#195096=CARTESIAN_POINT('Ctrl Pts',(-0.153561366595031,59.100861741971,
40.0326492435185));
#195097=CARTESIAN_POINT('Ctrl Pts',(-0.151842962926936,59.0985314603578,
40.0348233715062));
#195098=CARTESIAN_POINT('Ctrl Pts',(-0.150055686179523,59.096225375957,
40.0369753512356));
#195099=CARTESIAN_POINT('Ctrl Pts',(-0.148286670996087,59.0939428540559,
40.0391053430352));
#195100=CARTESIAN_POINT('Ctrl Pts',(-0.146452235168277,59.0916862380348,
40.041211089324));
#195101=CARTESIAN_POINT('Ctrl Pts',(-0.14455211660934,59.0894604907299,
40.0432881154904));
#195102=CARTESIAN_POINT('Ctrl Pts',(-0.144419986080793,59.0893057166152,
40.043432547828));
#195103=CARTESIAN_POINT('Ctrl Pts',(-0.144287542501473,59.0891510807051,
40.0435768364421));
#195104=CARTESIAN_POINT('Ctrl Pts',(-0.144154785043317,59.0889965840074,
40.0437209807855));
#195105=CARTESIAN_POINT('Ctrl Pts',(-0.138334211748934,59.0822228828154,
40.0500407968419));
#195106=CARTESIAN_POINT('Ctrl Pts',(-0.131883990153598,59.0757535782847,
40.0560490279343));
#195107=CARTESIAN_POINT('Ctrl Pts',(-0.12480841721487,59.0697047694309,
40.0616647108613));
#195108=CARTESIAN_POINT('Ctrl Pts',(-0.118212753509711,59.0640662283034,
40.0668995033484));
#195109=CARTESIAN_POINT('Ctrl Pts',(-0.111072931137106,59.0587927761315,
40.0717933267479));
#195110=CARTESIAN_POINT('Ctrl Pts',(-0.10338954476808,59.05400766547,40.076246030307));
#195111=CARTESIAN_POINT('Ctrl Pts',(-0.100578862632356,59.0522572100839,
40.0778748868746));
#195112=CARTESIAN_POINT('Ctrl Pts',(-0.0976954648433502,59.0505724231958,
40.0794443522247));
#195113=CARTESIAN_POINT('Ctrl Pts',(-0.0947395585247239,59.048960544286,
40.0809482021492));
#195114=CARTESIAN_POINT('Ctrl Pts',(-0.0940287618032278,59.0485729412563,
40.0813098278168));
#195115=CARTESIAN_POINT('Ctrl Pts',(-0.0933131922161319,59.0481896206935,
40.0816679525672));
#195116=CARTESIAN_POINT('Ctrl Pts',(-0.0925929271965458,59.0478106940136,
40.082022419258));
#195117=CARTESIAN_POINT('Ctrl Pts',(-0.0918951704588219,59.0474436087926,
40.0823658088648));
#195118=CARTESIAN_POINT('Ctrl Pts',(-0.0911930071928013,59.047080647127,
40.0827057654616));
#195119=CARTESIAN_POINT('Ctrl Pts',(-0.090486511587203,59.0467219102889,
40.0830421470151));
#195120=CARTESIAN_POINT('Ctrl Pts',(-0.0827460357491811,59.0427915336441,
40.0867275956807));
#195121=CARTESIAN_POINT('Ctrl Pts',(-0.0744802459935432,59.0393660724129,
40.0899823432031));
#195122=CARTESIAN_POINT('Ctrl Pts',(-0.0658168714599912,59.0365841602689,
40.0926299529357));
#195123=CARTESIAN_POINT('Ctrl Pts',(-0.0622239118135568,59.0354304183829,
40.0937279956085));
#195124=CARTESIAN_POINT('Ctrl Pts',(-0.0585629032857854,59.0343871039216,
40.0947220371803));
#195125=CARTESIAN_POINT('Ctrl Pts',(-0.0548440714993534,59.0334626554262,
40.0956014538693));
#195126=CARTESIAN_POINT('Ctrl Pts',(-0.0485012163577852,59.0318859121827,
40.097101390674));
#195127=CARTESIAN_POINT('Ctrl Pts',(-0.0419914004937971,59.0306571138137,
40.0982667904316));
#195128=CARTESIAN_POINT('Ctrl Pts',(-0.0353717968082022,59.0298212958157,
40.0990539325583));
#195129=CARTESIAN_POINT('Ctrl Pts',(-0.0320619949654048,59.0294033868167,
40.0994475036216));
#195130=CARTESIAN_POINT('Ctrl Pts',(-0.0287246785540554,59.0290851681639,
40.0997467259952));
#195131=CARTESIAN_POINT('Ctrl Pts',(-0.0253670368742458,59.0288723192866,
40.0999473488896));
#195132=CARTESIAN_POINT('Ctrl Pts',(-0.0220093951944362,59.0286594704093,
40.100147971784));
#195133=CARTESIAN_POINT('Ctrl Pts',(-0.0186314705073834,59.0285519740191,
40.10025));
#195134=CARTESIAN_POINT('Ctrl Pts',(-0.0152399999993761,59.0285534841296,
40.10025));
#195135=CARTESIAN_POINT('Origin',(6.10537907909441,57.9430040808457,39.92499));
#195136=CARTESIAN_POINT('Ctrl Pts',(6.73887200051396,62.2936141127569,39.92499));
#195137=CARTESIAN_POINT('Ctrl Pts',(6.73998108195387,62.3041663177856,39.934835464202));
#195138=CARTESIAN_POINT('Ctrl Pts',(6.74025426844153,62.3147747227671,39.9446440828461));
#195139=CARTESIAN_POINT('Ctrl Pts',(6.73970068257655,62.3253809467526,39.9543641760336));
#195140=CARTESIAN_POINT('Ctrl Pts',(6.73916508495579,62.3356425316146,39.9637684240719));
#195141=CARTESIAN_POINT('Ctrl Pts',(6.73785543637705,62.3459033574831,39.9730909636404));
#195142=CARTESIAN_POINT('Ctrl Pts',(6.73573381164837,62.3561113603653,39.982280897715));
#195143=CARTESIAN_POINT('Ctrl Pts',(6.73372688529716,62.3657675025193,39.990974009466));
#195144=CARTESIAN_POINT('Ctrl Pts',(6.73099321743859,62.3753772873486,39.9995492765013));
#195145=CARTESIAN_POINT('Ctrl Pts',(6.72746117704619,62.3848821415117,40.0079462328707));
#195146=CARTESIAN_POINT('Ctrl Pts',(6.72420791240112,62.3936367996045,40.0156804369703));
#195147=CARTESIAN_POINT('Ctrl Pts',(6.72027708243738,62.4023029415008,40.0232638017437));
#195148=CARTESIAN_POINT('Ctrl Pts',(6.71558140886323,62.4108128192398,40.0306257269982));
#195149=CARTESIAN_POINT('Ctrl Pts',(6.71421937245567,62.4132812112865,40.0327611416662));
#195150=CARTESIAN_POINT('Ctrl Pts',(6.71279278199565,62.415736279296,40.0348777427276));
#195151=CARTESIAN_POINT('Ctrl Pts',(6.71129899689659,62.4181758915948,40.0369733168701));
#195152=CARTESIAN_POINT('Ctrl Pts',(6.70967963780731,62.42082058818,40.039245053974));
#195153=CARTESIAN_POINT('Ctrl Pts',(6.70798448411237,62.4234440047028,40.041487875195));
#195154=CARTESIAN_POINT('Ctrl Pts',(6.70621108803186,62.4260429761972,40.0436985701601));
#195155=CARTESIAN_POINT('Ctrl Pts',(6.70134398857332,62.4331758738575,40.0497658398386));
#195156=CARTESIAN_POINT('Ctrl Pts',(6.69585818364757,62.4400912556837,40.0555581699984));
#195157=CARTESIAN_POINT('Ctrl Pts',(6.68976801333951,62.4466864116141,40.0609828468885));
#195158=CARTESIAN_POINT('Ctrl Pts',(6.68419583815079,62.4527206212309,40.0659461317303));
#195159=CARTESIAN_POINT('Ctrl Pts',(6.67811620689403,62.4584752900412,40.0706039980705));
#195160=CARTESIAN_POINT('Ctrl Pts',(6.67150703079275,62.4638645712583,40.0748843180601));
#195161=CARTESIAN_POINT('Ctrl Pts',(6.66826062508144,62.4665117685875,40.0769867972568));
#195162=CARTESIAN_POINT('Ctrl Pts',(6.66488629458054,62.4690703232299,40.0789976708174));
#195163=CARTESIAN_POINT('Ctrl Pts',(6.66138078591774,62.4715267736418,40.08090504915));
#195164=CARTESIAN_POINT('Ctrl Pts',(6.66071564979311,62.4719928611813,40.0812669556104));
#195165=CARTESIAN_POINT('Ctrl Pts',(6.66004526561052,62.4724551899379,40.0816253922032));
#195166=CARTESIAN_POINT('Ctrl Pts',(6.65936969820921,62.4729136358128,40.0819801989139));
#195167=CARTESIAN_POINT('Ctrl Pts',(6.65871524228918,62.4733577552541,40.0823239179149));
#195168=CARTESIAN_POINT('Ctrl Pts',(6.65805592206515,62.4737982306999,40.0826642303498));
#195169=CARTESIAN_POINT('Ctrl Pts',(6.65739180030973,62.4742349489458,40.0830009916099));
#195170=CARTESIAN_POINT('Ctrl Pts',(6.65015433826458,62.4789942144025,40.0866709464313));
#195171=CARTESIAN_POINT('Ctrl Pts',(6.6423416549749,62.483310062658,40.0899175831879));
#195172=CARTESIAN_POINT('Ctrl Pts',(6.63406423386157,62.4870273554129,40.0925642067064));
#195173=CARTESIAN_POINT('Ctrl Pts',(6.63056862752539,62.4885971912264,40.0936818922529));
#195174=CARTESIAN_POINT('Ctrl Pts',(6.62699051141418,62.490060506939,40.0946930094791));
#195175=CARTESIAN_POINT('Ctrl Pts',(6.62333954252063,62.491407022622,40.0955863397546));
#195176=CARTESIAN_POINT('Ctrl Pts',(6.61719140213135,62.4936745213866,40.0970906856166));
#195177=CARTESIAN_POINT('Ctrl Pts',(6.61083770188589,62.495608491139,40.0982599215483));
#195178=CARTESIAN_POINT('Ctrl Pts',(6.60433062536211,62.4971561593221,40.0990497370454));
#195179=CARTESIAN_POINT('Ctrl Pts',(6.60270385623117,62.4975430763678,40.0992471909196));
#195180=CARTESIAN_POINT('Ctrl Pts',(6.60106746196622,62.4979056188883,40.0994209989363));
#195181=CARTESIAN_POINT('Ctrl Pts',(6.5994222184581,62.4982426563695,40.0995705982975));
#195182=CARTESIAN_POINT('Ctrl Pts',(6.59695435319593,62.4987482125912,40.0997949973393));
#195183=CARTESIAN_POINT('Ctrl Pts',(6.59446659126666,62.4991963674672,40.0999649129781));
#195184=CARTESIAN_POINT('Ctrl Pts',(6.59196174500359,62.4995849724121,40.1000786629733));
#195185=CARTESIAN_POINT('Ctrl Pts',(6.58945689874052,62.4999735773569,40.1001924129685));
#195186=CARTESIAN_POINT('Ctrl Pts',(6.58693497617713,62.5003026407461,40.10025));
#195187=CARTESIAN_POINT('Ctrl Pts',(6.58439859103091,62.500570298093,40.10025));
#195188=CARTESIAN_POINT('Ctrl Pts',(6.18532049829458,58.7035958781038,40.10025));
#195189=CARTESIAN_POINT('Ctrl Pts',(6.19390281910209,58.7026899760169,40.10025));
#195190=CARTESIAN_POINT('Ctrl Pts',(6.20248552904414,58.7025003609928,40.0995786334241));
#195191=CARTESIAN_POINT('Ctrl Pts',(6.21093474935464,58.7029569544313,40.0983063763367));
#195192=CARTESIAN_POINT('Ctrl Pts',(6.21639207873535,58.7032518669434,40.0974846287993));
#195193=CARTESIAN_POINT('Ctrl Pts',(6.22179377937559,58.7038154335198,40.0964130309338));
#195194=CARTESIAN_POINT('Ctrl Pts',(6.22710604846914,58.7046202140515,40.0951176960924));
#195195=CARTESIAN_POINT('Ctrl Pts',(6.23414715684692,58.7056869045457,40.0934008039614));
#195196=CARTESIAN_POINT('Ctrl Pts',(6.24102913891695,58.7071827955651,40.0912909372156));
#195197=CARTESIAN_POINT('Ctrl Pts',(6.247679224408,58.7090548163569,40.0888630467851));
#195198=CARTESIAN_POINT('Ctrl Pts',(6.25100426715352,58.7099908267527,40.0876491015699));
#195199=CARTESIAN_POINT('Ctrl Pts',(6.25427153376716,58.7110208470227,40.0863558569271));
#195200=CARTESIAN_POINT('Ctrl Pts',(6.25747333351573,58.7121380880307,40.0849936342771));
#195201=CARTESIAN_POINT('Ctrl Pts',(6.25907423339001,58.7126967085346,40.0843125229521));
#195202=CARTESIAN_POINT('Ctrl Pts',(6.26065878288398,58.713277132457,40.0836141747074));
#195203=CARTESIAN_POINT('Ctrl Pts',(6.2622261232057,58.7138784999415,40.0828999161609));
#195204=CARTESIAN_POINT('Ctrl Pts',(6.26261795828614,58.7140288418126,40.0827213515243));
#195205=CARTESIAN_POINT('Ctrl Pts',(6.26300871814066,58.7141804926177,40.0825417925842));
#195206=CARTESIAN_POINT('Ctrl Pts',(6.2633983900511,58.7143334388435,40.082361260236));
#195207=CARTESIAN_POINT('Ctrl Pts',(6.26456740578241,58.7147922775207,40.0818196631917));
#195208=CARTESIAN_POINT('Ctrl Pts',(6.26572662828426,58.715262775183,40.0812693052021));
#195209=CARTESIAN_POINT('Ctrl Pts',(6.2668757296522,58.7157445651923,40.0807107531875));
#195210=CARTESIAN_POINT('Ctrl Pts',(6.27496985131196,58.7191382318077,40.0767763849182));
#195211=CARTESIAN_POINT('Ctrl Pts',(6.2826071619282,58.7230632421217,40.0724140586138));
#195212=CARTESIAN_POINT('Ctrl Pts',(6.28978339589494,58.7274000190313,40.0677221223769));
#195213=CARTESIAN_POINT('Ctrl Pts',(6.29326386161416,58.7295033511461,40.0654465383721));
#195214=CARTESIAN_POINT('Ctrl Pts',(6.2966359740898,58.731704109697,40.0630928000679));
#195215=CARTESIAN_POINT('Ctrl Pts',(6.29989941779205,58.7339915094193,40.0606689262479));
#195216=CARTESIAN_POINT('Ctrl Pts',(6.30489552208994,58.7374933585781,40.0569581447805));
#195217=CARTESIAN_POINT('Ctrl Pts',(6.30963480180928,58.7411954596216,40.0530843804605));
#195218=CARTESIAN_POINT('Ctrl Pts',(6.31410463171103,58.7450534628849,40.0490800251457));
#195219=CARTESIAN_POINT('Ctrl Pts',(6.31618044384123,58.7468451395591,40.0472203818218));
#195220=CARTESIAN_POINT('Ctrl Pts',(6.31819823791584,58.7486702031823,40.0453323608818));
#195221=CARTESIAN_POINT('Ctrl Pts',(6.32015576082374,58.7505249478604,40.0434201572162));
#195222=CARTESIAN_POINT('Ctrl Pts',(6.3203057972416,58.750667106732,40.0432735943397));
#195223=CARTESIAN_POINT('Ctrl Pts',(6.32045551058247,58.7508094261758,40.0431268995707));
#195224=CARTESIAN_POINT('Ctrl Pts',(6.32060490094056,58.7509519047345,40.0429800745037));
#195225=CARTESIAN_POINT('Ctrl Pts',(6.3227033850744,58.7529532989256,40.0409176249753));
#195226=CARTESIAN_POINT('Ctrl Pts',(6.32473679726686,58.7549876922214,40.0388310783332));
#195227=CARTESIAN_POINT('Ctrl Pts',(6.32670504965044,58.7570493794209,40.036725739981));
#195228=CARTESIAN_POINT('Ctrl Pts',(6.3337628526564,58.7644422230598,40.0291763710714));
#195229=CARTESIAN_POINT('Ctrl Pts',(6.34003880539004,58.7722418109929,40.0213310894587));
#195230=CARTESIAN_POINT('Ctrl Pts',(6.34560292136835,58.7803396486563,40.0132837551308));
#195231=CARTESIAN_POINT('Ctrl Pts',(6.35171732586353,58.7892383587484,40.0044405431308));
#195232=CARTESIAN_POINT('Ctrl Pts',(6.35697262978608,58.7984976730916,39.9953528710578));
#195233=CARTESIAN_POINT('Ctrl Pts',(6.36142852992988,58.8080148760677,39.9861103629527));
#195234=CARTESIAN_POINT('Ctrl Pts',(6.36623978380702,58.8182910667901,39.9761307737519));
#195235=CARTESIAN_POINT('Ctrl Pts',(6.3701196826395,58.8288688921899,39.9659696935964));
#195236=CARTESIAN_POINT('Ctrl Pts',(6.37309732670023,58.8396533761938,39.9557128217449));
#195237=CARTESIAN_POINT('Ctrl Pts',(6.37604999138599,58.8503473894549,39.9455419945122));
#195238=CARTESIAN_POINT('Ctrl Pts',(6.37811557911308,58.8612460403482,39.9352756289321));
#195239=CARTESIAN_POINT('Ctrl Pts',(6.37927424642637,58.872270023448,39.92499));
#195240=CARTESIAN_POINT('Origin',(-0.0151565136854075,0.0015930137801936,
39.92499));
#195241=CARTESIAN_POINT('Ctrl Pts',(6.55408556366009,62.5037563256534,40.10025));
#195242=CARTESIAN_POINT('Ctrl Pts',(6.54554330587477,62.5046505412977,40.10025));
#195243=CARTESIAN_POINT('Ctrl Pts',(6.53700226086738,62.5048232320878,40.0995859581842));
#195244=CARTESIAN_POINT('Ctrl Pts',(6.5285945717753,62.5043472028589,40.0983275959621));
#195245=CARTESIAN_POINT('Ctrl Pts',(6.52322245869558,62.5040430428431,40.0975235624068));
#195246=CARTESIAN_POINT('Ctrl Pts',(6.51790471489673,62.5034749678471,40.096477705949));
#195247=CARTESIAN_POINT('Ctrl Pts',(6.51267356740911,62.5026702669706,40.0952149915961));
#195248=CARTESIAN_POINT('Ctrl Pts',(6.50553410072716,62.5015720117389,40.0934916398701));
#195249=CARTESIAN_POINT('Ctrl Pts',(6.49855818190839,62.5000273428097,40.091364392163));
#195250=CARTESIAN_POINT('Ctrl Pts',(6.49182203260242,62.4980940659028,40.0889118607713));
#195251=CARTESIAN_POINT('Ctrl Pts',(6.48845395794943,62.4971274274494,40.0876855950754));
#195252=CARTESIAN_POINT('Ctrl Pts',(6.48514561818799,62.4960636607365,40.0863782327526));
#195253=CARTESIAN_POINT('Ctrl Pts',(6.48190505740227,62.4949101555729,40.0850006373334));
#195254=CARTESIAN_POINT('Ctrl Pts',(6.48028477700941,62.4943334029911,40.0843118396237));
#195255=CARTESIAN_POINT('Ctrl Pts',(6.47868142404744,62.4937342176672,40.0836054919164));
#195256=CARTESIAN_POINT('Ctrl Pts',(6.47709589524329,62.4931135352113,40.0828829920417));
#195257=CARTESIAN_POINT('Ctrl Pts',(6.47669951304225,62.4929583645973,40.0827023670731));
#195258=CARTESIAN_POINT('Ctrl Pts',(6.47630424448236,62.4928018504534,40.0825207326933));
#195259=CARTESIAN_POINT('Ctrl Pts',(6.47591010283136,62.4926440074816,40.0823381109275));
#195260=CARTESIAN_POINT('Ctrl Pts',(6.47472767787837,62.492170478566,40.0817902456303));
#195261=CARTESIAN_POINT('Ctrl Pts',(6.47355539694531,62.4916849899863,40.0812334935553));
#195262=CARTESIAN_POINT('Ctrl Pts',(6.47239360181873,62.4911879405751,40.0806684524227));
#195263=CARTESIAN_POINT('Ctrl Pts',(6.46436487665231,62.4877530207468,40.0767636676136));
#195264=CARTESIAN_POINT('Ctrl Pts',(6.45678933786444,62.4837949925046,40.0724404510887));
#195265=CARTESIAN_POINT('Ctrl Pts',(6.44966853564036,62.4794326364364,40.0677949937408));
#195266=CARTESIAN_POINT('Ctrl Pts',(6.44612951648131,62.4772645574451,40.0654862141905));
#195267=CARTESIAN_POINT('Ctrl Pts',(6.44270272394404,62.474996003895,40.0630972003215));
#195268=CARTESIAN_POINT('Ctrl Pts',(6.43938822718986,62.4726384024733,40.0606363359906));
#195269=CARTESIAN_POINT('Ctrl Pts',(6.43207595228416,62.4674371815966,40.0552073017123));
#195270=CARTESIAN_POINT('Ctrl Pts',(6.42530381744052,62.4618132330509,40.0494204304519));
#195271=CARTESIAN_POINT('Ctrl Pts',(6.41913840445487,62.455895762341,40.0434049749851));
#195272=CARTESIAN_POINT('Ctrl Pts',(6.41688610134127,62.4537340356674,40.0412074532442));
#195273=CARTESIAN_POINT('Ctrl Pts',(6.4147074139753,62.4515361835425,40.0389814735788));
#195274=CARTESIAN_POINT('Ctrl Pts',(6.41260146153701,62.4493074469122,40.0367321210017));
#195275=CARTESIAN_POINT('Ctrl Pts',(6.40552779014142,62.4418213564085,40.0291767837138));
#195276=CARTESIAN_POINT('Ctrl Pts',(6.39923601079921,62.4339335724859,40.0213235332571));
#195277=CARTESIAN_POINT('Ctrl Pts',(6.39365709371064,62.4257522463021,40.0132649215851));
#195278=CARTESIAN_POINT('Ctrl Pts',(6.38752520296412,62.4167599996842,40.0044075527522));
#195279=CARTESIAN_POINT('Ctrl Pts',(6.38225398283479,62.4074126717497,39.9953016253706));
#195280=CARTESIAN_POINT('Ctrl Pts',(6.37778536209598,62.3978127557438,39.9860353422341));
#195281=CARTESIAN_POINT('Ctrl Pts',(6.3729724660951,62.3874732348817,39.9760551582674));
#195282=CARTESIAN_POINT('Ctrl Pts',(6.36908997057791,62.3768396913499,39.9658879738131));
#195283=CARTESIAN_POINT('Ctrl Pts',(6.36611161569965,62.3660067738133,39.9556174643225));
#195284=CARTESIAN_POINT('Ctrl Pts',(6.36317347866869,62.355320137241,39.9454856413885));
#195285=CARTESIAN_POINT('Ctrl Pts',(6.36111515612501,62.344438041129,39.9352519465104));
#195286=CARTESIAN_POINT('Ctrl Pts',(6.35995915837865,62.3334394572618,39.92499));
#195287=CARTESIAN_POINT('Ctrl Pts',(6.00036140429106,58.9120953679529,39.92499));
#195288=CARTESIAN_POINT('Ctrl Pts',(5.99925510810176,58.9015696628136,39.9348107241731));
#195289=CARTESIAN_POINT('Ctrl Pts',(5.99898299131239,58.8909945468879,39.9446038383187));
#195290=CARTESIAN_POINT('Ctrl Pts',(5.99953795195324,58.8804276387757,39.9543158069411));
#195291=CARTESIAN_POINT('Ctrl Pts',(6.00007381527955,58.8702243592762,39.9636935671423));
#195292=CARTESIAN_POINT('Ctrl Pts',(6.0013809572776,58.8600274753995,39.9729968321026));
#195293=CARTESIAN_POINT('Ctrl Pts',(6.00349883564084,58.8498890377446,39.9821731151378));
#195294=CARTESIAN_POINT('Ctrl Pts',(6.00550089397251,58.8403050389987,39.9908475764398));
#195295=CARTESIAN_POINT('Ctrl Pts',(6.00822762538762,58.8307723843828,39.9994093733896));
#195296=CARTESIAN_POINT('Ctrl Pts',(6.01175153639814,58.8213500689001,40.0077966115894));
#195297=CARTESIAN_POINT('Ctrl Pts',(6.01499699932078,58.8126722744117,40.015521117265));
#195298=CARTESIAN_POINT('Ctrl Pts',(6.01891888229525,58.8040875818502,40.0230979941079));
#195299=CARTESIAN_POINT('Ctrl Pts',(6.02360485257848,58.7956642413002,40.0304554104807));
#195300=CARTESIAN_POINT('Ctrl Pts',(6.0250021143232,58.7931525711866,40.032649243522));
#195301=CARTESIAN_POINT('Ctrl Pts',(6.02646752363906,58.7906554330073,40.034823371508));
#195302=CARTESIAN_POINT('Ctrl Pts',(6.02800395803763,58.7881751602883,40.0369753512355));
#195303=CARTESIAN_POINT('Ctrl Pts',(6.0295246938641,58.7857202298424,40.0391053430351));
#195304=CARTESIAN_POINT('Ctrl Pts',(6.03111319985562,58.7832842250419,40.041211089324));
#195305=CARTESIAN_POINT('Ctrl Pts',(6.03277025542088,58.7808720541406,40.0432881154904));
#195306=CARTESIAN_POINT('Ctrl Pts',(6.0328854838242,58.7807043164936,40.0434325478279));
#195307=CARTESIAN_POINT('Ctrl Pts',(6.03300103800968,58.7805366835714,40.0435768364421));
#195308=CARTESIAN_POINT('Ctrl Pts',(6.0331169189062,58.7803691562897,40.0437209807855));
#195309=CARTESIAN_POINT('Ctrl Pts',(6.03819756191488,58.7730241465597,40.050040796842));
#195310=CARTESIAN_POINT('Ctrl Pts',(6.04393622206048,58.7659160498049,40.0560490279345));
#195311=CARTESIAN_POINT('Ctrl Pts',(6.05034076157633,58.7591607781928,40.0616647108615));
#195312=CARTESIAN_POINT('Ctrl Pts',(6.05631090550653,58.7528636909922,40.0668995033486));
#195313=CARTESIAN_POINT('Ctrl Pts',(6.06286038933357,58.7468728126824,40.0717933267482));
#195314=CARTESIAN_POINT('Ctrl Pts',(6.07000150504423,58.741310782788,40.0762460303072));
#195315=CARTESIAN_POINT('Ctrl Pts',(6.07261381755745,58.7392761202953,40.0778748868748));
#195316=CARTESIAN_POINT('Ctrl Pts',(6.07530531160718,58.7372991657064,40.0794443522247));
#195317=CARTESIAN_POINT('Ctrl Pts',(6.07807653793614,58.735387140493,40.0809482021492));
#195318=CARTESIAN_POINT('Ctrl Pts',(6.07874292528977,58.7349273623042,40.0813098278168));
#195319=CARTESIAN_POINT('Ctrl Pts',(6.07941450700242,58.7344713442222,40.0816679525672));
#195320=CARTESIAN_POINT('Ctrl Pts',(6.08009121771133,58.7340192051468,40.082022419258));
#195321=CARTESIAN_POINT('Ctrl Pts',(6.0807467812106,58.7335811954174,40.0823658088648));
#195322=CARTESIAN_POINT('Ctrl Pts',(6.08140715812765,58.7331468260467,40.0827057654616));
#195323=CARTESIAN_POINT('Ctrl Pts',(6.08207228526599,58.7327162055065,40.0830421470151));
#195324=CARTESIAN_POINT('Ctrl Pts',(6.08935952173653,58.727998259832,40.0867275956806));
#195325=CARTESIAN_POINT('Ctrl Pts',(6.09722197243233,58.7237275533351,40.089982343203));
#195326=CARTESIAN_POINT('Ctrl Pts',(6.10554709909211,58.7200553115703,40.0926299529355));
#195327=CARTESIAN_POINT('Ctrl Pts',(6.10899977726353,58.7185323234525,40.0937279956084));
#195328=CARTESIAN_POINT('Ctrl Pts',(6.11253167434641,58.7171120447815,40.0947220371802));
#195329=CARTESIAN_POINT('Ctrl Pts',(6.11613350280284,58.7158039367398,40.0956014538692));
#195330=CARTESIAN_POINT('Ctrl Pts',(6.12227679657208,58.7135728221601,40.097101390674));
#195331=CARTESIAN_POINT('Ctrl Pts',(6.12862250657844,58.7116702942287,40.0982667904316));
#195332=CARTESIAN_POINT('Ctrl Pts',(6.13511848061154,58.7101471179285,40.0990539325582));
#195333=CARTESIAN_POINT('Ctrl Pts',(6.13836646762808,58.7093855297784,40.0994475036216));
#195334=CARTESIAN_POINT('Ctrl Pts',(6.14165223896418,58.7087202098048,40.0997467259952));
#195335=CARTESIAN_POINT('Ctrl Pts',(6.14496923836549,58.7081575578109,40.0999473488896));
#195336=CARTESIAN_POINT('Ctrl Pts',(6.14828623776681,58.707594905817,40.100147971784));
#195337=CARTESIAN_POINT('Ctrl Pts',(6.15163442139651,58.7071349090266,40.10025));
#195338=CARTESIAN_POINT('Ctrl Pts',(6.15500747092375,58.7067819056642,40.10025));
#195339=CARTESIAN_POINT('Origin',(12.128626347365,56.9874003490101,39.92499));
#195340=CARTESIAN_POINT('Ctrl Pts',(13.21341150919,61.2479592423876,39.92499));
#195341=CARTESIAN_POINT('Ctrl Pts',(13.2156175207415,61.2583377107545,39.9348354642021));
#195342=CARTESIAN_POINT('Ctrl Pts',(13.2169980909554,61.2688594460197,39.9446440828464));
#195343=CARTESIAN_POINT('Ctrl Pts',(13.217556189986,61.2794654334803,39.954364176034));
#195344=CARTESIAN_POINT('Ctrl Pts',(13.2180961541214,61.2897267895029,39.9637684240723));
#195345=CARTESIAN_POINT('Ctrl Pts',(13.2178662282945,61.3000683010471,39.9730909636408));
#195346=CARTESIAN_POINT('Ctrl Pts',(13.2168232529023,61.310442153594,39.9822808977153));
#195347=CARTESIAN_POINT('Ctrl Pts',(13.2158366624041,61.3202551793184,39.9909740094663));
#195348=CARTESIAN_POINT('Ctrl Pts',(13.2141224659046,61.3300980668413,39.9995492765015));
#195349=CARTESIAN_POINT('Ctrl Pts',(13.2116033021983,61.3399200511732,40.0079462328709));
#195350=CARTESIAN_POINT('Ctrl Pts',(13.2092829702343,61.3489668090869,40.0156804369705));
#195351=CARTESIAN_POINT('Ctrl Pts',(13.2062795322632,61.3579963605666,40.0232638017438));
#195352=CARTESIAN_POINT('Ctrl Pts',(13.2024991065229,61.3669504518477,40.0306257269983));
#195353=CARTESIAN_POINT('Ctrl Pts',(13.2014025487207,61.3695476933571,40.0327611416663));
#195354=CARTESIAN_POINT('Ctrl Pts',(13.2002403977587,61.3721384315556,40.0348777427276));
#195355=CARTESIAN_POINT('Ctrl Pts',(13.1990098046953,61.3747208224638,40.0369733168701));
#195356=CARTESIAN_POINT('Ctrl Pts',(13.1976757626944,61.3775203002415,40.039245053974));
#195357=CARTESIAN_POINT('Ctrl Pts',(13.1962641169264,61.3803065372248,40.041487875195));
#195358=CARTESIAN_POINT('Ctrl Pts',(13.1947721021916,61.3830766416485,40.0436985701601));
#195359=CARTESIAN_POINT('Ctrl Pts',(13.1906772560442,61.390679214976,40.0497658398386));
#195360=CARTESIAN_POINT('Ctrl Pts',(13.185944357167,61.3981301363757,40.0555581699984));
#195361=CARTESIAN_POINT('Ctrl Pts',(13.1805769309636,61.4053257594952,40.0609828468885));
#195362=CARTESIAN_POINT('Ctrl Pts',(13.1756660273918,61.41190936399,40.0659461317304));
#195363=CARTESIAN_POINT('Ctrl Pts',(13.1702212276784,61.418268002635,40.0706039980706));
#195364=CARTESIAN_POINT('Ctrl Pts',(13.164211590619,61.4243186078272,40.0748843180603));
#195365=CARTESIAN_POINT('Ctrl Pts',(13.1612596765267,61.4272906453324,40.0769867972569));
#195366=CARTESIAN_POINT('Ctrl Pts',(13.1581712727464,61.4301878975265,40.0789976708174));
#195367=CARTESIAN_POINT('Ctrl Pts',(13.1549417366136,61.4329973166794,40.0809050491499));
#195368=CARTESIAN_POINT('Ctrl Pts',(13.1543289635885,61.4335303765996,40.0812669556104));
#195369=CARTESIAN_POINT('Ctrl Pts',(13.1537105783551,61.4340602468993,40.0816253922032));
#195370=CARTESIAN_POINT('Ctrl Pts',(13.1530866324254,61.434586797382,40.0819801989139));
#195371=CARTESIAN_POINT('Ctrl Pts',(13.1524821848061,61.4350968931621,40.0823239179149));
#195372=CARTESIAN_POINT('Ctrl Pts',(13.1518725186287,61.4356038733671,40.0826642303498));
#195373=CARTESIAN_POINT('Ctrl Pts',(13.1512576844889,61.4361076188514,40.0830009916099));
#195374=CARTESIAN_POINT('Ctrl Pts',(13.1445573487227,61.4415973333394,40.0866709464312));
#195375=CARTESIAN_POINT('Ctrl Pts',(13.1372385931155,61.4467061867047,40.0899175831878));
#195376=CARTESIAN_POINT('Ctrl Pts',(13.1293950794805,61.4512683418497,40.0925642067062));
#195377=CARTESIAN_POINT('Ctrl Pts',(13.1260827149666,61.453194968297,40.0936818922528));
#195378=CARTESIAN_POINT('Ctrl Pts',(13.1226771582924,61.4550242827915,40.094693009479));
#195379=CARTESIAN_POINT('Ctrl Pts',(13.1191869390034,61.4567450522887,40.0955863397545));
#195380=CARTESIAN_POINT('Ctrl Pts',(13.1133094969318,61.4596427851247,40.0970906856166));
#195381=CARTESIAN_POINT('Ctrl Pts',(13.1071927578073,61.4622303029111,40.0982599215483));
#195382=CARTESIAN_POINT('Ctrl Pts',(13.1008831031063,61.464449667515,40.0990497370454));
#195383=CARTESIAN_POINT('Ctrl Pts',(13.0993056894311,61.465004508666,40.0992471909196));
#195384=CARTESIAN_POINT('Ctrl Pts',(13.0977161555177,61.4655361149184,40.0994209989363));
#195385=CARTESIAN_POINT('Ctrl Pts',(13.0961151548356,61.4660432808487,40.0995705982975));
#195386=CARTESIAN_POINT('Ctrl Pts',(13.0937136538125,61.466804029744,40.0997949973393));
#195387=CARTESIAN_POINT('Ctrl Pts',(13.0912863650439,61.4675097715122,40.0999649129781));
#195388=CARTESIAN_POINT('Ctrl Pts',(13.0888358608685,61.4681580753691,40.1000786629733));
#195389=CARTESIAN_POINT('Ctrl Pts',(13.086385356693,61.4688063792261,40.1001924129685));
#195390=CARTESIAN_POINT('Ctrl Pts',(13.0839116459757,61.4693972526618,40.10025));
#195391=CARTESIAN_POINT('Ctrl Pts',(13.0814171332239,61.4699285681953,40.10025));
#195392=CARTESIAN_POINT('Ctrl Pts',(12.2876333308477,57.7354693911203,40.10025));
#195393=CARTESIAN_POINT('Ctrl Pts',(12.2960739442514,57.7336713548545,40.10025));
#195394=CARTESIAN_POINT('Ctrl Pts',(12.3045898170438,57.7325856410803,40.099578633424));
#195395=CARTESIAN_POINT('Ctrl Pts',(12.3130404786523,57.7321565492374,40.0983063763364));
#195396=CARTESIAN_POINT('Ctrl Pts',(12.3184987389629,57.7318793999342,40.0974846287991));
#195397=CARTESIAN_POINT('Ctrl Pts',(12.3239297572695,57.731875247767,40.0964130309337));
#195398=CARTESIAN_POINT('Ctrl Pts',(12.3292970476689,57.732120336302,40.0951176960923));
#195399=CARTESIAN_POINT('Ctrl Pts',(12.3364110836364,57.7324451871156,40.0934008039614));
#195400=CARTESIAN_POINT('Ctrl Pts',(12.3434117286781,57.7332135204775,40.0912909372156));
#195401=CARTESIAN_POINT('Ctrl Pts',(12.3502210637615,57.7343801629265,40.0888630467851));
#195402=CARTESIAN_POINT('Ctrl Pts',(12.3536257313032,57.734963484151,40.0876491015699));
#195403=CARTESIAN_POINT('Ctrl Pts',(12.3569827659245,57.735646339504,40.0863558569271));
#195404=CARTESIAN_POINT('Ctrl Pts',(12.3602838093647,57.7364227809414,40.0849936342771));
#195405=CARTESIAN_POINT('Ctrl Pts',(12.3619343310847,57.7368110016601,40.0843125229521));
#195406=CARTESIAN_POINT('Ctrl Pts',(12.3635708710714,57.7372226154359,40.0836141747074));
#195407=CARTESIAN_POINT('Ctrl Pts',(12.3651924853579,57.7376568568911,40.0828999161609));
#195408=CARTESIAN_POINT('Ctrl Pts',(12.3655978889295,57.7377654172549,40.0827213515243));
#195409=CARTESIAN_POINT('Ctrl Pts',(12.3660023599863,57.737875391774,40.0825417925841));
#195410=CARTESIAN_POINT('Ctrl Pts',(12.3664058844671,57.7379867683383,40.082361260236));
#195411=CARTESIAN_POINT('Ctrl Pts',(12.3676164579098,57.7383208980313,40.0818196631917));
#195412=CARTESIAN_POINT('Ctrl Pts',(12.3688185104671,57.7386676465114,40.0812693052021));
#195413=CARTESIAN_POINT('Ctrl Pts',(12.3700116777068,57.7390266834245,40.0807107531874));
#195414=CARTESIAN_POINT('Ctrl Pts',(12.3784161936773,57.7415556930806,40.0767763849182));
#195415=CARTESIAN_POINT('Ctrl Pts',(12.3864219416033,57.7446608854351,40.0724140586138));
#195416=CARTESIAN_POINT('Ctrl Pts',(12.3940121800354,57.7482237843184,40.0677221223769));
#195417=CARTESIAN_POINT('Ctrl Pts',(12.397693437473,57.7499517864267,40.0654465383721));
#195418=CARTESIAN_POINT('Ctrl Pts',(12.401277119073,57.751788007257,40.0630928000679));
#195419=CARTESIAN_POINT('Ctrl Pts',(12.4047617836671,57.7537217536092,40.0606689262479));
#195420=CARTESIAN_POINT('Ctrl Pts',(12.410096561694,57.7566821841673,40.0569581447805));
#195421=CARTESIAN_POINT('Ctrl Pts',(12.4151968540761,57.7598686150879,40.0530843804606));
#195422=CARTESIAN_POINT('Ctrl Pts',(12.4200454689344,57.763238259355,40.0490800251458));
#195423=CARTESIAN_POINT('Ctrl Pts',(12.422297190758,57.7648031395848,40.0472203818218));
#195424=CARTESIAN_POINT('Ctrl Pts',(12.4244947022414,57.7664072884047,40.0453323608818));
#195425=CARTESIAN_POINT('Ctrl Pts',(12.426635375245,57.7680472557361,40.0434201572162));
#195426=CARTESIAN_POINT('Ctrl Pts',(12.426799449396,57.7681729527702,40.0432735943397));
#195427=CARTESIAN_POINT('Ctrl Pts',(12.4269632190243,57.7682988432678,40.0431268995707));
#195428=CARTESIAN_POINT('Ctrl Pts',(12.4271266840712,57.7684249257695,40.0429800745037));
#195429=CARTESIAN_POINT('Ctrl Pts',(12.4294228751485,57.7701960047921,40.0409176249753));
#195430=CARTESIAN_POINT('Ctrl Pts',(12.4316578001011,57.7720067040169,40.0388310783332));
#195431=CARTESIAN_POINT('Ctrl Pts',(12.4338307751869,57.7738513586812,40.036725739981));
#195432=CARTESIAN_POINT('Ctrl Pts',(12.4416226773936,57.7804659622463,40.029176371072));
#195433=CARTESIAN_POINT('Ctrl Pts',(12.4486795287417,57.7875668075252,40.02133108946));
#195434=CARTESIAN_POINT('Ctrl Pts',(12.4550596184368,57.7950386758933,40.0132837551328));
#195435=CARTESIAN_POINT('Ctrl Pts',(12.4620706960749,57.8032495086139,40.0044405431337));
#195436=CARTESIAN_POINT('Ctrl Pts',(12.4682650727914,57.8119087706204,39.9953528710616));
#195437=CARTESIAN_POINT('Ctrl Pts',(12.4736913816495,57.8209080689672,39.9861103629574));
#195438=CARTESIAN_POINT('Ctrl Pts',(12.4795504333984,57.8306250526661,39.9761307737579));
#195439=CARTESIAN_POINT('Ctrl Pts',(12.4845147615727,57.8407393717674,39.965969693604));
#195440=CARTESIAN_POINT('Ctrl Pts',(12.4886033793277,57.8511535286802,39.9557128217539));
#195441=CARTESIAN_POINT('Ctrl Pts',(12.4926576977815,57.8614803215184,39.9455419945183));
#195442=CARTESIAN_POINT('Ctrl Pts',(12.4958511892337,57.872103355754,39.9352756289352));
#195443=CARTESIAN_POINT('Ctrl Pts',(12.4981558292594,57.8829458346104,39.92499));
#195444=CARTESIAN_POINT('Origin',(-0.0149069694351787,0.0031685741680573,
39.92499));
#195445=CARTESIAN_POINT('Ctrl Pts',(13.0516031943535,61.4762657165314,40.10025));
#195446=CARTESIAN_POINT('Ctrl Pts',(13.0432012029373,61.478047942648,40.10025));
#195447=CARTESIAN_POINT('Ctrl Pts',(13.0347249977711,61.4791124697292,40.0995859581842));
#195448=CARTESIAN_POINT('Ctrl Pts',(13.0263136082758,61.4795178910586,40.0983275959621));
#195449=CARTESIAN_POINT('Ctrl Pts',(13.0209391308145,61.4797769359879,40.0975235624068));
#195450=CARTESIAN_POINT('Ctrl Pts',(13.0155911381662,61.4797678285535,40.096477705949));
#195451=CARTESIAN_POINT('Ctrl Pts',(13.0103045333058,61.4795143397207,40.0952149915961));
#195452=CARTESIAN_POINT('Ctrl Pts',(13.0030893784377,61.4791683783268,40.0934916398701));
#195453=CARTESIAN_POINT('Ctrl Pts',(12.9959902125627,61.4783613533297,40.091364392163));
#195454=CARTESIAN_POINT('Ctrl Pts',(12.9890888821233,61.4771427864513,40.0889118607713));
#195455=CARTESIAN_POINT('Ctrl Pts',(12.9856382169037,61.4765335030121,40.0876855950754));
#195456=CARTESIAN_POINT('Ctrl Pts',(12.9822368066738,61.4758213793958,40.0863782327526));
#195457=CARTESIAN_POINT('Ctrl Pts',(12.978893423897,61.4750129240932,40.0850006373334));
#195458=CARTESIAN_POINT('Ctrl Pts',(12.9772217325086,61.474608696442,40.0843118396237));
#195459=CARTESIAN_POINT('Ctrl Pts',(12.9755645309608,61.4741803895392,40.0836054919164));
#195460=CARTESIAN_POINT('Ctrl Pts',(12.9739228088661,61.473728840136,40.0828829920417));
#195461=CARTESIAN_POINT('Ctrl Pts',(12.9735123783424,61.4736159527852,40.0827023670731));
#195462=CARTESIAN_POINT('Ctrl Pts',(12.9731029149221,61.4735016128573,40.0825207326933));
#195463=CARTESIAN_POINT('Ctrl Pts',(12.972694433337,61.4733858335869,40.0823381109275));
#195464=CARTESIAN_POINT('Ctrl Pts',(12.9714689885818,61.4730384957756,40.0817902456303));
#195465=CARTESIAN_POINT('Ctrl Pts',(12.9702523821512,61.4726782034776,40.0812334935553));
#195466=CARTESIAN_POINT('Ctrl Pts',(12.9690449956487,61.4723053176142,40.0806684524227));
#195467=CARTESIAN_POINT('Ctrl Pts',(12.9607012057877,61.4697284449398,40.0767636676136));
#195468=CARTESIAN_POINT('Ctrl Pts',(12.9527534399842,61.4665839586184,40.0724404510887));
#195469=CARTESIAN_POINT('Ctrl Pts',(12.9452156558837,61.4629898265069,40.0677949937407));
#195470=CARTESIAN_POINT('Ctrl Pts',(12.9414693978767,61.4612035527132,40.0654862141904));
#195471=CARTESIAN_POINT('Ctrl Pts',(12.9378242492511,61.4593056238947,40.0630972003215));
#195472=CARTESIAN_POINT('Ctrl Pts',(12.9342814732034,61.4573073969126,40.0606363359906));
#195473=CARTESIAN_POINT('Ctrl Pts',(12.9264655800794,61.4528990097269,40.0552073017123));
#195474=CARTESIAN_POINT('Ctrl Pts',(12.919142681,61.4480137506081,40.0494204304519));
#195475=CARTESIAN_POINT('Ctrl Pts',(12.912392498672,61.4427731575666,40.0434049749851));
#195476=CARTESIAN_POINT('Ctrl Pts',(12.9099265719433,61.4408587028412,40.0412074532442));
#195477=CARTESIAN_POINT('Ctrl Pts',(12.9075300815496,61.4389006256225,40.0389814735788));
#195478=CARTESIAN_POINT('Ctrl Pts',(12.9052026993241,61.4369042302168,40.0367321210016));
#195479=CARTESIAN_POINT('Ctrl Pts',(12.8973852687046,61.430198549301,40.029176783714));
#195480=CARTESIAN_POINT('Ctrl Pts',(12.8903034584561,61.4230116455102,40.0213235332574));
#195481=CARTESIAN_POINT('Ctrl Pts',(12.8838999218057,61.4154582931175,40.0132649215856));
#195482=CARTESIAN_POINT('Ctrl Pts',(12.8768616764782,61.4071562640844,40.004407552753));
#195483=CARTESIAN_POINT('Ctrl Pts',(12.8706422708197,61.3984111343304,39.9953016253716));
#195484=CARTESIAN_POINT('Ctrl Pts',(12.8651946651854,61.3893309057279,39.9860353422353));
#195485=CARTESIAN_POINT('Ctrl Pts',(12.8593273605059,61.3795511104661,39.9760551582689));
#195486=CARTESIAN_POINT('Ctrl Pts',(12.8543546257409,61.3693816498889,39.9658879738149));
#195487=CARTESIAN_POINT('Ctrl Pts',(12.8502602383795,61.3589193990669,39.9556174643247));
#195488=CARTESIAN_POINT('Ctrl Pts',(12.8462211390717,61.3485984239558,39.94548564139));
#195489=CARTESIAN_POINT('Ctrl Pts',(12.8430366034502,61.3379910943963,39.9352519465111));
#195490=CARTESIAN_POINT('Ctrl Pts',(12.8407372733105,61.3271735965892,39.92499));
#195491=CARTESIAN_POINT('Ctrl Pts',(12.1254815933798,57.9621601888119,39.92499));
#195492=CARTESIAN_POINT('Ctrl Pts',(12.1232811218139,57.9518077840282,39.9348107241723));
#195493=CARTESIAN_POINT('Ctrl Pts',(12.1219050950923,57.9413190436447,39.944603838317));
#195494=CARTESIAN_POINT('Ctrl Pts',(12.1213524729341,57.9307520129788,39.9543158069386));
#195495=CARTESIAN_POINT('Ctrl Pts',(12.1208188676186,57.9205486151425,39.9636935671393));
#195496=CARTESIAN_POINT('Ctrl Pts',(12.1210529843541,57.9102709573189,39.972996832099));
#195497=CARTESIAN_POINT('Ctrl Pts',(12.1220995054498,57.8999666805161,39.9821731151337));
#195498=CARTESIAN_POINT('Ctrl Pts',(12.1230887956353,57.8902259118377,39.9908475764355));
#195499=CARTESIAN_POINT('Ctrl Pts',(12.1248041559922,57.880460457057,39.9994093733849));
#195500=CARTESIAN_POINT('Ctrl Pts',(12.1273238624912,57.8707214090022,40.0077966115845));
#195501=CARTESIAN_POINT('Ctrl Pts',(12.1296444699056,57.8617519091283,40.01552111726));
#195502=CARTESIAN_POINT('Ctrl Pts',(12.1326475236733,57.8528042960108,40.0230979941027));
#195503=CARTESIAN_POINT('Ctrl Pts',(12.1364273448772,57.8439372821293,40.0304554104754));
#195504=CARTESIAN_POINT('Ctrl Pts',(12.1375544112595,57.8412933175823,40.0326492435185));
#195505=CARTESIAN_POINT('Ctrl Pts',(12.1387507708943,57.8386566820012,40.0348233715062));
#195506=CARTESIAN_POINT('Ctrl Pts',(12.1400195294497,57.836029395347,40.0369753512356));
#195507=CARTESIAN_POINT('Ctrl Pts',(12.1412753244192,57.833428953088,40.0391053430352));
#195508=CARTESIAN_POINT('Ctrl Pts',(12.1426004965704,57.8308402488864,40.041211089324));
#195509=CARTESIAN_POINT('Ctrl Pts',(12.1439963340944,57.828268082638,40.0432881154904));
#195510=CARTESIAN_POINT('Ctrl Pts',(12.144093397906,57.8280892192274,40.043432547828));
#195511=CARTESIAN_POINT('Ctrl Pts',(12.1441907966618,57.8279104259145,40.0435768364421));
#195512=CARTESIAN_POINT('Ctrl Pts',(12.1442885313814,57.8277317035127,40.0437209807855));
#195513=CARTESIAN_POINT('Ctrl Pts',(12.1485735795163,57.8198958587083,40.050040796842));
#195514=CARTESIAN_POINT('Ctrl Pts',(12.1535378042507,57.812226847525,40.0560490279346));
#195515=CARTESIAN_POINT('Ctrl Pts',(12.1592011408685,57.804839125324,40.0616647108616));
#195516=CARTESIAN_POINT('Ctrl Pts',(12.1644803548775,57.7979524842553,40.0668995033488));
#195517=CARTESIAN_POINT('Ctrl Pts',(12.1703677426437,57.791309817124,40.0717933267485));
#195518=CARTESIAN_POINT('Ctrl Pts',(12.176888348138,57.7850318067599,40.0762460303076));
#195519=CARTESIAN_POINT('Ctrl Pts',(12.1792736699861,57.7827352293489,40.0778748868751));
#195520=CARTESIAN_POINT('Ctrl Pts',(12.1817437717245,57.7804877669873,40.0794443522249));
#195521=CARTESIAN_POINT('Ctrl Pts',(12.1842999559281,57.7782965440187,40.0809482021492));
#195522=CARTESIAN_POINT('Ctrl Pts',(12.1849146328346,57.777769628097,40.0813098278168));
#195523=CARTESIAN_POINT('Ctrl Pts',(12.185534868683,57.7772459087254,40.0816679525672));
#195524=CARTESIAN_POINT('Ctrl Pts',(12.1861606108972,57.7767255109846,40.082022419258));
#195525=CARTESIAN_POINT('Ctrl Pts',(12.1867667986671,57.7762213756732,40.0823658088648));
#195526=CARTESIAN_POINT('Ctrl Pts',(12.1873781540075,57.7757203576391,40.0827057654616));
#195527=CARTESIAN_POINT('Ctrl Pts',(12.1879946254064,57.7752225713656,40.0830421470151));
#195528=CARTESIAN_POINT('Ctrl Pts',(12.194748782022,57.7697687474614,40.0867275956806));
#195529=CARTESIAN_POINT('Ctrl Pts',(12.202121751003,57.7646995864528,40.089982343203));
#195530=CARTESIAN_POINT('Ctrl Pts',(12.2100174179595,57.7601772489163,40.0926299529355));
#195531=CARTESIAN_POINT('Ctrl Pts',(12.2132919863911,57.7583017007434,40.0937279956084));
#195532=CARTESIAN_POINT('Ctrl Pts',(12.2166560758253,57.7565200187331,40.0947220371802));
#195533=CARTESIAN_POINT('Ctrl Pts',(12.2201014385652,57.7548425830506,40.0956014538692));
#195534=CARTESIAN_POINT('Ctrl Pts',(12.22597786375,57.7519815416929,40.097101390674));
#195535=CARTESIAN_POINT('Ctrl Pts',(12.232089942972,57.7494261286933,40.0982667904316));
#195536=CARTESIAN_POINT('Ctrl Pts',(12.2383911161017,57.7472322823293,40.0990539325582));
#195537=CARTESIAN_POINT('Ctrl Pts',(12.2415417026666,57.7461353591472,40.0994475036216));
#195538=CARTESIAN_POINT('Ctrl Pts',(12.2447399293291,57.7451302272376,40.0997467259952));
#195539=CARTESIAN_POINT('Ctrl Pts',(12.2479799447123,57.7442239366601,40.0999473488896));
#195540=CARTESIAN_POINT('Ctrl Pts',(12.2512199600955,57.7433176460826,40.100147971784));
#195541=CARTESIAN_POINT('Ctrl Pts',(12.2545017192674,57.7425101887131,40.10025));
#195542=CARTESIAN_POINT('Ctrl Pts',(12.2578193919774,57.7418065394564,40.10025));
#195543=CARTESIAN_POINT('Origin',(18.0189898472955,55.4074307335705,39.92499));
#195544=CARTESIAN_POINT('Ctrl Pts',(19.5431821162873,59.5312589135993,39.92499));
#195545=CARTESIAN_POINT('Ctrl Pts',(19.5464608884259,59.5413499366324,39.9348354642013));
#195546=CARTESIAN_POINT('Ctrl Pts',(19.5489337165498,59.5516697238473,39.9446440828447));
#195547=CARTESIAN_POINT('Ctrl Pts',(19.5505973858261,59.562159273364,39.9543641760315));
#195548=CARTESIAN_POINT('Ctrl Pts',(19.5522069957576,59.5723079749826,39.9637684240691));
#195549=CARTESIAN_POINT('Ctrl Pts',(19.5530593117981,59.5826168684372,39.973090963637));
#195550=CARTESIAN_POINT('Ctrl Pts',(19.5531064127995,59.5930429125487,39.982280897711));
#195551=CARTESIAN_POINT('Ctrl Pts',(19.5531509674464,59.6029053082793,39.9909740094614));
#195552=CARTESIAN_POINT('Ctrl Pts',(19.552475023402,59.6128734577595,39.999549276496));
#195553=CARTESIAN_POINT('Ctrl Pts',(19.550996336867,59.6229049605437,40.0079462328649));
#195554=CARTESIAN_POINT('Ctrl Pts',(19.549634359627,59.6321447001047,40.0156804369639));
#195555=CARTESIAN_POINT('Ctrl Pts',(19.5475912199442,59.6414387315114,40.0232638017367));
#195556=CARTESIAN_POINT('Ctrl Pts',(19.5447674611739,59.6507389334358,40.0306257269907));
#195557=CARTESIAN_POINT('Ctrl Pts',(19.543948396093,59.6534365684895,40.0327611416612));
#195558=CARTESIAN_POINT('Ctrl Pts',(19.5430634173972,59.6561345922103,40.0348777427251));
#195559=CARTESIAN_POINT('Ctrl Pts',(19.5421094990035,59.6588314685159,40.03697331687));
#195560=CARTESIAN_POINT('Ctrl Pts',(19.5410753901343,59.6617550558217,40.039245053974));
#195561=CARTESIAN_POINT('Ctrl Pts',(19.5399627185796,59.66467358667,40.041487875195));
#195562=CARTESIAN_POINT('Ctrl Pts',(19.5387684320161,59.6675844741793,40.04369857016));
#195563=CARTESIAN_POINT('Ctrl Pts',(19.5354907031712,59.6755734277897,40.0497658398386));
#195564=CARTESIAN_POINT('Ctrl Pts',(19.5315625649731,59.6834782549088,40.0555581699984));
#195565=CARTESIAN_POINT('Ctrl Pts',(19.5269766895189,59.6911955084647,40.0609828468885));
#195566=CARTESIAN_POINT('Ctrl Pts',(19.5227808624515,59.6982563764886,40.0659461317302));
#195567=CARTESIAN_POINT('Ctrl Pts',(19.5180305486469,59.7051493183924,40.0706039980703));
#195568=CARTESIAN_POINT('Ctrl Pts',(19.5126862934709,59.7117949558626,40.0748843180598));
#195569=CARTESIAN_POINT('Ctrl Pts',(19.5100612127859,59.7150592712795,40.0769867972566));
#195570=CARTESIAN_POINT('Ctrl Pts',(19.507292572924,59.7182634781242,40.0789976708173));
#195571=CARTESIAN_POINT('Ctrl Pts',(19.5043743927945,59.7213950854343,40.0809050491499));
#195572=CARTESIAN_POINT('Ctrl Pts',(19.5038206965385,59.7219892774191,40.0812669556104));
#195573=CARTESIAN_POINT('Ctrl Pts',(19.5032610854122,59.7225808838921,40.0816253922032));
#195574=CARTESIAN_POINT('Ctrl Pts',(19.5026955970365,59.7231697699853,40.0819801989139));
#195575=CARTESIAN_POINT('Ctrl Pts',(19.5021477801725,59.7237402533881,40.0823239179149));
#195576=CARTESIAN_POINT('Ctrl Pts',(19.5015944476719,59.7243081837712,40.0826642303498));
#195577=CARTESIAN_POINT('Ctrl Pts',(19.5010356373992,59.7248734373528,40.0830009916099));
#195578=CARTESIAN_POINT('Ctrl Pts',(19.4949458381923,59.7310334544117,40.0866709464313));
#195579=CARTESIAN_POINT('Ctrl Pts',(19.4882011960852,59.7368793392206,40.089917583188));
#195580=CARTESIAN_POINT('Ctrl Pts',(19.4808775251046,59.7422363728294,40.0925642067065));
#195581=CARTESIAN_POINT('Ctrl Pts',(19.4777846933723,59.7444986813876,40.093681892253));
#195582=CARTESIAN_POINT('Ctrl Pts',(19.4745890081271,59.7466739523115,40.0946930094791));
#195583=CARTESIAN_POINT('Ctrl Pts',(19.4712977780161,59.7487501225118,40.0955863397546));
#195584=CARTESIAN_POINT('Ctrl Pts',(19.4657554287474,59.7522463412518,40.0970906856166));
#195585=CARTESIAN_POINT('Ctrl Pts',(19.4599426670177,59.755459057686,40.0982599215483));
#195586=CARTESIAN_POINT('Ctrl Pts',(19.453899564037,59.7583258028885,40.0990497370453));
#195587=CARTESIAN_POINT('Ctrl Pts',(19.4523887882919,59.7590424891891,40.0992471909196));
#195588=CARTESIAN_POINT('Ctrl Pts',(19.4508635299961,59.7597373347841,40.0994209989363));
#195589=CARTESIAN_POINT('Ctrl Pts',(19.4493243130386,59.7604090725472,40.0995705982975));
#195590=CARTESIAN_POINT('Ctrl Pts',(19.4470154876024,59.761416679192,40.0997949973393));
#195591=CARTESIAN_POINT('Ctrl Pts',(19.4446752658781,59.7623722755977,40.0999649129781));
#195592=CARTESIAN_POINT('Ctrl Pts',(19.4423059520268,59.7632731754139,40.1000786629733));
#195593=CARTESIAN_POINT('Ctrl Pts',(19.4399366381755,59.7641740752301,40.1001924129685));
#195594=CARTESIAN_POINT('Ctrl Pts',(19.4375382417965,59.7650202849789,40.10025));
#195595=CARTESIAN_POINT('Ctrl Pts',(19.4351129318427,59.7658094374949,40.10025));
#195596=CARTESIAN_POINT('Ctrl Pts',(18.2553202812755,56.134781019564,40.10025));
#195597=CARTESIAN_POINT('Ctrl Pts',(18.2635267101477,56.1321105487809,40.10025));
#195598=CARTESIAN_POINT('Ctrl Pts',(18.2718824441053,56.1301406315641,40.0995786334241));
#195599=CARTESIAN_POINT('Ctrl Pts',(18.2802419597942,56.1288305556596,40.0983063763366));
#195600=CARTESIAN_POINT('Ctrl Pts',(18.2856413491931,56.1279843810469,40.0974846287992));
#195601=CARTESIAN_POINT('Ctrl Pts',(18.2910421817938,56.1274125556281,40.0964130309338));
#195602=CARTESIAN_POINT('Ctrl Pts',(18.296405688343,56.127095266925,40.0951176960924));
#195603=CARTESIAN_POINT('Ctrl Pts',(18.3035147090335,56.1266747189246,40.0934008039614));
#195604=CARTESIAN_POINT('Ctrl Pts',(18.3105573165147,56.1267070766079,40.0912909372156));
#195605=CARTESIAN_POINT('Ctrl Pts',(18.3174512966905,56.1271555587353,40.0888630467851));
#195606=CARTESIAN_POINT('Ctrl Pts',(18.3208982867784,56.127379799799,40.0876491015699));
#195607=CARTESIAN_POINT('Ctrl Pts',(18.3243083090334,56.1277080087288,40.0863558569271));
#195608=CARTESIAN_POINT('Ctrl Pts',(18.3276724292425,56.1281351437408,40.0849936342771));
#195609=CARTESIAN_POINT('Ctrl Pts',(18.329354489347,56.1283487112468,40.0843125229521));
#195610=CARTESIAN_POINT('Ctrl Pts',(18.3310250895519,56.1285870051494,40.0836141747074));
#195611=CARTESIAN_POINT('Ctrl Pts',(18.3326832110576,56.1288493629351,40.0828999161609));
#195612=CARTESIAN_POINT('Ctrl Pts',(18.333097741434,56.1289149523815,40.0827213515243));
#195613=CARTESIAN_POINT('Ctrl Pts',(18.3335114922235,56.1289820457107,40.0825417925842));
#195614=CARTESIAN_POINT('Ctrl Pts',(18.3339244481761,56.1290506323486,40.0823612602361));
#195615=CARTESIAN_POINT('Ctrl Pts',(18.3351633160341,56.1292563922626,40.0818196631917));
#195616=CARTESIAN_POINT('Ctrl Pts',(18.3363950287075,56.1294755925117,40.0812693052022));
#195617=CARTESIAN_POINT('Ctrl Pts',(18.337619189229,56.129707942645,40.0807107531875));
#195618=CARTESIAN_POINT('Ctrl Pts',(18.3462420178748,56.1313445869827,40.0767763849182));
#195619=CARTESIAN_POINT('Ctrl Pts',(18.354528490461,56.1335959402407,40.0724140586137));
#195620=CARTESIAN_POINT('Ctrl Pts',(18.3624495731179,56.136345925232,40.0677221223768));
#195621=CARTESIAN_POINT('Ctrl Pts',(18.3662912896469,56.1376796649811,40.065446538372));
#195622=CARTESIAN_POINT('Ctrl Pts',(18.3700472768056,56.139131230071,40.0630928000679));
#195623=CARTESIAN_POINT('Ctrl Pts',(18.3737149835769,56.1406901365232,40.0606689262479));
#195624=CARTESIAN_POINT('Ctrl Pts',(18.3793299863885,56.143076713384,40.0569581447805));
#195625=CARTESIAN_POINT('Ctrl Pts',(18.3847354115627,56.1457125629777,40.0530843804605));
#195626=CARTESIAN_POINT('Ctrl Pts',(18.3899096889384,56.1485569297208,40.0490800251457));
#195627=CARTESIAN_POINT('Ctrl Pts',(18.3923126501199,56.1498778683511,40.0472203818218));
#195628=CARTESIAN_POINT('Ctrl Pts',(18.3946658026165,56.1512435269775,40.0453323608818));
#195629=CARTESIAN_POINT('Ctrl Pts',(18.3969661720543,56.1526507491368,40.0434201572162));
#195630=CARTESIAN_POINT('Ctrl Pts',(18.3971424863078,56.1527586071706,40.0432735943397));
#195631=CARTESIAN_POINT('Ctrl Pts',(18.3973185179292,56.1528666894393,40.0431268995707));
#195632=CARTESIAN_POINT('Ctrl Pts',(18.3974942667076,56.1529749944977,40.0429800745037));
#195633=CARTESIAN_POINT('Ctrl Pts',(18.3999630071785,56.1544963540394,40.0409176249753));
#195634=CARTESIAN_POINT('Ctrl Pts',(18.4023749585858,56.1560635207936,40.0388310783332));
#195635=CARTESIAN_POINT('Ctrl Pts',(18.404728848804,56.1576709325002,40.036725739981));
#195636=CARTESIAN_POINT('Ctrl Pts',(18.4131694805014,56.1634348250116,40.0291763710716));
#195637=CARTESIAN_POINT('Ctrl Pts',(18.4209299141247,56.1697591292905,40.0213310894592));
#195638=CARTESIAN_POINT('Ctrl Pts',(18.4280560759394,56.1765231650108,40.0132837551316));
#195639=CARTESIAN_POINT('Ctrl Pts',(18.4358870118872,56.1839561607597,40.0044405431321));
#195640=CARTESIAN_POINT('Ctrl Pts',(18.4429525945108,56.1919204977441,39.9953528710597));
#195641=CARTESIAN_POINT('Ctrl Pts',(18.4492898603079,56.2003032932673,39.9861103629551));
#195642=CARTESIAN_POINT('Ctrl Pts',(18.4561325169321,56.2093546086376,39.9761307737553));
#195643=CARTESIAN_POINT('Ctrl Pts',(18.4621268842298,56.2188946068458,39.965969693601));
#195644=CARTESIAN_POINT('Ctrl Pts',(18.4672816799273,56.2288243369868,39.9557128217506));
#195645=CARTESIAN_POINT('Ctrl Pts',(18.4723932321855,56.2386707668949,39.945541994516));
#195646=CARTESIAN_POINT('Ctrl Pts',(18.4766796388007,56.2489017962824,39.9352756289341));
#195647=CARTESIAN_POINT('Ctrl Pts',(18.4801050014197,56.2594439784237,39.92499));
#195648=CARTESIAN_POINT('Origin',(-0.0144941013083342,0.004709418994269,
39.92499));
#195649=CARTESIAN_POINT('Ctrl Pts',(19.406124729226,59.7752282754835,40.10025));
#195650=CARTESIAN_POINT('Ctrl Pts',(19.3979550581551,59.77787898563,40.10025));
#195651=CARTESIAN_POINT('Ctrl Pts',(19.3896365599076,59.7798236858208,40.0995859581842));
#195652=CARTESIAN_POINT('Ctrl Pts',(19.3813136269527,59.7811061158277,40.0983275959621));
#195653=CARTESIAN_POINT('Ctrl Pts',(19.3759956690096,59.7819255275517,40.0975235624069));
#195654=CARTESIAN_POINT('Ctrl Pts',(19.3706760212385,59.7824754874619,40.0964777059491));
#195655=CARTESIAN_POINT('Ctrl Pts',(19.3653918801545,59.7827759879493,40.0952149915961));
#195656=CARTESIAN_POINT('Ctrl Pts',(19.3581800878468,59.7831861108188,40.0934916398701));
#195657=CARTESIAN_POINT('Ctrl Pts',(19.3510354548625,59.7831255716885,40.0913643921631));
#195658=CARTESIAN_POINT('Ctrl Pts',(19.3440445557102,59.7826350657122,40.0889118607713));
#195659=CARTESIAN_POINT('Ctrl Pts',(19.340549106134,59.7823898127241,40.0876855950754));
#195660=CARTESIAN_POINT('Ctrl Pts',(19.337091891998,59.7820371343797,40.0863782327527));
#195661=CARTESIAN_POINT('Ctrl Pts',(19.3336823180315,59.7815825865437,40.0850006373334));
#195662=CARTESIAN_POINT('Ctrl Pts',(19.3319775310482,59.7813553126257,40.0843118396238));
#195663=CARTESIAN_POINT('Ctrl Pts',(19.3302846375616,59.781102576764,40.0836054919165));
#195664=CARTESIAN_POINT('Ctrl Pts',(19.328604709227,59.7808251076834,40.0828829920418));
#195665=CARTESIAN_POINT('Ctrl Pts',(19.3281847271434,59.7807557404133,40.0827023670731));
#195666=CARTESIAN_POINT('Ctrl Pts',(19.3277655550296,59.7806848274336,40.0825207326933));
#195667=CARTESIAN_POINT('Ctrl Pts',(19.3273472089201,59.7806123803664,40.0823381109276));
#195668=CARTESIAN_POINT('Ctrl Pts',(19.3260921705918,59.7803950391651,40.0817902456304));
#195669=CARTESIAN_POINT('Ctrl Pts',(19.3248445680583,59.7801638905866,40.0812334935553));
#195670=CARTESIAN_POINT('Ctrl Pts',(19.3236048185592,59.7799192536867,40.0806684524227));
#195671=CARTESIAN_POINT('Ctrl Pts',(19.3150373803115,59.7782286609224,40.0767636676137));
#195672=CARTESIAN_POINT('Ctrl Pts',(19.3068044648779,59.775932168172,40.0724404510889));
#195673=CARTESIAN_POINT('Ctrl Pts',(19.2989322844411,59.7731456380808,40.067794993741));
#195674=CARTESIAN_POINT('Ctrl Pts',(19.2950198323727,59.7717607402743,40.0654862141906));
#195675=CARTESIAN_POINT('Ctrl Pts',(19.2911962646697,59.7702542302926,40.0630972003216));
#195676=CARTESIAN_POINT('Ctrl Pts',(19.287464024724,59.7686372707428,40.0606363359906));
#195677=CARTESIAN_POINT('Ctrl Pts',(19.2792301459423,59.7650700164608,40.0552073017123));
#195678=CARTESIAN_POINT('Ctrl Pts',(19.271436713842,59.76097697069,40.0494204304519));
#195679=CARTESIAN_POINT('Ctrl Pts',(19.2641757185818,59.7564706723511,40.0434049749851));
#195680=CARTESIAN_POINT('Ctrl Pts',(19.2615231854473,59.7548244647405,40.0412074532442));
#195681=CARTESIAN_POINT('Ctrl Pts',(19.2589351484761,59.7531276155317,40.0389814735788));
#195682=CARTESIAN_POINT('Ctrl Pts',(19.2564118357502,59.7513854342764,40.0367321210016));
#195683=CARTESIAN_POINT('Ctrl Pts',(19.247936295312,59.7455336317916,40.0291767837139));
#195684=CARTESIAN_POINT('Ctrl Pts',(19.240142043952,59.739126349354,40.0213235332572));
#195685=CARTESIAN_POINT('Ctrl Pts',(19.2329840462272,59.7322837268613,40.0132649215853));
#195686=CARTESIAN_POINT('Ctrl Pts',(19.225116558807,59.7247628741799,40.0044075527525));
#195687=CARTESIAN_POINT('Ctrl Pts',(19.2180171087291,59.7167157560773,39.995301625371));
#195688=CARTESIAN_POINT('Ctrl Pts',(19.2116502033063,59.7082546997624,39.9860353422346));
#195689=CARTESIAN_POINT('Ctrl Pts',(19.2047927733658,59.6991417795837,39.9760551582679));
#195690=CARTESIAN_POINT('Ctrl Pts',(19.1987842816757,59.6895478206984,39.9658879738136));
#195691=CARTESIAN_POINT('Ctrl Pts',(19.1936187207959,59.6795708631997,39.9556174643231));
#195692=CARTESIAN_POINT('Ctrl Pts',(19.1885229124294,59.6697286283143,39.9454856413889));
#195693=CARTESIAN_POINT('Ctrl Pts',(19.1842470541694,59.6595122814315,39.9352519465106));
#195694=CARTESIAN_POINT('Ctrl Pts',(19.1808295835788,59.6489943884562,39.92499));
#195695=CARTESIAN_POINT('Ctrl Pts',(18.1177524687112,56.3771794532805,39.92499));
#195696=CARTESIAN_POINT('Ctrl Pts',(18.1144819305957,56.3671137719648,39.9348107241721));
#195697=CARTESIAN_POINT('Ctrl Pts',(18.1120170699786,56.3568263239574,39.9446038383167));
#195698=CARTESIAN_POINT('Ctrl Pts',(18.1103629196656,56.3463749453362,39.9543158069381));
#195699=CARTESIAN_POINT('Ctrl Pts',(18.1087656919999,56.3362832197247,39.9636935671387));
#195700=CARTESIAN_POINT('Ctrl Pts',(18.1079242184411,56.3260373921235,39.9729968320983));
#195701=CARTESIAN_POINT('Ctrl Pts',(18.1078879163654,56.3156801719855,39.9821731151329));
#195702=CARTESIAN_POINT('Ctrl Pts',(18.1078535995347,56.3058893552744,39.9908475764345));
#195703=CARTESIAN_POINT('Ctrl Pts',(18.1085387949867,56.2959980926949,39.9994093733839));
#195704=CARTESIAN_POINT('Ctrl Pts',(18.110026690543,56.2860490151161,40.0077966115834));
#195705=CARTESIAN_POINT('Ctrl Pts',(18.1113970173889,56.2768860815744,40.0155211172587));
#195706=CARTESIAN_POINT('Ctrl Pts',(18.1134483398646,56.2676735798224,40.0230979941013));
#195707=CARTESIAN_POINT('Ctrl Pts',(18.1162805994776,56.258460041469,40.030455410474));
#195708=CARTESIAN_POINT('Ctrl Pts',(18.1171251221214,56.2557127503189,40.0326492435175));
#195709=CARTESIAN_POINT('Ctrl Pts',(18.1180393245076,56.2529655048686,40.0348233715058));
#195710=CARTESIAN_POINT('Ctrl Pts',(18.1190265064346,56.250219989383,40.0369753512355));
#195711=CARTESIAN_POINT('Ctrl Pts',(18.1200036017947,56.2475025263004,40.0391053430352));
#195712=CARTESIAN_POINT('Ctrl Pts',(18.1210509212422,56.2447894850828,40.041211089324));
#195713=CARTESIAN_POINT('Ctrl Pts',(18.122170247637,56.2420855046789,40.0432881154904));
#195714=CARTESIAN_POINT('Ctrl Pts',(18.1222480834054,56.2418974751697,40.0434325478279));
#195715=CARTESIAN_POINT('Ctrl Pts',(18.1223262596104,56.2417094803629,40.0435768364421));
#195716=CARTESIAN_POINT('Ctrl Pts',(18.1224047773509,56.2415215209612,40.0437209807855));
#195717=CARTESIAN_POINT('Ctrl Pts',(18.125847282728,56.233280692238,40.050040796842));
#195718=CARTESIAN_POINT('Ctrl Pts',(18.129982682966,56.2251347899176,40.0560490279344));
#195719=CARTESIAN_POINT('Ctrl Pts',(18.1348427679844,56.2171955585584,40.0616647108614));
#195720=CARTESIAN_POINT('Ctrl Pts',(18.1393732118986,56.2097948151026,40.0668995033484));
#195721=CARTESIAN_POINT('Ctrl Pts',(18.1445340001512,56.2025731376012,40.071793326748));
#195722=CARTESIAN_POINT('Ctrl Pts',(18.1503626543103,56.1956479299631,40.076246030307));
#195723=CARTESIAN_POINT('Ctrl Pts',(18.1524948514085,56.1931145994159,40.0778748868747));
#195724=CARTESIAN_POINT('Ctrl Pts',(18.1547164978844,56.1906212529491,40.0794443522247));
#195725=CARTESIAN_POINT('Ctrl Pts',(18.1570296338743,56.1881748397223,40.0809482021492));
#195726=CARTESIAN_POINT('Ctrl Pts',(18.1575858658048,56.1875865590687,40.0813098278168));
#195727=CARTESIAN_POINT('Ctrl Pts',(18.1581479603552,56.1870008763865,40.0816679525672));
#195728=CARTESIAN_POINT('Ctrl Pts',(18.1587158783119,56.186417921567,40.082022419258));
#195729=CARTESIAN_POINT('Ctrl Pts',(18.1592660488324,56.1858531840856,40.0823658088648));
#195730=CARTESIAN_POINT('Ctrl Pts',(18.1598216844591,56.1852910066464,40.0827057654616));
#195731=CARTESIAN_POINT('Ctrl Pts',(18.160382745929,56.1847315084902,40.0830421470151));
#195732=CARTESIAN_POINT('Ctrl Pts',(18.1665298227365,56.1786015595921,40.0867275956807));
#195733=CARTESIAN_POINT('Ctrl Pts',(18.1733325302119,56.1727894828604,40.0899823432032));
#195734=CARTESIAN_POINT('Ctrl Pts',(18.1807122308859,56.1674665972286,40.0926299529357));
#195735=CARTESIAN_POINT('Ctrl Pts',(18.1837728127205,56.165259037899,40.0937279956085));
#195736=CARTESIAN_POINT('Ctrl Pts',(18.186932236838,56.1631354730305,40.0947220371803));
#195737=CARTESIAN_POINT('Ctrl Pts',(18.1901833857459,56.1611070880436,40.0956014538692));
#195738=CARTESIAN_POINT('Ctrl Pts',(18.1957285590022,56.1576474660758,40.097101390674));
#195739=CARTESIAN_POINT('Ctrl Pts',(18.2015400422208,56.1544671656476,40.0982667904316));
#195740=CARTESIAN_POINT('Ctrl Pts',(18.2075773774757,56.1516266854592,40.0990539325582));
#195741=CARTESIAN_POINT('Ctrl Pts',(18.2105960451031,56.150206445365,40.0994475036216));
#195742=CARTESIAN_POINT('Ctrl Pts',(18.2136716866515,56.148872513955,40.0997467259952));
#195743=CARTESIAN_POINT('Ctrl Pts',(18.2167992197301,56.1476325143032,40.0999473488896));
#195744=CARTESIAN_POINT('Ctrl Pts',(18.2199267528088,56.1463925146513,40.100147971784));
#195745=CARTESIAN_POINT('Ctrl Pts',(18.2231061318825,56.145246443375,40.10025));
#195746=CARTESIAN_POINT('Ctrl Pts',(18.2263320786588,56.1441998575526,40.10025));
#195747=CARTESIAN_POINT('Origin',(23.7119335237431,53.2204057122635,39.92499));
#195748=CARTESIAN_POINT('Ctrl Pts',(25.6588335304447,57.1623216544368,39.92499));
#195749=CARTESIAN_POINT('Ctrl Pts',(25.6631491402573,57.1720146727777,39.9348354642023));
#195750=CARTESIAN_POINT('Ctrl Pts',(25.6666871334692,57.1820194461958,39.9446440828468));
#195751=CARTESIAN_POINT('Ctrl Pts',(25.6694381454826,57.1922776320709,39.9543641760345));
#195752=CARTESIAN_POINT('Ctrl Pts',(25.6720997659869,57.2022024879885,39.963768424073));
#195753=CARTESIAN_POINT('Ctrl Pts',(25.6740249857417,57.2123658169611,39.9730909636417));
#195754=CARTESIAN_POINT('Ctrl Pts',(25.6751616470875,57.2227298227177,39.9822808977164));
#195755=CARTESIAN_POINT('Ctrl Pts',(25.6762368587291,57.2325335339847,39.9909740094676));
#195756=CARTESIAN_POINT('Ctrl Pts',(25.6766065729233,57.2425177322924,39.999549276503));
#195757=CARTESIAN_POINT('Ctrl Pts',(25.6761845643577,57.2526488462869,40.0079462328725));
#195758=CARTESIAN_POINT('Ctrl Pts',(25.6757958639483,57.2619803349768,40.0156804369723));
#195759=CARTESIAN_POINT('Ctrl Pts',(25.6747354076183,57.2714370189594,40.0232638017457));
#195760=CARTESIAN_POINT('Ctrl Pts',(25.6728992535084,57.2809814365707,40.0306257270004));
#195761=CARTESIAN_POINT('Ctrl Pts',(25.6723666549989,57.2837499093074,40.0327611416676));
#195762=CARTESIAN_POINT('Ctrl Pts',(25.6717685445833,57.286525658431,40.0348777427283));
#195763=CARTESIAN_POINT('Ctrl Pts',(25.6711017521911,57.2893074725857,40.0369733168701));
#195764=CARTESIAN_POINT('Ctrl Pts',(25.6703789063668,57.2923231379853,40.039245053974));
#195765=CARTESIAN_POINT('Ctrl Pts',(25.669577399688,57.295341986664,40.041487875195));
#195766=CARTESIAN_POINT('Ctrl Pts',(25.6686939261493,57.2983617649661,40.0436985701601));
#195767=CARTESIAN_POINT('Ctrl Pts',(25.66626922609,57.306649570212,40.0497658398386));
#195768=CARTESIAN_POINT('Ctrl Pts',(25.6631888860751,57.3149216961103,40.0555581699984));
#195769=CARTESIAN_POINT('Ctrl Pts',(25.6594348051813,57.3230760282577,40.0609828468885));
#195770=CARTESIAN_POINT('Ctrl Pts',(25.6560000249773,57.3305367994636,40.0659461317305));
#195771=CARTESIAN_POINT('Ctrl Pts',(25.6519962425132,57.3378885241129,40.0706039980707));
#195772=CARTESIAN_POINT('Ctrl Pts',(25.6473759219981,57.3450563828668,40.0748843180604));
#195773=CARTESIAN_POINT('Ctrl Pts',(25.6451064356541,57.3485772116719,40.076986797257));
#195774=CARTESIAN_POINT('Ctrl Pts',(25.6426878935087,57.3520532672061,40.0789976708175));
#195775=CARTESIAN_POINT('Ctrl Pts',(25.6401130415753,57.3554727521278,40.08090504915));
#195776=CARTESIAN_POINT('Ctrl Pts',(25.6396244885003,57.3561215660855,40.0812669556105));
#195777=CARTESIAN_POINT('Ctrl Pts',(25.6391297826978,57.3567684269674,40.0816253922033));
#195778=CARTESIAN_POINT('Ctrl Pts',(25.638628947485,57.3574131967119,40.0819801989139));
#195779=CARTESIAN_POINT('Ctrl Pts',(25.6381437633725,57.3580378174019,40.0823239179149));
#195780=CARTESIAN_POINT('Ctrl Pts',(25.6376528269754,57.3586604755988,40.0826642303498));
#195781=CARTESIAN_POINT('Ctrl Pts',(25.6371561630121,57.3592810442412,40.0830009916099));
#195782=CARTESIAN_POINT('Ctrl Pts',(25.6317436214796,57.3660438734344,40.0866709464312));
#195783=CARTESIAN_POINT('Ctrl Pts',(25.6256469885835,57.3725627409491,40.0899175831877));
#195784=CARTESIAN_POINT('Ctrl Pts',(25.6189233999302,57.3786559602401,40.0925642067061));
#195785=CARTESIAN_POINT('Ctrl Pts',(25.6160839866903,57.3812291645838,40.0936818922527));
#195786=CARTESIAN_POINT('Ctrl Pts',(25.6131331854698,57.383726559214,40.094693009479));
#195787=CARTESIAN_POINT('Ctrl Pts',(25.6100770039418,57.3861353831629,40.0955863397546));
#195788=CARTESIAN_POINT('Ctrl Pts',(25.6049304706145,57.3901917825028,40.0970906856166));
#195789=CARTESIAN_POINT('Ctrl Pts',(25.5994853721135,57.3939944983911,40.0982599215483));
#195790=CARTESIAN_POINT('Ctrl Pts',(25.5937750303537,57.397477215531,40.0990497370454));
#195791=CARTESIAN_POINT('Ctrl Pts',(25.5923474449137,57.398347894816,40.0992471909196));
#195792=CARTESIAN_POINT('Ctrl Pts',(25.5909031732848,57.3991983668799,40.0994209989363));
#195793=CARTESIAN_POINT('Ctrl Pts',(25.589442604035,57.4000273167765,40.0995705982975));
#195794=CARTESIAN_POINT('Ctrl Pts',(25.5872517501602,57.4012707416214,40.0997949973393));
#195795=CARTESIAN_POINT('Ctrl Pts',(25.5850242354392,57.4024657229507,40.0999649129781));
#195796=CARTESIAN_POINT('Ctrl Pts',(25.5827620706104,57.4036093482794,40.1000786629733));
#195797=CARTESIAN_POINT('Ctrl Pts',(25.5804999057817,57.404752973608,40.1001924129685));
#195798=CARTESIAN_POINT('Ctrl Pts',(25.5782031010737,57.4058452484193,40.10025));
#195799=CARTESIAN_POINT('Ctrl Pts',(25.5758735661215,57.4068835917977,40.10025));
#195800=CARTESIAN_POINT('Ctrl Pts',(24.0229981225303,53.9190682401992,40.10025));
#195801=CARTESIAN_POINT('Ctrl Pts',(24.0308804555195,53.9155545931355,40.10025));
#195802=CARTESIAN_POINT('Ctrl Pts',(24.0389845034729,53.9127220553012,40.099578633424));
#195803=CARTESIAN_POINT('Ctrl Pts',(24.0471612846392,53.910545348801,40.0983063763365));
#195804=CARTESIAN_POINT('Ctrl Pts',(24.052442646286,53.9091394197449,40.0974846287991));
#195805=CARTESIAN_POINT('Ctrl Pts',(24.0577541205282,53.9080061861136,40.0964130309337));
#195806=CARTESIAN_POINT('Ctrl Pts',(24.0630550795266,53.9071299964539,40.0951176960924));
#195807=CARTESIAN_POINT('Ctrl Pts',(24.0700811970216,53.9059686572513,40.0934008039614));
#195808=CARTESIAN_POINT('Ctrl Pts',(24.0770886066611,53.9052646847383,40.0912909372156));
#195809=CARTESIAN_POINT('Ctrl Pts',(24.0839917000397,53.9049900928802,40.0888630467851));
#195810=CARTESIAN_POINT('Ctrl Pts',(24.0874432467291,53.9048527969511,40.0876491015699));
#195811=CARTESIAN_POINT('Ctrl Pts',(24.0908688957004,53.904822763532,40.0863558569271));
#195812=CARTESIAN_POINT('Ctrl Pts',(24.0942592346735,53.904895912338,40.0849936342771));
#195813=CARTESIAN_POINT('Ctrl Pts',(24.09595440416,53.904932486741,40.0843125229521));
#195814=CARTESIAN_POINT('Ctrl Pts',(24.0976407611376,53.9049948499725,40.0836141747074));
#195815=CARTESIAN_POINT('Ctrl Pts',(24.0993172231363,53.9050824496419,40.0828999161609));
#195816=CARTESIAN_POINT('Ctrl Pts',(24.099736338636,53.9051043495593,40.0827213515243));
#195817=CARTESIAN_POINT('Ctrl Pts',(24.100154836018,53.90512782661,40.0825417925842));
#195818=CARTESIAN_POINT('Ctrl Pts',(24.1005726990106,53.9051528718721,40.082361260236));
#195819=CARTESIAN_POINT('Ctrl Pts',(24.1018262879885,53.9052280076583,40.0818196631917));
#195820=CARTESIAN_POINT('Ctrl Pts',(24.1030741658761,53.9053172580725,40.0812693052021));
#195821=CARTESIAN_POINT('Ctrl Pts',(24.1043159075206,53.9054203757494,40.0807107531874));
#195822=CARTESIAN_POINT('Ctrl Pts',(24.1130625753263,53.9061467233508,40.0767763849181));
#195823=CARTESIAN_POINT('Ctrl Pts',(24.121538984245,53.9075195712147,40.0724140586137));
#195824=CARTESIAN_POINT('Ctrl Pts',(24.1297041260875,53.9094265129029,40.0677221223767));
#195825=CARTESIAN_POINT('Ctrl Pts',(24.1336642110577,53.910351377561,40.065446538372));
#195826=CARTESIAN_POINT('Ctrl Pts',(24.137551352394,53.9114023832598,40.0630928000679));
#195827=CARTESIAN_POINT('Ctrl Pts',(24.1413619171797,53.9125693701068,40.0606689262479));
#195828=CARTESIAN_POINT('Ctrl Pts',(24.1471956256301,53.9143559454347,40.0569581447805));
#195829=CARTESIAN_POINT('Ctrl Pts',(24.152846960627,53.9164123347818,40.0530843804605));
#195830=CARTESIAN_POINT('Ctrl Pts',(24.1582902100545,53.9187002605236,40.0490800251457));
#195831=CARTESIAN_POINT('Ctrl Pts',(24.1608180832483,53.9197627850743,40.0472203818218));
#195832=CARTESIAN_POINT('Ctrl Pts',(24.1633010951269,53.9208749910655,40.0453323608818));
#195833=CARTESIAN_POINT('Ctrl Pts',(24.16573595767,53.9220340502324,40.0434201572162));
#195834=CARTESIAN_POINT('Ctrl Pts',(24.1659225802901,53.9221228875506,40.0432735943397));
#195835=CARTESIAN_POINT('Ctrl Pts',(24.1661089452653,53.9222119774185,40.0431268995707));
#195836=CARTESIAN_POINT('Ctrl Pts',(24.1662950522348,53.9223013184207,40.0429800745037));
#195837=CARTESIAN_POINT('Ctrl Pts',(24.1689092940621,53.923556290148,40.0409176249753));
#195838=CARTESIAN_POINT('Ctrl Pts',(24.1714718460797,53.9248627542247,40.0388310783332));
#195839=CARTESIAN_POINT('Ctrl Pts',(24.1739808617166,53.9262153118346,40.036725739981));
#195840=CARTESIAN_POINT('Ctrl Pts',(24.182977745577,53.9310653428794,40.0291763710716));
#195841=CARTESIAN_POINT('Ctrl Pts',(24.1913567365406,53.9365438157568,40.0213310894591));
#195842=CARTESIAN_POINT('Ctrl Pts',(24.1991508947546,53.9425259106383,40.0132837551314));
#195843=CARTESIAN_POINT('Ctrl Pts',(24.2077158916391,53.9490996319582,40.0044405431318));
#195844=CARTESIAN_POINT('Ctrl Pts',(24.2155752681678,53.9562817849777,39.9953528710593));
#195845=CARTESIAN_POINT('Ctrl Pts',(24.2227540584938,53.9639562340148,39.9861103629547));
#195846=CARTESIAN_POINT('Ctrl Pts',(24.2305053504153,53.972242712951,39.9761307737548));
#195847=CARTESIAN_POINT('Ctrl Pts',(24.2374640812941,53.9811038680491,39.9659696936003));
#195848=CARTESIAN_POINT('Ctrl Pts',(24.2436285779137,53.9904403792169,39.9557128217498));
#195849=CARTESIAN_POINT('Ctrl Pts',(24.2497413607405,53.999698566649,39.9455419945155));
#195850=CARTESIAN_POINT('Ctrl Pts',(24.2550737197511,54.0094254978903,39.9352756289338));
#195851=CARTESIAN_POINT('Ctrl Pts',(24.2595822759739,54.0195518809638,39.92499));
#195852=CARTESIAN_POINT('Origin',(-0.0139224327744698,0.0061986664404702,
39.92499));
#195853=CARTESIAN_POINT('Ctrl Pts',(25.5480287005725,57.4192809246786,40.10025));
#195854=CARTESIAN_POINT('Ctrl Pts',(25.5401808584723,57.4227710771202,40.10025));
#195855=CARTESIAN_POINT('Ctrl Pts',(25.5321112063506,57.4255746438785,40.0995859581841));
#195856=CARTESIAN_POINT('Ctrl Pts',(25.5239679177306,57.4277200319913,40.0983275959619));
#195857=CARTESIAN_POINT('Ctrl Pts',(25.5187647439664,57.4290908328635,40.0975235624067));
#195858=CARTESIAN_POINT('Ctrl Pts',(25.5135317242471,57.4301938346423,40.0964777059489));
#195859=CARTESIAN_POINT('Ctrl Pts',(25.5083079410954,57.4310450321038,40.0952149915961));
#195860=CARTESIAN_POINT('Ctrl Pts',(25.5011785252539,57.4322067458446,40.0934916398701));
#195861=CARTESIAN_POINT('Ctrl Pts',(25.4940667032544,57.4328933558604,40.091364392163));
#195862=CARTESIAN_POINT('Ctrl Pts',(25.4870628291431,57.4331362848725,40.0889118607713));
#195863=CARTESIAN_POINT('Ctrl Pts',(25.4835608920875,57.4332577493785,40.0876855950754));
#195864=CARTESIAN_POINT('Ctrl Pts',(25.4800857520069,57.4332683803238,40.0863782327526));
#195865=CARTESIAN_POINT('Ctrl Pts',(25.4766473428565,57.4331727200755,40.0850006373333));
#195866=CARTESIAN_POINT('Ctrl Pts',(25.4749281382814,57.4331248899514,40.0843118396237));
#195867=CARTESIAN_POINT('Ctrl Pts',(25.4732181005511,57.4330504941579,40.0836054919164));
#195868=CARTESIAN_POINT('Ctrl Pts',(25.4715183716231,57.4329501454091,40.0828829920417));
#195869=CARTESIAN_POINT('Ctrl Pts',(25.4710934393911,57.4329250582219,40.082702367073));
#195870=CARTESIAN_POINT('Ctrl Pts',(25.4706691511212,57.4328983491279,40.0825207326932));
#195871=CARTESIAN_POINT('Ctrl Pts',(25.470245523975,57.4328700280093,40.0823381109275));
#195872=CARTESIAN_POINT('Ctrl Pts',(25.4689746425362,57.4327850646536,40.0817902456303));
#195873=CARTESIAN_POINT('Ctrl Pts',(25.4677097128942,57.4326855923068,40.0812334935553));
#195874=CARTESIAN_POINT('Ctrl Pts',(25.4664511833533,57.4325718846634,40.0806684524226));
#195875=CARTESIAN_POINT('Ctrl Pts',(25.457753963365,57.4317860942974,40.0767636676136));
#195876=CARTESIAN_POINT('Ctrl Pts',(25.4493260998454,57.4303627559729,40.0724404510888));
#195877=CARTESIAN_POINT('Ctrl Pts',(25.4412057723283,57.4284143577088,40.0677949937408));
#195878=CARTESIAN_POINT('Ctrl Pts',(25.4371699918423,57.4274460091197,40.0654862141905));
#195879=CARTESIAN_POINT('Ctrl Pts',(25.4332098968701,57.4263474236136,40.0630972003215));
#195880=CARTESIAN_POINT('Ctrl Pts',(25.4293290842285,57.4251294472435,40.0606363359906));
#195881=CARTESIAN_POINT('Ctrl Pts',(25.4207674318881,57.4224424094494,40.0552073017123));
#195882=CARTESIAN_POINT('Ctrl Pts',(25.4125888532397,57.4191864212926,40.0494204304519));
#195883=CARTESIAN_POINT('Ctrl Pts',(25.404896598031,57.4154637896038,40.0434049749851));
#195884=CARTESIAN_POINT('Ctrl Pts',(25.4020865201988,57.414103865303,40.0412074532442));
#195885=CARTESIAN_POINT('Ctrl Pts',(25.3993352917247,57.4126868351392,40.0389814735788));
#195886=CARTESIAN_POINT('Ctrl Pts',(25.3966436944405,57.4112179557367,40.0367321210016));
#195887=CARTESIAN_POINT('Ctrl Pts',(25.387602903979,57.4062841452558,40.0291767837142));
#195888=CARTESIAN_POINT('Ctrl Pts',(25.379181606957,57.4007266836991,40.0213235332579));
#195889=CARTESIAN_POINT('Ctrl Pts',(25.3713475726791,57.394669760311,40.0132649215864));
#195890=CARTESIAN_POINT('Ctrl Pts',(25.3627370410054,57.3880124840178,40.004407552754));
#195891=CARTESIAN_POINT('Ctrl Pts',(25.3548353295691,57.3807515434774,39.9953016253728));
#195892=CARTESIAN_POINT('Ctrl Pts',(25.3476188815065,57.3730023605543,39.9860353422369));
#195893=CARTESIAN_POINT('Ctrl Pts',(25.3398464577429,57.3646561585202,39.9760551582708));
#195894=CARTESIAN_POINT('Ctrl Pts',(25.3328680394203,57.3557428147491,39.9658879738171));
#195895=CARTESIAN_POINT('Ctrl Pts',(25.3266878999881,57.3463604602089,39.9556174643273));
#195896=CARTESIAN_POINT('Ctrl Pts',(25.3205912133042,57.3371047991325,39.9454856413917));
#195897=CARTESIAN_POINT('Ctrl Pts',(25.3152708796023,57.3273913673584,39.9352519465119));
#195898=CARTESIAN_POINT('Ctrl Pts',(25.3107727110829,57.3172883154487,39.92499));
#195899=CARTESIAN_POINT('Ctrl Pts',(23.9115214566121,54.1745185419757,39.92499));
#195900=CARTESIAN_POINT('Ctrl Pts',(23.9072166846468,54.1648498658383,39.9348107241724));
#195901=CARTESIAN_POINT('Ctrl Pts',(23.9036899956627,54.1548764216397,39.9446038383174));
#195902=CARTESIAN_POINT('Ctrl Pts',(23.9009524404119,54.144655202554,39.9543158069391));
#195903=CARTESIAN_POINT('Ctrl Pts',(23.8983090899566,54.1347857162244,39.9636935671399));
#195904=CARTESIAN_POINT('Ctrl Pts',(23.8964012454639,54.1246839742766,39.9729968320997));
#195905=CARTESIAN_POINT('Ctrl Pts',(23.8952825179501,54.1143872866741,39.9821731151345));
#195906=CARTESIAN_POINT('Ctrl Pts',(23.8942249700857,54.1046536921668,39.9908475764363));
#195907=CARTESIAN_POINT('Ctrl Pts',(23.8938724934883,54.0947449925308,39.9994093733858));
#195908=CARTESIAN_POINT('Ctrl Pts',(23.8943122764069,54.0846948896039,40.0077966115854));
#195909=CARTESIAN_POINT('Ctrl Pts',(23.894717309097,54.0754389134112,40.0155211172608));
#195910=CARTESIAN_POINT('Ctrl Pts',(23.8957944255627,54.0660624571215,40.0230979941035));
#195911=CARTESIAN_POINT('Ctrl Pts',(23.8976480927559,54.0566033397501,40.0304554104762));
#195912=CARTESIAN_POINT('Ctrl Pts',(23.8982008188942,54.0537828218952,40.032649243519));
#195913=CARTESIAN_POINT('Ctrl Pts',(23.8988228478387,54.0509550659734,40.0348233715065));
#195914=CARTESIAN_POINT('Ctrl Pts',(23.899517637365,54.0481214021,40.0369753512355));
#195915=CARTESIAN_POINT('Ctrl Pts',(23.9002053278545,54.0453166912881,40.0391053430352));
#195916=CARTESIAN_POINT('Ctrl Pts',(23.9009633199472,54.0425090377017,40.041211089324));
#195917=CARTESIAN_POINT('Ctrl Pts',(23.9017938716385,54.0397028685174,40.0432881154904));
#195918=CARTESIAN_POINT('Ctrl Pts',(23.9018516265789,54.0395077330003,40.0434325478279));
#195919=CARTESIAN_POINT('Ctrl Pts',(23.9019097237182,54.0393125964102,40.0435768364421));
#195920=CARTESIAN_POINT('Ctrl Pts',(23.9019681642229,54.0391174593309,40.0437209807855));
#195921=CARTESIAN_POINT('Ctrl Pts',(23.9045304100328,54.030561934933,40.050040796842));
#195922=CARTESIAN_POINT('Ctrl Pts',(23.9077916774641,54.022028389686,40.0560490279344));
#195923=CARTESIAN_POINT('Ctrl Pts',(23.9117952627748,54.0136246330485,40.0616647108614));
#195924=CARTESIAN_POINT('Ctrl Pts',(23.9155273001027,54.0057908712994,40.0668995033484));
#195925=CARTESIAN_POINT('Ctrl Pts',(23.9199049461658,53.9980693056376,40.071793326748));
#195926=CARTESIAN_POINT('Ctrl Pts',(23.9249777890354,53.9905727747493,40.0762460303071));
#195927=CARTESIAN_POINT('Ctrl Pts',(23.9268335005857,53.9878304467659,40.0778748868747));
#195928=CARTESIAN_POINT('Ctrl Pts',(23.9287823509752,53.9851185338199,40.0794443522247));
#195929=CARTESIAN_POINT('Ctrl Pts',(23.930827095549,53.9824437337504,40.0809482021492));
#195930=CARTESIAN_POINT('Ctrl Pts',(23.9313187883101,53.9818005336909,40.0813098278168));
#195931=CARTESIAN_POINT('Ctrl Pts',(23.931816583137,53.9811593045602,40.0816679525672));
#195932=CARTESIAN_POINT('Ctrl Pts',(23.9323204546083,53.9805201796369,40.082022419258));
#195933=CARTESIAN_POINT('Ctrl Pts',(23.932808580096,53.9799010273674,40.0823658088648));
#195934=CARTESIAN_POINT('Ctrl Pts',(23.9333024083488,53.9792838498568,40.0827057654616));
#195935=CARTESIAN_POINT('Ctrl Pts',(23.9338019127828,53.9786687697969,40.0830421470151));
#195936=CARTESIAN_POINT('Ctrl Pts',(23.939274561122,53.9719298569081,40.0867275956806));
#195937=CARTESIAN_POINT('Ctrl Pts',(23.9454324752048,53.9654385427825,40.089982343203));
#195938=CARTESIAN_POINT('Ctrl Pts',(23.9522153560509,53.9593734277044,40.0926299529355));
#195939=CARTESIAN_POINT('Ctrl Pts',(23.9550284189138,53.9568580436998,40.0937279956084));
#195940=CARTESIAN_POINT('Ctrl Pts',(23.9579485624032,53.9544158621938,40.0947220371802));
#195941=CARTESIAN_POINT('Ctrl Pts',(23.9609698772118,53.9520587513129,40.0956014538692));
#195942=CARTESIAN_POINT('Ctrl Pts',(23.966123044461,53.9480384530772,40.097101390674));
#195943=CARTESIAN_POINT('Ctrl Pts',(23.9715702598501,53.9442681092573,40.0982667904315));
#195944=CARTESIAN_POINT('Ctrl Pts',(23.9772776109217,53.9408121161403,40.0990539325582));
#195945=CARTESIAN_POINT('Ctrl Pts',(23.9801312864576,53.9390841195818,40.0994475036216));
#195946=CARTESIAN_POINT('Ctrl Pts',(23.9830506455193,53.937436003503,40.0997467259952));
#195947=CARTESIAN_POINT('Ctrl Pts',(23.9860314303864,53.9358758804724,40.0999473488896));
#195948=CARTESIAN_POINT('Ctrl Pts',(23.9890122152535,53.9343157574419,40.100147971784));
#195949=CARTESIAN_POINT('Ctrl Pts',(23.9920543802867,53.932843628855,40.10025));
#195950=CARTESIAN_POINT('Ctrl Pts',(23.9951532569813,53.9314655730802,40.10025));
#195951=CARTESIAN_POINT('Origin',(29.1450842944635,50.4502867888872,39.92499));
#195952=CARTESIAN_POINT('Ctrl Pts',(31.4933613949865,54.1671020372435,39.92499));
#195953=CARTESIAN_POINT('Ctrl Pts',(31.498666559748,54.1762908521529,39.9348354642007));
#195954=CARTESIAN_POINT('Ctrl Pts',(31.503230955053,54.1858709973805,39.9446440828436));
#195955=CARTESIAN_POINT('Ctrl Pts',(31.50703916914,54.1957854287804,39.9543641760299));
#195956=CARTESIAN_POINT('Ctrl Pts',(31.5107236389456,54.2053777001966,39.9637684240672));
#195957=CARTESIAN_POINT('Ctrl Pts',(31.5137006693043,54.2152841131259,39.9730909636348));
#195958=CARTESIAN_POINT('Ctrl Pts',(31.5159144374956,54.2254725303094,39.9822808977085));
#195959=CARTESIAN_POINT('Ctrl Pts',(31.5180085258885,54.2351101455984,39.9909740094586));
#195960=CARTESIAN_POINT('Ctrl Pts',(31.519419847656,54.245001003765,39.9995492764931));
#195961=CARTESIAN_POINT('Ctrl Pts',(31.520059140675,54.2551207303624,40.0079462328618));
#195962=CARTESIAN_POINT('Ctrl Pts',(31.5206479757804,54.2644417304357,40.0156804369606));
#195963=CARTESIAN_POINT('Ctrl Pts',(31.5205818213861,54.2739574575829,40.0232638017333));
#195964=CARTESIAN_POINT('Ctrl Pts',(31.5197533892273,54.2836415202415,40.0306257269871));
#195965=CARTESIAN_POINT('Ctrl Pts',(31.5195130925487,54.2864504987044,40.0327611416589));
#195966=CARTESIAN_POINT('Ctrl Pts',(31.5192084034343,54.2892735615522,40.0348777427239));
#195967=CARTESIAN_POINT('Ctrl Pts',(31.5188360425585,54.2921098354277,40.03697331687));
#195968=CARTESIAN_POINT('Ctrl Pts',(31.5184323794292,54.2951845386598,40.039245053974));
#195969=CARTESIAN_POINT('Ctrl Pts',(31.517950819101,54.2982706300311,40.041487875195));
#195970=CARTESIAN_POINT('Ctrl Pts',(31.5173878381082,54.301366213803,40.0436985701601));
#195971=CARTESIAN_POINT('Ctrl Pts',(31.5158427323556,54.3098620677556,40.0497658398386));
#195972=CARTESIAN_POINT('Ctrl Pts',(31.5136439393738,54.3184108612909,40.0555581699984));
#195973=CARTESIAN_POINT('Ctrl Pts',(31.5107627835363,54.3269129314604,40.0609828468885));
#195974=CARTESIAN_POINT('Ctrl Pts',(31.5081266823666,54.3346918640771,40.0659461317303));
#195975=CARTESIAN_POINT('Ctrl Pts',(31.5049132975218,54.3424218244375,40.0706039980704));
#195976=CARTESIAN_POINT('Ctrl Pts',(31.5010675328665,54.3500333719143,40.07488431806));
#195977=CARTESIAN_POINT('Ctrl Pts',(31.4991785058305,54.3537721391709,40.0769867972568));
#195978=CARTESIAN_POINT('Ctrl Pts',(31.4971365594552,54.3574819590032,40.0789976708174));
#195979=CARTESIAN_POINT('Ctrl Pts',(31.494933246334,54.3611518569447,40.0809050491499));
#195980=CARTESIAN_POINT('Ctrl Pts',(31.4945151891298,54.3618481843338,40.0812669556104));
#195981=CARTESIAN_POINT('Ctrl Pts',(31.4940908087514,54.3625432124814,40.0816253922032));
#195982=CARTESIAN_POINT('Ctrl Pts',(31.4936601139568,54.363236801645,40.0819801989139));
#195983=CARTESIAN_POINT('Ctrl Pts',(31.4932428783745,54.3639087161471,40.0823239179149));
#195984=CARTESIAN_POINT('Ctrl Pts',(31.4928197168828,54.3645792801845,40.0826642303498));
#195985=CARTESIAN_POINT('Ctrl Pts',(31.4923906407832,54.3652483648077,40.0830009916099));
#195986=CARTESIAN_POINT('Ctrl Pts',(31.4877146578623,54.3725399111641,40.0866709464313));
#195987=CARTESIAN_POINT('Ctrl Pts',(31.4823328301623,54.3796603393085,40.089917583188));
#195988=CARTESIAN_POINT('Ctrl Pts',(31.4762829888796,54.3864229856965,40.0925642067064));
#195989=CARTESIAN_POINT('Ctrl Pts',(31.4737281033385,54.3892788932598,40.0936818922529));
#195990=CARTESIAN_POINT('Ctrl Pts',(31.471054515739,54.3920710496177,40.0946930094791));
#195991=CARTESIAN_POINT('Ctrl Pts',(31.4682668669592,54.3947861357352,40.0955863397545));
#195992=CARTESIAN_POINT('Ctrl Pts',(31.4635725360693,54.3993582729149,40.0970906856166));
#195993=CARTESIAN_POINT('Ctrl Pts',(31.4585547584357,54.4037093249064,40.0982599215483));
#195994=CARTESIAN_POINT('Ctrl Pts',(31.4532397415962,54.4077698566063,40.0990497370453));
#195995=CARTESIAN_POINT('Ctrl Pts',(31.4519109873863,54.4087849895313,40.0992471909196));
#195996=CARTESIAN_POINT('Ctrl Pts',(31.4505635261664,54.4097817701141,40.0994209989363));
#195997=CARTESIAN_POINT('Ctrl Pts',(31.4491976069265,54.4107588499956,40.0995705982975));
#195998=CARTESIAN_POINT('Ctrl Pts',(31.4471487280667,54.412224469818,40.0997949973393));
#195999=CARTESIAN_POINT('Ctrl Pts',(31.4450583254664,54.4136457436052,40.0999649129781));
#196000=CARTESIAN_POINT('Ctrl Pts',(31.4429280944115,54.4150195646478,40.1000786629733));
#196001=CARTESIAN_POINT('Ctrl Pts',(31.4407978633565,54.4163933856905,40.1001924129685));
#196002=CARTESIAN_POINT('Ctrl Pts',(31.4386278145925,54.4177197583726,40.10025));
#196003=CARTESIAN_POINT('Ctrl Pts',(31.4364195775141,54.418995916306,40.10025));
#196004=CARTESIAN_POINT('Ctrl Pts',(29.5274749692191,51.1126068659043,40.10025));
#196005=CARTESIAN_POINT('Ctrl Pts',(29.534946845835,51.1082885388128,40.10025));
#196006=CARTESIAN_POINT('Ctrl Pts',(29.5427104181384,51.1046244142385,40.0995786334241));
#196007=CARTESIAN_POINT('Ctrl Pts',(29.550614878256,51.1016049255945,40.0983063763367));
#196008=CARTESIAN_POINT('Ctrl Pts',(29.5557203484479,51.0996546457478,40.0974846287993));
#196009=CARTESIAN_POINT('Ctrl Pts',(29.5608842707089,51.0979724198484,40.0964130309339));
#196010=CARTESIAN_POINT('Ctrl Pts',(29.5660646037411,51.0965469289494,40.0951176960924));
#196011=CARTESIAN_POINT('Ctrl Pts',(29.5729308384271,51.0946575224199,40.0934008039614));
#196012=CARTESIAN_POINT('Ctrl Pts',(29.5798262755784,51.093224932581,40.0912909372156));
#196013=CARTESIAN_POINT('Ctrl Pts',(29.5866628504243,51.0922302752231,40.0888630467851));
#196014=CARTESIAN_POINT('Ctrl Pts',(29.5900811378472,51.0917329465441,40.0876491015699));
#196015=CARTESIAN_POINT('Ctrl Pts',(29.5934848814079,51.0913449998286,40.0863558569271));
#196016=CARTESIAN_POINT('Ctrl Pts',(29.5968642938815,51.091063360995,40.0849936342771));
#196017=CARTESIAN_POINT('Ctrl Pts',(29.5985540001184,51.0909225415782,40.0843125229521));
#196018=CARTESIAN_POINT('Ctrl Pts',(29.6002376377887,51.090808290874,40.0836141747074));
#196019=CARTESIAN_POINT('Ctrl Pts',(29.6019140726121,51.0907201726668,40.0828999161609));
#196020=CARTESIAN_POINT('Ctrl Pts',(29.6023331813179,51.090698143115,40.0827213515243));
#196021=CARTESIAN_POINT('Ctrl Pts',(29.6027518401475,51.0906777466677,40.0825417925842));
#196022=CARTESIAN_POINT('Ctrl Pts',(29.6031700319857,51.0906589761527,40.0823612602361));
#196023=CARTESIAN_POINT('Ctrl Pts',(29.6044246075002,51.0906026646078,40.0818196631917));
#196024=CARTESIAN_POINT('Ctrl Pts',(29.6056749785909,51.090560987341,40.0812693052022));
#196025=CARTESIAN_POINT('Ctrl Pts',(29.606920696577,51.0905337427827,40.0807107531875));
#196026=CARTESIAN_POINT('Ctrl Pts',(29.6156953732198,51.0903418356314,40.0767763849182));
#196027=CARTESIAN_POINT('Ctrl Pts',(29.6242688491611,51.0908211368928,40.0724140586137));
#196028=CARTESIAN_POINT('Ctrl Pts',(29.6325885911864,51.0918641424257,40.0677221223768));
#196029=CARTESIAN_POINT('Ctrl Pts',(29.6366236570783,51.0923699989822,40.065446538372));
#196030=CARTESIAN_POINT('Ctrl Pts',(29.6405993642582,51.0930089302513,40.0630928000679));
#196031=CARTESIAN_POINT('Ctrl Pts',(29.644511037713,51.0937712117411,40.0606689262479));
#196032=CARTESIAN_POINT('Ctrl Pts',(29.6504995364717,51.0949382114429,40.0569581447805));
#196033=CARTESIAN_POINT('Ctrl Pts',(29.6563348640826,51.0963926103113,40.0530843804605));
#196034=CARTESIAN_POINT('Ctrl Pts',(29.661987448182,51.0980990280587,40.0490800251457));
#196035=CARTESIAN_POINT('Ctrl Pts',(29.6646125374804,51.0988914972884,40.0472203818218));
#196036=CARTESIAN_POINT('Ctrl Pts',(29.6671982043432,51.099738065083,40.0453323608818));
#196037=CARTESIAN_POINT('Ctrl Pts',(29.6697408831281,51.1006362623625,40.0434201572162));
#196038=CARTESIAN_POINT('Ctrl Pts',(29.6699357694383,51.1007051056449,40.0432735943397));
#196039=CARTESIAN_POINT('Ctrl Pts',(29.6701304259137,51.1007742270247,40.0431268995707));
#196040=CARTESIAN_POINT('Ctrl Pts',(29.6703248520474,51.1008436251321,40.0429800745037));
#196041=CARTESIAN_POINT('Ctrl Pts',(29.6730559530505,51.1018184593121,40.0409176249753));
#196042=CARTESIAN_POINT('Ctrl Pts',(29.6757410298223,51.1028499068175,40.0388310783332));
#196043=CARTESIAN_POINT('Ctrl Pts',(29.6783776815774,51.1039327914264,40.036725739981));
#196044=CARTESIAN_POINT('Ctrl Pts',(29.6878322458589,51.1078158230496,40.0291763710714));
#196045=CARTESIAN_POINT('Ctrl Pts',(29.6967379921843,51.1123884412304,40.0213310894587));
#196046=CARTESIAN_POINT('Ctrl Pts',(29.7051147523695,51.1175230541898,40.0132837551309));
#196047=CARTESIAN_POINT('Ctrl Pts',(29.7143199702928,51.1231654780145,40.0044405431309));
#196048=CARTESIAN_POINT('Ctrl Pts',(29.7228870317529,51.1294867578978,39.995352871058));
#196049=CARTESIAN_POINT('Ctrl Pts',(29.7308286942788,51.1363687775796,39.9861103629529));
#196050=CARTESIAN_POINT('Ctrl Pts',(29.7394036967218,51.1437996316849,39.9761307737523));
#196051=CARTESIAN_POINT('Ctrl Pts',(29.7472505498704,51.1518848590038,39.965969693597));
#196052=CARTESIAN_POINT('Ctrl Pts',(29.7543572078975,51.1605258584289,39.9557128217457));
#196053=CARTESIAN_POINT('Ctrl Pts',(29.7614042483641,51.1690943687453,39.9455419945127));
#196054=CARTESIAN_POINT('Ctrl Pts',(29.7677241373282,51.1782106315454,39.9352756289324));
#196055=CARTESIAN_POINT('Ctrl Pts',(29.7732664904686,51.1878102687781,39.92499));
#196056=CARTESIAN_POINT('Origin',(-0.0131982271536719,0.00761999999999528,
39.92499));
#196057=CARTESIAN_POINT('Ctrl Pts',(31.4100231232068,54.434235916306,40.10025));
#196058=CARTESIAN_POINT('Ctrl Pts',(31.4025830926779,54.4385272722021,40.10025));
#196059=CARTESIAN_POINT('Ctrl Pts',(31.3948506994797,54.4421589890638,40.0995859581841));
#196060=CARTESIAN_POINT('Ctrl Pts',(31.3869762747693,54.4451438299614,40.0983275959619));
#196061=CARTESIAN_POINT('Ctrl Pts',(31.3819448922441,54.4470510012006,40.0975235624067));
#196062=CARTESIAN_POINT('Ctrl Pts',(31.3768558346353,54.4486949601298,40.096477705949));
#196063=CARTESIAN_POINT('Ctrl Pts',(31.3717496422771,54.4500875286677,40.0952149915962));
#196064=CARTESIAN_POINT('Ctrl Pts',(31.3647807142736,54.451988105301,40.0934916398702));
#196065=CARTESIAN_POINT('Ctrl Pts',(31.3577796218689,54.45341434182,40.0913643921631));
#196066=CARTESIAN_POINT('Ctrl Pts',(31.3508395087091,54.4543880442393,40.0889118607714));
#196067=CARTESIAN_POINT('Ctrl Pts',(31.3473694521293,54.454874895449,40.0876855950755));
#196068=CARTESIAN_POINT('Ctrl Pts',(31.343914460466,54.4552487192091,40.0863782327527));
#196069=CARTESIAN_POINT('Ctrl Pts',(31.340484888062,54.4555129946222,40.0850006373334));
#196070=CARTESIAN_POINT('Ctrl Pts',(31.33877010186,54.4556451323288,40.0843118396238));
#196071=CARTESIAN_POINT('Ctrl Pts',(31.3370616554174,54.4557498916993,40.0836054919165));
#196072=CARTESIAN_POINT('Ctrl Pts',(31.3353607484818,54.4558277627243,40.0828829920418));
#196073=CARTESIAN_POINT('Ctrl Pts',(31.3349355217479,54.4558472304805,40.0827023670731));
#196074=CARTESIAN_POINT('Ctrl Pts',(31.334510765913,54.4558650179025,40.0825207326933));
#196075=CARTESIAN_POINT('Ctrl Pts',(31.3340864990776,54.4558811330246,40.0823381109276));
#196076=CARTESIAN_POINT('Ctrl Pts',(31.3328136985713,54.4559294783908,40.0817902456304));
#196077=CARTESIAN_POINT('Ctrl Pts',(31.3315453006546,54.4559627721155,40.0812334935553));
#196078=CARTESIAN_POINT('Ctrl Pts',(31.3302817797851,54.4559812395334,40.0806684524227));
#196079=CARTESIAN_POINT('Ctrl Pts',(31.3215500666183,54.4561088608493,40.0767636676136));
#196080=CARTESIAN_POINT('Ctrl Pts',(31.313019592449,54.4555742713435,40.0724404510887));
#196081=CARTESIAN_POINT('Ctrl Pts',(31.3047400858592,54.4544853519654,40.0677949937407));
#196082=CARTESIAN_POINT('Ctrl Pts',(31.3006251938112,54.4539441620235,40.0654862141904));
#196083=CARTESIAN_POINT('Ctrl Pts',(31.296571959199,54.4532655373256,40.0630972003215));
#196084=CARTESIAN_POINT('Ctrl Pts',(31.2925850928569,54.4524598885392,40.0606363359906));
#196085=CARTESIAN_POINT('Ctrl Pts',(31.2837894702125,54.4506825069815,40.0552073017124));
#196086=CARTESIAN_POINT('Ctrl Pts',(31.2753153512353,54.4482992497263,40.0494204304519));
#196087=CARTESIAN_POINT('Ctrl Pts',(31.2672761140357,54.4454010706195,40.0434049749851));
#196088=CARTESIAN_POINT('Ctrl Pts',(31.2643392793066,54.4443423292438,40.0412074532442));
#196089=CARTESIAN_POINT('Ctrl Pts',(31.2614550023645,54.443220643404,40.0389814735788));
#196090=CARTESIAN_POINT('Ctrl Pts',(31.2586246102252,54.4420411592045,40.0367321210016));
#196091=CARTESIAN_POINT('Ctrl Pts',(31.2491176225323,54.4380793965873,40.0291767837142));
#196092=CARTESIAN_POINT('Ctrl Pts',(31.2401615453403,54.433432644623,40.021323533258));
#196093=CARTESIAN_POINT('Ctrl Pts',(31.2317373058279,54.4282277812592,40.0132649215865));
#196094=CARTESIAN_POINT('Ctrl Pts',(31.222478068687,54.4225070198657,40.0044075527542));
#196095=CARTESIAN_POINT('Ctrl Pts',(31.2138606686962,54.4161118092708,39.9953016253731));
#196096=CARTESIAN_POINT('Ctrl Pts',(31.2058737429085,54.4091594014087,39.9860353422371));
#196097=CARTESIAN_POINT('Ctrl Pts',(31.1972714816225,54.4016713602542,39.9760551582709));
#196098=CARTESIAN_POINT('Ctrl Pts',(31.1893995936785,54.3935362880559,39.9658879738171));
#196099=CARTESIAN_POINT('Ctrl Pts',(31.1822725865947,54.3848513315129,39.9556174643269));
#196100=CARTESIAN_POINT('Ctrl Pts',(31.1752418181697,54.3762836512066,39.9454856413915));
#196101=CARTESIAN_POINT('Ctrl Pts',(31.1689352997164,54.3671795569343,39.9352519465119));
#196102=CARTESIAN_POINT('Ctrl Pts',(31.1634057161447,54.3576020372435,39.92499));
#196103=CARTESIAN_POINT('Ctrl Pts',(29.4433108116267,51.3783102687781,39.92499));
#196104=CARTESIAN_POINT('Ctrl Pts',(29.4380189697937,51.3691445298578,39.9348107241733));
#196105=CARTESIAN_POINT('Ctrl Pts',(29.433469091585,51.3595943606091,39.9446038383191));
#196106=CARTESIAN_POINT('Ctrl Pts',(29.4296781246243,51.3497152868736,39.9543158069416));
#196107=CARTESIAN_POINT('Ctrl Pts',(29.42601761248,51.3401761719831,39.963693567143));
#196108=CARTESIAN_POINT('Ctrl Pts',(29.423064299797,51.330329192487,39.9729968321034));
#196109=CARTESIAN_POINT('Ctrl Pts',(29.4208754038577,51.3202058500836,39.9821731151387));
#196110=CARTESIAN_POINT('Ctrl Pts',(29.4188062116754,51.310636121078,39.9908475764409));
#196111=CARTESIAN_POINT('Ctrl Pts',(29.4174199248359,51.3008185461718,39.9994093733908));
#196112=CARTESIAN_POINT('Ctrl Pts',(29.4168067767633,51.290777528927,40.0077966115908));
#196113=CARTESIAN_POINT('Ctrl Pts',(29.4162420776748,51.2815299204951,40.0155211172665));
#196114=CARTESIAN_POINT('Ctrl Pts',(29.4163331870173,51.2720922400845,40.0230979941095));
#196115=CARTESIAN_POINT('Ctrl Pts',(29.4171879526256,51.262491179764,40.0304554104825));
#196116=CARTESIAN_POINT('Ctrl Pts',(29.4174428264751,51.2596283373899,40.0326492435232));
#196117=CARTESIAN_POINT('Ctrl Pts',(29.4177658668987,51.256751052484,40.0348233715086));
#196118=CARTESIAN_POINT('Ctrl Pts',(29.4181606517648,51.2538602864391,40.0369753512356));
#196119=CARTESIAN_POINT('Ctrl Pts',(29.4185514029028,51.2509990568964,40.0391053430352));
#196120=CARTESIAN_POINT('Ctrl Pts',(29.4190117629207,51.2481275521815,40.041211089324));
#196121=CARTESIAN_POINT('Ctrl Pts',(29.4195444402105,51.2452499391936,40.0432881154904));
#196122=CARTESIAN_POINT('Ctrl Pts',(29.4195814815475,51.2450498356142,40.043432547828));
#196123=CARTESIAN_POINT('Ctrl Pts',(29.4196188630967,51.244849695198,40.0435768364421));
#196124=CARTESIAN_POINT('Ctrl Pts',(29.4196565860791,51.2446495184039,40.0437209807855));
#196125=CARTESIAN_POINT('Ctrl Pts',(29.4213104998207,51.2358730344468,40.0500407968419));
#196126=CARTESIAN_POINT('Ctrl Pts',(29.4236619033169,51.2270453415806,40.0560490279344));
#196127=CARTESIAN_POINT('Ctrl Pts',(29.4267651248013,51.2182691329813,40.0616647108614));
#196128=CARTESIAN_POINT('Ctrl Pts',(29.429657866561,51.210088181272,40.0668995033484));
#196129=CARTESIAN_POINT('Ctrl Pts',(29.4332044080282,51.2019513265394,40.0717933267479));
#196130=CARTESIAN_POINT('Ctrl Pts',(29.4374658604801,51.1939656059622,40.0762460303069));
#196131=CARTESIAN_POINT('Ctrl Pts',(29.4390247549186,51.1910443260617,40.0778748868746));
#196132=CARTESIAN_POINT('Ctrl Pts',(29.440679457209,51.1881435589221,40.0794443522246));
#196133=CARTESIAN_POINT('Ctrl Pts',(29.4424334077173,51.185269677679,40.0809482021492));
#196134=CARTESIAN_POINT('Ctrl Pts',(29.4428551742202,51.184578605248,40.0813098278168));
#196135=CARTESIAN_POINT('Ctrl Pts',(29.4432832153794,51.1838888551092,40.0816679525672));
#196136=CARTESIAN_POINT('Ctrl Pts',(29.4437175198439,51.1832005624685,40.0820224192581));
#196137=CARTESIAN_POINT('Ctrl Pts',(29.4441382522939,51.1825337789729,40.0823658088648));
#196138=CARTESIAN_POINT('Ctrl Pts',(29.4445648626871,51.1818683633169,40.0827057654617));
#196139=CARTESIAN_POINT('Ctrl Pts',(29.4449973374102,51.181204440299,40.0830421470151));
#196140=CARTESIAN_POINT('Ctrl Pts',(29.4497355978007,51.1739303963593,40.0867275956806));
#196141=CARTESIAN_POINT('Ctrl Pts',(29.4551812510957,51.1668309650357,40.089982343203));
#196142=CARTESIAN_POINT('Ctrl Pts',(29.4612929974521,51.1600900711813,40.0926299529355));
#196143=CARTESIAN_POINT('Ctrl Pts',(29.4638277208378,51.1572944215752,40.0937279956084));
#196144=CARTESIAN_POINT('Ctrl Pts',(29.4664765899958,51.1545603804836,40.0947220371802));
#196145=CARTESIAN_POINT('Ctrl Pts',(29.4692349685477,51.1519003687086,40.0956014538692));
#196146=CARTESIAN_POINT('Ctrl Pts',(29.4739396706111,51.1473634414338,40.097101390674));
#196147=CARTESIAN_POINT('Ctrl Pts',(29.4789629373388,51.1430443628981,40.0982667904316));
#196148=CARTESIAN_POINT('Ctrl Pts',(29.4842777732944,51.139010721436,40.0990539325583));
#196149=CARTESIAN_POINT('Ctrl Pts',(29.4869351912722,51.1369939007049,40.0994475036216));
#196150=CARTESIAN_POINT('Ctrl Pts',(29.4896662827385,51.135049657062,40.0997467259952));
#196151=CARTESIAN_POINT('Ctrl Pts',(29.4924676612914,51.1331865036872,40.0999473488896));
#196152=CARTESIAN_POINT('Ctrl Pts',(29.4952690398443,51.1313233503124,40.100147971784));
#196153=CARTESIAN_POINT('Ctrl Pts',(29.4981406602403,51.1295412933643,40.10025));
#196154=CARTESIAN_POINT('Ctrl Pts',(29.5010785149117,51.1278468659044,40.10025));
#196155=CARTESIAN_POINT('Origin',(34.2589154226527,47.1274239660506,39.92499));
#196156=CARTESIAN_POINT('Ctrl Pts',(36.9828414016752,50.5784163149353,39.92499));
#196157=CARTESIAN_POINT('Ctrl Pts',(36.9890779968915,50.5870002518363,39.9348354642018));
#196158=CARTESIAN_POINT('Ctrl Pts',(36.9946187858206,50.5960508068001,39.9446440828459));
#196159=CARTESIAN_POINT('Ctrl Pts',(36.9994424783912,50.6055128591423,39.9543641760333));
#196160=CARTESIAN_POINT('Ctrl Pts',(37.0041094296764,50.6146674511263,39.9637684240716));
#196161=CARTESIAN_POINT('Ctrl Pts',(37.0081056536714,50.6242084112816,39.9730909636401));
#196162=CARTESIAN_POINT('Ctrl Pts',(37.0113722742002,50.6341096134638,39.9822808977147));
#196163=CARTESIAN_POINT('Ctrl Pts',(37.0144622960735,50.6434755410474,39.9909740094658));
#196164=CARTESIAN_POINT('Ctrl Pts',(37.0168997626771,50.6531646927637,39.9995492765011));
#196165=CARTESIAN_POINT('Ctrl Pts',(37.0185933530516,50.6631621581244,40.0079462328707));
#196166=CARTESIAN_POINT('Ctrl Pts',(37.0201532722701,50.6723705467567,40.0156804369703));
#196167=CARTESIAN_POINT('Ctrl Pts',(37.0210821446117,50.6818410607736,40.0232638017438));
#196168=CARTESIAN_POINT('Ctrl Pts',(37.021270510878,50.6915586678658,40.0306257269984));
#196169=CARTESIAN_POINT('Ctrl Pts',(37.0213251487716,50.6943773762884,40.0327611416663));
#196170=CARTESIAN_POINT('Ctrl Pts',(37.0213172191971,50.6972168227826,40.0348777427277));
#196171=CARTESIAN_POINT('Ctrl Pts',(37.0212433695029,50.7000764815582,40.0369733168701));
#196172=CARTESIAN_POINT('Ctrl Pts',(37.0211633116864,50.7031765355309,40.039245053974));
#196173=CARTESIAN_POINT('Ctrl Pts',(37.0210069737846,50.7062960577318,40.041487875195));
#196174=CARTESIAN_POINT('Ctrl Pts',(37.0207706534752,50.70943353111,40.0436985701601));
#196175=CARTESIAN_POINT('Ctrl Pts',(37.0201220705314,50.7180443514156,40.0497658398386));
#196176=CARTESIAN_POINT('Ctrl Pts',(37.0188289150186,50.7267761502169,40.0555581699984));
#196177=CARTESIAN_POINT('Ctrl Pts',(37.0168522507837,50.7355328079485,40.0609828468886));
#196178=CARTESIAN_POINT('Ctrl Pts',(37.0150437103243,50.743544674363,40.0659461317305));
#196179=CARTESIAN_POINT('Ctrl Pts',(37.0126559296154,50.7515681793716,40.0706039980706));
#196180=CARTESIAN_POINT('Ctrl Pts',(37.0096268558221,50.7595400218645,40.0748843180603));
#196181=CARTESIAN_POINT('Ctrl Pts',(37.0081389846697,50.7634557648559,40.076986797257));
#196182=CARTESIAN_POINT('Ctrl Pts',(37.0064960060565,50.7673587034235,40.0789976708175));
#196183=CARTESIAN_POINT('Ctrl Pts',(37.0046883717073,50.7712388062146,40.08090504915));
#196184=CARTESIAN_POINT('Ctrl Pts',(37.0043453906961,50.7719750179265,40.0812669556105));
#196185=CARTESIAN_POINT('Ctrl Pts',(37.003995985342,50.772710598466,40.0816253922033));
#196186=CARTESIAN_POINT('Ctrl Pts',(37.003640149748,50.7734454079405,40.0819801989139));
#196187=CARTESIAN_POINT('Ctrl Pts',(37.0032954340162,50.774157254619,40.0823239179149));
#196188=CARTESIAN_POINT('Ctrl Pts',(37.0029446836758,50.7748683776568,40.0826642303498));
#196189=CARTESIAN_POINT('Ctrl Pts',(37.0025878964874,50.7755786476298,40.0830009916099));
#196190=CARTESIAN_POINT('Ctrl Pts',(36.9986997032258,50.7833190234411,40.0866709464312));
#196191=CARTESIAN_POINT('Ctrl Pts',(36.9940916451531,50.7909629993138,40.0899175831877));
#196192=CARTESIAN_POINT('Ctrl Pts',(36.9887818345687,50.7983209798294,40.0925642067062));
#196193=CARTESIAN_POINT('Ctrl Pts',(36.9865394685866,50.8014283006919,40.0936818922527));
#196194=CARTESIAN_POINT('Ctrl Pts',(36.9841723869928,50.8044846273286,40.0946930094791));
#196195=CARTESIAN_POINT('Ctrl Pts',(36.9816838130239,50.8074762285636,40.0955863397546));
#196196=CARTESIAN_POINT('Ctrl Pts',(36.9774931166431,50.8125140102914,40.0970906856166));
#196197=CARTESIAN_POINT('Ctrl Pts',(36.9729576356987,50.8173657273499,40.0982599215483));
#196198=CARTESIAN_POINT('Ctrl Pts',(36.9680961762161,50.8219595855747,40.0990497370453));
#196199=CARTESIAN_POINT('Ctrl Pts',(36.9668808113454,50.8231080501309,40.0992471909196));
#196200=CARTESIAN_POINT('Ctrl Pts',(36.9656449236016,50.8242402182961,40.0994209989363));
#196201=CARTESIAN_POINT('Ctrl Pts',(36.9643886196688,50.8253547230709,40.0995705982975));
#196202=CARTESIAN_POINT('Ctrl Pts',(36.9625041637695,50.8270264802331,40.0997949973393));
#196203=CARTESIAN_POINT('Ctrl Pts',(36.9605737761782,50.8286584747052,40.0999649129781));
#196204=CARTESIAN_POINT('Ctrl Pts',(36.9585988181543,50.830247439591,40.1000786629733));
#196205=CARTESIAN_POINT('Ctrl Pts',(36.9566238601303,50.8318364044769,40.1001924129685));
#196206=CARTESIAN_POINT('Ctrl Pts',(36.9546043428198,50.8333823430146,40.10025));
#196207=CARTESIAN_POINT('Ctrl Pts',(36.9525415975228,50.8348823336496,40.10025));
#196208=CARTESIAN_POINT('Ctrl Pts',(34.7084426211237,47.746145074786,40.10025));
#196209=CARTESIAN_POINT('Ctrl Pts',(34.7154221779238,47.7410693801611,40.10025));
#196210=CARTESIAN_POINT('Ctrl Pts',(34.7227602152557,47.7366138137618,40.0995786334239));
#196211=CARTESIAN_POINT('Ctrl Pts',(34.7303057514069,47.7327846251232,40.0983063763362));
#196212=CARTESIAN_POINT('Ctrl Pts',(34.7351793935427,47.7303113621607,40.0974846287989));
#196213=CARTESIAN_POINT('Ctrl Pts',(34.7401391868082,47.7280985748129,40.0964130309336));
#196214=CARTESIAN_POINT('Ctrl Pts',(34.74514213706,47.7261394006514,40.0951176960923));
#196215=CARTESIAN_POINT('Ctrl Pts',(34.751773261033,47.7235426275284,40.0934008039614));
#196216=CARTESIAN_POINT('Ctrl Pts',(34.7584811778437,47.7213971161176,40.0912909372156));
#196217=CARTESIAN_POINT('Ctrl Pts',(34.7651763312121,47.7196932909341,40.0888630467851));
#196218=CARTESIAN_POINT('Ctrl Pts',(34.7685239078963,47.7188413783424,40.0876491015699));
#196219=CARTESIAN_POINT('Ctrl Pts',(34.7718684539197,47.7180997687558,40.0863558569271));
#196220=CARTESIAN_POINT('Ctrl Pts',(34.7751999143437,47.7174664279766,40.0849936342771));
#196221=CARTESIAN_POINT('Ctrl Pts',(34.7768656445557,47.7171497575869,40.0843125229521));
#196222=CARTESIAN_POINT('Ctrl Pts',(34.7785281166323,47.7168601447017,40.0836141747074));
#196223=CARTESIAN_POINT('Ctrl Pts',(34.7801861569095,47.7165972740594,40.0828999161609));
#196224=CARTESIAN_POINT('Ctrl Pts',(34.7806006669788,47.7165315563988,40.0827213515243));
#196225=CARTESIAN_POINT('Ctrl Pts',(34.7810149003422,47.7164675099213,40.0825417925842));
#196226=CARTESIAN_POINT('Ctrl Pts',(34.7814288392286,47.716405129283,40.082361260236));
#196227=CARTESIAN_POINT('Ctrl Pts',(34.7826706558879,47.716217987368,40.0818196631917));
#196228=CARTESIAN_POINT('Ctrl Pts',(34.7839098208543,47.7160458390451,40.0812693052021));
#196229=CARTESIAN_POINT('Ctrl Pts',(34.7851458668351,47.7158885307485,40.0807107531875));
#196230=CARTESIAN_POINT('Ctrl Pts',(34.793852415122,47.7147804714195,40.076776384918));
#196231=CARTESIAN_POINT('Ctrl Pts',(34.8024290252897,47.7143609747534,40.0724140586133));
#196232=CARTESIAN_POINT('Ctrl Pts',(34.8108122146636,47.7145286167443,40.0677221223761));
#196233=CARTESIAN_POINT('Ctrl Pts',(34.8148780524504,47.7146099229287,40.0654465383716));
#196234=CARTESIAN_POINT('Ctrl Pts',(34.8188987667937,47.7148297795036,40.0630928000677));
#196235=CARTESIAN_POINT('Ctrl Pts',(34.8228686918044,47.7151790039206,40.0606689262479));
#196236=CARTESIAN_POINT('Ctrl Pts',(34.8289463696258,47.7157136421034,40.0569581447805));
#196237=CARTESIAN_POINT('Ctrl Pts',(34.8349017567801,47.7165501157948,40.0530843804605));
#196238=CARTESIAN_POINT('Ctrl Pts',(34.8407017446573,47.7176563296778,40.0490800251458));
#196239=CARTESIAN_POINT('Ctrl Pts',(34.8433952890326,47.7181700611279,40.0472203818218));
#196240=CARTESIAN_POINT('Ctrl Pts',(34.8460552817724,47.7187417155518,40.0453323608818));
#196241=CARTESIAN_POINT('Ctrl Pts',(34.8486779186782,47.7193692101067,40.0434201572162));
#196242=CARTESIAN_POINT('Ctrl Pts',(34.8488789334633,47.7194173050919,40.0432735943397));
#196243=CARTESIAN_POINT('Ctrl Pts',(34.8490797487417,47.7194657006753,40.0431268995707));
#196244=CARTESIAN_POINT('Ctrl Pts',(34.8492803638663,47.7195143955475,40.0429800745037));
#196245=CARTESIAN_POINT('Ctrl Pts',(34.8520984015311,47.720198411693,40.0409176249753));
#196246=CARTESIAN_POINT('Ctrl Pts',(34.8548765847941,47.7209435418723,40.0388310783332));
#196247=CARTESIAN_POINT('Ctrl Pts',(34.8576119849591,47.7217448891699,40.036725739981));
#196248=CARTESIAN_POINT('Ctrl Pts',(34.8674206434763,47.7246183780644,40.0291763710716));
#196249=CARTESIAN_POINT('Ctrl Pts',(34.8767555719428,47.7282350429865,40.0213310894592));
#196250=CARTESIAN_POINT('Ctrl Pts',(34.885623156561,47.7324659181294,40.0132837551315));
#196251=CARTESIAN_POINT('Ctrl Pts',(34.8953677412285,47.7371152248823,40.004440543132));
#196252=CARTESIAN_POINT('Ctrl Pts',(34.9045486251012,47.7425063743635,39.9953528710595));
#196253=CARTESIAN_POINT('Ctrl Pts',(34.9131661493101,47.7485205638414,39.9861103629549));
#196254=CARTESIAN_POINT('Ctrl Pts',(34.9224709127522,47.7550143791219,39.976130773755));
#196255=CARTESIAN_POINT('Ctrl Pts',(34.9311199164044,47.7622350952177,39.9659696936006));
#196256=CARTESIAN_POINT('Ctrl Pts',(34.9390908738059,47.7700859103005,39.9557128217502));
#196257=CARTESIAN_POINT('Ctrl Pts',(34.9469949630648,47.7778708651112,39.9455419945158));
#196258=CARTESIAN_POINT('Ctrl Pts',(34.9542331399582,47.7862765797896,39.9352756289339));
#196259=CARTESIAN_POINT('Ctrl Pts',(34.9607485668371,47.7952442955498,39.92499));
#196260=CARTESIAN_POINT('Origin',(-0.0123294189942718,0.00895784724493288,
39.92499));
#196261=CARTESIAN_POINT('Ctrl Pts',(36.9278827595333,50.8527980281381,40.10025));
#196262=CARTESIAN_POINT('Ctrl Pts',(36.9209320551076,50.8578435704952,40.10025));
#196263=CARTESIAN_POINT('Ctrl Pts',(36.9136216385513,50.8622636476101,40.0995859581842));
#196264=CARTESIAN_POINT('Ctrl Pts',(36.9061023515959,50.866055238751,40.0983275959621));
#196265=CARTESIAN_POINT('Ctrl Pts',(36.9012978851891,50.8684778849903,40.0975235624068));
#196266=CARTESIAN_POINT('Ctrl Pts',(36.8964085464706,50.8706447895119,40.0964777059491));
#196267=CARTESIAN_POINT('Ctrl Pts',(36.8914758894172,50.8725634718542,40.0952149915962));
#196268=CARTESIAN_POINT('Ctrl Pts',(36.8847438022853,50.8751820882647,40.0934916398702));
#196269=CARTESIAN_POINT('Ctrl Pts',(36.8779301449089,50.8773323251411,40.0913643921631));
#196270=CARTESIAN_POINT('Ctrl Pts',(36.8711298300328,50.8790261328801,40.0889118607714));
#196271=CARTESIAN_POINT('Ctrl Pts',(36.8677296725947,50.8798730367497,40.0876855950755));
#196272=CARTESIAN_POINT('Ctrl Pts',(36.8643326829605,50.8806059576333,40.0863782327527));
#196273=CARTESIAN_POINT('Ctrl Pts',(36.8609495224157,50.8812272732511,40.0850006373334));
#196274=CARTESIAN_POINT('Ctrl Pts',(36.8592579421434,50.88153793106,40.0843118396238));
#196275=CARTESIAN_POINT('Ctrl Pts',(36.8575698050851,50.881820697829,40.0836054919165));
#196276=CARTESIAN_POINT('Ctrl Pts',(36.8558863556343,50.8820759354565,40.0828829920418));
#196277=CARTESIAN_POINT('Ctrl Pts',(36.8554654932716,50.8821397448634,40.0827023670731));
#196278=CARTESIAN_POINT('Ctrl Pts',(36.8550449235855,50.8822018339186,40.0825207326933));
#196279=CARTESIAN_POINT('Ctrl Pts',(36.8546246654171,50.8822622087207,40.0823381109276));
#196280=CARTESIAN_POINT('Ctrl Pts',(36.853363890912,50.8824433331269,40.0817902456304));
#196281=CARTESIAN_POINT('Ctrl Pts',(36.8521059215537,50.8826090281502,40.0812334935553));
#196282=CARTESIAN_POINT('Ctrl Pts',(36.8508512527545,50.8827594682965,40.0806684524227));
#196283=CARTESIAN_POINT('Ctrl Pts',(36.8421807128862,50.8837991030484,40.0767636676137));
#196284=CARTESIAN_POINT('Ctrl Pts',(36.8336410897275,50.8841591194357,40.0724404510888));
#196285=CARTESIAN_POINT('Ctrl Pts',(36.825293116072,50.8839416093724,40.0677949937408));
#196286=CARTESIAN_POINT('Ctrl Pts',(36.8211441960801,50.8838335074679,40.0654862141905));
#196287=CARTESIAN_POINT('Ctrl Pts',(36.8170422299143,50.8835822787324,40.0630972003216));
#196288=CARTESIAN_POINT('Ctrl Pts',(36.8129929908136,50.8831977843863,40.0606363359906));
#196289=CARTESIAN_POINT('Ctrl Pts',(36.8040597645475,50.8823495324292,40.0552073017124));
#196290=CARTESIAN_POINT('Ctrl Pts',(36.7953829494622,50.8808651175409,40.0494204304519));
#196291=CARTESIAN_POINT('Ctrl Pts',(36.7870848098368,50.8788231440727,40.0434049749851));
#196292=CARTESIAN_POINT('Ctrl Pts',(36.7840533947866,50.8780771854142,40.0412074532442));
#196293=CARTESIAN_POINT('Ctrl Pts',(36.7810676701183,50.8772631333232,40.0389814735788));
#196294=CARTESIAN_POINT('Ctrl Pts',(36.7781294934924,50.8763859670022,40.0367321210017));
#196295=CARTESIAN_POINT('Ctrl Pts',(36.7682604691136,50.8734396581487,40.0291767837136));
#196296=CARTESIAN_POINT('Ctrl Pts',(36.7588677364067,50.8697545265632,40.0213235332565));
#196297=CARTESIAN_POINT('Ctrl Pts',(36.7499455893902,50.8654587487954,40.0132649215842));
#196298=CARTESIAN_POINT('Ctrl Pts',(36.7401390929214,50.8607371801604,40.004407552751));
#196299=CARTESIAN_POINT('Ctrl Pts',(36.730900418413,50.8552777667761,39.995301625369));
#196300=CARTESIAN_POINT('Ctrl Pts',(36.7222305213302,50.84919830601,39.9860353422322));
#196301=CARTESIAN_POINT('Ctrl Pts',(36.7128926706965,50.8426504662806,39.9760551582652));
#196302=CARTESIAN_POINT('Ctrl Pts',(36.7042135591825,50.8353827952082,39.9658879738106));
#196303=CARTESIAN_POINT('Ctrl Pts',(36.696217769428,50.8274903908632,39.9556174643197));
#196304=CARTESIAN_POINT('Ctrl Pts',(36.688329949834,50.8197045606266,39.9454856413866));
#196305=CARTESIAN_POINT('Ctrl Pts',(36.6811063421666,50.8113095502195,39.9352519465094));
#196306=CARTESIAN_POINT('Ctrl Pts',(36.6746059268184,50.8023624960587,39.92499));
#196307=CARTESIAN_POINT('Ctrl Pts',(34.6525130919802,48.0191904766733,39.92499));
#196308=CARTESIAN_POINT('Ctrl Pts',(34.6462921588066,48.0106280967246,39.934810724173));
#196309=CARTESIAN_POINT('Ctrl Pts',(34.6407689407914,48.0016058360797,39.9446038383186));
#196310=CARTESIAN_POINT('Ctrl Pts',(34.6359660967484,47.9921771448948,39.9543158069409));
#196311=CARTESIAN_POINT('Ctrl Pts',(34.6313285282523,47.9830729139833,39.9636935671419));
#196312=CARTESIAN_POINT('Ctrl Pts',(34.6273621044907,47.9735885825078,39.972996832102));
#196313=CARTESIAN_POINT('Ctrl Pts',(34.6241270221279,47.9637494987625,39.9821731151371));
#196314=CARTESIAN_POINT('Ctrl Pts',(34.6210688561301,47.9544484832132,39.9908475764388));
#196315=CARTESIAN_POINT('Ctrl Pts',(34.6186639474969,47.9448295964431,39.9994093733883));
#196316=CARTESIAN_POINT('Ctrl Pts',(34.6170045862113,47.9349076763676,40.007796611588));
#196317=CARTESIAN_POINT('Ctrl Pts',(34.6154763423052,47.925769754431,40.0155211172632));
#196318=CARTESIAN_POINT('Ctrl Pts',(34.6145804463109,47.9163742511024,40.0230979941057));
#196319=CARTESIAN_POINT('Ctrl Pts',(34.6144269453424,47.9067364390602,40.0304554104783));
#196320=CARTESIAN_POINT('Ctrl Pts',(34.6143811744522,47.9038626380626,40.0326492435204));
#196321=CARTESIAN_POINT('Ctrl Pts',(34.614401687057,47.9009673483035,40.0348233715072));
#196322=CARTESIAN_POINT('Ctrl Pts',(34.614492141918,47.8980511519202,40.0369753512356));
#196323=CARTESIAN_POINT('Ctrl Pts',(34.6145816725532,47.8951647518763,40.0391053430352));
#196324=CARTESIAN_POINT('Ctrl Pts',(34.6147393566957,47.8922608568395,40.041211089324));
#196325=CARTESIAN_POINT('Ctrl Pts',(34.61496832346,47.8893433277781,40.0432881154904));
#196326=CARTESIAN_POINT('Ctrl Pts',(34.614984245361,47.889140448513,40.043432547828));
#196327=CARTESIAN_POINT('Ctrl Pts',(34.6150005017601,47.8889374970511,40.0435768364421));
#196328=CARTESIAN_POINT('Ctrl Pts',(34.6150170939194,47.888734473721,40.0437209807855));
#196329=CARTESIAN_POINT('Ctrl Pts',(34.6157445549675,47.8798331871997,40.0500407968419));
#196330=CARTESIAN_POINT('Ctrl Pts',(34.6171603320598,47.8708080647648,40.0560490279342));
#196331=CARTESIAN_POINT('Ctrl Pts',(34.6193291901739,47.8617555581816,40.0616647108611));
#196332=CARTESIAN_POINT('Ctrl Pts',(34.6213509428813,47.8533170487311,40.0668995033481));
#196333=CARTESIAN_POINT('Ctrl Pts',(34.6240275231022,47.8448540540106,40.0717933267476));
#196334=CARTESIAN_POINT('Ctrl Pts',(34.6274308957716,47.8364666369703,40.0762460303065));
#196335=CARTESIAN_POINT('Ctrl Pts',(34.6286758935245,47.8333984113065,40.0778748868743));
#196336=CARTESIAN_POINT('Ctrl Pts',(34.6300183184514,47.830340571385,40.0794443522245));
#196337=CARTESIAN_POINT('Ctrl Pts',(34.6314622582454,47.8272990958126,40.0809482021492));
#196338=CARTESIAN_POINT('Ctrl Pts',(34.631809477528,47.8265677225443,40.0813098278168));
#196339=CARTESIAN_POINT('Ctrl Pts',(34.6321630753109,47.8258370084444,40.0816679525672));
#196340=CARTESIAN_POINT('Ctrl Pts',(34.6325230544381,47.8251070891645,40.082022419258));
#196341=CARTESIAN_POINT('Ctrl Pts',(34.6328717842176,47.8243999798622,40.0823658088648));
#196342=CARTESIAN_POINT('Ctrl Pts',(34.6332265027185,47.823693616494,40.0827057654616));
#196343=CARTESIAN_POINT('Ctrl Pts',(34.6335872094469,47.8229881245976,40.0830421470151));
#196344=CARTESIAN_POINT('Ctrl Pts',(34.6375391685168,47.815258645554,40.0867275956808));
#196345=CARTESIAN_POINT('Ctrl Pts',(34.6422128973073,47.8076288798872,40.0899823432034));
#196346=CARTESIAN_POINT('Ctrl Pts',(34.6475865476024,47.8002860618997,40.092629952936));
#196347=CARTESIAN_POINT('Ctrl Pts',(34.6498151605508,47.7972407764148,40.0937279956087));
#196348=CARTESIAN_POINT('Ctrl Pts',(34.6521637338122,47.7942448304644,40.0947220371803));
#196349=CARTESIAN_POINT('Ctrl Pts',(34.6546289547343,47.7913110614415,40.0956014538692));
#196350=CARTESIAN_POINT('Ctrl Pts',(34.6588336459116,47.7863072126522,40.097101390674));
#196351=CARTESIAN_POINT('Ctrl Pts',(34.6633779280164,47.781486720129,40.0982667904316));
#196352=CARTESIAN_POINT('Ctrl Pts',(34.6682420184012,47.776919623742,40.0990539325582));
#196353=CARTESIAN_POINT('Ctrl Pts',(34.6706740635936,47.7746360755484,40.0994475036216));
#196354=CARTESIAN_POINT('Ctrl Pts',(34.6731869650549,47.7724170058816,40.0997467259952));
#196355=CARTESIAN_POINT('Ctrl Pts',(34.6757782448039,47.7702712352608,40.0999473488896));
#196356=CARTESIAN_POINT('Ctrl Pts',(34.6783695245528,47.7681254646399,40.100147971784));
#196357=CARTESIAN_POINT('Ctrl Pts',(34.6810391382375,47.766053003919,40.10025));
#196358=CARTESIAN_POINT('Ctrl Pts',(34.6837837831351,47.7640607692759,40.10025));
#196359=CARTESIAN_POINT('Origin',(38.9973987043324,43.2882232241944,39.92499));
#196360=CARTESIAN_POINT('Ctrl Pts',(42.0671296588101,46.4355828792665,39.92499));
#196361=CARTESIAN_POINT('Ctrl Pts',(42.0742293550387,46.4434678907495,39.9348354642026));
#196362=CARTESIAN_POINT('Ctrl Pts',(42.0806858315487,46.4518896956747,39.9446440828474));
#196363=CARTESIAN_POINT('Ctrl Pts',(42.0864721532177,46.4607957007331,39.9543641760356));
#196364=CARTESIAN_POINT('Ctrl Pts',(42.0920704538875,46.4694123136588,39.9637684240743));
#196365=CARTESIAN_POINT('Ctrl Pts',(42.0970420880528,46.4784832882836,39.9730909636433));
#196366=CARTESIAN_POINT('Ctrl Pts',(42.1013257711412,46.487988795821,39.9822808977183));
#196367=CARTESIAN_POINT('Ctrl Pts',(42.1053778715688,46.496980420636,39.9909740094698));
#196368=CARTESIAN_POINT('Ctrl Pts',(42.1088147776146,46.5063617095277,39.9995492765054));
#196369=CARTESIAN_POINT('Ctrl Pts',(42.1115441100144,46.5161273793285,40.0079462328752));
#196370=CARTESIAN_POINT('Ctrl Pts',(42.1140580225451,46.5251222674863,40.0156804369753));
#196371=CARTESIAN_POINT('Ctrl Pts',(42.1159717447031,46.5344438074388,40.023263801749));
#196372=CARTESIAN_POINT('Ctrl Pts',(42.1171748456151,46.5440884908269,40.0306257270039));
#196373=CARTESIAN_POINT('Ctrl Pts',(42.1175238194559,46.5468860468525,40.0327611416699));
#196374=CARTESIAN_POINT('Ctrl Pts',(42.1178127362988,46.5497107674255,40.0348777427294));
#196375=CARTESIAN_POINT('Ctrl Pts',(42.118038206898,46.5525624800837,40.03697331687));
#196376=CARTESIAN_POINT('Ctrl Pts',(42.1182826315244,46.5556539199569,40.039245053974));
#196377=CARTESIAN_POINT('Ctrl Pts',(42.1184532289198,46.5587726948494,40.041487875195));
#196378=CARTESIAN_POINT('Ctrl Pts',(42.1185461584685,46.5619176830189,40.0436985701601));
#196379=CARTESIAN_POINT('Ctrl Pts',(42.118801204344,46.5705491277284,40.0497658398386));
#196380=CARTESIAN_POINT('Ctrl Pts',(42.1184278543826,46.5793682643807,40.0555581699984));
#196381=CARTESIAN_POINT('Ctrl Pts',(42.1173773384972,46.5882835698999,40.0609828468886));
#196382=CARTESIAN_POINT('Ctrl Pts',(42.1164161734959,46.5964405904273,40.0659461317308));
#196383=CARTESIAN_POINT('Ctrl Pts',(42.114880157948,46.6046697328847,40.0706039980713));
#196384=CARTESIAN_POINT('Ctrl Pts',(42.1127009621828,46.6129145292196,40.0748843180612));
#196385=CARTESIAN_POINT('Ctrl Pts',(42.1116305483418,46.6169643462457,40.0769867972576));
#196386=CARTESIAN_POINT('Ctrl Pts',(42.1104045383081,46.6210176421366,40.0789976708178));
#196387=CARTESIAN_POINT('Ctrl Pts',(42.1090123875513,46.6250654385587,40.08090504915));
#196388=CARTESIAN_POINT('Ctrl Pts',(42.1087482405049,46.6258334685039,40.0812669556105));
#196389=CARTESIAN_POINT('Ctrl Pts',(42.1084776383333,46.6266015422609,40.0816253922033));
#196390=CARTESIAN_POINT('Ctrl Pts',(42.1082005605491,46.6273695213201,40.081980198914));
#196391=CARTESIAN_POINT('Ctrl Pts',(42.1079321414455,46.6281135010337,40.082323917915));
#196392=CARTESIAN_POINT('Ctrl Pts',(42.1076576451506,46.6288573918592,40.0826642303499));
#196393=CARTESIAN_POINT('Ctrl Pts',(42.1073770559085,46.6296010653155,40.08300099161));
#196394=CARTESIAN_POINT('Ctrl Pts',(42.1043192521653,46.6377054654042,40.0866709464311));
#196395=CARTESIAN_POINT('Ctrl Pts',(42.1005354505683,46.6457892400059,40.0899175831875));
#196396=CARTESIAN_POINT('Ctrl Pts',(42.0960238460782,46.6536619390745,40.0925642067058));
#196397=CARTESIAN_POINT('Ctrl Pts',(42.094118567486,46.6569866287789,40.0936818922525));
#196398=CARTESIAN_POINT('Ctrl Pts',(42.0920839261391,46.6602736399403,40.094693009479));
#196399=CARTESIAN_POINT('Ctrl Pts',(42.0899216923184,46.6635089796838,40.0955863397546));
#196400=CARTESIAN_POINT('Ctrl Pts',(42.0862805445931,46.668957210969,40.0970906856167));
#196401=CARTESIAN_POINT('Ctrl Pts',(42.0822770520161,46.674256436667,40.0982599215483));
#196402=CARTESIAN_POINT('Ctrl Pts',(42.0779224130577,46.6793332901445,40.0990497370454));
#196403=CARTESIAN_POINT('Ctrl Pts',(42.0768337533181,46.6806025035139,40.0992471909196));
#196404=CARTESIAN_POINT('Ctrl Pts',(42.0757229796951,46.68185765499,40.0994209989363));
#196405=CARTESIAN_POINT('Ctrl Pts',(42.0745900553981,46.6830973739106,40.0995705982975));
#196406=CARTESIAN_POINT('Ctrl Pts',(42.0728906689526,46.6849569522914,40.0997949973393));
#196407=CARTESIAN_POINT('Ctrl Pts',(42.0711414461008,46.6867817869756,40.0999649129781));
#196408=CARTESIAN_POINT('Ctrl Pts',(42.0693433991613,46.6885684866728,40.1000786629733));
#196409=CARTESIAN_POINT('Ctrl Pts',(42.0675453522218,46.69035518637,40.1001924129685));
#196410=CARTESIAN_POINT('Ctrl Pts',(42.0656984926182,46.6921037531358,40.10025));
#196411=CARTESIAN_POINT('Ctrl Pts',(42.0638038389718,46.6938111422612,40.10025));
#196412=CARTESIAN_POINT('Ctrl Pts',(39.5091373124628,43.8565665267052,40.10025));
#196413=CARTESIAN_POINT('Ctrl Pts',(39.5155480799608,43.8507890749202,40.10025));
#196414=CARTESIAN_POINT('Ctrl Pts',(39.5223801852473,43.8455908828145,40.099578633424));
#196415=CARTESIAN_POINT('Ctrl Pts',(39.5294841269575,43.8409939475737,40.0983063763365));
#196416=CARTESIAN_POINT('Ctrl Pts',(39.5340725443954,43.8380247990812,40.0974846287991));
#196417=CARTESIAN_POINT('Ctrl Pts',(39.5387738681339,43.8353056940455,40.0964130309337));
#196418=CARTESIAN_POINT('Ctrl Pts',(39.5435446222369,43.8328343017432,40.0951176960924));
#196419=CARTESIAN_POINT('Ctrl Pts',(39.5498679835149,43.8295586128165,40.0934008039614));
#196420=CARTESIAN_POINT('Ctrl Pts',(39.5563148866448,43.8267236865057,40.0912909372156));
#196421=CARTESIAN_POINT('Ctrl Pts',(39.5627952650345,43.8243293609619,40.0888630467851));
#196422=CARTESIAN_POINT('Ctrl Pts',(39.5660354542293,43.82313219819,40.0876491015699));
#196423=CARTESIAN_POINT('Ctrl Pts',(39.5692841591691,43.8220450509621,40.0863558569271));
#196424=CARTESIAN_POINT('Ctrl Pts',(39.572531167366,43.8210669472514,40.0849936342771));
#196425=CARTESIAN_POINT('Ctrl Pts',(39.5741546714645,43.820577895396,40.0843125229521));
#196426=CARTESIAN_POINT('Ctrl Pts',(39.5757777635552,43.8201160933891,40.0836141747074));
#196427=CARTESIAN_POINT('Ctrl Pts',(39.57739924345,43.8196813503774,40.0828999161609));
#196428=CARTESIAN_POINT('Ctrl Pts',(39.5778046134237,43.8195726646245,40.0827213515243));
#196429=CARTESIAN_POINT('Ctrl Pts',(39.5782098828935,43.8194656698234,40.0825417925842));
#196430=CARTESIAN_POINT('Ctrl Pts',(39.5786150336271,43.8193603625171,40.0823612602361));
#196431=CARTESIAN_POINT('Ctrl Pts',(39.5798304858281,43.819044440598,40.0818196631917));
#196432=CARTESIAN_POINT('Ctrl Pts',(39.5810448681195,43.8187437073119,40.0812693052022));
#196433=CARTESIAN_POINT('Ctrl Pts',(39.5822576997166,43.8184580587797,40.0807107531875));
#196434=CARTESIAN_POINT('Ctrl Pts',(39.5908007288817,43.816445987403,40.0767763849182));
#196435=CARTESIAN_POINT('Ctrl Pts',(39.5992865061392,43.8151322889027,40.0724140586137));
#196436=CARTESIAN_POINT('Ctrl Pts',(39.6076412948839,43.8144227306307,40.0677221223768));
#196437=CARTESIAN_POINT('Ctrl Pts',(39.6116933583968,43.8140785956355,40.065446538372));
#196438=CARTESIAN_POINT('Ctrl Pts',(39.6157150281166,43.8138769687215,40.0630928000679));
#196439=CARTESIAN_POINT('Ctrl Pts',(39.6196997093547,43.8138093098899,40.0606689262479));
#196440=CARTESIAN_POINT('Ctrl Pts',(39.6257999779287,43.8137057289459,40.0569581447805));
#196441=CARTESIAN_POINT('Ctrl Pts',(39.6318101761586,43.8139151128795,40.0530843804605));
#196442=CARTESIAN_POINT('Ctrl Pts',(39.6376940219325,43.8144090029874,40.0490800251457));
#196443=CARTESIAN_POINT('Ctrl Pts',(39.6404265103489,43.8146383681085,40.0472203818218));
#196444=CARTESIAN_POINT('Ctrl Pts',(39.6431316855286,43.8149288459962,40.0453323608818));
#196445=CARTESIAN_POINT('Ctrl Pts',(39.6458055463966,43.8152787628648,40.0434201572162));
#196446=CARTESIAN_POINT('Ctrl Pts',(39.6460104872966,43.8153055826141,40.0432735943397));
#196447=CARTESIAN_POINT('Ctrl Pts',(39.6462152612038,43.8153327221689,40.0431268995707));
#196448=CARTESIAN_POINT('Ctrl Pts',(39.6464198673379,43.815360180295,40.0429800745037));
#196449=CARTESIAN_POINT('Ctrl Pts',(39.6492939666541,43.8157458841819,40.0409176249753));
#196450=CARTESIAN_POINT('Ctrl Pts',(39.6521348180511,43.816196533233,40.0388310783332));
#196451=CARTESIAN_POINT('Ctrl Pts',(39.6549389970093,43.8167075634905,40.036725739981));
#196452=CARTESIAN_POINT('Ctrl Pts',(39.6649942840468,43.8185400271106,40.029176371072));
#196453=CARTESIAN_POINT('Ctrl Pts',(39.6746561192245,43.8211611138364,40.0213310894599));
#196454=CARTESIAN_POINT('Ctrl Pts',(39.6839173731629,43.8244418968093,40.0132837551326));
#196455=CARTESIAN_POINT('Ctrl Pts',(39.6940945608659,43.8280471477127,40.0044405431333));
#196456=CARTESIAN_POINT('Ctrl Pts',(39.7037886794665,43.8324491002301,39.995352871061));
#196457=CARTESIAN_POINT('Ctrl Pts',(39.7129876499599,43.8375295667859,39.9861103629567));
#196458=CARTESIAN_POINT('Ctrl Pts',(39.7229202294665,43.8430151956431,39.9761307737567));
#196459=CARTESIAN_POINT('Ctrl Pts',(39.7322766233292,43.8492922888401,39.9659696936022));
#196460=CARTESIAN_POINT('Ctrl Pts',(39.7410245486281,43.8562669044084,39.9557128217517));
#196461=CARTESIAN_POINT('Ctrl Pts',(39.7496990878225,43.8631830101187,39.9455419945167));
#196462=CARTESIAN_POINT('Ctrl Pts',(39.7577762496639,43.8707860819054,39.9352756289344));
#196463=CARTESIAN_POINT('Ctrl Pts',(39.7651933659004,43.8790236240215,39.92499));
#196464=CARTESIAN_POINT('Origin',(-0.0113255271402735,0.010197550440905,
39.92499));
#196465=CARTESIAN_POINT('Ctrl Pts',(42.0411527846901,46.7142062431418,40.10025));
#196466=CARTESIAN_POINT('Ctrl Pts',(42.0347675597388,46.7199506919427,40.10025));
#196467=CARTESIAN_POINT('Ctrl Pts',(42.027959214277,46.7251107020217,40.099585958184));
#196468=CARTESIAN_POINT('Ctrl Pts',(42.0208774479568,46.7296675019402,40.0983275959617));
#196469=CARTESIAN_POINT('Ctrl Pts',(42.0163525364088,46.7325790801597,40.0975235624065));
#196470=CARTESIAN_POINT('Ctrl Pts',(42.0117164851997,46.7352451892138,40.0964777059488));
#196471=CARTESIAN_POINT('Ctrl Pts',(42.0070114066753,46.7376689638747,40.0952149915961));
#196472=CARTESIAN_POINT('Ctrl Pts',(42.0005899185703,46.740976929953,40.0934916398701));
#196473=CARTESIAN_POINT('Ctrl Pts',(41.9940383480783,46.7438276087415,40.0913643921631));
#196474=CARTESIAN_POINT('Ctrl Pts',(41.9874523371586,46.7462229640883,40.0889118607713));
#196475=CARTESIAN_POINT('Ctrl Pts',(41.9841593316988,46.7474206417617,40.0876855950754));
#196476=CARTESIAN_POINT('Ctrl Pts',(41.9808575622229,46.7485046297342,40.0863782327526));
#196477=CARTESIAN_POINT('Ctrl Pts',(41.9775578801523,46.7494761782928,40.0850006373334));
#196478=CARTESIAN_POINT('Ctrl Pts',(41.9759080391171,46.7499619525721,40.0843118396237));
#196479=CARTESIAN_POINT('Ctrl Pts',(41.9742587070261,46.7504196286876,40.0836054919164));
#196480=CARTESIAN_POINT('Ctrl Pts',(41.9726111592845,46.7508494364808,40.0828829920417));
#196481=CARTESIAN_POINT('Ctrl Pts',(41.9721992723491,46.7509568884291,40.0827023670731));
#196482=CARTESIAN_POINT('Ctrl Pts',(41.9717874966612,46.751062598857,40.0825207326932));
#196483=CARTESIAN_POINT('Ctrl Pts',(41.9713758515963,46.7511665718601,40.0823381109275));
#196484=CARTESIAN_POINT('Ctrl Pts',(41.9701409164017,46.7514784908694,40.0817902456303));
#196485=CARTESIAN_POINT('Ctrl Pts',(41.9689071581774,46.7517747718019,40.0812334935553));
#196486=CARTESIAN_POINT('Ctrl Pts',(41.9676750878624,46.7520555364228,40.0806684524227));
#196487=CARTESIAN_POINT('Ctrl Pts',(41.9591607175417,46.7539957941549,40.0767636676136));
#196488=CARTESIAN_POINT('Ctrl Pts',(41.9507055072917,46.7552464720204,40.0724404510887));
#196489=CARTESIAN_POINT('Ctrl Pts',(41.9423805287167,46.7559027543576,40.0677949937407));
#196490=CARTESIAN_POINT('Ctrl Pts',(41.9382430372167,46.7562289248776,40.0654862141904));
#196491=CARTESIAN_POINT('Ctrl Pts',(41.9341372814972,46.756407844619,40.0630972003215));
#196492=CARTESIAN_POINT('Ctrl Pts',(41.9300700339489,46.7564487173138,40.0606363359906));
#196493=CARTESIAN_POINT('Ctrl Pts',(41.9210970783574,46.7565388885834,40.0552073017123));
#196494=CARTESIAN_POINT('Ctrl Pts',(41.9123126321659,46.7559695796221,40.0494204304519));
#196495=CARTESIAN_POINT('Ctrl Pts',(41.903846506269,46.7548061840812,40.0434049749851));
#196496=CARTESIAN_POINT('Ctrl Pts',(41.9007537237153,46.754381181019,40.0412074532442));
#196497=CARTESIAN_POINT('Ctrl Pts',(41.8976992635451,46.7538836816018,40.0389814735788));
#196498=CARTESIAN_POINT('Ctrl Pts',(41.8946854937106,46.7533184435772,40.0367321210017));
#196499=CARTESIAN_POINT('Ctrl Pts',(41.8845625597433,46.7514198688641,40.0291767837137));
#196500=CARTESIAN_POINT('Ctrl Pts',(41.8748360802674,46.7487367327307,40.0213235332568));
#196501=CARTESIAN_POINT('Ctrl Pts',(41.8655137786572,46.7453971059997,40.0132649215846));
#196502=CARTESIAN_POINT('Ctrl Pts',(41.8552674648883,46.7417264606175,40.0044075527515));
#196503=CARTESIAN_POINT('Ctrl Pts',(41.8455087367141,46.7372626589199,39.9953016253697));
#196504=CARTESIAN_POINT('Ctrl Pts',(41.8362508575433,46.7321227530947,39.986035342233));
#196505=CARTESIAN_POINT('Ctrl Pts',(41.8262797250076,46.7265868542934,39.976055158266));
#196506=CARTESIAN_POINT('Ctrl Pts',(41.8168884800858,46.7202662104726,39.9658879738113));
#196507=CARTESIAN_POINT('Ctrl Pts',(41.8081115112066,46.7132528291601,39.9556174643203));
#196508=CARTESIAN_POINT('Ctrl Pts',(41.7994530610437,46.7063341521769,39.9454856413871));
#196509=CARTESIAN_POINT('Ctrl Pts',(41.791391507518,46.6987402031241,39.9352519465097));
#196510=CARTESIAN_POINT('Ctrl Pts',(41.7839914803032,46.6905216402892,39.92499));
#196511=CARTESIAN_POINT('Ctrl Pts',(39.4820551873935,44.1339623850442,39.92499));
#196512=CARTESIAN_POINT('Ctrl Pts',(39.4749733207254,44.1260971752943,39.9348107241722));
#196513=CARTESIAN_POINT('Ctrl Pts',(39.4685372764365,44.1177016730294,39.9446038383168));
#196514=CARTESIAN_POINT('Ctrl Pts',(39.4627751762759,44.1088266671093,39.9543158069383));
#196515=CARTESIAN_POINT('Ctrl Pts',(39.457211361599,44.100257068036,39.9636935671389));
#196516=CARTESIAN_POINT('Ctrl Pts',(39.4522752837276,44.0912392969017,39.9729968320986));
#196517=CARTESIAN_POINT('Ctrl Pts',(39.4480294591806,44.0817922708751,39.9821731151332));
#196518=CARTESIAN_POINT('Ctrl Pts',(39.4440158252738,44.0728618726545,39.9908475764349));
#196519=CARTESIAN_POINT('Ctrl Pts',(39.4406186435292,44.0635470605566,39.9994093733843));
#196520=CARTESIAN_POINT('Ctrl Pts',(39.43793124934,44.0538529442829,40.0077966115839));
#196521=CARTESIAN_POINT('Ctrl Pts',(39.4354562043761,44.0449248258259,40.0155211172592));
#196522=CARTESIAN_POINT('Ctrl Pts',(39.4335831186691,44.0356744386791,40.0230979941019));
#196523=CARTESIAN_POINT('Ctrl Pts',(39.4324230329126,44.0261054688002,40.0304554104745));
#196524=CARTESIAN_POINT('Ctrl Pts',(39.4320771187579,44.0232521951443,40.0326492435179));
#196525=CARTESIAN_POINT('Ctrl Pts',(39.431794878803,44.0203706219328,40.0348233715059));
#196526=CARTESIAN_POINT('Ctrl Pts',(39.4315800126161,44.0174609456692,40.0369753512355));
#196527=CARTESIAN_POINT('Ctrl Pts',(39.4313673418322,44.014580999127,40.0391053430352));
#196528=CARTESIAN_POINT('Ctrl Pts',(39.4312206224788,44.01167652945,40.041211089324));
#196529=CARTESIAN_POINT('Ctrl Pts',(39.4311433701099,44.0087510493741,40.0432881154904));
#196530=CARTESIAN_POINT('Ctrl Pts',(39.4311379981313,44.0085476172109,40.043432547828));
#196531=CARTESIAN_POINT('Ctrl Pts',(39.4311329512716,44.0083440782819,40.0435768364421));
#196532=CARTESIAN_POINT('Ctrl Pts',(39.4311282308207,44.008140432782,40.0437209807855));
#196533=CARTESIAN_POINT('Ctrl Pts',(39.4309212689598,43.9992118680539,40.0500407968421));
#196534=CARTESIAN_POINT('Ctrl Pts',(39.4313859080982,43.99008819718,40.0560490279346));
#196535=CARTESIAN_POINT('Ctrl Pts',(39.4325966403789,43.980858573769,40.0616647108617));
#196536=CARTESIAN_POINT('Ctrl Pts',(39.4337252532884,43.9722549606522,40.0668995033488));
#196537=CARTESIAN_POINT('Ctrl Pts',(39.4355025470901,43.9635585482846,40.0717933267485));
#196538=CARTESIAN_POINT('Ctrl Pts',(39.4380105519142,43.954861329077,40.0762460303076));
#196539=CARTESIAN_POINT('Ctrl Pts',(39.4389280125254,43.9516797737732,40.077874886875));
#196540=CARTESIAN_POINT('Ctrl Pts',(39.4399434521999,43.9484983634047,40.0794443522249));
#196541=CARTESIAN_POINT('Ctrl Pts',(39.4410615611728,43.9453226165467,40.0809482021492));
#196542=CARTESIAN_POINT('Ctrl Pts',(39.441330429028,43.9445589555196,40.0813098278169));
#196543=CARTESIAN_POINT('Ctrl Pts',(39.4416057093433,43.9437952833152,40.0816679525672));
#196544=CARTESIAN_POINT('Ctrl Pts',(39.4418874191266,43.9430317345445,40.0820224192581));
#196545=CARTESIAN_POINT('Ctrl Pts',(39.4421603254791,43.942292046673,40.0823658088648));
#196546=CARTESIAN_POINT('Ctrl Pts',(39.4424392657175,43.9415524746574,40.0827057654617));
#196547=CARTESIAN_POINT('Ctrl Pts',(39.442724252473,43.9408131433995,40.0830421470151));
#196548=CARTESIAN_POINT('Ctrl Pts',(39.445846611731,43.9327129150432,40.0867275956805));
#196549=CARTESIAN_POINT('Ctrl Pts',(39.4496972096654,43.9246364083437,40.0899823432028));
#196550=CARTESIAN_POINT('Ctrl Pts',(39.4542738890611,43.9167721156746,40.0926299529352));
#196551=CARTESIAN_POINT('Ctrl Pts',(39.456171974423,43.9135105590948,40.0937279956082));
#196552=CARTESIAN_POINT('Ctrl Pts',(39.4581945203286,43.910285532495,40.0947220371802));
#196553=CARTESIAN_POINT('Ctrl Pts',(39.4603395741455,43.9071101492104,40.0956014538693));
#196554=CARTESIAN_POINT('Ctrl Pts',(39.4639981869602,43.9016942021211,40.097101390674));
#196555=CARTESIAN_POINT('Ctrl Pts',(39.4680136963365,43.8964251099352,40.0982667904316));
#196556=CARTESIAN_POINT('Ctrl Pts',(39.4723737491585,43.8913745966871,40.0990539325582));
#196557=CARTESIAN_POINT('Ctrl Pts',(39.4745537755695,43.888849340063,40.0994475036216));
#196558=CARTESIAN_POINT('Ctrl Pts',(39.4768209551515,43.8863797569638,40.0997467259952));
#196559=CARTESIAN_POINT('Ctrl Pts',(39.4791737454933,43.8839748786089,40.0999473488896));
#196560=CARTESIAN_POINT('Ctrl Pts',(39.481526535835,43.8815700002539,40.100147971784));
#196561=CARTESIAN_POINT('Ctrl Pts',(39.4839648939622,43.8792298420736,40.10025));
#196562=CARTESIAN_POINT('Ctrl Pts',(39.4864862581822,43.876961627587,40.10025));
#196563=CARTESIAN_POINT('Origin',(43.3086183250771,38.9747476500508,39.92499));
#196564=CARTESIAN_POINT('Ctrl Pts',(46.6905216402902,41.7839914803021,39.92499));
#196565=CARTESIAN_POINT('Ctrl Pts',(46.6984066517725,41.7910911765301,39.9348354642018));
#196566=CARTESIAN_POINT('Ctrl Pts',(46.7057080773548,41.7987919603583,39.9446440828458));
#196567=CARTESIAN_POINT('Ctrl Pts',(46.7123936319703,41.8070443420764,39.9543641760331));
#196568=CARTESIAN_POINT('Ctrl Pts',(46.7188619458706,41.8150285705283,39.9637684240712));
#196569=CARTESIAN_POINT('Ctrl Pts',(46.7247545199412,41.8235301761251,39.9730909636396));
#196570=CARTESIAN_POINT('Ctrl Pts',(46.7300083326608,41.8325358446865,39.982280897714));
#196571=CARTESIAN_POINT('Ctrl Pts',(46.7349781159823,41.8410546526084,39.9909740094649));
#196572=CARTESIAN_POINT('Ctrl Pts',(46.7393768060084,41.8500252953099,39.9995492765001));
#196573=CARTESIAN_POINT('Ctrl Pts',(46.743111977297,41.8594521748273,40.0079462328694));
#196574=CARTESIAN_POINT('Ctrl Pts',(46.7465523401882,41.8681350126322,40.0156804369689));
#196575=CARTESIAN_POINT('Ctrl Pts',(46.7494299450227,41.8772054497762,40.0232638017421));
#196576=CARTESIAN_POINT('Ctrl Pts',(46.7516345991556,41.8866715402891,40.0306257269965));
#196577=CARTESIAN_POINT('Ctrl Pts',(46.7522740855143,41.8894172933139,40.0327611416651));
#196578=CARTESIAN_POINT('Ctrl Pts',(46.7528566833419,41.8921963397415,40.0348777427271));
#196579=CARTESIAN_POINT('Ctrl Pts',(46.7533790039321,41.8950088623274,40.0369733168701));
#196580=CARTESIAN_POINT('Ctrl Pts',(46.753945233034,41.898057817639,40.039245053974));
#196581=CARTESIAN_POINT('Ctrl Pts',(46.7544408966258,41.9011416752728,40.041487875195));
#196582=CARTESIAN_POINT('Ctrl Pts',(46.7548620578771,41.9042597210851,40.0436985701601));
#196583=CARTESIAN_POINT('Ctrl Pts',(46.7560179382359,41.9128172222839,40.0497658398386));
#196584=CARTESIAN_POINT('Ctrl Pts',(46.7565684843263,41.9216270724806,40.0555581699984));
#196585=CARTESIAN_POINT('Ctrl Pts',(46.7564556264623,41.9306033478345,40.0609828468885));
#196586=CARTESIAN_POINT('Ctrl Pts',(46.7563523676439,41.9388161524503,40.0659461317306));
#196587=CARTESIAN_POINT('Ctrl Pts',(46.7556849461651,41.9471607721488,40.070603998071));
#196588=CARTESIAN_POINT('Ctrl Pts',(46.7543795041532,41.955588190611,40.0748843180608));
#196589=CARTESIAN_POINT('Ctrl Pts',(46.7537382753015,41.9597277110298,40.0769867972572));
#196590=CARTESIAN_POINT('Ctrl Pts',(46.7529426662697,41.9638869554867,40.0789976708176));
#196591=CARTESIAN_POINT('Ctrl Pts',(46.7519812518,41.968058097036,40.0809050491499));
#196592=CARTESIAN_POINT('Ctrl Pts',(46.7517988327686,41.9688495305176,40.0812669556104));
#196593=CARTESIAN_POINT('Ctrl Pts',(46.7516099985535,41.9696416823153,40.0816253922032));
#196594=CARTESIAN_POINT('Ctrl Pts',(46.7514147143012,41.9704344168199,40.0819801989139));
#196595=CARTESIAN_POINT('Ctrl Pts',(46.7512255326818,41.9712023783711,40.0823239179149));
#196596=CARTESIAN_POINT('Ctrl Pts',(46.751030297871,41.9719708867607,40.0826642303498));
#196597=CARTESIAN_POINT('Ctrl Pts',(46.7508289807697,41.9727398158583,40.0830009916099));
#196598=CARTESIAN_POINT('Ctrl Pts',(46.7486350684821,41.9811194467227,40.0866709464314));
#196599=CARTESIAN_POINT('Ctrl Pts',(46.7457169794822,41.9895544525285,40.0899175831881));
#196600=CARTESIAN_POINT('Ctrl Pts',(46.7420530111684,41.9978556152131,40.0925642067066));
#196601=CARTESIAN_POINT('Ctrl Pts',(46.7405056945977,42.0013612477617,40.093681892253));
#196602=CARTESIAN_POINT('Ctrl Pts',(46.7388257854549,42.0048429302643,40.0946930094791));
#196603=CARTESIAN_POINT('Ctrl Pts',(46.7370135816694,42.0082865614558,40.0955863397545));
#196604=CARTESIAN_POINT('Ctrl Pts',(46.733961875776,42.0140855503361,40.0970906856166));
#196605=CARTESIAN_POINT('Ctrl Pts',(46.7305342346691,42.0197742252481,40.0982599215483));
#196606=CARTESIAN_POINT('Ctrl Pts',(46.7267341265709,42.0252784509096,40.0990497370453));
#196607=CARTESIAN_POINT('Ctrl Pts',(46.7257840995464,42.026654507325,40.0992471909196));
#196608=CARTESIAN_POINT('Ctrl Pts',(46.7248106099125,42.0280188904098,40.0994209989363));
#196609=CARTESIAN_POINT('Ctrl Pts',(46.723813477807,42.0293702408562,40.0995705982975));
#196610=CARTESIAN_POINT('Ctrl Pts',(46.7223177796487,42.0313972665257,40.0997949973393));
#196611=CARTESIAN_POINT('Ctrl Pts',(46.7207688863879,42.0333949481511,40.0999649129781));
#196612=CARTESIAN_POINT('Ctrl Pts',(46.7191674503113,42.0353598072039,40.1000786629733));
#196613=CARTESIAN_POINT('Ctrl Pts',(46.7175660142347,42.0373246662567,40.1001924129685));
#196614=CARTESIAN_POINT('Ctrl Pts',(46.7159120469168,42.0392567035858,40.10025));
#196615=CARTESIAN_POINT('Ctrl Pts',(46.7142062431428,42.041152784689,40.10025));
#196616=CARTESIAN_POINT('Ctrl Pts',(43.8769616275879,39.4864862581812,40.10025));
#196617=CARTESIAN_POINT('Ctrl Pts',(43.8827333680738,39.4800703482071,40.10025));
#196618=CARTESIAN_POINT('Ctrl Pts',(43.8889846873397,39.4741864828754,40.0995786334241));
#196619=CARTESIAN_POINT('Ctrl Pts',(43.895569202337,39.468872166017,40.0983063763367));
#196620=CARTESIAN_POINT('Ctrl Pts',(43.8998221234153,39.4654396626066,40.0974846287993));
#196621=CARTESIAN_POINT('Ctrl Pts',(43.90421346894,39.4622440309668,40.0964130309338));
#196622=CARTESIAN_POINT('Ctrl Pts',(43.9086997575138,39.4592874976149,40.0951176960923));
#196623=CARTESIAN_POINT('Ctrl Pts',(43.9146460760275,39.4553687820177,40.0934008039613));
#196624=CARTESIAN_POINT('Ctrl Pts',(43.9207613318567,39.4518755008528,40.0912909372156));
#196625=CARTESIAN_POINT('Ctrl Pts',(43.9269559348858,39.4488169076804,40.0888630467851));
#196626=CARTESIAN_POINT('Ctrl Pts',(43.9300532364004,39.4472876110942,40.0876491015698));
#196627=CARTESIAN_POINT('Ctrl Pts',(43.9331705067656,39.4458668372377,40.0863558569271));
#196628=CARTESIAN_POINT('Ctrl Pts',(43.936297487834,39.4445546869044,40.084993634277));
#196629=CARTESIAN_POINT('Ctrl Pts',(43.9378609783682,39.4438986117377,40.084312522952));
#196630=CARTESIAN_POINT('Ctrl Pts',(43.9394269075365,39.4432696802085,40.0836141747073));
#196631=CARTESIAN_POINT('Ctrl Pts',(43.9409940617759,39.4426678279629,40.0828999161609));
#196632=CARTESIAN_POINT('Ctrl Pts',(43.9413858503357,39.4425173649016,40.0827213515243));
#196633=CARTESIAN_POINT('Ctrl Pts',(43.9417777156948,39.4423685940343,40.0825417925841));
#196634=CARTESIAN_POINT('Ctrl Pts',(43.9421696393595,39.4422215138288,40.082361260236));
#196635=CARTESIAN_POINT('Ctrl Pts',(43.9433454103534,39.4417802732124,40.0818196631917));
#196636=CARTESIAN_POINT('Ctrl Pts',(43.9445217049433,39.4413542498599,40.0812693052021));
#196637=CARTESIAN_POINT('Ctrl Pts',(43.9456980341199,39.4409433907172,40.0807107531874));
#196638=CARTESIAN_POINT('Ctrl Pts',(43.953983944948,39.4380493519679,40.0767763849183));
#196639=CARTESIAN_POINT('Ctrl Pts',(43.962285917344,39.4358558447891,40.0724140586141));
#196640=CARTESIAN_POINT('Ctrl Pts',(43.9705207686456,39.4342768603232,40.0677221223774));
#196641=CARTESIAN_POINT('Ctrl Pts',(43.9745146626288,39.4335110545633,40.0654465383724));
#196642=CARTESIAN_POINT('Ctrl Pts',(43.97849322547,39.432890153227,40.0630928000681));
#196643=CARTESIAN_POINT('Ctrl Pts',(43.982449005934,39.4324063524311,40.0606689262479));
#196644=CARTESIAN_POINT('Ctrl Pts',(43.9885050294416,39.4316656872148,40.0569581447805));
#196645=CARTESIAN_POINT('Ctrl Pts',(43.9945041897575,39.4312456873364,40.0530843804605));
#196646=CARTESIAN_POINT('Ctrl Pts',(44.0004074287827,39.4311218425057,40.0490800251457));
#196647=CARTESIAN_POINT('Ctrl Pts',(44.0031489235253,39.4310643283256,40.0472203818218));
#196648=CARTESIAN_POINT('Ctrl Pts',(44.0058696426795,39.4310704471407,40.0453323608818));
#196649=CARTESIAN_POINT('Ctrl Pts',(44.0085654321305,39.4311389525606,40.0434201572162));
#196650=CARTESIAN_POINT('Ctrl Pts',(44.0087720537699,39.4311442032311,40.0432735943397));
#196651=CARTESIAN_POINT('Ctrl Pts',(44.0089785427603,39.4311497894108,40.0431268995707));
#196652=CARTESIAN_POINT('Ctrl Pts',(44.0091848981962,39.4311557099535,40.0429800745037));
#196653=CARTESIAN_POINT('Ctrl Pts',(44.0120835699302,39.4312388757294,40.0409176249753));
#196654=CARTESIAN_POINT('Ctrl Pts',(44.0149559644988,39.4313901062469,40.0388310783332));
#196655=CARTESIAN_POINT('Ctrl Pts',(44.0177981990788,39.4316052205101,40.036725739981));
#196656=CARTESIAN_POINT('Ctrl Pts',(44.0279899468071,39.4323765820008,40.0291763710725));
#196657=CARTESIAN_POINT('Ctrl Pts',(44.0378728316076,39.4339733733557,40.021331089461));
#196658=CARTESIAN_POINT('Ctrl Pts',(44.0474262866297,39.4362681192138,40.0132837551344));
#196659=CARTESIAN_POINT('Ctrl Pts',(44.057924573969,39.4387898143842,40.0044405431362));
#196660=CARTESIAN_POINT('Ctrl Pts',(44.0680257165045,39.4421543412245,39.9953528710651));
#196661=CARTESIAN_POINT('Ctrl Pts',(44.0777053474358,39.4462454222028,39.9861103629619));
#196662=CARTESIAN_POINT('Ctrl Pts',(44.088156919585,39.4506627629378,39.9761307737641));
#196663=CARTESIAN_POINT('Ctrl Pts',(44.0981181930469,39.4559274600877,39.9659696936119));
#196664=CARTESIAN_POINT('Ctrl Pts',(44.1075472421415,39.461949460792,39.9557128217636));
#196665=CARTESIAN_POINT('Ctrl Pts',(44.1168971912083,39.4679209431018,39.9455419945248));
#196666=CARTESIAN_POINT('Ctrl Pts',(44.1257248429258,39.4746380711531,39.9352756289384));
#196667=CARTESIAN_POINT('Ctrl Pts',(44.1339623850452,39.4820551873925,39.92499));
#196668=CARTESIAN_POINT('Origin',(-0.0101975504409074,0.0113255271402718,
39.92499));
#196669=CARTESIAN_POINT('Ctrl Pts',(46.6938111422609,42.0638038389695,40.10025));
#196670=CARTESIAN_POINT('Ctrl Pts',(46.6880613546461,42.07018425683,40.10025));
#196671=CARTESIAN_POINT('Ctrl Pts',(46.6818296739378,42.0760276657218,40.0995859581842));
#196672=CARTESIAN_POINT('Ctrl Pts',(46.6752630175681,42.0812997491639,40.0983275959621));
#196673=CARTESIAN_POINT('Ctrl Pts',(46.6710672367553,42.0846683595044,40.0975235624068));
#196674=CARTESIAN_POINT('Ctrl Pts',(46.6667352666015,42.0878044626432,40.096477705949));
#196675=CARTESIAN_POINT('Ctrl Pts',(46.6623093164294,42.0907067742411,40.0952149915961));
#196676=CARTESIAN_POINT('Ctrl Pts',(46.6562687825189,42.0946678472186,40.0934916398701));
#196677=CARTESIAN_POINT('Ctrl Pts',(46.6500510792886,42.098187735286,40.0913643921631));
#196678=CARTESIAN_POINT('Ctrl Pts',(46.6437515300393,42.101258394226,40.0889118607713));
#196679=CARTESIAN_POINT('Ctrl Pts',(46.6406017554146,42.1027937236961,40.0876855950755));
#196680=CARTESIAN_POINT('Ctrl Pts',(46.6374313809743,42.1042169023584,40.0863782327527));
#196681=CARTESIAN_POINT('Ctrl Pts',(46.6342513293852,42.1055280393685,40.0850006373334));
#196682=CARTESIAN_POINT('Ctrl Pts',(46.6326613035906,42.1061836078735,40.0843118396238));
#196683=CARTESIAN_POINT('Ctrl Pts',(46.6310688468945,42.1068111789402,40.0836054919165));
#196684=CARTESIAN_POINT('Ctrl Pts',(46.6294752517399,42.1074108478349,40.0828829920418));
#196685=CARTESIAN_POINT('Ctrl Pts',(46.6290768529512,42.1075607650586,40.0827023670731));
#196686=CARTESIAN_POINT('Ctrl Pts',(46.6286783827623,42.1077089386736,40.0825207326933));
#196687=CARTESIAN_POINT('Ctrl Pts',(46.6282798608704,42.1078553707278,40.0823381109276));
#196688=CARTESIAN_POINT('Ctrl Pts',(46.6270842951947,42.1082946668902,40.0817902456304));
#196689=CARTESIAN_POINT('Ctrl Pts',(46.6258882654176,42.108718287616,40.0812334935553));
#196690=CARTESIAN_POINT('Ctrl Pts',(46.6246922924071,42.1091263005955,40.0806684524227));
#196691=CARTESIAN_POINT('Ctrl Pts',(46.616427376857,42.1119459234381,40.0767636676137));
#196692=CARTESIAN_POINT('Ctrl Pts',(46.608149216569,42.1140735600934,40.0724404510889));
#196693=CARTESIAN_POINT('Ctrl Pts',(46.599938443282,42.1155964444644,40.067794993741));
#196694=CARTESIAN_POINT('Ctrl Pts',(46.5958577114965,42.1163533138166,40.0654862141906));
#196695=CARTESIAN_POINT('Ctrl Pts',(46.5917931497418,42.1169604217528,40.0630972003216));
#196696=CARTESIAN_POINT('Ctrl Pts',(46.5877524553609,42.1174262136787,40.0606363359906));
#196697=CARTESIAN_POINT('Ctrl Pts',(46.5788380800233,42.1184538202395,40.0552073017124));
#196698=CARTESIAN_POINT('Ctrl Pts',(46.5700422469563,42.1188058546733,40.0494204304519));
#196699=CARTESIAN_POINT('Ctrl Pts',(46.5615008914348,42.1185337834648,40.0434049749851));
#196700=CARTESIAN_POINT('Ctrl Pts',(46.5583806265506,42.1184343924214,40.0412074532442));
#196701=CARTESIAN_POINT('Ctrl Pts',(46.5552908961832,42.1182588963858,40.0389814735788));
#196702=CARTESIAN_POINT('Ctrl Pts',(46.5522345526332,42.1180117795237,40.0367321210016));
#196703=CARTESIAN_POINT('Ctrl Pts',(46.5419686180606,42.117181740133,40.0291767837139));
#196704=CARTESIAN_POINT('Ctrl Pts',(46.5320149571606,42.1155299964529,40.0213235332572));
#196705=CARTESIAN_POINT('Ctrl Pts',(46.5223946380443,42.1131831104082,40.0132649215852));
#196706=CARTESIAN_POINT('Ctrl Pts',(46.5118207677339,42.1106036046381,40.0044075527524));
#196707=CARTESIAN_POINT('Ctrl Pts',(46.5016489045623,42.107184320973,39.9953016253708));
#196708=CARTESIAN_POINT('Ctrl Pts',(46.4919044745653,42.1030402839728,39.9860353422344));
#196709=CARTESIAN_POINT('Ctrl Pts',(46.4814093059429,42.0985769785657,39.9760551582678));
#196710=CARTESIAN_POINT('Ctrl Pts',(46.4714088200582,42.0932726122933,39.9658879738136));
#196711=CARTESIAN_POINT('Ctrl Pts',(46.4619468343622,42.0872150940869,39.9556174643231));
#196712=CARTESIAN_POINT('Ctrl Pts',(46.4526126174212,42.0812393728293,39.9454856413889));
#196713=CARTESIAN_POINT('Ctrl Pts',(46.4438014421035,42.0745296860248,39.9352519465105));
#196714=CARTESIAN_POINT('Ctrl Pts',(46.4355828792675,42.067129658809,39.92499));
#196715=CARTESIAN_POINT('Ctrl Pts',(43.8790236240225,39.7651933658994,39.92499));
#196716=CARTESIAN_POINT('Ctrl Pts',(43.8711584142728,39.7581114992315,39.9348107241718));
#196717=CARTESIAN_POINT('Ctrl Pts',(43.8638800583581,39.7504347382259,39.9446038383161));
#196718=CARTESIAN_POINT('Ctrl Pts',(43.857221832855,39.7422106539921,39.9543158069372));
#196719=CARTESIAN_POINT('Ctrl Pts',(43.8507927303151,39.7342695770775,39.9636935671376));
#196720=CARTESIAN_POINT('Ctrl Pts',(43.8449410790361,39.7258171668717,39.972996832097));
#196721=CARTESIAN_POINT('Ctrl Pts',(43.8397310304473,39.7168657021576,39.9821731151314));
#196722=CARTESIAN_POINT('Ctrl Pts',(43.8348059028446,39.7084037645775,39.990847576433));
#196723=CARTESIAN_POINT('Ctrl Pts',(43.8304536682228,39.6994950821822,39.9994093733823));
#196724=CARTESIAN_POINT('Ctrl Pts',(43.8267676847832,39.6901349804769,40.0077966115818));
#196725=CARTESIAN_POINT('Ctrl Pts',(43.8233729558724,39.6815144838336,40.0155211172571));
#196726=CARTESIAN_POINT('Ctrl Pts',(43.8205432023716,39.6725105620462,40.0230979940998));
#196727=CARTESIAN_POINT('Ctrl Pts',(43.8183892419697,39.6631152739669,40.0304554104725));
#196728=CARTESIAN_POINT('Ctrl Pts',(43.8177469744581,39.6603137887169,40.0326492435165));
#196729=CARTESIAN_POINT('Ctrl Pts',(43.8171650742235,39.6574775031728,40.0348233715053));
#196730=CARTESIAN_POINT('Ctrl Pts',(43.8166472411075,39.6546062260516,40.0369753512355));
#196731=CARTESIAN_POINT('Ctrl Pts',(43.81613469897,39.6517642863081,40.0391053430352));
#196732=CARTESIAN_POINT('Ctrl Pts',(43.8156851836086,39.6488910639685,40.041211089324));
#196733=CARTESIAN_POINT('Ctrl Pts',(43.8153025584996,39.6459896850499,40.0432881154904));
#196734=CARTESIAN_POINT('Ctrl Pts',(43.8152759514979,39.6457879288341,40.043432547828));
#196735=CARTESIAN_POINT('Ctrl Pts',(43.815249656674,39.6455860324532,40.0435768364421));
#196736=CARTESIAN_POINT('Ctrl Pts',(43.815223675331,39.6453839959661,40.0437209807855));
#196737=CARTESIAN_POINT('Ctrl Pts',(43.8140845580787,39.6365259762551,40.050040796842));
#196738=CARTESIAN_POINT('Ctrl Pts',(43.8135929685794,39.6274037177898,40.0560490279344));
#196739=CARTESIAN_POINT('Ctrl Pts',(43.8138323099903,39.618098099237,40.0616647108614));
#196740=CARTESIAN_POINT('Ctrl Pts',(43.8140554177825,39.6094236454401,40.0668995033485));
#196741=CARTESIAN_POINT('Ctrl Pts',(43.8149139527621,39.6005890951397,40.0717933267481));
#196742=CARTESIAN_POINT('Ctrl Pts',(43.8164991115148,39.5916773623189,40.0762460303072));
#196743=CARTESIAN_POINT('Ctrl Pts',(43.817078983094,39.5884173351599,40.0778748868748));
#196744=CARTESIAN_POINT('Ctrl Pts',(43.817756312147,39.5851472105413,40.0794443522247));
#196745=CARTESIAN_POINT('Ctrl Pts',(43.8185363400632,39.581871986544,40.0809482021491));
#196746=CARTESIAN_POINT('Ctrl Pts',(43.8187239107186,39.5810844045881,40.0813098278168));
#196747=CARTESIAN_POINT('Ctrl Pts',(43.8189178575375,39.5802961412316,40.0816679525672));
#196748=CARTESIAN_POINT('Ctrl Pts',(43.8191182115055,39.5795073285703,40.082022419258));
#196749=CARTESIAN_POINT('Ctrl Pts',(43.819312304412,39.5787431663046,40.0823658088648));
#196750=CARTESIAN_POINT('Ctrl Pts',(43.8195124102603,39.5779784885475,40.0827057654616));
#196751=CARTESIAN_POINT('Ctrl Pts',(43.8197185546683,39.577213418196,40.0830421470151));
#196752=CARTESIAN_POINT('Ctrl Pts',(43.8219771048936,39.5688311883225,40.0867275956807));
#196753=CARTESIAN_POINT('Ctrl Pts',(43.824962384016,39.5603964284863,40.0899823432032));
#196754=CARTESIAN_POINT('Ctrl Pts',(43.8286919494561,39.5520968239707,40.0926299529357));
#196755=CARTESIAN_POINT('Ctrl Pts',(43.8302387114104,39.5486547305936,40.0937279956085));
#196756=CARTESIAN_POINT('Ctrl Pts',(43.8319130705232,39.5452359574122,40.0947220371803));
#196757=CARTESIAN_POINT('Ctrl Pts',(43.8337144555755,39.5418537500311,40.0956014538692));
#196758=CARTESIAN_POINT('Ctrl Pts',(43.8367869054999,39.5360850428914,40.097101390674));
#196759=CARTESIAN_POINT('Ctrl Pts',(43.8402296473868,39.5304250803195,40.0982667904316));
#196760=CARTESIAN_POINT('Ctrl Pts',(43.8440378929946,39.52494648469,40.0990539325582));
#196761=CARTESIAN_POINT('Ctrl Pts',(43.8459420157984,39.5222071868753,40.0994475036216));
#196762=CARTESIAN_POINT('Ctrl Pts',(43.8479386338072,39.5195141476131,40.0997467259952));
#196763=CARTESIAN_POINT('Ctrl Pts',(43.8500271570785,39.5168765098746,40.0999473488896));
#196764=CARTESIAN_POINT('Ctrl Pts',(43.8521156803499,39.5142388721361,40.100147971784));
#196765=CARTESIAN_POINT('Ctrl Pts',(43.8542960677578,39.5116566557593,40.10025));
#196766=CARTESIAN_POINT('Ctrl Pts',(43.8565665267061,39.5091373124617,40.10025));
#196767=CARTESIAN_POINT('Origin',(47.1453396605412,34.2342565846631,39.92499));
#196768=CARTESIAN_POINT('Ctrl Pts',(50.8023624960595,36.6746059268172,39.92499));
#196769=CARTESIAN_POINT('Ctrl Pts',(50.8109464329608,36.6808425220337,39.9348354642024));
#196770=CARTESIAN_POINT('Ctrl Pts',(50.8190128116699,36.6877379133671,39.944644082847));
#196771=CARTESIAN_POINT('Ctrl Pts',(50.8265243508974,36.6952462569251,39.9543641760349));
#196772=CARTESIAN_POINT('Ctrl Pts',(50.8337918098282,36.7025106240267,39.9637684240734));
#196773=CARTESIAN_POINT('Ctrl Pts',(50.8405407635302,36.7103497152267,39.9730909636422));
#196774=CARTESIAN_POINT('Ctrl Pts',(50.8467071440096,36.7187568768241,39.9822808977171));
#196775=CARTESIAN_POINT('Ctrl Pts',(50.8525401602392,36.726709534012,39.9909740094683));
#196776=CARTESIAN_POINT('Ctrl Pts',(50.8578524412773,36.7351712462859,39.9995492765038));
#196777=CARTESIAN_POINT('Ctrl Pts',(50.8625525281361,36.7441560526567,40.0079462328735));
#196778=CARTESIAN_POINT('Ctrl Pts',(50.866881648052,36.7524317091221,40.0156804369733));
#196779=CARTESIAN_POINT('Ctrl Pts',(50.8706916079218,36.7611516658517,40.0232638017468));
#196780=CARTESIAN_POINT('Ctrl Pts',(50.8738736606229,36.7703354510224,40.0306257270015));
#196781=CARTESIAN_POINT('Ctrl Pts',(50.8747966531518,36.7729993179964,40.0327611416684));
#196782=CARTESIAN_POINT('Ctrl Pts',(50.8756665488992,36.7757022424592,40.0348777427287));
#196783=CARTESIAN_POINT('Ctrl Pts',(50.8764799968257,36.7784447603813,40.03697331687));
#196784=CARTESIAN_POINT('Ctrl Pts',(50.8773618266786,36.7814178261388,40.039245053974));
#196785=CARTESIAN_POINT('Ctrl Pts',(50.8781771258728,36.7844329791242,40.041487875195));
#196786=CARTESIAN_POINT('Ctrl Pts',(50.8789219044958,36.7874899206169,40.0436985701601));
#196787=CARTESIAN_POINT('Ctrl Pts',(50.8809659552707,36.7958797205311,40.0497658398386));
#196788=CARTESIAN_POINT('Ctrl Pts',(50.8824343655147,36.8045837617098,40.0555581699984));
#196789=CARTESIAN_POINT('Ctrl Pts',(50.8832604021666,36.8135226609472,40.0609828468886));
#196790=CARTESIAN_POINT('Ctrl Pts',(50.8840161808564,36.8217012684452,40.0659461317304));
#196791=CARTESIAN_POINT('Ctrl Pts',(50.8842246658559,36.8300699399849,40.0706039980705));
#196792=CARTESIAN_POINT('Ctrl Pts',(50.8838072802932,36.8385876480138,40.0748843180601));
#196793=CARTESIAN_POINT('Ctrl Pts',(50.8836022618683,36.8427715183736,40.0769867972569));
#196794=CARTESIAN_POINT('Ctrl Pts',(50.8832457706974,36.8469911418441,40.0789976708175));
#196795=CARTESIAN_POINT('Ctrl Pts',(50.8827256259729,36.8512399286211,40.0809050491501));
#196796=CARTESIAN_POINT('Ctrl Pts',(50.8826269335777,36.8520460945283,40.0812669556106));
#196797=CARTESIAN_POINT('Ctrl Pts',(50.8825219362263,36.8528536453859,40.0816253922033));
#196798=CARTESIAN_POINT('Ctrl Pts',(50.8824105850811,36.8536624499707,40.081980198914));
#196799=CARTESIAN_POINT('Ctrl Pts',(50.8823027136591,36.8544459794122,40.082323917915));
#196800=CARTESIAN_POINT('Ctrl Pts',(50.8821888793662,36.8552306854272,40.0826642303499));
#196801=CARTESIAN_POINT('Ctrl Pts',(50.8820690400779,36.856016445618,40.08300099161));
#196802=CARTESIAN_POINT('Ctrl Pts',(50.8807630562085,36.8645794982668,40.0866709464312));
#196803=CARTESIAN_POINT('Ctrl Pts',(50.8787426510003,36.8732733195862,40.0899175831876));
#196804=CARTESIAN_POINT('Ctrl Pts',(50.8759664620674,36.8819119966094,40.092564206706));
#196805=CARTESIAN_POINT('Ctrl Pts',(50.8747940602417,36.8855601635604,40.0936818922527));
#196806=CARTESIAN_POINT('Ctrl Pts',(50.8734872887382,36.889198371364,40.094693009479));
#196807=CARTESIAN_POINT('Ctrl Pts',(50.8720449698708,36.8928125648611,40.0955863397546));
#196808=CARTESIAN_POINT('Ctrl Pts',(50.8696161409378,36.898898776401,40.0970906856167));
#196809=CARTESIAN_POINT('Ctrl Pts',(50.8668019052541,36.9049145742142,40.0982599215483));
#196810=CARTESIAN_POINT('Ctrl Pts',(50.863597962796,36.9107858666116,40.0990497370454));
#196811=CARTESIAN_POINT('Ctrl Pts',(50.8627969771814,36.912253689711,40.0992471909196));
#196812=CARTESIAN_POINT('Ctrl Pts',(50.8619714372928,36.913712355938,40.0994209989363));
#196813=CARTESIAN_POINT('Ctrl Pts',(50.8611210221667,36.9151605322318,40.0995705982975));
#196814=CARTESIAN_POINT('Ctrl Pts',(50.8598453994776,36.9173327966726,40.0997949973393));
#196815=CARTESIAN_POINT('Ctrl Pts',(50.8585138058065,36.9194814382213,40.0999649129781));
#196816=CARTESIAN_POINT('Ctrl Pts',(50.8571265262615,36.9216029292227,40.1000786629733));
#196817=CARTESIAN_POINT('Ctrl Pts',(50.8557392467166,36.923724420224,40.1001924129685));
#196818=CARTESIAN_POINT('Ctrl Pts',(50.8542962928989,36.9258187603134,40.10025));
#196819=CARTESIAN_POINT('Ctrl Pts',(50.8527980281403,36.9278827595331,40.10025));
#196820=CARTESIAN_POINT('Ctrl Pts',(47.7640607692767,34.683783783134,40.10025));
#196821=CARTESIAN_POINT('Ctrl Pts',(47.7691302463545,34.6767997090224,40.10025));
#196822=CARTESIAN_POINT('Ctrl Pts',(47.7747322888384,34.6702946353241,40.0995786334241));
#196823=CARTESIAN_POINT('Ctrl Pts',(47.7807252357994,34.6643211616153,40.0983063763366));
#196824=CARTESIAN_POINT('Ctrl Pts',(47.7845960646242,34.6604629105133,40.0974846287992));
#196825=CARTESIAN_POINT('Ctrl Pts',(47.7886293194339,34.6568257642789,40.0964130309338));
#196826=CARTESIAN_POINT('Ctrl Pts',(47.7927819897612,34.6534164822759,40.0951176960924));
#196827=CARTESIAN_POINT('Ctrl Pts',(47.7982861164005,34.6488976742765,40.0934008039614));
#196828=CARTESIAN_POINT('Ctrl Pts',(47.8040027249066,34.644784311377,40.0912909372157));
#196829=CARTESIAN_POINT('Ctrl Pts',(47.8098436832081,34.6410949611628,40.0888630467852));
#196830=CARTESIAN_POINT('Ctrl Pts',(47.8127641623589,34.6392502860557,40.0876491015699));
#196831=CARTESIAN_POINT('Ctrl Pts',(47.815715844683,34.6375114518661,40.0863558569271));
#196832=CARTESIAN_POINT('Ctrl Pts',(47.8186885387641,34.6358796311039,40.0849936342771));
#196833=CARTESIAN_POINT('Ctrl Pts',(47.8201748858046,34.6350637207227,40.0843125229521));
#196834=CARTESIAN_POINT('Ctrl Pts',(47.8216664954028,34.6342745503767,40.0836141747074));
#196835=CARTESIAN_POINT('Ctrl Pts',(47.8231621539169,34.6335121829164,40.082899916161));
#196836=CARTESIAN_POINT('Ctrl Pts',(47.8235360685455,34.6333215910513,40.0827213515243));
#196837=CARTESIAN_POINT('Ctrl Pts',(47.823910236435,34.6331326740826,40.0825417925842));
#196838=CARTESIAN_POINT('Ctrl Pts',(47.824284639033,34.6329454324195,40.0823612602361));
#196839=CARTESIAN_POINT('Ctrl Pts',(47.8254078468268,34.6323837074302,40.0818196631917));
#196840=CARTESIAN_POINT('Ctrl Pts',(47.8265331659854,34.6318370616124,40.0812693052022));
#196841=CARTESIAN_POINT('Ctrl Pts',(47.827660104633,34.631305493318,40.0807107531875));
#196842=CARTESIAN_POINT('Ctrl Pts',(47.8355981149521,34.6275611948897,40.076776384918));
#196843=CARTESIAN_POINT('Ctrl Pts',(47.8436253243409,34.6245119115559,40.0724140586133));
#196844=CARTESIAN_POINT('Ctrl Pts',(47.8516500154464,34.6220808005802,40.0677221223762));
#196845=CARTESIAN_POINT('Ctrl Pts',(47.8555419819605,34.6209017143842,40.0654465383716));
#196846=CARTESIAN_POINT('Ctrl Pts',(47.8594338479549,34.6198683413508,40.0630928000677));
#196847=CARTESIAN_POINT('Ctrl Pts',(47.8633173872852,34.6189736992135,40.0606689262479));
#196848=CARTESIAN_POINT('Ctrl Pts',(47.8692628146655,34.617604064608,40.0569581447805));
#196849=CARTESIAN_POINT('Ctrl Pts',(47.8751852090117,34.6165592825241,40.0530843804606));
#196850=CARTESIAN_POINT('Ctrl Pts',(47.881043164166,34.6158190596248,40.0490800251458));
#196851=CARTESIAN_POINT('Ctrl Pts',(47.8837636288446,34.6154752962809,40.0472203818218));
#196852=CARTESIAN_POINT('Ctrl Pts',(47.886470083205,34.6151969889843,40.0453323608818));
#196853=CARTESIAN_POINT('Ctrl Pts',(47.8891582656055,34.6149833323957,40.0434201572162));
#196854=CARTESIAN_POINT('Ctrl Pts',(47.8893643041946,34.61496695646,40.0432735943397));
#196855=CARTESIAN_POINT('Ctrl Pts',(47.8895702459314,34.6149509280612,40.0431268995707));
#196856=CARTESIAN_POINT('Ctrl Pts',(47.8897760897959,34.614935246154,40.0429800745037));
#196857=CARTESIAN_POINT('Ctrl Pts',(47.8926675754936,34.6147149626372,40.0409176249753));
#196858=CARTESIAN_POINT('Ctrl Pts',(47.8955400426778,34.614565117708,40.0388310783332));
#196859=CARTESIAN_POINT('Ctrl Pts',(47.8983891927627,34.6144819591398,40.036725739981));
#196860=CARTESIAN_POINT('Ctrl Pts',(47.9086057382628,34.6141837673035,40.0291763710718));
#196861=CARTESIAN_POINT('Ctrl Pts',(47.9186013937337,34.6147387685075,40.0213310894596));
#196862=CARTESIAN_POINT('Ctrl Pts',(47.9283423801886,34.6160223355356,40.0132837551323));
#196863=CARTESIAN_POINT('Ctrl Pts',(47.9390467457337,34.6174328467537,40.0044405431329));
#196864=CARTESIAN_POINT('Ctrl Pts',(47.9494442419749,34.619723085458,39.9953528710606));
#196865=CARTESIAN_POINT('Ctrl Pts',(47.959498481284,34.6227799581211,39.9861103629562));
#196866=CARTESIAN_POINT('Ctrl Pts',(47.9703545364683,34.6260806134269,39.9761307737563));
#196867=CARTESIAN_POINT('Ctrl Pts',(47.9808115517364,34.6302752334091,39.965969693602));
#196868=CARTESIAN_POINT('Ctrl Pts',(47.9908184179945,34.6352786409532,39.9557128217515));
#196869=CARTESIAN_POINT('Ctrl Pts',(48.000741336927,34.6402400750492,39.9455419945166));
#196870=CARTESIAN_POINT('Ctrl Pts',(48.0102227609135,34.6459976651,39.9352756289343));
#196871=CARTESIAN_POINT('Ctrl Pts',(48.019190476674,34.6525130919791,39.92499));
#196872=CARTESIAN_POINT('Origin',(-0.00895784724493606,0.012329418994271,
39.92499));
#196873=CARTESIAN_POINT('Ctrl Pts',(50.8348823336491,36.9525415975206,40.10025));
#196874=CARTESIAN_POINT('Ctrl Pts',(50.829830979246,36.9594880792485,40.10025));
#196875=CARTESIAN_POINT('Ctrl Pts',(50.8242442388878,36.9659508653435,40.0995859581841));
#196876=CARTESIAN_POINT('Ctrl Pts',(50.8182646381287,36.9718804702604,40.0983275959618));
#196877=CARTESIAN_POINT('Ctrl Pts',(50.8144439579048,36.9756692055211,40.0975235624065));
#196878=CARTESIAN_POINT('Ctrl Pts',(50.810463530779,36.9792409429414,40.0964777059488));
#196879=CARTESIAN_POINT('Ctrl Pts',(50.8063652005968,36.9825899931423,40.095214991596));
#196880=CARTESIAN_POINT('Ctrl Pts',(50.8007718022343,36.9871607746745,40.09349163987));
#196881=CARTESIAN_POINT('Ctrl Pts',(50.7949560887235,36.9913113073904,40.091364392163));
#196882=CARTESIAN_POINT('Ctrl Pts',(50.7890120203243,36.9950236271418,40.0889118607712));
#196883=CARTESIAN_POINT('Ctrl Pts',(50.7860399861247,36.9968797870175,40.0876855950754));
#196884=CARTESIAN_POINT('Ctrl Pts',(50.7830357420058,36.9986265637265,40.0863782327526));
#196885=CARTESIAN_POINT('Ctrl Pts',(50.7800101622089,37.0002629240965,40.0850006373333));
#196886=CARTESIAN_POINT('Ctrl Pts',(50.7784973723104,37.0010811042815,40.0843118396237));
#196887=CARTESIAN_POINT('Ctrl Pts',(50.7769792382978,37.0018716944995,40.0836054919164));
#196888=CARTESIAN_POINT('Ctrl Pts',(50.7754570554923,37.0026346543979,40.0828829920417));
#196889=CARTESIAN_POINT('Ctrl Pts',(50.7750765097909,37.0028253943725,40.082702367073));
#196890=CARTESIAN_POINT('Ctrl Pts',(50.7746957108236,37.0030144077534,40.0825207326932));
#196891=CARTESIAN_POINT('Ctrl Pts',(50.7743146783939,37.0032016945184,40.0823381109275));
#196892=CARTESIAN_POINT('Ctrl Pts',(50.7731715811049,37.0037635548134,40.0817902456303));
#196893=CARTESIAN_POINT('Ctrl Pts',(50.7720263837275,37.004309874055,40.0812334935552));
#196894=CARTESIAN_POINT('Ctrl Pts',(50.770879611352,37.0048406651177,40.0806684524226));
#196895=CARTESIAN_POINT('Ctrl Pts',(50.7629547027171,37.0085087606927,40.0767636676138));
#196896=CARTESIAN_POINT('Ctrl Pts',(50.7549442896476,37.0114900453053,40.0724404510891));
#196897=CARTESIAN_POINT('Ctrl Pts',(50.746937680599,37.0138628466703,40.0677949937414));
#196898=CARTESIAN_POINT('Ctrl Pts',(50.7429584178792,37.0150421224356,40.0654862141909));
#196899=CARTESIAN_POINT('Ctrl Pts',(50.7389795822785,37.0160707669652,40.0630972003217));
#196900=CARTESIAN_POINT('Ctrl Pts',(50.7350097117581,37.0169563748084,40.0606363359906));
#196901=CARTESIAN_POINT('Ctrl Pts',(50.726251584436,37.018910157988,40.0552073017123));
#196902=CARTESIAN_POINT('Ctrl Pts',(50.7175407334812,37.020179678854,40.0494204304519));
#196903=CARTESIAN_POINT('Ctrl Pts',(50.7090177292136,37.0208019128469,40.0434049749851));
#196904=CARTESIAN_POINT('Ctrl Pts',(50.7059041682739,37.0210292227713,40.0412074532442));
#196905=CARTESIAN_POINT('Ctrl Pts',(50.7028130194418,37.0211776528886,40.0389814735788));
#196906=CARTESIAN_POINT('Ctrl Pts',(50.6997475881157,37.021251364653,40.0367321210017));
#196907=CARTESIAN_POINT('Ctrl Pts',(50.6894511286649,37.0214989546697,40.029176783714));
#196908=CARTESIAN_POINT('Ctrl Pts',(50.6793793407323,37.020896700292,40.0213235332574));
#196909=CARTESIAN_POINT('Ctrl Pts',(50.6695664063391,37.019568267908,40.0132649215856));
#196910=CARTESIAN_POINT('Ctrl Pts',(50.6587808290224,37.0181081633547,40.0044075527529));
#196911=CARTESIAN_POINT('Ctrl Pts',(50.6483072759147,37.0157708601093,39.9953016253715));
#196912=CARTESIAN_POINT('Ctrl Pts',(50.6381830571056,37.0126680948705,39.9860353422352));
#196913=CARTESIAN_POINT('Ctrl Pts',(50.6272788396598,37.0093262837653,39.9760551582688));
#196914=CARTESIAN_POINT('Ctrl Pts',(50.6167786802283,37.0050963107879,39.9658879738147));
#196915=CARTESIAN_POINT('Ctrl Pts',(50.6067353452107,37.0000610231245,39.9556174643244));
#196916=CARTESIAN_POINT('Ctrl Pts',(50.5968276291265,36.9950937288458,39.9454856413898));
#196917=CARTESIAN_POINT('Ctrl Pts',(50.5873633690981,36.9893418170231,39.935251946511));
#196918=CARTESIAN_POINT('Ctrl Pts',(50.5784163149361,36.982841401674,39.92499));
#196919=CARTESIAN_POINT('Ctrl Pts',(47.7952442955506,34.960748566836,39.92499));
#196920=CARTESIAN_POINT('Ctrl Pts',(47.786681915603,34.9545276336631,39.9348107241719));
#196921=CARTESIAN_POINT('Ctrl Pts',(47.7786409912526,34.9476537221162,39.9446038383163));
#196922=CARTESIAN_POINT('Ctrl Pts',(47.7711595893187,34.9401706643562,39.9543158069375));
#196923=CARTESIAN_POINT('Ctrl Pts',(47.7639356375086,34.9329451137005,39.963693567138));
#196924=CARTESIAN_POINT('Ctrl Pts',(47.7572325247378,34.9251506707979,39.9729968320975));
#196925=CARTESIAN_POINT('Ctrl Pts',(47.7511153344897,34.9167928415166,39.9821731151319));
#196926=CARTESIAN_POINT('Ctrl Pts',(47.7453326739199,34.9088920753355,39.9908475764335));
#196927=CARTESIAN_POINT('Ctrl Pts',(47.7400730704142,34.9004871280313,39.9994093733829));
#196928=CARTESIAN_POINT('Ctrl Pts',(47.7354288821303,34.8915635921269,40.0077966115824));
#196929=CARTESIAN_POINT('Ctrl Pts',(47.7311516626329,34.8833451652624,40.0155211172578));
#196930=CARTESIAN_POINT('Ctrl Pts',(47.7273962447101,34.8746863576854,40.0230979941005));
#196931=CARTESIAN_POINT('Ctrl Pts',(47.7242720089038,34.865567688148,40.0304554104732));
#196932=CARTESIAN_POINT('Ctrl Pts',(47.7233404248529,34.8628486849635,40.032649243517));
#196933=CARTESIAN_POINT('Ctrl Pts',(47.7224652397594,34.860088762026,40.0348233715055));
#196934=CARTESIAN_POINT('Ctrl Pts',(47.7216501132023,34.8572873423615,40.0369753512355));
#196935=CARTESIAN_POINT('Ctrl Pts',(47.7208433152302,34.8545145463033,40.0391053430352));
#196936=CARTESIAN_POINT('Ctrl Pts',(47.7200959288452,34.8517040509262,40.041211089324));
#196937=CARTESIAN_POINT('Ctrl Pts',(47.7194121231169,34.8488585612795,40.0432881154904));
#196938=CARTESIAN_POINT('Ctrl Pts',(47.7193645726039,34.8486606914944,40.0434325478279));
#196939=CARTESIAN_POINT('Ctrl Pts',(47.7193173179074,34.8484626496805,40.0435768364421));
#196940=CARTESIAN_POINT('Ctrl Pts',(47.7192703603294,34.8482644357603,40.0437209807855));
#196941=CARTESIAN_POINT('Ctrl Pts',(47.7172115680926,34.8395740113841,40.0500407968419));
#196942=CARTESIAN_POINT('Ctrl Pts',(47.7157691359132,34.8305531107003,40.0560490279342));
#196943=CARTESIAN_POINT('Ctrl Pts',(47.7150344641797,34.8212734513099,40.0616647108611));
#196944=CARTESIAN_POINT('Ctrl Pts',(47.714349622439,34.8126231959642,40.0668995033481));
#196945=CARTESIAN_POINT('Ctrl Pts',(47.7142799923075,34.8037473009128,40.0717933267476));
#196946=CARTESIAN_POINT('Ctrl Pts',(47.7149249376578,34.7947186932888,40.0762460303065));
#196947=CARTESIAN_POINT('Ctrl Pts',(47.7151608670107,34.7914159118141,40.0778748868743));
#196948=CARTESIAN_POINT('Ctrl Pts',(47.7154926644833,34.7880929011149,40.0794443522245));
#196949=CARTESIAN_POINT('Ctrl Pts',(47.7159260651937,34.7847540840174,40.0809482021492));
#196950=CARTESIAN_POINT('Ctrl Pts',(47.7160302835859,34.7839512100456,40.0813098278168));
#196951=CARTESIAN_POINT('Ctrl Pts',(47.7161407719865,34.7831469919153,40.0816679525672));
#196952=CARTESIAN_POINT('Ctrl Pts',(47.7162575750192,34.7823415577599,40.082022419258));
#196953=CARTESIAN_POINT('Ctrl Pts',(47.716370727957,34.7815612934218,40.0823658088648));
#196954=CARTESIAN_POINT('Ctrl Pts',(47.7164898070138,34.7807798878926,40.0827057654616));
#196955=CARTESIAN_POINT('Ctrl Pts',(47.716614850513,34.7799974607183,40.0830421470151));
#196956=CARTESIAN_POINT('Ctrl Pts',(47.7179848465564,34.7714250667928,40.0867275956807));
#196957=CARTESIAN_POINT('Ctrl Pts',(47.7200720995238,34.7627244668144,40.0899823432033));
#196958=CARTESIAN_POINT('Ctrl Pts',(47.7229136891084,34.7540804826564,40.0926299529359));
#196959=CARTESIAN_POINT('Ctrl Pts',(47.7240921810077,34.7504955647771,40.0937279956086));
#196960=CARTESIAN_POINT('Ctrl Pts',(47.7254000086992,34.7469205018079,40.0947220371803));
#196961=CARTESIAN_POINT('Ctrl Pts',(47.7268379886356,34.7433685265016,40.0956014538692));
#196962=CARTESIAN_POINT('Ctrl Pts',(47.7292906132656,34.737310262474,40.097101390674));
#196963=CARTESIAN_POINT('Ctrl Pts',(47.7321228682624,34.7313214412505,40.0982667904316));
#196964=CARTESIAN_POINT('Ctrl Pts',(47.7353375827201,34.7254747878799,40.0990539325582));
#196965=CARTESIAN_POINT('Ctrl Pts',(47.7369449399489,34.7225514611946,40.0994475036216));
#196966=CARTESIAN_POINT('Ctrl Pts',(47.7386491210198,34.7196644712711,40.0997467259952));
#196967=CARTESIAN_POINT('Ctrl Pts',(47.7404504949227,34.7168229726601,40.0999473488896));
#196968=CARTESIAN_POINT('Ctrl Pts',(47.7422518688256,34.7139814740491,40.100147971784));
#196969=CARTESIAN_POINT('Ctrl Pts',(47.7441503967336,34.7111854907788,40.10025));
#196970=CARTESIAN_POINT('Ctrl Pts',(47.7461450747869,34.7084426211226,40.10025));
#196971=CARTESIAN_POINT('Origin',(50.4655267888879,29.1186878401549,39.92499));
#196972=CARTESIAN_POINT('Ctrl Pts',(54.3576020372442,31.1634057161433,39.92499));
#196973=CARTESIAN_POINT('Ctrl Pts',(54.3667908521541,31.1687108809051,39.9348354642012));
#196974=CARTESIAN_POINT('Ctrl Pts',(54.3755338070554,31.174725332392,39.9446440828447));
#196975=CARTESIAN_POINT('Ctrl Pts',(54.3837890328981,31.1814073748053,39.9543641760315));
#196976=CARTESIAN_POINT('Ctrl Pts',(54.3917760130576,31.1878722906292,39.9637684240692));
#196977=CARTESIAN_POINT('Ctrl Pts',(54.3993074034411,31.1949629807075,39.9730909636371));
#196978=CARTESIAN_POINT('Ctrl Pts',(54.4063187915247,31.2026795247176,39.9822808977112));
#196979=CARTESIAN_POINT('Ctrl Pts',(54.4129511329155,31.2099789001937,39.9909740094617));
#196980=CARTESIAN_POINT('Ctrl Pts',(54.4191188025025,31.2178389737479,39.9995492764965));
#196981=CARTESIAN_POINT('Ctrl Pts',(54.4247323097961,31.2262832675516,40.0079462328655));
#196982=CARTESIAN_POINT('Ctrl Pts',(54.4299027559928,31.2340610728517,40.0156804369646));
#196983=CARTESIAN_POINT('Ctrl Pts',(54.4346033281805,31.2423350114943,40.0232638017375));
#196984=CARTESIAN_POINT('Ctrl Pts',(54.4387279162148,31.2511358718486,40.0306257269917));
#196985=CARTESIAN_POINT('Ctrl Pts',(54.4399243024172,31.2536886668937,40.0327611416619));
#196986=CARTESIAN_POINT('Ctrl Pts',(54.4410719653269,31.2562858555917,40.0348777427254));
#196987=CARTESIAN_POINT('Ctrl Pts',(54.4421676282861,31.258928321256,40.03697331687));
#196988=CARTESIAN_POINT('Ctrl Pts',(54.4433553973776,31.2617929239288,40.039245053974));
#196989=CARTESIAN_POINT('Ctrl Pts',(54.4444813995856,31.2647063376188,40.041487875195));
#196990=CARTESIAN_POINT('Ctrl Pts',(54.4455416356299,31.2676686823013,40.04369857016));
#196991=CARTESIAN_POINT('Ctrl Pts',(54.448451461773,31.2757988605273,40.0497658398386));
#196992=CARTESIAN_POINT('Ctrl Pts',(54.4508216479607,31.2843017293915,40.0555581699984));
#196993=CARTESIAN_POINT('Ctrl Pts',(54.4525775288979,31.2931053160618,40.0609828468885));
#196994=CARTESIAN_POINT('Ctrl Pts',(54.4541840646265,31.3011601199075,40.0659461317306));
#196995=CARTESIAN_POINT('Ctrl Pts',(54.4552661718989,31.3094611543726,40.0706039980708));
#196996=CARTESIAN_POINT('Ctrl Pts',(54.4557414157489,31.3179758301775,40.0748843180606));
#196997=CARTESIAN_POINT('Ctrl Pts',(54.4559748539755,31.3221582111183,40.0769867972571));
#196998=CARTESIAN_POINT('Ctrl Pts',(54.4560613864574,31.3263919825238,40.0789976708176));
#196999=CARTESIAN_POINT('Ctrl Pts',(54.4559882102927,31.3306718639307,40.08090504915));
#197000=CARTESIAN_POINT('Ctrl Pts',(54.4559743258282,31.3314839297411,40.0812669556105));
#197001=CARTESIAN_POINT('Ctrl Pts',(54.4559543157134,31.3322980319624,40.0816253922032));
#197002=CARTESIAN_POINT('Ctrl Pts',(54.4559281176618,31.3331140451952,40.0819801989139));
#197003=CARTESIAN_POINT('Ctrl Pts',(54.4559027382992,31.3339045580144,40.0823239179149));
#197004=CARTESIAN_POINT('Ctrl Pts',(54.4558715517163,31.3346968642514,40.0826642303498));
#197005=CARTESIAN_POINT('Ctrl Pts',(54.4558345032254,31.3354908465822,40.0830009916099));
#197006=CARTESIAN_POINT('Ctrl Pts',(54.4554307564065,31.34414350242,40.0866709464312));
#197007=CARTESIAN_POINT('Ctrl Pts',(54.4543301709718,31.3530008879285,40.0899175831878));
#197008=CARTESIAN_POINT('Ctrl Pts',(54.4524721779262,31.3618824321384,40.0925642067062));
#197009=CARTESIAN_POINT('Ctrl Pts',(54.4516875359255,31.3656331634099,40.0936818922528));
#197010=CARTESIAN_POINT('Ctrl Pts',(54.4507682193239,31.3693880355472,40.0946930094791));
#197011=CARTESIAN_POINT('Ctrl Pts',(54.4497115877225,31.3731331934886,40.0955863397546));
#197012=CARTESIAN_POINT('Ctrl Pts',(54.4479322465079,31.3794399458808,40.0970906856166));
#197013=CARTESIAN_POINT('Ctrl Pts',(54.4457622496024,31.3857169562553,40.0982599215483));
#197014=CARTESIAN_POINT('Ctrl Pts',(54.4431895758475,31.39189098828,40.0990497370453));
#197015=CARTESIAN_POINT('Ctrl Pts',(54.4425464074088,31.3934344962862,40.0992471909196));
#197016=CARTESIAN_POINT('Ctrl Pts',(54.4418778620531,31.3949714642028,40.0994209989363));
#197017=CARTESIAN_POINT('Ctrl Pts',(54.4411834812327,31.3965005998217,40.0995705982975));
#197018=CARTESIAN_POINT('Ctrl Pts',(54.4401419100021,31.39879430325,40.0997949973393));
#197019=CARTESIAN_POINT('Ctrl Pts',(54.4390422051397,31.4010703637557,40.0999649129781));
#197020=CARTESIAN_POINT('Ctrl Pts',(54.4378842814515,31.4033252432064,40.1000786629733));
#197021=CARTESIAN_POINT('Ctrl Pts',(54.4367263577634,31.4055801226571,40.1001924129685));
#197022=CARTESIAN_POINT('Ctrl Pts',(54.435510226749,31.4078138194776,40.10025));
#197023=CARTESIAN_POINT('Ctrl Pts',(54.4342359163082,31.4100231232063,40.10025));
#197024=CARTESIAN_POINT('Ctrl Pts',(51.1278468659051,29.5010785149105,40.10025));
#197025=CARTESIAN_POINT('Ctrl Pts',(51.1321585373228,29.493602795639,40.10025));
#197026=CARTESIAN_POINT('Ctrl Pts',(51.1370499258748,29.486547784523,40.099578633424));
#197027=CARTESIAN_POINT('Ctrl Pts',(51.1423856448182,29.4799806005918,40.0983063763365));
#197028=CARTESIAN_POINT('Ctrl Pts',(51.145831971779,29.4757388736045,40.0974846287991));
#197029=CARTESIAN_POINT('Ctrl Pts',(51.1494629466902,29.4717000621106,40.0964130309337));
#197030=CARTESIAN_POINT('Ctrl Pts',(51.1532365012463,29.4678753842634,40.0951176960923));
#197031=CARTESIAN_POINT('Ctrl Pts',(51.158238131648,29.4628059928677,40.0934008039614));
#197032=CARTESIAN_POINT('Ctrl Pts',(51.1634934604718,29.4581176150984,40.0912909372156));
#197033=CARTESIAN_POINT('Ctrl Pts',(51.1689167792842,29.4538379291355,40.0888630467851));
#197034=CARTESIAN_POINT('Ctrl Pts',(51.1716284386905,29.451698086154,40.0876491015699));
#197035=CARTESIAN_POINT('Ctrl Pts',(51.1743821937243,29.4496602426627,40.0863558569271));
#197036=CARTESIAN_POINT('Ctrl Pts',(51.1771680313595,29.4477266300412,40.0849936342771));
#197037=CARTESIAN_POINT('Ctrl Pts',(51.1785609501771,29.4467598237305,40.0843125229521));
#197038=CARTESIAN_POINT('Ctrl Pts',(51.1799618978183,29.4458190608831,40.0836141747074));
#197039=CARTESIAN_POINT('Ctrl Pts',(51.1813696738596,29.4449045308654,40.0828999161609));
#197040=CARTESIAN_POINT('Ctrl Pts',(51.1817216178699,29.444675898361,40.0827213515243));
#197041=CARTESIAN_POINT('Ctrl Pts',(51.1820739888281,29.4444489051048,40.0825417925841));
#197042=CARTESIAN_POINT('Ctrl Pts',(51.1824267683262,29.4442235534429,40.082361260236));
#197043=CARTESIAN_POINT('Ctrl Pts',(51.1834851068203,29.4435474984572,40.0818196631917));
#197044=CARTESIAN_POINT('Ctrl Pts',(51.1845471213155,29.44288621934,40.0812693052021));
#197045=CARTESIAN_POINT('Ctrl Pts',(51.1856123224583,29.4422397658673,40.0807107531874));
#197046=CARTESIAN_POINT('Ctrl Pts',(51.1931154617654,29.4376862310777,40.0767763849181));
#197047=CARTESIAN_POINT('Ctrl Pts',(51.20077996036,29.4338145801754,40.0724140586136));
#197048=CARTESIAN_POINT('Ctrl Pts',(51.2085065710735,29.4305579784506,40.0677221223766));
#197049=CARTESIAN_POINT('Ctrl Pts',(51.2122539689199,29.4289785301332,40.0654465383719));
#197050=CARTESIAN_POINT('Ctrl Pts',(51.2160164979702,29.4275440072536,40.0630928000678));
#197051=CARTESIAN_POINT('Ctrl Pts',(51.2197852472982,29.4262483256613,40.0606689262479));
#197052=CARTESIAN_POINT('Ctrl Pts',(51.2255549392047,29.4242647276699,40.0569581447805));
#197053=CARTESIAN_POINT('Ctrl Pts',(51.2313356805893,29.4226066102317,40.0530843804605));
#197054=CARTESIAN_POINT('Ctrl Pts',(51.2370841708902,29.4212581193007,40.0490800251457));
#197055=CARTESIAN_POINT('Ctrl Pts',(51.2397537995247,29.4206318731362,40.0472203818218));
#197056=CARTESIAN_POINT('Ctrl Pts',(51.2424163366108,29.4200721889209,40.0453323608818));
#197057=CARTESIAN_POINT('Ctrl Pts',(51.245067459672,29.4195787111901,40.0434201572162));
#197058=CARTESIAN_POINT('Ctrl Pts',(51.2452706578087,29.4195408880665,40.0432735943397));
#197059=CARTESIAN_POINT('Ctrl Pts',(51.2454737959512,29.4195034206996,40.0431268995707));
#197060=CARTESIAN_POINT('Ctrl Pts',(51.2456768729759,29.4194663081567,40.0429800745037));
#197061=CARTESIAN_POINT('Ctrl Pts',(51.2485294929149,29.4189449888195,40.0409176249753));
#197062=CARTESIAN_POINT('Ctrl Pts',(51.2513705613631,29.4184957101759,40.0388310783332));
#197063=CARTESIAN_POINT('Ctrl Pts',(51.2541954110684,29.4181151898791,40.036725739981));
#197064=CARTESIAN_POINT('Ctrl Pts',(51.2643248197289,29.4167507117679,40.0291763710718));
#197065=CARTESIAN_POINT('Ctrl Pts',(51.2743237313762,29.4162578421115,40.0213310894596));
#197066=CARTESIAN_POINT('Ctrl Pts',(51.2841455249771,29.4165161672802,40.0132837551322));
#197067=CARTESIAN_POINT('Ctrl Pts',(51.2949386894578,29.4168000406897,40.0044405431328));
#197068=CARTESIAN_POINT('Ctrl Pts',(51.305518622259,29.4179908989228,39.9953528710605));
#197069=CARTESIAN_POINT('Ctrl Pts',(51.3158373135951,29.4199800715332,39.986110362956));
#197070=CARTESIAN_POINT('Ctrl Pts',(51.3269789106,29.4221278787384,39.9761307737562));
#197071=CARTESIAN_POINT('Ctrl Pts',(51.3378170984252,29.4252064644171,39.9659696936018));
#197072=CARTESIAN_POINT('Ctrl Pts',(51.3482921445245,29.4291364604191,39.9557128217513));
#197073=CARTESIAN_POINT('Ctrl Pts',(51.3586793157504,29.4330334877928,39.9455419945165));
#197074=CARTESIAN_POINT('Ctrl Pts',(51.3687106315444,29.437768458484,39.9352756289343));
#197075=CARTESIAN_POINT('Ctrl Pts',(51.3783102687789,29.4433108116255,39.92499));
#197076=CARTESIAN_POINT('Origin',(-0.00761999999999908,0.0131982271536721,
39.92499));
#197077=CARTESIAN_POINT('Ctrl Pts',(54.4189959163067,31.4364195775128,40.10025));
#197078=CARTESIAN_POINT('Ctrl Pts',(54.4146983388121,31.4438560159995,40.10025));
#197079=CARTESIAN_POINT('Ctrl Pts',(54.4098177483016,31.4508673716598,40.0995859581842));
#197080=CARTESIAN_POINT('Ctrl Pts',(54.4044907169114,31.4573895320582,40.0983275959621));
#197081=CARTESIAN_POINT('Ctrl Pts',(54.4010869974477,31.4615568820638,40.0975235624069));
#197082=CARTESIAN_POINT('Ctrl Pts',(54.3975017237414,31.4655251210641,40.0964777059491));
#197083=CARTESIAN_POINT('Ctrl Pts',(54.3937759157112,31.469284216974,40.0952149915961));
#197084=CARTESIAN_POINT('Ctrl Pts',(54.3886909353396,31.474414628622,40.0934916398701));
#197085=CARTESIAN_POINT('Ctrl Pts',(54.3833409297224,31.4791503318816,40.0913643921631));
#197086=CARTESIAN_POINT('Ctrl Pts',(54.3778174666306,31.4834636394923,40.0889118607713));
#197087=CARTESIAN_POINT('Ctrl Pts',(54.3750557350847,31.4856202932976,40.0876855950754));
#197088=CARTESIAN_POINT('Ctrl Pts',(54.3722505364145,31.487671530002,40.0863782327527));
#197089=CARTESIAN_POINT('Ctrl Pts',(54.3694125772951,31.4896151854254,40.0850006373334));
#197090=CARTESIAN_POINT('Ctrl Pts',(54.3679935977354,31.4905870131371,40.0843118396238));
#197091=CARTESIAN_POINT('Ctrl Pts',(54.3665664194003,31.4915319606345,40.0836054919165));
#197092=CARTESIAN_POINT('Ctrl Pts',(54.3651323262972,31.4924498523882,40.0828829920418));
#197093=CARTESIAN_POINT('Ctrl Pts',(54.3647738030214,31.4926793253266,40.0827023670731));
#197094=CARTESIAN_POINT('Ctrl Pts',(54.3644148473889,31.4929071076033,40.0825207326933));
#197095=CARTESIAN_POINT('Ctrl Pts',(54.3640554790925,31.4931331971262,40.0823381109276));
#197096=CARTESIAN_POINT('Ctrl Pts',(54.3629773742032,31.4938114656946,40.0817902456304));
#197097=CARTESIAN_POINT('Ctrl Pts',(54.3618955562477,31.4944744978644,40.0812334935553));
#197098=CARTESIAN_POINT('Ctrl Pts',(54.3608105487854,31.4951222515522,40.0806684524227));
#197099=CARTESIAN_POINT('Ctrl Pts',(54.3533124740225,31.499598631437,40.0767636676137));
#197100=CARTESIAN_POINT('Ctrl Pts',(54.3456575719328,31.503400900429,40.0724404510889));
#197101=CARTESIAN_POINT('Ctrl Pts',(54.3379428492064,31.5065976218797,40.067794993741));
#197102=CARTESIAN_POINT('Ctrl Pts',(54.3341086531879,31.5081863836659,40.0654862141906));
#197103=CARTESIAN_POINT('Ctrl Pts',(54.330259136697,31.509625294744,40.0630972003216));
#197104=CARTESIAN_POINT('Ctrl Pts',(54.3264035847699,31.5109210155995,40.0606363359906));
#197105=CARTESIAN_POINT('Ctrl Pts',(54.3178976613389,31.5137795693406,40.0552073017123));
#197106=CARTESIAN_POINT('Ctrl Pts',(54.3093672304024,31.5159526675024,40.0494204304519));
#197107=CARTESIAN_POINT('Ctrl Pts',(54.300955957207,31.517462389371,40.0434049749851));
#197108=CARTESIAN_POINT('Ctrl Pts',(54.297883213037,31.5180139098082,40.0412074532442));
#197109=CARTESIAN_POINT('Ctrl Pts',(54.2948245130138,31.5184846398469,40.0389814735788));
#197110=CARTESIAN_POINT('Ctrl Pts',(54.2917835794187,31.5188783726364,40.0367321210016));
#197111=CARTESIAN_POINT('Ctrl Pts',(54.2815694052538,31.5202008794127,40.0291767837137));
#197112=CARTESIAN_POINT('Ctrl Pts',(54.2714898389044,31.5206547127624,40.0213235332569));
#197113=CARTESIAN_POINT('Ctrl Pts',(54.2615918017967,31.5203592886222,40.0132649215848));
#197114=CARTESIAN_POINT('Ctrl Pts',(54.2507126865157,31.5200345824968,40.0044075527519));
#197115=CARTESIAN_POINT('Ctrl Pts',(54.240052193911,31.5188048676543,39.9953016253702));
#197116=CARTESIAN_POINT('Ctrl Pts',(54.2296591093493,31.5167773687219,39.9860353422336));
#197117=CARTESIAN_POINT('Ctrl Pts',(54.2184653119679,31.5145936655002,39.9760551582668));
#197118=CARTESIAN_POINT('Ctrl Pts',(54.2075805209331,31.5114844302865,39.9658879738124));
#197119=CARTESIAN_POINT('Ctrl Pts',(54.1970658734737,31.5075265408309,39.9556174643217));
#197120=CARTESIAN_POINT('Ctrl Pts',(54.1866932092582,31.503622096247,39.945485641388));
#197121=CARTESIAN_POINT('Ctrl Pts',(54.1766795569337,31.4988909785561,39.9352519465101));
#197122=CARTESIAN_POINT('Ctrl Pts',(54.1671020372442,31.4933613949852,39.92499));
#197123=CARTESIAN_POINT('Ctrl Pts',(51.1878102687789,29.7732664904673,39.92499));
#197124=CARTESIAN_POINT('Ctrl Pts',(51.1786445298598,29.7679746486351,39.9348107241719));
#197125=CARTESIAN_POINT('Ctrl Pts',(51.1699291351238,29.7619788985606,39.9446038383162));
#197126=CARTESIAN_POINT('Ctrl Pts',(51.1617065245643,29.7553188532212,39.9543158069374));
#197127=CARTESIAN_POINT('Ctrl Pts',(51.1537668706118,29.7488879934694,39.9636935671378));
#197128=CARTESIAN_POINT('Ctrl Pts',(51.1462857370555,29.7418369154177,39.9729968320973));
#197129=CARTESIAN_POINT('Ctrl Pts',(51.1393284263646,29.7341642916958,39.9821731151318));
#197130=CARTESIAN_POINT('Ctrl Pts',(51.1327515888668,29.7269112593616,39.9908475764334));
#197131=CARTESIAN_POINT('Ctrl Pts',(51.1266422417939,29.71910213351,39.9994093733828));
#197132=CARTESIAN_POINT('Ctrl Pts',(51.1210907313644,29.7107129315334,40.0077966115823));
#197133=CARTESIAN_POINT('Ctrl Pts',(51.1159778833923,29.7029866172523,40.0155211172576));
#197134=CARTESIAN_POINT('Ctrl Pts',(51.1113379461921,29.6947677915936,40.0230979941003));
#197135=CARTESIAN_POINT('Ctrl Pts',(51.1072776647626,29.6860256466498,40.030455410473));
#197136=CARTESIAN_POINT('Ctrl Pts',(51.1060669708021,29.6834189154984,40.0326492435169));
#197137=CARTESIAN_POINT('Ctrl Pts',(51.1049080895607,29.6807655934603,40.0348233715054));
#197138=CARTESIAN_POINT('Ctrl Pts',(51.1038046002597,29.6780647241921,40.0369753512355));
#197139=CARTESIAN_POINT('Ctrl Pts',(51.1027123859004,29.6753914511531,40.0391053430352));
#197140=CARTESIAN_POINT('Ctrl Pts',(51.1016753170134,29.672674475114,40.041211089324));
#197141=CARTESIAN_POINT('Ctrl Pts',(51.1006978225844,29.6699160505193,40.0432881154904));
#197142=CARTESIAN_POINT('Ctrl Pts',(51.1006298495335,29.6697242350676,40.043432547828));
#197143=CARTESIAN_POINT('Ctrl Pts',(51.1005621526966,29.6695322176083,40.0435768364421));
#197144=CARTESIAN_POINT('Ctrl Pts',(51.1004947333607,29.6693399979282,40.0437209807855));
#197145=CARTESIAN_POINT('Ctrl Pts',(51.097538822698,29.6609123829947,40.0500407968419));
#197146=CARTESIAN_POINT('Ctrl Pts',(51.0951613514272,29.6520916749677,40.0560490279343));
#197147=CARTESIAN_POINT('Ctrl Pts',(51.0934607157666,29.6429396446296,40.0616647108612));
#197148=CARTESIAN_POINT('Ctrl Pts',(51.0918754277624,29.6344083617422,40.0668995033483));
#197149=CARTESIAN_POINT('Ctrl Pts',(51.0908783954022,29.6255883681029,40.071793326748));
#197150=CARTESIAN_POINT('Ctrl Pts',(51.090576061194,29.6165418049894,40.0762460303071));
#197151=CARTESIAN_POINT('Ctrl Pts',(51.0904654634293,29.613232455165,40.0778748868747));
#197152=CARTESIAN_POINT('Ctrl Pts',(51.0904480940787,29.6098929659865,40.0794443522246));
#197153=CARTESIAN_POINT('Ctrl Pts',(51.0905301191544,29.6065271365686,40.0809482021491));
#197154=CARTESIAN_POINT('Ctrl Pts',(51.0905498434448,29.605717767036,40.0813098278168));
#197155=CARTESIAN_POINT('Ctrl Pts',(51.0905756628932,29.604906405314,40.0816679525672));
#197156=CARTESIAN_POINT('Ctrl Pts',(51.0906076352721,29.6040931741697,40.082022419258));
#197157=CARTESIAN_POINT('Ctrl Pts',(51.0906386085141,29.6033053564986,40.0823658088648));
#197158=CARTESIAN_POINT('Ctrl Pts',(51.0906753561242,29.6025157844399,40.0827057654616));
#197159=CARTESIAN_POINT('Ctrl Pts',(51.0907179287118,29.6017245728787,40.083042147015));
#197160=CARTESIAN_POINT('Ctrl Pts',(51.09118436061,29.5930559358433,40.0867275956805));
#197161=CARTESIAN_POINT('Ctrl Pts',(51.0923507190419,29.5841848213171,40.089982343203));
#197162=CARTESIAN_POINT('Ctrl Pts',(51.0942731997208,29.5752911628167,40.0926299529355));
#197163=CARTESIAN_POINT('Ctrl Pts',(51.0950705097614,29.571602697545,40.0937279956084));
#197164=CARTESIAN_POINT('Ctrl Pts',(51.0959974771977,29.5679105139257,40.0947220371802));
#197165=CARTESIAN_POINT('Ctrl Pts',(51.0970562972094,29.5642276868784,40.0956014538692));
#197166=CARTESIAN_POINT('Ctrl Pts',(51.0988622250761,29.5579462415715,40.097101390674));
#197167=CARTESIAN_POINT('Ctrl Pts',(51.1010529624044,29.5516941764749,40.0982667904315));
#197168=CARTESIAN_POINT('Ctrl Pts',(51.1036389246282,29.5455435225212,40.0990539325582));
#197169=CARTESIAN_POINT('Ctrl Pts',(51.1049319057401,29.5424681955444,40.0994475036216));
#197170=CARTESIAN_POINT('Ctrl Pts',(51.1063249785084,29.5394188854253,40.0997467259952));
#197171=CARTESIAN_POINT('Ctrl Pts',(51.1078194668134,29.5364046579951,40.0999473488896));
#197172=CARTESIAN_POINT('Ctrl Pts',(51.1093139551183,29.5333904305649,40.100147971784));
#197173=CARTESIAN_POINT('Ctrl Pts',(51.110909822857,29.5304113137787,40.10025));
#197174=CARTESIAN_POINT('Ctrl Pts',(51.1126068659051,29.5274749692178,40.10025));
#197175=CARTESIAN_POINT('Origin',(53.2328030451451,23.6840886581929,39.92499));
#197176=CARTESIAN_POINT('Ctrl Pts',(57.3172883154493,25.3107727110816,39.92499));
#197177=CARTESIAN_POINT('Ctrl Pts',(57.3269813337904,25.3150883208943,39.9348354642023));
#197178=CARTESIAN_POINT('Ctrl Pts',(57.3363050752422,25.3201559369469,39.9446440828468));
#197179=CARTESIAN_POINT('Ctrl Pts',(57.3452135417197,25.3259384683622,39.9543641760346));
#197180=CARTESIAN_POINT('Ctrl Pts',(57.3538325360831,25.3315331019391,39.9637684240732));
#197181=CARTESIAN_POINT('Ctrl Pts',(57.3620638476599,25.3377977038129,39.9730909636419));
#197182=CARTESIAN_POINT('Ctrl Pts',(57.3698434251136,25.3447390861666,39.9822808977167));
#197183=CARTESIAN_POINT('Ctrl Pts',(57.3772024263461,25.3513052064475,39.9909740094679));
#197184=CARTESIAN_POINT('Ctrl Pts',(57.3841579102039,25.3584775246735,39.9995492765034));
#197185=CARTESIAN_POINT('Ctrl Pts',(57.3906233351723,25.3662887884623,40.007946232873));
#197186=CARTESIAN_POINT('Ctrl Pts',(57.3965784591597,25.3734835273369,40.0156804369728));
#197187=CARTESIAN_POINT('Ctrl Pts',(57.4021181432129,25.381220796892,40.0232638017464));
#197188=CARTESIAN_POINT('Ctrl Pts',(57.4071400767309,25.389542308365,40.0306257270011));
#197189=CARTESIAN_POINT('Ctrl Pts',(57.4085967487453,25.3919560625171,40.0327611416681));
#197190=CARTESIAN_POINT('Ctrl Pts',(57.4100096047789,25.3944190601,40.0348777427285));
#197191=CARTESIAN_POINT('Ctrl Pts',(57.4113754784549,25.3969325220918,40.0369733168701));
#197192=CARTESIAN_POINT('Ctrl Pts',(57.4128561733383,25.3996572764936,40.039245053974));
#197193=CARTESIAN_POINT('Ctrl Pts',(57.4142805418443,25.4024370309181,40.041487875195));
#197194=CARTESIAN_POINT('Ctrl Pts',(57.4156446191419,25.405272322722,40.04369857016));
#197195=CARTESIAN_POINT('Ctrl Pts',(57.419388339989,25.413053803326,40.0497658398386));
#197196=CARTESIAN_POINT('Ctrl Pts',(57.4226343338645,25.421262340665,40.0555581699984));
#197197=CARTESIAN_POINT('Ctrl Pts',(57.4253008212881,25.4298341608304,40.0609828468885));
#197198=CARTESIAN_POINT('Ctrl Pts',(57.4277405125138,25.4376769109067,40.0659461317304));
#197199=CARTESIAN_POINT('Ctrl Pts',(57.4296843862655,25.445819360426,40.0706039980707));
#197200=CARTESIAN_POINT('Ctrl Pts',(57.431047052657,25.4542377154365,40.0748843180603));
#197201=CARTESIAN_POINT('Ctrl Pts',(57.4317163899372,25.4583727839179,40.076986797257));
#197202=CARTESIAN_POINT('Ctrl Pts',(57.432244998004,25.4625743171735,40.0789976708175));
#197203=CARTESIAN_POINT('Ctrl Pts',(57.4326195921325,25.4668384019344,40.08090504915));
#197204=CARTESIAN_POINT('Ctrl Pts',(57.4326906677197,25.4676474704851,40.0812669556105));
#197205=CARTESIAN_POINT('Ctrl Pts',(57.4327558640766,25.4684592045959,40.0816253922033));
#197206=CARTESIAN_POINT('Ctrl Pts',(57.4328151061499,25.4692734860648,40.081980198914));
#197207=CARTESIAN_POINT('Ctrl Pts',(57.4328724969083,25.4700623212378,40.0823239179149));
#197208=CARTESIAN_POINT('Ctrl Pts',(57.4329242997221,25.470853547024,40.0826642303499));
#197209=CARTESIAN_POINT('Ctrl Pts',(57.4329704479396,25.4716470524583,40.08300099161));
#197210=CARTESIAN_POINT('Ctrl Pts',(57.4334733617059,25.4802945111765,40.0866709464312));
#197211=CARTESIAN_POINT('Ctrl Pts',(57.4333046542892,25.4892184175045,40.0899175831877));
#197212=CARTESIAN_POINT('Ctrl Pts',(57.4323852136916,25.4982455208437,40.0925642067062));
#197213=CARTESIAN_POINT('Ctrl Pts',(57.4319969282178,25.5020577226394,40.0936818922527));
#197214=CARTESIAN_POINT('Ctrl Pts',(57.431475138743,25.505888119946,40.0946930094791));
#197215=CARTESIAN_POINT('Ctrl Pts',(57.4308157710843,25.509723209598,40.0955863397546));
#197216=CARTESIAN_POINT('Ctrl Pts',(57.4297054124229,25.5161814047435,40.0970906856166));
#197217=CARTESIAN_POINT('Ctrl Pts',(57.4282034292359,25.5226508554403,40.0982599215483));
#197218=CARTESIAN_POINT('Ctrl Pts',(57.4262902109372,25.5290599831058,40.0990497370454));
#197219=CARTESIAN_POINT('Ctrl Pts',(57.4258119063625,25.5306622650222,40.0992471909196));
#197220=CARTESIAN_POINT('Ctrl Pts',(57.4253076802627,25.5322606952864,40.0994209989363));
#197221=CARTESIAN_POINT('Ctrl Pts',(57.4247769415294,25.5338540367005,40.0995705982975));
#197222=CARTESIAN_POINT('Ctrl Pts',(57.4239808334294,25.5362440488215,40.0997949973393));
#197223=CARTESIAN_POINT('Ctrl Pts',(57.4231250659722,25.5386225912888,40.0999649129781));
#197224=CARTESIAN_POINT('Ctrl Pts',(57.4222091845949,25.5409861542576,40.1000786629733));
#197225=CARTESIAN_POINT('Ctrl Pts',(57.4212933032176,25.5433497172264,40.1001924129685));
#197226=CARTESIAN_POINT('Ctrl Pts',(57.4203173191904,25.5456982979273,40.10025));
#197227=CARTESIAN_POINT('Ctrl Pts',(57.4192809246792,25.5480287005711,40.10025));
#197228=CARTESIAN_POINT('Ctrl Pts',(53.9314655730807,23.9951532569801,40.10025));
#197229=CARTESIAN_POINT('Ctrl Pts',(53.934972199264,23.9872677980937,40.10025));
#197230=CARTESIAN_POINT('Ctrl Pts',(53.9390993428073,23.9797401457383,40.0995786334241));
#197231=CARTESIAN_POINT('Ctrl Pts',(53.9437193744796,23.9726512030264,40.0983063763366));
#197232=CARTESIAN_POINT('Ctrl Pts',(53.9467034408972,23.968072473402,40.0974846287992));
#197233=CARTESIAN_POINT('Ctrl Pts',(53.9498923541892,23.9636762467123,40.0964130309338));
#197234=CARTESIAN_POINT('Ctrl Pts',(53.9532454491208,23.9594780769915,40.0951176960923));
#197235=CARTESIAN_POINT('Ctrl Pts',(53.9576897843756,23.9539136435126,40.0934008039614));
#197236=CARTESIAN_POINT('Ctrl Pts',(53.9624262550348,23.9487016177214,40.0912909372156));
#197237=CARTESIAN_POINT('Ctrl Pts',(53.9673725153423,23.9438784851447,40.0888630467851));
#197238=CARTESIAN_POINT('Ctrl Pts',(53.9698456454961,23.9414669188563,40.0876491015699));
#197239=CARTESIAN_POINT('Ctrl Pts',(53.9723713025231,23.9391523931029,40.0863558569271));
#197240=CARTESIAN_POINT('Ctrl Pts',(53.9749397614924,23.9369381736868,40.0849936342771));
#197241=CARTESIAN_POINT('Ctrl Pts',(53.9762239909771,23.9358310639788,40.0843125229521));
#197242=CARTESIAN_POINT('Ctrl Pts',(53.9775189275858,23.9347490158246,40.0836141747074));
#197243=CARTESIAN_POINT('Ctrl Pts',(53.9788233972652,23.9336923430319,40.0828999161609));
#197244=CARTESIAN_POINT('Ctrl Pts',(53.9791495146851,23.9334281748337,40.0827213515243));
#197245=CARTESIAN_POINT('Ctrl Pts',(53.9794762280621,23.9331655922755,40.0825417925842));
#197246=CARTESIAN_POINT('Ctrl Pts',(53.9798035193342,23.9329045996148,40.0823612602361));
#197247=CARTESIAN_POINT('Ctrl Pts',(53.9807853931506,23.9321216216326,40.0818196631917));
#197248=CARTESIAN_POINT('Ctrl Pts',(53.9817724673294,23.9313529543285,40.0812693052022));
#197249=CARTESIAN_POINT('Ctrl Pts',(53.9827642604008,23.930598698357,40.0807107531875));
#197250=CARTESIAN_POINT('Ctrl Pts',(53.9897503227319,23.9252858166859,40.076776384918));
#197251=CARTESIAN_POINT('Ctrl Pts',(53.9969681366824,23.9206342168324,40.0724140586134));
#197252=CARTESIAN_POINT('Ctrl Pts',(54.0043120126403,23.9165878043684,40.0677221223762));
#197253=CARTESIAN_POINT('Ctrl Pts',(54.0078737845436,23.9146252986961,40.0654465383717));
#197254=CARTESIAN_POINT('Ctrl Pts',(54.0114657535938,23.9128053429035,40.0630928000677));
#197255=CARTESIAN_POINT('Ctrl Pts',(54.0150784217127,23.9111228176148,40.0606689262479));
#197256=CARTESIAN_POINT('Ctrl Pts',(54.0206091641934,23.9085469889523,40.0569581447805));
#197257=CARTESIAN_POINT('Ctrl Pts',(54.0261849176042,23.9062937028415,40.0530843804605));
#197258=CARTESIAN_POINT('Ctrl Pts',(54.0317609613889,23.9043517182276,40.0490800251457));
#197259=CARTESIAN_POINT('Ctrl Pts',(54.0343505049692,23.9034498505265,40.0472203818218));
#197260=CARTESIAN_POINT('Ctrl Pts',(54.0369399534677,23.9026149214098,40.0453323608818));
#197261=CARTESIAN_POINT('Ctrl Pts',(54.0395249709305,23.9018470291822,40.0434201572162));
#197262=CARTESIAN_POINT('Ctrl Pts',(54.0397231023336,23.9017881732686,40.0432735943397));
#197263=CARTESIAN_POINT('Ctrl Pts',(54.0399212112578,23.901729677434,40.0431268995707));
#197264=CARTESIAN_POINT('Ctrl Pts',(54.0401192964882,23.9016715408682,40.0429800745037));
#197265=CARTESIAN_POINT('Ctrl Pts',(54.0429017967675,23.9008548973944,40.0409176249753));
#197266=CARTESIAN_POINT('Ctrl Pts',(54.0456803391393,23.9001111074273,40.0388310783332));
#197267=CARTESIAN_POINT('Ctrl Pts',(54.0484499388205,23.8994373944618,40.036725739981));
#197268=CARTESIAN_POINT('Ctrl Pts',(54.0583812307207,23.8970215795832,40.0291763710716));
#197269=CARTESIAN_POINT('Ctrl Pts',(54.0682738483763,23.8954862390495,40.0213310894591));
#197270=CARTESIAN_POINT('Ctrl Pts',(54.0780688394974,23.8947164920944,40.0132837551314));
#197271=CARTESIAN_POINT('Ctrl Pts',(54.0888325507452,23.8938706175186,40.0044405431318));
#197272=CARTESIAN_POINT('Ctrl Pts',(54.0994790041488,23.8939490479886,39.9953528710593));
#197273=CARTESIAN_POINT('Ctrl Pts',(54.1099490937704,23.8948487267552,39.9861103629547));
#197274=CARTESIAN_POINT('Ctrl Pts',(54.1212541629277,23.8958201540345,39.9761307737549));
#197275=CARTESIAN_POINT('Ctrl Pts',(54.1323547778559,23.897748975781,39.9659696936005));
#197276=CARTESIAN_POINT('Ctrl Pts',(54.1431832369993,23.9005625023823,39.9557128217501));
#197277=CARTESIAN_POINT('Ctrl Pts',(54.1539208564967,23.9033524263863,39.9455419945157));
#197278=CARTESIAN_POINT('Ctrl Pts',(54.1643921589026,23.907012900388,39.9352756289339));
#197279=CARTESIAN_POINT('Ctrl Pts',(54.1745185419763,23.9115214566108,39.92499));
#197280=CARTESIAN_POINT('Origin',(-0.00619866644047451,0.013922432774471,
39.92499));
#197281=CARTESIAN_POINT('Ctrl Pts',(57.4068835917983,25.5758735661201,40.10025));
#197282=CARTESIAN_POINT('Ctrl Pts',(57.40338687637,25.5837184861902,40.10025));
#197283=CARTESIAN_POINT('Ctrl Pts',(57.3992659084774,25.5912015935366,40.0995859581842));
#197284=CARTESIAN_POINT('Ctrl Pts',(57.394649810526,25.5982448512631,40.098327595962));
#197285=CARTESIAN_POINT('Ctrl Pts',(57.3917003436858,25.6027451576541,40.0975235624068));
#197286=CARTESIAN_POINT('Ctrl Pts',(57.3885495044087,25.6070664213766,40.096477705949));
#197287=CARTESIAN_POINT('Ctrl Pts',(57.3852370392635,25.6111943775534,40.0952149915961));
#197288=CARTESIAN_POINT('Ctrl Pts',(57.380716188992,25.6168282094536,40.0934916398701));
#197289=CARTESIAN_POINT('Ctrl Pts',(57.3758905070496,25.6220971979008,40.0913643921631));
#197290=CARTESIAN_POINT('Ctrl Pts',(57.3708481654827,25.6269642358701,40.0889118607713));
#197291=CARTESIAN_POINT('Ctrl Pts',(57.3683269946992,25.6293977548547,40.0876855950754));
#197292=CARTESIAN_POINT('Ctrl Pts',(57.3657515758214,25.631730977776,40.0863782327527));
#197293=CARTESIAN_POINT('Ctrl Pts',(57.3631323306535,25.6339606331571,40.0850006373334));
#197294=CARTESIAN_POINT('Ctrl Pts',(57.3618227080695,25.6350754608477,40.0843118396237));
#197295=CARTESIAN_POINT('Ctrl Pts',(57.3605021218765,25.6361644125821,40.0836054919164));
#197296=CARTESIAN_POINT('Ctrl Pts',(57.3591718306999,25.6372271795769,40.0828829920418));
#197297=CARTESIAN_POINT('Ctrl Pts',(57.3588392579057,25.6374928713256,40.0827023670731));
#197298=CARTESIAN_POINT('Ctrl Pts',(57.3585060784011,25.6377569268679,40.0825207326933));
#197299=CARTESIAN_POINT('Ctrl Pts',(57.3581723115522,25.6380193420644,40.0823381109275));
#197300=CARTESIAN_POINT('Ctrl Pts',(57.3571710110054,25.638806587654,40.0817902456303));
#197301=CARTESIAN_POINT('Ctrl Pts',(57.3561644250956,25.6395790684325,40.0812334935553));
#197302=CARTESIAN_POINT('Ctrl Pts',(57.3551530701153,25.6403366878206,40.0806684524227));
#197303=CARTESIAN_POINT('Ctrl Pts',(57.3481639797008,25.6455723078605,40.0767636676136));
#197304=CARTESIAN_POINT('Ctrl Pts',(57.3409484573002,25.6501539027771,40.0724404510887));
#197305=CARTESIAN_POINT('Ctrl Pts',(57.3336101450127,25.6541395203644,40.0677949937408));
#197306=CARTESIAN_POINT('Ctrl Pts',(57.3299630239493,25.6561203613649,40.0654862141905));
#197307=CARTESIAN_POINT('Ctrl Pts',(57.3262850026764,25.6579537739806,40.0630972003215));
#197308=CARTESIAN_POINT('Ctrl Pts',(57.3225860115762,25.6596454116597,40.0606363359906));
#197309=CARTESIAN_POINT('Ctrl Pts',(57.3144254847134,25.6633774170491,40.0552073017123));
#197310=CARTESIAN_POINT('Ctrl Pts',(57.3061689349815,25.6664302835887,40.0494204304519));
#197311=CARTESIAN_POINT('Ctrl Pts',(57.2979615485277,25.6688109525042,40.0434049749851));
#197312=CARTESIAN_POINT('Ctrl Pts',(57.2949632867555,25.6696806408808,40.0412074532442));
#197313=CARTESIAN_POINT('Ctrl Pts',(57.2919705472986,25.6704685134241,40.0389814735788));
#197314=CARTESIAN_POINT('Ctrl Pts',(57.2889874285393,25.6711779534198,40.0367321210016));
#197315=CARTESIAN_POINT('Ctrl Pts',(57.278967448291,25.6735608872944,40.0291767837143));
#197316=CARTESIAN_POINT('Ctrl Pts',(57.2689905373642,25.6750658360784,40.0213235332581));
#197317=CARTESIAN_POINT('Ctrl Pts',(57.2591158425087,25.6758066569109,40.0132649215867));
#197318=CARTESIAN_POINT('Ctrl Pts',(57.2482623831279,25.6766209067617,40.0044075527544));
#197319=CARTESIAN_POINT('Ctrl Pts',(57.2375317496152,25.6765122533356,39.9953016253734));
#197320=CARTESIAN_POINT('Ctrl Pts',(57.2269836681111,25.6755822344125,39.9860353422375));
#197321=CARTESIAN_POINT('Ctrl Pts',(57.2156229323817,25.6745805641843,39.9760551582714));
#197322=CARTESIAN_POINT('Ctrl Pts',(57.2044727657929,25.6726261321667,39.9658879738178));
#197323=CARTESIAN_POINT('Ctrl Pts',(57.1936020065706,25.669789004385,39.9556174643279));
#197324=CARTESIAN_POINT('Ctrl Pts',(57.1828780393004,25.6669901874073,39.9454856413921));
#197325=CARTESIAN_POINT('Ctrl Pts',(57.1724247063471,25.6633316989627,39.9352519465122));
#197326=CARTESIAN_POINT('Ctrl Pts',(57.1623216544374,25.6588335304434,39.92499));
#197327=CARTESIAN_POINT('Ctrl Pts',(54.0195518809644,24.2595822759726,39.92499));
#197328=CARTESIAN_POINT('Ctrl Pts',(54.0098832048288,24.2552775040081,39.9348107241706));
#197329=CARTESIAN_POINT('Ctrl Pts',(54.0005888273967,24.250225606099,39.9446038383138));
#197330=CARTESIAN_POINT('Ctrl Pts',(53.9917150968546,24.2444615420316,39.9543158069337));
#197331=CARTESIAN_POINT('Ctrl Pts',(53.9831467292703,24.2388958310295,39.9636935671335));
#197332=CARTESIAN_POINT('Ctrl Pts',(53.9749695397937,24.2326653709158,39.9729968320924));
#197333=CARTESIAN_POINT('Ctrl Pts',(53.9672483344123,24.2257620156253,39.9821731151263));
#197334=CARTESIAN_POINT('Ctrl Pts',(53.9599493771946,24.2192361828783,39.9908475764277));
#197335=CARTESIAN_POINT('Ctrl Pts',(53.9530572218394,24.2121084368968,39.9994093733768));
#197336=CARTESIAN_POINT('Ctrl Pts',(53.9466592127742,24.204345482701,40.0077966115762));
#197337=CARTESIAN_POINT('Ctrl Pts',(53.9407667537595,24.1971959321197,40.0155211172516));
#197338=CARTESIAN_POINT('Ctrl Pts',(53.9352931334045,24.1895071355534,40.0230979940944));
#197339=CARTESIAN_POINT('Ctrl Pts',(53.9303412916447,24.1812372959729,40.0304554104673));
#197340=CARTESIAN_POINT('Ctrl Pts',(53.9288647523896,24.1787713967446,40.0326492435131));
#197341=CARTESIAN_POINT('Ctrl Pts',(53.9274348719444,24.1762537459554,40.0348233715036));
#197342=CARTESIAN_POINT('Ctrl Pts',(53.9260551099579,24.1736830183703,40.0369753512356));
#197343=CARTESIAN_POINT('Ctrl Pts',(53.9246894457405,24.1711385572892,40.0391053430352));
#197344=CARTESIAN_POINT('Ctrl Pts',(53.9233740566953,24.1685448683462,40.041211089324));
#197345=CARTESIAN_POINT('Ctrl Pts',(53.9221135831991,24.1659037306806,40.0432881154904));
#197346=CARTESIAN_POINT('Ctrl Pts',(53.9220259323373,24.1657200711326,40.043432547828));
#197347=CARTESIAN_POINT('Ctrl Pts',(53.9219385350609,24.1655361818113,40.0435768364421));
#197348=CARTESIAN_POINT('Ctrl Pts',(53.9218513926274,24.1653520623703,40.0437209807855));
#197349=CARTESIAN_POINT('Ctrl Pts',(53.9180307491145,24.1572795915923,40.0500407968419));
#197350=CARTESIAN_POINT('Ctrl Pts',(53.9147442868251,24.1487557177452,40.0560490279343));
#197351=CARTESIAN_POINT('Ctrl Pts',(53.9120963197575,24.139831588019,40.0616647108613));
#197352=CARTESIAN_POINT('Ctrl Pts',(53.909627954237,24.131512748111,40.0668995033483));
#197353=CARTESIAN_POINT('Ctrl Pts',(53.9077144433433,24.1228452895804,40.0717933267478));
#197354=CARTESIAN_POINT('Ctrl Pts',(53.9064681420134,24.1138798870166,40.0762460303068));
#197355=CARTESIAN_POINT('Ctrl Pts',(53.9060122288632,24.1106002267709,40.0778748868745));
#197356=CARTESIAN_POINT('Ctrl Pts',(53.9056458829919,24.107280847255,40.0794443522246));
#197357=CARTESIAN_POINT('Ctrl Pts',(53.9053756337488,24.1039248822475,40.0809482021492));
#197358=CARTESIAN_POINT('Ctrl Pts',(53.9053106478341,24.1031178847761,40.0813098278168));
#197359=CARTESIAN_POINT('Ctrl Pts',(53.9052515154469,24.1023082689112,40.0816679525672));
#197360=CARTESIAN_POINT('Ctrl Pts',(53.9051983068759,24.1014961507086,40.082022419258));
#197361=CARTESIAN_POINT('Ctrl Pts',(53.9051467610728,24.1007094111998,40.0823658088648));
#197362=CARTESIAN_POINT('Ctrl Pts',(53.9051007746217,24.0999203233282,40.0827057654617));
#197363=CARTESIAN_POINT('Ctrl Pts',(53.9050604098637,24.0991289960595,40.0830421470151));
#197364=CARTESIAN_POINT('Ctrl Pts',(53.9046181672912,24.0904590913151,40.0867275956807));
#197365=CARTESIAN_POINT('Ctrl Pts',(53.9048508523207,24.0815146560278,40.0899823432032));
#197366=CARTESIAN_POINT('Ctrl Pts',(53.9058331609935,24.072468763968,40.0926299529357));
#197367=CARTESIAN_POINT('Ctrl Pts',(53.9062405536795,24.0687171629018,40.0937279956085));
#197368=CARTESIAN_POINT('Ctrl Pts',(53.9067765048114,24.0649483109693,40.0947220371803));
#197369=CARTESIAN_POINT('Ctrl Pts',(53.9074445642445,24.0611749820054,40.0956014538692));
#197370=CARTESIAN_POINT('Ctrl Pts',(53.9085840092244,24.0547391762485,40.097101390674));
#197371=CARTESIAN_POINT('Ctrl Pts',(53.9101092267075,24.0482923662123,40.0982667904316));
#197372=CARTESIAN_POINT('Ctrl Pts',(53.9120381043535,24.0419050995271,40.0990539325582));
#197373=CARTESIAN_POINT('Ctrl Pts',(53.9130025431765,24.0387114661845,40.0994475036216));
#197374=CARTESIAN_POINT('Ctrl Pts',(53.9140692448457,24.0355332447496,40.0997467259952));
#197375=CARTESIAN_POINT('Ctrl Pts',(53.9152404736262,24.0323793130068,40.0999473488896));
#197376=CARTESIAN_POINT('Ctrl Pts',(53.9164117024067,24.029225381264,40.100147971784));
#197377=CARTESIAN_POINT('Ctrl Pts',(53.9176874253156,24.026095770789,40.10025));
#197378=CARTESIAN_POINT('Ctrl Pts',(53.9190682401998,24.022998122529,40.10025));
#197379=CARTESIAN_POINT('Origin',(55.4168495715594,17.9900016446776,39.92499));
#197380=CARTESIAN_POINT('Ctrl Pts',(59.6489943884567,19.1808295835774,39.92499));
#197381=CARTESIAN_POINT('Ctrl Pts',(59.6590854114904,19.1841083557162,39.9348354642021));
#197382=CARTESIAN_POINT('Ctrl Pts',(59.668887786629,19.1881736144719,39.9446440828463));
#197383=CARTESIAN_POINT('Ctrl Pts',(59.6783518907173,19.1929932802638,39.9543641760339));
#197384=CARTESIAN_POINT('Ctrl Pts',(59.6875084677778,19.1976563356168,39.9637684240722));
#197385=CARTESIAN_POINT('Ctrl Pts',(59.6963495165752,19.203026212996,39.9730909636406));
#197386=CARTESIAN_POINT('Ctrl Pts',(59.7048120487199,19.2091163824545,39.9822808977152));
#197387=CARTESIAN_POINT('Ctrl Pts',(59.712817083036,19.2148773077512,39.9909740094661));
#197388=CARTESIAN_POINT('Ctrl Pts',(59.7204841754277,19.2212832892283,39.9995492765013));
#197389=CARTESIAN_POINT('Ctrl Pts',(59.7277306815216,19.2283759411601,40.0079462328707));
#197390=CARTESIAN_POINT('Ctrl Pts',(59.7344052377146,19.234908786543,40.0156804369702));
#197391=CARTESIAN_POINT('Ctrl Pts',(59.7407233396953,19.2420246158644,40.0232638017434));
#197392=CARTESIAN_POINT('Ctrl Pts',(59.7465875973423,19.2497756062331,40.0306257269979));
#197393=CARTESIAN_POINT('Ctrl Pts',(59.7482885955682,19.2520238739014,40.032761141666));
#197394=CARTESIAN_POINT('Ctrl Pts',(59.7499511651817,19.2543256952568,40.0348777427275));
#197395=CARTESIAN_POINT('Ctrl Pts',(59.7515722847792,19.2566826155657,40.0369733168701));
#197396=CARTESIAN_POINT('Ctrl Pts',(59.7533296826515,19.2592376687171,40.039245053974));
#197397=CARTESIAN_POINT('Ctrl Pts',(59.755036811776,19.2618533083049,40.041487875195));
#197398=CARTESIAN_POINT('Ctrl Pts',(59.7566897852106,19.26453048318,40.04369857016));
#197399=CARTESIAN_POINT('Ctrl Pts',(59.7612263837727,19.271878010632,40.0497658398386));
#197400=CARTESIAN_POINT('Ctrl Pts',(59.7653126215478,19.279702281993,40.0555581699984));
#197401=CARTESIAN_POINT('Ctrl Pts',(59.7688605008636,19.2879484209979,40.0609828468885));
#197402=CARTESIAN_POINT('Ctrl Pts',(59.7721066178187,19.2954931904941,40.0659461317305));
#197403=CARTESIAN_POINT('Ctrl Pts',(59.7748909605622,19.303387844687,40.0706039980707));
#197404=CARTESIAN_POINT('Ctrl Pts',(59.7771261198371,19.3116176456442,40.0748843180604));
#197405=CARTESIAN_POINT('Ctrl Pts',(59.7782240227715,19.3156600969904,40.076986797257));
#197406=CARTESIAN_POINT('Ctrl Pts',(59.7791889148826,19.3197833592182,40.0789976708175));
#197407=CARTESIAN_POINT('Ctrl Pts',(59.7800071751725,19.323984929128,40.08090504915));
#197408=CARTESIAN_POINT('Ctrl Pts',(59.7801624320925,19.3247821360946,40.0812669556104));
#197409=CARTESIAN_POINT('Ctrl Pts',(59.7803121206161,19.3255826085659,40.0816253922032));
#197410=CARTESIAN_POINT('Ctrl Pts',(59.7804561537457,19.3263862368329,40.0819801989139));
#197411=CARTESIAN_POINT('Ctrl Pts',(59.7805956858399,19.3271647517165,40.0823239179149));
#197412=CARTESIAN_POINT('Ctrl Pts',(59.780729910488,19.3279462282165,40.0826642303498));
#197413=CARTESIAN_POINT('Ctrl Pts',(59.7808587498045,19.3287305629428,40.0830009916099));
#197414=CARTESIAN_POINT('Ctrl Pts',(59.7822628141275,19.3372780811743,40.0866709464312));
#197415=CARTESIAN_POINT('Ctrl Pts',(59.7830278331225,19.3461707361368,40.0899175831878));
#197416=CARTESIAN_POINT('Ctrl Pts',(59.7830570185565,19.3552444957722,40.0925642067062));
#197417=CARTESIAN_POINT('Ctrl Pts',(59.7830693437465,19.3590764008114,40.0936818922528));
#197418=CARTESIAN_POINT('Ctrl Pts',(59.7829507982332,19.3629403566526,40.094693009479));
#197419=CARTESIAN_POINT('Ctrl Pts',(59.7826959186874,19.3668233599702,40.0955863397546));
#197420=CARTESIAN_POINT('Ctrl Pts',(59.7822667079009,19.3733622405315,40.0970906856166));
#197421=CARTESIAN_POINT('Ctrl Pts',(59.7814491944745,19.3799532508949,40.0982599215483));
#197422=CARTESIAN_POINT('Ctrl Pts',(59.7802163932513,19.386527254457,40.0990497370454));
#197423=CARTESIAN_POINT('Ctrl Pts',(59.7799081929455,19.3881707553476,40.0992471909196));
#197424=CARTESIAN_POINT('Ctrl Pts',(59.7795738105081,19.3898131352229,40.0994209989363));
#197425=CARTESIAN_POINT('Ctrl Pts',(59.7792125287466,19.3914532254502,40.0995705982975));
#197426=CARTESIAN_POINT('Ctrl Pts',(59.7786706061044,19.3939133607911,40.0997949973393));
#197427=CARTESIAN_POINT('Ctrl Pts',(59.7780681520198,19.3963683254111,40.0999649129781));
#197428=CARTESIAN_POINT('Ctrl Pts',(59.7774043475416,19.3988146762076,40.1000786629733));
#197429=CARTESIAN_POINT('Ctrl Pts',(59.7767405430633,19.4012610270041,40.1001924129685));
#197430=CARTESIAN_POINT('Ctrl Pts',(59.7760153991104,19.4036987600447,40.10025));
#197431=CARTESIAN_POINT('Ctrl Pts',(59.7752282754839,19.4061247292246,40.10025));
#197432=CARTESIAN_POINT('Ctrl Pts',(56.144199857553,18.2263320786575,40.10025));
#197433=CARTESIAN_POINT('Ctrl Pts',(56.1468630191714,18.2181232748942,40.10025));
#197434=CARTESIAN_POINT('Ctrl Pts',(56.1501806998576,18.2102054558342,40.0995786334241));
#197435=CARTESIAN_POINT('Ctrl Pts',(56.1540344262249,18.2026724222816,40.0983063763368));
#197436=CARTESIAN_POINT('Ctrl Pts',(56.1565235380433,18.1978068555399,40.0974846287994));
#197437=CARTESIAN_POINT('Ctrl Pts',(56.1592354513147,18.1931013796336,40.0964130309339));
#197438=CARTESIAN_POINT('Ctrl Pts',(56.1621313494122,18.1885757140651,40.0951176960924));
#197439=CARTESIAN_POINT('Ctrl Pts',(56.165969696453,18.1825772036006,40.0934008039614));
#197440=CARTESIAN_POINT('Ctrl Pts',(56.1701354151838,18.1768986338326,40.0912909372156));
#197441=CARTESIAN_POINT('Ctrl Pts',(56.1745504247235,18.171584897892,40.0888630467851));
#197442=CARTESIAN_POINT('Ctrl Pts',(56.1767579294933,18.1689280299216,40.0876491015699));
#197443=CARTESIAN_POINT('Ctrl Pts',(56.1790278168867,18.1663621803347,40.0863558569271));
#197444=CARTESIAN_POINT('Ctrl Pts',(56.1813507566161,18.1638916135752,40.0849936342771));
#197445=CARTESIAN_POINT('Ctrl Pts',(56.1825122264809,18.1626563301955,40.0843125229521));
#197446=CARTESIAN_POINT('Ctrl Pts',(56.1836869644606,18.1614448518806,40.0836141747074));
#197447=CARTESIAN_POINT('Ctrl Pts',(56.1848738357354,18.160257613441,40.0828999161609));
#197448=CARTESIAN_POINT('Ctrl Pts',(56.1851705535541,18.1599608038311,40.0827213515243));
#197449=CARTESIAN_POINT('Ctrl Pts',(56.1854680298098,18.1596655088804,40.0825417925842));
#197450=CARTESIAN_POINT('Ctrl Pts',(56.1857662469844,18.1593717347111,40.082361260236));
#197451=CARTESIAN_POINT('Ctrl Pts',(56.186660898508,18.1584904122031,40.0818196631917));
#197452=CARTESIAN_POINT('Ctrl Pts',(56.1875622177791,18.1576227783918,40.0812693052021));
#197453=CARTESIAN_POINT('Ctrl Pts',(56.1884697364866,18.1567689837079,40.0807107531874));
#197454=CARTESIAN_POINT('Ctrl Pts',(56.1948621810804,18.150754964199,40.0767763849182));
#197455=CARTESIAN_POINT('Ctrl Pts',(56.2015542305059,18.1453743792962,40.0724140586139));
#197456=CARTESIAN_POINT('Ctrl Pts',(56.2084349106659,18.1405824894349,40.0677221223771));
#197457=CARTESIAN_POINT('Ctrl Pts',(56.2117720331084,18.1382584280302,40.0654465383723));
#197458=CARTESIAN_POINT('Ctrl Pts',(56.2151540877945,18.1360729791405,40.063092800068));
#197459=CARTESIAN_POINT('Ctrl Pts',(56.2185710935571,18.1340220442544,40.0606689262479));
#197460=CARTESIAN_POINT('Ctrl Pts',(56.22380229064,18.1308822062386,40.0569581447805));
#197461=CARTESIAN_POINT('Ctrl Pts',(56.2291119669557,18.1280584389292,40.0530843804605));
#197462=CARTESIAN_POINT('Ctrl Pts',(56.2344544719219,18.1255442374224,40.0490800251457));
#197463=CARTESIAN_POINT('Ctrl Pts',(56.2369355588666,18.1243766292358,40.0472203818218));
#197464=CARTESIAN_POINT('Ctrl Pts',(56.2394235482377,18.123275602876,40.0453323608818));
#197465=CARTESIAN_POINT('Ctrl Pts',(56.2419141381099,18.1222417093394,40.0434201572162));
#197466=CARTESIAN_POINT('Ctrl Pts',(56.2421050320102,18.1221624654736,40.0432735943397));
#197467=CARTESIAN_POINT('Ctrl Pts',(56.2422959411933,18.1220835820639,40.0431268995707));
#197468=CARTESIAN_POINT('Ctrl Pts',(56.2424868643662,18.1220050584315,40.0429800745037));
#197469=CARTESIAN_POINT('Ctrl Pts',(56.2451687593305,18.1209020381379,40.0409176249753));
#197470=CARTESIAN_POINT('Ctrl Pts',(56.2478543333342,18.1198718859658,40.0388310783332));
#197471=CARTESIAN_POINT('Ctrl Pts',(56.2505383386776,18.1189123616719,40.036725739981));
#197472=CARTESIAN_POINT('Ctrl Pts',(56.2601627045041,18.1154716781997,40.0291763710722));
#197473=CARTESIAN_POINT('Ctrl Pts',(56.2698406425778,18.112910688301,40.0213310894603));
#197474=CARTESIAN_POINT('Ctrl Pts',(56.2795015152455,18.1111213027306,40.0132837551333));
#197475=CARTESIAN_POINT('Ctrl Pts',(56.2901178437866,18.1091549477485,40.0044405431344));
#197476=CARTESIAN_POINT('Ctrl Pts',(56.3007141730202,18.1081200911546,39.9953528710626));
#197477=CARTESIAN_POINT('Ctrl Pts',(56.3112209484336,18.1079204190081,39.9861103629587));
#197478=CARTESIAN_POINT('Ctrl Pts',(56.3225656290391,18.1077048232008,39.9761307737596));
#197479=CARTESIAN_POINT('Ctrl Pts',(56.3338070504095,18.1084627484397,39.965969693606));
#197480=CARTESIAN_POINT('Ctrl Pts',(56.3448702837321,18.1101289800536,39.9557128217563));
#197481=CARTESIAN_POINT('Ctrl Pts',(56.3558407078974,18.1117812336967,39.9455419945199));
#197482=CARTESIAN_POINT('Ctrl Pts',(56.3666372711377,18.1143271060903,39.935275628936));
#197483=CARTESIAN_POINT('Ctrl Pts',(56.377179453281,18.1177524687099,39.92499));
#197484=CARTESIAN_POINT('Origin',(-0.00470941899427373,0.0144941013083365,
39.92499));
#197485=CARTESIAN_POINT('Ctrl Pts',(59.7658094374954,19.4351129318413,40.10025));
#197486=CARTESIAN_POINT('Ctrl Pts',(59.7631518948792,19.4432803829093,40.10025));
#197487=CARTESIAN_POINT('Ctrl Pts',(59.759835699791,19.4511532554524,40.099585958184));
#197488=CARTESIAN_POINT('Ctrl Pts',(59.7559811102134,19.4586404431018,40.0983275959617));
#197489=CARTESIAN_POINT('Ctrl Pts',(59.7535182109726,19.4634243995791,40.0975235624065));
#197490=CARTESIAN_POINT('Ctrl Pts',(59.7508363273794,19.4680513433538,40.0964777059488));
#197491=CARTESIAN_POINT('Ctrl Pts',(59.7479734971809,19.4725029330454,40.0952149915961));
#197492=CARTESIAN_POINT('Ctrl Pts',(59.744066308391,19.4785784597565,40.0934916398701));
#197493=CARTESIAN_POINT('Ctrl Pts',(59.7398178213045,19.4843230052514,40.0913643921631));
#197494=CARTESIAN_POINT('Ctrl Pts',(59.7353118462119,19.4896904492926,40.0889118607713));
#197495=CARTESIAN_POINT('Ctrl Pts',(59.7330588586655,19.4923741713132,40.0876855950754));
#197496=CARTESIAN_POINT('Ctrl Pts',(59.7307414364082,19.4949638171728,40.0863782327526));
#197497=CARTESIAN_POINT('Ctrl Pts',(59.72836960219,19.4974550439408,40.0850006373334));
#197498=CARTESIAN_POINT('Ctrl Pts',(59.7271836850809,19.4987006573248,40.0843118396237));
#197499=CARTESIAN_POINT('Ctrl Pts',(59.7259841596486,19.499921682513,40.0836054919164));
#197500=CARTESIAN_POINT('Ctrl Pts',(59.724772245347,19.5011176808515,40.0828829920418));
#197501=CARTESIAN_POINT('Ctrl Pts',(59.7244692667716,19.5014166804361,40.0827023670731));
#197502=CARTESIAN_POINT('Ctrl Pts',(59.7241655137792,19.5017141161961,40.0825207326933));
#197503=CARTESIAN_POINT('Ctrl Pts',(59.7238610051972,19.5020099819905,40.0823381109275));
#197504=CARTESIAN_POINT('Ctrl Pts',(59.7229474794513,19.5028975793738,40.0817902456303));
#197505=CARTESIAN_POINT('Ctrl Pts',(59.7220271539531,19.5037710453001,40.0812334935553));
#197506=CARTESIAN_POINT('Ctrl Pts',(59.7211005320716,19.5046302297518,40.0806684524227));
#197507=CARTESIAN_POINT('Ctrl Pts',(59.7146969999425,19.5105677273982,40.0767636676135));
#197508=CARTESIAN_POINT('Ctrl Pts',(59.7079999120043,19.5158784513267,40.0724404510885));
#197509=CARTESIAN_POINT('Ctrl Pts',(59.7011184102408,19.5206092977904,40.0677949937404));
#197510=CARTESIAN_POINT('Ctrl Pts',(59.6976983227541,19.5229605154966,40.0654862141902));
#197511=CARTESIAN_POINT('Ctrl Pts',(59.6942320938701,19.5251683423976,40.0630972003214));
#197512=CARTESIAN_POINT('Ctrl Pts',(59.6907301905173,19.5272373629636,40.0606363359906));
#197513=CARTESIAN_POINT('Ctrl Pts',(59.6830044686629,19.5318019313695,40.0552073017123));
#197514=CARTESIAN_POINT('Ctrl Pts',(59.6751122606222,19.5357011184421,40.0494204304519));
#197515=CARTESIAN_POINT('Ctrl Pts',(59.6671986827534,19.5389266512976,40.0434049749851));
#197516=CARTESIAN_POINT('Ctrl Pts',(59.6643077529625,19.5401049791258,40.0412074532442));
#197517=CARTESIAN_POINT('Ctrl Pts',(59.6614137631516,19.5412013620773,40.0389814735788));
#197518=CARTESIAN_POINT('Ctrl Pts',(59.6585211429015,19.5422187365061,40.0367321210016));
#197519=CARTESIAN_POINT('Ctrl Pts',(59.6488051375691,19.545635989557,40.0291767837141));
#197520=CARTESIAN_POINT('Ctrl Pts',(59.6390401911876,19.5481755652415,40.0213235332577));
#197521=CARTESIAN_POINT('Ctrl Pts',(59.6292970278066,19.5499445144584,40.0132649215861));
#197522=CARTESIAN_POINT('Ctrl Pts',(59.6185881370972,19.5518887991936,40.0044075527536));
#197523=CARTESIAN_POINT('Ctrl Pts',(59.6079049297416,19.5529023976132,39.9953016253723));
#197524=CARTESIAN_POINT('Ctrl Pts',(59.5973174182825,19.5530800481811,39.9860353422362));
#197525=CARTESIAN_POINT('Ctrl Pts',(59.5859142148021,19.5532713854545,39.9760551582698));
#197526=CARTESIAN_POINT('Ctrl Pts',(59.5746208362169,19.5524931697985,39.9658879738159));
#197527=CARTESIAN_POINT('Ctrl Pts',(59.5635130675436,19.5508078878555,39.9556174643256));
#197528=CARTESIAN_POINT('Ctrl Pts',(59.5525552912515,19.5491453629089,39.9454856413906));
#197529=CARTESIAN_POINT('Ctrl Pts',(59.5417768065759,19.5465995868767,39.9352519465114));
#197530=CARTESIAN_POINT('Ctrl Pts',(59.5312589135998,19.5431821162859,39.92499));
#197531=CARTESIAN_POINT('Ctrl Pts',(56.2594439784241,18.4801050014183,39.92499));
#197532=CARTESIAN_POINT('Ctrl Pts',(56.249378297109,18.4768344633031,39.9348107241714));
#197533=CARTESIAN_POINT('Ctrl Pts',(56.2396067681233,18.472781767209,39.9446038383154));
#197534=CARTESIAN_POINT('Ctrl Pts',(56.2301791400456,18.4679768367041,39.9543158069361));
#197535=CARTESIAN_POINT('Ctrl Pts',(56.2210759356573,18.4633372535452,39.9636935671363));
#197536=CARTESIAN_POINT('Ctrl Pts',(56.2122922812589,18.4579956735935,39.9729968320954));
#197537=CARTESIAN_POINT('Ctrl Pts',(56.2038917763283,18.4519372213383,39.9821731151296));
#197538=CARTESIAN_POINT('Ctrl Pts',(56.1959506682935,18.4462100865672,39.9908475764309));
#197539=CARTESIAN_POINT('Ctrl Pts',(56.1883512165526,18.4398418135318,39.9994093733799));
#197540=CARTESIAN_POINT('Ctrl Pts',(56.1811768067782,18.4327901596668,40.0077966115791));
#197541=CARTESIAN_POINT('Ctrl Pts',(56.1745692957356,18.4262957047575,40.0155211172542));
#197542=CARTESIAN_POINT('Ctrl Pts',(56.1683219623566,18.4192211773477,40.0230979940965));
#197543=CARTESIAN_POINT('Ctrl Pts',(56.1625328136815,18.4115142492234,40.0304554104689));
#197544=CARTESIAN_POINT('Ctrl Pts',(56.1608066064065,18.409216198829,40.0326492435142));
#197545=CARTESIAN_POINT('Ctrl Pts',(56.1591213928284,18.4068618032005,40.0348233715041));
#197546=CARTESIAN_POINT('Ctrl Pts',(56.1574804751189,18.4044493827308,40.0369753512356));
#197547=CARTESIAN_POINT('Ctrl Pts',(56.1558563235463,18.4020616112557,40.0391053430352));
#197548=CARTESIAN_POINT('Ctrl Pts',(56.1542770260205,18.3996196264076,40.041211089324));
#197549=CARTESIAN_POINT('Ctrl Pts',(56.1527473834686,18.397124712528,40.0432881154904));
#197550=CARTESIAN_POINT('Ctrl Pts',(56.152641015117,18.3969512210961,40.043432547828));
#197551=CARTESIAN_POINT('Ctrl Pts',(56.1525348749439,18.3967774746428,40.0435768364421));
#197552=CARTESIAN_POINT('Ctrl Pts',(56.1524289641635,18.3966034726919,40.0437209807855));
#197553=CARTESIAN_POINT('Ctrl Pts',(56.1477854475703,18.3889745897485,40.050040796842));
#197554=CARTESIAN_POINT('Ctrl Pts',(56.1436260014308,18.3808409394268,40.0560490279345));
#197555=CARTESIAN_POINT('Ctrl Pts',(56.1400597146376,18.3722424849452,40.0616647108616));
#197556=CARTESIAN_POINT('Ctrl Pts',(56.1367353155299,18.364227230967,40.0668995033487));
#197557=CARTESIAN_POINT('Ctrl Pts',(56.1339262909284,18.3558072700341,40.0717933267483));
#197558=CARTESIAN_POINT('Ctrl Pts',(56.131749677215,18.347021254846,40.0762460303074));
#197559=CARTESIAN_POINT('Ctrl Pts',(56.1309534437593,18.3438072168237,40.0778748868749));
#197560=CARTESIAN_POINT('Ctrl Pts',(56.1302421351293,18.3405443147874,40.0794443522248));
#197561=CARTESIAN_POINT('Ctrl Pts',(56.1296225724749,18.3372349828458,40.0809482021492));
#197562=CARTESIAN_POINT('Ctrl Pts',(56.1294735883543,18.3364391990689,40.0813098278168));
#197563=CARTESIAN_POINT('Ctrl Pts',(56.1293301519983,18.335640199382,40.0816679525672));
#197564=CARTESIAN_POINT('Ctrl Pts',(56.1291923454417,18.334838091858,40.082022419258));
#197565=CARTESIAN_POINT('Ctrl Pts',(56.1290588453401,18.3340610501941,40.0823658088648));
#197566=CARTESIAN_POINT('Ctrl Pts',(56.1289306286649,18.3332810919215,40.0827057654616));
#197567=CARTESIAN_POINT('Ctrl Pts',(56.128807768806,18.3324983188925,40.0830421470151));
#197568=CARTESIAN_POINT('Ctrl Pts',(56.127461697065,18.3239221357303,40.0867275956805));
#197569=CARTESIAN_POINT('Ctrl Pts',(56.1267581593462,18.3150023767871,40.089982343203));
#197570=CARTESIAN_POINT('Ctrl Pts',(56.1267895336333,18.3059033598548,40.0926299529354));
#197571=CARTESIAN_POINT('Ctrl Pts',(56.1268025454853,18.3021297263201,40.0937279956083));
#197572=CARTESIAN_POINT('Ctrl Pts',(56.12694160832,18.2983254984043,40.0947220371802));
#197573=CARTESIAN_POINT('Ctrl Pts',(56.1272115877757,18.294503008905,40.0956014538692));
#197574=CARTESIAN_POINT('Ctrl Pts',(56.1276720658711,18.2879833547327,40.097101390674));
#197575=CARTESIAN_POINT('Ctrl Pts',(56.1285150529072,18.2814124323567,40.0982667904316));
#197576=CARTESIAN_POINT('Ctrl Pts',(56.1297657127889,18.2748585331707,40.0990539325582));
#197577=CARTESIAN_POINT('Ctrl Pts',(56.1303910427298,18.2715815835777,40.0994475036216));
#197578=CARTESIAN_POINT('Ctrl Pts',(56.1311196862931,18.2683092720861,40.0997467259952));
#197579=CARTESIAN_POINT('Ctrl Pts',(56.1319548233213,18.2650501911668,40.0999473488896));
#197580=CARTESIAN_POINT('Ctrl Pts',(56.1327899603496,18.2617911102474,40.100147971784));
#197581=CARTESIAN_POINT('Ctrl Pts',(56.1337315613411,18.2585452947508,40.10025));
#197582=CARTESIAN_POINT('Ctrl Pts',(56.1347810195644,18.2553202812742,40.10025));
#197583=CARTESIAN_POINT('Origin',(56.9937374973465,12.0988124084933,39.92499));
#197584=CARTESIAN_POINT('Ctrl Pts',(61.3271735965895,12.840737273309,39.92499));
#197585=CARTESIAN_POINT('Ctrl Pts',(61.3375520649562,12.8429432848604,39.9348354642016));
#197586=CARTESIAN_POINT('Ctrl Pts',(61.3477256769083,12.8459616464936,39.9446440828453));
#197587=CARTESIAN_POINT('Ctrl Pts',(61.3576417279026,12.8497656413953,39.9543641760325));
#197588=CARTESIAN_POINT('Ctrl Pts',(61.3672355662859,12.853446029114,39.9637684240705));
#197589=CARTESIAN_POINT('Ctrl Pts',(61.376589487923,12.8578623484984,39.9730909636387));
#197590=CARTESIAN_POINT('Ctrl Pts',(61.3856422574854,12.8630345798907,39.982280897713));
#197591=CARTESIAN_POINT('Ctrl Pts',(61.394205620054,12.8679271923002,39.9909740094639));
#197592=CARTESIAN_POINT('Ctrl Pts',(61.4025003187107,12.8734966517548,39.9995492764989));
#197593=CARTESIAN_POINT('Ctrl Pts',(61.4104485116927,12.8797929832509,40.0079462328682));
#197594=CARTESIAN_POINT('Ctrl Pts',(61.417769372257,12.8855923599211,40.0156804369676));
#197595=CARTESIAN_POINT('Ctrl Pts',(61.4247966697177,12.8920087864938,40.0232638017408));
#197596=CARTESIAN_POINT('Ctrl Pts',(61.4314390014596,12.8991043342859,40.0306257269952));
#197597=CARTESIAN_POINT('Ctrl Pts',(61.4333656894045,12.9011624829789,40.0327611416642));
#197598=CARTESIAN_POINT('Ctrl Pts',(61.4352597571376,12.9032779088702,40.0348777427266));
#197599=CARTESIAN_POINT('Ctrl Pts',(61.4371183613309,12.9054524645837,40.0369733168701));
#197600=CARTESIAN_POINT('Ctrl Pts',(61.4391332077733,12.9078098227875,40.039245053974));
#197601=CARTESIAN_POINT('Ctrl Pts',(61.4411043938524,12.9102326900441,40.041487875195));
#197602=CARTESIAN_POINT('Ctrl Pts',(61.4430281531013,12.9127224163021,40.0436985701601));
#197603=CARTESIAN_POINT('Ctrl Pts',(61.4483079254551,12.9195554895538,40.0497658398386));
#197604=CARTESIAN_POINT('Ctrl Pts',(61.4531896374537,12.9269097705824,40.0555581699984));
#197605=CARTESIAN_POINT('Ctrl Pts',(61.4575800373535,12.9347398820023,40.0609828468885));
#197606=CARTESIAN_POINT('Ctrl Pts',(61.4615970149013,12.9419040088446,40.0659461317303));
#197607=CARTESIAN_POINT('Ctrl Pts',(61.4651913207946,12.9494643722274,40.0706039980704));
#197608=CARTESIAN_POINT('Ctrl Pts',(61.4682744840801,12.9574154517093,40.07488431806));
#197609=CARTESIAN_POINT('Ctrl Pts',(61.4697889238145,12.9613209959778,40.0769867972567));
#197610=CARTESIAN_POINT('Ctrl Pts',(61.4711795284101,12.9653208118544,40.0789976708173));
#197611=CARTESIAN_POINT('Ctrl Pts',(61.4724324898305,12.9694138336343,40.0809050491499));
#197612=CARTESIAN_POINT('Ctrl Pts',(61.4726702270561,12.9701904446504,40.0812669556104));
#197613=CARTESIAN_POINT('Ctrl Pts',(61.4729027677276,12.9709708853385,40.0816253922032));
#197614=CARTESIAN_POINT('Ctrl Pts',(61.4731300138564,12.9717550556841,40.0819801989139));
#197615=CARTESIAN_POINT('Ctrl Pts',(61.4733501585437,12.9725147207063,40.0823239179149));
#197616=CARTESIAN_POINT('Ctrl Pts',(61.4735653344327,12.9732778859001,40.0826642303498));
#197617=CARTESIAN_POINT('Ctrl Pts',(61.4737754532575,12.9740444565829,40.0830009916099));
#197618=CARTESIAN_POINT('Ctrl Pts',(61.4760652849148,12.9823983859293,40.0866709464313));
#197619=CARTESIAN_POINT('Ctrl Pts',(61.4777556486134,12.9911623597379,40.0899175831879));
#197620=CARTESIAN_POINT('Ctrl Pts',(61.4787331403172,13.0001833616603,40.0925642067064));
#197621=CARTESIAN_POINT('Ctrl Pts',(61.4791459411337,13.0039929867894,40.0936818922529));
#197622=CARTESIAN_POINT('Ctrl Pts',(61.4794319383913,13.0078481668562,40.0946930094791));
#197623=CARTESIAN_POINT('Ctrl Pts',(61.4795843394719,13.0117365408424,40.0955863397545));
#197624=CARTESIAN_POINT('Ctrl Pts',(61.4798409790836,13.0182844654757,40.0970906856166));
#197625=CARTESIAN_POINT('Ctrl Pts',(61.4797168922659,13.0249248230168,40.0982599215483));
#197626=CARTESIAN_POINT('Ctrl Pts',(61.4791780149468,13.031591676317,40.0990497370453));
#197627=CARTESIAN_POINT('Ctrl Pts',(61.4790432956171,13.033258389642,40.0992471909196));
#197628=CARTESIAN_POINT('Ctrl Pts',(61.4788824204062,13.0349267248709,40.0994209989363));
#197629=CARTESIAN_POINT('Ctrl Pts',(61.478694553895,13.0365955947397,40.0995705982975));
#197630=CARTESIAN_POINT('Ctrl Pts',(61.4784127541283,13.0390988995427,40.0997949973393));
#197631=CARTESIAN_POINT('Ctrl Pts',(61.4780702140293,13.0416033892093,40.0999649129781));
#197632=CARTESIAN_POINT('Ctrl Pts',(61.4776657592308,13.0441057251022,40.1000786629733));
#197633=CARTESIAN_POINT('Ctrl Pts',(61.4772613044323,13.0466080609951,40.1001924129685));
#197634=CARTESIAN_POINT('Ctrl Pts',(61.4767949453823,13.0491082380621,40.10025));
#197635=CARTESIAN_POINT('Ctrl Pts',(61.4762657165317,13.0516031943521,40.10025));
#197636=CARTESIAN_POINT('Ctrl Pts',(57.7418065394567,12.257819391976,40.10025));
#197637=CARTESIAN_POINT('Ctrl Pts',(57.7435970583547,12.2493771807065,40.10025));
#197638=CARTESIAN_POINT('Ctrl Pts',(57.7460689269805,12.2411559442234,40.099578633424));
#197639=CARTESIAN_POINT('Ctrl Pts',(57.7491141258108,12.2332613533211,40.0983063763364));
#197640=CARTESIAN_POINT('Ctrl Pts',(57.7510810117996,12.2281622576305,40.0974846287991));
#197641=CARTESIAN_POINT('Ctrl Pts',(57.7532862127607,12.2231990866875,40.0964130309337));
#197642=CARTESIAN_POINT('Ctrl Pts',(57.755693185958,12.2183955094112,40.0951176960923));
#197643=CARTESIAN_POINT('Ctrl Pts',(57.7588834910513,12.212028642897,40.0934008039613));
#197644=CARTESIAN_POINT('Ctrl Pts',(57.7624328173676,12.2059457447511,40.0912909372156));
#197645=CARTESIAN_POINT('Ctrl Pts',(57.766268204371,12.2001996238494,40.0888630467851));
#197646=CARTESIAN_POINT('Ctrl Pts',(57.7681858978727,12.1973265633985,40.0876491015698));
#197647=CARTESIAN_POINT('Ctrl Pts',(57.7701751462712,12.1945375019631,40.086355856927));
#197648=CARTESIAN_POINT('Ctrl Pts',(57.7722271161469,12.1918376559067,40.084993634277));
#197649=CARTESIAN_POINT('Ctrl Pts',(57.7732531010848,12.1904877328784,40.084312522952));
#197650=CARTESIAN_POINT('Ctrl Pts',(57.7742947697605,12.1891600976128,40.0836141747073));
#197651=CARTESIAN_POINT('Ctrl Pts',(57.7753510390206,12.1878553011591,40.0828999161609));
#197652=CARTESIAN_POINT('Ctrl Pts',(57.7756151063356,12.1875291020457,40.0827213515243));
#197653=CARTESIAN_POINT('Ctrl Pts',(57.7758800862579,12.1872043300158,40.0825417925841));
#197654=CARTESIAN_POINT('Ctrl Pts',(57.7761459620051,12.1868809929891,40.082361260236));
#197655=CARTESIAN_POINT('Ctrl Pts',(57.7769435892466,12.1859109819091,40.0818196631917));
#197656=CARTESIAN_POINT('Ctrl Pts',(57.7777492785675,12.1849538875683,40.0812693052021));
#197657=CARTESIAN_POINT('Ctrl Pts',(57.7785625799463,12.1840099085251,40.0807107531874));
#197658=CARTESIAN_POINT('Ctrl Pts',(57.7842913698425,12.1773606420343,40.0767763849182));
#197659=CARTESIAN_POINT('Ctrl Pts',(57.7903843352498,12.171310022896,40.0724140586138));
#197660=CARTESIAN_POINT('Ctrl Pts',(57.7967264334406,12.1658251565853,40.067722122377));
#197661=CARTESIAN_POINT('Ctrl Pts',(57.7998023442099,12.1631650023516,40.0654465383722));
#197662=CARTESIAN_POINT('Ctrl Pts',(57.8029374300325,12.1606380046006,40.063092800068));
#197663=CARTESIAN_POINT('Ctrl Pts',(57.8061213360081,12.1582411305891,40.0606689262479));
#197664=CARTESIAN_POINT('Ctrl Pts',(57.8109956736034,12.1545716839424,40.0569581447805));
#197665=CARTESIAN_POINT('Ctrl Pts',(57.8159810988991,12.15120837322,40.0530843804605));
#197666=CARTESIAN_POINT('Ctrl Pts',(57.8210315314442,12.148149500938,40.0490800251457));
#197667=CARTESIAN_POINT('Ctrl Pts',(57.8233769784456,12.1467289448257,40.0472203818218));
#197668=CARTESIAN_POINT('Ctrl Pts',(57.8257362497573,12.1453738842979,40.0453323608818));
#197669=CARTESIAN_POINT('Ctrl Pts',(57.828105124615,12.1440853170063,40.0434201572162));
#197670=CARTESIAN_POINT('Ctrl Pts',(57.828286689539,12.1439865534006,40.0432735943397));
#197671=CARTESIAN_POINT('Ctrl Pts',(57.8284683073401,12.143888146679,40.0431268995707));
#197672=CARTESIAN_POINT('Ctrl Pts',(57.8286499766612,12.1437900963014,40.0429800745037));
#197673=CARTESIAN_POINT('Ctrl Pts',(57.831201882908,12.1424127841091,40.0409176249753));
#197674=CARTESIAN_POINT('Ctrl Pts',(57.8337650648328,12.1411075562948,40.0388310783332));
#197675=CARTESIAN_POINT('Ctrl Pts',(57.8363340693142,12.1398727334214,40.036725739981));
#197676=CARTESIAN_POINT('Ctrl Pts',(57.8455460625016,12.1354448782036,40.0291763710723));
#197677=CARTESIAN_POINT('Ctrl Pts',(57.8549032874792,12.1318862976811,40.0213310894606));
#197678=CARTESIAN_POINT('Ctrl Pts',(57.8643241951516,12.1290968783783,40.0132837551337));
#197679=CARTESIAN_POINT('Ctrl Pts',(57.8746768262695,12.1260315867866,40.0044405431349));
#197680=CARTESIAN_POINT('Ctrl Pts',(57.8851069357333,12.1238947812343,39.9953528710631));
#197681=CARTESIAN_POINT('Ctrl Pts',(57.8955352825089,12.1225979458248,39.9861103629593));
#197682=CARTESIAN_POINT('Ctrl Pts',(57.9067952798687,12.1211976890439,39.9761307737602));
#197683=CARTESIAN_POINT('Ctrl Pts',(57.9180543443172,12.1207764137882,39.9659696936065));
#197684=CARTESIAN_POINT('Ctrl Pts',(57.9292311407202,12.121277094833,39.9557128217568));
#197685=CARTESIAN_POINT('Ctrl Pts',(57.9403141752885,12.1217735756784,39.9455419945202));
#197686=CARTESIAN_POINT('Ctrl Pts',(57.9513177099548,12.1231769533525,39.9352756289361));
#197687=CARTESIAN_POINT('Ctrl Pts',(57.9621601888122,12.1254815933784,39.92499));
#197688=CARTESIAN_POINT('Origin',(-0.00316857416806234,0.0149069694351821,
39.92499));
#197689=CARTESIAN_POINT('Ctrl Pts',(61.4699285681956,13.0814171332224,40.10025));
#197690=CARTESIAN_POINT('Ctrl Pts',(61.468139314985,13.0898176309843,40.10025));
#197691=CARTESIAN_POINT('Ctrl Pts',(61.465664225629,13.097994011884,40.0995859581841));
#197692=CARTESIAN_POINT('Ctrl Pts',(61.4626133761157,13.1058430982609,40.0983275959618));
#197693=CARTESIAN_POINT('Ctrl Pts',(61.4606640285135,13.1108582907973,40.0975235624066));
#197694=CARTESIAN_POINT('Ctrl Pts',(61.4584804838814,13.1157402208608,40.0964777059489));
#197695=CARTESIAN_POINT('Ctrl Pts',(61.4560986543957,13.12046667152,40.095214991596));
#197696=CARTESIAN_POINT('Ctrl Pts',(61.4528479350655,13.1269173282999,40.09349163987));
#197697=CARTESIAN_POINT('Ctrl Pts',(61.4492231901485,13.1330744923999,40.091364392163));
#197698=CARTESIAN_POINT('Ctrl Pts',(61.4453029499362,13.1388835356729,40.0889118607712));
#197699=CARTESIAN_POINT('Ctrl Pts',(61.4433428298301,13.1417880573095,40.0876855950754));
#197700=CARTESIAN_POINT('Ctrl Pts',(61.4413087943565,13.1446057534054,40.0863782327526));
#197701=CARTESIAN_POINT('Ctrl Pts',(61.4392103574,13.1473312571584,40.0850006373333));
#197702=CARTESIAN_POINT('Ctrl Pts',(61.4381611389218,13.148694009035,40.0843118396237));
#197703=CARTESIAN_POINT('Ctrl Pts',(61.4370958165018,13.1500337298695,40.0836054919164));
#197704=CARTESIAN_POINT('Ctrl Pts',(61.436015557062,13.1513498559435,40.0828829920417));
#197705=CARTESIAN_POINT('Ctrl Pts',(61.435745492202,13.151678887462,40.0827023670731));
#197706=CARTESIAN_POINT('Ctrl Pts',(61.4354744937032,13.1520064446712,40.0825207326932));
#197707=CARTESIAN_POINT('Ctrl Pts',(61.435202579648,13.152332519496,40.0823381109275));
#197708=CARTESIAN_POINT('Ctrl Pts',(61.4343868374822,13.1533107439703,40.0817902456303));
#197709=CARTESIAN_POINT('Ctrl Pts',(61.4335628556744,13.1542756251689,40.0812334935553));
#197710=CARTESIAN_POINT('Ctrl Pts',(61.4327311191548,13.1552269612796,40.0806684524227));
#197711=CARTESIAN_POINT('Ctrl Pts',(61.4269833037496,13.1618012840653,40.0767636676137));
#197712=CARTESIAN_POINT('Ctrl Pts',(61.4208780249712,13.1677829516029,40.0724404510888));
#197713=CARTESIAN_POINT('Ctrl Pts',(61.4145287289054,13.1732071947987,40.0677949937409));
#197714=CARTESIAN_POINT('Ctrl Pts',(61.4113731461892,13.1759030287778,40.0654862141905));
#197715=CARTESIAN_POINT('Ctrl Pts',(61.4081566864226,13.1784610805508,40.0630972003216));
#197716=CARTESIAN_POINT('Ctrl Pts',(61.4048902384028,13.1808848153819,40.0606363359906));
#197717=CARTESIAN_POINT('Ctrl Pts',(61.3976839661819,13.1862319364375,40.0552073017123));
#197718=CARTESIAN_POINT('Ctrl Pts',(61.3902425685154,13.1909347237336,40.0494204304519));
#197719=CARTESIAN_POINT('Ctrl Pts',(61.3827095020468,13.1949697809162,40.0434049749851));
#197720=CARTESIAN_POINT('Ctrl Pts',(61.3799575778688,13.1964438381897,40.0412074532442));
#197721=CARTESIAN_POINT('Ctrl Pts',(61.377194044862,13.1978367193484,40.0389814735788));
#197722=CARTESIAN_POINT('Ctrl Pts',(61.374423615274,13.1991508816431,40.0367321210016));
#197723=CARTESIAN_POINT('Ctrl Pts',(61.3651180354457,13.2035650137306,40.0291767837143));
#197724=CARTESIAN_POINT('Ctrl Pts',(61.3556720404061,13.2071113921929,40.0213235332581));
#197725=CARTESIAN_POINT('Ctrl Pts',(61.3461671566372,13.2098890888164,40.0132649215866));
#197726=CARTESIAN_POINT('Ctrl Pts',(61.3357201634477,13.2129421064455,40.0044075527543));
#197727=CARTESIAN_POINT('Ctrl Pts',(61.3252014297054,13.2150668515146,39.9953016253732));
#197728=CARTESIAN_POINT('Ctrl Pts',(61.3146904872832,13.2163502251969,39.9860353422374));
#197729=CARTESIAN_POINT('Ctrl Pts',(61.3033697519365,13.2177324736408,39.9760551582714));
#197730=CARTESIAN_POINT('Ctrl Pts',(61.2920568939748,13.2181390006405,39.9658879738179));
#197731=CARTESIAN_POINT('Ctrl Pts',(61.2808338148893,13.2176240288382,39.9556174643282));
#197732=CARTESIAN_POINT('Ctrl Pts',(61.2697622852632,13.217116010894,39.9454856413923));
#197733=CARTESIAN_POINT('Ctrl Pts',(61.2587767401965,13.2157108393287,39.9352519465122));
#197734=CARTESIAN_POINT('Ctrl Pts',(61.2479592423879,13.2134115091886,39.92499));
#197735=CARTESIAN_POINT('Ctrl Pts',(57.8829458346107,12.498155829258,39.92499));
#197736=CARTESIAN_POINT('Ctrl Pts',(57.8725934298277,12.4959553576923,39.9348107241715));
#197737=CARTESIAN_POINT('Ctrl Pts',(57.8624518082053,12.4929462656001,39.9446038383155));
#197738=CARTESIAN_POINT('Ctrl Pts',(57.8525735736588,12.4891531124825,39.9543158069363));
#197739=CARTESIAN_POINT('Ctrl Pts',(57.8430352690785,12.485490489411,39.9636935671367));
#197740=CARTESIAN_POINT('Ctrl Pts',(57.833741385314,12.4810963130892,39.972996832096));
#197741=CARTESIAN_POINT('Ctrl Pts',(57.8247536185241,12.4759491415402,39.9821731151303));
#197742=CARTESIAN_POINT('Ctrl Pts',(57.8162573641132,12.471083452432,39.990847576432));
#197743=CARTESIAN_POINT('Ctrl Pts',(57.8080338771698,12.4655444244744,39.9994093733814));
#197744=CARTESIAN_POINT('Ctrl Pts',(57.8001616710205,12.4592813303353,40.0077966115809));
#197745=CARTESIAN_POINT('Ctrl Pts',(57.7929115012229,12.4535131257044,40.0155211172564));
#197746=CARTESIAN_POINT('Ctrl Pts',(57.7859589019109,12.447130377453,40.0230979940993));
#197747=CARTESIAN_POINT('Ctrl Pts',(57.7793958734443,12.4400707995013,40.0304554104721));
#197748=CARTESIAN_POINT('Ctrl Pts',(57.7774389108381,12.4379657758621,40.0326492435163));
#197749=CARTESIAN_POINT('Ctrl Pts',(57.7755168276803,12.4358004306458,40.0348233715052));
#197750=CARTESIAN_POINT('Ctrl Pts',(57.7736327324862,12.4335727482754,40.0369753512355));
#197751=CARTESIAN_POINT('Ctrl Pts',(57.7717678881029,12.4313678273303,40.0391053430352));
#197752=CARTESIAN_POINT('Ctrl Pts',(57.7699419852107,12.4291043014742,40.041211089324));
#197753=CARTESIAN_POINT('Ctrl Pts',(57.7681599326869,12.4267829461791,40.0432881154904));
#197754=CARTESIAN_POINT('Ctrl Pts',(57.7680360122396,12.4266215236718,40.043432547828));
#197755=CARTESIAN_POINT('Ctrl Pts',(57.7679122920636,12.4264598236889,40.0435768364421));
#197756=CARTESIAN_POINT('Ctrl Pts',(57.7677887733171,12.4262978456301,40.0437209807855));
#197757=CARTESIAN_POINT('Ctrl Pts',(57.7623732589831,12.4191961341592,40.0500407968421));
#197758=CARTESIAN_POINT('Ctrl Pts',(57.7573864007558,12.4115418213379,40.0560490279346));
#197759=CARTESIAN_POINT('Ctrl Pts',(57.7529408672214,12.4033632485677,40.0616647108616));
#197760=CARTESIAN_POINT('Ctrl Pts',(57.7487968573387,12.3957393973195,40.0668995033488));
#197761=CARTESIAN_POINT('Ctrl Pts',(57.7451230952908,12.3876591848383,40.0717933267485));
#197762=CARTESIAN_POINT('Ctrl Pts',(57.7420400166293,12.3791488184473,40.0762460303076));
#197763=CARTESIAN_POINT('Ctrl Pts',(57.7409121865685,12.3760356163212,40.077874886875));
#197764=CARTESIAN_POINT('Ctrl Pts',(57.7398637084259,12.3728649408017,40.0794443522248));
#197765=CARTESIAN_POINT('Ctrl Pts',(57.7389016204183,12.3696384996591,40.0809482021492));
#197766=CARTESIAN_POINT('Ctrl Pts',(57.738670270393,12.3688626483501,40.0813098278168));
#197767=CARTESIAN_POINT('Ctrl Pts',(57.7384441015869,12.3680830188489,40.0816679525672));
#197768=CARTESIAN_POINT('Ctrl Pts',(57.7382232068823,12.3672997100614,40.082022419258));
#197769=CARTESIAN_POINT('Ctrl Pts',(57.7380092151371,12.3665408796735,40.0823658088648));
#197770=CARTESIAN_POINT('Ctrl Pts',(57.7378001730067,12.365778596386,40.0827057654616));
#197771=CARTESIAN_POINT('Ctrl Pts',(57.7375961641251,12.3650129538219,40.0830421470151));
#197772=CARTESIAN_POINT('Ctrl Pts',(57.7353610110592,12.3566244546988,40.0867275956806));
#197773=CARTESIAN_POINT('Ctrl Pts',(57.7337289586986,12.3478270988449,40.089982343203));
#197774=CARTESIAN_POINT('Ctrl Pts',(57.7328090548569,12.3387746477733,40.0926299529355));
#197775=CARTESIAN_POINT('Ctrl Pts',(57.7324275433144,12.3350203264891,40.0937279956084));
#197776=CARTESIAN_POINT('Ctrl Pts',(57.7321681942504,12.3312224025075,40.0947220371802));
#197777=CARTESIAN_POINT('Ctrl Pts',(57.7320371357771,12.3273926324681,40.0956014538692));
#197778=CARTESIAN_POINT('Ctrl Pts',(57.7318136018936,12.3208605605759,40.097101390674));
#197779=CARTESIAN_POINT('Ctrl Pts',(57.7319651225404,12.3142375182607,40.0982667904316));
#197780=CARTESIAN_POINT('Ctrl Pts',(57.7325238621659,12.3075887924647,40.0990539325582));
#197781=CARTESIAN_POINT('Ctrl Pts',(57.7328032319787,12.3042644295667,40.0994475036216));
#197782=CARTESIAN_POINT('Ctrl Pts',(57.7331858342648,12.3009338801479,40.0997467259952));
#197783=CARTESIAN_POINT('Ctrl Pts',(57.7336757296049,12.2976053572247,40.0999473488896));
#197784=CARTESIAN_POINT('Ctrl Pts',(57.734165624945,12.2942768343015,40.100147971784));
#197785=CARTESIAN_POINT('Ctrl Pts',(57.7347627876419,12.2909503756171,40.10025));
#197786=CARTESIAN_POINT('Ctrl Pts',(57.7354693911206,12.2876333308464,40.10025));
#197787=CARTESIAN_POINT('Origin',(57.9461901084063,6.07506605172221,39.92499));
#197788=CARTESIAN_POINT('Ctrl Pts',(62.333439457262,6.35995915837717,39.92499));
#197789=CARTESIAN_POINT('Ctrl Pts',(62.3439916622903,6.36106823981704,39.9348354642019));
#197790=CARTESIAN_POINT('Ctrl Pts',(62.3544250468349,6.3630066345261,39.944644082846));
#197791=CARTESIAN_POINT('Ctrl Pts',(62.3646844024058,6.36575328117367,39.9543641760333));
#197792=CARTESIAN_POINT('Ctrl Pts',(62.374610390011,6.36841067816039,39.9637684240714));
#197793=CARTESIAN_POINT('Ctrl Pts',(62.3843747009654,6.37182505343089,39.9730909636397));
#197794=CARTESIAN_POINT('Ctrl Pts',(62.3939185239082,6.37602267870788,39.9822808977141));
#197795=CARTESIAN_POINT('Ctrl Pts',(62.4029463927373,6.37999337374501,39.9909740094648));
#197796=CARTESIAN_POINT('Ctrl Pts',(62.4117778192049,6.38466529101412,39.9995492764998));
#197797=CARTESIAN_POINT('Ctrl Pts',(62.4203406170097,6.3900963181494,40.007946232869));
#197798=CARTESIAN_POINT('Ctrl Pts',(62.4282275730652,6.39509868692286,40.0156804369683));
#197799=CARTESIAN_POINT('Ctrl Pts',(62.4358870734644,6.40074541103499,40.0232638017414));
#197800=CARTESIAN_POINT('Ctrl Pts',(62.4432347045248,6.40710777594438,40.0306257269957));
#197801=CARTESIAN_POINT('Ctrl Pts',(62.4453659729914,6.40895325615324,40.0327611416646));
#197802=CARTESIAN_POINT('Ctrl Pts',(62.4474707870406,6.41085910953056,40.0348777427268));
#197803=CARTESIAN_POINT('Ctrl Pts',(62.4495465125726,6.41282747575996,40.03697331687));
#197804=CARTESIAN_POINT('Ctrl Pts',(62.4517967325057,6.41496131130661,40.039245053974));
#197805=CARTESIAN_POINT('Ctrl Pts',(62.4540103788123,6.41716486079117,40.041487875195));
#197806=CARTESIAN_POINT('Ctrl Pts',(62.4561838467663,6.41943986047027,40.04369857016));
#197807=CARTESIAN_POINT('Ctrl Pts',(62.4621489466212,6.42568361494116,40.0497658398386));
#197808=CARTESIAN_POINT('Ctrl Pts',(62.467772647785,6.4324873305955,40.0555581699984));
#197809=CARTESIAN_POINT('Ctrl Pts',(62.4729574661287,6.43981562609108,40.0609828468885));
#197810=CARTESIAN_POINT('Ctrl Pts',(62.4777012934231,6.44652061860752,40.0659461317308));
#197811=CARTESIAN_POINT('Ctrl Pts',(62.4820661824991,6.45366385825773,40.0706039980712));
#197812=CARTESIAN_POINT('Ctrl Pts',(62.4859635700134,6.46124910257484,40.0748843180611));
#197813=CARTESIAN_POINT('Ctrl Pts',(62.4878779540287,6.46497494980442,40.0769867972575));
#197814=CARTESIAN_POINT('Ctrl Pts',(62.4896790353534,6.4688074965091,40.0789976708177));
#197815=CARTESIAN_POINT('Ctrl Pts',(62.4913529701966,6.47274712615487,40.08090504915));
#197816=CARTESIAN_POINT('Ctrl Pts',(62.4916705830287,6.47349463250775,40.0812669556104));
#197817=CARTESIAN_POINT('Ctrl Pts',(62.4919834280839,6.47424649074103,40.0816253922032));
#197818=CARTESIAN_POINT('Ctrl Pts',(62.4922913974558,6.47500261163075,40.0819801989139));
#197819=CARTESIAN_POINT('Ctrl Pts',(62.4925897427848,6.47573510374267,40.0823239179149));
#197820=CARTESIAN_POINT('Ctrl Pts',(62.4928835124027,6.47647159623262,40.0826642303498));
#197821=CARTESIAN_POINT('Ctrl Pts',(62.4931726086302,6.47721200416321,40.0830009916099));
#197822=CARTESIAN_POINT('Ctrl Pts',(62.4963231197467,6.48528081722581,40.0866709464311));
#197823=CARTESIAN_POINT('Ctrl Pts',(62.4989203081702,6.49382008994854,40.0899175831876));
#197824=CARTESIAN_POINT('Ctrl Pts',(62.5008353965403,6.50268949817224,40.0925642067059));
#197825=CARTESIAN_POINT('Ctrl Pts',(62.5016441502512,6.50643510434183,40.0936818922526));
#197826=CARTESIAN_POINT('Ctrl Pts',(62.5023315568341,6.51023927047563,40.094693009479));
#197827=CARTESIAN_POINT('Ctrl Pts',(62.5028895688031,6.51409041329205,40.0955863397546));
#197828=CARTESIAN_POINT('Ctrl Pts',(62.5038292470156,6.52057564156488,40.0970906856166));
#197829=CARTESIAN_POINT('Ctrl Pts',(62.5043999463278,6.52719259313698,40.0982599215483));
#197830=CARTESIAN_POINT('Ctrl Pts',(62.5045608969644,6.53387925273521,40.0990497370454));
#197831=CARTESIAN_POINT('Ctrl Pts',(62.5046011346236,6.53555091763477,40.0992471909196));
#197832=CARTESIAN_POINT('Ctrl Pts',(62.5046155292217,6.5372269295873,40.0994209989363));
#197833=CARTESIAN_POINT('Ctrl Pts',(62.5046031362658,6.53890629460996,40.0995705982975));
#197834=CARTESIAN_POINT('Ctrl Pts',(62.5045845468319,6.54142534214396,40.0997949973393));
#197835=CARTESIAN_POINT('Ctrl Pts',(62.5045056736598,6.5439519171443,40.0999649129781));
#197836=CARTESIAN_POINT('Ctrl Pts',(62.5043649998326,6.54648282201788,40.1000786629733));
#197837=CARTESIAN_POINT('Ctrl Pts',(62.5042243260054,6.54901372689146,40.1001924129685));
#197838=CARTESIAN_POINT('Ctrl Pts',(62.5040218613862,6.55154895552175,40.10025));
#197839=CARTESIAN_POINT('Ctrl Pts',(62.5037563256536,6.55408556365861,40.10025));
#197840=CARTESIAN_POINT('Ctrl Pts',(58.7067819056644,6.15500747092236,40.10025));
#197841=CARTESIAN_POINT('Ctrl Pts',(58.7076801645418,6.14642434678071,40.10025));
#197842=CARTESIAN_POINT('Ctrl Pts',(58.7092791387969,6.13798976646238,40.099578633424));
#197843=CARTESIAN_POINT('Ctrl Pts',(58.7114824462543,6.12982011300101,40.0983063763365));
#197844=CARTESIAN_POINT('Ctrl Pts',(58.7129055567993,6.1245433551203,40.0974846287991));
#197845=CARTESIAN_POINT('Ctrl Pts',(58.7145798848071,6.11937686667937,40.0964130309337));
#197846=CARTESIAN_POINT('Ctrl Pts',(58.7164715618026,6.11434800669255,40.0951176960923));
#197847=CARTESIAN_POINT('Ctrl Pts',(58.7189788712982,6.10768254085054,40.0934008039614));
#197848=CARTESIAN_POINT('Ctrl Pts',(58.7218729180382,6.10126195983161,40.0912909372156));
#197849=CARTESIAN_POINT('Ctrl Pts',(58.7250866612027,6.09514640967194,40.0888630467851));
#197850=CARTESIAN_POINT('Ctrl Pts',(58.7266935327849,6.0920886345921,40.0876491015698));
#197851=CARTESIAN_POINT('Ctrl Pts',(58.7283803475667,6.08910691884893,40.0863558569271));
#197852=CARTESIAN_POINT('Ctrl Pts',(58.7301388657774,6.08620737357386,40.0849936342771));
#197853=CARTESIAN_POINT('Ctrl Pts',(58.7310181248828,6.08475760093632,40.0843125229521));
#197854=CARTESIAN_POINT('Ctrl Pts',(58.7319153115143,6.08332835456963,40.0836141747074));
#197855=CARTESIAN_POINT('Ctrl Pts',(58.7328294060528,6.0819202957249,40.0828999161609));
#197856=CARTESIAN_POINT('Ctrl Pts',(58.7330579296874,6.08156828101372,40.0827213515243));
#197857=CARTESIAN_POINT('Ctrl Pts',(58.7332875101007,6.08121759017488,40.0825417925841));
#197858=CARTESIAN_POINT('Ctrl Pts',(58.7335181314302,6.08086823283901,40.082361260236));
#197859=CARTESIAN_POINT('Ctrl Pts',(58.7342099954187,6.0798201608314,40.0818196631917));
#197860=CARTESIAN_POINT('Ctrl Pts',(58.7349112274886,6.07878409208698,40.0812693052021));
#197861=CARTESIAN_POINT('Ctrl Pts',(58.7356214008386,6.07776027111639,40.0807107531874));
#197862=CARTESIAN_POINT('Ctrl Pts',(58.7406237702163,6.07054860839872,40.076776384918));
#197863=CARTESIAN_POINT('Ctrl Pts',(58.7460508958015,6.06389424687405,40.0724140586135));
#197864=CARTESIAN_POINT('Ctrl Pts',(58.7517849266684,6.05777649745699,40.0677221223764));
#197865=CARTESIAN_POINT('Ctrl Pts',(58.7545659254424,6.05480939560084,40.0654465383718));
#197866=CARTESIAN_POINT('Ctrl Pts',(58.757419693745,6.05196853530499,40.0630928000678));
#197867=CARTESIAN_POINT('Ctrl Pts',(58.7603356163932,6.04925198282152,40.0606689262479));
#197868=CARTESIAN_POINT('Ctrl Pts',(58.7647996902381,6.04509313076913,40.0569581447805));
#197869=CARTESIAN_POINT('Ctrl Pts',(58.7694062431512,6.04122712576998,40.0530843804605));
#197870=CARTESIAN_POINT('Ctrl Pts',(58.7741092696794,6.03765709635755,40.0490800251457));
#197871=CARTESIAN_POINT('Ctrl Pts',(58.7762933795293,6.03599915622953,40.0472203818218));
#197872=CARTESIAN_POINT('Ctrl Pts',(58.7784980841112,6.03440490786043,40.0453323608818));
#197873=CARTESIAN_POINT('Ctrl Pts',(58.7807192900658,6.03287578462677,40.0434201572162));
#197874=CARTESIAN_POINT('Ctrl Pts',(58.7808895367502,6.03275858335596,40.0432735943397));
#197875=CARTESIAN_POINT('Ctrl Pts',(58.7810598733266,6.03264173148699,40.0431268995707));
#197876=CARTESIAN_POINT('Ctrl Pts',(58.7812302983889,6.0325252286247,40.0429800745037));
#197877=CARTESIAN_POINT('Ctrl Pts',(58.7836242566994,6.03088871465425,40.0409176249753));
#197878=CARTESIAN_POINT('Ctrl Pts',(58.7860369637877,6.02932271154683,40.0388310783332));
#197879=CARTESIAN_POINT('Ctrl Pts',(58.7884628208564,6.02782611907177,40.036725739981));
#197880=CARTESIAN_POINT('Ctrl Pts',(58.7971615128802,6.02245960461633,40.0291763710719));
#197881=CARTESIAN_POINT('Ctrl Pts',(58.8060955050474,6.01794242202273,40.0213310894597));
#197882=CARTESIAN_POINT('Ctrl Pts',(58.8151732302893,6.01418353044908,40.0132837551324));
#197883=CARTESIAN_POINT('Ctrl Pts',(58.8251487383915,6.01005288622384,40.0044405431332));
#197884=CARTESIAN_POINT('Ctrl Pts',(58.8352983536241,6.0068375430019,39.9953528710611));
#197885=CARTESIAN_POINT('Ctrl Pts',(58.8455340166129,6.0044577527297,39.9861103629569));
#197886=CARTESIAN_POINT('Ctrl Pts',(58.8565859638396,6.00188817648163,39.9761307737576));
#197887=CARTESIAN_POINT('Ctrl Pts',(58.8677393147001,6.00029231631139,39.9659696936038));
#197888=CARTESIAN_POINT('Ctrl Pts',(58.8789072188634,5.99962196122093,39.9557128217539));
#197889=CARTESIAN_POINT('Ctrl Pts',(58.8899814357874,5.99895722972078,39.9455419945182));
#197890=CARTESIAN_POINT('Ctrl Pts',(58.9010713848501,5.99920273697604,39.9352756289351));
#197891=CARTESIAN_POINT('Ctrl Pts',(58.9120953679531,6.00036140428966,39.92499));
#197892=CARTESIAN_POINT('Origin',(-0.00159301378019881,0.0151565136854119,
39.92499));
#197893=CARTESIAN_POINT('Ctrl Pts',(62.5005702980932,6.58439859102944,40.10025));
#197894=CARTESIAN_POINT('Ctrl Pts',(62.4996689377206,6.59294009787364,40.10025));
#197895=CARTESIAN_POINT('Ctrl Pts',(62.4980620716938,6.60133040498961,40.0995859581842));
#197896=CARTESIAN_POINT('Ctrl Pts',(62.4958483879906,6.60945539386096,40.0983275959621));
#197897=CARTESIAN_POINT('Ctrl Pts',(62.4944339494872,6.61464687495747,40.0975235624068));
#197898=CARTESIAN_POINT('Ctrl Pts',(62.4927726671884,6.61973030386259,40.096477705949));
#197899=CARTESIAN_POINT('Ctrl Pts',(62.4908979342377,6.62467983150676,40.0952149915961));
#197900=CARTESIAN_POINT('Ctrl Pts',(62.4883392999284,6.63143494361006,40.0934916398701));
#197901=CARTESIAN_POINT('Ctrl Pts',(62.4853780106449,6.63793726713676,40.0913643921631));
#197902=CARTESIAN_POINT('Ctrl Pts',(62.482086456285,6.64412426454807,40.0889118607713));
#197903=CARTESIAN_POINT('Ctrl Pts',(62.4804406791051,6.64721776325373,40.0876855950754));
#197904=CARTESIAN_POINT('Ctrl Pts',(62.4787123157335,6.65023263831788,40.0863782327527));
#197905=CARTESIAN_POINT('Ctrl Pts',(62.4769102669531,6.65316255786655,40.0850006373334));
#197906=CARTESIAN_POINT('Ctrl Pts',(62.476009242563,6.65462751764088,40.0843118396237));
#197907=CARTESIAN_POINT('Ctrl Pts',(62.4750897950507,6.65607125585996,40.0836054919164));
#197908=CARTESIAN_POINT('Ctrl Pts',(62.4741530260211,6.65749308991676,40.0828829920418));
#197909=CARTESIAN_POINT('Ctrl Pts',(62.4739188337637,6.65784854843096,40.0827023670731));
#197910=CARTESIAN_POINT('Ctrl Pts',(62.4736835588747,6.65820263830418,40.0825207326933));
#197911=CARTESIAN_POINT('Ctrl Pts',(62.4734472184935,6.65855534961529,40.0823381109275));
#197912=CARTESIAN_POINT('Ctrl Pts',(62.4727381973496,6.65961348354863,40.0817902456303));
#197913=CARTESIAN_POINT('Ctrl Pts',(62.4720195869493,6.66065920857923,40.0812334935553));
#197914=CARTESIAN_POINT('Ctrl Pts',(62.4712918484711,6.66169227331133,40.0806684524227));
#197915=CARTESIAN_POINT('Ctrl Pts',(62.4662627240579,6.66883139158041,40.0767636676137));
#197916=CARTESIAN_POINT('Ctrl Pts',(62.460816145151,6.67541846632582,40.0724404510889));
#197917=CARTESIAN_POINT('Ctrl Pts',(62.4550686189991,6.68147667711046,40.067794993741));
#197918=CARTESIAN_POINT('Ctrl Pts',(62.4522121142782,6.68448759124099,40.0654862141906));
#197919=CARTESIAN_POINT('Ctrl Pts',(62.4492806638355,6.6873678413353,40.0630972003216));
#197920=CARTESIAN_POINT('Ctrl Pts',(62.4462854590369,6.69011973548525,40.0606363359906));
#197921=CARTESIAN_POINT('Ctrl Pts',(62.4396775898762,6.69619082501338,40.0552073017123));
#197922=CARTESIAN_POINT('Ctrl Pts',(62.4327685320937,6.70164568781131,40.0494204304519));
#197923=CARTESIAN_POINT('Ctrl Pts',(62.425698510878,6.7064460603901,40.0434049749851));
#197924=CARTESIAN_POINT('Ctrl Pts',(62.4231157429702,6.70819969702901,40.0412074532442));
#197925=CARTESIAN_POINT('Ctrl Pts',(62.4205129446134,6.70987381569732,40.0389814735788));
#197926=CARTESIAN_POINT('Ctrl Pts',(62.4178950590936,6.71147036762092,40.0367321210016));
#197927=CARTESIAN_POINT('Ctrl Pts',(62.409101858649,6.71683301659034,40.0291767837143));
#197928=CARTESIAN_POINT('Ctrl Pts',(62.4000783072493,6.72134734296589,40.021323533258));
#197929=CARTESIAN_POINT('Ctrl Pts',(62.3909158405875,6.7251033539706,40.0132649215865));
#197930=CARTESIAN_POINT('Ctrl Pts',(62.3808452043606,6.72923165499357,40.0044075527542));
#197931=CARTESIAN_POINT('Ctrl Pts',(62.370606189679,6.73244426756049,39.9953016253731));
#197932=CARTESIAN_POINT('Ctrl Pts',(62.3602869763777,6.73481930344629,39.9860353422371));
#197933=CARTESIAN_POINT('Ctrl Pts',(62.349172741509,6.73737731885751,39.976055158271));
#197934=CARTESIAN_POINT('Ctrl Pts',(62.3379643502091,6.73896413451758,39.9658879738172));
#197935=CARTESIAN_POINT('Ctrl Pts',(62.3267489231138,6.73962511499463,39.9556174643272));
#197936=CARTESIAN_POINT('Ctrl Pts',(62.315684942151,6.74027717000357,39.9454856413917));
#197937=CARTESIAN_POINT('Ctrl Pts',(62.304612696626,6.74002799825903,39.935251946512));
#197938=CARTESIAN_POINT('Ctrl Pts',(62.293614112757,6.73887200051249,39.92499));
#197939=CARTESIAN_POINT('Ctrl Pts',(58.8722700234481,6.37927424642498,39.92499));
#197940=CARTESIAN_POINT('Ctrl Pts',(58.8617443183096,6.37816795023576,39.9348107241724));
#197941=CARTESIAN_POINT('Ctrl Pts',(58.8513437177784,6.37623543038788,39.9446038383172));
#197942=CARTESIAN_POINT('Ctrl Pts',(58.8411231047672,6.37349561323652,39.9543158069389));
#197943=CARTESIAN_POINT('Ctrl Pts',(58.8312542036559,6.37085007871718,39.9636935671396));
#197944=CARTESIAN_POINT('Ctrl Pts',(58.8215519162604,6.36745144954042,39.9729968320994));
#197945=CARTESIAN_POINT('Ctrl Pts',(58.8120753594649,6.36327195218611,39.9821731151341));
#197946=CARTESIAN_POINT('Ctrl Pts',(58.8031170454193,6.35932101824877,39.9908475764358));
#197947=CARTESIAN_POINT('Ctrl Pts',(58.7943596215174,6.35467192211852,39.9994093733852));
#197948=CARTESIAN_POINT('Ctrl Pts',(58.7858758685314,6.34926600747549,40.0077966115847));
#197949=CARTESIAN_POINT('Ctrl Pts',(58.778062474357,6.34428725078029,40.01552111726));
#197950=CARTESIAN_POINT('Ctrl Pts',(58.7704807832456,6.33866621241343,40.0230979941026));
#197951=CARTESIAN_POINT('Ctrl Pts',(58.7632157809012,6.33233133084835,40.0304554104753));
#197952=CARTESIAN_POINT('Ctrl Pts',(58.7610495038559,6.33044239704361,40.0326492435184));
#197953=CARTESIAN_POINT('Ctrl Pts',(58.7589116098638,6.32848982621457,40.0348233715062));
#197954=CARTESIAN_POINT('Ctrl Pts',(58.7568049797265,6.32647128889757,40.0369753512356));
#197955=CARTESIAN_POINT('Ctrl Pts',(58.7547198741579,6.32447337605771,40.0391053430352));
#197956=CARTESIAN_POINT('Ctrl Pts',(58.7526673708734,6.32241310885643,40.041211089324));
#197957=CARTESIAN_POINT('Ctrl Pts',(58.7506524329182,6.32029074540037,40.0432881154904));
#197958=CARTESIAN_POINT('Ctrl Pts',(58.7505123180733,6.32014316039632,40.043432547828));
#197959=CARTESIAN_POINT('Ctrl Pts',(58.7503723733987,6.31999527850274,40.0435768364421));
#197960=CARTESIAN_POINT('Ctrl Pts',(58.7502325999832,6.31984709900144,40.0437209807855));
#197961=CARTESIAN_POINT('Ctrl Pts',(58.7441044214169,6.31335036684033,40.050040796842));
#197962=CARTESIAN_POINT('Ctrl Pts',(58.7383447881643,6.30625925377274,40.0560490279344));
#197963=CARTESIAN_POINT('Ctrl Pts',(58.7330687140843,6.29859016886878,40.0616647108614));
#197964=CARTESIAN_POINT('Ctrl Pts',(58.7281504960664,6.29144124886035,40.0668995033484));
#197965=CARTESIAN_POINT('Ctrl Pts',(58.7236522470779,6.28378931333009,40.071793326748));
#197966=CARTESIAN_POINT('Ctrl Pts',(58.7196964823232,6.27564783709148,40.076246030307));
#197967=CARTESIAN_POINT('Ctrl Pts',(58.7182494123992,6.2726695797551,40.0778748868747));
#197968=CARTESIAN_POINT('Ctrl Pts',(58.7168752520898,6.26962586933659,40.0794443522247));
#197969=CARTESIAN_POINT('Ctrl Pts',(58.7155811795664,6.26651766855671,40.0809482021492));
#197970=CARTESIAN_POINT('Ctrl Pts',(58.7152699983557,6.26577025010498,40.0813098278168));
#197971=CARTESIAN_POINT('Ctrl Pts',(58.7149635750523,6.26501853257358,40.0816679525672));
#197972=CARTESIAN_POINT('Ctrl Pts',(58.7146620123681,6.2642626046176,40.082022419258));
#197973=CARTESIAN_POINT('Ctrl Pts',(58.7143698735178,6.26353029941025,40.0823658088648));
#197974=CARTESIAN_POINT('Ctrl Pts',(58.7140822962415,6.26279404284295,40.0827057654616));
#197975=CARTESIAN_POINT('Ctrl Pts',(58.7137993735012,6.26205391928379,40.0830421470151));
#197976=CARTESIAN_POINT('Ctrl Pts',(58.7106996279153,6.2539450103517,40.0867275956806));
#197977=CARTESIAN_POINT('Ctrl Pts',(58.70815694202,6.24536644325887,40.089982343203));
#197978=CARTESIAN_POINT('Ctrl Pts',(58.7062958387085,6.23645973859628,40.0926299529355));
#197979=CARTESIAN_POINT('Ctrl Pts',(58.7055239836916,6.23276586269223,40.0937279956084));
#197980=CARTESIAN_POINT('Ctrl Pts',(58.7048690642116,6.22901585349474,40.0947220371802));
#197981=CARTESIAN_POINT('Ctrl Pts',(58.7043384037134,6.22522076267719,40.0956014538692));
#197982=CARTESIAN_POINT('Ctrl Pts',(58.7034333069352,6.21874783981155,40.097101390674));
#197983=CARTESIAN_POINT('Ctrl Pts',(58.7028917011006,6.21214524099482,40.0982667904316));
#197984=CARTESIAN_POINT('Ctrl Pts',(58.7027523988018,6.20547453341993,40.0990539325582));
#197985=CARTESIAN_POINT('Ctrl Pts',(58.7026827476524,6.20213917963249,40.0994475036216));
#197986=CARTESIAN_POINT('Ctrl Pts',(58.7027151167905,6.19878688248287,40.0997467259952));
#197987=CARTESIAN_POINT('Ctrl Pts',(58.7028544030466,6.19542538554944,40.0999473488896));
#197988=CARTESIAN_POINT('Ctrl Pts',(58.7029936893027,6.19206388861602,40.100147971784));
#197989=CARTESIAN_POINT('Ctrl Pts',(58.7032398710655,6.18869323212136,40.10025));
#197990=CARTESIAN_POINT('Ctrl Pts',(58.703595878104,6.18532049829319,40.10025));
#197991=CARTESIAN_POINT('Origin',(61.0544000815101,-6.73632490863785,39.1925554495077));
#197992=CARTESIAN_POINT('Origin',(61.0983782637162,-6.74099917687776,39.1160373285247));
#197993=CARTESIAN_POINT('Origin',(60.9730100652054,-6.72777047351124,39.3343017080178));
#197994=CARTESIAN_POINT('Ctrl Pts',(60.8636883187845,-6.7157078966941,39.2708017080178));
#197995=CARTESIAN_POINT('Ctrl Pts',(60.8773920302461,-6.59002106156467,
39.2710850691866));
#197996=CARTESIAN_POINT('Ctrl Pts',(60.9862851800404,-6.60146619279947,
39.3343017080178));
#197997=CARTESIAN_POINT('Ctrl Pts',(60.818916972731,-6.71111871849805,39.3487519293518));
#197998=CARTESIAN_POINT('Ctrl Pts',(60.8324022194113,-6.58529244190234,
39.3492068662923));
#197999=CARTESIAN_POINT('Ctrl Pts',(60.9191469903169,-6.59440968471146,
39.4512271248733));
#198000=CARTESIAN_POINT('Ctrl Pts',(60.7340977611529,-6.7024250897622,39.3978017080178));
#198001=CARTESIAN_POINT('Ctrl Pts',(60.7472645033904,-6.57634410736721,
39.3980347781183));
#198002=CARTESIAN_POINT('Ctrl Pts',(60.7919547682785,-6.58104124348236,
39.5248015355195));
#198003=CARTESIAN_POINT('Ctrl Pts',(60.6448574988554,-6.69328024897455,
39.3978017080178));
#198004=CARTESIAN_POINT('Ctrl Pts',(60.6581326136904,-6.56697596826278,
39.3978017080178));
#198005=CARTESIAN_POINT('Ctrl Pts',(60.6581326136904,-6.56697596826278,
39.5248017080178));
#198006=CARTESIAN_POINT('Origin',(60.6448574988554,-6.69328024897455,39.5248017080178));
#198007=CARTESIAN_POINT('Origin',(-0.0331877870874745,-0.315760701779427,
39.116));
#198008=CARTESIAN_POINT('Origin',(61.4975385923862,-6.78290064323561,39.116));
#198009=CARTESIAN_POINT('Origin',(-0.0331877870874745,-0.315760701779427,
39.5248017080178));
#198010=CARTESIAN_POINT('Origin',(60.4944777170594,-6.67747469700946,39.5248017080178));
#198011=CARTESIAN_POINT('Ctrl Pts',(62.0330459552232,-6.8397366303026,39.2875012672119));
#198012=CARTESIAN_POINT('Ctrl Pts',(62.046864023402,-6.71274550335202,39.287208709576));
#198013=CARTESIAN_POINT('Ctrl Pts',(61.9391074687683,-6.70161199370823,
39.3549016990124));
#198014=CARTESIAN_POINT('Ctrl Pts',(61.9187065474465,-6.82760205123564,
39.103493917393));
#198015=CARTESIAN_POINT('Ctrl Pts',(61.9323544653035,-6.70071032544322,
39.1031692336349));
#198016=CARTESIAN_POINT('Ctrl Pts',(61.8476598279018,-6.6920004592178,39.2077507202315));
#198017=CARTESIAN_POINT('Ctrl Pts',(61.7133000470647,-6.80580199871467,
38.989));
#198018=CARTESIAN_POINT('Ctrl Pts',(61.7268034525359,-6.67910652125777,
38.9887769311152));
#198019=CARTESIAN_POINT('Ctrl Pts',(61.6833778591502,-6.67473372828934,
39.1161898712895));
#198020=CARTESIAN_POINT('Ctrl Pts',(61.4975385923862,-6.78290064323561,
38.989));
#198021=CARTESIAN_POINT('Ctrl Pts',(61.5108335396272,-6.65640766978507,
38.989));
#198022=CARTESIAN_POINT('Ctrl Pts',(61.510813692429,-6.65659650326253,39.1161895903858));
#198023=CARTESIAN_POINT('Origin',(61.9259926140919,-6.82793297553349,39.3548010137695));
#198024=CARTESIAN_POINT('Ctrl Pts',(60.4944777170594,-6.67747469700946,
39.3978017080178));
#198025=CARTESIAN_POINT('Ctrl Pts',(60.5077528318944,-6.55117041629769,
39.3978017080178));
#198026=CARTESIAN_POINT('Ctrl Pts',(60.5077528318944,-6.55117041629769,
39.5248017080178));
#198027=CARTESIAN_POINT('Ctrl Pts',(60.404935774755,-6.66829952659935,39.3978017080178));
#198028=CARTESIAN_POINT('Ctrl Pts',(60.4181493202566,-6.5417527077301,39.3975666025021));
#198029=CARTESIAN_POINT('Ctrl Pts',(60.3734783767965,-6.53705760237891,
39.5248015517177));
#198030=CARTESIAN_POINT('Ctrl Pts',(60.3202668847283,-6.65962554481688,
39.3484894016716));
#198031=CARTESIAN_POINT('Ctrl Pts',(60.333852472875,-6.53289275204992,39.3480259000039));
#198032=CARTESIAN_POINT('Ctrl Pts',(60.2465123062132,-6.52371293062557,
39.4508333188947));
#198033=CARTESIAN_POINT('Ctrl Pts',(60.2756459899119,-6.65505462397395,
39.2708017080178));
#198034=CARTESIAN_POINT('Ctrl Pts',(60.2894805317162,-6.52822907310778,
39.27051194648));
#198035=CARTESIAN_POINT('Ctrl Pts',(60.1796001951995,-6.51668018436747,
39.3343017080178));
#198036=CARTESIAN_POINT('Origin',(60.1663250803646,-6.64298446507924,39.3343017080178));
#198037=CARTESIAN_POINT('Origin',(62.1031658061135,-6.84655462836804,39.6398955068193));
#198038=CARTESIAN_POINT('Origin',(62.2803389979219,-6.8651762812251,39.92499));
#198039=CARTESIAN_POINT('Origin',(60.0854204576119,-6.634481046568,39.1934008539943));
#198040=CARTESIAN_POINT('Origin',(60.0409538388296,-6.62985850077847,39.1160402713849));
#198041=CARTESIAN_POINT('Ctrl Pts',(62.6076796697354,-6.59568250079886,
40.1599502534424));
#198042=CARTESIAN_POINT('Ctrl Pts',(62.5705801176609,-6.59177408464774,
40.10025));
#198043=CARTESIAN_POINT('Ctrl Pts',(62.5005702980931,-6.58439859103029,
40.10025));
#198044=CARTESIAN_POINT('Ctrl Pts',(62.598447729079,-6.68331293653951,40.1599500538448));
#198045=CARTESIAN_POINT('Ctrl Pts',(62.5638523220891,-6.65560500345244,
40.1002448353502));
#198046=CARTESIAN_POINT('Ctrl Pts',(62.4952175264232,-6.63512154272615,
40.10025));
#198047=CARTESIAN_POINT('Ctrl Pts',(62.565050454942,-6.76155265492241,40.1202442001041));
#198048=CARTESIAN_POINT('Ctrl Pts',(62.5346567608587,-6.71196843232399,
40.063387386802));
#198049=CARTESIAN_POINT('Ctrl Pts',(62.4653998062676,-6.67930776339544,
40.077227172354));
#198050=CARTESIAN_POINT('Ctrl Pts',(62.4816328770699,-6.86003002196291,
40.004599599816));
#198051=CARTESIAN_POINT('Ctrl Pts',(62.4676069047243,-6.7686325824506,39.9663485808311));
#198052=CARTESIAN_POINT('Ctrl Pts',(62.3866783619496,-6.7331110463148,40.0101727202463));
#198053=CARTESIAN_POINT('Ctrl Pts',(62.4326191774619,-6.88172985342165,
39.9304654349861));
#198054=CARTESIAN_POINT('Ctrl Pts',(62.429206244915,-6.76853939445059,39.9051900162963));
#198055=CARTESIAN_POINT('Ctrl Pts',(62.338838812382,-6.74362530798255,39.9671857458188));
#198056=CARTESIAN_POINT('Ctrl Pts',(62.3873926810691,-6.87697683366565,
39.8576902534424));
#198057=CARTESIAN_POINT('Ctrl Pts',(62.4011871104969,-6.75017837817602,
39.8573998014387));
#198058=CARTESIAN_POINT('Ctrl Pts',(62.2936141127569,-6.73887200051333,
39.92499));
#198059=CARTESIAN_POINT('Origin',(62.5005702980931,-6.58439859103029,40.22725));
#198060=CARTESIAN_POINT('Origin',(-0.0331877870874745,-0.315760701779427,
39.116));
#198061=CARTESIAN_POINT('Origin',(59.6417962403143,-6.58785426247096,39.116));
#198062=CARTESIAN_POINT('Origin',(5.50069060731754E-15,5.71212024007692E-15,
40.22725));
#198063=CARTESIAN_POINT('Origin',(62.5037563256535,-6.55408556365946,40.22725));
#198064=CARTESIAN_POINT('Ctrl Pts',(59.6417962403143,-6.58785426247096,
38.989));
#198065=CARTESIAN_POINT('Ctrl Pts',(59.6550912418708,-6.46136077224313,
38.989));
#198066=CARTESIAN_POINT('Ctrl Pts',(59.655071340276,-6.46155012326924,39.1161901092323));
#198067=CARTESIAN_POINT('Ctrl Pts',(59.4260321009469,-6.56494565834876,
38.989));
#198068=CARTESIAN_POINT('Ctrl Pts',(59.4394927947735,-6.43870097938002,
38.989229898976));
#198069=CARTESIAN_POINT('Ctrl Pts',(59.4825041216649,-6.44341257746672,
39.1161900493203));
#198070=CARTESIAN_POINT('Ctrl Pts',(59.2206282517276,-6.54313468201959,
39.1034966344368));
#198071=CARTESIAN_POINT('Ctrl Pts',(59.234195551358,-6.41712387095933,39.1038314102551));
#198072=CARTESIAN_POINT('Ctrl Pts',(59.3182233753697,-6.42614597500977,
39.2077528789596));
#198073=CARTESIAN_POINT('Ctrl Pts',(59.1062911958296,-6.53099325080055,
39.2875012672119));
#198074=CARTESIAN_POINT('Ctrl Pts',(59.1200087130389,-6.40512262640552,
39.2878045257868));
#198075=CARTESIAN_POINT('Ctrl Pts',(59.2267768553865,-6.41653455832026,
39.35490152959));
#198076=CARTESIAN_POINT('Origin',(59.2133417798936,-6.54282188406228,39.3548010137695));
#198077=CARTESIAN_POINT('Ctrl Pts',(62.4538823482275,-6.2443699078806,39.8576902534424));
#198078=CARTESIAN_POINT('Ctrl Pts',(62.4410124550018,-6.37126553604071,
39.8573998014387));
#198079=CARTESIAN_POINT('Ctrl Pts',(62.3334394572619,-6.35995915837802,
39.92499));
#198080=CARTESIAN_POINT('Ctrl Pts',(62.4991292864732,-6.24912604340899,
39.930498490249));
#198081=CARTESIAN_POINT('Ctrl Pts',(62.4722545055303,-6.3591243783161,39.9052171569792));
#198082=CARTESIAN_POINT('Ctrl Pts',(62.3786847639676,-6.36471463173867,
39.9672049726604));
#198083=CARTESIAN_POINT('Ctrl Pts',(62.5423796567684,-6.28053011789743,
40.0043437678662));
#198084=CARTESIAN_POINT('Ctrl Pts',(62.509694696565,-6.367085334999,39.9661628577642));
#198085=CARTESIAN_POINT('Ctrl Pts',(62.4231124872028,-6.38493060453713,
40.0100243556236));
#198086=CARTESIAN_POINT('Ctrl Pts',(62.6032845425345,-6.39322569848883,
40.1194874821987));
#198087=CARTESIAN_POINT('Ctrl Pts',(62.5632890102007,-6.43576006824441,
40.062755148314));
#198088=CARTESIAN_POINT('Ctrl Pts',(62.4886705126496,-6.45334792019192,
40.0767884282376));
#198089=CARTESIAN_POINT('Ctrl Pts',(62.6200908675645,-6.4773924351049,40.1599502015381));
#198090=CARTESIAN_POINT('Ctrl Pts',(62.5804859237118,-6.49734694408353,
40.1002449453872));
#198091=CARTESIAN_POINT('Ctrl Pts',(62.5090840872014,-6.50319024212508,
40.10025));
#198092=CARTESIAN_POINT('Ctrl Pts',(62.6108711573006,-6.56531752495302,
40.1599502534424));
#198093=CARTESIAN_POINT('Ctrl Pts',(62.5737697140402,-6.56142710223352,
40.10025));
#198094=CARTESIAN_POINT('Ctrl Pts',(62.5037563256535,-6.55408556365946,
40.10025));
#198095=CARTESIAN_POINT('Origin',(62.3467145720969,-6.23365487766625,39.92499));
#198096=CARTESIAN_POINT('Origin',(59.0361683443304,-6.52420020557798,39.6398955069312));
#198097=CARTESIAN_POINT('Origin',(58.858994908613,-6.50557852713755,39.92499));
#198098=CARTESIAN_POINT('Origin',(62.169541380269,-6.21503322484993,39.6398955068287));
#198099=CARTESIAN_POINT('Origin',(61.9923681882669,-6.19641157197464,39.3548010137695));
#198100=CARTESIAN_POINT('Ctrl Pts',(58.7519447039088,-6.49374646112741,
39.8576902534424));
#198101=CARTESIAN_POINT('Ctrl Pts',(58.7656442740271,-6.36806742857326,
39.8579948730703));
#198102=CARTESIAN_POINT('Ctrl Pts',(58.872270023448,-6.37927424642578,39.92499));
#198103=CARTESIAN_POINT('Ctrl Pts',(58.7067576262547,-6.48899657309051,
39.930402071123));
#198104=CARTESIAN_POINT('Ctrl Pts',(58.7342098038494,-6.38004220452783,
39.9058915297388));
#198105=CARTESIAN_POINT('Ctrl Pts',(58.8270810177601,-6.37452469054053,
39.9671523786039));
#198106=CARTESIAN_POINT('Ctrl Pts',(58.6637560248473,-6.45774144355308,
40.0043257306694));
#198107=CARTESIAN_POINT('Ctrl Pts',(58.6967899354326,-6.37187117938123,
39.9667894847835));
#198108=CARTESIAN_POINT('Ctrl Pts',(58.7829167175848,-6.3543526691276,40.0100138975201));
#198109=CARTESIAN_POINT('Ctrl Pts',(58.6035914159081,-6.34539908016329,
40.1195533054856));
#198110=CARTESIAN_POINT('Ctrl Pts',(58.6436439608621,-6.30313135363851,
40.0630813209236));
#198111=CARTESIAN_POINT('Ctrl Pts',(58.7181337176191,-6.28595874576521,
40.0768265942419));
#198112=CARTESIAN_POINT('Ctrl Pts',(58.5872698677174,-6.26151010025721,
40.1599502027509));
#198113=CARTESIAN_POINT('Ctrl Pts',(58.6268645946692,-6.24170554357537,
40.1002552791541));
#198114=CARTESIAN_POINT('Ctrl Pts',(58.6982323944365,-6.23613328458267,
40.10025));
#198115=CARTESIAN_POINT('Ctrl Pts',(58.5964866834551,-6.1740349085902,40.1599502534424));
#198116=CARTESIAN_POINT('Ctrl Pts',(58.6335861742242,-6.17794390662172,
40.10025));
#198117=CARTESIAN_POINT('Ctrl Pts',(58.7035958781039,-6.18532049829399,
40.10025));
#198118=CARTESIAN_POINT('Origin',(58.7035958781039,-6.18532049829399,40.22725));
#198119=CARTESIAN_POINT('Ctrl Pts',(61.5639141665612,-6.15137923967676,
38.989));
#198120=CARTESIAN_POINT('Ctrl Pts',(61.5506192181748,-6.2778722240245,38.989));
#198121=CARTESIAN_POINT('Ctrl Pts',(61.5506390665201,-6.2776833796336,39.1161896013267));
#198122=CARTESIAN_POINT('Ctrl Pts',(61.7797255331386,-6.17383801205359,
38.989));
#198123=CARTESIAN_POINT('Ctrl Pts',(61.7665923920133,-6.30057242039953,
38.988776927546));
#198124=CARTESIAN_POINT('Ctrl Pts',(61.7232059145528,-6.29582088597892,
39.1161898821824));
#198125=CARTESIAN_POINT('Ctrl Pts',(61.9851742714891,-6.19522058691241,
39.1034967087243));
#198126=CARTESIAN_POINT('Ctrl Pts',(61.9721416759911,-6.32217699854488,
39.1031720232716));
#198127=CARTESIAN_POINT('Ctrl Pts',(61.887486582017,-6.31308747966678,39.2077529615019));
#198128=CARTESIAN_POINT('Ctrl Pts',(62.0995362748659,-6.20712349654464,
39.2875012672119));
#198129=CARTESIAN_POINT('Ctrl Pts',(62.086649444066,-6.33421251157703,39.2872087095507));
#198130=CARTESIAN_POINT('Ctrl Pts',(61.9789328337398,-6.3226988678917,39.3549017048228));
#198131=CARTESIAN_POINT('Origin',(61.5639141665612,-6.15137923967676,39.116));
#198132=CARTESIAN_POINT('Origin',(5.72301283402738E-15,5.24657654254566E-15,
40.22725));
#198133=CARTESIAN_POINT('Origin',(58.7067819056643,-6.15500747092316,40.22725));
#198134=CARTESIAN_POINT('Origin',(61.5757885448747,-6.15262728712865,39.116));
#198135=CARTESIAN_POINT('Origin',(61.1647646440473,-6.1093749596204,39.1160373285264));
#198136=CARTESIAN_POINT('Ctrl Pts',(58.5996668978648,-6.14377718965322,
40.1599502534424));
#198137=CARTESIAN_POINT('Ctrl Pts',(58.6367684021392,-6.14766703046171,
40.10025));
#198138=CARTESIAN_POINT('Ctrl Pts',(58.7067819056643,-6.15500747092316,
40.10025));
#198139=CARTESIAN_POINT('Ctrl Pts',(58.6088074259634,-6.05659553606703,
40.1599500566034));
#198140=CARTESIAN_POINT('Ctrl Pts',(58.6434243604386,-6.08415140319802,
40.1002551305369));
#198141=CARTESIAN_POINT('Ctrl Pts',(58.7120821529696,-6.10436324506821,
40.10025));
#198142=CARTESIAN_POINT('Ctrl Pts',(58.641681736514,-5.97852000021518,40.1203070619046));
#198143=CARTESIAN_POINT('Ctrl Pts',(58.6721826510718,-6.02785839131264,
40.0637098684499));
#198144=CARTESIAN_POINT('Ctrl Pts',(58.7414038195498,-6.06008468706693,
40.0772636213363));
#198145=CARTESIAN_POINT('Ctrl Pts',(58.7242744516463,-5.88025093392472,
40.0046102245802));
#198146=CARTESIAN_POINT('Ctrl Pts',(58.7387860695147,-5.97104363802146,
39.9670001894012));
#198147=CARTESIAN_POINT('Ctrl Pts',(58.8193360415241,-6.00614981441022,
40.0101788811209));
#198148=CARTESIAN_POINT('Ctrl Pts',(58.7730316211507,-5.85862682030274,
39.9303710930186));
#198149=CARTESIAN_POINT('Ctrl Pts',(58.7772266151804,-5.97091547255841,
39.9058663574101));
#198150=CARTESIAN_POINT('Ctrl Pts',(58.8669255556781,-5.99561386571421,
39.9671344706357));
#198151=CARTESIAN_POINT('Ctrl Pts',(58.8181995570485,-5.8633736414958,39.8576902534424));
#198152=CARTESIAN_POINT('Ctrl Pts',(58.805469618532,-5.98915458643795,39.8579948730703));
#198153=CARTESIAN_POINT('Ctrl Pts',(58.912095367953,-6.00036140429046,39.92499));
#198154=CARTESIAN_POINT('Origin',(58.925370482788,-5.87405712357869,39.92499));
#198155=CARTESIAN_POINT('Origin',(61.1207756545813,-6.10480350526346,39.192555448885));
#198156=CARTESIAN_POINT('Origin',(61.0393856393804,-6.09624906995239,39.3343017080178));
#198157=CARTESIAN_POINT('Origin',(59.1025439184835,-5.89267880207615,39.6398955069214));
#198158=CARTESIAN_POINT('Origin',(59.2797173540686,-5.91130048050343,39.3548010137695));
#198159=CARTESIAN_POINT('Ctrl Pts',(60.7112330730304,-6.0617588454157,39.3978017080178));
#198160=CARTESIAN_POINT('Ctrl Pts',(60.6979579581954,-6.18806312612747,
39.3978017080178));
#198161=CARTESIAN_POINT('Ctrl Pts',(60.6979579581954,-6.18806312612747,
39.5248017080178));
#198162=CARTESIAN_POINT('Ctrl Pts',(60.8007259828526,-6.07140041118235,
39.3978017080178));
#198163=CARTESIAN_POINT('Ctrl Pts',(60.7873912833632,-6.19746294737652,
39.3980355775177));
#198164=CARTESIAN_POINT('Ctrl Pts',(60.832232401263,-6.20217593878182,39.5248015517192));
#198165=CARTESIAN_POINT('Ctrl Pts',(60.885348460727,-6.08051542067561,39.3484893995498));
#198166=CARTESIAN_POINT('Ctrl Pts',(60.8723790316477,-6.20639551966723,
39.3489438303425));
#198167=CARTESIAN_POINT('Ctrl Pts',(60.9591984396283,-6.21552060714891,
39.4508333155593));
#198168=CARTESIAN_POINT('Ctrl Pts',(60.929944884669,-6.0853187813832,39.2708017080178));
#198169=CARTESIAN_POINT('Ctrl Pts',(60.917217374751,-6.21110821942935,39.2710850691866));
#198170=CARTESIAN_POINT('Ctrl Pts',(61.0261105245454,-6.22255335066416,
39.3343017080178));
#198171=CARTESIAN_POINT('Origin',(60.7112330730304,-6.0617588454157,39.5248017080178));
#198172=CARTESIAN_POINT('Ctrl Pts',(59.1725467709677,-5.90061356181257,
39.2875012672119));
#198173=CARTESIAN_POINT('Ctrl Pts',(59.1597945546413,-6.02658562874793,
39.2878045257519));
#198174=CARTESIAN_POINT('Ctrl Pts',(59.2666022171586,-6.03762143316751,
39.3549015218347));
#198175=CARTESIAN_POINT('Ctrl Pts',(59.2869113614505,-5.91250964036448,
39.1034938540228));
#198176=CARTESIAN_POINT('Ctrl Pts',(59.2739830624786,-6.03858760028837,
39.1038286278814));
#198177=CARTESIAN_POINT('Ctrl Pts',(59.3580501215753,-6.04723299508892,
39.2077506434033));
#198178=CARTESIAN_POINT('Ctrl Pts',(59.4923630227875,-5.93388131656882,
38.989));
#198179=CARTESIAN_POINT('Ctrl Pts',(59.4792818168365,-6.06016587018146,
38.9892298954611));
#198180=CARTESIAN_POINT('Ctrl Pts',(59.5223321697726,-6.06449973388389,
39.1161900347288));
#198181=CARTESIAN_POINT('Ctrl Pts',(59.7081718144892,-5.9563328589121,38.989));
#198182=CARTESIAN_POINT('Ctrl Pts',(59.6948768144683,-6.08282633453058,
38.989));
#198183=CARTESIAN_POINT('Ctrl Pts',(59.6948967145253,-6.08263699813566,
39.1161900945645));
#198184=CARTESIAN_POINT('Origin',(59.7081718144892,-5.95633285891211,39.116));
#198185=CARTESIAN_POINT('Origin',(60.0850508448141,-5.99594444118207,39.5248017080178));
#198186=CARTESIAN_POINT('Origin',(60.5608532912343,-6.04595329345061,39.5248017080178));
#198187=CARTESIAN_POINT('Origin',(59.851607889689,-5.97140859790549,39.116));
#198188=CARTESIAN_POINT('Origin',(60.1073400339997,-5.99823604520099,39.1160402713849));
#198189=CARTESIAN_POINT('Ctrl Pts',(60.3421421670675,-6.02238575970276,
39.2708017080178));
#198190=CARTESIAN_POINT('Ctrl Pts',(60.3293058762211,-6.14931623097247,
39.27051194648));
#198191=CARTESIAN_POINT('Ctrl Pts',(60.2194255397045,-6.13776734223215,
39.3343017080178));
#198192=CARTESIAN_POINT('Ctrl Pts',(60.3868890390928,-6.02720817145206,
39.3487519301185));
#198193=CARTESIAN_POINT('Ctrl Pts',(60.3738278099516,-6.15399567476902,
39.3482879463981));
#198194=CARTESIAN_POINT('Ctrl Pts',(60.2865637544299,-6.14482385294797,
39.4512271261641));
#198195=CARTESIAN_POINT('Ctrl Pts',(60.4716618705782,-6.03634362557897,
39.3978017080178));
#198196=CARTESIAN_POINT('Ctrl Pts',(60.4582762833192,-6.16287156698251,
39.3975673827397));
#198197=CARTESIAN_POINT('Ctrl Pts',(60.4137560077509,-6.15819229746499,
39.524801535518));
#198198=CARTESIAN_POINT('Ctrl Pts',(60.5608532912343,-6.04595329345061,
39.3978017080178));
#198199=CARTESIAN_POINT('Ctrl Pts',(60.5475781763993,-6.17225757416238,
39.3978017080178));
#198200=CARTESIAN_POINT('Ctrl Pts',(60.5475781763993,-6.17225757416238,
39.5248017080178));
#198201=CARTESIAN_POINT('Origin',(60.2327006545395,-6.01146306152038,39.3343017080178));
#198202=CARTESIAN_POINT('Origin',(60.1517960329188,-6.00295964283163,39.193400853355));
#198203=CARTESIAN_POINT('Origin',(60.0157999988656,-13.0813452322044,39.1925554495083));
#198204=CARTESIAN_POINT('Origin',(60.0590486699125,-13.0905908661188,39.1160373285276));
#198205=CARTESIAN_POINT('Origin',(59.9357500275433,-13.0643300858382,39.3343017080178));
#198206=CARTESIAN_POINT('Ctrl Pts',(59.8282880397055,-13.0409063549239,
39.2708017080178));
#198207=CARTESIAN_POINT('Ctrl Pts',(59.8550545325309,-12.9173404733283,
39.2710850691866));
#198208=CARTESIAN_POINT('Ctrl Pts',(59.9621548122771,-12.940105340545,39.3343017080178));
#198209=CARTESIAN_POINT('Ctrl Pts',(59.7842416555146,-13.0316624367248,
39.3487519293518));
#198210=CARTESIAN_POINT('Ctrl Pts',(59.8108054559361,-12.9079350417513,
39.349206866293));
#198211=CARTESIAN_POINT('Ctrl Pts',(59.8961220185298,-12.9260696369486,
39.4512271248737));
#198212=CARTESIAN_POINT('Ctrl Pts',(59.7007958241044,-13.014150410755,39.3978017080178));
#198213=CARTESIAN_POINT('Ctrl Pts',(59.7270694888854,-12.8901364125059,
39.3980347781183));
#198214=CARTESIAN_POINT('Ctrl Pts',(59.7710239514072,-12.8994792219295,
39.5248015355195));
#198215=CARTESIAN_POINT('Ctrl Pts',(59.6130003254555,-12.9957275188824,
39.3978017080178));
#198216=CARTESIAN_POINT('Ctrl Pts',(59.6394051101893,-12.8715027735892,
39.3978017080178));
#198217=CARTESIAN_POINT('Ctrl Pts',(59.6394051101893,-12.8715027735892,
39.5248017080178));
#198218=CARTESIAN_POINT('Origin',(59.6130003254555,-12.9957275188824,39.5248017080178));
#198219=CARTESIAN_POINT('Origin',(-0.0660119618346332,-0.310561863232983,
39.116));
#198220=CARTESIAN_POINT('Origin',(60.4516424606489,-13.1739864076107,39.116));
#198221=CARTESIAN_POINT('Origin',(-0.0660119618346331,-0.310561863232983,
39.5248017080178));
#198222=CARTESIAN_POINT('Origin',(59.4650964698966,-12.9642895838871,39.5248017080178));
#198223=CARTESIAN_POINT('Ctrl Pts',(60.9782752797348,-13.2864868028996,
39.2875012672119));
#198224=CARTESIAN_POINT('Ctrl Pts',(61.0052918384389,-13.1616357280625,
39.287208709576));
#198225=CARTESIAN_POINT('Ctrl Pts',(60.8992893541409,-13.139299581886,39.354901699012));
#198226=CARTESIAN_POINT('Ctrl Pts',(60.8658306440996,-13.2624669757406,
39.103493917393));
#198227=CARTESIAN_POINT('Ctrl Pts',(60.8926675943295,-13.13769697198,39.1031692336354));
#198228=CARTESIAN_POINT('Ctrl Pts',(60.8093473519447,-13.120181819017,39.207750720232));
#198229=CARTESIAN_POINT('Ctrl Pts',(60.663828108008,-13.2193155203585,38.989));
#198230=CARTESIAN_POINT('Ctrl Pts',(60.690500823975,-13.0947255842078,38.9887769311158));
#198231=CARTESIAN_POINT('Ctrl Pts',(60.6477702018642,-13.0858375353126,
39.1161898712887));
#198232=CARTESIAN_POINT('Ctrl Pts',(60.4516424606489,-13.1739864076107,
38.989));
#198233=CARTESIAN_POINT('Ctrl Pts',(60.4780866929066,-13.049576076309,38.989));
#198234=CARTESIAN_POINT('Ctrl Pts',(60.4780472159604,-13.049761800739,39.116189590385));
#198235=CARTESIAN_POINT('Origin',(60.8730422059013,-13.2635576885502,39.3548010137695));
#198236=CARTESIAN_POINT('Ctrl Pts',(59.4650964698966,-12.9642895838871,
39.3978017080178));
#198237=CARTESIAN_POINT('Ctrl Pts',(59.4915012546305,-12.8400648385939,
39.3978017080178));
#198238=CARTESIAN_POINT('Ctrl Pts',(59.4915012546305,-12.8400648385939,
39.5248017080178));
#198239=CARTESIAN_POINT('Ctrl Pts',(59.3770041141843,-12.9458049943939,
39.3978017080178));
#198240=CARTESIAN_POINT('Ctrl Pts',(59.4033730190112,-12.8213326038453,
39.3975666025021));
#198241=CARTESIAN_POINT('Ctrl Pts',(59.3594375597982,-12.8119938336989,
39.5248015517177));
#198242=CARTESIAN_POINT('Ctrl Pts',(59.2937057271824,-12.9283282206295,
39.3484894016716));
#198243=CARTESIAN_POINT('Ctrl Pts',(59.3204640761264,-12.803709764012,39.3480259000047));
#198244=CARTESIAN_POINT('Ctrl Pts',(59.2345619206657,-12.7854506972085,
39.4508333188947));
#198245=CARTESIAN_POINT('Ctrl Pts',(59.2498070616279,-12.9191181862046,
39.2708017080178));
#198246=CARTESIAN_POINT('Ctrl Pts',(59.2768226962998,-12.7944335023708,
39.27051194648));
#198247=CARTESIAN_POINT('Ctrl Pts',(59.1687514833561,-12.771462256932,39.3343017080178));
#198248=CARTESIAN_POINT('Origin',(59.1423466986222,-12.8956870022252,39.3343017080178));
#198249=CARTESIAN_POINT('Origin',(61.047298331886,-13.3005969715158,39.6398955068186));
#198250=CARTESIAN_POINT('Origin',(61.2215544576539,-13.3376362544826,39.92499));
#198251=CARTESIAN_POINT('Origin',(59.062774129127,-12.8787733304434,39.1934008539945));
#198252=CARTESIAN_POINT('Origin',(59.0190342907435,-12.8695280801147,39.1160402713849));
#198253=CARTESIAN_POINT('Ctrl Pts',(61.5752716937451,-13.1038352065728,
40.1599502534424));
#198254=CARTESIAN_POINT('Ctrl Pts',(61.5387839176328,-13.096070241968,40.10025));
#198255=CARTESIAN_POINT('Ctrl Pts',(61.4699285681954,-13.0814171332233,
40.10025));
#198256=CARTESIAN_POINT('Ctrl Pts',(61.5569304518434,-13.1900205930478,
40.1599500538467));
#198257=CARTESIAN_POINT('Ctrl Pts',(61.5254208297825,-13.1588482421895,
40.1002448353503));
#198258=CARTESIAN_POINT('Ctrl Pts',(61.4593031273768,-13.1313027022857,
40.10025));
#198259=CARTESIAN_POINT('Ctrl Pts',(61.515537853938,-13.2643407403244,40.120244200104));
#198260=CARTESIAN_POINT('Ctrl Pts',(61.4904936222818,-13.2118511391498,
40.0633873868018));
#198261=CARTESIAN_POINT('Ctrl Pts',(61.4250300340666,-13.172130065749,40.0772271723537));
#198262=CARTESIAN_POINT('Ctrl Pts',(61.4222835584426,-13.3535591268193,
40.0045995998161));
#198263=CARTESIAN_POINT('Ctrl Pts',(61.4178880557397,-13.2611962587088,
39.9663485808315));
#198264=CARTESIAN_POINT('Ctrl Pts',(61.3411158595754,-13.2174099770538,
40.0101727202466));
#198265=CARTESIAN_POINT('Ctrl Pts',(61.3712701109737,-13.370016757632,39.930465434986));
#198266=CARTESIAN_POINT('Ctrl Pts',(61.3797074995639,-13.2570896192432,
39.9051900162951));
#198267=CARTESIAN_POINT('Ctrl Pts',(61.2924393404518,-13.2228660458967,
39.9671857458178));
#198268=CARTESIAN_POINT('Ctrl Pts',(61.3267881959113,-13.3605623192487,
39.8576902534424));
#198269=CARTESIAN_POINT('Ctrl Pts',(61.3537611057083,-13.2359003894751,
39.8573998014387));
#198270=CARTESIAN_POINT('Ctrl Pts',(61.2479592423878,-13.2134115091894,
39.92499));
#198271=CARTESIAN_POINT('Origin',(61.4699285681954,-13.0814171332233,40.22725));
#198272=CARTESIAN_POINT('Origin',(-0.0660119618346332,-0.310561863232983,
39.116));
#198273=CARTESIAN_POINT('Origin',(58.6264539577984,-12.7860306150452,39.116));
#198274=CARTESIAN_POINT('Origin',(5.5033905580924E-15,5.72916705837122E-15,
40.22725));
#198275=CARTESIAN_POINT('Origin',(61.4762657165316,-13.0516031943529,40.22725));
#198276=CARTESIAN_POINT('Ctrl Pts',(58.6264539577984,-12.7860306150452,
38.989));
#198277=CARTESIAN_POINT('Ctrl Pts',(58.6528982980922,-12.6616197754736,
38.989));
#198278=CARTESIAN_POINT('Ctrl Pts',(58.6528587129486,-12.6618060089321,
39.1161901092325));
#198279=CARTESIAN_POINT('Ctrl Pts',(58.4142663981466,-12.7406940127373,
38.989));
#198280=CARTESIAN_POINT('Ctrl Pts',(58.4408495151711,-12.616547940969,38.989229898976));
#198281=CARTESIAN_POINT('Ctrl Pts',(58.4831327254079,-12.6257296363316,
39.1161900493205));
#198282=CARTESIAN_POINT('Ctrl Pts',(58.2122676405433,-12.6975319705099,
39.1034966344368));
#198283=CARTESIAN_POINT('Ctrl Pts',(58.2389323335232,-12.5736296288409,
39.1038314102556));
#198284=CARTESIAN_POINT('Ctrl Pts',(58.3215567776494,-12.5913856081746,
39.2077528789596));
#198285=CARTESIAN_POINT('Ctrl Pts',(58.099826060148,-12.6735055745741,39.2875012672119));
#198286=CARTESIAN_POINT('Ctrl Pts',(58.1266254943013,-12.5497583536231,
39.2878045257868));
#198287=CARTESIAN_POINT('Ctrl Pts',(58.231615877888,-12.5722680796265,39.3549015295901));
#198288=CARTESIAN_POINT('Origin',(58.2050537810542,-12.6964592423893,39.3548010137695));
#198289=CARTESIAN_POINT('Ctrl Pts',(61.4590390555209,-12.7383709431251,
39.8576902534424));
#198290=CARTESIAN_POINT('Ctrl Pts',(61.4329754599099,-12.8632261535955,
39.8573998014387));
#198291=CARTESIAN_POINT('Ctrl Pts',(61.3271735965893,-12.8407372733098,
39.92499));
#198292=CARTESIAN_POINT('Ctrl Pts',(61.5035409747667,-12.7478306169679,
39.9304984902491));
#198293=CARTESIAN_POINT('Ctrl Pts',(61.4653154597762,-12.8544171899347,
39.9052171569788));
#198294=CARTESIAN_POINT('Ctrl Pts',(61.3716739624479,-12.8501961180698,
39.9672049726605));
#198295=CARTESIAN_POINT('Ctrl Pts',(61.5432717953614,-12.783583551393,40.0043437678662));
#198296=CARTESIAN_POINT('Ctrl Pts',(61.501718402959,-12.8662481012965,39.9661628577646));
#198297=CARTESIAN_POINT('Ctrl Pts',(61.4137451613974,-12.8749453072904,
40.0100243556235));
#198298=CARTESIAN_POINT('Ctrl Pts',(61.5920631419345,-12.9020280679171,
40.1194874821987));
#198299=CARTESIAN_POINT('Ctrl Pts',(61.5478406570046,-12.9401487584127,
40.0627551483138));
#198300=CARTESIAN_POINT('Ctrl Pts',(61.4717924962542,-12.9498405053861,
40.0767884282377));
#198301=CARTESIAN_POINT('Ctrl Pts',(61.5999795805211,-12.987490469672,40.1599502015386));
#198302=CARTESIAN_POINT('Ctrl Pts',(61.5585057825379,-13.003195821844,40.1002449453872));
#198303=CARTESIAN_POINT('Ctrl Pts',(61.4868843017925,-13.0015435854425,
40.10025));
#198304=CARTESIAN_POINT('Ctrl Pts',(61.5816197022698,-13.0739701745325,
40.1599502534424));
#198305=CARTESIAN_POINT('Ctrl Pts',(61.5451281645059,-13.0662229071067,
40.10025));
#198306=CARTESIAN_POINT('Ctrl Pts',(61.4762657165316,-13.0516031943529,
40.10025));
#198307=CARTESIAN_POINT('Origin',(61.3535783813232,-12.7165125280166,39.92499));
#198308=CARTESIAN_POINT('Origin',(58.0307974155447,-12.6594199084569,39.6398955069314));
#198309=CARTESIAN_POINT('Origin',(57.8565410498767,-12.6223805745519,39.92499));
#198310=CARTESIAN_POINT('Origin',(61.1793222555322,-12.6794732450928,39.6398955068271));
#198311=CARTESIAN_POINT('Origin',(61.0050661295706,-12.6424339620842,39.3548010137695));
#198312=CARTESIAN_POINT('Ctrl Pts',(57.751314065072,-12.5994235324472,39.8576902534424));
#198313=CARTESIAN_POINT('Ctrl Pts',(57.7780756236495,-12.4758649777953,
39.8579948730703));
#198314=CARTESIAN_POINT('Ctrl Pts',(57.8829458346105,-12.4981558292588,
39.92499));
#198315=CARTESIAN_POINT('Ctrl Pts',(57.7068710254545,-12.5899763290071,
39.930402071123));
#198316=CARTESIAN_POINT('Ctrl Pts',(57.7455616498603,-12.4844883578131,
39.9058915297386));
#198317=CARTESIAN_POINT('Ctrl Pts',(57.8385008428013,-12.4887087546163,
39.967152378603));
#198318=CARTESIAN_POINT('Ctrl Pts',(57.6673720419786,-12.5543975270268,
40.0043257306693));
#198319=CARTESIAN_POINT('Ctrl Pts',(57.709200876099,-12.4724506530559,39.9667894847835));
#198320=CARTESIAN_POINT('Ctrl Pts',(57.7966870296826,-12.4640308112188,
40.01001389752));
#198321=CARTESIAN_POINT('Ctrl Pts',(57.6192799956674,-12.4363816727421,
40.1195533054857));
#198322=CARTESIAN_POINT('Ctrl Pts',(57.6635313090893,-12.39853212422,40.0630813209236));
#198323=CARTESIAN_POINT('Ctrl Pts',(57.7394080294762,-12.3892398894926,
40.076826594242));
#198324=CARTESIAN_POINT('Ctrl Pts',(57.6118166447792,-12.3512461790953,
40.1599502027523));
#198325=CARTESIAN_POINT('Ctrl Pts',(57.6532646075463,-12.3356888898082,
40.1002552791529));
#198326=CARTESIAN_POINT('Ctrl Pts',(57.7248239067121,-12.3376071226704,
40.10025));
#198327=CARTESIAN_POINT('Ctrl Pts',(57.6301266171957,-12.2652136052661,
40.1599502534424));
#198328=CARTESIAN_POINT('Ctrl Pts',(57.6666142715155,-12.2729791421555,
40.10025));
#198329=CARTESIAN_POINT('Ctrl Pts',(57.7354693911205,-12.2876333308471,
40.10025));
#198330=CARTESIAN_POINT('Origin',(57.7354693911204,-12.2876333308471,40.22725));
#198331=CARTESIAN_POINT('Ctrl Pts',(60.5836663843182,-12.5528626811448,
38.989));
#198332=CARTESIAN_POINT('Ctrl Pts',(60.5572221497821,-12.6772730231653,
38.989));
#198333=CARTESIAN_POINT('Ctrl Pts',(60.5572616290101,-12.6770872880005,
39.1161896013269));
#198334=CARTESIAN_POINT('Ctrl Pts',(60.7959479326852,-12.597756852521,38.989));
#198335=CARTESIAN_POINT('Ctrl Pts',(60.7696393833305,-12.7224242094576,
38.9887769275436));
#198336=CARTESIAN_POINT('Ctrl Pts',(60.7269872521261,-12.7131635826238,
39.1161898821827));
#198337=CARTESIAN_POINT('Ctrl Pts',(60.9980361136598,-12.6404975322982,
39.1034967087243));
#198338=CARTESIAN_POINT('Ctrl Pts',(60.9718043534777,-12.7653961862451,
39.1031720232722));
#198339=CARTESIAN_POINT('Ctrl Pts',(60.8885631224039,-12.74750759382,39.2077529615016));
#198340=CARTESIAN_POINT('Ctrl Pts',(61.1105274371641,-12.6642893210142,
39.2875012672119));
#198341=CARTESIAN_POINT('Ctrl Pts',(61.0844267823321,-12.789335088505,39.2872087095507));
#198342=CARTESIAN_POINT('Ctrl Pts',(60.9785037583488,-12.7666250660184,
39.3549017048229));
#198343=CARTESIAN_POINT('Origin',(60.5836663843182,-12.5528626811448,39.116));
#198344=CARTESIAN_POINT('Origin',(5.72205236298458E-15,5.24051236704441E-15,
40.22725));
#198345=CARTESIAN_POINT('Origin',(57.7418065394566,-12.2578193919768,40.22725));
#198346=CARTESIAN_POINT('Origin',(59.5987607253194,-12.3435145206986,39.116));
#198347=CARTESIAN_POINT('Origin',(60.1910940874965,-12.4693660187271,39.1160373285252));
#198348=CARTESIAN_POINT('Ctrl Pts',(57.6364522029207,-12.2354540642045,
40.1599502534424));
#198349=CARTESIAN_POINT('Ctrl Pts',(57.6729438621906,-12.2432007592847,
40.10025));
#198350=CARTESIAN_POINT('Ctrl Pts',(57.7418065394566,-12.2578193919768,
40.10025));
#198351=CARTESIAN_POINT('Ctrl Pts',(57.654655622525,-12.1497054461942,40.1599500566025));
#198352=CARTESIAN_POINT('Ctrl Pts',(57.6862025493675,-12.1807288143661,
40.1002551305369));
#198353=CARTESIAN_POINT('Ctrl Pts',(57.7523715145553,-12.2080066271958,
40.10025));
#198354=CARTESIAN_POINT('Ctrl Pts',(57.6955109599433,-12.0754939174599,
40.1203070619049));
#198355=CARTESIAN_POINT('Ctrl Pts',(57.7206875210982,-12.1277502414153,
40.0637098684502));
#198356=CARTESIAN_POINT('Ctrl Pts',(57.7861609236007,-12.1670355805164,
40.0772636213365));
#198357=CARTESIAN_POINT('Ctrl Pts',(57.7879231380269,-11.9863964689862,
40.0046102245799));
#198358=CARTESIAN_POINT('Ctrl Pts',(57.7928648378991,-12.0782086782658,
39.9670001894009));
#198359=CARTESIAN_POINT('Ctrl Pts',(57.8693039540645,-12.1215423041371,
40.0101788811207));
#198360=CARTESIAN_POINT('Ctrl Pts',(57.8386735460213,-11.9699873265228,
39.9303710930188));
#198361=CARTESIAN_POINT('Ctrl Pts',(57.8311081991733,-12.0820993460726,
39.9058663574113));
#198362=CARTESIAN_POINT('Ctrl Pts',(57.917734074407,-12.1160385312529,39.9671344706364));
#198363=CARTESIAN_POINT('Ctrl Pts',(57.8830978693156,-11.9794294790612,
39.8576902534424));
#198364=CARTESIAN_POINT('Ctrl Pts',(57.8572899778511,-12.1031907419157,
39.8579948730703));
#198365=CARTESIAN_POINT('Ctrl Pts',(57.9621601888121,-12.1254815933792,
39.92499));
#198366=CARTESIAN_POINT('Origin',(57.9885649735459,-12.001256848086,39.92499));
#198367=CARTESIAN_POINT('Origin',(60.1478239214166,-12.4602215058058,39.1925554488848));
#198368=CARTESIAN_POINT('Origin',(60.0677739512126,-12.4432063593722,39.3343017080178));
#198369=CARTESIAN_POINT('Origin',(58.1628213391873,-12.038296182045,39.6398955069221));
#198370=CARTESIAN_POINT('Origin',(58.3370777047235,-12.0753355159233,39.3548010137695));
#198371=CARTESIAN_POINT('Ctrl Pts',(59.7450242491248,-12.3746037924164,
39.3978017080178));
#198372=CARTESIAN_POINT('Ctrl Pts',(59.7186194643909,-12.4988285377096,
39.3978017080178));
#198373=CARTESIAN_POINT('Ctrl Pts',(59.7186194643909,-12.4988285377096,
39.5248017080178));
#198374=CARTESIAN_POINT('Ctrl Pts',(59.8330190893701,-12.393547097014,39.3978017080178));
#198375=CARTESIAN_POINT('Ctrl Pts',(59.8065803155759,-12.5175251937991,
39.3980355775177));
#198376=CARTESIAN_POINT('Ctrl Pts',(59.8506831473905,-12.5268995400895,
39.5248015517192));
#198377=CARTESIAN_POINT('Ctrl Pts',(59.9162252185215,-12.4114576311016,
39.3484893995498));
#198378=CARTESIAN_POINT('Ctrl Pts',(59.8901687840278,-12.5352924712485,
39.3489438303424));
#198379=CARTESIAN_POINT('Ctrl Pts',(59.9755587548367,-12.5534426698447,
39.4508333155594));
#198380=CARTESIAN_POINT('Ctrl Pts',(59.9600752506737,-12.4208962741587,
39.2708017080178));
#198381=CARTESIAN_POINT('Ctrl Pts',(59.9342688867325,-12.5446662374487,
39.2710850691866));
#198382=CARTESIAN_POINT('Ctrl Pts',(60.0413691664787,-12.5674311046654,
39.3343017080178));
#198383=CARTESIAN_POINT('Origin',(59.7450242491248,-12.3746037924164,39.5248017080178));
#198384=CARTESIAN_POINT('Ctrl Pts',(58.2316113004781,-12.0535047649322,
39.2875012672119));
#198385=CARTESIAN_POINT('Ctrl Pts',(58.2057612755556,-12.1774537741283,
39.2878045257518));
#198386=CARTESIAN_POINT('Ctrl Pts',(58.3108302788452,-12.1995935640848,
39.3549015218346));
#198387=CARTESIAN_POINT('Ctrl Pts',(58.344105910958,-12.0772900304171,39.1034938540228));
#198388=CARTESIAN_POINT('Ctrl Pts',(58.3180696991572,-12.2013259468575,
39.1038286278792));
#198389=CARTESIAN_POINT('Ctrl Pts',(58.400772540276,-12.2187113817821,39.2077506434033));
#198390=CARTESIAN_POINT('Ctrl Pts',(58.5461981381265,-12.1200201767772,
38.989));
#198391=CARTESIAN_POINT('Ctrl Pts',(58.5199882620678,-12.2442455720362,
38.9892298954635));
#198392=CARTESIAN_POINT('Ctrl Pts',(58.562349768552,-12.2530556816157,39.1161900347287));
#198393=CARTESIAN_POINT('Ctrl Pts',(58.7584778814676,-12.1649068885792,
38.989));
#198394=CARTESIAN_POINT('Ctrl Pts',(58.7320335442281,-12.2893177137816,
38.989));
#198395=CARTESIAN_POINT('Ctrl Pts',(58.7320731263129,-12.2891314947137,
39.1161900945644));
#198396=CARTESIAN_POINT('Origin',(58.7584778814676,-12.1649068885792,39.116));
#198397=CARTESIAN_POINT('Origin',(58.1567073854021,-12.036996621021,39.5248017080178));
#198398=CARTESIAN_POINT('Origin',(59.5971203935659,-12.3431658574211,39.5248017080178));
#198399=CARTESIAN_POINT('Origin',(57.9308881865554,-11.9889972685551,39.116));
#198400=CARTESIAN_POINT('Origin',(59.1510793400372,-12.2483049654002,39.1160402713847));
#198401=CARTESIAN_POINT('Ctrl Pts',(59.3820708699071,-12.2968658913803,
39.2708017080178));
#198402=CARTESIAN_POINT('Ctrl Pts',(59.3560370505014,-12.4217592664913,
39.27051194648));
#198403=CARTESIAN_POINT('Ctrl Pts',(59.2479658375576,-12.3987880210524,
39.3343017080178));
#198404=CARTESIAN_POINT('Ctrl Pts',(59.4260685345961,-12.3063392072221,
39.3487519301185));
#198405=CARTESIAN_POINT('Ctrl Pts',(59.3998259533489,-12.4310668851215,
39.3482879464001));
#198406=CARTESIAN_POINT('Ctrl Pts',(59.3139986558974,-12.4128237298761,
39.4512271261639));
#198407=CARTESIAN_POINT('Ctrl Pts',(59.5094220566594,-12.324285790178,39.3978017080178));
#198408=CARTESIAN_POINT('Ctrl Pts',(59.4828840257742,-12.448721423414,39.3975673827378));
#198409=CARTESIAN_POINT('Ctrl Pts',(59.4390967537837,-12.4394141514343,
39.524801535518));
#198410=CARTESIAN_POINT('Ctrl Pts',(59.5971203935659,-12.3431658574211,
39.3978017080178));
#198411=CARTESIAN_POINT('Ctrl Pts',(59.570715608832,-12.4673906027143,39.3978017080178));
#198412=CARTESIAN_POINT('Ctrl Pts',(59.5707156088321,-12.4673906027143,
39.5248017080178));
#198413=CARTESIAN_POINT('Origin',(59.2743706222915,-12.2745632757592,39.3343017080178));
#198414=CARTESIAN_POINT('Origin',(59.1947980539408,-12.257649603918,39.1934008533553));
#198415=CARTESIAN_POINT('Origin',(58.3196542523186,-19.283043599959,39.192555449508));
#198416=CARTESIAN_POINT('Origin',(58.3616995707151,-19.2967593024457,39.1160373285266));
#198417=CARTESIAN_POINT('Origin',(58.2418213702174,-19.2577541638579,39.3343017080178));
#198418=CARTESIAN_POINT('Ctrl Pts',(58.1373965169893,-19.223225914144,39.2708017080178));
#198419=CARTESIAN_POINT('Ctrl Pts',(58.1769325318819,-19.1031347997388,
39.2710850691866));
#198420=CARTESIAN_POINT('Ctrl Pts',(58.281066528503,-19.1369699862884,39.3343017080178));
#198421=CARTESIAN_POINT('Ctrl Pts',(58.094557676063,-19.209428534246,39.3487519293517));
#198422=CARTESIAN_POINT('Ctrl Pts',(58.1339089916609,-19.0891556041226,
39.3492068662912));
#198423=CARTESIAN_POINT('Ctrl Pts',(58.2168625998349,-19.1161088652886,
39.4512271248732));
#198424=CARTESIAN_POINT('Ctrl Pts',(58.0133994748126,-19.1832899764602,
39.3978017080178));
#198425=CARTESIAN_POINT('Ctrl Pts',(58.0524922023745,-19.0627016856742,
39.3980347781183));
#198426=CARTESIAN_POINT('Ctrl Pts',(58.095229288236,-19.0765878066321,39.5248015355195));
#198427=CARTESIAN_POINT('Ctrl Pts',(57.9280106456676,-19.1557908785626,
39.3978017080178));
#198428=CARTESIAN_POINT('Ctrl Pts',(57.9672558039532,-19.0350067009931,
39.3978017080178));
#198429=CARTESIAN_POINT('Ctrl Pts',(57.9672558039532,-19.0350067009931,
39.5248017080178));
#198430=CARTESIAN_POINT('Origin',(57.9280106456676,-19.1557908785626,39.5248017080178));
#198431=CARTESIAN_POINT('Origin',(-0.0981128957140405,-0.301960443923711,
39.116));
#198432=CARTESIAN_POINT('Origin',(58.7434254837932,-19.4207352200701,39.116));
#198433=CARTESIAN_POINT('Origin',(-0.0981128957140404,-0.301960443923711,
39.5248017080178));
#198434=CARTESIAN_POINT('Origin',(57.7842031819383,-19.1090650011316,39.5248017080178));
#198435=CARTESIAN_POINT('Ctrl Pts',(59.2554138597571,-19.5876674457079,
39.2875012672119));
#198436=CARTESIAN_POINT('Ctrl Pts',(59.2953329099159,-19.4663243174861,
39.287208709576));
#198437=CARTESIAN_POINT('Ctrl Pts',(59.1922458813531,-19.4330302542693,
39.3549016990121));
#198438=CARTESIAN_POINT('Ctrl Pts',(59.1460959632223,-19.5520255367093,
39.1034939173931));
#198439=CARTESIAN_POINT('Ctrl Pts',(59.185827914589,-19.4307442612481,39.1031692336334));
#198440=CARTESIAN_POINT('Ctrl Pts',(59.1047949412315,-19.4046157212334,
39.2077507202299));
#198441=CARTESIAN_POINT('Ctrl Pts',(58.9497105734782,-19.4879954548404,
38.989));
#198442=CARTESIAN_POINT('Ctrl Pts',(58.9892603680794,-19.3668760934057,
38.9887769311176));
#198443=CARTESIAN_POINT('Ctrl Pts',(58.9476928828796,-19.3535701679106,
39.1161898712914));
#198444=CARTESIAN_POINT('Ctrl Pts',(58.7434254837932,-19.4207352200701,
38.989));
#198445=CARTESIAN_POINT('Ctrl Pts',(58.7827292725254,-19.2997705965405,
38.989));
#198446=CARTESIAN_POINT('Ctrl Pts',(58.7826705983486,-19.2999511770884,
39.1161895903853));
#198447=CARTESIAN_POINT('Origin',(59.1531540087999,-19.5538640879533,39.3548010137695));
#198448=CARTESIAN_POINT('Ctrl Pts',(57.7842031819382,-19.1090650011316,
39.3978017080178));
#198449=CARTESIAN_POINT('Ctrl Pts',(57.8234483402239,-18.9882808235621,
39.3978017080178));
#198450=CARTESIAN_POINT('Ctrl Pts',(57.8234483402239,-18.9882808235621,
39.5248017080178));
#198451=CARTESIAN_POINT('Ctrl Pts',(57.698525571102,-19.0814735135845,39.3978017080178));
#198452=CARTESIAN_POINT('Ctrl Pts',(57.737760932012,-18.9604392969146,39.3975666025026));
#198453=CARTESIAN_POINT('Ctrl Pts',(57.695042323134,-18.9465591794948,39.5248015517177));
#198454=CARTESIAN_POINT('Ctrl Pts',(57.6175103216835,-19.0553854270314,
39.3484894016716));
#198455=CARTESIAN_POINT('Ctrl Pts',(57.6571482613574,-18.934246652454,39.3480259000042));
#198456=CARTESIAN_POINT('Ctrl Pts',(57.5736252790861,-18.9071083904253,
39.4508333188947));
#198457=CARTESIAN_POINT('Ctrl Pts',(57.5748148483576,-19.0416371860878,
39.2708017080178));
#198458=CARTESIAN_POINT('Ctrl Pts',(57.6147155869502,-18.9204594407746,
39.27051194648));
#198459=CARTESIAN_POINT('Ctrl Pts',(57.5096375484037,-18.8863175164093,
39.3343017080178));
#198460=CARTESIAN_POINT('Origin',(57.4703923901181,-19.0071016939788,39.3343017080178));
#198461=CARTESIAN_POINT('Origin',(59.3225838821613,-19.608915190917,39.6398955068204));
#198462=CARTESIAN_POINT('Origin',(59.4920137553139,-19.6639662938562,39.92499));
#198463=CARTESIAN_POINT('Origin',(57.3930236876035,-18.9819630786538,39.1934008539947));
#198464=CARTESIAN_POINT('Origin',(57.3504898524414,-18.9681964166828,39.1160402713844));
#198465=CARTESIAN_POINT('Ctrl Pts',(59.8682321556242,-19.4684195516697,
40.1599502534424));
#198466=CARTESIAN_POINT('Ctrl Pts',(59.8327559231846,-19.4568831131884,
40.10025));
#198467=CARTESIAN_POINT('Ctrl Pts',(59.7658094374951,-19.4351129318421,
40.10025));
#198468=CARTESIAN_POINT('Ctrl Pts',(59.8409825629599,-19.5522156237493,
40.159950053846));
#198469=CARTESIAN_POINT('Ctrl Pts',(59.812903951836,-19.5179203859178,40.1002448353493));
#198470=CARTESIAN_POINT('Ctrl Pts',(59.7500277420787,-19.4836145615369,
40.10025));
#198471=CARTESIAN_POINT('Ctrl Pts',(59.7920481472525,-19.6218019328334,
40.1202442001039));
#198472=CARTESIAN_POINT('Ctrl Pts',(59.7726277678658,-19.5669820401377,
40.0633873868017));
#198473=CARTESIAN_POINT('Ctrl Pts',(59.7116747787989,-19.5206357546568,
40.0772271723536));
#198474=CARTESIAN_POINT('Ctrl Pts',(59.6899788477098,-19.7007838434707,
40.0045995998162));
#198475=CARTESIAN_POINT('Ctrl Pts',(59.6952619726974,-19.6084674936726,
39.9663485808314));
#198476=CARTESIAN_POINT('Ctrl Pts',(59.6234872553896,-19.5568961981634,
40.0101727202467));
#198477=CARTESIAN_POINT('Ctrl Pts',(59.6375245663856,-19.7118189603903,
39.9304654349859));
#198478=CARTESIAN_POINT('Ctrl Pts',(59.6577198343148,-19.600392395946,39.9051900162946));
#198479=CARTESIAN_POINT('Ctrl Pts',(59.5745070768395,-19.5572342963492,
39.9671857458179));
#198480=CARTESIAN_POINT('Ctrl Pts',(59.5942745858236,-19.6977666881846,
39.8576902534424));
#198481=CARTESIAN_POINT('Ctrl Pts',(59.6341304551457,-19.5766071063169,
39.8573998014387));
#198482=CARTESIAN_POINT('Ctrl Pts',(59.5312589135995,-19.5431821162867,
39.92499));
#198483=CARTESIAN_POINT('Origin',(59.7658094374951,-19.4351129318421,40.22725));
#198484=CARTESIAN_POINT('Origin',(-0.0981128957140405,-0.301960443923711,
39.116));
#198485=CARTESIAN_POINT('Origin',(56.9687879773466,-18.844120540552,39.116));
#198486=CARTESIAN_POINT('Origin',(5.50785759597432E-15,5.74583827070587E-15,
40.22725));
#198487=CARTESIAN_POINT('Origin',(59.7752282754837,-19.4061247292254,40.22725));
#198488=CARTESIAN_POINT('Ctrl Pts',(56.9687879773466,-18.844120540552,38.989));
#198489=CARTESIAN_POINT('Ctrl Pts',(57.0080919266514,-18.7231554228306,
38.989));
#198490=CARTESIAN_POINT('Ctrl Pts',(57.0080330916623,-18.7233364983079,
39.1161901092319));
#198491=CARTESIAN_POINT('Ctrl Pts',(56.7625017687173,-18.7768526573602,
38.989));
#198492=CARTESIAN_POINT('Ctrl Pts',(56.8019160587434,-18.6561653631331,
38.989229898976));
#198493=CARTESIAN_POINT('Ctrl Pts',(56.8430078886248,-18.6697165591959,
39.1161900493199));
#198494=CARTESIAN_POINT('Ctrl Pts',(56.5661212433894,-18.7128124416009,
39.1034966344368));
#198495=CARTESIAN_POINT('Ctrl Pts',(56.6055911857666,-18.5923760693073,
39.1038314102573));
#198496=CARTESIAN_POINT('Ctrl Pts',(56.6859069993073,-18.6186713857008,
39.2077528789603));
#198497=CARTESIAN_POINT('Ctrl Pts',(56.4568070719811,-18.677164319171,39.2875012672119));
#198498=CARTESIAN_POINT('Ctrl Pts',(56.4963948028695,-18.5568963021133,
39.2878045257868));
#198499=CARTESIAN_POINT('Ctrl Pts',(56.5984571310816,-18.590257200936,39.3549015295897));
#198500=CARTESIAN_POINT('Origin',(56.5590590327989,-18.7109915363517,39.3548010137695));
#198501=CARTESIAN_POINT('Ctrl Pts',(59.7908376697911,-19.0928077206412,
39.8576902534424));
#198502=CARTESIAN_POINT('Ctrl Pts',(59.7518659300026,-19.2142545736084,
39.8573998014387));
#198503=CARTESIAN_POINT('Ctrl Pts',(59.6489943884564,-19.1808295835782,
39.92499));
#198504=CARTESIAN_POINT('Ctrl Pts',(59.8341069976972,-19.1068672906321,
39.9304984902491));
#198505=CARTESIAN_POINT('Ctrl Pts',(59.7849495554016,-19.2088743168612,
39.9052171569785));
#198506=CARTESIAN_POINT('Ctrl Pts',(59.6922622581486,-19.1948881666553,
39.9672049726599));
#198507=CARTESIAN_POINT('Ctrl Pts',(59.8698829694067,-19.1465773683628,
40.0043437678661));
#198508=CARTESIAN_POINT('Ctrl Pts',(59.8199164124673,-19.2244455609615,
39.966162857764));
#198509=CARTESIAN_POINT('Ctrl Pts',(59.7315159919505,-19.2238994150012,
40.0100243556235));
#198510=CARTESIAN_POINT('Ctrl Pts',(59.9060262085836,-19.2694731179102,
40.1194874821988));
#198511=CARTESIAN_POINT('Ctrl Pts',(59.8580612818573,-19.3027624708828,
40.0627551483143));
#198512=CARTESIAN_POINT('Ctrl Pts',(59.7814166574712,-19.3044519280752,
40.0767884282378));
#198513=CARTESIAN_POINT('Ctrl Pts',(59.9049660265691,-19.3552948408465,
40.1599502015395));
#198514=CARTESIAN_POINT('Ctrl Pts',(59.8620777700652,-19.3665789650879,
40.1002449453869));
#198515=CARTESIAN_POINT('Ctrl Pts',(59.7910213450144,-19.3574492964897,
40.10025));
#198516=CARTESIAN_POINT('Ctrl Pts',(59.8776671349985,-19.4393816709757,
40.1599502534424));
#198517=CARTESIAN_POINT('Ctrl Pts',(59.8421853116552,-19.4278624395267,
40.10025));
#198518=CARTESIAN_POINT('Ctrl Pts',(59.7752282754837,-19.4061247292254,
40.10025));
#198519=CARTESIAN_POINT('Origin',(59.688239546742,-19.0600454060087,39.92499));
#198520=CARTESIAN_POINT('Origin',(56.3896289265489,-18.6559403576676,39.639895506932));
#198521=CARTESIAN_POINT('Origin',(56.2201988201383,-18.6008891789886,39.92499));
#198522=CARTESIAN_POINT('Origin',(59.5188096735645,-19.0049943031082,39.6398955068277));
#198523=CARTESIAN_POINT('Origin',(59.349379800228,-18.9499432001058,39.3548010137695));
#198524=CARTESIAN_POINT('Ctrl Pts',(56.1179479440988,-18.5670586829466,
39.8576902534424));
#198525=CARTESIAN_POINT('Ctrl Pts',(56.1574782858997,-18.446974339578,39.8579948730703));
#198526=CARTESIAN_POINT('Ctrl Pts',(56.2594439784239,-18.4801050014191,
39.92499));
#198527=CARTESIAN_POINT('Ctrl Pts',(56.0747358697604,-18.5530176696407,
39.9304020711232));
#198528=CARTESIAN_POINT('Ctrl Pts',(56.1242410383992,-18.4521518441035,
39.9058915297388));
#198529=CARTESIAN_POINT('Ctrl Pts',(56.2162299491247,-18.4660639121462,
39.9671523786032));
#198530=CARTESIAN_POINT('Ctrl Pts',(56.0391722633447,-18.5135050040175,
40.0043257306691));
#198531=CARTESIAN_POINT('Ctrl Pts',(56.0893377355418,-18.436379347347,39.9667894847835));
#198532=CARTESIAN_POINT('Ctrl Pts',(56.17722474395,-18.4371504234763,40.0100138975201));
#198533=CARTESIAN_POINT('Ctrl Pts',(56.0036796861845,-18.3911086652346,
40.1195533054859));
#198534=CARTESIAN_POINT('Ctrl Pts',(56.051644941423,-18.3580919822894,40.0630813209236));
#198535=CARTESIAN_POINT('Ctrl Pts',(56.1280773042132,-18.3567819283754,
40.076826594242));
#198536=CARTESIAN_POINT('Ctrl Pts',(56.0051563026344,-18.3056594201306,
40.1599502027516));
#198537=CARTESIAN_POINT('Ctrl Pts',(56.0480033886682,-18.2945198471559,
40.1002552791553));
#198538=CARTESIAN_POINT('Ctrl Pts',(56.1189701685708,-18.3039075553119,
40.10025));
#198539=CARTESIAN_POINT('Ctrl Pts',(56.0323588238391,-18.2220120550217,
40.1599502534424));
#198540=CARTESIAN_POINT('Ctrl Pts',(56.0678348753332,-18.2335490499218,
40.10025));
#198541=CARTESIAN_POINT('Ctrl Pts',(56.1347810195642,-18.2553202812749,
40.10025));
#198542=CARTESIAN_POINT('Origin',(56.1347810195642,-18.2553202812749,40.22725));
#198543=CARTESIAN_POINT('Ctrl Pts',(58.9396512752213,-18.8168143322227,
38.989));
#198544=CARTESIAN_POINT('Ctrl Pts',(58.9003474831029,-18.9377789661741,
38.989));
#198545=CARTESIAN_POINT('Ctrl Pts',(58.9004061606709,-18.9375983751889,
39.116189601327));
#198546=CARTESIAN_POINT('Ctrl Pts',(59.1460772043118,-18.8836520326604,
38.989));
#198547=CARTESIAN_POINT('Ctrl Pts',(59.1068814887033,-19.0048864565372,
38.9887769275436));
#198548=CARTESIAN_POINT('Ctrl Pts',(59.0654310094272,-18.991218198657,39.1161898821827));
#198549=CARTESIAN_POINT('Ctrl Pts',(59.3425907075097,-18.9472825415245,
39.1034967087243));
#198550=CARTESIAN_POINT('Ctrl Pts',(59.3034471832928,-19.0687550219954,
39.1031720232724));
#198551=CARTESIAN_POINT('Ctrl Pts',(59.2225318234694,-19.0422633471879,
39.2077529615016));
#198552=CARTESIAN_POINT('Ctrl Pts',(59.4519788726607,-18.9827025415097,
39.2875012672119));
#198553=CARTESIAN_POINT('Ctrl Pts',(59.4129503580329,-19.1043350338627,
39.2872087095507));
#198554=CARTESIAN_POINT('Ctrl Pts',(59.3099814352092,-19.0706774483338,
39.3549017048229));
#198555=CARTESIAN_POINT('Origin',(58.9396512752213,-18.8168143322227,39.116));
#198556=CARTESIAN_POINT('Origin',(5.72046327455653E-15,5.23458180829319E-15,
40.22725));
#198557=CARTESIAN_POINT('Origin',(56.1441998575527,-18.2263320786583,40.22725));
#198558=CARTESIAN_POINT('Origin',(56.3788528200606,-17.9847604760582,39.116));
#198559=CARTESIAN_POINT('Origin',(58.5579573083287,-18.6927400943497,39.1160373285264));
#198560=CARTESIAN_POINT('Ctrl Pts',(56.0417604764383,-18.193076743595,40.1599502534424));
#198561=CARTESIAN_POINT('Ctrl Pts',(56.0772424804484,-18.2045954185346,
40.10025));
#198562=CARTESIAN_POINT('Ctrl Pts',(56.1441998575527,-18.2263320786583,
40.10025));
#198563=CARTESIAN_POINT('Ctrl Pts',(56.0688273470726,-18.1097006409636,
40.1599500566036));
#198564=CARTESIAN_POINT('Ctrl Pts',(56.0969586315475,-18.1438516116618,
40.1002551305369));
#198565=CARTESIAN_POINT('Ctrl Pts',(56.1599138083653,-18.1778965340263,
40.10025));
#198566=CARTESIAN_POINT('Ctrl Pts',(56.1172160917342,-18.040166196385,40.1203070619044));
#198567=CARTESIAN_POINT('Ctrl Pts',(56.1367924598137,-18.0947679219781,
40.0637098684496));
#198568=CARTESIAN_POINT('Ctrl Pts',(56.1978007560413,-18.1406818860294,
40.0772636213361));
#198569=CARTESIAN_POINT('Ctrl Pts',(56.2184352456062,-17.9612165360192,
40.0046102245804));
#198570=CARTESIAN_POINT('Ctrl Pts',(56.2137528851844,-18.0530423367033,
39.9670001894015));
#198571=CARTESIAN_POINT('Ctrl Pts',(56.2852436625535,-18.1041286397846,
40.0101788811211));
#198572=CARTESIAN_POINT('Ctrl Pts',(56.2706228600015,-17.9502021467126,
39.9303710930184));
#198573=CARTESIAN_POINT('Ctrl Pts',(56.2513800597972,-18.0609092108094,
39.9058663574111));
#198574=CARTESIAN_POINT('Ctrl Pts',(56.3339837785517,-18.1037173431991,
39.9671344706364));
#198575=CARTESIAN_POINT('Ctrl Pts',(56.3138168485095,-17.9642361803973,
39.8576902534424));
#198576=CARTESIAN_POINT('Ctrl Pts',(56.2752137607566,-18.0846218068695,
39.8579948730703));
#198577=CARTESIAN_POINT('Ctrl Pts',(56.3771794532807,-18.1177524687107,
39.92499));
#198578=CARTESIAN_POINT('Origin',(56.4164246115663,-17.9969682911412,39.92499));
#198579=CARTESIAN_POINT('Origin',(58.5158800426272,-18.6791227120619,39.1925554488844));
#198580=CARTESIAN_POINT('Origin',(58.4380471616454,-18.6538332760105,39.3343017080178));
#198581=CARTESIAN_POINT('Origin',(56.5858547179429,-18.0520194698694,39.6398955069213));
#198582=CARTESIAN_POINT('Origin',(56.755284824227,-18.1070706485043,39.3548010137695));
#198583=CARTESIAN_POINT('Ctrl Pts',(58.1242364370956,-18.5518699907151,
39.3978017080178));
#198584=CARTESIAN_POINT('Ctrl Pts',(58.08499127881,-18.6726541682846,39.3978017080178));
#198585=CARTESIAN_POINT('Ctrl Pts',(58.08499127881,-18.6726541682846,39.5248017080178));
#198586=CARTESIAN_POINT('Ctrl Pts',(58.2097691178803,-18.5799074873343,
39.3978017080178));
#198587=CARTESIAN_POINT('Ctrl Pts',(58.1705159385207,-18.7004428147369,
39.3980355775177));
#198588=CARTESIAN_POINT('Ctrl Pts',(58.2133972843949,-18.7143758086137,
39.5248015517192));
#198589=CARTESIAN_POINT('Ctrl Pts',(58.2906472745453,-18.6064173144581,
39.3484893995498));
#198590=CARTESIAN_POINT('Ctrl Pts',(58.2517893143854,-18.7268501353373,
39.3489438303421));
#198591=CARTESIAN_POINT('Ctrl Pts',(58.3348142976339,-18.7538265876729,
39.4508333155594));
#198592=CARTESIAN_POINT('Ctrl Pts',(58.3332704847796,-18.6203878281148,
39.2708017080178));
#198593=CARTESIAN_POINT('Ctrl Pts',(58.2946680067388,-18.7407822670303,
39.2710850691866));
#198594=CARTESIAN_POINT('Ctrl Pts',(58.3988020033598,-18.77461745358,39.3343017080178));
#198595=CARTESIAN_POINT('Origin',(58.1242364370957,-18.5518699907151,39.5248017080178));
#198596=CARTESIAN_POINT('Ctrl Pts',(56.6526781108323,-18.0743352474892,
39.2875012672119));
#198597=CARTESIAN_POINT('Ctrl Pts',(56.6140134955962,-18.1949031876634,
39.2878045257519));
#198598=CARTESIAN_POINT('Ctrl Pts',(56.7161926816711,-18.2279043949848,
39.3549015218347));
#198599=CARTESIAN_POINT('Ctrl Pts',(56.7620702268162,-18.1097491035597,
39.1034938540228));
#198600=CARTESIAN_POINT('Ctrl Pts',(56.7232113603685,-18.2303840130645,
39.1038286278802));
#198601=CARTESIAN_POINT('Ctrl Pts',(56.803643873878,-18.2563190096466,39.2077506434033));
#198602=CARTESIAN_POINT('Ctrl Pts',(56.9585888550845,-18.1733695596523,
38.989));
#198603=CARTESIAN_POINT('Ctrl Pts',(56.9195374698062,-18.294174757132,38.9892298954611));
#198604=CARTESIAN_POINT('Ctrl Pts',(56.9607460083078,-18.307364587183,39.1161900347288));
#198605=CARTESIAN_POINT('Ctrl Pts',(57.1650137687747,-18.2401996527046,
38.989));
#198606=CARTESIAN_POINT('Ctrl Pts',(57.1257098240092,-18.3611647564555,
38.989));
#198607=CARTESIAN_POINT('Ctrl Pts',(57.1257686544522,-18.3609836949695,
39.1161900945645));
#198608=CARTESIAN_POINT('Origin',(57.1650137687747,-18.2401996527046,39.116));
#198609=CARTESIAN_POINT('Origin',(55.0155724295758,-17.5418038257016,39.5248017080178));
#198610=CARTESIAN_POINT('Origin',(57.9804289733664,-18.5051441132842,39.5248017080178));
#198611=CARTESIAN_POINT('Origin',(54.8020887275094,-17.4724387660755,39.116));
#198612=CARTESIAN_POINT('Origin',(57.5467470426661,-18.3641788932756,39.1160402713847));
#198613=CARTESIAN_POINT('Ctrl Pts',(57.7713971777987,-18.4366189870673,
39.2708017080178));
#198614=CARTESIAN_POINT('Ctrl Pts',(57.732451061807,-18.5581069080661,39.27051194648));
#198615=CARTESIAN_POINT('Ctrl Pts',(57.6273730232605,-18.5239649837008,
39.3343017080178));
#198616=CARTESIAN_POINT('Ctrl Pts',(57.8141635875301,-18.4506394153709,
39.3487519301186));
#198617=CARTESIAN_POINT('Ctrl Pts',(57.7750271733926,-18.5719407253083,
39.3482879463999));
#198618=CARTESIAN_POINT('Ctrl Pts',(57.6915769758382,-18.5448261124693,
39.451227126164));
#198619=CARTESIAN_POINT('Ctrl Pts',(57.8951845615408,-18.4772005006368,
39.3978017080178));
#198620=CARTESIAN_POINT('Ctrl Pts',(57.8557848432467,-18.5981804828678,
39.3975673827378));
#198621=CARTESIAN_POINT('Ctrl Pts',(57.8132103173517,-18.5843471808457,
39.524801535518));
#198622=CARTESIAN_POINT('Ctrl Pts',(57.9804289733664,-18.5051441132842,
39.3978017080178));
#198623=CARTESIAN_POINT('Ctrl Pts',(57.9411838150807,-18.6259282908537,
39.3978017080178));
#198624=CARTESIAN_POINT('Ctrl Pts',(57.9411838150807,-18.6259282908537,
39.5248017080178));
#198625=CARTESIAN_POINT('Origin',(57.6666181815461,-18.4031808061313,39.3343017080178));
#198626=CARTESIAN_POINT('Origin',(57.5892494801768,-18.3780421908668,39.1934008533551));
#198627=CARTESIAN_POINT('Origin',(55.9845461696115,-25.273472906795,39.1925554495078));
#198628=CARTESIAN_POINT('Origin',(56.0249274780511,-25.2915084057492,39.1160373285264));
#198629=CARTESIAN_POINT('Origin',(55.9097831300746,-25.2401862573142,39.3343017080178));
#198630=CARTESIAN_POINT('Ctrl Pts',(55.8095395120007,-25.1949317875302,
39.2708017080178));
#198631=CARTESIAN_POINT('Ctrl Pts',(55.8614118841079,-25.0796311836954,
39.2710850691866));
#198632=CARTESIAN_POINT('Ctrl Pts',(55.9614386837453,-25.1241659841936,
39.3343017080178));
#198633=CARTESIAN_POINT('Ctrl Pts',(55.7683775656457,-25.1767321129114,
39.3487519293518));
#198634=CARTESIAN_POINT('Ctrl Pts',(55.8200852551805,-25.0612313830316,
39.3492068662923));
#198635=CARTESIAN_POINT('Ctrl Pts',(55.8997670518367,-25.0967080045981,
39.4512271248733));
#198636=CARTESIAN_POINT('Ctrl Pts',(55.6903961807902,-25.1422534028232,
39.3978017080178));
#198637=CARTESIAN_POINT('Ctrl Pts',(55.7418796630219,-25.026412010048,39.3980347781178));
#198638=CARTESIAN_POINT('Ctrl Pts',(55.7829311357729,-25.0446893032922,
39.5248015355195));
#198639=CARTESIAN_POINT('Ctrl Pts',(55.6083495590301,-25.1059793847702,
39.3978017080178));
#198640=CARTESIAN_POINT('Ctrl Pts',(55.6600051127008,-24.9899591116496,
39.3978017080178));
#198641=CARTESIAN_POINT('Ctrl Pts',(55.6600051127007,-24.9899591116496,
39.5248017080178));
#198642=CARTESIAN_POINT('Origin',(55.6083495590301,-25.1059793847702,39.5248017080178));
#198643=CARTESIAN_POINT('Origin',(-0.129138884176561,-0.290050682801526,
39.116));
#198644=CARTESIAN_POINT('Origin',(56.391603244485,-25.4547063934084,39.116));
#198645=CARTESIAN_POINT('Origin',(-0.129138884176561,-0.290050682801526,
39.5248017080178));
#198646=CARTESIAN_POINT('Origin',(55.4702140717966,-25.0444775033948,39.5248017080178));
#198647=CARTESIAN_POINT('Ctrl Pts',(56.8833377255394,-25.6742415049981,
39.2875012672119));
#198648=CARTESIAN_POINT('Ctrl Pts',(56.9357219056859,-25.5577357840968,
39.287208709576));
#198649=CARTESIAN_POINT('Ctrl Pts',(56.8366797759152,-25.5138485805637,
39.3549016990124));
#198650=CARTESIAN_POINT('Ctrl Pts',(56.7783442778552,-25.6273680143744,
39.103493917393));
#198651=CARTESIAN_POINT('Ctrl Pts',(56.8305359187841,-25.510904250251,39.1031692336322));
#198652=CARTESIAN_POINT('Ctrl Pts',(56.7526780286692,-25.4764485929319,
39.2077507202294));
#198653=CARTESIAN_POINT('Ctrl Pts',(56.589727673885,-25.5431608329955,38.989));
#198654=CARTESIAN_POINT('Ctrl Pts',(56.6417212312941,-25.4268390553472,
38.9887769311182));
#198655=CARTESIAN_POINT('Ctrl Pts',(56.6017723050717,-25.4092610357534,
39.1161898712918));
#198656=CARTESIAN_POINT('Ctrl Pts',(56.391603244485,-25.4547063934084,38.989));
#198657=CARTESIAN_POINT('Ctrl Pts',(56.4433359691576,-25.3385127913796,
38.989));
#198658=CARTESIAN_POINT('Ctrl Pts',(56.4432587405967,-25.3386862495672,
39.1161895903857));
#198659=CARTESIAN_POINT('Origin',(56.7851714777847,-25.6299342604996,39.3548010137695));
#198660=CARTESIAN_POINT('Ctrl Pts',(55.4702140717966,-25.0444775033948,
39.3978017080178));
#198661=CARTESIAN_POINT('Ctrl Pts',(55.5218696254673,-24.9284572302742,
39.3978017080178));
#198662=CARTESIAN_POINT('Ctrl Pts',(55.5218696254673,-24.9284572302742,
39.5248017080178));
#198663=CARTESIAN_POINT('Ctrl Pts',(55.3878899076696,-25.0080814159061,
39.3978017080178));
#198664=CARTESIAN_POINT('Ctrl Pts',(55.4395618538391,-24.8918114493207,
39.3975666025007));
#198665=CARTESIAN_POINT('Ctrl Pts',(55.3985281293138,-24.8735420580978,
39.5248015517177));
#198666=CARTESIAN_POINT('Ctrl Pts',(55.310045415862,-24.9736678430965,39.3484894016716));
#198667=CARTESIAN_POINT('Ctrl Pts',(55.3621286647035,-24.8573359723221,
39.3480259000056));
#198668=CARTESIAN_POINT('Ctrl Pts',(55.2818999508933,-24.8216158475497,
39.4508333188947));
#198669=CARTESIAN_POINT('Ctrl Pts',(55.269020915304,-24.9555320242416,39.2708017080178));
#198670=CARTESIAN_POINT('Ctrl Pts',(55.3213695969755,-24.8391888661845,
39.27051194648));
#198671=CARTESIAN_POINT('Ctrl Pts',(55.2204359898056,-24.7942503289608,
39.3343017080178));
#198672=CARTESIAN_POINT('Origin',(55.168780436135,-24.9102706020814,39.3343017080178));
#198673=CARTESIAN_POINT('Origin',(56.9479187893821,-25.7023940320519,39.639895506819));
#198674=CARTESIAN_POINT('Origin',(57.1106661007665,-25.7748538035648,39.92499));
#198675=CARTESIAN_POINT('Origin',(55.0944632682975,-24.8771824671421,39.1934008539943));
#198676=CARTESIAN_POINT('Origin',(55.0536014459542,-24.8590452239599,39.1160402713843));
#198677=CARTESIAN_POINT('Ctrl Pts',(57.5052637377732,-25.6197038181298,
40.1599502534424));
#198678=CARTESIAN_POINT('Ctrl Pts',(57.4711877340329,-25.6045223014062,
40.10025));
#198679=CARTESIAN_POINT('Ctrl Pts',(57.4068835917979,-25.5758735661209,
40.10025));
#198680=CARTESIAN_POINT('Ctrl Pts',(57.4694043465863,-25.7001924885131,
40.1599500538461));
#198681=CARTESIAN_POINT('Ctrl Pts',(57.4450643815388,-25.6631501095107,
40.1002448353478));
#198682=CARTESIAN_POINT('Ctrl Pts',(57.3861185493426,-25.622459862444,40.10025));
#198683=CARTESIAN_POINT('Ctrl Pts',(57.4134642487753,-25.76428255724,40.1202442001039));
#198684=CARTESIAN_POINT('Ctrl Pts',(57.3998804953989,-25.7077329912391,
40.0633873868017));
#198685=CARTESIAN_POINT('Ctrl Pts',(57.3441059191831,-25.6552692732805,
40.0772271723538));
#198686=CARTESIAN_POINT('Ctrl Pts',(57.3036982377902,-25.8321626496791,
40.0045995998162));
#198687=CARTESIAN_POINT('Ctrl Pts',(57.3186021074451,-25.7409042554406,
39.9663485808314));
#198688=CARTESIAN_POINT('Ctrl Pts',(57.2526112478171,-25.6821129719826,
40.0101727202466));
#198689=CARTESIAN_POINT('Ctrl Pts',(57.2503778226941,-25.8376543496545,
39.9304654349859));
#198690=CARTESIAN_POINT('Ctrl Pts',(57.28210970638,-25.7289491719111,39.905190016295));
#198691=CARTESIAN_POINT('Ctrl Pts',(57.203864046926,-25.6773293952366,39.9671857458181));
#198692=CARTESIAN_POINT('Ctrl Pts',(57.2088336324698,-25.8191582032621,
39.8576902534424));
#198693=CARTESIAN_POINT('Ctrl Pts',(57.2611357920724,-25.7028284190334,
39.8573998014387));
#198694=CARTESIAN_POINT('Ctrl Pts',(57.1623216544371,-25.6588335304441,
39.92499));
#198695=CARTESIAN_POINT('Origin',(57.4068835917979,-25.5758735661209,40.22725));
#198696=CARTESIAN_POINT('Origin',(-0.129138884176561,-0.290050682801526,
39.116));
#198697=CARTESIAN_POINT('Origin',(54.6869600343297,-24.6957503380308,39.116));
#198698=CARTESIAN_POINT('Origin',(5.51404277916147E-15,5.76195122378986E-15,
40.22725));
#198699=CARTESIAN_POINT('Origin',(57.4192809246789,-25.5480287005719,40.22725));
#198700=CARTESIAN_POINT('Ctrl Pts',(54.6869600343297,-24.6957503380308,
38.989));
#198701=CARTESIAN_POINT('Ctrl Pts',(54.7386929703524,-24.5795562613018,
38.989));
#198702=CARTESIAN_POINT('Ctrl Pts',(54.738615530126,-24.5797301948982,39.1161901092324));
#198703=CARTESIAN_POINT('Ctrl Pts',(54.4888352915926,-24.6072881749603,
38.989));
#198704=CARTESIAN_POINT('Ctrl Pts',(54.5406489234191,-24.4913819335269,
38.9892298989766));
#198705=CARTESIAN_POINT('Ctrl Pts',(54.5800991622563,-24.5091541605502,
39.1161900493204));
#198706=CARTESIAN_POINT('Ctrl Pts',(54.3002245846702,-24.5230714236766,
39.1034966344368));
#198707=CARTESIAN_POINT('Ctrl Pts',(54.3520673354864,-24.4074205468509,
39.1038314102554));
#198708=CARTESIAN_POINT('Ctrl Pts',(54.4291945615848,-24.4419671033155,
39.2077528789597));
#198709=CARTESIAN_POINT('Ctrl Pts',(54.1952354911872,-24.4761921430393,
39.2875012672119));
#198710=CARTESIAN_POINT('Ctrl Pts',(54.2471777873472,-24.3607210114364,
39.2878045257868));
#198711=CARTESIAN_POINT('Ctrl Pts',(54.3451938439593,-24.4045675740909,
39.35490152959));
#198712=CARTESIAN_POINT('Origin',(54.2933913980363,-24.5205222915152,39.3548010137695));
#198713=CARTESIAN_POINT('Ctrl Pts',(57.467555354514,-25.2380597013431,39.8576902534424));
#198714=CARTESIAN_POINT('Ctrl Pts',(57.4161024530843,-25.3547675996716,
39.8573998014387));
#198715=CARTESIAN_POINT('Ctrl Pts',(57.317288315449,-25.3107727110823,39.92499));
#198716=CARTESIAN_POINT('Ctrl Pts',(57.5091180232691,-25.256565127891,39.9304984902491));
#198717=CARTESIAN_POINT('Ctrl Pts',(57.4495672328902,-25.3528749970549,
39.9052171569785));
#198718=CARTESIAN_POINT('Ctrl Pts',(57.3588496371383,-25.3292770036978,
39.9672049726604));
#198719=CARTESIAN_POINT('Ctrl Pts',(57.540547177061,-25.2997972770056,40.0043437678662));
#198720=CARTESIAN_POINT('Ctrl Pts',(57.4827148996401,-25.372015972086,39.9661628577643));
#198721=CARTESIAN_POINT('Ctrl Pts',(57.3948558336735,-25.3622324578621,
40.0100243556233));
#198722=CARTESIAN_POINT('Ctrl Pts',(57.5636463159493,-25.4257977880273,
40.1194874821987));
#198723=CARTESIAN_POINT('Ctrl Pts',(57.5124644611998,-25.4538910783597,
40.062755148314));
#198724=CARTESIAN_POINT('Ctrl Pts',(57.4360631077221,-25.4475597357237,
40.0767884282379));
#198725=CARTESIAN_POINT('Ctrl Pts',(57.5536211289093,-25.5110385513885,
40.159950201539));
#198726=CARTESIAN_POINT('Ctrl Pts',(57.5097883065949,-25.5177778164711,
40.1002449453884));
#198727=CARTESIAN_POINT('Ctrl Pts',(57.4400754463057,-25.5012707422382,
40.10025));
#198728=CARTESIAN_POINT('Ctrl Pts',(57.5176823163888,-25.5918112338795,
40.1599502534424));
#198729=CARTESIAN_POINT('Ctrl Pts',(57.4835989537477,-25.5766462455177,
40.10025));
#198730=CARTESIAN_POINT('Ctrl Pts',(57.4192809246789,-25.5480287005719,
40.10025));
#198731=CARTESIAN_POINT('Origin',(57.3689438691196,-25.1947524379617,39.92499));
#198732=CARTESIAN_POINT('Origin',(54.1306438627446,-24.4480624203072,39.6398955069309));
#198733=CARTESIAN_POINT('Origin',(53.9678963272934,-24.375602549094,39.92499));
#198734=CARTESIAN_POINT('Origin',(57.2061965577021,-25.1222926664875,39.639895506828));
#198735=CARTESIAN_POINT('Origin',(57.0434492461379,-25.0498328948966,39.3548010137695));
#198736=CARTESIAN_POINT('Ctrl Pts',(53.8697418420145,-24.3312692531089,
39.8576902534424));
#198737=CARTESIAN_POINT('Ctrl Pts',(53.9216078643417,-24.2159747902187,
39.8579948730703));
#198738=CARTESIAN_POINT('Ctrl Pts',(54.0195518809641,-24.2595822759734,
39.92499));
#198739=CARTESIAN_POINT('Ctrl Pts',(53.8282341734846,-24.3127882662175,
39.9304020711228));
#198740=CARTESIAN_POINT('Ctrl Pts',(53.88801149737,-24.2176496934284,39.905891529739));
#198741=CARTESIAN_POINT('Ctrl Pts',(53.9780422761236,-24.2411010091825,
39.9671523786032));
#198742=CARTESIAN_POINT('Ctrl Pts',(53.7969955864427,-24.2697746459838,
40.0043257306697));
#198743=CARTESIAN_POINT('Ctrl Pts',(53.8549480733038,-24.1983152114488,
39.9667894847838));
#198744=CARTESIAN_POINT('Ctrl Pts',(53.9422730280819,-24.2082687574721,
40.0100138975202));
#198745=CARTESIAN_POINT('Ctrl Pts',(53.7744913425366,-24.1443388226042,
40.1195533054853));
#198746=CARTESIAN_POINT('Ctrl Pts',(53.8256450222193,-24.1165167429224,
40.0630813209234));
#198747=CARTESIAN_POINT('Ctrl Pts',(53.9017956184508,-24.1232032230476,
40.0768265942419));
#198748=CARTESIAN_POINT('Ctrl Pts',(53.7848917482049,-24.0595120258532,
40.1599502027519));
#198749=CARTESIAN_POINT('Ctrl Pts',(53.828668515863,-24.052912216684,40.1002552791553));
#198750=CARTESIAN_POINT('Ctrl Pts',(53.8982652496115,-24.0696665464379,
40.10025));
#198751=CARTESIAN_POINT('Ctrl Pts',(53.8206887816836,-23.9791663275014,
40.1599502534424));
#198752=CARTESIAN_POINT('Ctrl Pts',(53.8547645473081,-23.9943483786818,
40.10025));
#198753=CARTESIAN_POINT('Ctrl Pts',(53.9190682401995,-24.0229981225297,
40.10025));
#198754=CARTESIAN_POINT('Origin',(53.9190682401995,-24.0229981225297,40.22725));
#198755=CARTESIAN_POINT('Ctrl Pts',(56.6498810128382,-24.8746050278053,
38.989));
#198756=CARTESIAN_POINT('Ctrl Pts',(56.5981482837089,-24.9907986398441,
38.989));
#198757=CARTESIAN_POINT('Ctrl Pts',(56.5982255167331,-24.9906251716316,
39.1161896013266));
#198758=CARTESIAN_POINT('Ctrl Pts',(56.8481896769747,-24.9626539694743,
38.989));
#198759=CARTESIAN_POINT('Ctrl Pts',(56.7965362315769,-25.0791271905737,
38.9887769275436));
#198760=CARTESIAN_POINT('Ctrl Pts',(56.756741544355,-25.0612010539386,39.1161898821824));
#198761=CARTESIAN_POINT('Ctrl Pts',(57.0369754593327,-25.0464771582524,
39.1034967087243));
#198762=CARTESIAN_POINT('Ctrl Pts',(56.9853490357212,-25.1631925873307,
39.1031720232733));
#198763=CARTESIAN_POINT('Ctrl Pts',(56.9076460727631,-25.1283880784731,
39.207752961502));
#198764=CARTESIAN_POINT('Ctrl Pts',(57.1420619865021,-25.0931373005746,
39.2875012672119));
#198765=CARTESIAN_POINT('Ctrl Pts',(57.0905332166521,-25.2100238867499,
39.2872087095507));
#198766=CARTESIAN_POINT('Ctrl Pts',(56.9916465440542,-25.1657874977295,
39.3549017048227));
#198767=CARTESIAN_POINT('Origin',(56.6498810128382,-24.8746050278053,39.116));
#198768=CARTESIAN_POINT('Origin',(5.71826297912856E-15,5.2288498427347E-15,
40.22725));
#198769=CARTESIAN_POINT('Origin',(53.9314655730804,-23.9951532569808,40.22725));
#198770=CARTESIAN_POINT('Origin',(52.0578415156894,-22.8300973196049,39.116));
#198771=CARTESIAN_POINT('Origin',(56.2832472948507,-24.7113125977907,39.1160373285278));
#198772=CARTESIAN_POINT('Ctrl Pts',(53.8330634946837,-23.9513722670365,
40.1599502534424));
#198773=CARTESIAN_POINT('Ctrl Pts',(53.867147095173,-23.9665367208225,40.10025));
#198774=CARTESIAN_POINT('Ctrl Pts',(53.9314655730804,-23.9951532569808,
40.10025));
#198775=CARTESIAN_POINT('Ctrl Pts',(53.8686972660496,-23.8712821658118,
40.1599500566043));
#198776=CARTESIAN_POINT('Ctrl Pts',(53.8931046959182,-23.9081865738548,
40.1002551305372));
#198777=CARTESIAN_POINT('Ctrl Pts',(53.9521563342717,-23.9486256024593,
40.10025));
#198778=CARTESIAN_POINT('Ctrl Pts',(53.9240892607411,-23.8071866393154,
40.1203070619045));
#198779=CARTESIAN_POINT('Ctrl Pts',(53.93785095296,-23.8635355386145,40.0637098684499));
#198780=CARTESIAN_POINT('Ctrl Pts',(53.9937257232527,-23.9155750846179,
40.0772636213363));
#198781=CARTESIAN_POINT('Ctrl Pts',(54.0330064121713,-23.739249756057,40.0046102245803));
#198782=CARTESIAN_POINT('Ctrl Pts',(54.018751292376,-23.8300830854575,39.9670001894012));
#198783=CARTESIAN_POINT('Ctrl Pts',(54.0845104630313,-23.8883623535216,
40.0101788811209));
#198784=CARTESIAN_POINT('Ctrl Pts',(54.0860594545423,-23.7337507958619,
39.9303710930185));
#198785=CARTESIAN_POINT('Ctrl Pts',(54.055350029128,-23.8418399747435,39.9058663574109));
#198786=CARTESIAN_POINT('Ctrl Pts',(54.1330265677739,-23.8930480394867,
39.9671344706363));
#198787=CARTESIAN_POINT('Ctrl Pts',(54.1275498658873,-23.7522229508828,
39.8576902534424));
#198788=CARTESIAN_POINT('Ctrl Pts',(54.0765745253536,-23.8679139708569,
39.8579948730703));
#198789=CARTESIAN_POINT('Ctrl Pts',(54.1745185419759,-23.9115214566115,
39.92499));
#198790=CARTESIAN_POINT('Origin',(54.2261740956466,-23.7955011834909,39.92499));
#198791=CARTESIAN_POINT('Origin',(56.2428239368584,-24.6933715410261,39.1925554488854));
#198792=CARTESIAN_POINT('Origin',(56.1680608984278,-24.6600848917112,39.3343017080178));
#198793=CARTESIAN_POINT('Origin',(54.3889216310581,-23.8679610547541,39.639895506921));
#198794=CARTESIAN_POINT('Origin',(54.5516691663895,-23.9404209259122,39.3548010137695));
#198795=CARTESIAN_POINT('Ctrl Pts',(55.8666273273833,-24.5258780191672,
39.3978017080178));
#198796=CARTESIAN_POINT('Ctrl Pts',(55.8149717737126,-24.6418982922878,
39.3978017080178));
#198797=CARTESIAN_POINT('Ctrl Pts',(55.8149717737126,-24.6418982922878,
39.5248017080178));
#198798=CARTESIAN_POINT('Ctrl Pts',(55.9487607347573,-24.5627025231285,
39.3978017080178));
#198799=CARTESIAN_POINT('Ctrl Pts',(55.8971232158787,-24.6784744708791,
39.3980355775201));
#198800=CARTESIAN_POINT('Ctrl Pts',(55.9383132588166,-24.6968134595446,
39.5248015517192));
#198801=CARTESIAN_POINT('Ctrl Pts',(56.0264248009279,-24.5975211960716,
39.3484893995498));
#198802=CARTESIAN_POINT('Ctrl Pts',(55.9751910510459,-24.7132325104956,
39.3489438303403));
#198803=CARTESIAN_POINT('Ctrl Pts',(56.0549414076394,-24.748739656915,39.4508333155588));
#198804=CARTESIAN_POINT('Ctrl Pts',(56.0673542004326,-24.6158705164594,
39.2708017080178));
#198805=CARTESIAN_POINT('Ctrl Pts',(56.0163785451197,-24.7315703643336,
39.2710850691866));
#198806=CARTESIAN_POINT('Ctrl Pts',(56.1164053447572,-24.7761051648318,
39.3343017080178));
#198807=CARTESIAN_POINT('Origin',(55.8666273273833,-24.5258780191672,39.5248017080178));
#198808=CARTESIAN_POINT('Ctrl Pts',(54.4530463244692,-23.8971395307769,
39.2875012672119));
#198809=CARTESIAN_POINT('Ctrl Pts',(54.4019907365351,-24.0130054343463,
39.2878045257519));
#198810=CARTESIAN_POINT('Ctrl Pts',(54.5001606088505,-24.0565064908993,
39.3549015218348));
#198811=CARTESIAN_POINT('Ctrl Pts',(54.5581374230424,-23.9437939758158,
39.1034938540228));
#198812=CARTESIAN_POINT('Ctrl Pts',(54.5068816478264,-24.0597061770704,
39.1038286278777));
#198813=CARTESIAN_POINT('Ctrl Pts',(54.5841625982698,-24.0939065860605,
39.207750643403));
#198814=CARTESIAN_POINT('Ctrl Pts',(54.7469293531951,-24.02760770261,38.989));
#198815=CARTESIAN_POINT('Ctrl Pts',(54.6954643138426,-24.1436691352852,
38.9892298954653));
#198816=CARTESIAN_POINT('Ctrl Pts',(54.7350683949955,-24.1610941752714,
39.116190034729));
#198817=CARTESIAN_POINT('Ctrl Pts',(54.9452378026828,-24.1156489724277,
38.989));
#198818=CARTESIAN_POINT('Ctrl Pts',(54.893504872635,-24.231843035737,38.989));
#198819=CARTESIAN_POINT('Ctrl Pts',(54.8935823068776,-24.2316691155805,
39.1161900945647));
#198820=CARTESIAN_POINT('Origin',(54.9452378026828,-24.1156489724277,39.116));
#198821=CARTESIAN_POINT('Origin',(50.7999799080414,-22.2700612497317,39.5248017080178));
#198822=CARTESIAN_POINT('Origin',(55.7284918401498,-24.4643761377918,39.5248017080178));
#198823=CARTESIAN_POINT('Origin',(50.6030043228557,-22.1823620689016,39.116));
#198824=CARTESIAN_POINT('Origin',(55.3119205422644,-24.2788510342443,39.116040271385));
#198825=CARTESIAN_POINT('Ctrl Pts',(55.5277679687683,-24.3743766270215,
39.2708017080178));
#198826=CARTESIAN_POINT('Ctrl Pts',(55.4763362579874,-24.4911280468227,
39.27051194648));
#198827=CARTESIAN_POINT('Ctrl Pts',(55.3754026508175,-24.4461895095989,
39.3343017080178));
#198828=CARTESIAN_POINT('Ctrl Pts',(55.5688345658079,-24.3927905570397,
39.3487519301186));
#198829=CARTESIAN_POINT('Ctrl Pts',(55.5172331055236,-24.5093364964848,
39.3482879463991));
#198830=CARTESIAN_POINT('Ctrl Pts',(55.4370743056947,-24.4736474994207,
39.4512271261635));
#198831=CARTESIAN_POINT('Ctrl Pts',(55.6466353090197,-24.4276751358079,
39.3978017080178));
#198832=CARTESIAN_POINT('Ctrl Pts',(55.5948055748743,-24.5438739850305,
39.3975673827378));
#198833=CARTESIAN_POINT('Ctrl Pts',(55.5539102504896,-24.5256662135185,
39.524801535518));
#198834=CARTESIAN_POINT('Ctrl Pts',(55.7284918401498,-24.4643761377918,
39.3978017080178));
#198835=CARTESIAN_POINT('Ctrl Pts',(55.6768362864792,-24.5803964109124,
39.3978017080178));
#198836=CARTESIAN_POINT('Ctrl Pts',(55.6768362864792,-24.5803964109124,
39.5248017080178));
#198837=CARTESIAN_POINT('Origin',(55.4270582044881,-24.3301692364783,39.3343017080178));
#198838=CARTESIAN_POINT('Origin',(55.3527410377822,-24.2970811017181,39.1934008533554));
#198839=CARTESIAN_POINT('Origin',(53.0360596835511,-30.9870007556522,39.1925554495084));
#198840=CARTESIAN_POINT('Origin',(53.0743345559682,-31.0091584503702,39.1160373285271));
#198841=CARTESIAN_POINT('Origin',(52.9651856060845,-30.9460815882869,39.3343017080178));
#198842=CARTESIAN_POINT('Ctrl Pts',(52.8702215132216,-30.8905967158737,
39.2708017080178));
#198843=CARTESIAN_POINT('Ctrl Pts',(52.9338619179795,-30.7813498801533,
39.2710850691866));
#198844=CARTESIAN_POINT('Ctrl Pts',(53.0286856060846,-30.8360963620063,
39.3343017080178));
#198845=CARTESIAN_POINT('Ctrl Pts',(52.8311874403366,-30.8681941459771,
39.3487519293518));
#198846=CARTESIAN_POINT('Ctrl Pts',(52.8946849835388,-30.7587310665065,
39.3492068662923));
#198847=CARTESIAN_POINT('Ctrl Pts',(52.9702219582398,-30.8023423591853,
39.4512271248733));
#198848=CARTESIAN_POINT('Ctrl Pts',(52.7572372522455,-30.8257530395517,
39.3978017080178));
#198849=CARTESIAN_POINT('Ctrl Pts',(52.8205474253444,-30.7159277273278,
39.3980347781178));
#198850=CARTESIAN_POINT('Ctrl Pts',(52.8594635164578,-30.7383959430075,
39.5248015355195));
#198851=CARTESIAN_POINT('Ctrl Pts',(52.6794317578287,-30.7811015270744,
39.3978017080178));
#198852=CARTESIAN_POINT('Ctrl Pts',(52.7429317578287,-30.6711163007938,
39.3978017080178));
#198853=CARTESIAN_POINT('Ctrl Pts',(52.7429317578287,-30.6711163007938,
39.5248017080178));
#198854=CARTESIAN_POINT('Origin',(52.6794317578287,-30.7811015270744,39.5248017080178));
#198855=CARTESIAN_POINT('Origin',(-0.158749999999995,-0.274963065701559,
39.116));
#198856=CARTESIAN_POINT('Origin',(53.4219427993286,-31.2097904767607,39.116));
#198857=CARTESIAN_POINT('Origin',(-0.158749999999995,-0.274963065701559,
39.5248017080178));
#198858=CARTESIAN_POINT('Origin',(52.5484816883959,-30.705497469237,39.5248017080178));
#198859=CARTESIAN_POINT('Ctrl Pts',(53.888035839597,-31.479523201679,39.2875012672119));
#198860=CARTESIAN_POINT('Ctrl Pts',(53.9523112176912,-31.3691313491576,
39.287208709576));
#198861=CARTESIAN_POINT('Ctrl Pts',(53.8583991130131,-31.3151318426936,
39.3549016990122));
#198862=CARTESIAN_POINT('Ctrl Pts',(53.7885171709483,-31.4219316852008,
39.1034939173931));
#198863=CARTESIAN_POINT('Ctrl Pts',(53.8525966788904,-31.3115614337832,
39.1031692336328));
#198864=CARTESIAN_POINT('Ctrl Pts',(53.7787668993595,-31.2691561625549,
39.2077507202297));
#198865=CARTESIAN_POINT('Ctrl Pts',(53.6097358757348,-31.3184699958138,
38.989));
#198866=CARTESIAN_POINT('Ctrl Pts',(53.673603543663,-31.2082202476927,38.98877693112));
#198867=CARTESIAN_POINT('Ctrl Pts',(53.6357108652107,-31.1865627224601,
39.1161898712915));
#198868=CARTESIAN_POINT('Ctrl Pts',(53.4219427993286,-31.2097904767607,
38.989));
#198869=CARTESIAN_POINT('Ctrl Pts',(53.485537665384,-31.0996409376522,38.989));
#198870=CARTESIAN_POINT('Ctrl Pts',(53.4854427285717,-31.0998053730347,
39.1161895903854));
#198871=CARTESIAN_POINT('Origin',(53.7950387249979,-31.4251975098794,39.3548010137695));
#198872=CARTESIAN_POINT('Ctrl Pts',(52.5484816883959,-30.705497469237,39.3978017080178));
#198873=CARTESIAN_POINT('Ctrl Pts',(52.6119816883959,-30.5955122429563,
39.3978017080178));
#198874=CARTESIAN_POINT('Ctrl Pts',(52.6119816883959,-30.5955122429563,
39.5248017080178));
#198875=CARTESIAN_POINT('Ctrl Pts',(52.4704129317475,-30.6606955449584,
39.3978017080178));
#198876=CARTESIAN_POINT('Ctrl Pts',(52.5339553345207,-30.5504637065424,
39.3975666025026));
#198877=CARTESIAN_POINT('Ctrl Pts',(52.495056068421,-30.5280052047887,39.5248015517177));
#198878=CARTESIAN_POINT('Ctrl Pts',(52.3965920780923,-30.6183335281988,
39.3484894016716));
#198879=CARTESIAN_POINT('Ctrl Pts',(52.4605500011273,-30.5080831175497,
39.3480259000042));
#198880=CARTESIAN_POINT('Ctrl Pts',(52.3844945583579,-30.4641724871917,
39.4508333188945));
#198881=CARTESIAN_POINT('Ctrl Pts',(52.3576880233162,-30.5960088312569,
39.2708017080178));
#198882=CARTESIAN_POINT('Ctrl Pts',(52.4219111049556,-30.4857749404421,
39.27051194648));
#198883=CARTESIAN_POINT('Ctrl Pts',(52.3262277788841,-30.4305321463777,
39.3343017080178));
#198884=CARTESIAN_POINT('Origin',(52.2627277788841,-30.5405173726584,39.3343017080178));
#198885=CARTESIAN_POINT('Origin',(53.9493203812237,-31.5142720656047,39.6398955068192));
#198886=CARTESIAN_POINT('Origin',(54.1036020372438,-31.6033466212666,39.92499));
#198887=CARTESIAN_POINT('Origin',(52.1922763801647,-30.4998422386361,39.1934008539946));
#198888=CARTESIAN_POINT('Origin',(52.1535342613175,-30.4775331296741,39.1160402713851));
#198889=CARTESIAN_POINT('Ctrl Pts',(54.5122556166611,-31.4902932482909,
40.1599502534424));
#198890=CARTESIAN_POINT('Ctrl Pts',(54.4799531854479,-31.471632985199,40.10025));
#198891=CARTESIAN_POINT('Ctrl Pts',(54.4189959163063,-31.4364195775136,
40.10025));
#198892=CARTESIAN_POINT('Ctrl Pts',(54.4681793099457,-31.5665926662617,
40.1599500538463));
#198893=CARTESIAN_POINT('Ctrl Pts',(54.4478446647267,-31.5272089901453,
40.1002448353502));
#198894=CARTESIAN_POINT('Ctrl Pts',(54.3934750329626,-31.4805801312538,
40.10025));
#198895=CARTESIAN_POINT('Ctrl Pts',(54.4058464214488,-31.624484310427,40.120244200104));
#198896=CARTESIAN_POINT('Ctrl Pts',(54.3982481205269,-31.5668246399991,
40.0633873868021));
#198897=CARTESIAN_POINT('Ctrl Pts',(54.3482630350907,-31.5088182930358,
40.0772271723539));
#198898=CARTESIAN_POINT('Ctrl Pts',(54.2895863184075,-31.68051887617,40.0045995998161));
#198899=CARTESIAN_POINT('Ctrl Pts',(54.3139476428155,-31.5913182835559,
39.9663485808311));
#198900=CARTESIAN_POINT('Ctrl Pts',(54.2544636505348,-31.5259511417534,
40.0101727202464));
#198901=CARTESIAN_POINT('Ctrl Pts',(54.2359839591653,-31.6804069909876,
39.930465434986));
#198902=CARTESIAN_POINT('Ctrl Pts',(54.2789047974524,-31.5756141966193,
39.9051900162949));
#198903=CARTESIAN_POINT('Ctrl Pts',(54.2064835118365,-31.5160982999431,
39.9671857458177));
#198904=CARTESIAN_POINT('Ctrl Pts',(54.1966007261207,-31.6576696180585,
39.8576902534424));
#198905=CARTESIAN_POINT('Ctrl Pts',(54.2607761425982,-31.5474441649284,
39.8573998014387));
#198906=CARTESIAN_POINT('Ctrl Pts',(54.1671020372438,-31.493361394986,39.92499));
#198907=CARTESIAN_POINT('Origin',(54.4189959163063,-31.4364195775136,40.22725));
#198908=CARTESIAN_POINT('Origin',(-0.158749999999995,-0.274963065701559,
39.116));
#198909=CARTESIAN_POINT('Origin',(51.8059703131946,-30.2768083268881,39.116));
#198910=CARTESIAN_POINT('Origin',(5.52187834149254E-15,5.77732938073734E-15,
40.22725));
#198911=CARTESIAN_POINT('Origin',(54.4342359163063,-31.4100231232062,40.22725));
#198912=CARTESIAN_POINT('Ctrl Pts',(51.8059703131946,-30.2768083268881,
38.989));
#198913=CARTESIAN_POINT('Ctrl Pts',(51.8695654390622,-30.1666583377718,
38.989));
#198914=CARTESIAN_POINT('Ctrl Pts',(51.8694702420498,-30.1668232238339,
39.1161901092325));
#198915=CARTESIAN_POINT('Ctrl Pts',(51.6181777324916,-30.1681210939088,
38.989));
#198916=CARTESIAN_POINT('Ctrl Pts',(51.6818230251202,-30.0582657983057,
38.989229898976));
#198917=CARTESIAN_POINT('Ctrl Pts',(51.7191994478434,-30.0800643400506,
39.1161900493205));
#198918=CARTESIAN_POINT('Ctrl Pts',(51.4394033023489,-30.0646505034511,
39.1034966344368));
#198919=CARTESIAN_POINT('Ctrl Pts',(51.5030508615836,-29.9550522173033,
39.1038314102562));
#198920=CARTESIAN_POINT('Ctrl Pts',(51.5761444782074,-29.9974715145367,
39.2077528789596));
#198921=CARTESIAN_POINT('Ctrl Pts',(51.3398895692697,-30.0070536838159,
39.2875012672119));
#198922=CARTESIAN_POINT('Ctrl Pts',(51.4036173400347,-29.89764456355,39.2878045257868));
#198923=CARTESIAN_POINT('Ctrl Pts',(51.4965132406194,-29.9514963979198,
39.3549015295901));
#198924=CARTESIAN_POINT('Origin',(51.4328740054943,-30.0614010732037,39.3548010137695));
#198925=CARTESIAN_POINT('Ctrl Pts',(54.5146464769138,-31.1067982185536,
39.8576902534424));
#198926=CARTESIAN_POINT('Ctrl Pts',(54.4512761425982,-31.2174884860866,
39.8573998014387));
#198927=CARTESIAN_POINT('Ctrl Pts',(54.3576020372438,-31.1634057161441,
39.92499));
#198928=CARTESIAN_POINT('Ctrl Pts',(54.5540471172213,-31.1295467523332,
39.930498490249));
#198929=CARTESIAN_POINT('Ctrl Pts',(54.4847554296804,-31.2191042733502,
39.9052171569796));
#198930=CARTESIAN_POINT('Ctrl Pts',(54.3970014563933,-31.186152981396,39.9672049726602));
#198931=CARTESIAN_POINT('Ctrl Pts',(54.5807851087098,-31.1758273123588,
40.0043437678663));
#198932=CARTESIAN_POINT('Ctrl Pts',(54.5157207333391,-31.2416052667848,
39.9661628577649));
#198933=CARTESIAN_POINT('Ctrl Pts',(54.4293656242365,-31.2226915745263,
40.0100243556234));
#198934=CARTESIAN_POINT('Ctrl Pts',(54.5905870683102,-31.3035520968883,
40.1194874821986));
#198935=CARTESIAN_POINT('Ctrl Pts',(54.5367490446502,-31.3261415286131,
40.0627551483135));
#198936=CARTESIAN_POINT('Ctrl Pts',(54.4614280312964,-31.3118587536634,
40.0767884282378));
#198937=CARTESIAN_POINT('Ctrl Pts',(54.5717067142913,-31.3872779850332,
40.1599502015378));
#198938=CARTESIAN_POINT('Ctrl Pts',(54.5274095677394,-31.3893985541585,
40.1002449453863));
#198939=CARTESIAN_POINT('Ctrl Pts',(54.4598040608964,-31.3656949292499,
40.10025));
#198940=CARTESIAN_POINT('Ctrl Pts',(54.5275217339719,-31.4638515574741,
40.1599502534424));
#198941=CARTESIAN_POINT('Ctrl Pts',(54.4952102564865,-31.4452069629854,
40.10025));
#198942=CARTESIAN_POINT('Ctrl Pts',(54.4342359163063,-31.4100231232062,
40.10025));
#198943=CARTESIAN_POINT('Origin',(54.4211020372438,-31.0534204898635,39.92499));
#198944=CARTESIAN_POINT('Origin',(51.2785921372171,-29.9723263949888,39.6398955069324));
#198945=CARTESIAN_POINT('Origin',(51.1243102687785,-29.8832517167487,39.92499));
#198946=CARTESIAN_POINT('Origin',(54.2668203811903,-30.9643459342374,39.6398955068261));
#198947=CARTESIAN_POINT('Origin',(54.1125387249979,-30.8752713784762,39.3548010137695));
#198948=CARTESIAN_POINT('Ctrl Pts',(51.0313275753408,-29.8289013456886,
39.8576902534424));
#198949=CARTESIAN_POINT('Ctrl Pts',(51.0949610232001,-29.7196599535393,
39.8579948730703));
#198950=CARTESIAN_POINT('Ctrl Pts',(51.1878102687784,-29.7732664904681,
39.92499));
#198951=CARTESIAN_POINT('Ctrl Pts',(50.9919790793208,-29.8061828667725,
39.9304020711234));
#198952=CARTESIAN_POINT('Ctrl Pts',(51.0613736255819,-29.7178139048433,
39.9058915297385));
#198953=CARTESIAN_POINT('Ctrl Pts',(51.1484598763128,-29.7505475307853,
39.9671523786031));
#198954=CARTESIAN_POINT('Ctrl Pts',(50.9654077681509,-29.7601395581528,
40.0043257306689));
#198955=CARTESIAN_POINT('Ctrl Pts',(51.0305123301031,-29.695129270271,39.9667894847832));
#198956=CARTESIAN_POINT('Ctrl Pts',(51.1163184807719,-29.7141562330558,
40.0100138975197));
#198957=CARTESIAN_POINT('Ctrl Pts',(50.9561384187037,-29.6330385513047,
40.1195533054861));
#198958=CARTESIAN_POINT('Ctrl Pts',(51.009920072411,-29.6107158994144,40.0630813209239));
#198959=CARTESIAN_POINT('Ctrl Pts',(51.0849545802166,-29.6253256551027,
40.0768265942423));
#198960=CARTESIAN_POINT('Ctrl Pts',(50.9753486645701,-29.5497635830446,
40.1599502027516));
#198961=CARTESIAN_POINT('Ctrl Pts',(51.0195754864255,-29.5477758465709,
40.1002552791557));
#198962=CARTESIAN_POINT('Ctrl Pts',(51.087039657642,-29.5717132339806,40.10025));
#198963=CARTESIAN_POINT('Ctrl Pts',(51.0193480105327,-29.4735998357338,
40.1599502534424));
#198964=CARTESIAN_POINT('Ctrl Pts',(51.0516501490686,-29.4922606054647,
40.10025));
#198965=CARTESIAN_POINT('Ctrl Pts',(51.1126068659047,-29.5274749692186,
40.10025));
#198966=CARTESIAN_POINT('Origin',(51.1126068659047,-29.5274749692186,40.22725));
#198967=CARTESIAN_POINT('Ctrl Pts',(53.7394427993286,-30.6598643453575,
38.989));
#198968=CARTESIAN_POINT('Ctrl Pts',(53.6758479277944,-30.7700138939557,
38.989));
#198969=CARTESIAN_POINT('Ctrl Pts',(53.6759428700937,-30.7698494490694,
39.1161896013268));
#198970=CARTESIAN_POINT('Ctrl Pts',(53.9274614872889,-30.7681598456259,
38.989));
#198971=CARTESIAN_POINT('Ctrl Pts',(53.8639162380529,-30.8785957589612,
38.9887769275478));
#198972=CARTESIAN_POINT('Ctrl Pts',(53.8262133418071,-30.856608146078,39.116189882185));
#198973=CARTESIAN_POINT('Ctrl Pts',(54.1064511722697,-30.8712573299205,
39.1034967087243));
#198974=CARTESIAN_POINT('Ctrl Pts',(54.0429074791709,-30.9819369489461,
39.1031720232688));
#198975=CARTESIAN_POINT('Ctrl Pts',(53.9692682429978,-30.9392009315196,
39.2077529614995));
#198976=CARTESIAN_POINT('Ctrl Pts',(54.2060847114741,-30.9286463962979,
39.2875012672119));
#198977=CARTESIAN_POINT('Ctrl Pts',(54.1426202463873,-31.0395064423977,
39.2872087095507));
#198978=CARTESIAN_POINT('Ctrl Pts',(54.0488992470933,-30.9851759130203,
39.3549017048228));
#198979=CARTESIAN_POINT('Origin',(53.7394427993286,-30.6598643453575,39.116));
#198980=CARTESIAN_POINT('Origin',(5.71547558359784E-15,5.22337927098311E-15,
40.22725));
#198981=CARTESIAN_POINT('Origin',(51.1278468659047,-29.5010785149112,40.22725));
#198982=CARTESIAN_POINT('Origin',(46.8255917980722,-26.6681506086452,39.116));
#198983=CARTESIAN_POINT('Origin',(53.3918862459806,-30.4591427892376,39.1160373285258));
#198984=CARTESIAN_POINT('Ctrl Pts',(51.0345602039887,-29.4472515437736,
40.1599502534424));
#198985=CARTESIAN_POINT('Ctrl Pts',(51.0668719738977,-29.4658956314768,
40.10025));
#198986=CARTESIAN_POINT('Ctrl Pts',(51.1278468659047,-29.5010785149112,
40.10025));
#198987=CARTESIAN_POINT('Ctrl Pts',(51.0783704650306,-29.3713249278649,
40.159950056604));
#198988=CARTESIAN_POINT('Ctrl Pts',(51.0987866273847,-29.4105784408364,
40.1002551305372));
#198989=CARTESIAN_POINT('Ctrl Pts',(51.1532877451689,-29.4569685172212,
40.10025));
#198990=CARTESIAN_POINT('Ctrl Pts',(51.1401588234665,-29.313370563451,40.1203070619045));
#198991=CARTESIAN_POINT('Ctrl Pts',(51.1479550638452,-29.3708492661234,
40.0637098684496));
#198992=CARTESIAN_POINT('Ctrl Pts',(51.1980841325266,-29.4284442379231,
40.0772636213363));
#198993=CARTESIAN_POINT('Ctrl Pts',(51.2555806533509,-29.2571907880104,
40.0046102245803));
#198994=CARTESIAN_POINT('Ctrl Pts',(51.2319089562572,-29.3460364571626,
39.9670001894015));
#198995=CARTESIAN_POINT('Ctrl Pts',(51.2912160489646,-29.4108701703525,
40.0101788811209));
#198996=CARTESIAN_POINT('Ctrl Pts',(51.3089178634638,-29.2572675046848,
39.9303710930185));
#198997=CARTESIAN_POINT('Ctrl Pts',(51.2670782717319,-29.3615545506881,
39.9058663574108));
#198998=CARTESIAN_POINT('Ctrl Pts',(51.3389765898564,-29.4206015015123,
39.967134470637));
#198999=CARTESIAN_POINT('Ctrl Pts',(51.3482501200165,-29.2799753962463,
39.8576902534424));
#199000=CARTESIAN_POINT('Ctrl Pts',(51.2854610232001,-29.3897042746975,
39.8579948730703));
#199001=CARTESIAN_POINT('Ctrl Pts',(51.3783102687785,-29.4433108116262,
39.92499));
#199002=CARTESIAN_POINT('Origin',(51.4418102687785,-29.3333255853456,39.92499));
#199003=CARTESIAN_POINT('Origin',(53.3535596824668,-30.4370746239674,39.1925554488849));
#199004=CARTESIAN_POINT('Origin',(53.2826856060845,-30.3961554568838,39.3343017080178));
#199005=CARTESIAN_POINT('Origin',(51.5960921371721,-29.4224002636276,39.6398955069211));
#199006=CARTESIAN_POINT('Origin',(51.7503740054943,-29.5114749418006,39.3548010137695));
#199007=CARTESIAN_POINT('Ctrl Pts',(52.9969317578287,-30.2311753956713,
39.3978017080178));
#199008=CARTESIAN_POINT('Ctrl Pts',(52.9334317578287,-30.3411606219519,
39.3978017080178));
#199009=CARTESIAN_POINT('Ctrl Pts',(52.9334317578287,-30.3411606219519,
39.5248017080178));
#199010=CARTESIAN_POINT('Ctrl Pts',(53.0747660209943,-30.2763834500017,
39.3978017080178));
#199011=CARTESIAN_POINT('Ctrl Pts',(53.01130991406,-30.3861235964155,39.3980355775177));
#199012=CARTESIAN_POINT('Ctrl Pts',(53.0503573673287,-30.4086676540719,
39.5248015517192));
#199013=CARTESIAN_POINT('Ctrl Pts',(53.1483650929077,-30.3191294881007,
39.3484893995498));
#199014=CARTESIAN_POINT('Ctrl Pts',(53.0853168809867,-30.4288515386937,
39.3489438303415));
#199015=CARTESIAN_POINT('Ctrl Pts',(53.1609188493341,-30.4725003554697,
39.4508333155587));
#199016=CARTESIAN_POINT('Ctrl Pts',(53.1871522506175,-30.3416565762237,
39.2708017080178));
#199017=CARTESIAN_POINT('Ctrl Pts',(53.1243619179795,-30.4513942013114,
39.2710850691866));
#199018=CARTESIAN_POINT('Ctrl Pts',(53.2191856060846,-30.5061406831644,
39.3343017080178));
#199019=CARTESIAN_POINT('Origin',(52.9969317578287,-30.2311753956713,39.5248017080178));
#199020=CARTESIAN_POINT('Ctrl Pts',(51.6568155675427,-29.4581217525674,
39.2875012672119));
#199021=CARTESIAN_POINT('Ctrl Pts',(51.5939283826162,-29.5680161684457,
39.2878045257519));
#199022=CARTESIAN_POINT('Ctrl Pts',(51.6870133715071,-29.6215404675517,
39.3549015218347));
#199023=CARTESIAN_POINT('Ctrl Pts',(51.7564542486366,-29.5155056307135,
39.1034938540228));
#199024=CARTESIAN_POINT('Ctrl Pts',(51.6933631336526,-29.6254251653838,
39.1038286278802));
#199025=CARTESIAN_POINT('Ctrl Pts',(51.7666458147672,-29.6675162799446,
39.2077506434033));
#199026=CARTESIAN_POINT('Ctrl Pts',(51.9354510367802,-29.6185943474781,
38.989));
#199027=CARTESIAN_POINT('Ctrl Pts',(51.8721362050942,-29.7286404220051,
38.9892298954629));
#199028=CARTESIAN_POINT('Ctrl Pts',(51.9097019182957,-29.7501097595404,
39.1161900347288));
#199029=CARTESIAN_POINT('Ctrl Pts',(52.1234703131946,-29.726882195485,38.989));
#199030=CARTESIAN_POINT('Ctrl Pts',(52.059875194672,-29.8370321718795,38.989));
#199031=CARTESIAN_POINT('Ctrl Pts',(52.0599703843284,-29.8368672985583,
39.1161900945645));
#199032=CARTESIAN_POINT('Origin',(52.1234703131946,-29.726882195485,39.116));
#199033=CARTESIAN_POINT('Origin',(45.6951875,-26.0155113828601,39.5248017080178));
#199034=CARTESIAN_POINT('Origin',(52.8659816883959,-30.1555713378339,39.5248017080178));
#199035=CARTESIAN_POINT('Origin',(45.518171167873,-25.9133109558556,39.116));
#199036=CARTESIAN_POINT('Origin',(52.4710850656383,-29.9275190026069,39.1160402713844));
#199037=CARTESIAN_POINT('Ctrl Pts',(52.6757649139395,-30.0450834959837,
39.2708017080178));
#199038=CARTESIAN_POINT('Ctrl Pts',(52.6124111049556,-30.1558192616002,
39.27051194648));
#199039=CARTESIAN_POINT('Ctrl Pts',(52.5167277788841,-30.1005764675359,
39.3343017080178));
#199040=CARTESIAN_POINT('Ctrl Pts',(52.7146817640556,-30.0676891808479,
39.3487519301186));
#199041=CARTESIAN_POINT('Ctrl Pts',(52.6511806140165,-30.1782028480937,
39.3482879463998));
#199042=CARTESIAN_POINT('Ctrl Pts',(52.5751914485008,-30.1343304829269,
39.451227126164));
#199043=CARTESIAN_POINT('Ctrl Pts',(52.7884098752456,-30.1105150503719,
39.3978017080178));
#199044=CARTESIAN_POINT('Ctrl Pts',(52.7247179826675,-30.2206596676788,
39.3975673827383));
#199045=CARTESIAN_POINT('Ctrl Pts',(52.6859499175227,-30.1982769148317,
39.524801535518));
#199046=CARTESIAN_POINT('Ctrl Pts',(52.8659816883959,-30.1555713378339,
39.3978017080178));
#199047=CARTESIAN_POINT('Ctrl Pts',(52.8024816883959,-30.2655565641145,
39.3978017080178));
#199048=CARTESIAN_POINT('Ctrl Pts',(52.8024816883959,-30.2655565641145,
39.5248017080178));
#199049=CARTESIAN_POINT('Origin',(52.5802277788841,-29.9905912412552,39.3343017080178));
#199050=CARTESIAN_POINT('Origin',(52.5097763812718,-29.9499161075303,39.1934008533552));
#199051=CARTESIAN_POINT('Origin',(49.5064990290885,-36.3610285397819,39.1925554495083));
#199052=CARTESIAN_POINT('Origin',(49.5422481179708,-36.3870656659259,39.1160373285269));
#199053=CARTESIAN_POINT('Origin',(49.4402904249165,-36.3129251734944,39.3343017080178));
#199054=CARTESIAN_POINT('Ctrl Pts',(49.3516463037385,-36.2478178023251,
39.2708017080178));
#199055=CARTESIAN_POINT('Ctrl Pts',(49.4263574835551,-36.1458216659126,
39.2710850691866));
#199056=CARTESIAN_POINT('Ctrl Pts',(49.5149391519577,-36.2101800152087,
39.3343017080178));
#199057=CARTESIAN_POINT('Ctrl Pts',(49.3151677697926,-36.221457784398,39.3487519293518));
#199058=CARTESIAN_POINT('Ctrl Pts',(49.3897594742889,-36.1192316557404,
39.3492068662938));
#199059=CARTESIAN_POINT('Ctrl Pts',(49.4603240281391,-36.1704998050822,
39.4512271248739));
#199060=CARTESIAN_POINT('Ctrl Pts',(49.2460589922044,-36.1715192752735,
39.3978017080178));
#199061=CARTESIAN_POINT('Ctrl Pts',(49.3205022166686,-36.0689133127034,
39.398034778115));
#199062=CARTESIAN_POINT('Ctrl Pts',(49.3568565533009,-36.0953262843471,
39.5248015355195));
#199063=CARTESIAN_POINT('Ctrl Pts',(49.1733470784087,-36.1189794796884,
39.3978017080178));
#199064=CARTESIAN_POINT('Ctrl Pts',(49.2479958054498,-36.0162343214027,
39.3978017080178));
#199065=CARTESIAN_POINT('Ctrl Pts',(49.2479958054498,-36.0162343214027,
39.5248017080178));
#199066=CARTESIAN_POINT('Origin',(49.1733470784087,-36.1189794796884,39.5248017080178));
#199067=CARTESIAN_POINT('Origin',(-0.186621817602855,-0.256862895714046,
39.116));
#199068=CARTESIAN_POINT('Origin',(49.8669803696025,-36.622933564581,39.116));
#199069=CARTESIAN_POINT('Origin',(-0.186621817602855,-0.256862895714046,
39.5248017080178));
#199070=CARTESIAN_POINT('Origin',(49.0510171431403,-36.0301015792677,39.5248017080178));
#199071=CARTESIAN_POINT('Ctrl Pts',(50.3023253561995,-36.9399086546487,
39.2875012672119));
#199072=CARTESIAN_POINT('Ctrl Pts',(50.3777877177488,-36.8368401467437,
39.287208709576));
#199073=CARTESIAN_POINT('Ctrl Pts',(50.2900345588337,-36.7733199672421,
39.3549016990124));
#199074=CARTESIAN_POINT('Ctrl Pts',(50.2093718139448,-36.8722300970239,
39.1034939173931));
#199075=CARTESIAN_POINT('Ctrl Pts',(50.2846371204137,-36.7691625978866,
39.1031692336317));
#199076=CARTESIAN_POINT('Ctrl Pts',(50.2156443459739,-36.7192723137719,
39.207750720229));
#199077=CARTESIAN_POINT('Ctrl Pts',(50.0423845927703,-36.7506474475485,
38.989));
#199078=CARTESIAN_POINT('Ctrl Pts',(50.1174266236752,-36.6476776482607,
38.9887769311194));
#199079=CARTESIAN_POINT('Ctrl Pts',(50.0820053531129,-36.6221779017697,
39.1161898712918));
#199080=CARTESIAN_POINT('Ctrl Pts',(49.8669803696025,-36.622933564581,38.989));
#199081=CARTESIAN_POINT('Ctrl Pts',(49.9417406183804,-36.5200349097932,
38.989));
#199082=CARTESIAN_POINT('Ctrl Pts',(49.9416290134639,-36.5201885207826,
39.1161895903857));
#199083=CARTESIAN_POINT('Origin',(50.2155162706044,-36.8761597191955,39.3548010137695));
#199084=CARTESIAN_POINT('Ctrl Pts',(49.0510171431403,-36.0301015792677,
39.3978017080178));
#199085=CARTESIAN_POINT('Ctrl Pts',(49.1256658701815,-35.9273564209821,
39.3978017080178));
#199086=CARTESIAN_POINT('Ctrl Pts',(49.1256658701815,-35.9273564209821,
39.5248017080178));
#199087=CARTESIAN_POINT('Ctrl Pts',(48.9780591316059,-35.977384677456,39.3978017080178));
#199088=CARTESIAN_POINT('Ctrl Pts',(49.0527758071209,-35.8743986902987,
39.3975666025003));
#199089=CARTESIAN_POINT('Ctrl Pts',(49.0164371879474,-35.8479971380611,
39.5248015517177));
#199090=CARTESIAN_POINT('Ctrl Pts',(48.9090707128239,-35.9275383438668,
39.3484894016716));
#199091=CARTESIAN_POINT('Ctrl Pts',(48.9842025736662,-35.8245773199091,
39.348025900006));
#199092=CARTESIAN_POINT('Ctrl Pts',(48.9131536812787,-35.7729572780248,
39.450833318895));
#199093=CARTESIAN_POINT('Ctrl Pts',(48.8727133447943,-35.9012693628905,
39.2708017080178));
#199094=CARTESIAN_POINT('Ctrl Pts',(48.9481071848796,-35.7983524848936,
39.27051194648));
#199095=CARTESIAN_POINT('Ctrl Pts',(48.85872246645,-35.7334106856007,39.3343017080178));
#199096=CARTESIAN_POINT('Origin',(48.7840737394089,-35.8361558438863,39.3343017080178));
#199097=CARTESIAN_POINT('Origin',(50.3596419293498,-36.9808731396198,39.6398955068187));
#199098=CARTESIAN_POINT('Origin',(50.5037675878945,-37.0855865599603,39.92499));
#199099=CARTESIAN_POINT('Origin',(48.7182599900762,-35.788339356061,39.1934008539944));
#199100=CARTESIAN_POINT('Origin',(48.6820620414866,-35.7621028045849,39.1160402713842));
#199101=CARTESIAN_POINT('Ctrl Pts',(50.9219998155899,-37.015868435856,40.1599502534424));
#199102=CARTESIAN_POINT('Ctrl Pts',(50.8918248691,-36.9939338721434,40.10025));
#199103=CARTESIAN_POINT('Ctrl Pts',(50.8348823336486,-36.9525415975213,
40.10025));
#199104=CARTESIAN_POINT('Ctrl Pts',(50.8701895025857,-37.0871426490242,
40.1599500538461));
#199105=CARTESIAN_POINT('Ctrl Pts',(50.8540829678232,-37.0458491715906,
40.1002448353499));
#199106=CARTESIAN_POINT('Ctrl Pts',(50.8048852215543,-36.9937925764098,
40.10025));
#199107=CARTESIAN_POINT('Ctrl Pts',(50.8021467555734,-37.1382015956601,
40.120244200104));
#199108=CARTESIAN_POINT('Ctrl Pts',(50.8006171556815,-37.0800635522214,
40.0633873868017));
#199109=CARTESIAN_POINT('Ctrl Pts',(50.7569692080814,-37.0171501059293,
40.0772271723536));
#199110=CARTESIAN_POINT('Ctrl Pts',(50.6806663304943,-37.1817767082786,
40.0045995998161));
#199111=CARTESIAN_POINT('Ctrl Pts',(50.7142182018865,-37.0956112176473,
39.9663485808314));
#199112=CARTESIAN_POINT('Ctrl Pts',(50.66189279602,-37.0243843935847,40.0101727202468));
#199113=CARTESIAN_POINT('Ctrl Pts',(50.627369305771,-37.1760624637753,39.930465434986));
#199114=CARTESIAN_POINT('Ctrl Pts',(50.6810088489711,-37.0763301845677,
39.9051900162952));
#199115=CARTESIAN_POINT('Ctrl Pts',(50.6152053999547,-37.0095702365075,
39.9671857458188));
#199116=CARTESIAN_POINT('Ctrl Pts',(50.5905785208484,-37.1493329797261,
39.8576902534424));
#199117=CARTESIAN_POINT('Ctrl Pts',(50.6659240749083,-37.0464195108254,
39.8573998014387));
#199118=CARTESIAN_POINT('Ctrl Pts',(50.5784163149356,-36.9828414016747,
39.92499));
#199119=CARTESIAN_POINT('Origin',(50.8348823336486,-36.9525415975213,40.22725));
#199120=CARTESIAN_POINT('Origin',(-0.186621817602855,-0.256862895714046,
39.116));
#199121=CARTESIAN_POINT('Origin',(48.3573835402119,-35.5261472678866,39.116));
#199122=CARTESIAN_POINT('Origin',(5.53127843490691E-15,5.79180425524272E-15,
40.22725));
#199123=CARTESIAN_POINT('Origin',(50.8527980281384,-36.9278827595327,40.22725));
#199124=CARTESIAN_POINT('Ctrl Pts',(48.3573835402119,-35.5261472678866,
38.989));
#199125=CARTESIAN_POINT('Ctrl Pts',(48.4321440944169,-35.4232481927144,
38.989));
#199126=CARTESIAN_POINT('Ctrl Pts',(48.4320321836173,-35.4234022247157,
39.116190109232));
#199127=CARTESIAN_POINT('Ctrl Pts',(48.1819806163554,-35.3984257650676,
38.989));
#199128=CARTESIAN_POINT('Ctrl Pts',(48.2567602586447,-35.2958250128969,
38.9892298989754));
#199129=CARTESIAN_POINT('Ctrl Pts',(48.2916533613393,-35.3214110399816,
39.11619004932));
#199130=CARTESIAN_POINT('Ctrl Pts',(48.015001153061,-35.2768349808754,39.1034966344368));
#199131=CARTESIAN_POINT('Ctrl Pts',(48.0897561847329,-35.174490067168,39.103831410257));
#199132=CARTESIAN_POINT('Ctrl Pts',(48.1580153629272,-35.224317350472,39.2077528789602));
#199133=CARTESIAN_POINT('Ctrl Pts',(47.9220530736687,-35.2091516650529,
39.2875012672119));
#199134=CARTESIAN_POINT('Ctrl Pts',(47.9968681042461,-35.1070032653414,
39.2878045257868));
#199135=CARTESIAN_POINT('Ctrl Pts',(48.0836260618767,-35.1702703594593,
39.3549015295898));
#199136=CARTESIAN_POINT('Origin',(48.0088472823272,-35.2729208539816,39.3548010137695));
#199137=CARTESIAN_POINT('Ctrl Pts',(50.9644637245892,-36.6347241449655,
39.8576902534424));
#199138=CARTESIAN_POINT('Ctrl Pts',(50.8898702560317,-36.7381840359685,
39.8573998014387));
#199139=CARTESIAN_POINT('Ctrl Pts',(50.8023624960591,-36.6746059268179,
39.92499));
#199140=CARTESIAN_POINT('Ctrl Pts',(51.0012706547892,-36.6614665482797,
39.930498490249));
#199141=CARTESIAN_POINT('Ctrl Pts',(50.9229972443175,-36.7432905102106,
39.9052171569798));
#199142=CARTESIAN_POINT('Ctrl Pts',(50.8391683443881,-36.7013469409082,
39.9672049726599));
#199143=CARTESIAN_POINT('Ctrl Pts',(51.0230245369438,-36.7102884597167,
40.0043437678662));
#199144=CARTESIAN_POINT('Ctrl Pts',(50.9514409225347,-36.7689049964551,
39.9661628577646));
#199145=CARTESIAN_POINT('Ctrl Pts',(50.8675358949426,-36.7410683485315,
40.0100243556238));
#199146=CARTESIAN_POINT('Ctrl Pts',(51.0194219249361,-36.8383381382862,
40.1194874821987));
#199147=CARTESIAN_POINT('Ctrl Pts',(50.9635175930198,-36.8551762168616,
40.0627551483138));
#199148=CARTESIAN_POINT('Ctrl Pts',(50.8901021525742,-36.8330984946703,
40.0767884282374));
#199149=CARTESIAN_POINT('Ctrl Pts',(50.9918932610486,-36.9196318328644,
40.1599502015385));
#199150=CARTESIAN_POINT('Ctrl Pts',(50.9476171190673,-36.9171104726339,
40.1002449453869));
#199151=CARTESIAN_POINT('Ctrl Pts',(50.8828596657514,-36.8864699989243,
40.10025));
#199152=CARTESIAN_POINT('Ctrl Pts',(50.9399462128201,-36.9911673391708,
40.1599502534424));
#199153=CARTESIAN_POINT('Ctrl Pts',(50.9097606317993,-36.9692474126341,
40.10025));
#199154=CARTESIAN_POINT('Ctrl Pts',(50.8527980281385,-36.9278827595327,
40.10025));
#199155=CARTESIAN_POINT('Origin',(50.8770112231002,-36.5718607685322,39.92499));
#199156=CARTESIAN_POINT('Origin',(47.8647214254963,-35.1682072895739,39.6398955069324));
#199157=CARTESIAN_POINT('Origin',(47.720595568509,-35.0634937251222,39.92499));
#199158=CARTESIAN_POINT('Origin',(50.7328855645148,-36.4671473482219,39.6398955068281));
#199159=CARTESIAN_POINT('Origin',(50.5887599058101,-36.3624339277674,39.3548010137695));
#199160=CARTESIAN_POINT('Ctrl Pts',(47.6338034047599,-34.9997217530261,
39.8576902534424));
#199161=CARTESIAN_POINT('Ctrl Pts',(47.7085070967803,-34.8977303031703,
39.8579948730703));
#199162=CARTESIAN_POINT('Ctrl Pts',(47.7952442955502,-34.9607485668366,
39.92499));
#199163=CARTESIAN_POINT('Ctrl Pts',(47.5970451916076,-34.9730146904934,
39.9304020711229));
#199164=CARTESIAN_POINT('Ctrl Pts',(47.6752966590745,-34.8923835282623,
39.905891529738));
#199165=CARTESIAN_POINT('Ctrl Pts',(47.7584842465947,-34.9340408279389,
39.9671523786029));
#199166=CARTESIAN_POINT('Ctrl Pts',(47.5754322771535,-34.9244461536122,
40.0043257306695));
#199167=CARTESIAN_POINT('Ctrl Pts',(47.646975614992,-34.866597278702,39.9667894847838));
#199168=CARTESIAN_POINT('Ctrl Pts',(47.7303228514092,-34.8944891948622,
40.0100138975201));
#199169=CARTESIAN_POINT('Ctrl Pts',(47.5794993790985,-34.7970725085259,
40.1195533054855));
#199170=CARTESIAN_POINT('Ctrl Pts',(47.6353197637778,-34.7804938560726,
40.0630813209234));
#199171=CARTESIAN_POINT('Ctrl Pts',(47.7084160893875,-34.8028668197834,
40.076826594242));
#199172=CARTESIAN_POINT('Ctrl Pts',(47.607308993689,-34.7162617467342,40.1599502027513));
#199173=CARTESIAN_POINT('Ctrl Pts',(47.6515013114247,-34.7189078610121,
40.1002552791553));
#199174=CARTESIAN_POINT('Ctrl Pts',(47.7160937685333,-34.7497660430526,
40.10025));
#199175=CARTESIAN_POINT('Ctrl Pts',(47.6590285860935,-34.6451144164186,
40.1599502534424));
#199176=CARTESIAN_POINT('Ctrl Pts',(47.6892031885513,-34.6670494534018,
40.10025));
#199177=CARTESIAN_POINT('Ctrl Pts',(47.7461450747864,-34.7084426211232,
40.10025));
#199178=CARTESIAN_POINT('Origin',(47.7461450747864,-34.7084426211232,40.22725));
#199179=CARTESIAN_POINT('Ctrl Pts',(50.2402240048083,-36.1092077731529,
38.989));
#199180=CARTESIAN_POINT('Ctrl Pts',(50.1654637495898,-36.2121064368054,
38.989));
#199181=CARTESIAN_POINT('Ctrl Pts',(50.1655753609565,-36.2119528169382,
39.1161896013266));
#199182=CARTESIAN_POINT('Ctrl Pts',(50.4158927445019,-36.2365633238569,
38.989));
#199183=CARTESIAN_POINT('Ctrl Pts',(50.3411519064808,-36.3397519704545,
38.988776927546));
#199184=CARTESIAN_POINT('Ctrl Pts',(50.305953882031,-36.3139437822107,39.1161898821848));
#199185=CARTESIAN_POINT('Ctrl Pts',(50.5831252836581,-36.3578055460602,
39.1034967087243));
#199186=CARTESIAN_POINT('Ctrl Pts',(50.5083605190648,-36.4612367259614,
39.1031720232708));
#199187=CARTESIAN_POINT('Ctrl Pts',(50.4395918165621,-36.4110374247136,
39.2077529615001));
#199188=CARTESIAN_POINT('Ctrl Pts',(50.6762142289948,-36.4252947698679,
39.2875012672119));
#199189=CARTESIAN_POINT('Ctrl Pts',(50.6015093986316,-36.5289136700279,
39.2872087095507));
#199190=CARTESIAN_POINT('Ctrl Pts',(50.5139808995223,-36.4650842569433,
39.3549017048227));
#199191=CARTESIAN_POINT('Origin',(50.2402240048083,-36.1092077731529,39.116));
#199192=CARTESIAN_POINT('Origin',(5.7121316272531E-15,5.21823002976732E-15,
40.22725));
#199193=CARTESIAN_POINT('Origin',(47.7640607692763,-34.6837837831347,40.22725));
#199194=CARTESIAN_POINT('Origin',(40.9117478092586,-29.3316730956005,39.116));
#199195=CARTESIAN_POINT('Origin',(49.915552518432,-35.8732562382992,39.1160373285272));
#199196=CARTESIAN_POINT('Ctrl Pts',(47.6769115920304,-34.6205005703635,
40.1599502534424));
#199197=CARTESIAN_POINT('Ctrl Pts',(47.7070975168464,-34.6424200234575,
40.10025));
#199198=CARTESIAN_POINT('Ctrl Pts',(47.7640607692763,-34.6837837831347,
40.10025));
#199199=CARTESIAN_POINT('Ctrl Pts',(47.7284183483606,-34.5495693076631,
40.1599500566037));
#199200=CARTESIAN_POINT('Ctrl Pts',(47.7446195594518,-34.5907418558593,
40.1002551305372));
#199201=CARTESIAN_POINT('Ctrl Pts',(47.7939730310155,-34.6425747206412,
40.10025));
#199202=CARTESIAN_POINT('Ctrl Pts',(47.7959261043554,-34.4983910654767,
40.1203070619046));
#199203=CARTESIAN_POINT('Ctrl Pts',(47.797671475652,-34.5563698228277,40.0637098684499));
#199204=CARTESIAN_POINT('Ctrl Pts',(47.8415056181568,-34.61888919786,40.0772636213363));
#199205=CARTESIAN_POINT('Ctrl Pts',(47.9165880269728,-34.4545839152292,
40.0046102245802));
#199206=CARTESIAN_POINT('Ctrl Pts',(47.8837591046489,-34.5404685123897,
39.9670001894012));
#199207=CARTESIAN_POINT('Ctrl Pts',(47.9359643384884,-34.6111463389765,
40.0101788811208));
#199208=CARTESIAN_POINT('Ctrl Pts',(47.9696250311906,-34.4602354682513,
39.9303710930186));
#199209=CARTESIAN_POINT('Ctrl Pts',(47.9171136764635,-34.5595777906764,
39.9058663574114));
#199210=CARTESIAN_POINT('Ctrl Pts',(47.9824460410477,-34.62581669683,39.9671344706362));
#199211=CARTESIAN_POINT('Ctrl Pts',(48.0063682005187,-34.4869303039397,
39.8576902534424));
#199212=CARTESIAN_POINT('Ctrl Pts',(47.9324532779037,-34.5894948283134,
39.8579948730703));
#199213=CARTESIAN_POINT('Ctrl Pts',(48.0191904766736,-34.6525130919798,
39.92499));
#199214=CARTESIAN_POINT('Origin',(48.0938392037147,-34.5497679336941,39.92499));
#199215=CARTESIAN_POINT('Origin',(49.8797426632453,-35.8473027479611,39.1925554488851));
#199216=CARTESIAN_POINT('Origin',(49.8135340601223,-35.7991993820663,39.3343017080178));
#199217=CARTESIAN_POINT('Origin',(48.237965060651,-34.6544814981838,39.6398955069206));
#199218=CARTESIAN_POINT('Origin',(48.3820909175329,-34.7591950625535,39.3548010137695));
#199219=CARTESIAN_POINT('Ctrl Pts',(49.5465907136144,-35.6052536882603,
39.3978017080178));
#199220=CARTESIAN_POINT('Ctrl Pts',(49.4719419865733,-35.7079988465459,
39.3978017080178));
#199221=CARTESIAN_POINT('Ctrl Pts',(49.4719419865733,-35.7079988465459,
39.5248017080178));
#199222=CARTESIAN_POINT('Ctrl Pts',(49.6192730640956,-35.6583499840576,
39.3978017080178));
#199223=CARTESIAN_POINT('Ctrl Pts',(49.544693607491,-35.7608559931226,39.3980355775163));
#199224=CARTESIAN_POINT('Ctrl Pts',(49.5811706590223,-35.7873581223577,
39.5248015517192));
#199225=CARTESIAN_POINT('Ctrl Pts',(49.6880007749198,-35.7085550527712,
39.3484893995498));
#199226=CARTESIAN_POINT('Ctrl Pts',(49.6138288703675,-35.8110857017868,
39.348943830343));
#199227=CARTESIAN_POINT('Ctrl Pts',(49.6844541394794,-35.8623979633502,
39.450833315559));
#199228=CARTESIAN_POINT('Ctrl Pts',(49.7242207306175,-35.735013097139,39.2708017080178));
#199229=CARTESIAN_POINT('Ctrl Pts',(49.6503036646785,-35.8375861910557,
39.2710850691866));
#199230=CARTESIAN_POINT('Ctrl Pts',(49.7388853330811,-35.9019445403519,
39.3343017080178));
#199231=CARTESIAN_POINT('Origin',(49.5465907136144,-35.6052536882603,39.5248017080178));
#199232=CARTESIAN_POINT('Ctrl Pts',(48.2946219293746,-34.6963546279286,
39.2875012672119));
#199233=CARTESIAN_POINT('Ctrl Pts',(48.2205921526136,-34.7990735298986,
39.2878045257519));
#199234=CARTESIAN_POINT('Ctrl Pts',(48.3075723994627,-34.8620346481358,
39.3549015218347));
#199235=CARTESIAN_POINT('Ctrl Pts',(48.3877165307504,-34.7638392294009,
39.1034938540228));
#199236=CARTESIAN_POINT('Ctrl Pts',(48.3134813154502,-34.8665617960632,
39.1038286278789));
#199237=CARTESIAN_POINT('Ctrl Pts',(48.3819628268489,-34.9160824571376,
39.207750643403));
#199238=CARTESIAN_POINT('Ctrl Pts',(48.5549570506147,-34.8850734745854,
38.989));
#199239=CARTESIAN_POINT('Ctrl Pts',(48.4804861171459,-34.9878985031429,
38.9892298954635));
#199240=CARTESIAN_POINT('Ctrl Pts',(48.5156018845772,-35.0131769156741,
39.1161900347288));
#199241=CARTESIAN_POINT('Ctrl Pts',(48.7306271754176,-35.0124214764585,
38.989));
#199242=CARTESIAN_POINT('Ctrl Pts',(48.6558666298469,-35.1153205397466,
38.989));
#199243=CARTESIAN_POINT('Ctrl Pts',(48.6559785319992,-35.1151665196473,
39.1161900945645));
#199244=CARTESIAN_POINT('Origin',(48.7306271754176,-35.0124214764585,39.116));
#199245=CARTESIAN_POINT('Origin',(39.9252688514646,-28.6149541797807,39.5248017080178));
#199246=CARTESIAN_POINT('Origin',(49.424260778346,-35.5163757878396,39.5248017080178));
#199247=CARTESIAN_POINT('Origin',(39.7707905934405,-28.502719155674,39.116));
#199248=CARTESIAN_POINT('Origin',(49.0553654007526,-35.2482948100397,39.1160402713847));
#199249=CARTESIAN_POINT('Ctrl Pts',(49.2466351556012,-35.386610142826,39.2708017080178));
#199250=CARTESIAN_POINT('Ctrl Pts',(49.1720533660031,-35.4901170100368,
39.27051194648));
#199251=CARTESIAN_POINT('Ctrl Pts',(49.0826686475734,-35.4251752107438,
39.3343017080178));
#199252=CARTESIAN_POINT('Ctrl Pts',(49.282975877639,-35.4131599099231,39.3487519301185));
#199253=CARTESIAN_POINT('Ctrl Pts',(49.2082707697374,-35.5164304941056,
39.3482879463985));
#199254=CARTESIAN_POINT('Ctrl Pts',(49.1372837917337,-35.4648554356494,
39.4512271261637));
#199255=CARTESIAN_POINT('Ctrl Pts',(49.3518235761932,-35.4634578610138,
39.3978017080178));
#199256=CARTESIAN_POINT('Ctrl Pts',(49.2769673468822,-35.5663414789297,
39.3975673827401));
#199257=CARTESIAN_POINT('Ctrl Pts',(49.2407512920135,-35.5400289748691,
39.524801535518));
#199258=CARTESIAN_POINT('Ctrl Pts',(49.424260778346,-35.5163757878396,39.3978017080178));
#199259=CARTESIAN_POINT('Ctrl Pts',(49.3496120513049,-35.6191209461252,
39.3978017080178));
#199260=CARTESIAN_POINT('Ctrl Pts',(49.3496120513049,-35.6191209461252,
39.5248017080178));
#199261=CARTESIAN_POINT('Origin',(49.1573173746146,-35.3224300524582,39.3343017080178));
#199262=CARTESIAN_POINT('Origin',(49.0915036263516,-35.2746135650469,39.1934008533543));
#199263=CARTESIAN_POINT('Origin',(45.4345348113611,-41.3366772861974,39.1925554495085));
#199264=CARTESIAN_POINT('Origin',(45.4673664422103,-41.3663085755639,39.116037328527));
#199265=CARTESIAN_POINT('Origin',(45.3737170758072,-41.2819167515329,39.3343017080178));
#199266=CARTESIAN_POINT('Ctrl Pts',(45.2923641298557,-41.2079002115908,
39.2708017080178));
#199267=CARTESIAN_POINT('Ctrl Pts',(45.3773275334105,-41.1142722655007,
39.2710850691866));
#199268=CARTESIAN_POINT('Ctrl Pts',(45.4586966628148,-41.1875373586973,
39.3343017080178));
#199269=CARTESIAN_POINT('Ctrl Pts',(45.2588408013013,-41.1778715515042,
39.3487519293518));
#199270=CARTESIAN_POINT('Ctrl Pts',(45.3437094247724,-41.084002384522,39.3492068662926));
#199271=CARTESIAN_POINT('Ctrl Pts',(45.4085284377449,-41.1423656859491,
39.451227124874));
#199272=CARTESIAN_POINT('Ctrl Pts',(45.1953306044459,-41.1209827764365,
39.3978017080178));
#199273=CARTESIAN_POINT('Ctrl Pts',(45.280091264722,-41.0267203359205,39.3980347781178));
#199274=CARTESIAN_POINT('Ctrl Pts',(45.313485541162,-41.0567886774841,39.524801535519));
#199275=CARTESIAN_POINT('Ctrl Pts',(45.1285089182132,-41.0611303347405,
39.3978017080178));
#199276=CARTESIAN_POINT('Ctrl Pts',(45.2134885052208,-40.9667509419048,
39.3978017080178));
#199277=CARTESIAN_POINT('Ctrl Pts',(45.2134885052208,-40.9667509419048,
39.5248017080178));
#199278=CARTESIAN_POINT('Origin',(45.1285089182132,-41.0611303347405,39.5248017080178));
#199279=CARTESIAN_POINT('Origin',(-0.212448967518932,-0.235948482089072,
39.116));
#199280=CARTESIAN_POINT('Origin',(45.7656648676106,-41.6348281284263,39.116));
#199281=CARTESIAN_POINT('Origin',(-0.212448967518932,-0.235948482089072,
39.5248017080178));
#199282=CARTESIAN_POINT('Origin',(45.0161393894793,-40.9599523566126,39.5248017080178));
#199283=CARTESIAN_POINT('Ctrl Pts',(46.1654920697611,-41.9955727382251,
39.2875012672119));
#199284=CARTESIAN_POINT('Ctrl Pts',(46.2513146333407,-41.900956815078,39.287208709576));
#199285=CARTESIAN_POINT('Ctrl Pts',(46.1706818621617,-41.8286119029176,
39.3549016990124));
#199286=CARTESIAN_POINT('Ctrl Pts',(46.0801220723611,-41.9185486398936,
39.103493917393));
#199287=CARTESIAN_POINT('Ctrl Pts',(46.1657485549058,-41.823913122125,39.1031692336314));
#199288=CARTESIAN_POINT('Ctrl Pts',(46.1023486848322,-41.767084433516,39.207750720229));
#199289=CARTESIAN_POINT('Ctrl Pts',(45.9267584721677,-41.780177115277,38.989));
#199290=CARTESIAN_POINT('Ctrl Pts',(46.0121526898533,-41.6856154234966,
38.9887769311188));
#199291=CARTESIAN_POINT('Ctrl Pts',(45.979590910035,-41.6565528363053,39.1161898712919));
#199292=CARTESIAN_POINT('Ctrl Pts',(45.7656648676106,-41.6348281284263,
38.989));
#199293=CARTESIAN_POINT('Ctrl Pts',(45.8507714101807,-41.540307737154,38.989));
#199294=CARTESIAN_POINT('Ctrl Pts',(45.8506443599268,-41.5404488407559,
39.1161895903858));
#199295=CARTESIAN_POINT('Origin',(46.0858221116777,-41.9230990057956,39.3548010137695));
#199296=CARTESIAN_POINT('Ctrl Pts',(45.0161393894793,-40.9599523566126,
39.3978017080178));
#199297=CARTESIAN_POINT('Ctrl Pts',(45.1011189764868,-40.8655729637769,
39.3978017080178));
#199298=CARTESIAN_POINT('Ctrl Pts',(45.1011189764868,-40.8655729637769,
39.5248017080178));
#199299=CARTESIAN_POINT('Ctrl Pts',(44.9490914662989,-40.8998980546777,
39.3978017080178));
#199300=CARTESIAN_POINT('Ctrl Pts',(45.0341638030263,-40.8052862548056,
39.3975666025017));
#199301=CARTESIAN_POINT('Ctrl Pts',(45.0007839642924,-40.7752309130124,
39.5248015517177));
#199302=CARTESIAN_POINT('Ctrl Pts',(44.8856913339435,-40.8431135311203,
39.3484894016716));
#199303=CARTESIAN_POINT('Ctrl Pts',(44.9711739721975,-40.7485699563814,
39.3480259000057));
#199304=CARTESIAN_POINT('Ctrl Pts',(44.9059100567339,-40.6898060629484,
39.4508333188949));
#199305=CARTESIAN_POINT('Ctrl Pts',(44.8522789915941,-40.8131880745607,
39.2708017080178));
#199306=CARTESIAN_POINT('Ctrl Pts',(44.9380175594362,-40.7187157882338,
39.27051194648));
#199307=CARTESIAN_POINT('Ctrl Pts',(44.8559107663285,-40.6447864996553,
39.3343017080178));
#199308=CARTESIAN_POINT('Origin',(44.7709311793209,-40.739165892491,39.3343017080178));
#199309=CARTESIAN_POINT('Origin',(46.2182127020628,-42.0423040287724,39.6398955068193));
#199310=CARTESIAN_POINT('Origin',(46.3506032922594,-42.1615090516453,39.92499));
#199311=CARTESIAN_POINT('Origin',(44.7104761485842,-40.6847319383096,39.1934008539945));
#199312=CARTESIAN_POINT('Origin',(44.6772189625507,-40.6548553974685,39.1160402713855));
#199313=CARTESIAN_POINT('Ctrl Pts',(46.7738319284257,-42.1358900227696,
40.1599502534424));
#199314=CARTESIAN_POINT('Ctrl Pts',(46.7461150696872,-42.1109214781062,
40.10025));
#199315=CARTESIAN_POINT('Ctrl Pts',(46.6938111422604,-42.0638038389701,
40.10025));
#199316=CARTESIAN_POINT('Ctrl Pts',(46.7148552537636,-42.2013581359407,
40.1599500538455));
#199317=CARTESIAN_POINT('Ctrl Pts',(46.703153296022,-42.1586072771686,40.100244835349));
#199318=CARTESIAN_POINT('Ctrl Pts',(46.6596664560525,-42.1016932886499,
40.10025));
#199319=CARTESIAN_POINT('Ctrl Pts',(46.6418481388116,-42.2450249725426,
40.120244200104));
#199320=CARTESIAN_POINT('Ctrl Pts',(46.646403998566,-42.1870455286631,40.0633873868017));
#199321=CARTESIAN_POINT('Ctrl Pts',(46.6095714048493,-42.1199142759248,
40.0772271723538));
#199322=CARTESIAN_POINT('Ctrl Pts',(46.5164783566526,-42.2756632139847,
40.0045995998161));
#199323=CARTESIAN_POINT('Ctrl Pts',(46.5588531737051,-42.1934768724827,
39.9663485808314));
#199324=CARTESIAN_POINT('Ctrl Pts',(46.5142596423498,-42.1171707421502,
40.0101727202466));
#199325=CARTESIAN_POINT('Ctrl Pts',(46.4640705998044,-42.2644092166192,
39.930465434986));
#199326=CARTESIAN_POINT('Ctrl Pts',(46.5278411618568,-42.1708301402936,
39.9051900162956));
#199327=CARTESIAN_POINT('Ctrl Pts',(46.4693765058,-42.0975575768115,39.9671857458174));
#199328=CARTESIAN_POINT('Ctrl Pts',(46.4302753505424,-42.2339804752702,
39.8576902534424));
#199329=CARTESIAN_POINT('Ctrl Pts',(46.5159655405274,-42.1395065321,39.8573998014387));
#199330=CARTESIAN_POINT('Ctrl Pts',(46.435582879267,-42.0671296588096,39.92499));
#199331=CARTESIAN_POINT('Origin',(46.6938111422604,-42.0638038389701,40.22725));
#199332=CARTESIAN_POINT('Origin',(-0.212448967518932,-0.235948482089072,
39.116));
#199333=CARTESIAN_POINT('Origin',(44.3789831537295,-40.3862543050939,39.116));
#199334=CARTESIAN_POINT('Origin',(5.54214007001405E-15,5.80521725755185E-15,
40.22725));
#199335=CARTESIAN_POINT('Origin',(46.7142062431422,-42.0411527846896,40.22725));
#199336=CARTESIAN_POINT('Ctrl Pts',(44.3789831537295,-40.3862543050939,
38.989));
#199337=CARTESIAN_POINT('Ctrl Pts',(44.4640900439955,-40.2917335276662,
38.989));
#199338=CARTESIAN_POINT('Ctrl Pts',(44.4639626455268,-40.291875018,39.1161901092318));
#199339=CARTESIAN_POINT('Ctrl Pts',(44.2178916378581,-40.2408978759481,
38.989));
#199340=CARTESIAN_POINT('Ctrl Pts',(44.3029863283941,-40.1466757825273,
38.989229898976));
#199341=CARTESIAN_POINT('Ctrl Pts',(44.335013814932,-40.1757689690791,39.1161900493198));
#199342=CARTESIAN_POINT('Ctrl Pts',(44.0645366033547,-40.102519072098,39.1034966344368));
#199343=CARTESIAN_POINT('Ctrl Pts',(44.1495800756973,-40.0085488431172,
39.1038314102568));
#199344=CARTESIAN_POINT('Ctrl Pts',(44.2122569536161,-40.0652381943521,
39.2077528789601));
#199345=CARTESIAN_POINT('Ctrl Pts',(43.9791725362582,-40.0254908126589,
39.2875012672119));
#199346=CARTESIAN_POINT('Ctrl Pts',(44.0642551375171,-39.9317222927448,
39.2878045257868));
#199347=CARTESIAN_POINT('Ctrl Pts',(44.1439246138545,-40.0037114790884,
39.3549015295897));
#199348=CARTESIAN_POINT('Origin',(44.0588255818377,-40.09798313255,39.3548010137695));
#199349=CARTESIAN_POINT('Ctrl Pts',(46.8559036426985,-41.7612723673363,
39.8576902534424));
#199350=CARTESIAN_POINT('Ctrl Pts',(46.7709043015502,-41.8563683535931,
39.8573998014387));
#199351=CARTESIAN_POINT('Ctrl Pts',(46.6905216402897,-41.7839914803027,
39.92499));
#199352=CARTESIAN_POINT('Ctrl Pts',(46.8897135983611,-41.7917156448187,
39.9304984902491));
#199353=CARTESIAN_POINT('Ctrl Pts',(46.8033160448235,-41.8649095672142,
39.9052171569788));
#199354=CARTESIAN_POINT('Ctrl Pts',(46.7243306652218,-41.8144332630854,
39.9672049726596));
#199355=CARTESIAN_POINT('Ctrl Pts',(46.9062450310968,-41.8425440045878,
40.0043437678661));
#199356=CARTESIAN_POINT('Ctrl Pts',(46.8289264627109,-41.8933569085955,
39.9661628577642));
#199357=CARTESIAN_POINT('Ctrl Pts',(46.748390797668,-41.8569022891471,40.0100243556237));
#199358=CARTESIAN_POINT('Ctrl Pts',(46.8892773184517,-41.9695156381235,
40.1194874821988));
#199359=CARTESIAN_POINT('Ctrl Pts',(46.8319191778365,-41.9804178820374,
40.062755148314));
#199360=CARTESIAN_POINT('Ctrl Pts',(46.7612136652292,-41.9507871007487,
40.0767884282376));
#199361=CARTESIAN_POINT('Ctrl Pts',(46.8534019544983,-42.047486468405,40.1599502015393));
#199362=CARTESIAN_POINT('Ctrl Pts',(46.8096319157679,-42.0403508033703,
40.1002449453869));
#199363=CARTESIAN_POINT('Ctrl Pts',(46.7484320121873,-42.0031091843017,
40.10025));
#199364=CARTESIAN_POINT('Ctrl Pts',(46.7942619810916,-42.1132001506002,
40.1599502534424));
#199365=CARTESIAN_POINT('Ctrl Pts',(46.7665330160779,-42.0882450513176,
40.10025));
#199366=CARTESIAN_POINT('Ctrl Pts',(46.7142062431422,-42.0411527846896,
40.10025));
#199367=CARTESIAN_POINT('Origin',(46.7755012272973,-41.6896120874671,39.92499));
#199368=CARTESIAN_POINT('Origin',(43.9264348095014,-39.9787779456746,39.639895506933));
#199369=CARTESIAN_POINT('Origin',(43.7940440370144,-39.8595727587356,39.92499));
#199370=CARTESIAN_POINT('Origin',(46.6431106370589,-41.5704070646205,39.6398955068277));
#199371=CARTESIAN_POINT('Origin',(46.5107200467156,-41.4512020416175,39.3548010137695));
#199372=CARTESIAN_POINT('Ctrl Pts',(43.7143933160623,-39.7870778846748,
39.8576902534424));
#199373=CARTESIAN_POINT('Ctrl Pts',(43.7993487829612,-39.6934538167801,
39.8579948730703));
#199374=CARTESIAN_POINT('Ctrl Pts',(43.8790236240219,-39.7651933658999,
39.92499));
#199375=CARTESIAN_POINT('Ctrl Pts',(43.6806281164521,-39.7566748466922,
39.9304020711231));
#199376=CARTESIAN_POINT('Ctrl Pts',(43.7668791656721,-39.684664896048,39.9058915297382));
#199377=CARTESIAN_POINT('Ctrl Pts',(43.8452566693654,-39.7347894633636,
39.9671523786035));
#199378=CARTESIAN_POINT('Ctrl Pts',(43.6642103943287,-39.7061132086029,
40.0043257306693));
#199379=CARTESIAN_POINT('Ctrl Pts',(43.7414086642734,-39.656059551044,39.9667894847838));
#199380=CARTESIAN_POINT('Ctrl Pts',(43.8213838166748,-39.6925108309093,
40.01001389752));
#199381=CARTESIAN_POINT('Ctrl Pts',(43.6815693876452,-39.5798624575878,
40.1195533054857));
#199382=CARTESIAN_POINT('Ctrl Pts',(43.7388169234803,-39.5692094437564,
40.0630813209233));
#199383=CARTESIAN_POINT('Ctrl Pts',(43.8091742082547,-39.5991004926177,
40.076826594242));
#199384=CARTESIAN_POINT('Ctrl Pts',(43.7176736830029,-39.5024012818818,
40.1599502027513));
#199385=CARTESIAN_POINT('Ctrl Pts',(43.76134731634,-39.5096522555309,40.1002552791529));
#199386=CARTESIAN_POINT('Ctrl Pts',(43.822360370862,-39.5470931435016,40.10025));
#199387=CARTESIAN_POINT('Ctrl Pts',(43.7765468711722,-39.4370498736009,
40.1599502534424));
#199388=CARTESIAN_POINT('Ctrl Pts',(43.8042633382929,-39.462018852981,40.10025));
#199389=CARTESIAN_POINT('Ctrl Pts',(43.8565665267056,-39.5091373124623,
40.10025));
#199390=CARTESIAN_POINT('Origin',(43.8565665267056,-39.5091373124623,40.22725));
#199391=CARTESIAN_POINT('Ctrl Pts',(46.1905628026484,-41.1629311642481,
38.989));
#199392=CARTESIAN_POINT('Ctrl Pts',(46.1054562527464,-41.2574515636633,
38.989));
#199393=CARTESIAN_POINT('Ctrl Pts',(46.1055833103431,-41.2573104519063,
39.1161896013268));
#199394=CARTESIAN_POINT('Ctrl Pts',(46.3519569306012,-41.307951431325,38.989));
#199395=CARTESIAN_POINT('Ctrl Pts',(46.2668393800559,-41.4027622547783,
38.988776927546));
#199396=CARTESIAN_POINT('Ctrl Pts',(46.2345318643234,-41.3734162510828,
39.1161898821849));
#199397=CARTESIAN_POINT('Ctrl Pts',(46.5056000892405,-41.446010036275,39.1034967087243));
#199398=CARTESIAN_POINT('Ctrl Pts',(46.4204333915643,-41.541059563397,39.103172023271));
#199399=CARTESIAN_POINT('Ctrl Pts',(46.3572886670237,-41.4839469723849,
39.2077529614999));
#199400=CARTESIAN_POINT('Ctrl Pts',(46.5911245387429,-41.5228599914563,
39.2875012672119));
#199401=CARTESIAN_POINT('Ctrl Pts',(46.5059978248576,-41.618102475323,39.2872087095507));
#199402=CARTESIAN_POINT('Ctrl Pts',(46.4256208064858,-41.5454735069376,
39.3549017048228));
#199403=CARTESIAN_POINT('Origin',(46.1905628026484,-41.1629311642481,39.116));
#199404=CARTESIAN_POINT('Origin',(5.70826774717982E-15,5.21345853525163E-15,
40.22725));
#199405=CARTESIAN_POINT('Origin',(43.8769616275874,-39.4864862581817,40.22725));
#199406=CARTESIAN_POINT('Origin',(34.5756856720385,-30.7048488218244,39.116));
#199407=CARTESIAN_POINT('Origin',(45.8923335519876,-40.8943347850527,39.1160373285247));
#199408=CARTESIAN_POINT('Ctrl Pts',(43.7969047596346,-39.414440147899,40.1599502534424));
#199409=CARTESIAN_POINT('Ctrl Pts',(43.8246341160485,-39.4393948122689,
40.10025));
#199410=CARTESIAN_POINT('Ctrl Pts',(43.8769616275874,-39.4864862581817,
40.10025));
#199411=CARTESIAN_POINT('Ctrl Pts',(43.8555436924521,-39.3492813761645,
40.1599500566037));
#199412=CARTESIAN_POINT('Ctrl Pts',(43.8673524484227,-39.3919218645331,
40.100255130536));
#199413=CARTESIAN_POINT('Ctrl Pts',(43.9110175468023,-39.4486296259968,
40.10025));
#199414=CARTESIAN_POINT('Ctrl Pts',(43.9280312169046,-39.3054399757363,
40.1203070619049));
#199415=CARTESIAN_POINT('Ctrl Pts',(43.9237065964669,-39.3632835603675,
40.0637098684502));
#199416=CARTESIAN_POINT('Ctrl Pts',(43.9607655567556,-39.4300423632768,
40.0772636213365));
#199417=CARTESIAN_POINT('Ctrl Pts',(44.0526112349805,-39.2744854109878,
40.0046102245799));
#199418=CARTESIAN_POINT('Ctrl Pts',(44.0109847679681,-39.3564679665376,
39.9670001894009));
#199419=CARTESIAN_POINT('Ctrl Pts',(44.0555161714745,-39.4322155454628,
40.0101788811207));
#199420=CARTESIAN_POINT('Ctrl Pts',(44.1047669487881,-39.2856498807571,
39.9303710930188));
#199421=CARTESIAN_POINT('Ctrl Pts',(44.0421591564547,-39.3789590643325,
39.9058663574113));
#199422=CARTESIAN_POINT('Ctrl Pts',(44.1002097724418,-39.4516641984998,
39.9671344706366));
#199423=CARTESIAN_POINT('Ctrl Pts',(44.1385184650375,-39.316039186369,39.8576902534424));
#199424=CARTESIAN_POINT('Ctrl Pts',(44.054287543984,-39.4103156382732,39.8579948730703));
#199425=CARTESIAN_POINT('Ctrl Pts',(44.1339623850447,-39.4820551873931,
39.92499));
#199426=CARTESIAN_POINT('Origin',(44.2189419720523,-39.3876757945574,39.92499));
#199427=CARTESIAN_POINT('Origin',(45.8594327453956,-40.8647803215175,39.1925554488842));
#199428=CARTESIAN_POINT('Origin',(45.7986150108451,-40.8100197873548,39.3343017080178));
#199429=CARTESIAN_POINT('Origin',(44.3513327444874,-39.5068809815262,39.6398955069214));
#199430=CARTESIAN_POINT('Origin',(44.4837235168756,-39.6260861683718,39.3548010137695));
#199431=CARTESIAN_POINT('Ctrl Pts',(45.5534068532511,-40.5892333705623,
39.3978017080178));
#199432=CARTESIAN_POINT('Ctrl Pts',(45.4684272662435,-40.6836127633979,
39.3978017080178));
#199433=CARTESIAN_POINT('Ctrl Pts',(45.4684272662435,-40.683612763398,39.5248017080178));
#199434=CARTESIAN_POINT('Ctrl Pts',(45.6201409680063,-40.6496361736986,
39.3978017080178));
#199435=CARTESIAN_POINT('Ctrl Pts',(45.5352552698599,-40.7437849681286,
39.3980355775196));
#199436=CARTESIAN_POINT('Ctrl Pts',(45.5687622694472,-40.7739548060672,
39.5248015517192));
#199437=CARTESIAN_POINT('Ctrl Pts',(45.6832443225597,-40.7067502157879,
39.3484893995498));
#199438=CARTESIAN_POINT('Ctrl Pts',(45.5987613682844,-40.8009661159867,
39.3489438303423));
#199439=CARTESIAN_POINT('Ctrl Pts',(45.6636361529341,-40.8593796344571,
39.4508333155601));
#199440=CARTESIAN_POINT('Ctrl Pts',(45.7165002428306,-40.7368493365298,
39.2708017080178));
#199441=CARTESIAN_POINT('Ctrl Pts',(45.6322662944332,-40.8311340869938,
39.2710850691866));
#199442=CARTESIAN_POINT('Ctrl Pts',(45.7136354238375,-40.9043991801904,
39.3343017080178));
#199443=CARTESIAN_POINT('Origin',(45.5534068532511,-40.5892333705623,39.5248017080178));
#199444=CARTESIAN_POINT('Ctrl Pts',(44.4033023070489,-39.5544469813071,
39.2875012672119));
#199445=CARTESIAN_POINT('Ctrl Pts',(44.3189410241795,-39.6488649595835,
39.2878045257519));
#199446=CARTESIAN_POINT('Ctrl Pts',(44.3988635552003,-39.7205730817651,
39.3549015218346));
#199447=CARTESIAN_POINT('Ctrl Pts',(44.4888328647691,-39.6312929306947,
39.1034938540228));
#199448=CARTESIAN_POINT('Ctrl Pts',(44.4042668857107,-39.7256930794144,
39.1038286278794));
#199449=CARTESIAN_POINT('Ctrl Pts',(44.4671969296255,-39.7821007282721,
39.2077506434035));
#199450=CARTESIAN_POINT('Ctrl Pts',(44.6424847942248,-39.7693444365338,
38.989));
#199451=CARTESIAN_POINT('Ctrl Pts',(44.5576736780985,-39.8638218465935,
38.9892298954635));
#199452=CARTESIAN_POINT('Ctrl Pts',(44.5899547640672,-39.8926323785399,
39.1161900347286));
#199453=CARTESIAN_POINT('Ctrl Pts',(44.8038810887674,-39.9143573409157,
38.989));
#199454=CARTESIAN_POINT('Ctrl Pts',(44.7187742083306,-40.008878107427,38.989));
#199455=CARTESIAN_POINT('Ctrl Pts',(44.7189015969554,-40.008736628026,39.1161900945643));
#199456=CARTESIAN_POINT('Origin',(44.8038810887674,-39.9143573409157,39.116));
#199457=CARTESIAN_POINT('Origin',(33.7433098572246,-29.9553742717902,39.5248017080178));
#199458=CARTESIAN_POINT('Origin',(45.4410373245171,-40.4880553924344,39.5248017080178));
#199459=CARTESIAN_POINT('Origin',(33.6129634723596,-29.8380098596982,39.116));
#199460=CARTESIAN_POINT('Origin',(45.1021848870409,-40.1828829233545,39.1160402713845));
#199461=CARTESIAN_POINT('Ctrl Pts',(45.2779489569772,-40.3404336838193,
39.2708017080178));
#199462=CARTESIAN_POINT('Ctrl Pts',(45.1929563204589,-40.4355776097269,
39.27051194648));
#199463=CARTESIAN_POINT('Ctrl Pts',(45.1108495273512,-40.3616483211485,
39.3343017080178));
#199464=CARTESIAN_POINT('Ctrl Pts',(45.3113153943832,-40.370636648342,39.3487519301186));
#199465=CARTESIAN_POINT('Ctrl Pts',(45.2262248134205,-40.465532695337,39.3482879463991));
#199466=CARTESIAN_POINT('Ctrl Pts',(45.1610177711089,-40.4068200107232,
39.4512271261626));
#199467=CARTESIAN_POINT('Ctrl Pts',(45.3745283705085,-40.4278556061229,
39.3978017080178));
#199468=CARTESIAN_POINT('Ctrl Pts',(45.2893279449735,-40.5223510101945,
39.3975673827364));
#199469=CARTESIAN_POINT('Ctrl Pts',(45.2560606910578,-40.492397040227,39.524801535518));
#199470=CARTESIAN_POINT('Ctrl Pts',(45.4410373245171,-40.4880553924344,
39.3978017080178));
#199471=CARTESIAN_POINT('Ctrl Pts',(45.3560577375095,-40.58243478527,39.3978017080178));
#199472=CARTESIAN_POINT('Ctrl Pts',(45.3560577375095,-40.58243478527,39.5248017080178));
#199473=CARTESIAN_POINT('Origin',(45.1958291143588,-40.2672689283128,39.3343017080178));
#199474=CARTESIAN_POINT('Origin',(45.1353740846438,-40.2128349746504,39.1934008533557));
#199475=CARTESIAN_POINT('Origin',(40.8647803224533,-45.8594327460076,39.1925554495083));
#199476=CARTESIAN_POINT('Origin',(40.8943347850522,-45.8923335519897,39.1160373285272));
#199477=CARTESIAN_POINT('Origin',(40.8100197873546,-45.7986150108452,39.3343017080178));
#199478=CARTESIAN_POINT('Ctrl Pts',(40.7368493365296,-45.7165002428308,
39.2708017080178));
#199479=CARTESIAN_POINT('Ctrl Pts',(40.8311340869937,-45.6322662944333,
39.2710850691866));
#199480=CARTESIAN_POINT('Ctrl Pts',(40.9043991801903,-45.7136354238377,
39.3343017080178));
#199481=CARTESIAN_POINT('Ctrl Pts',(40.7066485019706,-45.6831319408677,
39.3487519293518));
#199482=CARTESIAN_POINT('Ctrl Pts',(40.8008642060144,-45.5986481857943,
39.3492068662913));
#199483=CARTESIAN_POINT('Ctrl Pts',(40.8592275074406,-45.6634671987661,
39.4512271248735));
#199484=CARTESIAN_POINT('Ctrl Pts',(40.6494327168505,-45.6199161851861,
39.3978017080178));
#199485=CARTESIAN_POINT('Ctrl Pts',(40.7435821574126,-45.5350300257468,
39.3980347781192));
#199486=CARTESIAN_POINT('Ctrl Pts',(40.7736504989782,-45.5684243021861,
39.524801535519));
#199487=CARTESIAN_POINT('Ctrl Pts',(40.5892333705622,-45.5534068532512,
39.3978017080178));
#199488=CARTESIAN_POINT('Ctrl Pts',(40.6836127633978,-45.4684272662437,
39.3978017080178));
#199489=CARTESIAN_POINT('Ctrl Pts',(40.6836127633978,-45.4684272662437,
39.5248017080178));
#199490=CARTESIAN_POINT('Origin',(40.5892333705622,-45.5534068532512,39.5248017080178));
#199491=CARTESIAN_POINT('Origin',(-0.235948482089068,-0.212448967518937,
39.116));
#199492=CARTESIAN_POINT('Origin',(41.162931164248,-46.1905628026486,39.116));
#199493=CARTESIAN_POINT('Origin',(-0.235948482089068,-0.212448967518937,
39.5248017080178));
#199494=CARTESIAN_POINT('Origin',(40.4880553924343,-45.4410373245173,39.5248017080178));
#199495=CARTESIAN_POINT('Ctrl Pts',(41.5228599914562,-46.5911245387431,
39.2875012672119));
#199496=CARTESIAN_POINT('Ctrl Pts',(41.6181024670999,-46.5059978322074,
39.287208709576));
#199497=CARTESIAN_POINT('Ctrl Pts',(41.5454735131716,-46.4256208133851,
39.3549016990124));
#199498=CARTESIAN_POINT('Ctrl Pts',(41.4460088704669,-46.5055987918445,
39.1034939173931));
#199499=CARTESIAN_POINT('Ctrl Pts',(41.5410583874238,-46.4204321019783,
39.103169233633));
#199500=CARTESIAN_POINT('Ctrl Pts',(41.4839460439617,-46.3572876358811,
39.2077507202293));
#199501=CARTESIAN_POINT('Ctrl Pts',(41.3079491749537,-46.3519544194652,
38.989));
#199502=CARTESIAN_POINT('Ctrl Pts',(41.4027599825089,-46.2668368728713,
38.988776931117));
#199503=CARTESIAN_POINT('Ctrl Pts',(41.3734144470997,-46.234529860773,39.1161898712918));
#199504=CARTESIAN_POINT('Ctrl Pts',(41.162931164248,-46.1905628026486,38.989));
#199505=CARTESIAN_POINT('Ctrl Pts',(41.2574515555201,-46.1054562600785,
38.989));
#199506=CARTESIAN_POINT('Ctrl Pts',(41.2573104519183,-46.1055833103323,
39.1161895903857));
#199507=CARTESIAN_POINT('Origin',(41.4512020416173,-46.5107200467158,39.3548010137695));
#199508=CARTESIAN_POINT('Ctrl Pts',(40.4880553924343,-45.4410373245172,
39.3978017080178));
#199509=CARTESIAN_POINT('Ctrl Pts',(40.5824347852699,-45.3560577375097,
39.3978017080178));
#199510=CARTESIAN_POINT('Ctrl Pts',(40.5824347852699,-45.3560577375097,
39.5248017080178));
#199511=CARTESIAN_POINT('Ctrl Pts',(40.4276521486881,-45.3743035899551,
39.3978017080178));
#199512=CARTESIAN_POINT('Ctrl Pts',(40.5221480763004,-45.2891025640488,
39.3975666025036));
#199513=CARTESIAN_POINT('Ctrl Pts',(40.4920927345059,-45.2557227253158,
39.5248015517196));
#199514=CARTESIAN_POINT('Ctrl Pts',(40.370534927875,-45.3112030195541,39.3484894016716));
#199515=CARTESIAN_POINT('Ctrl Pts',(40.4654317778746,-45.2261127332183,
39.3480259000047));
#199516=CARTESIAN_POINT('Ctrl Pts',(40.4066678844406,-45.1608488177559,
39.4508333188937));
#199517=CARTESIAN_POINT('Ctrl Pts',(40.3404336838192,-45.2779489569773,
39.2708017080178));
#199518=CARTESIAN_POINT('Ctrl Pts',(40.4355776097268,-45.192956320459,39.27051194648));
#199519=CARTESIAN_POINT('Ctrl Pts',(40.3616483211483,-45.1108495273513,
39.3343017080178));
#199520=CARTESIAN_POINT('Origin',(40.2672689283127,-45.1958291143589,39.3343017080178));
#199521=CARTESIAN_POINT('Origin',(41.5704070646291,-46.64311063707,39.639895506819));
#199522=CARTESIAN_POINT('Origin',(41.689612087467,-46.7755012272974,39.92499));
#199523=CARTESIAN_POINT('Origin',(40.2128349741407,-45.1353740836146,39.1934008539941));
#199524=CARTESIAN_POINT('Origin',(40.182882923354,-45.1021848870412,39.1160402713849));
#199525=CARTESIAN_POINT('Ctrl Pts',(42.1132001506,-46.7942619810918,40.1599502534424));
#199526=CARTESIAN_POINT('Ctrl Pts',(42.0882450513174,-46.766533016078,40.10025));
#199527=CARTESIAN_POINT('Ctrl Pts',(42.0411527846894,-46.7142062431423,
40.10025));
#199528=CARTESIAN_POINT('Ctrl Pts',(42.0477032750703,-46.8532067119187,
40.1599500538472));
#199529=CARTESIAN_POINT('Ctrl Pts',(42.0405341034511,-46.8094668591672,
40.1002448353499));
#199530=CARTESIAN_POINT('Ctrl Pts',(42.0032346206983,-46.7483190388769,
40.10025));
#199531=CARTESIAN_POINT('Ctrl Pts',(41.9705316734067,-46.8890030154862,
40.120244200104));
#199532=CARTESIAN_POINT('Ctrl Pts',(41.9811230778542,-46.8318174060854,
40.0633873868017));
#199533=CARTESIAN_POINT('Ctrl Pts',(41.9515093836259,-46.7612038509546,
40.0772271723539));
#199534=CARTESIAN_POINT('Ctrl Pts',(41.8426461117365,-46.906368706767,40.0045995998161));
#199535=CARTESIAN_POINT('Ctrl Pts',(41.8933796070866,-46.8290619651512,
39.9663485808314));
#199536=CARTESIAN_POINT('Ctrl Pts',(41.8570065263034,-46.7485125544801,
40.0101727202464));
#199537=CARTESIAN_POINT('Ctrl Pts',(41.7917018131133,-46.8896982576907,
39.930465434986));
#199538=CARTESIAN_POINT('Ctrl Pts',(41.8649047103979,-46.8032976561885,
39.9051900162954));
#199539=CARTESIAN_POINT('Ctrl Pts',(41.8144193983038,-46.7243152668222,
39.9671857458183));
#199540=CARTESIAN_POINT('Ctrl Pts',(41.7612723673362,-46.8559036426986,
39.8576902534424));
#199541=CARTESIAN_POINT('Ctrl Pts',(41.8563683535929,-46.7709043015503,
39.8573998014387));
#199542=CARTESIAN_POINT('Ctrl Pts',(41.7839914803026,-46.6905216402898,
39.92499));
#199543=CARTESIAN_POINT('Origin',(42.0411527846894,-46.7142062431423,40.22725));
#199544=CARTESIAN_POINT('Origin',(-0.235948482089068,-0.212448967518937,
39.116));
#199545=CARTESIAN_POINT('Origin',(39.9143573409156,-44.8038810887675,39.116));
#199546=CARTESIAN_POINT('Origin',(5.55434424446679E-15,5.81742143200459E-15,
40.22725));
#199547=CARTESIAN_POINT('Origin',(42.06380383897,-46.6938111422605,40.22725));
#199548=CARTESIAN_POINT('Ctrl Pts',(39.9143573409156,-44.8038810887675,
38.989));
#199549=CARTESIAN_POINT('Ctrl Pts',(40.0088781183437,-44.7187741985011,
38.989));
#199550=CARTESIAN_POINT('Ctrl Pts',(40.0087366280095,-44.7189015969702,
39.1161901092324));
#199551=CARTESIAN_POINT('Ctrl Pts',(39.7693421853883,-44.6424822887497,
38.989));
#199552=CARTESIAN_POINT('Ctrl Pts',(39.8638196089385,-44.5576711710515,
38.9892298989766));
#199553=CARTESIAN_POINT('Ctrl Pts',(39.8926305794723,-44.5899527660332,
39.1161900493204));
#199554=CARTESIAN_POINT('Ctrl Pts',(39.6312917695235,-44.4888315723763,
39.1034966344367));
#199555=CARTESIAN_POINT('Ctrl Pts',(39.7256919284523,-44.4042655856149,
39.1038314102555));
#199556=CARTESIAN_POINT('Ctrl Pts',(39.7820998051095,-44.4671959043825,
39.2077528789597));
#199557=CARTESIAN_POINT('Ctrl Pts',(39.554446981307,-44.403302307049,39.2875012672119));
#199558=CARTESIAN_POINT('Ctrl Pts',(39.6488649704638,-44.3189410144581,
39.2878045257868));
#199559=CARTESIAN_POINT('Ctrl Pts',(39.7205730900534,-44.3988635644383,
39.35490152959));
#199560=CARTESIAN_POINT('Origin',(39.6260861683717,-44.4837235168757,39.3548010137695));
#199561=CARTESIAN_POINT('Ctrl Pts',(42.2339804752701,-46.4302753505426,
39.8576902534424));
#199562=CARTESIAN_POINT('Ctrl Pts',(42.1395065320998,-46.5159655405276,
39.8573998014387));
#199563=CARTESIAN_POINT('Ctrl Pts',(42.0671296588095,-46.4355828792671,
39.92499));
#199564=CARTESIAN_POINT('Ctrl Pts',(42.2644230274452,-46.4640859592745,
39.9304984902489));
#199565=CARTESIAN_POINT('Ctrl Pts',(42.1708479205168,-46.5278479142009,
39.9052171569801));
#199566=CARTESIAN_POINT('Ctrl Pts',(42.0975714415913,-46.4693919041982,
39.9672049726605));
#199567=CARTESIAN_POINT('Ctrl Pts',(42.2755508889261,-46.51636388123,40.0043437678664));
#199568=CARTESIAN_POINT('Ctrl Pts',(42.1933444849779,-46.5588164356977,
39.9661628577643));
#199569=CARTESIAN_POINT('Ctrl Pts',(42.1170605480851,-46.5141432491637,
40.0100243556237));
#199570=CARTESIAN_POINT('Ctrl Pts',(42.2454039774546,-46.6408663419432,
40.1194874821985));
#199571=CARTESIAN_POINT('Ctrl Pts',(42.1872204559323,-46.6457133039297,
40.062755148314));
#199572=CARTESIAN_POINT('Ctrl Pts',(42.1199995355544,-46.6088541045838,
40.0767884282375));
#199573=CARTESIAN_POINT('Ctrl Pts',(42.2015749714288,-46.7146600431953,
40.1599502015385));
#199574=CARTESIAN_POINT('Ctrl Pts',(42.1587905896505,-46.7029882531943,
40.1002449453872));
#199575=CARTESIAN_POINT('Ctrl Pts',(42.1018187547553,-46.6595535157369,
40.10025));
#199576=CARTESIAN_POINT('Ctrl Pts',(42.1358900227694,-46.7738319284258,
40.1599502534424));
#199577=CARTESIAN_POINT('Ctrl Pts',(42.110921478106,-46.7461150696873,40.10025));
#199578=CARTESIAN_POINT('Ctrl Pts',(42.06380383897,-46.6938111422605,40.10025));
#199579=CARTESIAN_POINT('Origin',(42.1615090516451,-46.3506032922595,39.92499));
#199580=CARTESIAN_POINT('Origin',(39.5068809815359,-44.3513327445003,39.6398955069314));
#199581=CARTESIAN_POINT('Origin',(39.3876757945573,-44.2189419720524,39.92499));
#199582=CARTESIAN_POINT('Origin',(42.0423040287636,-46.2182127020529,39.6398955068275));
#199583=CARTESIAN_POINT('Origin',(41.9230990057955,-46.0858221116779,39.3548010137695));
#199584=CARTESIAN_POINT('Ctrl Pts',(39.3160391863689,-44.1385184650377,
39.8576902534424));
#199585=CARTESIAN_POINT('Ctrl Pts',(39.4103156382731,-44.0542875439841,
39.8579948730703));
#199586=CARTESIAN_POINT('Ctrl Pts',(39.4820551873929,-44.1339623850448,
39.92499));
#199587=CARTESIAN_POINT('Ctrl Pts',(39.285636938894,-44.1047525536513,39.9304020711229));
#199588=CARTESIAN_POINT('Ctrl Pts',(39.3789425853238,-44.0421527706792,
39.905891529738));
#199589=CARTESIAN_POINT('Ctrl Pts',(39.4516512848569,-44.1001954303886,
39.9671523786034));
#199590=CARTESIAN_POINT('Ctrl Pts',(39.2745942850999,-44.0527517782417,
40.0043257306695));
#199591=CARTESIAN_POINT('Ctrl Pts',(39.3566016867496,-44.0110417363798,
39.9667894847838));
#199592=CARTESIAN_POINT('Ctrl Pts',(39.4323285306301,-44.0556530121001,
40.0100138975203));
#199593=CARTESIAN_POINT('Ctrl Pts',(39.3050549810251,-43.9290071509457,
40.1195533054855));
#199594=CARTESIAN_POINT('Ctrl Pts',(39.3631024520342,-43.9243964923859,
40.0630813209234));
#199595=CARTESIAN_POINT('Ctrl Pts',(39.4299498468379,-43.9614781338113,
40.0768265942418));
#199596=CARTESIAN_POINT('Ctrl Pts',(39.3490583909343,-43.8557442421764,
40.1599502027513));
#199597=CARTESIAN_POINT('Ctrl Pts',(39.3917348424054,-43.8675206320107,
40.1002552791541));
#199598=CARTESIAN_POINT('Ctrl Pts',(39.4485000225483,-43.9111340157082,
40.10025));
#199599=CARTESIAN_POINT('Ctrl Pts',(39.4144401478989,-43.7969047596347,
40.1599502534424));
#199600=CARTESIAN_POINT('Ctrl Pts',(39.4393948122687,-43.8246341160486,
40.10025));
#199601=CARTESIAN_POINT('Ctrl Pts',(39.4864862581816,-43.8769616275875,
40.10025));
#199602=CARTESIAN_POINT('Origin',(39.4864862581816,-43.8769616275875,40.22725));
#199603=CARTESIAN_POINT('Ctrl Pts',(41.6348281284261,-45.7656648676107,
38.989));
#199604=CARTESIAN_POINT('Ctrl Pts',(41.5403077290112,-45.8507714175125,
38.989));
#199605=CARTESIAN_POINT('Ctrl Pts',(41.540448840768,-45.8506443599161,39.1161896013264));
#199606=CARTESIAN_POINT('Ctrl Pts',(41.7801793767999,-45.926760978665,38.989));
#199607=CARTESIAN_POINT('Ctrl Pts',(41.6856176794255,-46.0121552117511,
38.9887769275454));
#199608=CARTESIAN_POINT('Ctrl Pts',(41.6565546403139,-45.9795929135655,
39.1161898821845));
#199609=CARTESIAN_POINT('Ctrl Pts',(41.9185498083238,-46.0801233673961,
39.1034967087243));
#199610=CARTESIAN_POINT('Ctrl Pts',(41.8239142817211,-46.1657498592376,
39.1031720232711));
#199611=CARTESIAN_POINT('Ctrl Pts',(41.7670853619614,-46.1023497159511,
39.2077529615));
#199612=CARTESIAN_POINT('Ctrl Pts',(41.995572738225,-46.1654920697613,39.2875012672119));
#199613=CARTESIAN_POINT('Ctrl Pts',(41.9009568069092,-46.2513146407502,
39.2872087095507));
#199614=CARTESIAN_POINT('Ctrl Pts',(41.828611896708,-46.170681855241,39.3549017048226));
#199615=CARTESIAN_POINT('Origin',(41.6348281284261,-45.7656648676107,39.116));
#199616=CARTESIAN_POINT('Origin',(5.70392627685665E-15,5.20911706492846E-15,
40.22725));
#199617=CARTESIAN_POINT('Origin',(39.5091373124621,-43.8565665267057,40.22725));
#199618=CARTESIAN_POINT('Origin',(28.0951675083324,-30.7283483363945,39.116));
#199619=CARTESIAN_POINT('Origin',(41.3663085755633,-45.4673664422111,39.1160373285272));
#199620=CARTESIAN_POINT('Ctrl Pts',(39.4370498736007,-43.7765468711723,
40.1599502534424));
#199621=CARTESIAN_POINT('Ctrl Pts',(39.4620188529809,-43.804263338293,40.10025));
#199622=CARTESIAN_POINT('Ctrl Pts',(39.5091373124622,-43.8565665267057,
40.10025));
#199623=CARTESIAN_POINT('Ctrl Pts',(39.5021785224865,-43.717874483542,40.159950056604));
#199624=CARTESIAN_POINT('Ctrl Pts',(39.509465444133,-43.7615157339673,40.1002551305381));
#199625=CARTESIAN_POINT('Ctrl Pts',(39.5469637653745,-43.8224770900131,
40.10025));
#199626=CARTESIAN_POINT('Ctrl Pts',(39.57885162691,-43.6818502604296,40.1203070619049));
#199627=CARTESIAN_POINT('Ctrl Pts',(39.5685043961841,-43.7389249259232,
40.0637098684502));
#199628=CARTESIAN_POINT('Ctrl Pts',(39.5983821485331,-43.8091917332944,
40.0772636213363));
#199629=CARTESIAN_POINT('Ctrl Pts',(39.7059848156959,-43.6640874258692,
40.0046102245799));
#199630=CARTESIAN_POINT('Ctrl Pts',(39.656016872279,-43.7412697217739,39.9670001894009));
#199631=CARTESIAN_POINT('Ctrl Pts',(39.6923865500763,-43.8212571467117,
40.0101788811209));
#199632=CARTESIAN_POINT('Ctrl Pts',(39.7566878101774,-43.6806424921204,
39.9303710930188));
#199633=CARTESIAN_POINT('Ctrl Pts',(39.6846695243114,-43.7668962219027,
39.9058663574106));
#199634=CARTESIAN_POINT('Ctrl Pts',(39.7348023770065,-43.8452710114192,
39.9671344706366));
#199635=CARTESIAN_POINT('Ctrl Pts',(39.7870778846746,-43.7143933160624,
39.8576902534424));
#199636=CARTESIAN_POINT('Ctrl Pts',(39.69345381678,-43.7993487829614,39.8579948730703));
#199637=CARTESIAN_POINT('Ctrl Pts',(39.7651933658998,-43.8790236240221,
39.92499));
#199638=CARTESIAN_POINT('Origin',(39.8595727587354,-43.7940440370145,39.92499));
#199639=CARTESIAN_POINT('Origin',(41.3366772856869,-45.4345348103663,39.1925554488845));
#199640=CARTESIAN_POINT('Origin',(41.2819167515328,-45.3737170758073,39.3343017080178));
#199641=CARTESIAN_POINT('Origin',(39.9787779456623,-43.9264348094891,39.6398955069222));
#199642=CARTESIAN_POINT('Origin',(40.0979831325498,-44.0588255818379,39.3548010137695));
#199643=CARTESIAN_POINT('Ctrl Pts',(41.0611303347403,-45.1285089182134,
39.3978017080178));
#199644=CARTESIAN_POINT('Ctrl Pts',(40.9667509419047,-45.2134885052209,
39.3978017080178));
#199645=CARTESIAN_POINT('Ctrl Pts',(40.9667509419047,-45.2134885052209,
39.5248017080178));
#199646=CARTESIAN_POINT('Ctrl Pts',(41.1211850608443,-45.1955564429362,
39.3978017080178));
#199647=CARTESIAN_POINT('Ctrl Pts',(41.0269231466362,-45.2803165088384,
39.3980355775172));
#199648=CARTESIAN_POINT('Ctrl Pts',(41.057092984575,-45.3138235084259,39.5248015517192));
#199649=CARTESIAN_POINT('Ctrl Pts',(41.177972685568,-45.2589537050056,39.3484893995498));
#199650=CARTESIAN_POINT('Ctrl Pts',(41.0841042944919,-45.3438226072607,
39.3489438303435));
#199651=CARTESIAN_POINT('Ctrl Pts',(41.1425178129623,-45.4086973919099,
39.4508333155595));
#199652=CARTESIAN_POINT('Ctrl Pts',(41.2079002115907,-45.2923641298558,
39.2708017080178));
#199653=CARTESIAN_POINT('Ctrl Pts',(41.1142722655005,-45.3773275334106,
39.2710850691866));
#199654=CARTESIAN_POINT('Ctrl Pts',(41.1875373586971,-45.4586966628149,
39.3343017080178));
#199655=CARTESIAN_POINT('Origin',(41.0611303347403,-45.1285089182134,39.5248017080178));
#199656=CARTESIAN_POINT('Ctrl Pts',(40.0254908126588,-43.9791725362583,
39.2875012672119));
#199657=CARTESIAN_POINT('Ctrl Pts',(39.9317223035496,-44.0642551277131,
39.2878045257518));
#199658=CARTESIAN_POINT('Ctrl Pts',(40.0037114707678,-44.1439246046465,
39.3549015218347));
#199659=CARTESIAN_POINT('Ctrl Pts',(40.1025202360375,-44.0645378932548,
39.1034938540228));
#199660=CARTESIAN_POINT('Ctrl Pts',(40.0085500157865,-44.149581356248,39.1038286278812));
#199661=CARTESIAN_POINT('Ctrl Pts',(40.0652391174793,-44.2122579788857,
39.2077506434032));
#199662=CARTESIAN_POINT('Ctrl Pts',(40.2409001323908,-44.2178941385635,
38.989));
#199663=CARTESIAN_POINT('Ctrl Pts',(40.1466780419433,-44.3029888158473,
38.9892298954623));
#199664=CARTESIAN_POINT('Ctrl Pts',(40.1757707681161,-44.3350158129981,
39.1161900347288));
#199665=CARTESIAN_POINT('Ctrl Pts',(40.3862543050938,-44.3789831537296,
38.989));
#199666=CARTESIAN_POINT('Ctrl Pts',(40.2917335385824,-44.4640900341666,
38.989));
#199667=CARTESIAN_POINT('Ctrl Pts',(40.2918750179835,-44.4639626455416,
39.1161900945645));
#199668=CARTESIAN_POINT('Origin',(40.3862543050938,-44.3789831537296,39.116));
#199669=CARTESIAN_POINT('Origin',(27.4203375923833,-29.9788737863603,39.5248017080178));
#199670=CARTESIAN_POINT('Origin',(40.9599523566124,-45.0161393894794,39.5248017080178));
#199671=CARTESIAN_POINT('Origin',(27.314662201079,-29.8615093742683,39.116));
#199672=CARTESIAN_POINT('Origin',(40.654855397468,-44.6772189625516,39.1160402713848));
#199673=CARTESIAN_POINT('Ctrl Pts',(40.8131880745606,-44.8522789915942,
39.2708017080178));
#199674=CARTESIAN_POINT('Ctrl Pts',(40.7187157882337,-44.9380175594363,
39.27051194648));
#199675=CARTESIAN_POINT('Ctrl Pts',(40.6447864996552,-44.8559107663286,
39.3343017080178));
#199676=CARTESIAN_POINT('Ctrl Pts',(40.8432146576643,-44.8858042435433,
39.3487519301185));
#199677=CARTESIAN_POINT('Ctrl Pts',(40.7486708738394,-44.9712860523915,
39.3482879463973));
#199678=CARTESIAN_POINT('Ctrl Pts',(40.6899581892273,-44.9060790100834,
39.4512271261623));
#199679=CARTESIAN_POINT('Ctrl Pts',(40.9001003367647,-44.9493173051403,
39.3978017080178));
#199680=CARTESIAN_POINT('Ctrl Pts',(40.8054891887053,-45.034389183955,39.3975673827415));
#199681=CARTESIAN_POINT('Ctrl Pts',(40.7755352187358,-45.0011219300374,
39.5248015355199));
#199682=CARTESIAN_POINT('Ctrl Pts',(40.9599523566124,-45.0161393894794,
39.3978017080178));
#199683=CARTESIAN_POINT('Ctrl Pts',(40.8655729637768,-45.1011189764869,
39.3978017080178));
#199684=CARTESIAN_POINT('Ctrl Pts',(40.8655729637768,-45.101118976487,39.5248017080178));
#199685=CARTESIAN_POINT('Origin',(40.7391658924908,-44.7709311793211,39.3343017080178));
#199686=CARTESIAN_POINT('Origin',(40.684731939279,-44.710476149201,39.1934008533553));
#199687=CARTESIAN_POINT('Origin',(35.8473027488288,-49.8797426639489,39.1925554495083));
#199688=CARTESIAN_POINT('Origin',(35.8732562382987,-49.9155525184317,39.1160373285263));
#199689=CARTESIAN_POINT('Origin',(35.7991993820661,-49.8135340601224,39.3343017080178));
#199690=CARTESIAN_POINT('Ctrl Pts',(35.7350130971388,-49.7242207306176,
39.2708017080178));
#199691=CARTESIAN_POINT('Ctrl Pts',(35.8375861910555,-49.6503036646786,
39.2710850691866));
#199692=CARTESIAN_POINT('Ctrl Pts',(35.9019445403517,-49.7388853330812,
39.3343017080178));
#199693=CARTESIAN_POINT('Ctrl Pts',(35.7084656432366,-49.6878783768789,
39.3487519293518));
#199694=CARTESIAN_POINT('Ctrl Pts',(35.8109961808879,-49.6137056554146,
39.3492068662942));
#199695=CARTESIAN_POINT('Ctrl Pts',(35.8622643302253,-49.6842702092628,
39.4512271248743));
#199696=CARTESIAN_POINT('Ctrl Pts',(35.6581711379713,-49.6190282456268,
39.3978017080178));
#199697=CARTESIAN_POINT('Ctrl Pts',(35.7606778378466,-49.5444483977879,
39.3980347781159));
#199698=CARTESIAN_POINT('Ctrl Pts',(35.78709080949,-49.5808027344244,39.524801535519));
#199699=CARTESIAN_POINT('Ctrl Pts',(35.6052536882601,-49.5465907136145,
39.3978017080178));
#199700=CARTESIAN_POINT('Ctrl Pts',(35.7079988465457,-49.4719419865734,
39.3978017080178));
#199701=CARTESIAN_POINT('Ctrl Pts',(35.7079988465457,-49.4719419865734,
39.5248017080178));
#199702=CARTESIAN_POINT('Origin',(35.6052536882601,-49.5465907136145,39.5248017080178));
#199703=CARTESIAN_POINT('Origin',(-0.256862895714041,-0.18662181760286,
39.116));
#199704=CARTESIAN_POINT('Origin',(36.1092077731528,-50.2402240048084,39.116));
#199705=CARTESIAN_POINT('Origin',(-0.256862895714041,-0.18662181760286,
39.5248017080178));
#199706=CARTESIAN_POINT('Origin',(35.5163757878395,-49.4242607783462,39.5248017080178));
#199707=CARTESIAN_POINT('Ctrl Pts',(36.4252947698678,-50.6762142289949,
39.2875012672119));
#199708=CARTESIAN_POINT('Ctrl Pts',(36.5289136610815,-50.6015094050816,
39.287208709576));
#199709=CARTESIAN_POINT('Ctrl Pts',(36.465084262422,-50.5139809070355,39.3549016990122));
#199710=CARTESIAN_POINT('Ctrl Pts',(36.3578045222547,-50.5831238715082,
39.1034939173931));
#199711=CARTESIAN_POINT('Ctrl Pts',(36.4612356912236,-50.5083591136214,
39.1031692336309));
#199712=CARTESIAN_POINT('Ctrl Pts',(36.4110366091595,-50.4395906940207,
39.2077507202297));
#199713=CARTESIAN_POINT('Ctrl Pts',(36.2365613423298,-50.4158900112683,
38.989));
#199714=CARTESIAN_POINT('Ctrl Pts',(36.3397499727042,-50.3411491755169,
38.9887769311206));
#199715=CARTESIAN_POINT('Ctrl Pts',(36.3139421975387,-50.3059517008895,
39.1161898712915));
#199716=CARTESIAN_POINT('Ctrl Pts',(36.1092077731528,-50.2402240048084,
38.989));
#199717=CARTESIAN_POINT('Ctrl Pts',(36.2121064279403,-50.1654637560306,
38.989));
#199718=CARTESIAN_POINT('Ctrl Pts',(36.2119528169512,-50.165575360947,39.1161895903854));
#199719=CARTESIAN_POINT('Origin',(36.3624339277672,-50.5887599058102,39.3548010137695));
#199720=CARTESIAN_POINT('Ctrl Pts',(35.5163757878395,-49.4242607783461,
39.3978017080178));
#199721=CARTESIAN_POINT('Ctrl Pts',(35.6191209461251,-49.349612051305,39.3978017080178));
#199722=CARTESIAN_POINT('Ctrl Pts',(35.6191209461251,-49.349612051305,39.5248017080178));
#199723=CARTESIAN_POINT('Ctrl Pts',(35.463279014105,-49.3515787599188,39.3978017080178));
#199724=CARTESIAN_POINT('Ctrl Pts',(35.5661632154433,-49.2767219882452,
39.3975666025064));
#199725=CARTESIAN_POINT('Ctrl Pts',(35.5397616632044,-49.2403833690714,
39.5248015517196));
#199726=CARTESIAN_POINT('Ctrl Pts',(35.4130704930576,-49.2828534857283,
39.3484894016717));
#199727=CARTESIAN_POINT('Ctrl Pts',(35.5163418450515,-49.2081487547874,
39.348025900002));
#199728=CARTESIAN_POINT('Ctrl Pts',(35.4647218031673,-49.1370998624016,
39.4508333188939));
#199729=CARTESIAN_POINT('Ctrl Pts',(35.3866101428259,-49.2466351556013,
39.2708017080178));
#199730=CARTESIAN_POINT('Ctrl Pts',(35.4901170100366,-49.1720533660032,
39.27051194648));
#199731=CARTESIAN_POINT('Ctrl Pts',(35.4251752107437,-49.0826686475735,
39.3343017080178));
#199732=CARTESIAN_POINT('Origin',(35.3224300524581,-49.1573173746147,39.3343017080178));
#199733=CARTESIAN_POINT('Origin',(36.4671473482325,-50.7328855645261,39.6398955068185));
#199734=CARTESIAN_POINT('Origin',(36.5718607685321,-50.8770112231003,39.92499));
#199735=CARTESIAN_POINT('Origin',(35.2746135646418,-49.0915036252741,39.193400853995));
#199736=CARTESIAN_POINT('Origin',(35.248294810039,-49.0553654007527,39.1160402713851));
#199737=CARTESIAN_POINT('Ctrl Pts',(36.9911673391707,-50.9399462128202,
40.1599502534424));
#199738=CARTESIAN_POINT('Ctrl Pts',(36.9692474126339,-50.9097606317995,
40.10025));
#199739=CARTESIAN_POINT('Ctrl Pts',(36.9278827595326,-50.8527980281386,
40.10025));
#199740=CARTESIAN_POINT('Ctrl Pts',(36.9198678602471,-50.9917217504954,
40.159950053846));
#199741=CARTESIAN_POINT('Ctrl Pts',(36.9173100216891,-50.9474721267378,
40.100244835349));
#199742=CARTESIAN_POINT('Ctrl Pts',(36.8866065570941,-50.8827604229948,
40.10025));
#199743=CARTESIAN_POINT('Ctrl Pts',(36.8393772800888,-51.019255329238,40.1202442001039));
#199744=CARTESIAN_POINT('Ctrl Pts',(36.8558881875866,-50.96349009182,40.0633873868017));
#199745=CARTESIAN_POINT('Ctrl Pts',(36.8338178466776,-50.890167891183,40.0772271723535));
#199746=CARTESIAN_POINT('Ctrl Pts',(36.7103770798844,-51.0231582082087,
40.0045995998162));
#199747=CARTESIAN_POINT('Ctrl Pts',(36.7689134067395,-50.951578055317,39.9663485808314));
#199748=CARTESIAN_POINT('Ctrl Pts',(36.7411592876131,-50.8676678805073,
40.0101727202468));
#199749=CARTESIAN_POINT('Ctrl Pts',(36.6614543958834,-51.0012539523492,
39.9304654349859));
#199750=CARTESIAN_POINT('Ctrl Pts',(36.7432876021378,-50.9229784487434,
39.9051900162952));
#199751=CARTESIAN_POINT('Ctrl Pts',(36.7013347616514,-50.8391515810796,
39.9671857458171));
#199752=CARTESIAN_POINT('Ctrl Pts',(36.6347241449653,-50.9644637245894,
39.8576902534424));
#199753=CARTESIAN_POINT('Ctrl Pts',(36.7381840359683,-50.8898702560319,
39.8573998014387));
#199754=CARTESIAN_POINT('Ctrl Pts',(36.6746059268177,-50.8023624960592,
39.92499));
#199755=CARTESIAN_POINT('Origin',(36.9278827595326,-50.8527980281386,40.22725));
#199756=CARTESIAN_POINT('Origin',(-0.256862895714041,-0.18662181760286,
39.116));
#199757=CARTESIAN_POINT('Origin',(35.0124214764584,-48.7306271754177,39.116));
#199758=CARTESIAN_POINT('Origin',(5.56775724677592E-15,5.82828306711173E-15,
40.22725));
#199759=CARTESIAN_POINT('Origin',(36.9525415975211,-50.8348823336487,40.22725));
#199760=CARTESIAN_POINT('Ctrl Pts',(35.0124214764584,-48.7306271754177,
38.989));
#199761=CARTESIAN_POINT('Ctrl Pts',(35.115320551631,-48.6558666212124,38.989));
#199762=CARTESIAN_POINT('Ctrl Pts',(35.1151665196293,-48.6559785320122,
39.1161901092325));
#199763=CARTESIAN_POINT('Ctrl Pts',(34.8850714976643,-48.5549543235569,
38.989));
#199764=CARTESIAN_POINT('Ctrl Pts',(34.9878965398057,-48.4804833899301,
38.9892298989718));
#199765=CARTESIAN_POINT('Ctrl Pts',(35.0131753353122,-48.5155997094333,
39.1161900493187));
#199766=CARTESIAN_POINT('Ctrl Pts',(34.7638382096871,-48.3877151240587,
39.1034966344368));
#199767=CARTESIAN_POINT('Ctrl Pts',(34.8665607873104,-48.3134799021662,
39.1038314102594));
#199768=CARTESIAN_POINT('Ctrl Pts',(34.9160816462009,-48.3819617107278,
39.2077528789613));
#199769=CARTESIAN_POINT('Ctrl Pts',(34.6963546279284,-48.2946219293747,
39.2875012672119));
#199770=CARTESIAN_POINT('Ctrl Pts',(34.7990735417353,-48.2205921440829,
39.2878045257868));
#199771=CARTESIAN_POINT('Ctrl Pts',(34.862034655413,-48.3075724095164,39.35490152959));
#199772=CARTESIAN_POINT('Origin',(34.7591950625533,-48.382090917533,39.3548010137695));
#199773=CARTESIAN_POINT('Ctrl Pts',(37.149332979726,-50.5905785208485,39.8576902534424));
#199774=CARTESIAN_POINT('Ctrl Pts',(37.0464195108252,-50.6659240749084,
39.8573998014387));
#199775=CARTESIAN_POINT('Ctrl Pts',(36.9828414016746,-50.5784163149358,
39.92499));
#199776=CARTESIAN_POINT('Ctrl Pts',(37.1760745934432,-50.6273860247244,
39.9304984902492));
#199777=CARTESIAN_POINT('Ctrl Pts',(37.0763471615772,-50.6810174228634,
39.9052171569798));
#199778=CARTESIAN_POINT('Ctrl Pts',(37.0095824157648,-50.6152221632646,
39.96720497266));
#199779=CARTESIAN_POINT('Ctrl Pts',(37.1816769644889,-50.6805407410137,
40.004343767866));
#199780=CARTESIAN_POINT('Ctrl Pts',(37.0954833955433,-50.7141678268707,
39.9661628577643));
#199781=CARTESIAN_POINT('Ctrl Pts',(37.0242869695758,-50.6617655220317,
40.0100243556233));
#199782=CARTESIAN_POINT('Ctrl Pts',(37.138681150061,-50.8012099538926,40.1194874821989));
#199783=CARTESIAN_POINT('Ctrl Pts',(37.0803097184689,-50.799948529622,40.0627551483141));
#199784=CARTESIAN_POINT('Ctrl Pts',(37.0173098767915,-50.7562647493197,
40.0767884282379));
#199785=CARTESIAN_POINT('Ctrl Pts',(37.0873787017263,-50.8700180268817,
40.1599502015399));
#199786=CARTESIAN_POINT('Ctrl Pts',(37.0460487315422,-50.8539379904903,
40.1002449453869));
#199787=CARTESIAN_POINT('Ctrl Pts',(36.9939291606774,-50.8047860147175,
40.10025));
#199788=CARTESIAN_POINT('Ctrl Pts',(37.0158684358559,-50.9219998155901,
40.1599502534424));
#199789=CARTESIAN_POINT('Ctrl Pts',(36.9939338721432,-50.8918248691001,
40.10025));
#199790=CARTESIAN_POINT('Ctrl Pts',(36.9525415975211,-50.8348823336487,
40.10025));
#199791=CARTESIAN_POINT('Origin',(37.0855865599602,-50.5037675878946,39.92499));
#199792=CARTESIAN_POINT('Origin',(34.6544814981912,-48.2379650606676,39.6398955069316));
#199793=CARTESIAN_POINT('Origin',(34.549767933694,-48.0938392037149,39.92499));
#199794=CARTESIAN_POINT('Origin',(36.980873139611,-50.35964192934,39.6398955068268));
#199795=CARTESIAN_POINT('Origin',(36.8761597191953,-50.2155162706045,39.3548010137695));
#199796=CARTESIAN_POINT('Ctrl Pts',(34.4869303039396,-48.0063682005188,
39.8576902534424));
#199797=CARTESIAN_POINT('Ctrl Pts',(34.5894948283132,-47.9324532779038,
39.8579948730703));
#199798=CARTESIAN_POINT('Ctrl Pts',(34.6525130919796,-48.0191904766737,
39.92499));
#199799=CARTESIAN_POINT('Ctrl Pts',(34.4602241019854,-47.9696093621194,
39.9304020711232));
#199800=CARTESIAN_POINT('Ctrl Pts',(34.5595620694348,-47.9171056031439,
39.9058915297378));
#199801=CARTESIAN_POINT('Ctrl Pts',(34.6258053530817,-47.982430427718,39.9671523786029));
#199802=CARTESIAN_POINT('Ctrl Pts',(34.4546775021467,-47.9167391807672,
40.0043257306691));
#199803=CARTESIAN_POINT('Ctrl Pts',(34.5405955452487,-47.8838297385501,
39.9667894847831));
#199804=CARTESIAN_POINT('Ctrl Pts',(34.611244401459,-47.9361122396534,40.01001389752));
#199805=CARTESIAN_POINT('Ctrl Pts',(34.4979061669209,-47.796856449222,40.1195533054859));
#199806=CARTESIAN_POINT('Ctrl Pts',(34.5561175928638,-47.7983386612733,
40.0630813209239));
#199807=CARTESIAN_POINT('Ctrl Pts',(34.6187227036512,-47.8422046210389,
40.0768265942421));
#199808=CARTESIAN_POINT('Ctrl Pts',(34.5493265808148,-47.7285944911488,
40.1599502027517));
#199809=CARTESIAN_POINT('Ctrl Pts',(34.5905382782863,-47.7447672725759,
40.1002552791544));
#199810=CARTESIAN_POINT('Ctrl Pts',(34.6424336528575,-47.7940753146429,
40.10025));
#199811=CARTESIAN_POINT('Ctrl Pts',(34.6205005703634,-47.6769115920305,
40.1599502534424));
#199812=CARTESIAN_POINT('Ctrl Pts',(34.6424200234574,-47.7070975168465,
40.10025));
#199813=CARTESIAN_POINT('Ctrl Pts',(34.6837837831345,-47.7640607692764,
40.10025));
#199814=CARTESIAN_POINT('Origin',(34.6837837831345,-47.7640607692764,40.22725));
#199815=CARTESIAN_POINT('Ctrl Pts',(36.6229335645808,-49.8669803696027,
38.989));
#199816=CARTESIAN_POINT('Ctrl Pts',(36.5200349009287,-49.9417406248209,
38.989));
#199817=CARTESIAN_POINT('Ctrl Pts',(36.5201885207956,-49.9416290134544,
39.1161896013263));
#199818=CARTESIAN_POINT('Ctrl Pts',(36.7506494346807,-50.0423873219315,
38.989));
#199819=CARTESIAN_POINT('Ctrl Pts',(36.647679628225,-50.1174293675636,38.988776927546));
#199820=CARTESIAN_POINT('Ctrl Pts',(36.6221794864701,-50.0820075342383,
39.1161898821844));
#199821=CARTESIAN_POINT('Ctrl Pts',(36.872231123687,-50.2093732240185,39.1034967087243));
#199822=CARTESIAN_POINT('Ctrl Pts',(36.7691636147949,-50.2846385388079,
39.1031720232715));
#199823=CARTESIAN_POINT('Ctrl Pts',(36.7192731293496,-50.2156454684929,
39.2077529615002));
#199824=CARTESIAN_POINT('Ctrl Pts',(36.9399086546485,-50.3023253561996,
39.2875012672119));
#199825=CARTESIAN_POINT('Ctrl Pts',(36.8368401378453,-50.3777877242638,
39.2872087095508));
#199826=CARTESIAN_POINT('Ctrl Pts',(36.7733199617899,-50.2900345513019,
39.3549017048226));
#199827=CARTESIAN_POINT('Origin',(36.6229335645808,-49.8669803696026,39.116));
#199828=CARTESIAN_POINT('Origin',(5.69915478234096E-15,5.20525318485518E-15,
40.22725));
#199829=CARTESIAN_POINT('Origin',(34.7084426211231,-47.7461450747865,40.22725));
#199830=CARTESIAN_POINT('Origin',(21.7541926348211,-29.4019141737116,39.116));
#199831=CARTESIAN_POINT('Origin',(36.3870656659257,-49.5422481179703,39.1160373285258));
#199832=CARTESIAN_POINT('Ctrl Pts',(34.6451144164185,-47.6590285860936,
40.1599502534424));
#199833=CARTESIAN_POINT('Ctrl Pts',(34.6670494534017,-47.6892031885514,
40.10025));
#199834=CARTESIAN_POINT('Ctrl Pts',(34.7084426211231,-47.7461450747865,
40.10025));
#199835=CARTESIAN_POINT('Ctrl Pts',(34.7160192182665,-47.6074854095245,
40.1599500566037));
#199836=CARTESIAN_POINT('Ctrl Pts',(34.718704468552,-47.6516492793353,40.1002551305372));
#199837=CARTESIAN_POINT('Ctrl Pts',(34.7496251732003,-47.7161963245896,
40.10025));
#199838=CARTESIAN_POINT('Ctrl Pts',(34.7960378560836,-47.5796730526551,
40.1203070619048));
#199839=CARTESIAN_POINT('Ctrl Pts',(34.7797813814945,-47.6353534770325,
40.0637098684496));
#199840=CARTESIAN_POINT('Ctrl Pts',(34.8021505789969,-47.7083584310193,
40.0772636213363));
#199841=CARTESIAN_POINT('Ctrl Pts',(34.9243313177593,-47.5752965616148,
40.00461022458));
#199842=CARTESIAN_POINT('Ctrl Pts',(34.8665693571826,-47.6468329724886,
39.9670001894015));
#199843=CARTESIAN_POINT('Ctrl Pts',(34.8943788354697,-47.7301838844735,
40.0101788811209));
#199844=CARTESIAN_POINT('Ctrl Pts',(34.973026080298,-47.5970608435766,39.9303710930188));
#199845=CARTESIAN_POINT('Ctrl Pts',(34.8923863483134,-47.6753141056561,
39.9058663574116));
#199846=CARTESIAN_POINT('Ctrl Pts',(34.9340521716871,-47.7584998599249,
39.9671344706372));
#199847=CARTESIAN_POINT('Ctrl Pts',(34.9997217530259,-47.63380340476,39.8576902534424));
#199848=CARTESIAN_POINT('Ctrl Pts',(34.8977303031701,-47.7085070967804,
39.8579948730703));
#199849=CARTESIAN_POINT('Ctrl Pts',(34.9607485668365,-47.7952442955503,
39.92499));
#199850=CARTESIAN_POINT('Origin',(35.0634937251221,-47.7205955685091,39.92499));
#199851=CARTESIAN_POINT('Origin',(36.3610285393807,-49.5064990280457,39.1925554488851));
#199852=CARTESIAN_POINT('Origin',(36.3129251734942,-49.4402904249166,39.3343017080178));
#199853=CARTESIAN_POINT('Origin',(35.1682072895601,-47.8647214254832,39.6398955069207));
#199854=CARTESIAN_POINT('Origin',(35.2729208539814,-48.0088472823273,39.3548010137695));
#199855=CARTESIAN_POINT('Ctrl Pts',(36.1189794796882,-49.1733470784088,
39.3978017080178));
#199856=CARTESIAN_POINT('Ctrl Pts',(36.0162343214026,-49.24799580545,39.3978017080178));
#199857=CARTESIAN_POINT('Ctrl Pts',(36.0162343214026,-49.24799580545,39.5248017080178));
#199858=CARTESIAN_POINT('Ctrl Pts',(36.1716968449935,-49.2463047380076,
39.3978017080178));
#199859=CARTESIAN_POINT('Ctrl Pts',(36.0690914679803,-49.3207474263657,
39.3980355775177));
#199860=CARTESIAN_POINT('Ctrl Pts',(36.0955935972132,-49.3572244778974,
39.5248015517192));
#199861=CARTESIAN_POINT('Ctrl Pts',(36.221546562787,-49.3152906263877,39.3484893995498));
#199862=CARTESIAN_POINT('Ctrl Pts',(36.1193211766474,-49.389882689243,39.3489438303423));
#199863=CARTESIAN_POINT('Ctrl Pts',(36.1706334382084,-49.4605079583582,
39.4508333155597));
#199864=CARTESIAN_POINT('Ctrl Pts',(36.247817802325,-49.3516463037386,39.2708017080178));
#199865=CARTESIAN_POINT('Ctrl Pts',(36.1458216659124,-49.4263574835552,
39.2710850691866));
#199866=CARTESIAN_POINT('Ctrl Pts',(36.2101800152086,-49.5149391519578,
39.3343017080178));
#199867=CARTESIAN_POINT('Origin',(36.1189794796882,-49.1733470784088,39.5248017080178));
#199868=CARTESIAN_POINT('Ctrl Pts',(35.2091516650527,-47.9220530736688,
39.2875012672119));
#199869=CARTESIAN_POINT('Ctrl Pts',(35.1070032771119,-47.9968680956252,
39.2878045257518));
#199870=CARTESIAN_POINT('Ctrl Pts',(35.1702703521467,-48.0836260518493,
39.3549015218348));
#199871=CARTESIAN_POINT('Ctrl Pts',(35.2768360036064,-48.0150025575606,
39.1034938540228));
#199872=CARTESIAN_POINT('Ctrl Pts',(35.1744910995523,-48.0897575808465,
39.1038286278812));
#199873=CARTESIAN_POINT('Ctrl Pts',(35.2243181613714,-48.158016479072,39.2077506434027));
#199874=CARTESIAN_POINT('Ctrl Pts',(35.3984277477543,-48.1819833392241,
38.989));
#199875=CARTESIAN_POINT('Ctrl Pts',(35.2958269999289,-48.2567629686459,
38.9892298954605));
#199876=CARTESIAN_POINT('Ctrl Pts',(35.3214126203093,-48.2916555365114,
39.1161900347289));
#199877=CARTESIAN_POINT('Ctrl Pts',(35.5261472678865,-48.357383540212,38.989));
#199878=CARTESIAN_POINT('Ctrl Pts',(35.4232482045983,-48.4321440857828,
38.989));
#199879=CARTESIAN_POINT('Ctrl Pts',(35.4234022246977,-48.4320321836304,
39.1161900945646));
#199880=CARTESIAN_POINT('Origin',(35.5261472678865,-48.357383540212,39.116));
#199881=CARTESIAN_POINT('Origin',(21.2334658618522,-28.6851952578918,39.5248017080178));
#199882=CARTESIAN_POINT('Origin',(36.0301015792676,-49.0510171431404,39.5248017080178));
#199883=CARTESIAN_POINT('Origin',(21.151922343707,-28.5729602337851,39.116));
#199884=CARTESIAN_POINT('Origin',(35.762102804585,-48.6820620414862,39.1160402713848));
#199885=CARTESIAN_POINT('Ctrl Pts',(35.9012693628904,-48.8727133447944,
39.2708017080178));
#199886=CARTESIAN_POINT('Ctrl Pts',(35.7983524848935,-48.9481071848797,
39.27051194648));
#199887=CARTESIAN_POINT('Ctrl Pts',(35.7334106856005,-48.8587224664501,
39.3343017080178));
#199888=CARTESIAN_POINT('Ctrl Pts',(35.9276271141644,-48.9091935744936,
39.3487519301186));
#199889=CARTESIAN_POINT('Ctrl Pts',(35.8246659689634,-48.9843245886171,
39.3482879463969));
#199890=CARTESIAN_POINT('Ctrl Pts',(35.773090910506,-48.9133376106102,39.4512271261627));
#199891=CARTESIAN_POINT('Ctrl Pts',(35.9775622448344,-48.9783048775136,
39.3978017080178));
#199892=CARTESIAN_POINT('Ctrl Pts',(35.8745769537838,-49.0530211657578,
39.3975673827411));
#199893=CARTESIAN_POINT('Ctrl Pts',(35.8482644497259,-49.0168051108904,
39.5248015355194));
#199894=CARTESIAN_POINT('Ctrl Pts',(36.0301015792676,-49.0510171431404,
39.3978017080178));
#199895=CARTESIAN_POINT('Ctrl Pts',(35.927356420982,-49.1256658701816,39.3978017080178));
#199896=CARTESIAN_POINT('Ctrl Pts',(35.927356420982,-49.1256658701816,39.5248017080178));
#199897=CARTESIAN_POINT('Origin',(35.8361558438862,-48.784073739409,39.3343017080178));
#199898=CARTESIAN_POINT('Origin',(35.7883393569609,-48.7182599907918,39.1934008533547));
#199899=CARTESIAN_POINT('Origin',(30.4370746247567,-53.3535596832589,39.1925554495088));
#199900=CARTESIAN_POINT('Origin',(30.4591427892365,-53.3918862459835,39.1160373285291));
#199901=CARTESIAN_POINT('Origin',(30.3961554568836,-53.2826856060846,39.3343017080178));
#199902=CARTESIAN_POINT('Ctrl Pts',(30.3416565762235,-53.1871522506176,
39.2708017080178));
#199903=CARTESIAN_POINT('Ctrl Pts',(30.4513942013112,-53.1243619179796,
39.2710850691866));
#199904=CARTESIAN_POINT('Ctrl Pts',(30.5061406831642,-53.2191856060846,
39.3343017080178));
#199905=CARTESIAN_POINT('Ctrl Pts',(30.3190533624391,-53.1482340195353,
39.3487519293518));
#199906=CARTESIAN_POINT('Ctrl Pts',(30.4287753876654,-53.0851849835372,
39.3492068662939));
#199907=CARTESIAN_POINT('Ctrl Pts',(30.4723866803437,-53.1607219582407,
39.4512271248739));
#199908=CARTESIAN_POINT('Ctrl Pts',(30.2762311741517,-53.0745038491598,
39.3978017080178));
#199909=CARTESIAN_POINT('Ctrl Pts',(30.3859720484856,-53.0110474253454,
39.3980347781155));
#199910=CARTESIAN_POINT('Ctrl Pts',(30.4084402641651,-53.0499635164573,
39.524801535519));
#199911=CARTESIAN_POINT('Ctrl Pts',(30.2311753956711,-52.9969317578288,
39.3978017080178));
#199912=CARTESIAN_POINT('Ctrl Pts',(30.3411606219517,-52.9334317578288,
39.3978017080178));
#199913=CARTESIAN_POINT('Ctrl Pts',(30.3411606219517,-52.9334317578288,
39.5248017080178));
#199914=CARTESIAN_POINT('Origin',(30.2311753956711,-52.9969317578288,39.5248017080178));
#199915=CARTESIAN_POINT('Origin',(-0.274963065701554,-0.158749999999999,
39.116));
#199916=CARTESIAN_POINT('Origin',(30.6598643453574,-53.7394427993287,39.116));
#199917=CARTESIAN_POINT('Origin',(-0.274963065701554,-0.158749999999999,
39.5248017080178));
#199918=CARTESIAN_POINT('Origin',(30.1555713378337,-52.865981688396,39.5248017080178));
#199919=CARTESIAN_POINT('Ctrl Pts',(30.9286463962977,-54.2060847114742,
39.2875012672119));
#199920=CARTESIAN_POINT('Ctrl Pts',(31.0395064328261,-54.1426202518668,
39.287208709576));
#199921=CARTESIAN_POINT('Ctrl Pts',(30.9851759176836,-54.048899255138,39.3549016990124));
#199922=CARTESIAN_POINT('Ctrl Pts',(30.8712564593359,-54.1064496608375,
39.1034939173931));
#199923=CARTESIAN_POINT('Ctrl Pts',(30.9819360667855,-54.0429059732659,
39.1031692336342));
#199924=CARTESIAN_POINT('Ctrl Pts',(30.9392002377702,-53.9692670413563,
39.2077507202308));
#199925=CARTESIAN_POINT('Ctrl Pts',(30.7681581606542,-53.9274585619024,
38.989));
#199926=CARTESIAN_POINT('Ctrl Pts',(30.8785940576193,-53.8639133132281,
38.9887769311158));
#199927=CARTESIAN_POINT('Ctrl Pts',(30.8566067980787,-53.8262110069715,
39.11618987129));
#199928=CARTESIAN_POINT('Ctrl Pts',(30.6598643453574,-53.7394427993287,
38.989));
#199929=CARTESIAN_POINT('Ctrl Pts',(30.770013884466,-53.6758479332732,38.989));
#199930=CARTESIAN_POINT('Ctrl Pts',(30.7698494490833,-53.6759428700857,
39.1161895903856));
#199931=CARTESIAN_POINT('Origin',(30.8752713784761,-54.112538724998,39.3548010137695));
#199932=CARTESIAN_POINT('Ctrl Pts',(30.1555713378337,-52.865981688396,39.3978017080178));
#199933=CARTESIAN_POINT('Ctrl Pts',(30.2655565641143,-52.802481688396,39.3978017080178));
#199934=CARTESIAN_POINT('Ctrl Pts',(30.2655565641143,-52.802481688396,39.5248017080178));
#199935=CARTESIAN_POINT('Ctrl Pts',(30.1103627734745,-52.7881477055076,
39.3978017080178));
#199936=CARTESIAN_POINT('Ctrl Pts',(30.2205080277021,-52.7244553345209,
39.397566602504));
#199937=CARTESIAN_POINT('Ctrl Pts',(30.1980495259466,-52.6855560684211,
39.5248015517196));
#199938=CARTESIAN_POINT('Ctrl Pts',(30.0676130472596,-52.7145506960108,
39.3484894016716));
#199939=CARTESIAN_POINT('Ctrl Pts',(30.1781274387069,-52.6510500011263,
39.3480259000035));
#199940=CARTESIAN_POINT('Ctrl Pts',(30.1342168083496,-52.5749945583579,
39.4508333188932));
#199941=CARTESIAN_POINT('Ctrl Pts',(30.0450834959835,-52.6757649139396,
39.2708017080178));
#199942=CARTESIAN_POINT('Ctrl Pts',(30.1558192616,-52.6124111049557,39.27051194648));
#199943=CARTESIAN_POINT('Ctrl Pts',(30.1005764675357,-52.5167277788842,
39.3343017080178));
#199944=CARTESIAN_POINT('Origin',(29.9905912412551,-52.5802277788842,39.3343017080178));
#199945=CARTESIAN_POINT('Origin',(30.9643459342435,-54.2668203812016,39.6398955068181));
#199946=CARTESIAN_POINT('Origin',(31.0534204898633,-54.4211020372439,39.92499));
#199947=CARTESIAN_POINT('Origin',(29.9499161072417,-52.5097763801582,39.1934008539954));
#199948=CARTESIAN_POINT('Origin',(29.9275190026059,-52.4710850656384,39.116040271385));
#199949=CARTESIAN_POINT('Ctrl Pts',(31.4638515574739,-54.527521733972,40.1599502534424));
#199950=CARTESIAN_POINT('Ctrl Pts',(31.4452069629852,-54.4952102564866,
40.10025));
#199951=CARTESIAN_POINT('Ctrl Pts',(31.410023123206,-54.4342359163064,40.10025));
#199952=CARTESIAN_POINT('Ctrl Pts',(31.3875306471682,-54.5715608148713,
40.1599500538469));
#199953=CARTESIAN_POINT('Ctrl Pts',(31.3896121658908,-54.5272862282519,
40.100244835349));
#199954=CARTESIAN_POINT('Ctrl Pts',(31.365841113034,-54.4597196360198,40.10025));
#199955=CARTESIAN_POINT('Ctrl Pts',(31.3046029601556,-54.5905300051366,
40.1202442001039));
#199956=CARTESIAN_POINT('Ctrl Pts',(31.3268524737457,-54.5367961153117,
40.0633873868018));
#199957=CARTESIAN_POINT('Ctrl Pts',(31.3125672934292,-54.4615686025423,
40.0772271723537));
#199958=CARTESIAN_POINT('Ctrl Pts',(31.1759014746041,-54.5809273110395,
40.0045995998162));
#199959=CARTESIAN_POINT('Ctrl Pts',(31.2415992967183,-54.5158579940066,
39.9663485808315));
#199960=CARTESIAN_POINT('Ctrl Pts',(31.2227682191859,-54.4295063924928,
40.0101727202466));
#199961=CARTESIAN_POINT('Ctrl Pts',(31.1295364123887,-54.554029236008,39.9304654349859));
#199962=CARTESIAN_POINT('Ctrl Pts',(31.2191033458799,-54.4847364330952,
39.905190016295));
#199963=CARTESIAN_POINT('Ctrl Pts',(31.1861426211016,-54.3969835118376,
39.9671857458165));
#199964=CARTESIAN_POINT('Ctrl Pts',(31.1067982185534,-54.5146464769138,
39.8576902534424));
#199965=CARTESIAN_POINT('Ctrl Pts',(31.2174884860864,-54.4512761425983,
39.8573998014387));
#199966=CARTESIAN_POINT('Ctrl Pts',(31.1634057161439,-54.3576020372439,
39.92499));
#199967=CARTESIAN_POINT('Origin',(31.410023123206,-54.4342359163064,40.22725));
#199968=CARTESIAN_POINT('Origin',(-0.274963065701554,-0.158749999999999,
39.116));
#199969=CARTESIAN_POINT('Origin',(29.7268821954849,-52.1234703131947,39.116));
#199970=CARTESIAN_POINT('Origin',(5.5822321212813E-15,5.8376831605261E-15,
40.22725));
#199971=CARTESIAN_POINT('Origin',(31.4364195775134,-54.4189959163064,40.22725));
#199972=CARTESIAN_POINT('Ctrl Pts',(29.7268821954848,-52.1234703131947,
38.989));
#199973=CARTESIAN_POINT('Ctrl Pts',(29.8370321846012,-52.0598751873271,
38.989));
#199974=CARTESIAN_POINT('Ctrl Pts',(29.8368672985391,-52.0599703843395,
39.1161901092324));
#199975=CARTESIAN_POINT('Ctrl Pts',(29.6185926664433,-51.9354481180161,
38.989));
#199976=CARTESIAN_POINT('Ctrl Pts',(29.7286387544941,-51.8721332875975,
38.9892298989718));
#199977=CARTESIAN_POINT('Ctrl Pts',(29.7501084152006,-51.909699589875,39.1161900493186));
#199978=CARTESIAN_POINT('Ctrl Pts',(29.5155047636238,-51.7564527430626,
39.1034966344367));
#199979=CARTESIAN_POINT('Ctrl Pts',(29.6254243098799,-51.6933616226663,
39.1038314102593));
#199980=CARTESIAN_POINT('Ctrl Pts',(29.6675155901163,-51.7666446199937,
39.2077528789613));
#199981=CARTESIAN_POINT('Ctrl Pts',(29.4581217525673,-51.6568155675428,
39.2875012672119));
#199982=CARTESIAN_POINT('Ctrl Pts',(29.5680161811093,-51.5939283753694,
39.2878045257868));
#199983=CARTESIAN_POINT('Ctrl Pts',(29.6215404737381,-51.6870133822663,
39.35490152959));
#199984=CARTESIAN_POINT('Origin',(29.5114749418004,-51.7503740054944,39.3548010137695));
#199985=CARTESIAN_POINT('Ctrl Pts',(31.6576696180583,-54.1966007261208,
39.8576902534424));
#199986=CARTESIAN_POINT('Ctrl Pts',(31.5474441649283,-54.2607761425983,
39.8573998014387));
#199987=CARTESIAN_POINT('Ctrl Pts',(31.4933613949858,-54.1671020372439,
39.92499));
#199988=CARTESIAN_POINT('Ctrl Pts',(31.6804173065997,-54.236001854427,39.9304984902492));
#199989=CARTESIAN_POINT('Ctrl Pts',(31.5756301844092,-54.2789150989588,
39.9052171569805));
#199990=CARTESIAN_POINT('Ctrl Pts',(31.5161086602375,-54.2065014563931,
39.9672049726609));
#199991=CARTESIAN_POINT('Ctrl Pts',(31.6804328064621,-54.2894509908545,
40.004343767866));
#199992=CARTESIAN_POINT('Ctrl Pts',(31.5911964272957,-54.3138841827105,
39.9661628577643));
#199993=CARTESIAN_POINT('Ctrl Pts',(31.5258675551963,-54.2543268901839,
40.0100243556238));
#199994=CARTESIAN_POINT('Ctrl Pts',(31.6250591602192,-54.4049648787499,
40.1194874821989));
#199995=CARTESIAN_POINT('Ctrl Pts',(31.5671393481785,-54.397608888651,40.062755148314));
#199996=CARTESIAN_POINT('Ctrl Pts',(31.5090508246496,-54.3475791360314,
40.0767884282374));
#199997=CARTESIAN_POINT('Ctrl Pts',(31.5668453499337,-54.4680334478297,
40.1599502015398));
#199998=CARTESIAN_POINT('Ctrl Pts',(31.5274226111431,-54.4477213412894,
40.1002449453872));
#199999=CARTESIAN_POINT('Ctrl Pts',(31.4807263372353,-54.3933906465337,
40.10025));
#200000=CARTESIAN_POINT('Ctrl Pts',(31.4902932482907,-54.5122556166611,
40.1599502534424));
#200001=CARTESIAN_POINT('Ctrl Pts',(31.4716329851988,-54.479953185448,40.10025));
#200002=CARTESIAN_POINT('Ctrl Pts',(31.4364195775134,-54.4189959163064,
40.10025));
#200003=CARTESIAN_POINT('Origin',(31.6033466212664,-54.1036020372439,39.92499));
#200004=CARTESIAN_POINT('Origin',(29.4224002636353,-51.5960921371865,39.6398955069314));
#200005=CARTESIAN_POINT('Origin',(29.3333255853454,-51.4418102687786,39.92499));
#200006=CARTESIAN_POINT('Origin',(31.5142720655984,-53.9493203812121,39.6398955068274));
#200007=CARTESIAN_POINT('Origin',(31.4251975098792,-53.795038724998,39.3548010137695));
#200008=CARTESIAN_POINT('Ctrl Pts',(29.2799753962461,-51.3482501200166,
39.8576902534424));
#200009=CARTESIAN_POINT('Ctrl Pts',(29.3897042746973,-51.2854610232002,
39.8579948730703));
#200010=CARTESIAN_POINT('Ctrl Pts',(29.443310811626,-51.3783102687785,39.92499));
#200011=CARTESIAN_POINT('Ctrl Pts',(29.2572578385502,-51.3089010921302,
39.9304020711229));
#200012=CARTESIAN_POINT('Ctrl Pts',(29.3615397594609,-51.2670685993237,
39.9058915297382));
#200013=CARTESIAN_POINT('Ctrl Pts',(29.4205918519434,-51.3389598763132,
39.9671523786028));
#200014=CARTESIAN_POINT('Ctrl Pts',(29.2572680623749,-51.2557407616056,
40.0043257306695));
#200015=CARTESIAN_POINT('Ctrl Pts',(29.3461554108688,-51.2319924817688,
39.9667894847835));
#200016=CARTESIAN_POINT('Ctrl Pts',(29.4109522357567,-51.2913733902315,
40.0100138975202));
#200017=CARTESIAN_POINT('Ctrl Pts',(29.3127910737013,-51.1410333861057,
40.1195533054855));
#200018=CARTESIAN_POINT('Ctrl Pts',(29.3705286780144,-51.1485922293424,
40.0630813209237));
#200019=CARTESIAN_POINT('Ctrl Pts',(29.4282055900901,-51.1987619028146,
40.0768265942419));
#200020=CARTESIAN_POINT('Ctrl Pts',(29.3710651187649,-51.0785202710263,
40.1599502027508));
#200021=CARTESIAN_POINT('Ctrl Pts',(29.410360538257,-51.0989122516717,40.1002552791554));
#200022=CARTESIAN_POINT('Ctrl Pts',(29.4568175306717,-51.1533747228777,
40.10025));
#200023=CARTESIAN_POINT('Ctrl Pts',(29.4472515437734,-51.0345602039887,
40.1599502534424));
#200024=CARTESIAN_POINT('Ctrl Pts',(29.4658956314766,-51.0668719738978,
40.10025));
#200025=CARTESIAN_POINT('Ctrl Pts',(29.501078514911,-51.1278468659048,40.10025));
#200026=CARTESIAN_POINT('Origin',(29.501078514911,-51.1278468659048,40.22725));
#200027=CARTESIAN_POINT('Ctrl Pts',(31.2097904767605,-53.4219427993287,
38.989));
#200028=CARTESIAN_POINT('Ctrl Pts',(31.0996409281621,-53.4855376708631,
38.989));
#200029=CARTESIAN_POINT('Ctrl Pts',(31.0998053730487,-53.4854427285636,
39.1161896013271));
#200030=CARTESIAN_POINT('Ctrl Pts',(31.3184716867874,-53.609738797656,38.989));
#200031=CARTESIAN_POINT('Ctrl Pts',(31.2082219299917,-53.6736064794771,
38.988776927543));
#200032=CARTESIAN_POINT('Ctrl Pts',(31.1865640704867,-53.6357132000289,
39.1161898821828));
#200033=CARTESIAN_POINT('Ctrl Pts',(31.4219325588463,-53.7885186806134,
39.1034967087243));
#200034=CARTESIAN_POINT('Ctrl Pts',(31.3115622968597,-53.8525981958206,
39.1031720232726));
#200035=CARTESIAN_POINT('Ctrl Pts',(31.269156856333,-53.7787681009861,39.2077529615015));
#200036=CARTESIAN_POINT('Ctrl Pts',(31.4795232016789,-53.8880358395971,
39.2875012672119));
#200037=CARTESIAN_POINT('Ctrl Pts',(31.369131339626,-53.9523112232409,39.2872087095507));
#200038=CARTESIAN_POINT('Ctrl Pts',(31.3151318380581,-53.8583991049518,
39.354901704823));
#200039=CARTESIAN_POINT('Origin',(31.2097904767605,-53.4219427993287,39.116));
#200040=CARTESIAN_POINT('Origin',(5.69400554112516E-15,5.20190922851043E-15,
40.22725));
#200041=CARTESIAN_POINT('Origin',(29.5274749692184,-51.1126068659048,40.22725));
#200042=CARTESIAN_POINT('Origin',(15.8305769983922,-26.7843636743467,39.116));
#200043=CARTESIAN_POINT('Origin',(31.0091584503693,-53.0743345559677,39.1160373285256));
#200044=CARTESIAN_POINT('Ctrl Pts',(29.4735998357337,-51.0193480105328,
40.1599502534424));
#200045=CARTESIAN_POINT('Ctrl Pts',(29.4922606054645,-51.0516501490687,
40.10025));
#200046=CARTESIAN_POINT('Ctrl Pts',(29.5274749692184,-51.1126068659048,
40.10025));
#200047=CARTESIAN_POINT('Ctrl Pts',(29.5495039426969,-50.9754987628534,
40.1599500566039));
#200048=CARTESIAN_POINT('Ctrl Pts',(29.5475581014577,-51.019701383452,40.1002551305372));
#200049=CARTESIAN_POINT('Ctrl Pts',(29.5715624157998,-51.0871269269751,
40.10025));
#200050=CARTESIAN_POINT('Ctrl Pts',(29.6319914129672,-50.956202990229,40.1203070619044));
#200051=CARTESIAN_POINT('Ctrl Pts',(29.6100038038528,-51.0098791271087,
40.0637098684496));
#200052=CARTESIAN_POINT('Ctrl Pts',(29.6246193648995,-51.0848223701583,
40.077263621336));
#200053=CARTESIAN_POINT('Ctrl Pts',(29.7600395375189,-50.9652607924604,
40.0046102245804));
#200054=CARTESIAN_POINT('Ctrl Pts',(29.6951164119093,-51.0303675504162,
39.9670001894015));
#200055=CARTESIAN_POINT('Ctrl Pts',(29.7140610042231,-51.1161687394138,
40.0101788811211));
#200056=CARTESIAN_POINT('Ctrl Pts',(29.8061925581062,-50.9919958361061,
39.9303710930185));
#200057=CARTESIAN_POINT('Ctrl Pts',(29.7178148857788,-51.0613912713643,
39.9058663574108));
#200058=CARTESIAN_POINT('Ctrl Pts',(29.7505571803536,-51.1484765898558,
39.9671344706362));
#200059=CARTESIAN_POINT('Ctrl Pts',(29.8289013456884,-51.0313275753409,
39.8576902534424));
#200060=CARTESIAN_POINT('Ctrl Pts',(29.7196599535391,-51.0949610232002,
39.8579948730703));
#200061=CARTESIAN_POINT('Ctrl Pts',(29.7732664904679,-51.1878102687786,
39.92499));
#200062=CARTESIAN_POINT('Origin',(29.8832517167485,-51.1243102687785,39.92499));
#200063=CARTESIAN_POINT('Origin',(30.9870007553618,-53.0360596824716,39.1925554488848));
#200064=CARTESIAN_POINT('Origin',(30.9460815882867,-52.9651856060847,39.3343017080178));
#200065=CARTESIAN_POINT('Origin',(29.9723263949823,-51.2785921372022,39.6398955069223));
#200066=CARTESIAN_POINT('Origin',(30.0614010732035,-51.4328740054944,39.3548010137695));
#200067=CARTESIAN_POINT('Ctrl Pts',(30.7811015270742,-52.6794317578288,
39.3978017080178));
#200068=CARTESIAN_POINT('Ctrl Pts',(30.6711163007936,-52.7429317578288,
39.3978017080178));
#200069=CARTESIAN_POINT('Ctrl Pts',(30.6711163007936,-52.7429317578288,
39.5248017080178));
#200070=CARTESIAN_POINT('Ctrl Pts',(30.8259039490945,-52.7575002129179,
39.3978017080178));
#200071=CARTESIAN_POINT('Ctrl Pts',(30.7160792752579,-52.820809914058,39.3980355775196));
#200072=CARTESIAN_POINT('Ctrl Pts',(30.7386233329129,-52.8598573673276,
39.5248015517192));
#200073=CARTESIAN_POINT('Ctrl Pts',(30.8682695960185,-52.8313189037786,
39.3484893995498));
#200074=CARTESIAN_POINT('Ctrl Pts',(30.7588072175367,-52.8948168809884,
39.3489438303406));
#200075=CARTESIAN_POINT('Ctrl Pts',(30.8024560343124,-52.9704188493359,
39.4508333155592));
#200076=CARTESIAN_POINT('Ctrl Pts',(30.8905967158735,-52.8702215132217,
39.2708017080178));
#200077=CARTESIAN_POINT('Ctrl Pts',(30.7813498801531,-52.9338619179796,
39.2710850691866));
#200078=CARTESIAN_POINT('Ctrl Pts',(30.8360963620061,-53.0286856060847,
39.3343017080178));
#200079=CARTESIAN_POINT('Origin',(30.7811015270742,-52.6794317578288,39.5248017080178));
#200080=CARTESIAN_POINT('Ctrl Pts',(30.0070536838157,-51.3398895692698,
39.2875012672119));
#200081=CARTESIAN_POINT('Ctrl Pts',(29.8976445761572,-51.4036173326914,
39.2878045257519));
#200082=CARTESIAN_POINT('Ctrl Pts',(29.9514963916954,-51.4965132298826,
39.354901521835));
#200083=CARTESIAN_POINT('Ctrl Pts',(30.0646513737714,-51.4394048060578,
39.1034938540228));
#200084=CARTESIAN_POINT('Ctrl Pts',(29.9550530981044,-51.5030523579581,
39.1038286278815));
#200085=CARTESIAN_POINT('Ctrl Pts',(29.9974722043256,-51.576145673001,39.2077506434039));
#200086=CARTESIAN_POINT('Ctrl Pts',(30.1681227811155,-51.6181806476923,
38.989));
#200087=CARTESIAN_POINT('Ctrl Pts',(30.0582674911768,-51.6818259279801,
38.9892298954593));
#200088=CARTESIAN_POINT('Ctrl Pts',(30.0800656843532,-51.7192017762879,
39.1161900347276));
#200089=CARTESIAN_POINT('Ctrl Pts',(30.276808326888,-51.8059703131947,38.989));
#200090=CARTESIAN_POINT('Ctrl Pts',(30.166658350493,-51.8695654317175,38.989));
#200091=CARTESIAN_POINT('Ctrl Pts',(30.1668232238147,-51.8694702420609,
39.116190094565));
#200092=CARTESIAN_POINT('Origin',(30.276808326888,-51.8059703131947,39.116));
#200093=CARTESIAN_POINT('Origin',(15.4537755657014,-26.1317244485615,39.5248017080178));
#200094=CARTESIAN_POINT('Origin',(30.7054974692368,-52.548481688396,39.5248017080178));
#200095=CARTESIAN_POINT('Origin',(15.3947701216591,-26.0295240215571,39.116));
#200096=CARTESIAN_POINT('Origin',(30.4775331296737,-52.1535342613181,39.1160402713845));
#200097=CARTESIAN_POINT('Ctrl Pts',(30.5960088312567,-52.3576880233163,
39.2708017080178));
#200098=CARTESIAN_POINT('Ctrl Pts',(30.4857749404419,-52.4219111049557,
39.27051194648));
#200099=CARTESIAN_POINT('Ctrl Pts',(30.4305321463775,-52.3262277788842,
39.3343017080178));
#200100=CARTESIAN_POINT('Ctrl Pts',(30.6184089696605,-52.3967235457366,
39.3487519301185));
#200101=CARTESIAN_POINT('Ctrl Pts',(30.5081585269353,-52.4606806140183,
39.348287946398));
#200102=CARTESIAN_POINT('Ctrl Pts',(30.4642861617686,-52.3846914485009,
39.4512271261629));
#200103=CARTESIAN_POINT('Ctrl Pts',(30.6608464521624,-52.4706758922784,
39.3978017080178));
#200104=CARTESIAN_POINT('Ctrl Pts',(30.5506153465204,-52.5342179826664,
39.3975673827401));
#200105=CARTESIAN_POINT('Ctrl Pts',(30.5282325936734,-52.4954499175227,
39.5248015355194));
#200106=CARTESIAN_POINT('Ctrl Pts',(30.7054974692368,-52.548481688396,39.3978017080178));
#200107=CARTESIAN_POINT('Ctrl Pts',(30.5955122429562,-52.611981688396,39.3978017080178));
#200108=CARTESIAN_POINT('Ctrl Pts',(30.5955122429562,-52.611981688396,39.5248017080178));
#200109=CARTESIAN_POINT('Origin',(30.5405173726582,-52.2627277788842,39.3343017080178));
#200110=CARTESIAN_POINT('Origin',(30.4998422394562,-52.1922763809696,39.1934008533555));
#200111=CARTESIAN_POINT('Origin',(24.6933715417282,-56.2428239377257,39.1925554495077));
#200112=CARTESIAN_POINT('Origin',(24.7113125977915,-56.2832472948485,39.1160373285247));
#200113=CARTESIAN_POINT('Origin',(24.660084891711,-56.1680608984279,39.3343017080178));
#200114=CARTESIAN_POINT('Ctrl Pts',(24.6158705164593,-56.0673542004326,
39.2708017080178));
#200115=CARTESIAN_POINT('Ctrl Pts',(24.7315703643334,-56.0163785451198,
39.2710850691866));
#200116=CARTESIAN_POINT('Ctrl Pts',(24.7761051648316,-56.1164053447572,
39.3343017080178));
#200117=CARTESIAN_POINT('Ctrl Pts',(24.5974591883334,-56.0262864882904,
39.3487519293518));
#200118=CARTESIAN_POINT('Ctrl Pts',(24.7131705636691,-55.9750519161932,
39.3492068662935));
#200119=CARTESIAN_POINT('Ctrl Pts',(24.748647185237,-56.0547337128505,39.4512271248753));
#200120=CARTESIAN_POINT('Ctrl Pts',(24.5625784858799,-55.9484840819673,
39.3978017080178));
#200121=CARTESIAN_POINT('Ctrl Pts',(24.6783511906875,-55.8968463240328,
39.3980347781164));
#200122=CARTESIAN_POINT('Ctrl Pts',(24.6966284839296,-55.9378977967835,
39.5248015355176));
#200123=CARTESIAN_POINT('Ctrl Pts',(24.525878019167,-55.8666273273833,39.3978017080178));
#200124=CARTESIAN_POINT('Ctrl Pts',(24.6418982922876,-55.8149717737127,
39.3978017080178));
#200125=CARTESIAN_POINT('Ctrl Pts',(24.6418982922876,-55.8149717737127,
39.5248017080178));
#200126=CARTESIAN_POINT('Origin',(24.525878019167,-55.8666273273833,39.5248017080178));
#200127=CARTESIAN_POINT('Origin',(-0.290050682801521,-0.129138884176566,
39.116));
#200128=CARTESIAN_POINT('Origin',(24.8746050278051,-56.6498810128382,39.116));
#200129=CARTESIAN_POINT('Origin',(-0.29005068280152,-0.129138884176566,
39.5248017080178));
#200130=CARTESIAN_POINT('Origin',(24.4643761377916,-55.7284918401499,39.5248017080178));
#200131=CARTESIAN_POINT('Ctrl Pts',(25.0931373005745,-57.1420619865022,
39.2875012672119));
#200132=CARTESIAN_POINT('Ctrl Pts',(25.210023876658,-57.090533221101,39.287208709576));
#200133=CARTESIAN_POINT('Ctrl Pts',(25.1657875015263,-56.9916465525422,
39.3549016990123));
#200134=CARTESIAN_POINT('Ctrl Pts',(25.0464764504219,-57.0369738651805,
39.103493917393));
#200135=CARTESIAN_POINT('Ctrl Pts',(25.1631918674162,-56.9853474458573,
39.1031692336327));
#200136=CARTESIAN_POINT('Ctrl Pts',(25.1283875141308,-56.9076448051896,
39.207750720231));
#200137=CARTESIAN_POINT('Ctrl Pts',(24.9626525995183,-56.8481865914868,
38.989));
#200138=CARTESIAN_POINT('Ctrl Pts',(25.0791258042758,-56.7965331449343,
38.9887769311182));
#200139=CARTESIAN_POINT('Ctrl Pts',(25.0611999573799,-56.7567390814041,
39.1161898712898));
#200140=CARTESIAN_POINT('Ctrl Pts',(24.8746050278051,-56.6498810128382,
38.989));
#200141=CARTESIAN_POINT('Ctrl Pts',(24.9907986298338,-56.5981482881658,
38.989));
#200142=CARTESIAN_POINT('Ctrl Pts',(24.9906251716464,-56.5982255167265,
39.1161895903855));
#200143=CARTESIAN_POINT('Origin',(25.0498328948964,-57.0434492461379,39.3548010137695));
#200144=CARTESIAN_POINT('Ctrl Pts',(24.4643761377916,-55.7284918401499,
39.3978017080178));
#200145=CARTESIAN_POINT('Ctrl Pts',(24.5803964109122,-55.6768362864792,
39.3978017080178));
#200146=CARTESIAN_POINT('Ctrl Pts',(24.5803964109122,-55.6768362864792,
39.5248017080178));
#200147=CARTESIAN_POINT('Ctrl Pts',(24.4275510972985,-55.6463586582051,
39.3978017080178));
#200148=CARTESIAN_POINT('Ctrl Pts',(24.5437506299576,-55.594528514849,39.3975666025031));
#200149=CARTESIAN_POINT('Ctrl Pts',(24.5254812387363,-55.5534947903269,
39.5248015517182));
#200150=CARTESIAN_POINT('Ctrl Pts',(24.3927285408595,-55.568696257641,39.3484894016716));
#200151=CARTESIAN_POINT('Ctrl Pts',(24.509275152962,-55.5170953257179,39.3480259000031));
#200152=CARTESIAN_POINT('Ctrl Pts',(24.473555028187,-55.4368666119038,39.4508333188948));
#200153=CARTESIAN_POINT('Ctrl Pts',(24.3743766270213,-55.5277679687683,
39.2708017080178));
#200154=CARTESIAN_POINT('Ctrl Pts',(24.4911280468225,-55.4763362579875,
39.27051194648));
#200155=CARTESIAN_POINT('Ctrl Pts',(24.4461895095988,-55.3754026508175,
39.3343017080178));
#200156=CARTESIAN_POINT('Origin',(24.3301692364782,-55.4270582044882,39.3343017080178));
#200157=CARTESIAN_POINT('Origin',(25.1222926664938,-57.2061965577167,39.6398955068181));
#200158=CARTESIAN_POINT('Origin',(25.1947524379615,-57.3689438691197,39.92499));
#200159=CARTESIAN_POINT('Origin',(24.2970811015499,-55.3527410366444,39.1934008539951));
#200160=CARTESIAN_POINT('Origin',(24.2788510342446,-55.3119205422646,39.1160402713846));
#200161=CARTESIAN_POINT('Ctrl Pts',(25.5918112338793,-57.5176823163889,
40.1599502534424));
#200162=CARTESIAN_POINT('Ctrl Pts',(25.5766462455175,-57.4835989537478,
40.10025));
#200163=CARTESIAN_POINT('Ctrl Pts',(25.5480287005717,-57.419280924679,40.10025));
#200164=CARTESIAN_POINT('Ctrl Pts',(25.5113050800558,-57.5535024391256,
40.1599500538468));
#200165=CARTESIAN_POINT('Ctrl Pts',(25.518003150502,-57.5096879712785,40.1002448353481));
#200166=CARTESIAN_POINT('Ctrl Pts',(25.5014249500148,-57.4400067642829,
40.10025));
#200167=CARTESIAN_POINT('Ctrl Pts',(25.4268488592815,-57.5636994104961,
40.1202442001038));
#200168=CARTESIAN_POINT('Ctrl Pts',(25.4545932086373,-57.5125855880057,
40.0633873868015));
#200169=CARTESIAN_POINT('Ctrl Pts',(25.4482497003382,-57.4362769714772,
40.0772271723536));
#200170=CARTESIAN_POINT('Ctrl Pts',(25.2998561687915,-57.5406963524571,
40.0045995998163));
#200171=CARTESIAN_POINT('Ctrl Pts',(25.371995687077,-57.4828507843371,39.9663485808318));
#200172=CARTESIAN_POINT('Ctrl Pts',(25.3622939683648,-57.3950038423346,
40.0101727202467));
#200173=CARTESIAN_POINT('Ctrl Pts',(25.2565567136857,-57.5090991591923,
39.9304654349858));
#200174=CARTESIAN_POINT('Ctrl Pts',(25.3528760603499,-57.4495482434202,
39.9051900162955));
#200175=CARTESIAN_POINT('Ctrl Pts',(25.3292685758747,-57.3588307079383,
39.9671857458176));
#200176=CARTESIAN_POINT('Ctrl Pts',(25.2380597013429,-57.4675553545141,
39.8576902534424));
#200177=CARTESIAN_POINT('Ctrl Pts',(25.3547675996714,-57.4161024530844,
39.8573998014387));
#200178=CARTESIAN_POINT('Ctrl Pts',(25.3107727110821,-57.317288315449,39.92499));
#200179=CARTESIAN_POINT('Origin',(25.5480287005717,-57.419280924679,40.22725));
#200180=CARTESIAN_POINT('Origin',(-0.290050682801521,-0.129138884176566,
39.116));
#200181=CARTESIAN_POINT('Origin',(24.1156489724276,-54.9452378026829,39.116));
#200182=CARTESIAN_POINT('Origin',(5.59761027822878E-15,5.84551872285717E-15,
40.22725));
#200183=CARTESIAN_POINT('Origin',(25.5758735661207,-57.406883591798,40.22725));
#200184=CARTESIAN_POINT('Ctrl Pts',(24.1156489724276,-54.9452378026829,
38.989));
#200185=CARTESIAN_POINT('Ctrl Pts',(24.2318430491565,-54.8935048666603,
38.989));
#200186=CARTESIAN_POINT('Ctrl Pts',(24.2316691155602,-54.8935823068866,
39.1161901092323));
#200187=CARTESIAN_POINT('Ctrl Pts',(24.0276063358807,-54.7469262747032,
38.989));
#200188=CARTESIAN_POINT('Ctrl Pts',(24.1436677818728,-54.6954612380236,
38.9892298989724));
#200189=CARTESIAN_POINT('Ctrl Pts',(24.1610930816817,-54.7350659388072,
39.1161900493185));
#200190=CARTESIAN_POINT('Ctrl Pts',(23.9437932708506,-54.5581358350809,
39.1034966344368));
#200191=CARTESIAN_POINT('Ctrl Pts',(24.0597054841937,-54.5068800556947,
39.1038314102585));
#200192=CARTESIAN_POINT('Ctrl Pts',(24.0939060248995,-54.5841613379358,
39.2077528789612));
#200193=CARTESIAN_POINT('Ctrl Pts',(23.8971395307767,-54.4530463244693,
39.2875012672119));
#200194=CARTESIAN_POINT('Ctrl Pts',(24.0130054476977,-54.4019907306519,
39.2878045257868));
#200195=CARTESIAN_POINT('Ctrl Pts',(24.056506495927,-54.5001606201971,39.35490152959));
#200196=CARTESIAN_POINT('Origin',(23.940420925912,-54.5516691663895,39.3548010137695));
#200197=CARTESIAN_POINT('Ctrl Pts',(25.8191582032619,-57.2088336324699,
39.8576902534424));
#200198=CARTESIAN_POINT('Ctrl Pts',(25.7028284190332,-57.2611357920725,
39.8573998014387));
#200199=CARTESIAN_POINT('Ctrl Pts',(25.658833530444,-57.1623216544372,39.92499));
#200200=CARTESIAN_POINT('Ctrl Pts',(25.8376627381929,-57.2503966981986,
39.9304984902491));
#200201=CARTESIAN_POINT('Ctrl Pts',(25.7289639953175,-57.2821216226331,
39.9052171569798));
#200202=CARTESIAN_POINT('Ctrl Pts',(25.6773378230594,-57.2038829761266,
39.9672049726603));
#200203=CARTESIAN_POINT('Ctrl Pts',(25.8320911970517,-57.3035546548412,
40.0043437678662));
#200204=CARTESIAN_POINT('Ctrl Pts',(25.7407897001106,-57.3185262575349,
39.9661628577643));
#200205=CARTESIAN_POINT('Ctrl Pts',(25.6820441386715,-57.25246649948,40.0100243556235));
#200206=CARTESIAN_POINT('Ctrl Pts',(25.7649464042482,-57.4126476234251,
40.1194874821987));
#200207=CARTESIAN_POINT('Ctrl Pts',(25.7081127933384,-57.3992776612634,
40.062755148314));
#200208=CARTESIAN_POINT('Ctrl Pts',(25.6555720179789,-57.343450072766,40.0767884282377));
#200209=CARTESIAN_POINT('Ctrl Pts',(25.7004590347003,-57.4692856961534,
40.1599502015384));
#200210=CARTESIAN_POINT('Ctrl Pts',(25.663375451079,-57.4449640631517,40.1002449453881));
#200211=CARTESIAN_POINT('Ctrl Pts',(25.622614088277,-57.3860499078761,40.10025));
#200212=CARTESIAN_POINT('Ctrl Pts',(25.6197038181297,-57.5052637377733,
40.1599502534424));
#200213=CARTESIAN_POINT('Ctrl Pts',(25.604522301406,-57.471187734033,40.10025));
#200214=CARTESIAN_POINT('Ctrl Pts',(25.5758735661207,-57.406883591798,40.10025));
#200215=CARTESIAN_POINT('Origin',(25.7748538035646,-57.1106661007665,39.92499));
#200216=CARTESIAN_POINT('Origin',(23.8679610547593,-54.3889216310736,39.6398955069312));
#200217=CARTESIAN_POINT('Origin',(23.7955011834907,-54.2261740956467,39.92499));
#200218=CARTESIAN_POINT('Origin',(25.7023940320485,-56.9479187893674,39.6398955068282));
#200219=CARTESIAN_POINT('Origin',(25.6299342604994,-56.7851714777848,39.3548010137695));
#200220=CARTESIAN_POINT('Ctrl Pts',(23.7522229508827,-54.1275498658874,
39.8576902534424));
#200221=CARTESIAN_POINT('Ctrl Pts',(23.8679139708567,-54.0765745253536,
39.8579948730703));
#200222=CARTESIAN_POINT('Ctrl Pts',(23.9115214566113,-54.174518541976,39.92499));
#200223=CARTESIAN_POINT('Ctrl Pts',(23.7337429357606,-54.0860417646979,
39.9304020711229));
#200224=CARTESIAN_POINT('Ctrl Pts',(23.8418262755855,-54.0553388636016,
39.9058915297373));
#200225=CARTESIAN_POINT('Ctrl Pts',(23.8930401898204,-54.1330089371351,
39.9671523786029));
#200226=CARTESIAN_POINT('Ctrl Pts',(23.7393098712348,-54.0331737207068,
40.0043257306695));
#200227=CARTESIAN_POINT('Ctrl Pts',(23.8301926567299,-54.0188467943736,
39.9667894847838));
#200228=CARTESIAN_POINT('Ctrl Pts',(23.8884275227222,-54.0846755205371,
40.0100138975201));
#200229=CARTESIAN_POINT('Ctrl Pts',(23.8065189073823,-53.9248984592618,
40.1195533054855));
#200230=CARTESIAN_POINT('Ctrl Pts',(23.86315010479,-53.9384511174162,40.0630813209233));
#200231=CARTESIAN_POINT('Ctrl Pts',(23.9152668978359,-53.9943748351526,
40.076826594242));
#200232=CARTESIAN_POINT('Ctrl Pts',(23.8710081209825,-53.8688190939457,
40.1599502027523));
#200233=CARTESIAN_POINT('Ctrl Pts',(23.9079567336543,-53.8932068549978,
40.1002552791544));
#200234=CARTESIAN_POINT('Ctrl Pts',(23.9484663513833,-53.952227053115,40.10025));
#200235=CARTESIAN_POINT('Ctrl Pts',(23.9513722670364,-53.8330634946838,
40.1599502534424));
#200236=CARTESIAN_POINT('Ctrl Pts',(23.9665367208223,-53.8671470951731,
40.10025));
#200237=CARTESIAN_POINT('Ctrl Pts',(23.9951532569806,-53.9314655730805,
40.10025));
#200238=CARTESIAN_POINT('Origin',(23.9951532569806,-53.9314655730805,40.22725));
#200239=CARTESIAN_POINT('Ctrl Pts',(25.4547063934082,-56.3916032444851,
38.989));
#200240=CARTESIAN_POINT('Ctrl Pts',(25.3385127813692,-56.4433359736145,
38.989));
#200241=CARTESIAN_POINT('Ctrl Pts',(25.3386862495819,-56.4432587405902,
39.1161896013269));
#200242=CARTESIAN_POINT('Ctrl Pts',(25.5431622092827,-56.5897307565541,
38.989));
#200243=CARTESIAN_POINT('Ctrl Pts',(25.4268404215568,-56.6417243268789,
38.9887769275436));
#200244=CARTESIAN_POINT('Ctrl Pts',(25.4092621323414,-56.601774768009,39.1161898821826));
#200245=CARTESIAN_POINT('Ctrl Pts',(25.6273687254298,-56.7783458705714,
39.1034967087243));
#200246=CARTESIAN_POINT('Ctrl Pts',(25.5109049500366,-56.830537517612,39.1031720232724));
#200247=CARTESIAN_POINT('Ctrl Pts',(25.4764491573041,-56.7526792962301,
39.2077529615017));
#200248=CARTESIAN_POINT('Ctrl Pts',(25.6742415049979,-56.8833377255395,
39.2875012672119));
#200249=CARTESIAN_POINT('Ctrl Pts',(25.5577357740377,-56.9357219102088,
39.2872087095508));
#200250=CARTESIAN_POINT('Ctrl Pts',(25.5138485767964,-56.8366797674139,
39.3549017048229));
#200251=CARTESIAN_POINT('Origin',(25.4547063934082,-56.3916032444851,39.116));
#200252=CARTESIAN_POINT('Origin',(5.68853496937358E-15,5.19912183297972E-15,
40.22725));
#200253=CARTESIAN_POINT('Origin',(24.0229981225296,-53.9190682401995,40.22725));
#200254=CARTESIAN_POINT('Origin',(10.5838037820516,-22.9910091182297,39.116));
#200255=CARTESIAN_POINT('Origin',(25.2915084057492,-56.0249274780511,39.1160373285268));
#200256=CARTESIAN_POINT('Ctrl Pts',(23.9791663275012,-53.8206887816837,
40.1599502534424));
#200257=CARTESIAN_POINT('Ctrl Pts',(23.9943483786816,-53.8547645473081,
40.10025));
#200258=CARTESIAN_POINT('Ctrl Pts',(24.0229981225296,-53.9190682401995,
40.10025));
#200259=CARTESIAN_POINT('Ctrl Pts',(24.0592381183001,-53.7850138844278,
40.1599500566035));
#200260=CARTESIAN_POINT('Ctrl Pts',(24.0526825045793,-53.8287709626516,
40.1002551305357));
#200261=CARTESIAN_POINT('Ctrl Pts',(24.0695074323267,-53.8983362760826,
40.10025));
#200262=CARTESIAN_POINT('Ctrl Pts',(24.1432906710371,-53.7744461045708,
40.1203070619045));
#200263=CARTESIAN_POINT('Ctrl Pts',(24.1158128282441,-53.8255298669645,
40.0637098684499));
#200264=CARTESIAN_POINT('Ctrl Pts',(24.1225146216897,-53.901590305224,40.0772636213363));
#200265=CARTESIAN_POINT('Ctrl Pts',(24.2696905364172,-53.7968389608975,
40.0046102245803));
#200266=CARTESIAN_POINT('Ctrl Pts',(24.198317557125,-53.8548027426708,39.9670001894012));
#200267=CARTESIAN_POINT('Ctrl Pts',(24.2081897025475,-53.9421141528985,
40.0101788811208));
#200268=CARTESIAN_POINT('Ctrl Pts',(24.3127961529013,-53.8282518514936,
39.9303710930185));
#200269=CARTESIAN_POINT('Ctrl Pts',(24.2176488245051,-53.8880291490197,
39.9058663574099));
#200270=CARTESIAN_POINT('Ctrl Pts',(24.241108858848,-53.9780599067614,39.9671344706353));
#200271=CARTESIAN_POINT('Ctrl Pts',(24.3312692531087,-53.8697418420146,
39.8576902534424));
#200272=CARTESIAN_POINT('Ctrl Pts',(24.2159747902185,-53.9216078643418,
39.8579948730703));
#200273=CARTESIAN_POINT('Ctrl Pts',(24.2595822759732,-54.0195518809642,
39.92499));
#200274=CARTESIAN_POINT('Origin',(24.3756025490938,-53.9678963272935,39.92499));
#200275=CARTESIAN_POINT('Origin',(25.2734729066189,-55.9845461685081,39.1925554488845));
#200276=CARTESIAN_POINT('Origin',(25.2401862573141,-55.9097831300747,39.3343017080178));
#200277=CARTESIAN_POINT('Origin',(24.4480624203036,-54.1306438627315,39.6398955069225));
#200278=CARTESIAN_POINT('Origin',(24.5205222915151,-54.2933913980364,39.3548010137695));
#200279=CARTESIAN_POINT('Ctrl Pts',(25.10597938477,-55.6083495590302,39.3978017080178));
#200280=CARTESIAN_POINT('Ctrl Pts',(24.9899591116494,-55.6600051127008,
39.3978017080178));
#200281=CARTESIAN_POINT('Ctrl Pts',(24.9899591116494,-55.6600051127008,
39.5248017080178));
#200282=CARTESIAN_POINT('Ctrl Pts',(25.1423759987949,-55.6906734752781,
39.3978017080178));
#200283=CARTESIAN_POINT('Ctrl Pts',(25.0265352902399,-55.742156554866,39.3980355775168));
#200284=CARTESIAN_POINT('Ctrl Pts',(25.0448742789057,-55.7833465978035,
39.5248015517178));
#200285=CARTESIAN_POINT('Ctrl Pts',(25.1767934079551,-55.7685161955953,
39.3484893995498));
#200286=CARTESIAN_POINT('Ctrl Pts',(25.0612933298571,-55.8202243900358,
39.3489438303432));
#200287=CARTESIAN_POINT('Ctrl Pts',(25.0968004762774,-55.8999747466294,
39.4508333155604));
#200288=CARTESIAN_POINT('Ctrl Pts',(25.19493178753,-55.8095395120008,39.2708017080178));
#200289=CARTESIAN_POINT('Ctrl Pts',(25.0796311836953,-55.8614118841079,
39.2710850691866));
#200290=CARTESIAN_POINT('Ctrl Pts',(25.1241659841935,-55.9614386837454,
39.3343017080178));
#200291=CARTESIAN_POINT('Origin',(25.10597938477,-55.6083495590302,39.5248017080178));
#200292=CARTESIAN_POINT('Ctrl Pts',(24.4761921430391,-54.1952354911873,
39.2875012672119));
#200293=CARTESIAN_POINT('Ctrl Pts',(24.3607210247425,-54.2471777813617,
39.2878045257519));
#200294=CARTESIAN_POINT('Ctrl Pts',(24.4045675690228,-54.3451938326304,
39.3549015218347));
#200295=CARTESIAN_POINT('Ctrl Pts',(24.5230721320475,-54.3002261711154,
39.1034938540228));
#200296=CARTESIAN_POINT('Ctrl Pts',(24.4074212664131,-54.352068915742,39.1038286278836));
#200297=CARTESIAN_POINT('Ctrl Pts',(24.4419676644372,-54.4291958219391,
39.2077506434048));
#200298=CARTESIAN_POINT('Ctrl Pts',(24.6072895482034,-54.4888383671843,
38.989));
#200299=CARTESIAN_POINT('Ctrl Pts',(24.4913833136921,-54.5406519873231,
38.9892298954593));
#200300=CARTESIAN_POINT('Ctrl Pts',(24.5091552540986,-54.5801016184604,
39.1161900347271));
#200301=CARTESIAN_POINT('Ctrl Pts',(24.6957503380306,-54.6869600343298,
38.989));
#200302=CARTESIAN_POINT('Ctrl Pts',(24.5795562747214,-54.7386929643776,
38.989));
#200303=CARTESIAN_POINT('Ctrl Pts',(24.5797301948779,-54.738615530135,39.1161900945646));
#200304=CARTESIAN_POINT('Origin',(24.6957503380306,-54.6869600343298,39.116));
#200305=CARTESIAN_POINT('Origin',(10.3344596589366,-22.4309730483565,39.5248017080178));
#200306=CARTESIAN_POINT('Origin',(25.0444775033946,-55.4702140717967,39.5248017080178));
#200307=CARTESIAN_POINT('Origin',(10.295413467953,-22.3432738675264,39.116));
#200308=CARTESIAN_POINT('Origin',(24.8590452239601,-55.0536014459537,39.1160402713849));
#200309=CARTESIAN_POINT('Ctrl Pts',(24.9555320242414,-55.2690209153041,
39.2708017080178));
#200310=CARTESIAN_POINT('Ctrl Pts',(24.8391888661843,-55.3213695969756,
39.27051194648));
#200311=CARTESIAN_POINT('Ctrl Pts',(24.7942503289606,-55.2204359898057,
39.3343017080178));
#200312=CARTESIAN_POINT('Ctrl Pts',(24.9737291291708,-55.3101840490929,
39.3487519301186));
#200313=CARTESIAN_POINT('Ctrl Pts',(24.8573973158434,-55.3622664445116,
39.3482879463981));
#200314=CARTESIAN_POINT('Ctrl Pts',(24.8217083187823,-55.2821076446826,
39.4512271261636));
#200315=CARTESIAN_POINT('Ctrl Pts',(25.0082040095654,-55.3881672017729,
39.3978017080178));
#200316=CARTESIAN_POINT('Ctrl Pts',(24.8919348043925,-55.4398389138634,
39.3975673827397));
#200317=CARTESIAN_POINT('Ctrl Pts',(24.8737270328803,-55.398943589478,39.5248015355181));
#200318=CARTESIAN_POINT('Ctrl Pts',(25.0444775033946,-55.4702140717967,
39.3978017080178));
#200319=CARTESIAN_POINT('Ctrl Pts',(24.928457230274,-55.5218696254674,39.3978017080178));
#200320=CARTESIAN_POINT('Ctrl Pts',(24.928457230274,-55.5218696254674,39.5248017080178));
#200321=CARTESIAN_POINT('Origin',(24.9102706020812,-55.168780436135,39.3343017080178));
#200322=CARTESIAN_POINT('Origin',(24.8771824678742,-55.0944632691847,39.1934008533544));
#200323=CARTESIAN_POINT('Origin',(18.6791227126689,-58.5158800435653,39.1925554495079));
#200324=CARTESIAN_POINT('Origin',(18.6927400943506,-58.557957308327,39.1160373285241));
#200325=CARTESIAN_POINT('Origin',(18.6538332760103,-58.4380471616455,39.3343017080178));
#200326=CARTESIAN_POINT('Ctrl Pts',(18.6203878281146,-58.3332704847796,
39.2708017080178));
#200327=CARTESIAN_POINT('Ctrl Pts',(18.7407822670301,-58.2946680067388,
39.2710850691866));
#200328=CARTESIAN_POINT('Ctrl Pts',(18.7746174535798,-58.3988020033599,
39.3343017080178));
#200329=CARTESIAN_POINT('Ctrl Pts',(18.6063701040112,-58.2905032380256,
39.3487519293518));
#200330=CARTESIAN_POINT('Ctrl Pts',(18.7268030714131,-58.2516444665215,
39.3492068662938));
#200331=CARTESIAN_POINT('Ctrl Pts',(18.7537563325802,-58.3345980746926,
39.4512271248748));
#200332=CARTESIAN_POINT('Ctrl Pts',(18.579813047667,-58.2094810151997,39.3978017080178));
#200333=CARTESIAN_POINT('Ctrl Pts',(18.700349152967,-58.1702276772284,39.398034778116));
#200334=CARTESIAN_POINT('Ctrl Pts',(18.7142352739233,-58.2129647630923,
39.5248015355176));
#200335=CARTESIAN_POINT('Ctrl Pts',(18.5518699907149,-58.1242364370957,
39.3978017080178));
#200336=CARTESIAN_POINT('Ctrl Pts',(18.6726541682844,-58.0849912788101,
39.3978017080178));
#200337=CARTESIAN_POINT('Ctrl Pts',(18.6726541682844,-58.0849912788101,
39.5248017080178));
#200338=CARTESIAN_POINT('Origin',(18.5518699907149,-58.1242364370957,39.5248017080178));
#200339=CARTESIAN_POINT('Origin',(-0.301960443923706,-0.098112895714045,
39.116));
#200340=CARTESIAN_POINT('Origin',(18.8168143322225,-58.9396512752214,39.116));
#200341=CARTESIAN_POINT('Origin',(-0.301960443923706,-0.098112895714045,
39.5248017080178));
#200342=CARTESIAN_POINT('Origin',(18.505144113284,-57.9804289733664,39.5248017080178));
#200343=CARTESIAN_POINT('Ctrl Pts',(18.9827025415095,-59.4519788726608,
39.2875012672119));
#200344=CARTESIAN_POINT('Ctrl Pts',(19.1043350233607,-59.4129503614027,
39.287208709576));
#200345=CARTESIAN_POINT('Ctrl Pts',(19.0706774512227,-59.3099814440479,
39.3549016990123));
#200346=CARTESIAN_POINT('Ctrl Pts',(18.9472820042064,-59.3425890481019,
39.1034939173931));
#200347=CARTESIAN_POINT('Ctrl Pts',(19.0687544722092,-59.3034455268815,
39.1031692336348));
#200348=CARTESIAN_POINT('Ctrl Pts',(19.0422629184334,-59.2225305038466,
39.2077507202313));
#200349=CARTESIAN_POINT('Ctrl Pts',(18.8836509927318,-59.1460739925267,
38.989));
#200350=CARTESIAN_POINT('Ctrl Pts',(19.0048854004789,-59.1068782740656,
38.9887769311164));
#200351=CARTESIAN_POINT('Ctrl Pts',(18.9912173655547,-59.0654284453498,
39.1161898712898));
#200352=CARTESIAN_POINT('Ctrl Pts',(18.8168143322225,-58.9396512752214,
38.989));
#200353=CARTESIAN_POINT('Ctrl Pts',(18.9377789557524,-58.9003474864891,
38.989));
#200354=CARTESIAN_POINT('Ctrl Pts',(18.9375983752043,-58.900406160666,39.1161895903855));
#200355=CARTESIAN_POINT('Origin',(18.9499432001057,-59.349379800228,39.3548010137695));
#200356=CARTESIAN_POINT('Ctrl Pts',(18.505144113284,-57.9804289733664,39.3978017080178));
#200357=CARTESIAN_POINT('Ctrl Pts',(18.6259282908535,-57.9411838150808,
39.3978017080178));
#200358=CARTESIAN_POINT('Ctrl Pts',(18.6259282908535,-57.9411838150808,
39.5248017080178));
#200359=CARTESIAN_POINT('Ctrl Pts',(18.4771060595094,-57.894896460693,39.3978017080178));
#200360=CARTESIAN_POINT('Ctrl Pts',(18.5980867642078,-57.8554964068678,
39.3975666025021));
#200361=CARTESIAN_POINT('Ctrl Pts',(18.5842066467862,-57.8127777979909,
39.5248015517178));
#200362=CARTESIAN_POINT('Ctrl Pts',(18.4505921960617,-57.8140195545739,
39.3484894016716));
#200363=CARTESIAN_POINT('Ctrl Pts',(18.5718941197436,-57.7748837362156,
39.3480259000044));
#200364=CARTESIAN_POINT('Ctrl Pts',(18.5447558577167,-57.6913607539431,
39.4508333188947));
#200365=CARTESIAN_POINT('Ctrl Pts',(18.4366189870672,-57.7713971777987,
39.2708017080178));
#200366=CARTESIAN_POINT('Ctrl Pts',(18.5581069080659,-57.7324510618071,
39.27051194648));
#200367=CARTESIAN_POINT('Ctrl Pts',(18.5239649837007,-57.6273730232606,
39.3343017080178));
#200368=CARTESIAN_POINT('Origin',(18.4031808061312,-57.6666181815462,39.3343017080178));
#200369=CARTESIAN_POINT('Origin',(19.0049943031108,-59.5188096735779,39.6398955068193));
#200370=CARTESIAN_POINT('Origin',(19.0600454060086,-59.6882395467421,39.92499));
#200371=CARTESIAN_POINT('Origin',(18.378042190817,-57.5892494790284,39.1934008539945));
#200372=CARTESIAN_POINT('Origin',(18.3641788932754,-57.5467470426662,39.1160402713846));
#200373=CARTESIAN_POINT('Ctrl Pts',(19.4393816709755,-59.8776671349986,
40.1599502534424));
#200374=CARTESIAN_POINT('Ctrl Pts',(19.4278624395265,-59.8421853116553,
40.10025));
#200375=CARTESIAN_POINT('Ctrl Pts',(19.4061247292252,-59.7752282754837,
40.10025));
#200376=CARTESIAN_POINT('Ctrl Pts',(19.355572315902,-59.9048758468122,40.1599500538465));
#200377=CARTESIAN_POINT('Ctrl Pts',(19.3668135526099,-59.8620015382123,
40.1002448353478));
#200378=CARTESIAN_POINT('Ctrl Pts',(19.3576098387254,-59.7909691583392,
40.10025));
#200379=CARTESIAN_POINT('Ctrl Pts',(19.2705128813954,-59.9061888791355,
40.1202442001037));
#200380=CARTESIAN_POINT('Ctrl Pts',(19.3034480936187,-59.8582551377152,
40.0633873868015));
#200381=CARTESIAN_POINT('Ctrl Pts',(19.3051157581417,-59.7817014705979,
40.0772271723538));
#200382=CARTESIAN_POINT('Ctrl Pts',(19.1466203444578,-59.8700374834726,
40.0045995998164));
#200383=CARTESIAN_POINT('Ctrl Pts',(19.2244111832567,-59.8200494324147,
39.9663485808318));
#200384=CARTESIAN_POINT('Ctrl Pts',(19.2239451174251,-59.7316696194042,
40.0101727202465));
#200385=CARTESIAN_POINT('Ctrl Pts',(19.1068608943534,-59.8340873574359,
39.9304654349858));
#200386=CARTESIAN_POINT('Ctrl Pts',(19.208877359269,-59.7849307811027,39.9051900162941));
#200387=CARTESIAN_POINT('Ctrl Pts',(19.1948817636406,-59.6922425516964,
39.9671857458175));
#200388=CARTESIAN_POINT('Ctrl Pts',(19.092807720641,-59.7908376697912,39.8576902534424));
#200389=CARTESIAN_POINT('Ctrl Pts',(19.2142545736082,-59.7518659300026,
39.8573998014387));
#200390=CARTESIAN_POINT('Ctrl Pts',(19.180829583578,-59.6489943884565,39.92499));
#200391=CARTESIAN_POINT('Origin',(19.4061247292252,-59.7752282754837,40.22725));
#200392=CARTESIAN_POINT('Origin',(-0.301960443923706,-0.098112895714045,
39.116));
#200393=CARTESIAN_POINT('Origin',(18.2401996527044,-57.1650137687747,39.116));
#200394=CARTESIAN_POINT('Origin',(5.61372323131277E-15,5.85170390604432E-15,
40.22725));
#200395=CARTESIAN_POINT('Origin',(19.4351129318419,-59.7658094374952,40.22725));
#200396=CARTESIAN_POINT('Ctrl Pts',(18.2401996527044,-57.1650137687747,
38.989));
#200397=CARTESIAN_POINT('Ctrl Pts',(18.3611647704264,-57.1257098194697,
38.989));
#200398=CARTESIAN_POINT('Ctrl Pts',(18.3609836949485,-57.125768654459,39.1161901092325));
#200399=CARTESIAN_POINT('Ctrl Pts',(18.1733685221991,-56.9585856505952,
38.989));
#200400=CARTESIAN_POINT('Ctrl Pts',(18.2941737326426,-56.9195342693655,
38.9892298989742));
#200401=CARTESIAN_POINT('Ctrl Pts',(18.3073637563263,-56.9607434512653,
39.1161900493187));
#200402=CARTESIAN_POINT('Ctrl Pts',(18.1097485684451,-56.7620685738642,
39.1034966344368));
#200403=CARTESIAN_POINT('Ctrl Pts',(18.2303834904095,-56.7232097045349,
39.1038314102571));
#200404=CARTESIAN_POINT('Ctrl Pts',(18.2563185832999,-56.8036425617893,
39.2077528789613));
#200405=CARTESIAN_POINT('Ctrl Pts',(18.074335247489,-56.6526781108324,39.2875012672119));
#200406=CARTESIAN_POINT('Ctrl Pts',(18.194903201557,-56.6140134911407,39.2878045257868));
#200407=CARTESIAN_POINT('Ctrl Pts',(18.2279043987991,-56.7161926934816,
39.3549015295901));
#200408=CARTESIAN_POINT('Origin',(18.1070706485041,-56.7552848242271,39.3548010137695));
#200409=CARTESIAN_POINT('Ctrl Pts',(19.6977666881844,-59.5942745858236,
39.8576902534424));
#200410=CARTESIAN_POINT('Ctrl Pts',(19.5766071063167,-59.6341304551457,
39.8573998014387));
#200411=CARTESIAN_POINT('Ctrl Pts',(19.5431821162865,-59.5312589135996,
39.92499));
#200412=CARTESIAN_POINT('Ctrl Pts',(19.7118253299484,-59.6375442153288,
39.930498490249));
#200413=CARTESIAN_POINT('Ctrl Pts',(19.6004058925601,-59.6577332347592,
39.9052171569784));
#200414=CARTESIAN_POINT('Ctrl Pts',(19.5572406993632,-59.5745267832908,
39.9672049726602));
#200415=CARTESIAN_POINT('Ctrl Pts',(19.7007277907734,-59.6898285824899,
40.0043437678663));
#200416=CARTESIAN_POINT('Ctrl Pts',(19.6083614943636,-59.695174564008,39.9661628577646));
#200417=CARTESIAN_POINT('Ctrl Pts',(19.55684287225,-59.6233361049593,40.0100243556235));
#200418=CARTESIAN_POINT('Ctrl Pts',(19.6225475038109,-59.791305386369,40.1194874821986));
#200419=CARTESIAN_POINT('Ctrl Pts',(19.5674227749668,-59.7720679362488,
40.0627551483138));
#200420=CARTESIAN_POINT('Ctrl Pts',(19.5210053955058,-59.7110541706146,
40.0767884282377));
#200421=CARTESIAN_POINT('Ctrl Pts',(19.5524931121163,-59.8408924241702,
40.159950201539));
#200422=CARTESIAN_POINT('Ctrl Pts',(19.5181549791688,-59.8128277376124,
40.1002449453872));
#200423=CARTESIAN_POINT('Ctrl Pts',(19.4837751174925,-59.7499755976286,
40.10025));
#200424=CARTESIAN_POINT('Ctrl Pts',(19.4684195516695,-59.8682321556242,
40.1599502534424));
#200425=CARTESIAN_POINT('Ctrl Pts',(19.4568831131883,-59.8327559231846,
40.10025));
#200426=CARTESIAN_POINT('Ctrl Pts',(19.4351129318419,-59.7658094374952,
40.10025));
#200427=CARTESIAN_POINT('Origin',(19.663966293856,-59.492013755314,39.92499));
#200428=CARTESIAN_POINT('Origin',(18.0520194698745,-56.5858547179583,39.6398955069314));
#200429=CARTESIAN_POINT('Origin',(17.996968291141,-56.4164246115664,39.92499));
#200430=CARTESIAN_POINT('Origin',(19.6089151909103,-59.3225838821502,39.6398955068283));
#200431=CARTESIAN_POINT('Origin',(19.5538640879531,-59.1531540087999,39.3548010137695));
#200432=CARTESIAN_POINT('Ctrl Pts',(17.9642361803971,-56.3138168485095,
39.8576902534424));
#200433=CARTESIAN_POINT('Ctrl Pts',(18.0846218068694,-56.2752137607566,
39.8579948730703));
#200434=CARTESIAN_POINT('Ctrl Pts',(18.1177524687105,-56.3771794532808,
39.92499));
#200435=CARTESIAN_POINT('Ctrl Pts',(17.9501961787629,-56.2706044454591,
39.9304020711231));
#200436=CARTESIAN_POINT('Ctrl Pts',(18.0608967538138,-56.2513675234836,
39.9058915297377));
#200437=CARTESIAN_POINT('Ctrl Pts',(18.1037113794378,-56.3339654239822,
39.9671523786037));
#200438=CARTESIAN_POINT('Ctrl Pts',(17.9612588333756,-56.2186079213554,
40.0043257306693));
#200439=CARTESIAN_POINT('Ctrl Pts',(18.0531413250551,-56.2138593173289,
39.9667894847839));
#200440=CARTESIAN_POINT('Ctrl Pts',(18.1041761987737,-56.2854146278934,
40.0100138975199));
#200441=CARTESIAN_POINT('Ctrl Pts',(18.0394175380795,-56.1179510603876,
40.1195533054857));
#200442=CARTESIAN_POINT('Ctrl Pts',(18.0943218653327,-56.1373490477006,
40.0630813209234));
#200443=CARTESIAN_POINT('Ctrl Pts',(18.140307536858,-56.1984140977477,40.0768265942422));
#200444=CARTESIAN_POINT('Ctrl Pts',(18.1094153628979,-56.0689198620982,
40.1599502027512));
#200445=CARTESIAN_POINT('Ctrl Pts',(18.1436123520191,-56.0970362061497,
40.1002552791541));
#200446=CARTESIAN_POINT('Ctrl Pts',(18.1777307632117,-56.1599674935319,
40.10025));
#200447=CARTESIAN_POINT('Ctrl Pts',(18.1930767435948,-56.0417604764384,
40.1599502534424));
#200448=CARTESIAN_POINT('Ctrl Pts',(18.2045954185344,-56.0772424804485,
40.10025));
#200449=CARTESIAN_POINT('Ctrl Pts',(18.2263320786581,-56.1441998575528,
40.10025));
#200450=CARTESIAN_POINT('Origin',(18.2263320786581,-56.1441998575528,40.22725));
#200451=CARTESIAN_POINT('Ctrl Pts',(19.42073522007,-58.7434254837933,38.989));
#200452=CARTESIAN_POINT('Ctrl Pts',(19.2997705861194,-58.7827292759114,
38.989));
#200453=CARTESIAN_POINT('Ctrl Pts',(19.2999511771037,-58.7826705983436,
39.1161896013261));
#200454=CARTESIAN_POINT('Ctrl Pts',(19.4879965013588,-58.9497137831223,
38.989));
#200455=CARTESIAN_POINT('Ctrl Pts',(19.3668771285546,-58.9892635895195,
38.9887769275436));
#200456=CARTESIAN_POINT('Ctrl Pts',(19.3535710010449,-58.947695446951,39.1161898821819));
#200457=CARTESIAN_POINT('Ctrl Pts',(19.5520260773869,-59.1460976215385,
39.1034967087243));
#200458=CARTESIAN_POINT('Ctrl Pts',(19.4307447900779,-59.1858295777984,
39.103172023275));
#200459=CARTESIAN_POINT('Ctrl Pts',(19.4046161500171,-59.1047962608395,
39.2077529615026));
#200460=CARTESIAN_POINT('Ctrl Pts',(19.5876674457077,-59.2554138597572,
39.2875012672119));
#200461=CARTESIAN_POINT('Ctrl Pts',(19.4663243070096,-59.2953329133624,
39.2872087095508));
#200462=CARTESIAN_POINT('Ctrl Pts',(19.4330302514114,-59.1922458725048,
39.3549017048225));
#200463=CARTESIAN_POINT('Origin',(19.42073522007,-58.7434254837933,39.116));
#200464=CARTESIAN_POINT('Origin',(5.68280300381509E-15,5.19692153755175E-15,
40.22725));
#200465=CARTESIAN_POINT('Origin',(18.2553202812748,-56.1347810195642,40.22725));
#200466=CARTESIAN_POINT('Origin',(6.24367625034007,-18.1886080242677,39.116));
#200467=CARTESIAN_POINT('Origin',(19.2967593024463,-58.3616995707159,39.1160373285276));
#200468=CARTESIAN_POINT('Ctrl Pts',(18.2220120550216,-56.0323588238392,
40.1599502534424));
#200469=CARTESIAN_POINT('Ctrl Pts',(18.2335490499217,-56.0678348753333,
40.10025));
#200470=CARTESIAN_POINT('Ctrl Pts',(18.2553202812748,-56.1347810195643,
40.10025));
#200471=CARTESIAN_POINT('Ctrl Pts',(18.3053742463598,-56.0052491386465,
40.1599500566035));
#200472=CARTESIAN_POINT('Ctrl Pts',(18.2942806848329,-56.0480812627881,
40.1002551305372));
#200473=CARTESIAN_POINT('Ctrl Pts',(18.3037418885565,-56.1190241739981,
40.10025));
#200474=CARTESIAN_POINT('Ctrl Pts',(18.3900709842069,-56.0035251343647,
40.1203070619044));
#200475=CARTESIAN_POINT('Ctrl Pts',(18.3574039607305,-56.0514568378823,
40.0637098684496));
#200476=CARTESIAN_POINT('Ctrl Pts',(18.3561185603241,-56.1278011372721,
40.0772636213362));
#200477=CARTESIAN_POINT('Ctrl Pts',(18.513437727039,-56.0390077039667,40.0046102245804));
#200478=CARTESIAN_POINT('Ctrl Pts',(18.4363968713616,-56.0891934462338,
39.9670001894015));
#200479=CARTESIAN_POINT('Ctrl Pts',(18.4370884086013,-56.1770584756118,
40.010178881121));
#200480=CARTESIAN_POINT('Ctrl Pts',(18.5530236652638,-56.0747542753111,
39.9303710930184));
#200481=CARTESIAN_POINT('Ctrl Pts',(18.4521491348396,-56.1242585025267,
39.9058663574108));
#200482=CARTESIAN_POINT('Ctrl Pts',(18.4660698759074,-56.2162483036948,
39.9671344706364));
#200483=CARTESIAN_POINT('Ctrl Pts',(18.5670586829464,-56.1179479440989,
39.8576902534424));
#200484=CARTESIAN_POINT('Ctrl Pts',(18.4469743395778,-56.1574782858998,
39.8579948730703));
#200485=CARTESIAN_POINT('Ctrl Pts',(18.4801050014189,-56.2594439784239,
39.92499));
#200486=CARTESIAN_POINT('Origin',(18.6008891789884,-56.2201988201383,39.92499));
#200487=CARTESIAN_POINT('Origin',(19.2830435998985,-58.3196542512026,39.1925554488844));
#200488=CARTESIAN_POINT('Origin',(19.2577541638577,-58.2418213702174,39.3343017080178));
#200489=CARTESIAN_POINT('Origin',(18.6559403576616,-56.389628926533,39.6398955069214));
#200490=CARTESIAN_POINT('Origin',(18.7109915363516,-56.559059032799,39.3548010137695));
#200491=CARTESIAN_POINT('Ctrl Pts',(19.1557908785624,-57.9280106456676,
39.3978017080178));
#200492=CARTESIAN_POINT('Ctrl Pts',(19.0350067009929,-57.9672558039532,
39.3978017080178));
#200493=CARTESIAN_POINT('Ctrl Pts',(19.0350067009929,-57.9672558039532,
39.5248017080178));
#200494=CARTESIAN_POINT('Ctrl Pts',(19.1833829156713,-58.013688065021,39.3978017080178));
#200495=CARTESIAN_POINT('Ctrl Pts',(19.0627953474457,-58.052780463663,39.3980355775177));
#200496=CARTESIAN_POINT('Ctrl Pts',(19.0767283413222,-58.0956618095388,
39.5248015517178));
#200497=CARTESIAN_POINT('Ctrl Pts',(19.2094750027322,-58.0947019536604,
39.3484893995498));
#200498=CARTESIAN_POINT('Ctrl Pts',(19.0892026680444,-58.13405383953,39.3489438303424));
#200499=CARTESIAN_POINT('Ctrl Pts',(19.1161791203808,-58.2170788227761,
39.4508333155602));
#200500=CARTESIAN_POINT('Ctrl Pts',(19.2232259141438,-58.1373965169894,
39.2708017080178));
#200501=CARTESIAN_POINT('Ctrl Pts',(19.1031347997386,-58.176932531882,39.2710850691866));
#200502=CARTESIAN_POINT('Ctrl Pts',(19.1369699862882,-58.281066528503,39.3343017080178));
#200503=CARTESIAN_POINT('Origin',(19.1557908785624,-57.9280106456676,39.5248017080178));
#200504=CARTESIAN_POINT('Ctrl Pts',(18.6771643191709,-56.4568070719812,
39.2875012672119));
#200505=CARTESIAN_POINT('Ctrl Pts',(18.5568963159717,-56.4963947983079,
39.2878045257518));
#200506=CARTESIAN_POINT('Ctrl Pts',(18.59025719708,-56.5984571192853,39.3549015218347));
#200507=CARTESIAN_POINT('Ctrl Pts',(18.7128129802643,-56.5661228951883,
39.1034938540228));
#200508=CARTESIAN_POINT('Ctrl Pts',(18.5923766197439,-56.605592832571,39.1038286278807));
#200509=CARTESIAN_POINT('Ctrl Pts',(18.6186718120043,-56.6859083114058,
39.2077506434026));
#200510=CARTESIAN_POINT('Ctrl Pts',(18.7768537015931,-56.7625049710038,
38.989));
#200511=CARTESIAN_POINT('Ctrl Pts',(18.6561664154745,-56.8019192501362,
38.9892298954617));
#200512=CARTESIAN_POINT('Ctrl Pts',(18.6697173900117,-56.8430104456845,
39.1161900347295));
#200513=CARTESIAN_POINT('Ctrl Pts',(18.8441205405518,-56.9687879773467,
38.989));
#200514=CARTESIAN_POINT('Ctrl Pts',(18.7231554368008,-57.0080919221122,
38.989));
#200515=CARTESIAN_POINT('Ctrl Pts',(18.7233364982868,-57.0080330916692,
39.1161900945646));
#200516=CARTESIAN_POINT('Origin',(18.8441205405518,-56.9687879773467,39.116));
#200517=CARTESIAN_POINT('Origin',(6.09975091006187,-17.7456513739111,39.5248017080178));
#200518=CARTESIAN_POINT('Origin',(19.1090650011314,-57.7842031819383,39.5248017080178));
#200519=CARTESIAN_POINT('Origin',(6.07721283595898,-17.676286314285,39.116));
#200520=CARTESIAN_POINT('Origin',(18.9681964166832,-57.3504898524408,39.1160402713852));
#200521=CARTESIAN_POINT('Ctrl Pts',(19.0416371860877,-57.5748148483576,
39.2708017080178));
#200522=CARTESIAN_POINT('Ctrl Pts',(18.9204594407744,-57.6147155869502,
39.27051194648));
#200523=CARTESIAN_POINT('Ctrl Pts',(18.8863175164091,-57.5096375484037,
39.3343017080178));
#200524=CARTESIAN_POINT('Ctrl Pts',(19.0554318862548,-57.6176546016065,
39.3487519301185));
#200525=CARTESIAN_POINT('Ctrl Pts',(18.9342932580175,-57.657291698537,39.3482879463977));
#200526=CARTESIAN_POINT('Ctrl Pts',(18.9071786451782,-57.5738415009833,
39.4512271261633));
#200527=CARTESIAN_POINT('Ctrl Pts',(19.0815664505371,-57.6988141606857,
39.3978017080178));
#200528=CARTESIAN_POINT('Ctrl Pts',(18.960533015575,-57.7380493683891,39.3975673827401));
#200529=CARTESIAN_POINT('Ctrl Pts',(18.9466997135535,-57.6954748424935,
39.5248015355181));
#200530=CARTESIAN_POINT('Ctrl Pts',(19.1090650011314,-57.7842031819383,
39.3978017080178));
#200531=CARTESIAN_POINT('Ctrl Pts',(18.9882808235619,-57.8234483402239,
39.3978017080178));
#200532=CARTESIAN_POINT('Ctrl Pts',(18.9882808235619,-57.8234483402239,
39.5248017080178));
#200533=CARTESIAN_POINT('Origin',(19.0071016939786,-57.4703923901181,39.3343017080178));
#200534=CARTESIAN_POINT('Origin',(18.9819630792892,-57.3930236885616,39.1934008533552));
#200535=CARTESIAN_POINT('Origin',(12.4602215063119,-60.1478239224126,39.192555449508));
#200536=CARTESIAN_POINT('Origin',(12.4693660187275,-60.1910940874965,39.116037328525));
#200537=CARTESIAN_POINT('Origin',(12.443206359372,-60.0677739512126,39.3343017080178));
#200538=CARTESIAN_POINT('Ctrl Pts',(12.4208962741585,-59.9600752506737,
39.2708017080178));
#200539=CARTESIAN_POINT('Ctrl Pts',(12.5446662374485,-59.9342688867325,
39.2710850691866));
#200540=CARTESIAN_POINT('Ctrl Pts',(12.5674311046652,-60.0413691664788,
39.3343017080178));
#200541=CARTESIAN_POINT('Ctrl Pts',(12.4114257351943,-59.9160770362135,
39.3487519293518));
#200542=CARTESIAN_POINT('Ctrl Pts',(12.5352608058713,-59.8900198101361,
39.3492068662929));
#200543=CARTESIAN_POINT('Ctrl Pts',(12.553395401069,-59.975336372732,39.4512271248739));
#200544=CARTESIAN_POINT('Ctrl Pts',(12.3934832896272,-59.8327226933129,
39.3978017080178));
#200545=CARTESIAN_POINT('Ctrl Pts',(12.5174621766264,-59.8062838430882,
39.3980347781178));
#200546=CARTESIAN_POINT('Ctrl Pts',(12.5268049860496,-59.8502383056083,
39.5248015355195));
#200547=CARTESIAN_POINT('Ctrl Pts',(12.3746037924162,-59.7450242491248,
39.3978017080178));
#200548=CARTESIAN_POINT('Ctrl Pts',(12.4988285377094,-59.7186194643909,
39.3978017080178));
#200549=CARTESIAN_POINT('Ctrl Pts',(12.4988285377094,-59.7186194643909,
39.5248017080178));
#200550=CARTESIAN_POINT('Origin',(12.3746037924162,-59.7450242491248,39.5248017080178));
#200551=CARTESIAN_POINT('Origin',(-0.310561863232978,-0.0660119618346377,
39.116));
#200552=CARTESIAN_POINT('Origin',(12.5528626811445,-60.5836663843182,39.116));
#200553=CARTESIAN_POINT('Origin',(-0.310561863232978,-0.0660119618346377,
39.5248017080178));
#200554=CARTESIAN_POINT('Origin',(12.3431658574209,-59.5971203935659,39.5248017080178));
#200555=CARTESIAN_POINT('Ctrl Pts',(12.664289321014,-61.1105274371641,39.2875012672119));
#200556=CARTESIAN_POINT('Ctrl Pts',(12.7893350777082,-61.0844267845857,
39.287208709576));
#200557=CARTESIAN_POINT('Ctrl Pts',(12.7666250679676,-60.9785037674412,
39.3549016990122));
#200558=CARTESIAN_POINT('Ctrl Pts',(12.6404971713781,-60.9980344071775,
39.1034939173931));
#200559=CARTESIAN_POINT('Ctrl Pts',(12.7653958126118,-60.9718026486705,
39.1031692336359));
#200560=CARTESIAN_POINT('Ctrl Pts',(12.7475073053525,-60.8885617651932,
39.2077507202317));
#200561=CARTESIAN_POINT('Ctrl Pts',(12.5977561540111,-60.7959446297926,
38.989));
#200562=CARTESIAN_POINT('Ctrl Pts',(12.7224234952041,-60.7696360759163,
38.9887769311152));
#200563=CARTESIAN_POINT('Ctrl Pts',(12.7131630221044,-60.7269846150121,
39.1161898712891));
#200564=CARTESIAN_POINT('Ctrl Pts',(12.5528626811445,-60.5836663843182,
38.989));
#200565=CARTESIAN_POINT('Ctrl Pts',(12.6772730124466,-60.5572221520604,
38.989));
#200566=CARTESIAN_POINT('Ctrl Pts',(12.6770872880162,-60.5572616290068,
39.1161895903854));
#200567=CARTESIAN_POINT('Origin',(12.642433962084,-61.0050661295707,39.3548010137695));
#200568=CARTESIAN_POINT('Ctrl Pts',(12.3431658574209,-59.5971203935659,
39.3978017080178));
#200569=CARTESIAN_POINT('Ctrl Pts',(12.4673906027141,-59.5707156088321,
39.3978017080178));
#200570=CARTESIAN_POINT('Ctrl Pts',(12.4673906027141,-59.5707156088321,
39.5248017080178));
#200571=CARTESIAN_POINT('Ctrl Pts',(12.3242219811461,-59.5091256622727,
39.3978017080178));
#200572=CARTESIAN_POINT('Ctrl Pts',(12.4486583679645,-59.4825873732142,
39.3975666025021));
#200573=CARTESIAN_POINT('Ctrl Pts',(12.4393195978195,-59.4386519140016,
39.5248015517178));
#200574=CARTESIAN_POINT('Ctrl Pts',(12.3063073021301,-59.4259203549055,
39.3484894016716));
#200575=CARTESIAN_POINT('Ctrl Pts',(12.4310355281337,-59.3996784303259,
39.3480259000051));
#200576=CARTESIAN_POINT('Ctrl Pts',(12.4127764613282,-59.3137762748649,
39.4508333188953));
#200577=CARTESIAN_POINT('Ctrl Pts',(12.2968658913801,-59.3820708699071,
39.2708017080178));
#200578=CARTESIAN_POINT('Ctrl Pts',(12.4217592664911,-59.3560370505014,
39.27051194648));
#200579=CARTESIAN_POINT('Ctrl Pts',(12.3987880210522,-59.2479658375577,
39.3343017080178));
#200580=CARTESIAN_POINT('Origin',(12.274563275759,-59.2743706222915,39.3343017080178));
#200581=CARTESIAN_POINT('Origin',(12.6794732450922,-61.1793222555443,39.6398955068198));
#200582=CARTESIAN_POINT('Origin',(12.7165125280164,-61.3535783813232,39.92499));
#200583=CARTESIAN_POINT('Origin',(12.2576496039896,-59.1947980527942,39.1934008539943));
#200584=CARTESIAN_POINT('Origin',(12.2483049653993,-59.151079340037,39.1160402713853));
#200585=CARTESIAN_POINT('Ctrl Pts',(13.0739701745323,-61.5816197022698,
40.1599502534424));
#200586=CARTESIAN_POINT('Ctrl Pts',(13.0662229071065,-61.5451281645059,
40.10025));
#200587=CARTESIAN_POINT('Ctrl Pts',(13.0516031943527,-61.4762657165316,
40.10025));
#200588=CARTESIAN_POINT('Ctrl Pts',(12.9877758510419,-61.5999188988202,
40.1599500538472));
#200589=CARTESIAN_POINT('Ctrl Pts',(13.0034370926714,-61.5584544893711,
40.100244835349));
#200590=CARTESIAN_POINT('Ctrl Pts',(13.0017087032042,-61.4868491822357,
40.10025));
#200591=CARTESIAN_POINT('Ctrl Pts',(12.9030451317659,-61.5923336062396,
40.1202442001039));
#200592=CARTESIAN_POINT('Ctrl Pts',(12.9408103617801,-61.5481051179917,
40.0633873868018));
#200593=CARTESIAN_POINT('Ctrl Pts',(12.9504709278438,-61.4721451382825,
40.0772271723538));
#200594=CARTESIAN_POINT('Ctrl Pts',(12.7836101409429,-61.5434299552079,
40.0045995998162));
#200595=CARTESIAN_POINT('Ctrl Pts',(12.8662000075463,-61.5018471007595,
39.9663485808315));
#200596=CARTESIAN_POINT('Ctrl Pts',(12.8749747009097,-61.4139027244671,
40.0101727202466));
#200597=CARTESIAN_POINT('Ctrl Pts',(12.7478263086951,-61.5035207735036,
39.9304654349859));
#200598=CARTESIAN_POINT('Ctrl Pts',(12.8544221781243,-61.465297106343,39.9051900162953));
#200599=CARTESIAN_POINT('Ctrl Pts',(12.8501918100168,-61.3716536946533,
39.9671857458179));
#200600=CARTESIAN_POINT('Ctrl Pts',(12.7383709431249,-61.4590390555209,
39.8576902534424));
#200601=CARTESIAN_POINT('Ctrl Pts',(12.8632261535953,-61.4329754599099,
39.8573998014387));
#200602=CARTESIAN_POINT('Ctrl Pts',(12.8407372733096,-61.3271735965894,
39.92499));
#200603=CARTESIAN_POINT('Origin',(13.0516031943527,-61.4762657165316,40.22725));
#200604=CARTESIAN_POINT('Origin',(-0.310561863232978,-0.0660119618346377,
39.116));
#200605=CARTESIAN_POINT('Origin',(12.164906888579,-58.7584778814677,39.116));
#200606=CARTESIAN_POINT('Origin',(5.63039444364742E-15,5.85617094392624E-15,
40.22725));
#200607=CARTESIAN_POINT('Origin',(13.0814171332231,-61.4699285681955,40.22725));
#200608=CARTESIAN_POINT('Ctrl Pts',(12.164906888579,-58.7584778814677,38.989));
#200609=CARTESIAN_POINT('Ctrl Pts',(12.2893177281499,-58.732033541174,38.989));
#200610=CARTESIAN_POINT('Ctrl Pts',(12.289131494692,-58.7320731263175,39.1161901092319));
#200611=CARTESIAN_POINT('Ctrl Pts',(12.1200194799681,-58.5461948427482,
38.989));
#200612=CARTESIAN_POINT('Ctrl Pts',(12.2442448876954,-58.5199849720709,
38.9892298989766));
#200613=CARTESIAN_POINT('Ctrl Pts',(12.2530551225939,-58.5623471386674,
39.1161900493205));
#200614=CARTESIAN_POINT('Ctrl Pts',(12.0772896710129,-58.3441042111267,
39.1034966344368));
#200615=CARTESIAN_POINT('Ctrl Pts',(12.201325600148,-58.3180679977624,39.1038314102563));
#200616=CARTESIAN_POINT('Ctrl Pts',(12.2187110949219,-58.4007711908112,
39.2077528789595));
#200617=CARTESIAN_POINT('Ctrl Pts',(12.053504764932,-58.2316113004781,39.2875012672119));
#200618=CARTESIAN_POINT('Ctrl Pts',(12.1774537884109,-58.2057612725768,
39.2878045257868));
#200619=CARTESIAN_POINT('Ctrl Pts',(12.1995935666435,-58.3108302909891,
39.3549015295897));
#200620=CARTESIAN_POINT('Origin',(12.0753355159231,-58.3370777047235,39.3548010137695));
#200621=CARTESIAN_POINT('Ctrl Pts',(13.3605623192485,-61.3267881959113,
39.8576902534424));
#200622=CARTESIAN_POINT('Ctrl Pts',(13.2359003894749,-61.3537611057083,
39.8573998014387));
#200623=CARTESIAN_POINT('Ctrl Pts',(13.2134115091892,-61.2479592423878,
39.92499));
#200624=CARTESIAN_POINT('Ctrl Pts',(13.3700210384233,-61.371290318078,39.9304984902491));
#200625=CARTESIAN_POINT('Ctrl Pts',(13.2571016411968,-61.3797222373779,
39.9052171569789));
#200626=CARTESIAN_POINT('Ctrl Pts',(13.2228703539491,-61.2924596082463,
39.9672049726608));
#200627=CARTESIAN_POINT('Ctrl Pts',(13.3535190881771,-61.422128257289,40.0043437678663));
#200628=CARTESIAN_POINT('Ctrl Pts',(13.2610999767702,-61.4177900459393,
39.9661628577643));
#200629=CARTESIAN_POINT('Ctrl Pts',(13.2173727427872,-61.3409599630865,
40.0100243556235));
#200630=CARTESIAN_POINT('Ctrl Pts',(13.2651598666398,-61.5148770953648,
40.1194874821986));
#200631=CARTESIAN_POINT('Ctrl Pts',(13.2123479779268,-61.4899829268154,
40.062755148314));
#200632=CARTESIAN_POINT('Ctrl Pts',(13.1725625528868,-61.4244514636296,
40.0767884282377));
#200633=CARTESIAN_POINT('Ctrl Pts',(13.1903059833735,-61.5568698122755,
40.1599502015388));
#200634=CARTESIAN_POINT('Ctrl Pts',(13.1590895168688,-61.5253695547383,
40.100244945386));
#200635=CARTESIAN_POINT('Ctrl Pts',(13.1314678292776,-61.4592680512443,
40.10025));
#200636=CARTESIAN_POINT('Ctrl Pts',(13.1038352065726,-61.5752716937452,
40.1599502534424));
#200637=CARTESIAN_POINT('Ctrl Pts',(13.0960702419678,-61.5387839176328,
40.10025));
#200638=CARTESIAN_POINT('Ctrl Pts',(13.0814171332231,-61.4699285681955,
40.10025));
#200639=CARTESIAN_POINT('Origin',(13.3376362544824,-61.2215544576539,39.92499));
#200640=CARTESIAN_POINT('Origin',(12.0382961820475,-58.1628213392055,39.6398955069336));
#200641=CARTESIAN_POINT('Origin',(12.0012568480858,-57.988564973546,39.92499));
#200642=CARTESIAN_POINT('Origin',(13.3005969715137,-61.0472983318708,39.6398955068282));
#200643=CARTESIAN_POINT('Origin',(13.26355768855,-60.8730422059014,39.3548010137695));
#200644=CARTESIAN_POINT('Ctrl Pts',(11.9794294790611,-57.8830978693156,
39.8576902534424));
#200645=CARTESIAN_POINT('Ctrl Pts',(12.1031907419155,-57.8572899778511,
39.8579948730703));
#200646=CARTESIAN_POINT('Ctrl Pts',(12.125481593379,-57.9621601888121,39.92499));
#200647=CARTESIAN_POINT('Ctrl Pts',(11.9699833161086,-57.8386546085355,
39.9304020711231));
#200648=CARTESIAN_POINT('Ctrl Pts',(12.0820882677174,-57.8310944294283,
39.9058915297392));
#200649=CARTESIAN_POINT('Ctrl Pts',(12.1160345187366,-57.9177151970032,
39.9671523786037));
#200650=CARTESIAN_POINT('Ctrl Pts',(11.986420485103,-57.7880992891175,40.0043257306692));
#200651=CARTESIAN_POINT('Ctrl Pts',(12.0782959991611,-57.7929810340975,
39.9667894847835));
#200652=CARTESIAN_POINT('Ctrl Pts',(12.1215717318493,-57.8694789541066,
40.01001389752));
#200653=CARTESIAN_POINT('Ctrl Pts',(12.0746725352387,-57.6961636462597,
40.1195533054858));
#200654=CARTESIAN_POINT('Ctrl Pts',(12.1272484490378,-57.7211944343229,
40.0630813209236));
#200655=CARTESIAN_POINT('Ctrl Pts',(12.1665991704024,-57.7867317752132,
40.0768265942421));
#200656=CARTESIAN_POINT('Ctrl Pts',(12.1494120604582,-57.654717811065,40.1599502027512));
#200657=CARTESIAN_POINT('Ctrl Pts',(12.1804827566585,-57.6862546895626,
40.1002552791541));
#200658=CARTESIAN_POINT('Ctrl Pts',(12.2078361528634,-57.7524075778604,
40.10025));
#200659=CARTESIAN_POINT('Ctrl Pts',(12.2354540642043,-57.6364522029207,
40.1599502534424));
#200660=CARTESIAN_POINT('Ctrl Pts',(12.2432007592846,-57.6729438621906,
40.10025));
#200661=CARTESIAN_POINT('Ctrl Pts',(12.2578193919766,-57.7418065394566,
40.10025));
#200662=CARTESIAN_POINT('Origin',(12.2578193919766,-57.7418065394566,40.22725));
#200663=CARTESIAN_POINT('Ctrl Pts',(13.1739864076105,-60.4516424606489,
38.989));
#200664=CARTESIAN_POINT('Ctrl Pts',(13.0495760655905,-60.4780866951849,
38.989));
#200665=CARTESIAN_POINT('Ctrl Pts',(13.0497618007548,-60.478047215957,39.1161896013264));
#200666=CARTESIAN_POINT('Ctrl Pts',(13.2193162256451,-60.6638314094601,
38.989));
#200667=CARTESIAN_POINT('Ctrl Pts',(13.0947262769526,-60.6905041359647,
38.988776927546));
#200668=CARTESIAN_POINT('Ctrl Pts',(13.0858380958638,-60.6477728389725,
39.1161898821822));
#200669=CARTESIAN_POINT('Ctrl Pts',(13.2624673401144,-60.8658323498478,
39.1034967087243));
#200670=CARTESIAN_POINT('Ctrl Pts',(13.1376973240545,-60.8926693037143,
39.1031720232717));
#200671=CARTESIAN_POINT('Ctrl Pts',(13.1201821075159,-60.8093487091476,
39.2077529615022));
#200672=CARTESIAN_POINT('Ctrl Pts',(13.2864868028994,-60.9782752797348,
39.2875012672119));
#200673=CARTESIAN_POINT('Ctrl Pts',(13.1616357172827,-61.0052918407715,
39.2872087095507));
#200674=CARTESIAN_POINT('Ctrl Pts',(13.1392995799685,-60.8992893450419,
39.3549017048226));
#200675=CARTESIAN_POINT('Origin',(13.1739864076105,-60.4516424606489,39.116));
#200676=CARTESIAN_POINT('Origin',(5.67687244506386E-15,5.19533244912369E-15,
40.22725));
#200677=CARTESIAN_POINT('Origin',(12.2876333308469,-57.7354693911205,40.22725));
#200678=CARTESIAN_POINT('Origin',(3.00026883051124,-12.5880644220968,39.116));
#200679=CARTESIAN_POINT('Origin',(13.0905908661165,-60.0590486699117,39.1160373285255));
#200680=CARTESIAN_POINT('Ctrl Pts',(12.2652136052659,-57.6301266171958,
40.1599502534424));
#200681=CARTESIAN_POINT('Ctrl Pts',(12.2729791421553,-57.6666142715155,
40.10025));
#200682=CARTESIAN_POINT('Ctrl Pts',(12.2876333308469,-57.7354693911205,
40.10025));
#200683=CARTESIAN_POINT('Ctrl Pts',(12.3509528635304,-57.61187916345,40.159950056604));
#200684=CARTESIAN_POINT('Ctrl Pts',(12.3354428975794,-57.6533170557954,
40.100255130536));
#200685=CARTESIAN_POINT('Ctrl Pts',(12.3374367183506,-57.7248602994014,
40.10025));
#200686=CARTESIAN_POINT('Ctrl Pts',(12.4353658313041,-57.6190178232951,
40.1203070619047));
#200687=CARTESIAN_POINT('Ctrl Pts',(12.3978675338896,-57.6632723181624,
40.0637098684499));
#200688=CARTESIAN_POINT('Ctrl Pts',(12.3886090227466,-57.7390640345628,
40.0772636213363));
#200689=CARTESIAN_POINT('Ctrl Pts',(12.5543478197374,-57.6672013517152,
40.0046102245801));
#200690=CARTESIAN_POINT('Ctrl Pts',(12.4724831634114,-57.7090592089822,
39.9670001894012));
#200691=CARTESIAN_POINT('Ctrl Pts',(12.463986515842,-57.7965151898608,40.0101788811209));
#200692=CARTESIAN_POINT('Ctrl Pts',(12.5899803678813,-57.7068899568909,
39.9303710930187));
#200693=CARTESIAN_POINT('Ctrl Pts',(12.4844838378943,-57.7455787351216,
39.9058663574104));
#200694=CARTESIAN_POINT('Ctrl Pts',(12.4887127671323,-57.8385197202055,
39.9671344706363));
#200695=CARTESIAN_POINT('Ctrl Pts',(12.599423532447,-57.751314065072,39.8576902534424));
#200696=CARTESIAN_POINT('Ctrl Pts',(12.4758649777951,-57.7780756236496,
39.8579948730703));
#200697=CARTESIAN_POINT('Ctrl Pts',(12.4981558292586,-57.8829458346106,
39.92499));
#200698=CARTESIAN_POINT('Origin',(12.6223805745518,-57.8565410498767,39.92499));
#200699=CARTESIAN_POINT('Origin',(13.081345232263,-60.0157999977505,39.1925554488856));
#200700=CARTESIAN_POINT('Origin',(13.064330085838,-59.9357500275433,39.3343017080178));
#200701=CARTESIAN_POINT('Origin',(12.6594199084528,-58.0307974155296,39.6398955069217));
#200702=CARTESIAN_POINT('Origin',(12.6964592423891,-58.2050537810542,39.3548010137695));
#200703=CARTESIAN_POINT('Ctrl Pts',(12.9957275188822,-59.6130003254555,
39.3978017080178));
#200704=CARTESIAN_POINT('Ctrl Pts',(12.871502773589,-59.6394051101894,39.3978017080178));
#200705=CARTESIAN_POINT('Ctrl Pts',(12.871502773589,-59.6394051101894,39.5248017080178));
#200706=CARTESIAN_POINT('Ctrl Pts',(13.0142126749438,-59.7010925481784,
39.3978017080178));
#200707=CARTESIAN_POINT('Ctrl Pts',(12.8901994296791,-59.7273659613754,
39.3980355775177));
#200708=CARTESIAN_POINT('Ctrl Pts',(12.899573775969,-59.7714687931893,39.5248015517192));
#200709=CARTESIAN_POINT('Ctrl Pts',(13.0316935695382,-59.7843900000233,
39.3484893995498));
#200710=CARTESIAN_POINT('Ctrl Pts',(12.9079667071292,-59.8109544298246,
39.3489438303421));
#200711=CARTESIAN_POINT('Ctrl Pts',(12.926116905724,-59.8963444006346,39.4508333155593));
#200712=CARTESIAN_POINT('Ctrl Pts',(13.0409063549237,-59.8282880397055,
39.2708017080178));
#200713=CARTESIAN_POINT('Ctrl Pts',(12.9173404733281,-59.855054532531,39.2710850691866));
#200714=CARTESIAN_POINT('Ctrl Pts',(12.9401053405448,-59.9621548122772,
39.3343017080178));
#200715=CARTESIAN_POINT('Origin',(12.9957275188822,-59.6130003254555,39.5248017080178));
#200716=CARTESIAN_POINT('Ctrl Pts',(12.6735055745739,-58.099826060148,39.2875012672119));
#200717=CARTESIAN_POINT('Ctrl Pts',(12.549758367883,-58.1266254912131,39.2878045257518));
#200718=CARTESIAN_POINT('Ctrl Pts',(12.5722680770246,-58.2316158657527,
39.3549015218347));
#200719=CARTESIAN_POINT('Ctrl Pts',(12.697532333562,-58.2122693395992,39.1034938540228));
#200720=CARTESIAN_POINT('Ctrl Pts',(12.5736300041254,-58.2389340288469,
39.1038286278789));
#200721=CARTESIAN_POINT('Ctrl Pts',(12.5913858949919,-58.3215581271248,
39.2077506434029));
#200722=CARTESIAN_POINT('Ctrl Pts',(12.7406947165197,-58.4142696920427,
38.989));
#200723=CARTESIAN_POINT('Ctrl Pts',(12.6165486539537,-58.4408527990775,
38.9892298954635));
#200724=CARTESIAN_POINT('Ctrl Pts',(12.6257301953099,-58.4831353553001,
39.1161900347288));
#200725=CARTESIAN_POINT('Ctrl Pts',(12.786030615045,-58.6264539577984,38.989));
#200726=CARTESIAN_POINT('Ctrl Pts',(12.6616197898425,-58.652898295038,38.989));
#200727=CARTESIAN_POINT('Ctrl Pts',(12.6618060089105,-58.6528587129532,
39.1161900945645));
#200728=CARTESIAN_POINT('Origin',(12.786030615045,-58.6264539577984,39.116));
#200729=CARTESIAN_POINT('Origin',(2.93511643966546,-12.2815465224192,39.5248017080178));
#200730=CARTESIAN_POINT('Origin',(12.9642895838869,-59.4650964698967,39.5248017080178));
#200731=CARTESIAN_POINT('Origin',(2.92491386234291,-12.2335471699533,39.116));
#200732=CARTESIAN_POINT('Origin',(12.8695280801142,-59.0190342907437,39.1160402713847));
#200733=CARTESIAN_POINT('Ctrl Pts',(12.9191181862044,-59.249807061628,39.2708017080178));
#200734=CARTESIAN_POINT('Ctrl Pts',(12.7944335023706,-59.2768226962998,
39.27051194648));
#200735=CARTESIAN_POINT('Ctrl Pts',(12.7714622569318,-59.1687514833561,
39.3343017080178));
#200736=CARTESIAN_POINT('Ctrl Pts',(12.9283593439858,-59.2938540730361,
39.3487519301186));
#200737=CARTESIAN_POINT('Ctrl Pts',(12.8037411209993,-59.3206115991491,
39.3482879463997));
#200738=CARTESIAN_POINT('Ctrl Pts',(12.7854979657559,-59.2347843016977,
39.4512271261635));
#200739=CARTESIAN_POINT('Ctrl Pts',(12.9458672564005,-59.3773008374013,
39.3978017080178));
#200740=CARTESIAN_POINT('Ctrl Pts',(12.8213956592929,-59.4036696715717,
39.3975673827378));
#200741=CARTESIAN_POINT('Ctrl Pts',(12.8120883873134,-59.3598823995808,
39.5248015355181));
#200742=CARTESIAN_POINT('Ctrl Pts',(12.9642895838869,-59.4650964698967,
39.3978017080178));
#200743=CARTESIAN_POINT('Ctrl Pts',(12.8400648385937,-59.4915012546305,
39.3978017080178));
#200744=CARTESIAN_POINT('Ctrl Pts',(12.8400648385937,-59.4915012546305,
39.5248017080178));
#200745=CARTESIAN_POINT('Origin',(12.895687002225,-59.1423466986222,39.3343017080178));
#200746=CARTESIAN_POINT('Origin',(12.8787733309747,-59.0627741301463,39.1934008533551));
#200747=CARTESIAN_POINT('Origin',(6.10480350566306,-61.1207756556249,39.1925554495084));
#200748=CARTESIAN_POINT('Origin',(6.10937495962084,-61.1647646440469,39.1160373285258));
#200749=CARTESIAN_POINT('Origin',(6.09624906995219,-61.0393856393804,39.3343017080178));
#200750=CARTESIAN_POINT('Ctrl Pts',(6.08531878138301,-60.929944884669,39.2708017080178));
#200751=CARTESIAN_POINT('Ctrl Pts',(6.21110821942915,-60.9172173747511,
39.2710850691866));
#200752=CARTESIAN_POINT('Ctrl Pts',(6.22255335066396,-61.0261105245454,
39.3343017080178));
#200753=CARTESIAN_POINT('Ctrl Pts',(6.08049918876647,-60.885197756147,39.3487519293518));
#200754=CARTESIAN_POINT('Ctrl Pts',(6.20637959976528,-60.8722275639167,
39.3492068662927));
#200755=CARTESIAN_POINT('Ctrl Pts',(6.21549684257599,-60.9589723348223,
39.4512271248734));
#200756=CARTESIAN_POINT('Ctrl Pts',(6.07136793516305,-60.800424540796,39.3978017080178));
#200757=CARTESIAN_POINT('Ctrl Pts',(6.19743126523188,-60.7870898478952,
39.3980347781178));
#200758=CARTESIAN_POINT('Ctrl Pts',(6.20212840134683,-60.8317801127832,
39.5248015355195));
#200759=CARTESIAN_POINT('Ctrl Pts',(6.0617588454155,-60.7112330730304,39.3978017080178));
#200760=CARTESIAN_POINT('Ctrl Pts',(6.18806312612727,-60.6979579581954,
39.3978017080178));
#200761=CARTESIAN_POINT('Ctrl Pts',(6.18806312612727,-60.6979579581954,
39.5248017080178));
#200762=CARTESIAN_POINT('Origin',(6.0617588454155,-60.7112330730304,39.5248017080178));
#200763=CARTESIAN_POINT('Origin',(-0.315760701779421,-0.033187787087479,
39.116));
#200764=CARTESIAN_POINT('Origin',(6.15137923967656,-61.5639141665612,39.116));
#200765=CARTESIAN_POINT('Origin',(-0.315760701779421,-0.033187787087479,
39.5248017080178));
#200766=CARTESIAN_POINT('Origin',(6.04595329345041,-60.5608532912344,39.5248017080178));
#200767=CARTESIAN_POINT('Ctrl Pts',(6.20712349654444,-62.0995362748659,
39.2875012672119));
#200768=CARTESIAN_POINT('Ctrl Pts',(6.33421250060443,-62.0866494451786,
39.287208709576));
#200769=CARTESIAN_POINT('Ctrl Pts',(6.32269886887976,-61.9789328429856,
39.3549016990124));
#200770=CARTESIAN_POINT('Ctrl Pts',(6.19522040634661,-61.9851725366286,
39.1034939173931));
#200771=CARTESIAN_POINT('Ctrl Pts',(6.32217680516354,-61.9721399414744,
39.1031692336332));
#200772=CARTESIAN_POINT('Ctrl Pts',(6.31308733464728,-61.8874852020939,
39.2077507202291));
#200773=CARTESIAN_POINT('Ctrl Pts',(6.17383766261684,-61.7797221753254,
38.989));
#200774=CARTESIAN_POINT('Ctrl Pts',(6.30057205577867,-61.7665890280522,
38.9887769311176));
#200775=CARTESIAN_POINT('Ctrl Pts',(6.29582060418312,-61.7232032332902,
39.1161898712918));
#200776=CARTESIAN_POINT('Ctrl Pts',(6.15137923967656,-61.5639141665612,
38.989));
#200777=CARTESIAN_POINT('Ctrl Pts',(6.27787221312702,-61.5506192193202,
38.989));
#200778=CARTESIAN_POINT('Ctrl Pts',(6.27768337964964,-61.5506390665185,
39.1161895903857));
#200779=CARTESIAN_POINT('Origin',(6.19641157197444,-61.9923681882669,39.3548010137695));
#200780=CARTESIAN_POINT('Ctrl Pts',(6.04595329345041,-60.5608532912344,
39.3978017080178));
#200781=CARTESIAN_POINT('Ctrl Pts',(6.17225757416218,-60.5475781763994,
39.3978017080178));
#200782=CARTESIAN_POINT('Ctrl Pts',(6.17225757416218,-60.5475781763994,
39.5248017080178));
#200783=CARTESIAN_POINT('Ctrl Pts',(6.03631114775037,-60.4713604300107,
39.3978017080178));
#200784=CARTESIAN_POINT('Ctrl Pts',(6.16283986559496,-60.4579746647645,
39.3975666025021));
#200785=CARTESIAN_POINT('Ctrl Pts',(6.1581447602436,-60.4133037213034,39.5248015517178));
#200786=CARTESIAN_POINT('Ctrl Pts',(6.02719193013407,-60.3867383361558,
39.3484894016716));
#200787=CARTESIAN_POINT('Ctrl Pts',(6.1539799099135,-60.3736778173762,39.3480259000049));
#200788=CARTESIAN_POINT('Ctrl Pts',(6.14480008848979,-60.2863376507156,
39.4508333188954));
#200789=CARTESIAN_POINT('Ctrl Pts',(6.02238575970256,-60.3421421670675,
39.2708017080178));
#200790=CARTESIAN_POINT('Ctrl Pts',(6.14931623097228,-60.3293058762212,
39.27051194648));
#200791=CARTESIAN_POINT('Ctrl Pts',(6.13776734223196,-60.2194255397045,
39.3343017080178));
#200792=CARTESIAN_POINT('Origin',(6.01146306152019,-60.2327006545395,39.3343017080178));
#200793=CARTESIAN_POINT('Origin',(6.21503322485551,-62.1695413802827,39.6398955068198));
#200794=CARTESIAN_POINT('Origin',(6.23365487766605,-62.3467145720969,39.92499));
#200795=CARTESIAN_POINT('Origin',(6.00295964302158,-60.1517960317859,39.193400853994));
#200796=CARTESIAN_POINT('Origin',(5.99823604520051,-60.1073400339996,39.1160402713852));
#200797=CARTESIAN_POINT('Ctrl Pts',(6.56531752495282,-62.6108711573006,
40.1599502534424));
#200798=CARTESIAN_POINT('Ctrl Pts',(6.56142710223332,-62.5737697140402,
40.10025));
#200799=CARTESIAN_POINT('Ctrl Pts',(6.55408556365926,-62.5037563256535,
40.10025));
#200800=CARTESIAN_POINT('Ctrl Pts',(6.47768259609056,-62.6200603487595,
40.159950053845));
#200801=CARTESIAN_POINT('Ctrl Pts',(6.49759225479931,-62.5804601311999,
40.1002448353481));
#200802=CARTESIAN_POINT('Ctrl Pts',(6.50335812634734,-62.5090664195357,
40.10025));
#200803=CARTESIAN_POINT('Ctrl Pts',(6.39420891953743,-62.603659837329,40.1202442001038));
#200804=CARTESIAN_POINT('Ctrl Pts',(6.43639040357922,-62.5636211788254,
40.0633873868017));
#200805=CARTESIAN_POINT('Ctrl Pts',(6.45393802800009,-62.489087119958,40.0772271723538));
#200806=CARTESIAN_POINT('Ctrl Pts',(6.28054002958119,-62.5425397295636,
40.0045995998163));
#200807=CARTESIAN_POINT('Ctrl Pts',(6.36702405212767,-62.5098176621807,
39.9663485808314));
#200808=CARTESIAN_POINT('Ctrl Pts',(6.3849433673096,-62.423272259596,40.0101727202465));
#200809=CARTESIAN_POINT('Ctrl Pts',(6.24912387034454,-62.4991087455376,
39.9304654349858));
#200810=CARTESIAN_POINT('Ctrl Pts',(6.35913125763746,-62.4722367740488,
39.9051900162944));
#200811=CARTESIAN_POINT('Ctrl Pts',(6.36471246584704,-62.3786641568871,
39.9671857458182));
#200812=CARTESIAN_POINT('Ctrl Pts',(6.24436990788039,-62.4538823482276,
39.8576902534424));
#200813=CARTESIAN_POINT('Ctrl Pts',(6.37126553604051,-62.4410124550018,
39.8573998014387));
#200814=CARTESIAN_POINT('Ctrl Pts',(6.35995915837782,-62.3334394572619,
39.92499));
#200815=CARTESIAN_POINT('Origin',(6.55408556365926,-62.5037563256535,40.22725));
#200816=CARTESIAN_POINT('Origin',(-0.315760701779421,-0.033187787087479,
39.116));
#200817=CARTESIAN_POINT('Origin',(5.95633285891191,-59.7081718144893,39.116));
#200818=CARTESIAN_POINT('Origin',(5.64744126194172E-15,5.8588708947011E-15,
40.22725));
#200819=CARTESIAN_POINT('Origin',(6.58439859103008,-62.5005702980931,40.22725));
#200820=CARTESIAN_POINT('Ctrl Pts',(5.95633285891191,-59.7081718144893,
38.989));
#200821=CARTESIAN_POINT('Ctrl Pts',(6.08282634913978,-59.6948768129328,
38.989));
#200822=CARTESIAN_POINT('Ctrl Pts',(6.08263699811363,-59.6948967145276,
39.1161901092323));
#200823=CARTESIAN_POINT('Ctrl Pts',(5.93388096803615,-59.4923596726254,
38.989));
#200824=CARTESIAN_POINT('Ctrl Pts',(6.06016553348747,-59.479278473332,38.9892298989736));
#200825=CARTESIAN_POINT('Ctrl Pts',(6.06449945282236,-59.5223294958622,
39.1161900493203));
#200826=CARTESIAN_POINT('Ctrl Pts',(5.91250946061109,-59.286909633363,39.1034966344368));
#200827=CARTESIAN_POINT('Ctrl Pts',(6.03858743331853,-59.2739813341604,
39.103831410258));
#200828=CARTESIAN_POINT('Ctrl Pts',(6.04723285085757,-59.3580487495167,
39.2077528789598));
#200829=CARTESIAN_POINT('Ctrl Pts',(5.90061356181238,-59.1725467709678,
39.2875012672119));
#200830=CARTESIAN_POINT('Ctrl Pts',(6.0265856432641,-59.1597945531718,39.2878045257868));
#200831=CARTESIAN_POINT('Ctrl Pts',(6.03762143444287,-59.2666022295038,
39.35490152959));
#200832=CARTESIAN_POINT('Origin',(5.91130048050323,-59.2797173540686,39.3548010137695));
#200833=CARTESIAN_POINT('Ctrl Pts',(6.87697683366544,-62.3873926810691,
39.8576902534424));
#200834=CARTESIAN_POINT('Ctrl Pts',(6.75017837817581,-62.4011871104969,
39.8573998014387));
#200835=CARTESIAN_POINT('Ctrl Pts',(6.73887200051313,-62.2936141127569,
39.92499));
#200836=CARTESIAN_POINT('Ctrl Pts',(6.88173199854475,-62.4326397213341,
39.9304984902491));
#200837=CARTESIAN_POINT('Ctrl Pts',(6.76854981002449,-62.4292221586344,
39.9052171569777));
#200838=CARTESIAN_POINT('Ctrl Pts',(6.74362747387393,-62.338859419464,39.967204972659));
#200839=CARTESIAN_POINT('Ctrl Pts',(6.8600064360469,-62.4814742414947,40.0043437678662));
#200840=CARTESIAN_POINT('Ctrl Pts',(6.7685470727683,-62.4674993676294,39.966162857764));
#200841=CARTESIAN_POINT('Ctrl Pts',(6.73309031164146,-62.3865194274371,
40.0100243556237));
#200842=CARTESIAN_POINT('Ctrl Pts',(6.76243636205699,-62.5644789380883,
40.1194874821987));
#200843=CARTESIAN_POINT('Ctrl Pts',(6.71251593157865,-62.5342007968287,
40.0627551483143));
#200844=CARTESIAN_POINT('Ctrl Pts',(6.6797983584025,-62.4648696125161,40.0767884282376));
#200845=CARTESIAN_POINT('Ctrl Pts',(6.6836031020277,-62.5984172531142,40.1599502015384));
#200846=CARTESIAN_POINT('Ctrl Pts',(6.65585031610595,-62.5638265480122,
40.1002449453885));
#200847=CARTESIAN_POINT('Ctrl Pts',(6.63528943158912,-62.4951999029129,
40.10025));
#200848=CARTESIAN_POINT('Ctrl Pts',(6.59568250079866,-62.6076796697354,
40.1599502534424));
#200849=CARTESIAN_POINT('Ctrl Pts',(6.59177408464754,-62.5705801176609,
40.10025));
#200850=CARTESIAN_POINT('Ctrl Pts',(6.58439859103009,-62.5005702980931,
40.10025));
#200851=CARTESIAN_POINT('Origin',(6.8651762812249,-62.2803389979219,39.92499));
#200852=CARTESIAN_POINT('Origin',(5.8926788020772,-59.1025439185011,39.6398955069324));
#200853=CARTESIAN_POINT('Origin',(5.8740571235785,-58.925370482788,39.92499));
#200854=CARTESIAN_POINT('Origin',(6.84655462836501,-62.1031658061012,39.6398955068271));
#200855=CARTESIAN_POINT('Origin',(6.82793297553329,-61.925992614092,39.3548010137695));
#200856=CARTESIAN_POINT('Ctrl Pts',(5.86337364149561,-58.8181995570485,
39.8576902534424));
#200857=CARTESIAN_POINT('Ctrl Pts',(5.98915458643775,-58.8054696185321,
39.8579948730703));
#200858=CARTESIAN_POINT('Ctrl Pts',(6.00036140429027,-58.912095367953,39.92499));
#200859=CARTESIAN_POINT('Ctrl Pts',(5.85862481136451,-58.7730123682041,
39.930402071123));
#200860=CARTESIAN_POINT('Ctrl Pts',(5.97090589422215,-58.777211762863,39.9058915297377));
#200861=CARTESIAN_POINT('Ctrl Pts',(5.99561184840486,-58.8669063622634,
39.9671523786019));
#200862=CARTESIAN_POINT('Ctrl Pts',(5.88025640567557,-58.7244521481307,
40.0043257306694));
#200863=CARTESIAN_POINT('Ctrl Pts',(5.97111833475366,-58.7389107566976,
39.9667894847838));
#200864=CARTESIAN_POINT('Ctrl Pts',(6.00616078842874,-58.819513158931,40.0100138975201));
#200865=CARTESIAN_POINT('Ctrl Pts',(5.97763489331428,-58.642244989525,40.1195533054856));
#200866=CARTESIAN_POINT('Ctrl Pts',(6.02730636094602,-58.6726343357862,
40.0630813209234));
#200867=CARTESIAN_POINT('Ctrl Pts',(6.05959099741146,-58.7419259266991,
40.076826594242));
#200868=CARTESIAN_POINT('Ctrl Pts',(6.05629725705608,-58.608838606668,40.1599502027522));
#200869=CARTESIAN_POINT('Ctrl Pts',(6.08390124328572,-58.6434504949695,
40.1002552791541));
#200870=CARTESIAN_POINT('Ctrl Pts',(6.10418993496999,-58.712100199295,40.10025));
#200871=CARTESIAN_POINT('Ctrl Pts',(6.14377718965303,-58.5996668978649,
40.1599502534424));
#200872=CARTESIAN_POINT('Ctrl Pts',(6.14766703046152,-58.6367684021393,
40.10025));
#200873=CARTESIAN_POINT('Ctrl Pts',(6.15500747092297,-58.7067819056643,
40.10025));
#200874=CARTESIAN_POINT('Origin',(6.15500747092297,-58.7067819056643,40.22725));
#200875=CARTESIAN_POINT('Ctrl Pts',(6.78290064323541,-61.4975385923862,
38.989));
#200876=CARTESIAN_POINT('Ctrl Pts',(6.65640765888775,-61.5108335407726,
38.989));
#200877=CARTESIAN_POINT('Ctrl Pts',(6.65659650327857,-61.5108136924273,
39.1161896013266));
#200878=CARTESIAN_POINT('Ctrl Pts',(6.80580235504215,-61.7133034041536,
38.989));
#200879=CARTESIAN_POINT('Ctrl Pts',(6.67910686401115,-61.7268068187933,
38.988776927546));
#200880=CARTESIAN_POINT('Ctrl Pts',(6.67473401011708,-61.6833805404075,
39.1161898821847));
#200881=CARTESIAN_POINT('Ctrl Pts',(6.82760223531318,-61.9187082819379,
39.1034967087243));
#200882=CARTESIAN_POINT('Ctrl Pts',(6.70071049691542,-61.9323562021257,
39.1031720232707));
#200883=CARTESIAN_POINT('Ctrl Pts',(6.69200060426978,-61.8476612078244,
39.2077529614998));
#200884=CARTESIAN_POINT('Ctrl Pts',(6.8397366303024,-62.0330459552232,39.2875012672119));
#200885=CARTESIAN_POINT('Ctrl Pts',(6.71274549238803,-62.046864024595,39.2872087095507));
#200886=CARTESIAN_POINT('Ctrl Pts',(6.7016119927524,-61.9391074595193,39.3549017048227));
#200887=CARTESIAN_POINT('Origin',(6.78290064323541,-61.4975385923862,39.116));
#200888=CARTESIAN_POINT('Origin',(5.67080826956262E-15,5.1943719780809E-15,
40.22725));
#200889=CARTESIAN_POINT('Origin',(6.1853204982938,-58.7035958781039,40.22725));
#200890=CARTESIAN_POINT('Origin',(0.995615674755264,-6.4352002018204,39.116));
#200891=CARTESIAN_POINT('Origin',(6.74099917688066,-61.0983782637179,39.1160373285285));
#200892=CARTESIAN_POINT('Ctrl Pts',(6.17403490859001,-58.5964866834551,
40.1599502534424));
#200893=CARTESIAN_POINT('Ctrl Pts',(6.17794390662153,-58.6335861742242,
40.10025));
#200894=CARTESIAN_POINT('Ctrl Pts',(6.1853204982938,-58.7035958781039,40.10025));
#200895=CARTESIAN_POINT('Ctrl Pts',(6.26121185652522,-58.5873013840786,
40.1599500566036));
#200896=CARTESIAN_POINT('Ctrl Pts',(6.2414554165825,-58.6268910424075,40.1002551305369));
#200897=CARTESIAN_POINT('Ctrl Pts',(6.23596000968374,-58.6982507756602,
40.10025));
#200898=CARTESIAN_POINT('Ctrl Pts',(6.34441620808589,-58.603224495399,40.1203070619047));
#200899=CARTESIAN_POINT('Ctrl Pts',(6.30249747592711,-58.6433169201088,
40.06370986845));
#200900=CARTESIAN_POINT('Ctrl Pts',(6.28536729223303,-58.7177256636152,
40.0772636213363));
#200901=CARTESIAN_POINT('Ctrl Pts',(6.45770985055653,-58.6635810738165,
40.0046102245801));
#200902=CARTESIAN_POINT('Ctrl Pts',(6.37191831988761,-58.6966524426403,
39.9670001894012));
#200903=CARTESIAN_POINT('Ctrl Pts',(6.35432657855794,-58.7827411889911,
40.0101788811209));
#200904=CARTESIAN_POINT('Ctrl Pts',(6.48899861096521,-58.7067768761601,
39.9303710930186));
#200905=CARTESIAN_POINT('Ctrl Pts',(6.38003592347219,-58.7342263230566,
39.9058663574114));
#200906=CARTESIAN_POINT('Ctrl Pts',(6.37452670784946,-58.8271002111743,
39.967134470637));
#200907=CARTESIAN_POINT('Ctrl Pts',(6.49374646112722,-58.7519447039089,
39.8576902534424));
#200908=CARTESIAN_POINT('Ctrl Pts',(6.36806742857306,-58.7656442740271,
39.8579948730703));
#200909=CARTESIAN_POINT('Ctrl Pts',(6.37927424642559,-58.8722700234481,
39.92499));
#200910=CARTESIAN_POINT('Origin',(6.50557852713736,-58.8589949086131,39.92499));
#200911=CARTESIAN_POINT('Origin',(6.73632490881042,-61.0544000804059,39.1925554488841));
#200912=CARTESIAN_POINT('Origin',(6.72777047351104,-60.9730100652055,39.3343017080178));
#200913=CARTESIAN_POINT('Origin',(6.5242002055762,-59.036168344314,39.639895506921));
#200914=CARTESIAN_POINT('Origin',(6.54282188406209,-59.2133417798936,39.3548010137695));
#200915=CARTESIAN_POINT('Ctrl Pts',(6.69328024897436,-60.6448574988554,
39.3978017080178));
#200916=CARTESIAN_POINT('Ctrl Pts',(6.56697596826259,-60.6581326136904,
39.3978017080178));
#200917=CARTESIAN_POINT('Ctrl Pts',(6.56697596826259,-60.6581326136904,
39.5248017080178));
#200918=CARTESIAN_POINT('Ctrl Pts',(6.70245599674994,-60.7343993681214,
39.3978017080178));
#200919=CARTESIAN_POINT('Ctrl Pts',(6.57637578951157,-60.7475659388567,
39.3980355775177));
#200920=CARTESIAN_POINT('Ctrl Pts',(6.58108878091675,-60.7924070567563,
39.5248015517192));
#200921=CARTESIAN_POINT('Ctrl Pts',(6.71113417453894,-60.819067758858,39.3484893995498));
#200922=CARTESIAN_POINT('Ctrl Pts',(6.58530836180071,-60.8325536871448,
39.348943830343));
#200923=CARTESIAN_POINT('Ctrl Pts',(6.59443344928427,-60.9193730951256,
39.4508333155599));
#200924=CARTESIAN_POINT('Ctrl Pts',(6.7157078966939,-60.8636883187845,39.2708017080178));
#200925=CARTESIAN_POINT('Ctrl Pts',(6.59002106156447,-60.8773920302461,
39.2710850691866));
#200926=CARTESIAN_POINT('Ctrl Pts',(6.60146619279927,-60.9862851800404,
39.3343017080178));
#200927=CARTESIAN_POINT('Origin',(6.69328024897435,-60.6448574988554,39.5248017080178));
#200928=CARTESIAN_POINT('Ctrl Pts',(6.53099325080036,-59.1062911958297,
39.2875012672119));
#200929=CARTESIAN_POINT('Ctrl Pts',(6.40512264090967,-59.1200087114582,
39.2878045257519));
#200930=CARTESIAN_POINT('Ctrl Pts',(6.41653455700107,-59.2267768430462,
39.3549015218348));
#200931=CARTESIAN_POINT('Ctrl Pts',(6.54313486548324,-59.2206299794251,
39.1034938540228));
#200932=CARTESIAN_POINT('Ctrl Pts',(6.41712406698121,-59.2341972766239,
39.1038286278807));
#200933=CARTESIAN_POINT('Ctrl Pts',(6.42614611919711,-59.3182247474317,
39.2077506434029));
#200934=CARTESIAN_POINT('Ctrl Pts',(6.56494601397037,-59.426035450364,38.989));
#200935=CARTESIAN_POINT('Ctrl Pts',(6.43870134519723,-59.4394961352161,
38.9892298954611));
#200936=CARTESIAN_POINT('Ctrl Pts',(6.4434128584844,-59.482506795581,39.1161900347291));
#200937=CARTESIAN_POINT('Ctrl Pts',(6.58785426247077,-59.6417962403143,
38.989));
#200938=CARTESIAN_POINT('Ctrl Pts',(6.461360786852,-59.6550912403353,38.989));
#200939=CARTESIAN_POINT('Ctrl Pts',(6.46155012324721,-59.6550713402783,
39.1161900945647));
#200940=CARTESIAN_POINT('Origin',(6.58785426247077,-59.6417962403143,39.116));
#200941=CARTESIAN_POINT('Origin',(0.979147644052797,-6.27851735587382,39.5248017080178));
#200942=CARTESIAN_POINT('Origin',(6.67747469700926,-60.4944777170594,39.5248017080178));
#200943=CARTESIAN_POINT('Origin',(0.976568823008617,-6.25398151259724,39.116));
#200944=CARTESIAN_POINT('Origin',(6.62985850077836,-60.0409538388296,39.116040271385));
#200945=CARTESIAN_POINT('Ctrl Pts',(6.65505462397376,-60.2756459899119,
39.2708017080178));
#200946=CARTESIAN_POINT('Ctrl Pts',(6.52822907310758,-60.2894805317162,
39.27051194648));
#200947=CARTESIAN_POINT('Ctrl Pts',(6.51668018436727,-60.1796001951995,
39.3343017080178));
#200948=CARTESIAN_POINT('Ctrl Pts',(6.65964099131233,-60.3204176712045,
39.3487519301186));
#200949=CARTESIAN_POINT('Ctrl Pts',(6.53290851690466,-60.3340024654484,
39.3482879463988));
#200950=CARTESIAN_POINT('Ctrl Pts',(6.52373669508343,-60.2467384099282,
39.4512271261633));
#200951=CARTESIAN_POINT('Ctrl Pts',(6.6683304315064,-60.4052373806432,39.3978017080178));
#200952=CARTESIAN_POINT('Ctrl Pts',(6.54178440911728,-60.4184509388129,
39.3975673827383));
#200953=CARTESIAN_POINT('Ctrl Pts',(6.53710513959985,-60.3739306632435,
39.5248015355181));
#200954=CARTESIAN_POINT('Ctrl Pts',(6.67747469700926,-60.4944777170594,
39.3978017080178));
#200955=CARTESIAN_POINT('Ctrl Pts',(6.5511704162975,-60.5077528318944,39.3978017080178));
#200956=CARTESIAN_POINT('Ctrl Pts',(6.55117041629749,-60.5077528318944,
39.5248017080178));
#200957=CARTESIAN_POINT('Origin',(6.64298446507904,-60.1663250803646,39.3343017080178));
#200958=CARTESIAN_POINT('Origin',(6.6344810469906,-60.085420458681,39.1934008533549));
#200959=CARTESIAN_POINT('Origin',(-0.317499999708329,-61.4240753804096,
39.1925554495087));
#200960=CARTESIAN_POINT('Origin',(-0.31755169001553,-61.4683012396086,39.1160373285286));
#200961=CARTESIAN_POINT('Origin',(-0.317500000000209,-61.3422370451705,
39.3343017080178));
#200962=CARTESIAN_POINT('Ctrl Pts',(-0.316930737396123,-61.2322532920972,
39.2708017080178));
#200963=CARTESIAN_POINT('Ctrl Pts',(-0.190500000000209,-61.2327440814645,
39.2710850691866));
#200964=CARTESIAN_POINT('Ctrl Pts',(-0.190500000000209,-61.3422370451705,
39.3343017080178));
#200965=CARTESIAN_POINT('Ctrl Pts',(-0.317046579199844,-61.1872475084174,
39.3487519293518));
#200966=CARTESIAN_POINT('Ctrl Pts',(-0.190500000000221,-61.187506454175,
39.3492068662925));
#200967=CARTESIAN_POINT('Ctrl Pts',(-0.190500000000208,-61.2747290395312,
39.451227124874));
#200968=CARTESIAN_POINT('Ctrl Pts',(-0.317266596913697,-61.1019842137032,
39.3978017080178));
#200969=CARTESIAN_POINT('Ctrl Pts',(-0.190500000000202,-61.1018997758114,
39.3980347781183));
#200970=CARTESIAN_POINT('Ctrl Pts',(-0.190500000000208,-61.146836207171,
39.5248015355195));
#200971=CARTESIAN_POINT('Ctrl Pts',(-0.317500000000208,-61.0122769227456,
39.3978017080178));
#200972=CARTESIAN_POINT('Ctrl Pts',(-0.190500000000207,-61.0122769227456,
39.3978017080178));
#200973=CARTESIAN_POINT('Ctrl Pts',(-0.190500000000207,-61.0122769227456,
39.5248017080178));
#200974=CARTESIAN_POINT('Origin',(-0.317500000000208,-61.0122769227456,
39.5248017080178));
#200975=CARTESIAN_POINT('Origin',(-0.317499999999994,1.10854532508269E-15,
39.116));
#200976=CARTESIAN_POINT('Origin',(-0.317500000000211,-61.8696548221181,
39.116));
#200977=CARTESIAN_POINT('Origin',(-0.317499999999994,1.10854532508269E-15,
39.5248017080178));
#200978=CARTESIAN_POINT('Origin',(-0.317500000000207,-60.8610688070707,
39.5248017080178));
#200979=CARTESIAN_POINT('Ctrl Pts',(-0.318048871877342,-62.4081695979768,
39.2875012672119));
#200980=CARTESIAN_POINT('Ctrl Pts',(-0.190309034175712,-62.4086377819835,
39.287208709576));
#200981=CARTESIAN_POINT('Ctrl Pts',(-0.190500142125266,-62.3003077603773,
39.3549016990123));
#200982=CARTESIAN_POINT('Ctrl Pts',(-0.317932489890162,-62.2931881445371,
39.1034939173931));
#200983=CARTESIAN_POINT('Ctrl Pts',(-0.190309294368566,-62.2934975005725,
39.1031692336334));
#200984=CARTESIAN_POINT('Ctrl Pts',(-0.190500141995678,-62.2083564003264,
39.2077507202293));
#200985=CARTESIAN_POINT('Ctrl Pts',(-0.317722686167617,-62.0866281564673,
38.989));
#200986=CARTESIAN_POINT('Ctrl Pts',(-0.190309769570069,-62.0868143053097,
38.9887769311176));
#200987=CARTESIAN_POINT('Ctrl Pts',(-0.190500141762077,-62.043169520538,
39.1161898712916));
#200988=CARTESIAN_POINT('Ctrl Pts',(-0.31750000000021,-61.8696548221181,
38.989));
#200989=CARTESIAN_POINT('Ctrl Pts',(-0.190310267889348,-61.8696548221181,
38.989));
#200990=CARTESIAN_POINT('Ctrl Pts',(-0.190500141514125,-61.8696548221181,
39.1161895903855));
#200991=CARTESIAN_POINT('Origin',(-0.317500000000212,-62.3004688883554,
39.3548010137695));
#200992=CARTESIAN_POINT('Ctrl Pts',(-0.317500000000207,-60.8610688070707,
39.3978017080178));
#200993=CARTESIAN_POINT('Ctrl Pts',(-0.190500000000207,-60.8610688070707,
39.3978017080178));
#200994=CARTESIAN_POINT('Ctrl Pts',(-0.190500000000207,-60.8610688070707,
39.5248017080178));
#200995=CARTESIAN_POINT('Ctrl Pts',(-0.317734773760476,-60.7710583184321,
39.3978017080178));
#200996=CARTESIAN_POINT('Ctrl Pts',(-0.190500000000205,-60.770971734242,
39.3975666025021));
#200997=CARTESIAN_POINT('Ctrl Pts',(-0.190500000000206,-60.7260547307358,
39.5248015517178));
#200998=CARTESIAN_POINT('Ctrl Pts',(-0.317958617919243,-60.6859465754578,
39.3484894016716));
#200999=CARTESIAN_POINT('Ctrl Pts',(-0.190500000000603,-60.6862105562563,
39.3480259000043));
#201000=CARTESIAN_POINT('Ctrl Pts',(-0.190500000000206,-60.5983892955408,
39.4508333188947));
#201001=CARTESIAN_POINT('Ctrl Pts',(-0.318076890623573,-60.6410923272405,
39.2708017080178));
#201002=CARTESIAN_POINT('Ctrl Pts',(-0.190500000000206,-60.6415942020422,
39.27051194648));
#201003=CARTESIAN_POINT('Ctrl Pts',(-0.190500000000206,-60.5311086139135,
39.3343017080178));
#201004=CARTESIAN_POINT('Origin',(-0.317500000000206,-60.5311086139135,
39.3343017080178));
#201005=CARTESIAN_POINT('Origin',(-0.317499999976942,-62.4786179998487,
39.6398955068185));
#201006=CARTESIAN_POINT('Origin',(-0.317500000000213,-62.6567671111299,
39.92499));
#201007=CARTESIAN_POINT('Origin',(-0.31749999999388,-60.4497583458792,39.1934008539947));
#201008=CARTESIAN_POINT('Origin',(-0.317550804320733,-60.4050521322802,
39.1160402713848));
#201009=CARTESIAN_POINT('Ctrl Pts',(-0.015266117311081,-62.9541448057648,
40.1599502534424));
#201010=CARTESIAN_POINT('Ctrl Pts',(-0.0152570710388482,-62.9168399481843,
40.10025));
#201011=CARTESIAN_POINT('Ctrl Pts',(-0.0152400000002138,-62.8464427007196,
40.10025));
#201012=CARTESIAN_POINT('Ctrl Pts',(-0.103381504925368,-62.9541233134297,
40.1599500538463));
#201013=CARTESIAN_POINT('Ctrl Pts',(-0.0794415635237479,-62.9168211560341,
40.100244835349));
#201014=CARTESIAN_POINT('Ctrl Pts',(-0.0662446030561434,-62.8464212442881,
40.10025));
#201015=CARTESIAN_POINT('Ctrl Pts',(-0.184683583688078,-62.9290872705826,
40.1202442001037));
#201016=CARTESIAN_POINT('Ctrl Pts',(-0.138547994784559,-62.8936771137448,
40.0633873868015));
#201017=CARTESIAN_POINT('Ctrl Pts',(-0.11330556745179,-62.8213855864655,
40.0772271723537));
#201018=CARTESIAN_POINT('Ctrl Pts',(-0.29134099263186,-62.8564203507742,
40.0045995998164));
#201019=CARTESIAN_POINT('Ctrl Pts',(-0.20191035119152,-62.8329175802742,
39.9663485808317));
#201020=CARTESIAN_POINT('Ctrl Pts',(-0.175042741958046,-62.7487193609389,
40.0101727202466));
#201021=CARTESIAN_POINT('Ctrl Pts',(-0.318045276842851,-62.8099434033761,
39.9304654349858));
#201022=CARTESIAN_POINT('Ctrl Pts',(-0.205831635643045,-62.7947175425015,
39.9051900162937));
#201023=CARTESIAN_POINT('Ctrl Pts',(-0.190500000000215,-62.7022409210455,
39.9671857458166));
#201024=CARTESIAN_POINT('Ctrl Pts',(-0.318045750793259,-62.7644678366119,
39.8576902534424));
#201025=CARTESIAN_POINT('Ctrl Pts',(-0.190500000000209,-62.7649326510149,
39.8573998014387));
#201026=CARTESIAN_POINT('Ctrl Pts',(-0.190500000000213,-62.6567671111299,
39.92499));
#201027=CARTESIAN_POINT('Origin',(-0.0152400000002138,-62.8464427007196,
40.22725));
#201028=CARTESIAN_POINT('Origin',(-0.317499999999994,1.10854532508269E-15,
39.116));
#201029=CARTESIAN_POINT('Origin',(-0.317500000000204,-60.0036905223731,
39.116));
#201030=CARTESIAN_POINT('Origin',(-3.02076666443335E-17,1.64889592811714E-16,
40.22725));
#201031=CARTESIAN_POINT('Origin',(0.0152399999997862,-62.8464427007196,
40.22725));
#201032=CARTESIAN_POINT('Ctrl Pts',(-0.317500000000204,-60.0036905223731,
38.989));
#201033=CARTESIAN_POINT('Ctrl Pts',(-0.19030974826544,-60.003690522373,
38.989));
#201034=CARTESIAN_POINT('Ctrl Pts',(-0.190500142289733,-60.0036905223731,
39.1161901092321));
#201035=CARTESIAN_POINT('Ctrl Pts',(-0.317270385524616,-59.7867137603524,
38.989));
#201036=CARTESIAN_POINT('Ctrl Pts',(-0.190310262476514,-59.786904552798,
38.989229898976));
#201037=CARTESIAN_POINT('Ctrl Pts',(-0.190500142032665,-59.8301727552495,
39.1161900493201));
#201038=CARTESIAN_POINT('Ctrl Pts',(-0.317049440713822,-59.5801552670728,
39.1034966344368));
#201039=CARTESIAN_POINT('Ctrl Pts',(-0.190310761081983,-59.5804765271857,
39.1038314102564));
#201040=CARTESIAN_POINT('Ctrl Pts',(-0.190500141785309,-59.664987104655,
39.2077528789601));
#201041=CARTESIAN_POINT('Ctrl Pts',(-0.316925998273249,-59.4651754363832,
39.2875012672119));
#201042=CARTESIAN_POINT('Ctrl Pts',(-0.19031103533518,-59.4656607446593,
39.2878045257868));
#201043=CARTESIAN_POINT('Ctrl Pts',(-0.190500141647105,-59.5730368716576,
39.3549015295899));
#201044=CARTESIAN_POINT('Origin',(-0.317500000000203,-59.5728760150042,
39.3548010137695));
#201045=CARTESIAN_POINT('Ctrl Pts',(0.318045750792832,-62.7644678366119,
39.8576902534424));
#201046=CARTESIAN_POINT('Ctrl Pts',(0.190499999999787,-62.7649326510149,
39.8573998014387));
#201047=CARTESIAN_POINT('Ctrl Pts',(0.190499999999787,-62.6567671111299,
39.92499));
#201048=CARTESIAN_POINT('Ctrl Pts',(0.318045262794968,-62.8099640589334,
39.930498490249));
#201049=CARTESIAN_POINT('Ctrl Pts',(0.205840330722736,-62.794734457763,
39.9052171569785));
#201050=CARTESIAN_POINT('Ctrl Pts',(0.190499999999787,-62.7022616416336,
39.9672049726603));
#201051=CARTESIAN_POINT('Ctrl Pts',(0.291334117855151,-62.8562601188215,
40.0043437678664));
#201052=CARTESIAN_POINT('Ctrl Pts',(0.201836550627533,-62.8328016940825,
39.9661628577643));
#201053=CARTESIAN_POINT('Ctrl Pts',(0.175038734051849,-62.7485591297232,
40.0100243556236));
#201054=CARTESIAN_POINT('Ctrl Pts',(0.18562218956022,-62.928611257107,40.1194874821985));
#201055=CARTESIAN_POINT('Ctrl Pts',(0.139140155999885,-62.8932808767899,
40.062755148314));
#201056=CARTESIAN_POINT('Ctrl Pts',(0.113848895265595,-62.8209095783125,
40.0767884282376));
#201057=CARTESIAN_POINT('Ctrl Pts',(0.10367326646258,-62.9541233349674,
40.1599502015391));
#201058=CARTESIAN_POINT('Ctrl Pts',(0.0796882264534641,-62.9168211653022,
40.1002449453869));
#201059=CARTESIAN_POINT('Ctrl Pts',(0.0664134143648399,-62.8464212664863,
40.10025));
#201060=CARTESIAN_POINT('Ctrl Pts',(0.0152661173106522,-62.9541448057648,
40.1599502534424));
#201061=CARTESIAN_POINT('Ctrl Pts',(0.0152570710384197,-62.9168399481843,
40.10025));
#201062=CARTESIAN_POINT('Ctrl Pts',(0.0152399999997859,-62.8464427007196,
40.10025));
#201063=CARTESIAN_POINT('Origin',(0.317499999999787,-62.6567671111299,39.92499));
#201064=CARTESIAN_POINT('Origin',(-0.31749999997078,-59.3947266586231,39.639895506931));
#201065=CARTESIAN_POINT('Origin',(-0.317500000000201,-59.2165773020941,
39.92499));
#201066=CARTESIAN_POINT('Origin',(0.317499999978187,-62.4786179998349,39.6398955068271));
#201067=CARTESIAN_POINT('Origin',(0.317499999999788,-62.3004688883555,39.3548010137695));
#201068=CARTESIAN_POINT('Ctrl Pts',(-0.316922544675889,-59.1088767419348,
39.8576902534424));
#201069=CARTESIAN_POINT('Ctrl Pts',(-0.190500000000201,-59.1093642282367,
39.8579948730703));
#201070=CARTESIAN_POINT('Ctrl Pts',(-0.190500000000201,-59.2165773020941,
39.92499));
#201071=CARTESIAN_POINT('Ctrl Pts',(-0.316922012809372,-59.0634407053228,
39.9304020711232));
#201072=CARTESIAN_POINT('Ctrl Pts',(-0.205694973740961,-59.0793536643045,
39.9058915297389));
#201073=CARTESIAN_POINT('Ctrl Pts',(-0.190500000000201,-59.1711393827293,
39.9671523786037));
#201074=CARTESIAN_POINT('Ctrl Pts',(-0.290332993455254,-59.0174076205277,
40.0043257306692));
#201075=CARTESIAN_POINT('Ctrl Pts',(-0.201480151666078,-59.0412846811398,
39.9667894847832));
#201076=CARTESIAN_POINT('Ctrl Pts',(-0.175054909460048,-59.1251084688124,
40.0100138975199));
#201077=CARTESIAN_POINT('Ctrl Pts',(-0.184894967401715,-58.9458296250061,
40.1195533054858));
#201078=CARTESIAN_POINT('Ctrl Pts',(-0.138672156931401,-58.9812445774289,
40.0630813209239));
#201079=CARTESIAN_POINT('Ctrl Pts',(-0.113807322597838,-59.053531245193,
40.0768265942422));
#201080=CARTESIAN_POINT('Ctrl Pts',(-0.103171606455975,-58.9208287018091,
40.1599502027518));
#201081=CARTESIAN_POINT('Ctrl Pts',(-0.0793367652460264,-58.9581363848269,
40.1002552791538));
#201082=CARTESIAN_POINT('Ctrl Pts',(-0.0663350652346691,-59.0285307646513,
40.10025));
#201083=CARTESIAN_POINT('Ctrl Pts',(-0.0152121934561203,-58.9208513795073,
40.1599502534424));
#201084=CARTESIAN_POINT('Ctrl Pts',(-0.0152218248293074,-58.9581562369413,
40.10025));
#201085=CARTESIAN_POINT('Ctrl Pts',(-0.0152400000002007,-59.0285534841296,
40.10025));
#201086=CARTESIAN_POINT('Origin',(-0.0152400000002004,-59.0285534841296,
40.22725));
#201087=CARTESIAN_POINT('Ctrl Pts',(0.31749999999979,-61.8696548221181,
38.989));
#201088=CARTESIAN_POINT('Ctrl Pts',(0.190310256931471,-61.8696548221181,
38.989));
#201089=CARTESIAN_POINT('Ctrl Pts',(0.190500141530038,-61.8696548221181,
39.1161896013266));
#201090=CARTESIAN_POINT('Ctrl Pts',(0.317722689632019,-62.0866315324121,
38.989));
#201091=CARTESIAN_POINT('Ctrl Pts',(0.190309758575691,-62.0868176889529,
38.988776927546));
#201092=CARTESIAN_POINT('Ctrl Pts',(0.190500141778021,-62.043172216566,
39.1161898821848));
#201093=CARTESIAN_POINT('Ctrl Pts',(0.31793249165548,-62.2931898887681,
39.1034967087243));
#201094=CARTESIAN_POINT('Ctrl Pts',(0.190309283350388,-62.2934992458053,
39.1031720232706));
#201095=CARTESIAN_POINT('Ctrl Pts',(0.190500142011646,-62.2083577878513,
39.2077529614998));
#201096=CARTESIAN_POINT('Ctrl Pts',(0.318048871876917,-62.4081695979768,
39.2875012672119));
#201097=CARTESIAN_POINT('Ctrl Pts',(0.190309023146547,-62.4086377820239,
39.2872087095508));
#201098=CARTESIAN_POINT('Ctrl Pts',(0.190500142141246,-62.3003077510787,
39.3549017048227));
#201099=CARTESIAN_POINT('Origin',(0.31749999999979,-61.8696548221181,39.116));
#201100=CARTESIAN_POINT('Origin',(4.1196902326603E-16,-5.86572468760199E-17,
40.22725));
#201101=CARTESIAN_POINT('Origin',(0.0152399999997996,-59.0285534841296,
40.22725));
#201102=CARTESIAN_POINT('Origin',(0.317500000000005,2.1613999771587E-13,
39.116));
#201103=CARTESIAN_POINT('Origin',(0.317551690012274,-61.4683012396062,39.1160373285252));
#201104=CARTESIAN_POINT('Ctrl Pts',(0.0152121934557198,-58.9208513795073,
40.1599502534424));
#201105=CARTESIAN_POINT('Ctrl Pts',(0.0152218248289066,-58.9581562369413,
40.10025));
#201106=CARTESIAN_POINT('Ctrl Pts',(0.0152399999997995,-59.0285534841296,
40.10025));
#201107=CARTESIAN_POINT('Ctrl Pts',(0.102871702177192,-58.9208288705618,
40.1599500566038));
#201108=CARTESIAN_POINT('Ctrl Pts',(0.0790852439331834,-58.9581365422964,
40.100255130536));
#201109=CARTESIAN_POINT('Ctrl Pts',(0.0661608181923067,-59.0285309330218,
40.10025));
#201110=CARTESIAN_POINT('Ctrl Pts',(0.183955833237311,-58.9453619764183,
40.1203070619046));
#201111=CARTESIAN_POINT('Ctrl Pts',(0.138075936735767,-58.9808530699761,
40.0637098684499));
#201112=CARTESIAN_POINT('Ctrl Pts',(0.113261762367961,-59.0530636028226,
40.0772636213363));
#201113=CARTESIAN_POINT('Ctrl Pts',(0.290319860890461,-59.0172303255294,
40.0046102245801));
#201114=CARTESIAN_POINT('Ctrl Pts',(0.201541405841739,-59.0411528690721,
39.9670001894012));
#201115=CARTESIAN_POINT('Ctrl Pts',(0.175047309550988,-59.1249311745757,
40.0101788811209));
#201116=CARTESIAN_POINT('Ctrl Pts',(0.316922027357148,-59.0634600627911,
39.9303710930187));
#201117=CARTESIAN_POINT('Ctrl Pts',(0.20568700036638,-59.0793694364682,
39.905866357411));
#201118=CARTESIAN_POINT('Ctrl Pts',(0.190499999999799,-59.1711586818657,
39.9671344706363));
#201119=CARTESIAN_POINT('Ctrl Pts',(0.316922544675488,-59.1088767419348,
39.8576902534424));
#201120=CARTESIAN_POINT('Ctrl Pts',(0.190499999999799,-59.1093642282366,
39.8579948730703));
#201121=CARTESIAN_POINT('Ctrl Pts',(0.190499999999799,-59.2165773020941,
39.92499));
#201122=CARTESIAN_POINT('Origin',(0.317499999999799,-59.2165773020941,39.92499));
#201123=CARTESIAN_POINT('Origin',(0.317499999994104,-61.4240753793282,39.1925554488844));
#201124=CARTESIAN_POINT('Origin',(0.317499999999791,-61.3422370451705,39.3343017080178));
#201125=CARTESIAN_POINT('Origin',(0.317499999970067,-59.3947266586071,39.639895506921));
#201126=CARTESIAN_POINT('Origin',(0.317499999999798,-59.5728760150042,39.3548010137695));
#201127=CARTESIAN_POINT('Ctrl Pts',(0.317499999999793,-61.0122769227456,
39.3978017080178));
#201128=CARTESIAN_POINT('Ctrl Pts',(0.190499999999793,-61.0122769227456,
39.3978017080178));
#201129=CARTESIAN_POINT('Ctrl Pts',(0.190499999999793,-61.0122769227456,
39.5248017080178));
#201130=CARTESIAN_POINT('Ctrl Pts',(0.317265808076182,-61.1022873990971,
39.3978017080178));
#201131=CARTESIAN_POINT('Ctrl Pts',(0.190499999999776,-61.1022028716704,
39.3980355775177));
#201132=CARTESIAN_POINT('Ctrl Pts',(0.190499999999792,-61.1472909869838,
39.5248015517192));
#201133=CARTESIAN_POINT('Ctrl Pts',(0.31704618912888,-61.1873990841185,
39.3484893995498));
#201134=CARTESIAN_POINT('Ctrl Pts',(0.190500000001004,-61.1876587562325,
39.3489438303426));
#201135=CARTESIAN_POINT('Ctrl Pts',(0.190499999999792,-61.2749563897836,
39.4508333155593));
#201136=CARTESIAN_POINT('Ctrl Pts',(0.316930737395706,-61.2322532920972,
39.2708017080178));
#201137=CARTESIAN_POINT('Ctrl Pts',(0.190499999999785,-61.2327440814646,
39.2710850691866));
#201138=CARTESIAN_POINT('Ctrl Pts',(0.190499999999791,-61.3422370451705,
39.3343017080178));
#201139=CARTESIAN_POINT('Origin',(0.317499999999793,-61.0122769227456,39.5248017080178));
#201140=CARTESIAN_POINT('Ctrl Pts',(0.316925998272845,-59.4651754363832,
39.2875012672119));
#201141=CARTESIAN_POINT('Ctrl Pts',(0.190311049925075,-59.4656607446034,
39.2878045257519));
#201142=CARTESIAN_POINT('Ctrl Pts',(0.190500141624843,-59.5730368592469,
39.3549015218346));
#201143=CARTESIAN_POINT('Ctrl Pts',(0.317049442578974,-59.5801570044831,
39.1034938540228));
#201144=CARTESIAN_POINT('Ctrl Pts',(0.19031077568779,-59.5804782634875,
39.1038286278812));
#201145=CARTESIAN_POINT('Ctrl Pts',(0.190500141763029,-59.6649884842717,
39.2077506434031));
#201146=CARTESIAN_POINT('Ctrl Pts',(0.317270389088641,-59.7867171285936,
38.989));
#201147=CARTESIAN_POINT('Ctrl Pts',(0.190310277118154,-59.7869079131817,
38.9892298954611));
#201148=CARTESIAN_POINT('Ctrl Pts',(0.190500142010347,-59.8301754438924,
39.1161900347287));
#201149=CARTESIAN_POINT('Ctrl Pts',(0.317499999999796,-60.0036905223731,
38.989));
#201150=CARTESIAN_POINT('Ctrl Pts',(0.190309762954753,-60.0036905223731,
38.989));
#201151=CARTESIAN_POINT('Ctrl Pts',(0.190500142267369,-60.0036905223731,
39.1161900945644));
#201152=CARTESIAN_POINT('Origin',(0.317499999999796,-60.0036905223731,39.116));
#201153=CARTESIAN_POINT('Origin',(0.317500000000005,2.10877617033113E-13,
39.5248017080178));
#201154=CARTESIAN_POINT('Origin',(0.317499999999793,-60.8610688070707,39.5248017080178));
#201155=CARTESIAN_POINT('Origin',(0.317500000000005,2.10053551406057E-13,
39.116));
#201156=CARTESIAN_POINT('Origin',(0.317550804320415,-60.4050521322802,39.1160402713848));
#201157=CARTESIAN_POINT('Ctrl Pts',(0.31807689062316,-60.6410923272405,
39.2708017080178));
#201158=CARTESIAN_POINT('Ctrl Pts',(0.1904999999998,-60.6415942020422,39.27051194648));
#201159=CARTESIAN_POINT('Ctrl Pts',(0.190499999999794,-60.5311086139135,
39.3343017080178));
#201160=CARTESIAN_POINT('Ctrl Pts',(0.317958218318564,-60.6860981505083,
39.3487519301186));
#201161=CARTESIAN_POINT('Ctrl Pts',(0.190499999998582,-60.6863613750267,
39.348287946399));
#201162=CARTESIAN_POINT('Ctrl Pts',(0.190499999999794,-60.598616644694,
39.4512271261644));
#201163=CARTESIAN_POINT('Ctrl Pts',(0.317733982967334,-60.771361502534,
39.3978017080178));
#201164=CARTESIAN_POINT('Ctrl Pts',(0.190499999999793,-60.7712750142006,
39.3975673827397));
#201165=CARTESIAN_POINT('Ctrl Pts',(0.190499999999794,-60.7265095085063,
39.5248015355181));
#201166=CARTESIAN_POINT('Ctrl Pts',(0.317499999999793,-60.8610688070707,
39.3978017080178));
#201167=CARTESIAN_POINT('Ctrl Pts',(0.190499999999793,-60.8610688070707,
39.3978017080178));
#201168=CARTESIAN_POINT('Ctrl Pts',(0.190499999999793,-60.8610688070707,
39.5248017080178));
#201169=CARTESIAN_POINT('Origin',(0.317499999999794,-60.5311086139135,39.3343017080178));
#201170=CARTESIAN_POINT('Origin',(0.317500000300197,-60.4497583469878,39.1934008533546));
#201171=CARTESIAN_POINT('Origin',(-6.73632490863922,-61.0544000815109,39.1925554495083));
#201172=CARTESIAN_POINT('Origin',(-6.74099917688029,-61.0983782637176,39.1160373285273));
#201173=CARTESIAN_POINT('Origin',(-6.72777047351144,-60.9730100652054,39.3343017080178));
#201174=CARTESIAN_POINT('Ctrl Pts',(-6.7157078966943,-60.8636883187844,
39.2708017080178));
#201175=CARTESIAN_POINT('Ctrl Pts',(-6.59002106156486,-60.877392030246,
39.2710850691866));
#201176=CARTESIAN_POINT('Ctrl Pts',(-6.60146619279967,-60.9862851800404,
39.3343017080178));
#201177=CARTESIAN_POINT('Ctrl Pts',(-6.71111871849837,-60.8189169727309,
39.3487519293517));
#201178=CARTESIAN_POINT('Ctrl Pts',(-6.58529244190256,-60.832402219412,
39.3492068662929));
#201179=CARTESIAN_POINT('Ctrl Pts',(-6.59440968471164,-60.9191469903167,
39.4512271248736));
#201180=CARTESIAN_POINT('Ctrl Pts',(-6.70242508976246,-60.7340977611528,
39.3978017080178));
#201181=CARTESIAN_POINT('Ctrl Pts',(-6.57634410736735,-60.7472645033898,
39.3980347781178));
#201182=CARTESIAN_POINT('Ctrl Pts',(-6.58104124348259,-60.7919547682786,
39.524801535519));
#201183=CARTESIAN_POINT('Ctrl Pts',(-6.69328024897476,-60.6448574988554,
39.3978017080178));
#201184=CARTESIAN_POINT('Ctrl Pts',(-6.56697596826299,-60.6581326136904,
39.3978017080178));
#201185=CARTESIAN_POINT('Ctrl Pts',(-6.56697596826298,-60.6581326136904,
39.5248017080178));
#201186=CARTESIAN_POINT('Origin',(-6.69328024897475,-60.6448574988554,39.5248017080178));
#201187=CARTESIAN_POINT('Origin',(-0.315760701779421,0.0331877870874811,
39.116));
#201188=CARTESIAN_POINT('Origin',(-6.78290064323581,-61.4975385923862,39.116));
#201189=CARTESIAN_POINT('Origin',(-0.315760701779421,0.0331877870874811,
39.5248017080178));
#201190=CARTESIAN_POINT('Origin',(-6.67747469700966,-60.4944777170594,39.5248017080178));
#201191=CARTESIAN_POINT('Ctrl Pts',(-6.83973663030281,-62.0330459552232,
39.2875012672119));
#201192=CARTESIAN_POINT('Ctrl Pts',(-6.71274550335251,-62.0468640234019,
39.287208709576));
#201193=CARTESIAN_POINT('Ctrl Pts',(-6.70161199370846,-61.9391074687685,
39.3549016990123));
#201194=CARTESIAN_POINT('Ctrl Pts',(-6.82760205123578,-61.9187065474465,
39.1034939173931));
#201195=CARTESIAN_POINT('Ctrl Pts',(-6.70071032544293,-61.9323544653044,
39.1031692336329));
#201196=CARTESIAN_POINT('Ctrl Pts',(-6.69200045921796,-61.8476598279013,
39.2077507202296));
#201197=CARTESIAN_POINT('Ctrl Pts',(-6.80580199871494,-61.7133000470646,
38.989));
#201198=CARTESIAN_POINT('Ctrl Pts',(-6.67910652125822,-61.7268034525352,
38.9887769311176));
#201199=CARTESIAN_POINT('Ctrl Pts',(-6.67473372828961,-61.6833778591508,
39.1161898712916));
#201200=CARTESIAN_POINT('Ctrl Pts',(-6.78290064323581,-61.4975385923862,
38.989));
#201201=CARTESIAN_POINT('Ctrl Pts',(-6.65640766978554,-61.5108335396272,
38.989));
#201202=CARTESIAN_POINT('Ctrl Pts',(-6.65659650326273,-61.510813692429,
39.1161895903855));
#201203=CARTESIAN_POINT('Origin',(-6.8279329755337,-61.9259926140919,39.3548010137695));
#201204=CARTESIAN_POINT('Ctrl Pts',(-6.67747469700966,-60.4944777170594,
39.3978017080178));
#201205=CARTESIAN_POINT('Ctrl Pts',(-6.55117041629789,-60.5077528318944,
39.3978017080178));
#201206=CARTESIAN_POINT('Ctrl Pts',(-6.55117041629789,-60.5077528318944,
39.5248017080178));
#201207=CARTESIAN_POINT('Ctrl Pts',(-6.66829952659983,-60.404935774755,
39.3978017080178));
#201208=CARTESIAN_POINT('Ctrl Pts',(-6.54175270773085,-60.4181493202587,
39.397566602504));
#201209=CARTESIAN_POINT('Ctrl Pts',(-6.53705760237928,-60.373478376798,
39.5248015517196));
#201210=CARTESIAN_POINT('Ctrl Pts',(-6.65962554481717,-60.3202668847283,
39.3484894016716));
#201211=CARTESIAN_POINT('Ctrl Pts',(-6.53289275205199,-60.3338524728719,
39.3480259000033));
#201212=CARTESIAN_POINT('Ctrl Pts',(-6.52371293062554,-60.246512306211,
39.4508333188939));
#201213=CARTESIAN_POINT('Ctrl Pts',(-6.65505462397415,-60.2756459899119,
39.2708017080178));
#201214=CARTESIAN_POINT('Ctrl Pts',(-6.52822907310799,-60.2894805317161,
39.27051194648));
#201215=CARTESIAN_POINT('Ctrl Pts',(-6.51668018436767,-60.1796001951995,
39.3343017080178));
#201216=CARTESIAN_POINT('Origin',(-6.64298446507943,-60.1663250803645,39.3343017080178));
#201217=CARTESIAN_POINT('Origin',(-6.84655462836824,-62.1031658061144,39.6398955068187));
#201218=CARTESIAN_POINT('Origin',(-6.86517628122531,-62.2803389979219,39.92499));
#201219=CARTESIAN_POINT('Origin',(-6.63448104656953,-60.0854204576115,39.1934008539944));
#201220=CARTESIAN_POINT('Origin',(-6.62985850077867,-60.0409538388295,39.1160402713849));
#201221=CARTESIAN_POINT('Ctrl Pts',(-6.59568250079906,-62.6076796697354,
40.1599502534424));
#201222=CARTESIAN_POINT('Ctrl Pts',(-6.59177408464795,-62.5705801176609,
40.10025));
#201223=CARTESIAN_POINT('Ctrl Pts',(-6.58439859103049,-62.5005702980931,
40.10025));
#201224=CARTESIAN_POINT('Ctrl Pts',(-6.68331293653979,-62.5984477290802,
40.1599500538468));
#201225=CARTESIAN_POINT('Ctrl Pts',(-6.65560500345307,-62.5638523220933,
40.1002448353502));
#201226=CARTESIAN_POINT('Ctrl Pts',(-6.6351215427267,-62.4952175264275,
40.10025));
#201227=CARTESIAN_POINT('Ctrl Pts',(-6.76155265492271,-62.5650504549418,
40.1202442001039));
#201228=CARTESIAN_POINT('Ctrl Pts',(-6.71196843232426,-62.5346567608587,
40.0633873868018));
#201229=CARTESIAN_POINT('Ctrl Pts',(-6.6793077633958,-62.4653998062673,
40.0772271723538));
#201230=CARTESIAN_POINT('Ctrl Pts',(-6.86003002196301,-62.48163287707,40.0045995998162));
#201231=CARTESIAN_POINT('Ctrl Pts',(-6.76863258245072,-62.4676069047243,
39.9663485808315));
#201232=CARTESIAN_POINT('Ctrl Pts',(-6.73311104631486,-62.3866783619499,
40.0101727202465));
#201233=CARTESIAN_POINT('Ctrl Pts',(-6.88172985342185,-62.4326191774618,
39.930465434986));
#201234=CARTESIAN_POINT('Ctrl Pts',(-6.76853939445034,-62.4292062449171,
39.9051900162951));
#201235=CARTESIAN_POINT('Ctrl Pts',(-6.74362530798287,-62.3388388123831,
39.9671857458173));
#201236=CARTESIAN_POINT('Ctrl Pts',(-6.87697683366585,-62.3873926810691,
39.8576902534424));
#201237=CARTESIAN_POINT('Ctrl Pts',(-6.75017837817623,-62.4011871104968,
39.8573998014387));
#201238=CARTESIAN_POINT('Ctrl Pts',(-6.73887200051354,-62.2936141127569,
39.92499));
#201239=CARTESIAN_POINT('Origin',(-6.58439859103049,-62.5005702980931,40.22725));
#201240=CARTESIAN_POINT('Origin',(-0.315760701779421,0.0331877870874811,
39.116));
#201241=CARTESIAN_POINT('Origin',(-6.58785426247116,-59.6417962403142,39.116));
#201242=CARTESIAN_POINT('Origin',(-1.29720108988942E-17,1.63986310369608E-16,
40.22725));
#201243=CARTESIAN_POINT('Origin',(-6.55408556365967,-62.5037563256534,40.22725));
#201244=CARTESIAN_POINT('Ctrl Pts',(-6.58785426247116,-59.6417962403142,
38.989));
#201245=CARTESIAN_POINT('Ctrl Pts',(-6.46136077224317,-59.6550912418708,
38.989));
#201246=CARTESIAN_POINT('Ctrl Pts',(-6.46155012326944,-59.6550713402759,
39.1161901092324));
#201247=CARTESIAN_POINT('Ctrl Pts',(-6.56494565834866,-59.4260321009469,
38.989));
#201248=CARTESIAN_POINT('Ctrl Pts',(-6.43870097937981,-59.4394927947734,
38.989229898976));
#201249=CARTESIAN_POINT('Ctrl Pts',(-6.44341257746702,-59.4825041216658,
39.1161900493204));
#201250=CARTESIAN_POINT('Ctrl Pts',(-6.543134682019,-59.2206282517276,39.1034966344368));
#201251=CARTESIAN_POINT('Ctrl Pts',(-6.41712387096028,-59.234195551358,
39.1038314102552));
#201252=CARTESIAN_POINT('Ctrl Pts',(-6.42614597500986,-59.3182233753686,
39.2077528789594));
#201253=CARTESIAN_POINT('Ctrl Pts',(-6.53099325080075,-59.1062911958296,
39.2875012672119));
#201254=CARTESIAN_POINT('Ctrl Pts',(-6.40512262640556,-59.1200087130389,
39.2878045257868));
#201255=CARTESIAN_POINT('Ctrl Pts',(-6.41653455832048,-59.2267768553867,
39.3549015295901));
#201256=CARTESIAN_POINT('Origin',(-6.54282188406247,-59.2133417798936,39.3548010137695));
#201257=CARTESIAN_POINT('Ctrl Pts',(-6.2443699078808,-62.4538823482275,
39.8576902534424));
#201258=CARTESIAN_POINT('Ctrl Pts',(-6.37126553604092,-62.4410124550018,
39.8573998014387));
#201259=CARTESIAN_POINT('Ctrl Pts',(-6.35995915837823,-62.3334394572619,
39.92499));
#201260=CARTESIAN_POINT('Ctrl Pts',(-6.24912604340947,-62.4991292864732,
39.9304984902492));
#201261=CARTESIAN_POINT('Ctrl Pts',(-6.3591243783171,-62.4722545055304,
39.9052171569797));
#201262=CARTESIAN_POINT('Ctrl Pts',(-6.36471463173893,-62.378684763968,
39.9672049726599));
#201263=CARTESIAN_POINT('Ctrl Pts',(-6.28053011789757,-62.5423796567682,
40.004343767866));
#201264=CARTESIAN_POINT('Ctrl Pts',(-6.36708533499896,-62.5096946965644,
39.9661628577643));
#201265=CARTESIAN_POINT('Ctrl Pts',(-6.38493060453732,-62.4231124872028,
40.0100243556236));
#201266=CARTESIAN_POINT('Ctrl Pts',(-6.39322569848911,-62.6032845425346,
40.1194874821989));
#201267=CARTESIAN_POINT('Ctrl Pts',(-6.43576006824497,-62.5632890102013,
40.062755148314));
#201268=CARTESIAN_POINT('Ctrl Pts',(-6.45334792019214,-62.4886705126496,
40.0767884282376));
#201269=CARTESIAN_POINT('Ctrl Pts',(-6.47739243510511,-62.620090867565,
40.1599502015389));
#201270=CARTESIAN_POINT('Ctrl Pts',(-6.49734694408379,-62.5804859237136,
40.1002449453872));
#201271=CARTESIAN_POINT('Ctrl Pts',(-6.50319024212544,-62.5090840872032,
40.10025));
#201272=CARTESIAN_POINT('Ctrl Pts',(-6.56531752495323,-62.6108711573005,
40.1599502534424));
#201273=CARTESIAN_POINT('Ctrl Pts',(-6.56142710223373,-62.5737697140402,
40.10025));
#201274=CARTESIAN_POINT('Ctrl Pts',(-6.55408556365967,-62.5037563256534,
40.10025));
#201275=CARTESIAN_POINT('Origin',(-6.23365487766645,-62.3467145720969,39.92499));
#201276=CARTESIAN_POINT('Origin',(-6.52420020558083,-59.0361683443333,39.6398955069332));
#201277=CARTESIAN_POINT('Origin',(-6.50557852713774,-58.858994908613,39.92499));
#201278=CARTESIAN_POINT('Origin',(-6.21503322485401,-62.1695413802712,39.6398955068271));
#201279=CARTESIAN_POINT('Origin',(-6.19641157197484,-61.9923681882669,39.3548010137695));
#201280=CARTESIAN_POINT('Ctrl Pts',(-6.4937464611276,-58.7519447039088,
39.8576902534424));
#201281=CARTESIAN_POINT('Ctrl Pts',(-6.36806742857345,-58.765644274027,
39.8579948730703));
#201282=CARTESIAN_POINT('Ctrl Pts',(-6.37927424642597,-58.872270023448,
39.92499));
#201283=CARTESIAN_POINT('Ctrl Pts',(-6.48899657309077,-58.7067576262546,
39.9304020711232));
#201284=CARTESIAN_POINT('Ctrl Pts',(-6.3800422045293,-58.7342098038493,
39.905891529738));
#201285=CARTESIAN_POINT('Ctrl Pts',(-6.37452469054062,-58.827081017759,
39.9671523786028));
#201286=CARTESIAN_POINT('Ctrl Pts',(-6.45774144355347,-58.6637560248474,
40.0043257306692));
#201287=CARTESIAN_POINT('Ctrl Pts',(-6.37187117938172,-58.6967899354323,
39.9667894847838));
#201288=CARTESIAN_POINT('Ctrl Pts',(-6.35435266912786,-58.7829167175848,
40.01001389752));
#201289=CARTESIAN_POINT('Ctrl Pts',(-6.34539908016329,-58.603591415908,
40.1195533054858));
#201290=CARTESIAN_POINT('Ctrl Pts',(-6.30313135363842,-58.6436439608623,
40.0630813209233));
#201291=CARTESIAN_POINT('Ctrl Pts',(-6.28595874576534,-58.7181337176191,
40.076826594242));
#201292=CARTESIAN_POINT('Ctrl Pts',(-6.26151010025752,-58.587269867717,
40.1599502027514));
#201293=CARTESIAN_POINT('Ctrl Pts',(-6.24170554357568,-58.626864594668,
40.1002552791541));
#201294=CARTESIAN_POINT('Ctrl Pts',(-6.23613328458281,-58.6982323944353,
40.10025));
#201295=CARTESIAN_POINT('Ctrl Pts',(-6.1740349085904,-58.5964866834551,
40.1599502534424));
#201296=CARTESIAN_POINT('Ctrl Pts',(-6.17794390662191,-58.6335861742242,
40.10025));
#201297=CARTESIAN_POINT('Ctrl Pts',(-6.18532049829418,-58.7035958781039,
40.10025));
#201298=CARTESIAN_POINT('Origin',(-6.18532049829418,-58.7035958781039,40.22725));
#201299=CARTESIAN_POINT('Ctrl Pts',(-6.15137923967696,-61.5639141665612,
38.989));
#201300=CARTESIAN_POINT('Ctrl Pts',(-6.27787222402478,-61.5506192181748,
38.989));
#201301=CARTESIAN_POINT('Ctrl Pts',(-6.2776833796338,-61.5506390665201,
39.1161896013267));
#201302=CARTESIAN_POINT('Ctrl Pts',(-6.17383801205357,-61.7797255331386,
38.989));
#201303=CARTESIAN_POINT('Ctrl Pts',(-6.30057242039932,-61.7665923920114,
38.988776927546));
#201304=CARTESIAN_POINT('Ctrl Pts',(-6.29582088597906,-61.723205914552,
39.1161898821849));
#201305=CARTESIAN_POINT('Ctrl Pts',(-6.19522058691281,-61.985174271489,
39.1034967087243));
#201306=CARTESIAN_POINT('Ctrl Pts',(-6.32217699854699,-61.9721416759935,
39.1031720232709));
#201307=CARTESIAN_POINT('Ctrl Pts',(-6.31308747966708,-61.8874865820179,
39.2077529615));
#201308=CARTESIAN_POINT('Ctrl Pts',(-6.20712349654484,-62.0995362748658,
39.2875012672119));
#201309=CARTESIAN_POINT('Ctrl Pts',(-6.33421251157731,-62.0866494440659,
39.2872087095507));
#201310=CARTESIAN_POINT('Ctrl Pts',(-6.3226988678919,-61.9789328337398,
39.3549017048228));
#201311=CARTESIAN_POINT('Origin',(-6.15137923967696,-61.5639141665612,39.116));
#201312=CARTESIAN_POINT('Origin',(4.05837671390568E-16,-5.83359163402241E-17,
40.22725));
#201313=CARTESIAN_POINT('Origin',(-6.15500747092336,-58.7067819056643,40.22725));
#201314=CARTESIAN_POINT('Origin',(0.995615674755347,6.43520020182081,39.116));
#201315=CARTESIAN_POINT('Origin',(-6.1093749596203,-61.1647646440474,39.1160373285266));
#201316=CARTESIAN_POINT('Ctrl Pts',(-6.14377718965342,-58.5996668978648,
40.1599502534424));
#201317=CARTESIAN_POINT('Ctrl Pts',(-6.1476670304619,-58.6367684021392,
40.10025));
#201318=CARTESIAN_POINT('Ctrl Pts',(-6.15500747092336,-58.7067819056643,
40.10025));
#201319=CARTESIAN_POINT('Ctrl Pts',(-6.0565955360672,-58.6088074259633,
40.1599500566035));
#201320=CARTESIAN_POINT('Ctrl Pts',(-6.08415140319836,-58.6434243604401,
40.1002551305372));
#201321=CARTESIAN_POINT('Ctrl Pts',(-6.10436324506832,-58.712082152969,
40.10025));
#201322=CARTESIAN_POINT('Ctrl Pts',(-5.97852000021541,-58.641681736514,
40.1203070619045));
#201323=CARTESIAN_POINT('Ctrl Pts',(-6.02785839131288,-58.6721826510718,
40.0637098684497));
#201324=CARTESIAN_POINT('Ctrl Pts',(-6.06008468706716,-58.7414038195498,
40.0772636213363));
#201325=CARTESIAN_POINT('Ctrl Pts',(-5.88025093392488,-58.7242744516463,
40.0046102245802));
#201326=CARTESIAN_POINT('Ctrl Pts',(-5.97104363802162,-58.7387860695147,
39.9670001894015));
#201327=CARTESIAN_POINT('Ctrl Pts',(-6.00614981441038,-58.8193360415241,
40.0101788811209));
#201328=CARTESIAN_POINT('Ctrl Pts',(-5.85862682030279,-58.7730316211507,
39.9303710930186));
#201329=CARTESIAN_POINT('Ctrl Pts',(-5.97091547255937,-58.7772266151797,
39.9058663574098));
#201330=CARTESIAN_POINT('Ctrl Pts',(-5.99561386571446,-58.8669255556785,
39.9671344706363));
#201331=CARTESIAN_POINT('Ctrl Pts',(-5.863373641496,-58.8181995570485,39.8576902534424));
#201332=CARTESIAN_POINT('Ctrl Pts',(-5.98915458643814,-58.805469618532,
39.8579948730703));
#201333=CARTESIAN_POINT('Ctrl Pts',(-6.00036140429066,-58.912095367953,
39.92499));
#201334=CARTESIAN_POINT('Origin',(-5.87405712357889,-58.925370482788,39.92499));
#201335=CARTESIAN_POINT('Origin',(-6.10480350526348,-61.1207756545809,39.1925554488848));
#201336=CARTESIAN_POINT('Origin',(-6.09624906995259,-61.0393856393804,39.3343017080178));
#201337=CARTESIAN_POINT('Origin',(-5.89267880207433,-59.1025439184843,39.6398955069217));
#201338=CARTESIAN_POINT('Origin',(-5.91130048050362,-59.2797173540686,39.3548010137695));
#201339=CARTESIAN_POINT('Ctrl Pts',(-6.0617588454159,-60.7112330730304,
39.3978017080178));
#201340=CARTESIAN_POINT('Ctrl Pts',(-6.18806312612767,-60.6979579581954,
39.3978017080178));
#201341=CARTESIAN_POINT('Ctrl Pts',(-6.18806312612767,-60.6979579581954,
39.5248017080178));
#201342=CARTESIAN_POINT('Ctrl Pts',(-6.07140041118272,-60.8007259828525,
39.3978017080178));
#201343=CARTESIAN_POINT('Ctrl Pts',(-6.19746294737672,-60.787391283361,
39.3980355775196));
#201344=CARTESIAN_POINT('Ctrl Pts',(-6.20217593878193,-60.8322324012621,
39.5248015517192));
#201345=CARTESIAN_POINT('Ctrl Pts',(-6.08051542067571,-60.885348460727,
39.3484893995498));
#201346=CARTESIAN_POINT('Ctrl Pts',(-6.20639551966706,-60.8723790316504,
39.3489438303418));
#201347=CARTESIAN_POINT('Ctrl Pts',(-6.21552060714923,-60.9591984396293,
39.4508333155596));
#201348=CARTESIAN_POINT('Ctrl Pts',(-6.08531878138341,-60.929944884669,
39.2708017080178));
#201349=CARTESIAN_POINT('Ctrl Pts',(-6.21110821942955,-60.917217374751,
39.2710850691866));
#201350=CARTESIAN_POINT('Ctrl Pts',(-6.22255335066436,-61.0261105245454,
39.3343017080178));
#201351=CARTESIAN_POINT('Origin',(-6.0617588454159,-60.7112330730304,39.5248017080178));
#201352=CARTESIAN_POINT('Ctrl Pts',(-5.90061356181277,-59.1725467709677,
39.2875012672119));
#201353=CARTESIAN_POINT('Ctrl Pts',(-6.02658562874827,-59.1597945546412,
39.2878045257519));
#201354=CARTESIAN_POINT('Ctrl Pts',(-6.03762143316772,-59.2666022171587,
39.3549015218348));
#201355=CARTESIAN_POINT('Ctrl Pts',(-5.91250964036485,-59.2869113614505,
39.1034938540228));
#201356=CARTESIAN_POINT('Ctrl Pts',(-6.03858760028461,-59.2739830624742,
39.1038286278801));
#201357=CARTESIAN_POINT('Ctrl Pts',(-6.0472329950889,-59.3580501215732,
39.2077506434028));
#201358=CARTESIAN_POINT('Ctrl Pts',(-5.93388131656949,-59.4923630227874,
38.989));
#201359=CARTESIAN_POINT('Ctrl Pts',(-6.06016587018276,-59.47928181684,38.9892298954611));
#201360=CARTESIAN_POINT('Ctrl Pts',(-6.06449973388426,-59.5223321697742,
39.1161900347289));
#201361=CARTESIAN_POINT('Ctrl Pts',(-5.9563328589123,-59.7081718144892,
38.989));
#201362=CARTESIAN_POINT('Ctrl Pts',(-6.08282633453093,-59.6948768144682,
38.989));
#201363=CARTESIAN_POINT('Ctrl Pts',(-6.08263699813586,-59.6948967145252,
39.1161900945646));
#201364=CARTESIAN_POINT('Origin',(-5.9563328589123,-59.7081718144892,39.116));
#201365=CARTESIAN_POINT('Origin',(0.97914764405288,6.27851735587422,39.5248017080178));
#201366=CARTESIAN_POINT('Origin',(-6.04595329345081,-60.5608532912343,39.5248017080178));
#201367=CARTESIAN_POINT('Origin',(0.9765688230087,6.25398151259764,39.116));
#201368=CARTESIAN_POINT('Origin',(-5.99823604520128,-60.1073400339997,39.1160402713849));
#201369=CARTESIAN_POINT('Ctrl Pts',(-6.02238575970296,-60.3421421670675,
39.2708017080178));
#201370=CARTESIAN_POINT('Ctrl Pts',(-6.14931623097267,-60.3293058762211,
39.27051194648));
#201371=CARTESIAN_POINT('Ctrl Pts',(-6.13776734223235,-60.2194255397045,
39.3343017080178));
#201372=CARTESIAN_POINT('Ctrl Pts',(-6.02720817145255,-60.3868890390928,
39.3487519301185));
#201373=CARTESIAN_POINT('Ctrl Pts',(-6.1539956747704,-60.3738278099523,
39.3482879463979));
#201374=CARTESIAN_POINT('Ctrl Pts',(-6.14482385294844,-60.2865637544324,
39.4512271261634));
#201375=CARTESIAN_POINT('Ctrl Pts',(-6.03634362557914,-60.4716618705782,
39.3978017080178));
#201376=CARTESIAN_POINT('Ctrl Pts',(-6.16287156698238,-60.4582762833186,
39.3975673827397));
#201377=CARTESIAN_POINT('Ctrl Pts',(-6.15819229746499,-60.413756007749,
39.5248015355181));
#201378=CARTESIAN_POINT('Ctrl Pts',(-6.04595329345081,-60.5608532912343,
39.3978017080178));
#201379=CARTESIAN_POINT('Ctrl Pts',(-6.17225757416258,-60.5475781763993,
39.3978017080178));
#201380=CARTESIAN_POINT('Ctrl Pts',(-6.17225757416258,-60.5475781763993,
39.5248017080178));
#201381=CARTESIAN_POINT('Origin',(-6.01146306152058,-60.2327006545395,39.3343017080178));
#201382=CARTESIAN_POINT('Origin',(-6.00295964283318,-60.151796032919,39.1934008533548));
#201383=CARTESIAN_POINT('Origin',(-13.0813452322046,-60.0157999988656,39.1925554495083));
#201384=CARTESIAN_POINT('Origin',(-13.0905908661199,-60.0590486699125,39.116037328528));
#201385=CARTESIAN_POINT('Origin',(-13.0643300858384,-59.9357500275432,39.3343017080178));
#201386=CARTESIAN_POINT('Ctrl Pts',(-13.0409063549241,-59.8282880397054,
39.2708017080178));
#201387=CARTESIAN_POINT('Ctrl Pts',(-12.9173404733285,-59.8550545325309,
39.2710850691866));
#201388=CARTESIAN_POINT('Ctrl Pts',(-12.9401053405452,-59.9621548122771,
39.3343017080178));
#201389=CARTESIAN_POINT('Ctrl Pts',(-13.0316624367249,-59.7842416555146,
39.3487519293518));
#201390=CARTESIAN_POINT('Ctrl Pts',(-12.9079350417483,-59.8108054559364,
39.3492068662935));
#201391=CARTESIAN_POINT('Ctrl Pts',(-12.9260696369488,-59.8961220185296,
39.451227124874));
#201392=CARTESIAN_POINT('Ctrl Pts',(-13.0141504107554,-59.7007958241043,
39.3978017080178));
#201393=CARTESIAN_POINT('Ctrl Pts',(-12.8901364125064,-59.7270694888856,
39.3980347781174));
#201394=CARTESIAN_POINT('Ctrl Pts',(-12.8994792219297,-59.7710239514073,
39.524801535519));
#201395=CARTESIAN_POINT('Ctrl Pts',(-12.9957275188826,-59.6130003254554,
39.3978017080178));
#201396=CARTESIAN_POINT('Ctrl Pts',(-12.8715027735894,-59.6394051101893,
39.3978017080178));
#201397=CARTESIAN_POINT('Ctrl Pts',(-12.8715027735894,-59.6394051101893,
39.5248017080178));
#201398=CARTESIAN_POINT('Origin',(-12.9957275188826,-59.6130003254554,39.5248017080178));
#201399=CARTESIAN_POINT('Origin',(-0.310561863232978,0.0660119618346398,
39.116));
#201400=CARTESIAN_POINT('Origin',(-13.1739864076109,-60.4516424606488,39.116));
#201401=CARTESIAN_POINT('Origin',(-0.310561863232978,0.0660119618346398,
39.5248017080178));
#201402=CARTESIAN_POINT('Origin',(-12.9642895838873,-59.4650964698966,39.5248017080178));
#201403=CARTESIAN_POINT('Ctrl Pts',(-13.2864868028998,-60.9782752797347,
39.2875012672119));
#201404=CARTESIAN_POINT('Ctrl Pts',(-13.1616357280625,-61.0052918384389,
39.287208709576));
#201405=CARTESIAN_POINT('Ctrl Pts',(-13.1392995818862,-60.8992893541407,
39.3549016990122));
#201406=CARTESIAN_POINT('Ctrl Pts',(-13.2624669757412,-60.8658306440995,
39.1034939173931));
#201407=CARTESIAN_POINT('Ctrl Pts',(-13.1376969719812,-60.8926675943312,
39.1031692336336));
#201408=CARTESIAN_POINT('Ctrl Pts',(-13.1201818190176,-60.8093473519465,
39.2077507202299));
#201409=CARTESIAN_POINT('Ctrl Pts',(-13.2193155203585,-60.663828108008,
38.989));
#201410=CARTESIAN_POINT('Ctrl Pts',(-13.0947255842069,-60.6905008239737,
38.9887769311176));
#201411=CARTESIAN_POINT('Ctrl Pts',(-13.0858375353125,-60.6477702018626,
39.1161898712914));
#201412=CARTESIAN_POINT('Ctrl Pts',(-13.1739864076109,-60.4516424606489,
38.989));
#201413=CARTESIAN_POINT('Ctrl Pts',(-13.049576076309,-60.4780866929066,
38.989));
#201414=CARTESIAN_POINT('Ctrl Pts',(-13.0497618007392,-60.4780472159603,
39.1161895903853));
#201415=CARTESIAN_POINT('Origin',(-13.2635576885504,-60.8730422059013,39.3548010137695));
#201416=CARTESIAN_POINT('Ctrl Pts',(-12.9642895838873,-59.4650964698966,
39.3978017080178));
#201417=CARTESIAN_POINT('Ctrl Pts',(-12.8400648385941,-59.4915012546304,
39.3978017080178));
#201418=CARTESIAN_POINT('Ctrl Pts',(-12.8400648385941,-59.4915012546304,
39.5248017080178));
#201419=CARTESIAN_POINT('Ctrl Pts',(-12.9458049943937,-59.3770041141843,
39.3978017080178));
#201420=CARTESIAN_POINT('Ctrl Pts',(-12.8213326038448,-59.4033730190105,
39.3975666025045));
#201421=CARTESIAN_POINT('Ctrl Pts',(-12.8119938336989,-59.3594375597974,
39.5248015517196));
#201422=CARTESIAN_POINT('Ctrl Pts',(-12.9283282206293,-59.2937057271824,
39.3484894016716));
#201423=CARTESIAN_POINT('Ctrl Pts',(-12.8037097640135,-59.320464076127,
39.3480259000027));
#201424=CARTESIAN_POINT('Ctrl Pts',(-12.7854506972089,-59.2345619206666,
39.450833318893));
#201425=CARTESIAN_POINT('Ctrl Pts',(-12.9191181862048,-59.2498070616279,
39.2708017080178));
#201426=CARTESIAN_POINT('Ctrl Pts',(-12.794433502371,-59.2768226962998,
39.2705119464801));
#201427=CARTESIAN_POINT('Ctrl Pts',(-12.7714622569322,-59.168751483356,
39.3343017080178));
#201428=CARTESIAN_POINT('Origin',(-12.8956870022254,-59.1423466986221,39.3343017080178));
#201429=CARTESIAN_POINT('Origin',(-13.3005969715153,-61.0472983318868,39.6398955068182));
#201430=CARTESIAN_POINT('Origin',(-13.3376362544828,-61.2215544576539,39.92499));
#201431=CARTESIAN_POINT('Origin',(-12.8787733304449,-59.0627741291261,39.1934008539949));
#201432=CARTESIAN_POINT('Origin',(-12.8695280801149,-59.0190342907433,39.116040271385));
#201433=CARTESIAN_POINT('Ctrl Pts',(-13.103835206573,-61.5752716937451,
40.1599502534424));
#201434=CARTESIAN_POINT('Ctrl Pts',(-13.0960702419682,-61.5387839176327,
40.10025));
#201435=CARTESIAN_POINT('Ctrl Pts',(-13.0814171332235,-61.4699285681954,
40.10025));
#201436=CARTESIAN_POINT('Ctrl Pts',(-13.1900205930483,-61.556930451844,
40.1599500538479));
#201437=CARTESIAN_POINT('Ctrl Pts',(-13.15884824219,-61.5254208297837,40.100244835349));
#201438=CARTESIAN_POINT('Ctrl Pts',(-13.1313027022865,-61.4593031273792,
40.10025));
#201439=CARTESIAN_POINT('Ctrl Pts',(-13.2643407403244,-61.5155378539379,
40.1202442001038));
#201440=CARTESIAN_POINT('Ctrl Pts',(-13.2118511391498,-61.4904936222814,
40.0633873868017));
#201441=CARTESIAN_POINT('Ctrl Pts',(-13.1721300657491,-61.4250300340662,
40.0772271723538));
#201442=CARTESIAN_POINT('Ctrl Pts',(-13.3535591268198,-61.4222835584426,
40.0045995998163));
#201443=CARTESIAN_POINT('Ctrl Pts',(-13.2611962587091,-61.41788805574,39.9663485808314));
#201444=CARTESIAN_POINT('Ctrl Pts',(-13.2174099770541,-61.3411158595757,
40.0101727202465));
#201445=CARTESIAN_POINT('Ctrl Pts',(-13.3700167576322,-61.3712701109736,
39.9304654349859));
#201446=CARTESIAN_POINT('Ctrl Pts',(-13.2570896192442,-61.379707499563,
39.9051900162951));
#201447=CARTESIAN_POINT('Ctrl Pts',(-13.2228660458969,-61.2924393404518,
39.9671857458177));
#201448=CARTESIAN_POINT('Ctrl Pts',(-13.3605623192489,-61.3267881959112,
39.8576902534424));
#201449=CARTESIAN_POINT('Ctrl Pts',(-13.2359003894753,-61.3537611057082,
39.8573998014387));
#201450=CARTESIAN_POINT('Ctrl Pts',(-13.2134115091896,-61.2479592423877,
39.92499));
#201451=CARTESIAN_POINT('Origin',(-13.0814171332235,-61.4699285681954,40.22725));
#201452=CARTESIAN_POINT('Origin',(-0.310561863232978,0.0660119618346398,
39.116));
#201453=CARTESIAN_POINT('Origin',(-12.7860306150453,-58.6264539577983,39.116));
#201454=CARTESIAN_POINT('Origin',(4.07480739540194E-18,1.61286359594752E-16,
40.22725));
#201455=CARTESIAN_POINT('Origin',(-13.0516031943531,-61.4762657165315,40.22725));
#201456=CARTESIAN_POINT('Ctrl Pts',(-12.7860306150453,-58.6264539577983,
38.989));
#201457=CARTESIAN_POINT('Ctrl Pts',(-12.6616197754742,-58.652898298092,
38.989));
#201458=CARTESIAN_POINT('Ctrl Pts',(-12.6618060089323,-58.6528587129485,
39.1161901092321));
#201459=CARTESIAN_POINT('Ctrl Pts',(-12.740694012737,-58.4142663981467,
38.989));
#201460=CARTESIAN_POINT('Ctrl Pts',(-12.6165479409688,-58.4408495151692,
38.989229898976));
#201461=CARTESIAN_POINT('Ctrl Pts',(-12.6257296363315,-58.4831327254063,
39.1161900493201));
#201462=CARTESIAN_POINT('Ctrl Pts',(-12.6975319705099,-58.2122676405433,
39.1034966344368));
#201463=CARTESIAN_POINT('Ctrl Pts',(-12.5736296288407,-58.2389323335259,
39.1038314102563));
#201464=CARTESIAN_POINT('Ctrl Pts',(-12.5913856081751,-58.3215567776509,
39.2077528789598));
#201465=CARTESIAN_POINT('Ctrl Pts',(-12.6735055745743,-58.0998260601479,
39.2875012672119));
#201466=CARTESIAN_POINT('Ctrl Pts',(-12.5497583536237,-58.1266254943012,
39.2878045257868));
#201467=CARTESIAN_POINT('Ctrl Pts',(-12.5722680796266,-58.2316158778876,
39.3549015295899));
#201468=CARTESIAN_POINT('Origin',(-12.6964592423895,-58.2050537810541,39.3548010137695));
#201469=CARTESIAN_POINT('Ctrl Pts',(-12.7383709431253,-61.4590390555208,
39.8576902534424));
#201470=CARTESIAN_POINT('Ctrl Pts',(-12.8632261535957,-61.4329754599098,
39.8573998014387));
#201471=CARTESIAN_POINT('Ctrl Pts',(-12.84073727331,-61.3271735965893,39.92499));
#201472=CARTESIAN_POINT('Ctrl Pts',(-12.7478306169676,-61.5035409747668,
39.9304984902492));
#201473=CARTESIAN_POINT('Ctrl Pts',(-12.8544171899343,-61.4653154597763,
39.9052171569791));
#201474=CARTESIAN_POINT('Ctrl Pts',(-12.8501961180702,-61.3716739624489,
39.9672049726596));
#201475=CARTESIAN_POINT('Ctrl Pts',(-12.7835835513933,-61.5432717953612,
40.004343767866));
#201476=CARTESIAN_POINT('Ctrl Pts',(-12.8662481012968,-61.5017184029583,
39.9661628577643));
#201477=CARTESIAN_POINT('Ctrl Pts',(-12.8749453072906,-61.4137451613971,
40.0100243556236));
#201478=CARTESIAN_POINT('Ctrl Pts',(-12.9020280679172,-61.5920631419345,
40.1194874821989));
#201479=CARTESIAN_POINT('Ctrl Pts',(-12.9401487584128,-61.5478406570052,
40.0627551483141));
#201480=CARTESIAN_POINT('Ctrl Pts',(-12.9498405053863,-61.4717924962545,
40.0767884282376));
#201481=CARTESIAN_POINT('Ctrl Pts',(-12.9874904696724,-61.5999795805213,
40.1599502015392));
#201482=CARTESIAN_POINT('Ctrl Pts',(-13.0031958218444,-61.5585057825378,
40.1002449453869));
#201483=CARTESIAN_POINT('Ctrl Pts',(-13.0015435854427,-61.4868843017924,
40.10025));
#201484=CARTESIAN_POINT('Ctrl Pts',(-13.0739701745327,-61.5816197022697,
40.1599502534424));
#201485=CARTESIAN_POINT('Ctrl Pts',(-13.0662229071069,-61.5451281645058,
40.10025));
#201486=CARTESIAN_POINT('Ctrl Pts',(-13.0516031943531,-61.4762657165315,
40.10025));
#201487=CARTESIAN_POINT('Origin',(-12.7165125280168,-61.3535783813231,39.92499));
#201488=CARTESIAN_POINT('Origin',(-12.6594199084569,-58.0307974155441,39.6398955069311));
#201489=CARTESIAN_POINT('Origin',(-12.6223805745521,-57.8565410498766,39.92499));
#201490=CARTESIAN_POINT('Origin',(-12.6794732450936,-61.1793222555334,39.6398955068263));
#201491=CARTESIAN_POINT('Origin',(-12.6424339620844,-61.0050661295706,39.3548010137695));
#201492=CARTESIAN_POINT('Ctrl Pts',(-12.5994235324474,-57.751314065072,
39.8576902534424));
#201493=CARTESIAN_POINT('Ctrl Pts',(-12.4758649777955,-57.7780756236495,
39.8579948730703));
#201494=CARTESIAN_POINT('Ctrl Pts',(-12.4981558292589,-57.8829458346105,
39.92499));
#201495=CARTESIAN_POINT('Ctrl Pts',(-12.5899763290075,-57.7068710254543,
39.9304020711231));
#201496=CARTESIAN_POINT('Ctrl Pts',(-12.4844883578144,-57.7455616498582,
39.9058915297372));
#201497=CARTESIAN_POINT('Ctrl Pts',(-12.4887087546164,-57.8385008428006,
39.9671523786025));
#201498=CARTESIAN_POINT('Ctrl Pts',(-12.5543975270269,-57.6673720419787,
40.0043257306692));
#201499=CARTESIAN_POINT('Ctrl Pts',(-12.4724506530561,-57.7092008760993,
39.9667894847835));
#201500=CARTESIAN_POINT('Ctrl Pts',(-12.4640308112191,-57.7966870296829,
40.01001389752));
#201501=CARTESIAN_POINT('Ctrl Pts',(-12.4363816727424,-57.6192799956673,
40.1195533054858));
#201502=CARTESIAN_POINT('Ctrl Pts',(-12.3985321242201,-57.663531309089,
40.0630813209236));
#201503=CARTESIAN_POINT('Ctrl Pts',(-12.3892398894927,-57.7394080294759,
40.076826594242));
#201504=CARTESIAN_POINT('Ctrl Pts',(-12.3512461790954,-57.6118166447794,
40.1599502027519));
#201505=CARTESIAN_POINT('Ctrl Pts',(-12.3356888898088,-57.6532646075484,
40.1002552791541));
#201506=CARTESIAN_POINT('Ctrl Pts',(-12.3376071226707,-57.7248239067129,
40.10025));
#201507=CARTESIAN_POINT('Ctrl Pts',(-12.2652136052663,-57.6301266171957,
40.1599502534424));
#201508=CARTESIAN_POINT('Ctrl Pts',(-12.2729791421557,-57.6666142715155,
40.10025));
#201509=CARTESIAN_POINT('Ctrl Pts',(-12.2876333308473,-57.7354693911204,
40.10025));
#201510=CARTESIAN_POINT('Origin',(-12.2876333308473,-57.7354693911204,40.22725));
#201511=CARTESIAN_POINT('Ctrl Pts',(-12.5528626811449,-60.5836663843181,
38.989));
#201512=CARTESIAN_POINT('Ctrl Pts',(-12.6772730231648,-60.5572221497822,
38.989));
#201513=CARTESIAN_POINT('Ctrl Pts',(-12.6770872880007,-60.55726162901,39.1161896013262));
#201514=CARTESIAN_POINT('Ctrl Pts',(-12.5977568525207,-60.7959479326852,
38.989));
#201515=CARTESIAN_POINT('Ctrl Pts',(-12.722424209458,-60.7696393833347,
38.988776927546));
#201516=CARTESIAN_POINT('Ctrl Pts',(-12.7131635826247,-60.7269872521295,
39.1161898821844));
#201517=CARTESIAN_POINT('Ctrl Pts',(-12.6404975322974,-60.9980361136599,
39.1034967087243));
#201518=CARTESIAN_POINT('Ctrl Pts',(-12.765396186243,-60.9718043534724,
39.1031720232721));
#201519=CARTESIAN_POINT('Ctrl Pts',(-12.7475075938194,-60.8885631224,39.2077529615005));
#201520=CARTESIAN_POINT('Ctrl Pts',(-12.6642893210144,-61.1105274371641,
39.2875012672119));
#201521=CARTESIAN_POINT('Ctrl Pts',(-12.7893350885046,-61.0844267823322,
39.2872087095508));
#201522=CARTESIAN_POINT('Ctrl Pts',(-12.7666250660187,-60.9785037583493,
39.3549017048226));
#201523=CARTESIAN_POINT('Origin',(-12.5528626811449,-60.5836663843181,39.116));
#201524=CARTESIAN_POINT('Origin',(3.9977349588932E-16,-5.73754452974295E-17,
40.22725));
#201525=CARTESIAN_POINT('Origin',(-12.257819391977,-57.7418065394565,40.22725));
#201526=CARTESIAN_POINT('Origin',(3.00026883051142,12.5880644220972,39.116));
#201527=CARTESIAN_POINT('Origin',(-12.469366018727,-60.1910940874972,39.1160373285259));
#201528=CARTESIAN_POINT('Ctrl Pts',(-12.2354540642047,-57.6364522029206,
40.1599502534424));
#201529=CARTESIAN_POINT('Ctrl Pts',(-12.2432007592849,-57.6729438621906,
40.10025));
#201530=CARTESIAN_POINT('Ctrl Pts',(-12.257819391977,-57.7418065394565,
40.10025));
#201531=CARTESIAN_POINT('Ctrl Pts',(-12.1497054461945,-57.6546556225247,
40.1599500566029));
#201532=CARTESIAN_POINT('Ctrl Pts',(-12.1807288143664,-57.6862025493679,
40.1002551305372));
#201533=CARTESIAN_POINT('Ctrl Pts',(-12.2080066271961,-57.7523715145548,
40.10025));
#201534=CARTESIAN_POINT('Ctrl Pts',(-12.0754939174599,-57.6955109599434,
40.1203070619046));
#201535=CARTESIAN_POINT('Ctrl Pts',(-12.1277502414153,-57.720687521098,
40.0637098684499));
#201536=CARTESIAN_POINT('Ctrl Pts',(-12.1670355805164,-57.7861609236007,
40.0772636213363));
#201537=CARTESIAN_POINT('Ctrl Pts',(-11.9863964689866,-57.7879231380266,
40.0046102245801));
#201538=CARTESIAN_POINT('Ctrl Pts',(-12.0782086782661,-57.7928648378994,
39.9670001894012));
#201539=CARTESIAN_POINT('Ctrl Pts',(-12.1215423041375,-57.8693039540645,
40.0101788811209));
#201540=CARTESIAN_POINT('Ctrl Pts',(-11.9699873265229,-57.8386735460214,
39.9303710930186));
#201541=CARTESIAN_POINT('Ctrl Pts',(-12.0820993460742,-57.8311081991722,
39.9058663574113));
#201542=CARTESIAN_POINT('Ctrl Pts',(-12.1160385312532,-57.9177340744077,
39.9671344706371));
#201543=CARTESIAN_POINT('Ctrl Pts',(-11.9794294790614,-57.8830978693155,
39.8576902534424));
#201544=CARTESIAN_POINT('Ctrl Pts',(-12.1031907419159,-57.8572899778511,
39.8579948730703));
#201545=CARTESIAN_POINT('Ctrl Pts',(-12.1254815933794,-57.962160188812,
39.92499));
#201546=CARTESIAN_POINT('Origin',(-12.0012568480862,-57.9885649735459,39.92499));
#201547=CARTESIAN_POINT('Origin',(-12.4602215058057,-60.1478239214168,39.1925554488849));
#201548=CARTESIAN_POINT('Origin',(-12.4432063593724,-60.0677739512125,39.3343017080178));
#201549=CARTESIAN_POINT('Origin',(-12.038296182044,-58.1628213391889,39.639895506923));
#201550=CARTESIAN_POINT('Origin',(-12.0753355159235,-58.3370777047234,39.3548010137695));
#201551=CARTESIAN_POINT('Ctrl Pts',(-12.3746037924166,-59.7450242491247,
39.3978017080178));
#201552=CARTESIAN_POINT('Ctrl Pts',(-12.4988285377098,-59.7186194643909,
39.3978017080178));
#201553=CARTESIAN_POINT('Ctrl Pts',(-12.4988285377098,-59.7186194643909,
39.5248017080178));
#201554=CARTESIAN_POINT('Ctrl Pts',(-12.3935470970146,-59.8330190893699,
39.3978017080178));
#201555=CARTESIAN_POINT('Ctrl Pts',(-12.5175251938,-59.8065803155777,39.3980355775177));
#201556=CARTESIAN_POINT('Ctrl Pts',(-12.5268995400901,-59.8506831473923,
39.5248015517192));
#201557=CARTESIAN_POINT('Ctrl Pts',(-12.411457631102,-59.9162252185215,
39.3484893995498));
#201558=CARTESIAN_POINT('Ctrl Pts',(-12.5352924712471,-59.8901687840256,
39.3489438303418));
#201559=CARTESIAN_POINT('Ctrl Pts',(-12.5534426698444,-59.9755587548341,
39.4508333155588));
#201560=CARTESIAN_POINT('Ctrl Pts',(-12.4208962741589,-59.9600752506737,
39.2708017080178));
#201561=CARTESIAN_POINT('Ctrl Pts',(-12.5446662374489,-59.9342688867324,
39.2710850691866));
#201562=CARTESIAN_POINT('Ctrl Pts',(-12.5674311046656,-60.0413691664787,
39.3343017080178));
#201563=CARTESIAN_POINT('Origin',(-12.3746037924166,-59.7450242491247,39.5248017080178));
#201564=CARTESIAN_POINT('Ctrl Pts',(-12.0535047649324,-58.2316113004781,
39.2875012672119));
#201565=CARTESIAN_POINT('Ctrl Pts',(-12.1774537741287,-58.2057612755555,
39.2878045257518));
#201566=CARTESIAN_POINT('Ctrl Pts',(-12.199593564085,-58.3108302788453,
39.3549015218347));
#201567=CARTESIAN_POINT('Ctrl Pts',(-12.0772900304169,-58.344105910958,
39.1034938540228));
#201568=CARTESIAN_POINT('Ctrl Pts',(-12.2013259468593,-58.3180696991549,
39.1038286278806));
#201569=CARTESIAN_POINT('Ctrl Pts',(-12.2187113817821,-58.4007725402752,
39.2077506434031));
#201570=CARTESIAN_POINT('Ctrl Pts',(-12.1200201767776,-58.5461981381264,
38.989));
#201571=CARTESIAN_POINT('Ctrl Pts',(-12.2442455720364,-58.5199882620691,
38.9892298954611));
#201572=CARTESIAN_POINT('Ctrl Pts',(-12.2530556816161,-58.5623497685526,
39.1161900347289));
#201573=CARTESIAN_POINT('Ctrl Pts',(-12.1649068885794,-58.7584778814676,
38.989));
#201574=CARTESIAN_POINT('Ctrl Pts',(-12.289317713782,-58.732033544228,38.989));
#201575=CARTESIAN_POINT('Ctrl Pts',(-12.2891314947139,-58.7320731263128,
39.1161900945646));
#201576=CARTESIAN_POINT('Origin',(-12.1649068885794,-58.7584778814676,39.116));
#201577=CARTESIAN_POINT('Origin',(2.93511643966563,12.2815465224196,39.5248017080178));
#201578=CARTESIAN_POINT('Origin',(-12.3431658574213,-59.5971203935659,39.5248017080178));
#201579=CARTESIAN_POINT('Origin',(2.92491386234308,12.2335471699536,39.116));
#201580=CARTESIAN_POINT('Origin',(-12.2483049654005,-59.1510793400372,39.1160402713846));
#201581=CARTESIAN_POINT('Ctrl Pts',(-12.2968658913805,-59.382070869907,
39.2708017080178));
#201582=CARTESIAN_POINT('Ctrl Pts',(-12.4217592664914,-59.3560370505013,
39.27051194648));
#201583=CARTESIAN_POINT('Ctrl Pts',(-12.3987880210526,-59.2479658375576,
39.3343017080178));
#201584=CARTESIAN_POINT('Ctrl Pts',(-12.3063392072228,-59.426068534596,
39.3487519301186));
#201585=CARTESIAN_POINT('Ctrl Pts',(-12.4310668851217,-59.3998259533469,
39.3482879463995));
#201586=CARTESIAN_POINT('Ctrl Pts',(-12.4128237298761,-59.3139986558962,
39.4512271261633));
#201587=CARTESIAN_POINT('Ctrl Pts',(-12.3242857901775,-59.5094220566595,
39.3978017080178));
#201588=CARTESIAN_POINT('Ctrl Pts',(-12.4487214234138,-59.4828840257757,
39.3975673827392));
#201589=CARTESIAN_POINT('Ctrl Pts',(-12.4394141514347,-59.4390967537845,
39.5248015355194));
#201590=CARTESIAN_POINT('Ctrl Pts',(-12.3431658574213,-59.5971203935659,
39.3978017080178));
#201591=CARTESIAN_POINT('Ctrl Pts',(-12.4673906027145,-59.570715608832,
39.3978017080178));
#201592=CARTESIAN_POINT('Ctrl Pts',(-12.4673906027145,-59.570715608832,
39.5248017080178));
#201593=CARTESIAN_POINT('Origin',(-12.2745632757594,-59.2743706222914,39.3343017080178));
#201594=CARTESIAN_POINT('Origin',(-12.2576496039189,-59.1947980539411,39.193400853355));
#201595=CARTESIAN_POINT('Origin',(-19.2830435999589,-58.3196542523186,39.192555449508));
#201596=CARTESIAN_POINT('Origin',(-19.296759302446,-58.3616995707147,39.1160373285266));
#201597=CARTESIAN_POINT('Origin',(-19.2577541638581,-58.2418213702173,39.3343017080178));
#201598=CARTESIAN_POINT('Ctrl Pts',(-19.2232259141442,-58.1373965169892,
39.2708017080178));
#201599=CARTESIAN_POINT('Ctrl Pts',(-19.103134799739,-58.1769325318819,
39.2710850691866));
#201600=CARTESIAN_POINT('Ctrl Pts',(-19.1369699862886,-58.2810665285029,
39.3343017080178));
#201601=CARTESIAN_POINT('Ctrl Pts',(-19.2094285342437,-58.0945576760637,
39.3487519293518));
#201602=CARTESIAN_POINT('Ctrl Pts',(-19.0891556041211,-58.1339089916654,
39.3492068662929));
#201603=CARTESIAN_POINT('Ctrl Pts',(-19.1161088652898,-58.2168625998377,
39.4512271248744));
#201604=CARTESIAN_POINT('Ctrl Pts',(-19.1832899764611,-58.0133994748124,
39.3978017080178));
#201605=CARTESIAN_POINT('Ctrl Pts',(-19.0627016856737,-58.0524922023716,
39.3980347781174));
#201606=CARTESIAN_POINT('Ctrl Pts',(-19.0765878066316,-58.0952292882338,
39.524801535519));
#201607=CARTESIAN_POINT('Ctrl Pts',(-19.1557908785627,-57.9280106456675,
39.3978017080178));
#201608=CARTESIAN_POINT('Ctrl Pts',(-19.0350067009933,-57.9672558039531,
39.3978017080178));
#201609=CARTESIAN_POINT('Ctrl Pts',(-19.0350067009933,-57.9672558039531,
39.5248017080178));
#201610=CARTESIAN_POINT('Origin',(-19.1557908785627,-57.9280106456675,39.5248017080178));
#201611=CARTESIAN_POINT('Origin',(-0.301960443923705,0.0981128957140471,
39.116));
#201612=CARTESIAN_POINT('Origin',(-19.4207352200703,-58.7434254837931,39.116));
#201613=CARTESIAN_POINT('Origin',(-0.301960443923705,0.0981128957140471,
39.5248017080178));
#201614=CARTESIAN_POINT('Origin',(-19.1090650011318,-57.7842031819382,39.5248017080178));
#201615=CARTESIAN_POINT('Ctrl Pts',(-19.5876674457081,-59.255413859757,
39.2875012672119));
#201616=CARTESIAN_POINT('Ctrl Pts',(-19.4663243174858,-59.295332909916,
39.287208709576));
#201617=CARTESIAN_POINT('Ctrl Pts',(-19.4330302542694,-59.1922458813525,
39.3549016990124));
#201618=CARTESIAN_POINT('Ctrl Pts',(-19.5520255367085,-59.1460959632225,
39.1034939173931));
#201619=CARTESIAN_POINT('Ctrl Pts',(-19.4307442612488,-59.1858279145903,
39.1031692336344));
#201620=CARTESIAN_POINT('Ctrl Pts',(-19.4046157212345,-59.104794941234,
39.2077507202309));
#201621=CARTESIAN_POINT('Ctrl Pts',(-19.4879954548414,-58.9497105734779,
38.989));
#201622=CARTESIAN_POINT('Ctrl Pts',(-19.3668760934073,-58.9892603680778,
38.9887769311158));
#201623=CARTESIAN_POINT('Ctrl Pts',(-19.35357016791,-58.9476928828771,39.1161898712901));
#201624=CARTESIAN_POINT('Ctrl Pts',(-19.4207352200704,-58.7434254837931,
38.989));
#201625=CARTESIAN_POINT('Ctrl Pts',(-19.2997705965402,-58.7827292725255,
38.989));
#201626=CARTESIAN_POINT('Ctrl Pts',(-19.2999511770886,-58.7826705983486,
39.1161895903858));
#201627=CARTESIAN_POINT('Origin',(-19.5538640879535,-59.1531540087998,39.3548010137695));
#201628=CARTESIAN_POINT('Ctrl Pts',(-19.1090650011318,-57.7842031819382,
39.3978017080178));
#201629=CARTESIAN_POINT('Ctrl Pts',(-18.9882808235623,-57.8234483402238,
39.3978017080178));
#201630=CARTESIAN_POINT('Ctrl Pts',(-18.9882808235623,-57.8234483402238,
39.5248017080178));
#201631=CARTESIAN_POINT('Ctrl Pts',(-19.081473513585,-57.6985255711017,
39.3978017080178));
#201632=CARTESIAN_POINT('Ctrl Pts',(-18.9604392969164,-57.7377609320145,
39.397566602504));
#201633=CARTESIAN_POINT('Ctrl Pts',(-18.9465591794958,-57.6950423231364,
39.5248015517196));
#201634=CARTESIAN_POINT('Ctrl Pts',(-19.0553854270307,-57.6175103216838,
39.3484894016716));
#201635=CARTESIAN_POINT('Ctrl Pts',(-18.934246652452,-57.657148261354,39.3480259000042));
#201636=CARTESIAN_POINT('Ctrl Pts',(-18.9071083904244,-57.5736252790828,
39.4508333188942));
#201637=CARTESIAN_POINT('Ctrl Pts',(-19.041637186088,-57.5748148483575,
39.2708017080178));
#201638=CARTESIAN_POINT('Ctrl Pts',(-18.9204594407748,-57.6147155869501,
39.27051194648));
#201639=CARTESIAN_POINT('Ctrl Pts',(-18.8863175164095,-57.5096375484036,
39.3343017080178));
#201640=CARTESIAN_POINT('Origin',(-19.007101693979,-57.470392390118,39.3343017080178));
#201641=CARTESIAN_POINT('Origin',(-19.6089151909176,-59.3225838821614,39.6398955068202));
#201642=CARTESIAN_POINT('Origin',(-19.6639662938564,-59.4920137553138,39.92499));
#201643=CARTESIAN_POINT('Origin',(-18.9819630786536,-57.3930236876028,39.1934008539951));
#201644=CARTESIAN_POINT('Origin',(-18.9681964166836,-57.3504898524408,39.1160402713851));
#201645=CARTESIAN_POINT('Ctrl Pts',(-19.4684195516699,-59.8682321556241,
40.1599502534424));
#201646=CARTESIAN_POINT('Ctrl Pts',(-19.4568831131887,-59.8327559231845,
40.10025));
#201647=CARTESIAN_POINT('Ctrl Pts',(-19.4351129318423,-59.765809437495,
40.10025));
#201648=CARTESIAN_POINT('Ctrl Pts',(-19.5522156237499,-59.8409825629603,
40.1599500538469));
#201649=CARTESIAN_POINT('Ctrl Pts',(-19.5179203859188,-59.8129039518375,
40.100244835349));
#201650=CARTESIAN_POINT('Ctrl Pts',(-19.4836145615377,-59.7500277420804,
40.10025));
#201651=CARTESIAN_POINT('Ctrl Pts',(-19.6218019328333,-59.7920481472525,
40.1202442001039));
#201652=CARTESIAN_POINT('Ctrl Pts',(-19.5669820401374,-59.7726277678654,
40.0633873868017));
#201653=CARTESIAN_POINT('Ctrl Pts',(-19.5206357546566,-59.7116747787981,
40.0772271723538));
#201654=CARTESIAN_POINT('Ctrl Pts',(-19.7007838434712,-59.6899788477096,
40.0045995998162));
#201655=CARTESIAN_POINT('Ctrl Pts',(-19.6084674936732,-59.6952619726976,
39.9663485808314));
#201656=CARTESIAN_POINT('Ctrl Pts',(-19.556896198164,-59.6234872553901,
40.0101727202466));
#201657=CARTESIAN_POINT('Ctrl Pts',(-19.7118189603903,-59.6375245663857,
39.930465434986));
#201658=CARTESIAN_POINT('Ctrl Pts',(-19.6003923959451,-59.6577198343135,
39.9051900162954));
#201659=CARTESIAN_POINT('Ctrl Pts',(-19.5572342963491,-59.5745070768384,
39.9671857458186));
#201660=CARTESIAN_POINT('Ctrl Pts',(-19.6977666881848,-59.5942745858235,
39.8576902534424));
#201661=CARTESIAN_POINT('Ctrl Pts',(-19.5766071063171,-59.6341304551456,
39.8573998014387));
#201662=CARTESIAN_POINT('Ctrl Pts',(-19.5431821162869,-59.5312589135995,
39.92499));
#201663=CARTESIAN_POINT('Origin',(-19.4351129318423,-59.765809437495,40.22725));
#201664=CARTESIAN_POINT('Origin',(-0.301960443923705,0.0981128957140471,
39.116));
#201665=CARTESIAN_POINT('Origin',(-18.8441205405522,-56.9687879773465,39.116));
#201666=CARTESIAN_POINT('Origin',(2.07460197300515E-17,1.56819321712835E-16,
40.22725));
#201667=CARTESIAN_POINT('Origin',(-19.4061247292256,-59.7752282754836,40.22725));
#201668=CARTESIAN_POINT('Ctrl Pts',(-18.8441205405522,-56.9687879773465,
38.989));
#201669=CARTESIAN_POINT('Ctrl Pts',(-18.7231554228301,-57.0080919266516,
38.989));
#201670=CARTESIAN_POINT('Ctrl Pts',(-18.7233364983081,-57.0080330916622,
39.1161901092326));
#201671=CARTESIAN_POINT('Ctrl Pts',(-18.7768526573593,-56.7625017687175,
38.989));
#201672=CARTESIAN_POINT('Ctrl Pts',(-18.6561653631324,-56.8019160587458,
38.9892298989742));
#201673=CARTESIAN_POINT('Ctrl Pts',(-18.6697165591974,-56.8430078886289,
39.1161900493188));
#201674=CARTESIAN_POINT('Ctrl Pts',(-18.7128124416024,-56.5661212433889,
39.1034966344368));
#201675=CARTESIAN_POINT('Ctrl Pts',(-18.5923760693053,-56.6055911857644,
39.1038314102579));
#201676=CARTESIAN_POINT('Ctrl Pts',(-18.6186713856995,-56.6859069993025,
39.2077528789608));
#201677=CARTESIAN_POINT('Ctrl Pts',(-18.6771643191712,-56.456807071981,
39.2875012672119));
#201678=CARTESIAN_POINT('Ctrl Pts',(-18.5568963021129,-56.4963948028697,
39.2878045257868));
#201679=CARTESIAN_POINT('Ctrl Pts',(-18.5902572009364,-56.5984571310821,
39.3549015295901));
#201680=CARTESIAN_POINT('Origin',(-18.7109915363519,-56.5590590327989,39.3548010137695));
#201681=CARTESIAN_POINT('Ctrl Pts',(-19.0928077206414,-59.7908376697911,
39.8576902534424));
#201682=CARTESIAN_POINT('Ctrl Pts',(-19.2142545736086,-59.7518659300025,
39.8573998014387));
#201683=CARTESIAN_POINT('Ctrl Pts',(-19.1808295835784,-59.6489943884563,
39.92499));
#201684=CARTESIAN_POINT('Ctrl Pts',(-19.1068672906322,-59.8341069976972,
39.9304984902492));
#201685=CARTESIAN_POINT('Ctrl Pts',(-19.2088743168615,-59.7849495553993,
39.9052171569797));
#201686=CARTESIAN_POINT('Ctrl Pts',(-19.1948881666553,-59.6922622581479,
39.9672049726605));
#201687=CARTESIAN_POINT('Ctrl Pts',(-19.1465773683627,-59.8698829694067,
40.004343767866));
#201688=CARTESIAN_POINT('Ctrl Pts',(-19.2244455609613,-59.8199164124675,
39.9661628577643));
#201689=CARTESIAN_POINT('Ctrl Pts',(-19.2238994150014,-59.7315159919507,
40.0100243556234));
#201690=CARTESIAN_POINT('Ctrl Pts',(-19.2694731179107,-59.9060262085835,
40.1194874821989));
#201691=CARTESIAN_POINT('Ctrl Pts',(-19.3027624708833,-59.8580612818569,
40.062755148314));
#201692=CARTESIAN_POINT('Ctrl Pts',(-19.3044519280755,-59.7814166574708,
40.0767884282379));
#201693=CARTESIAN_POINT('Ctrl Pts',(-19.3552948408465,-59.9049660265689,
40.1599502015391));
#201694=CARTESIAN_POINT('Ctrl Pts',(-19.3665789650869,-59.8620777700625,
40.1002449453872));
#201695=CARTESIAN_POINT('Ctrl Pts',(-19.3574492964901,-59.7910213450151,
40.10025));
#201696=CARTESIAN_POINT('Ctrl Pts',(-19.4393816709759,-59.8776671349984,
40.1599502534424));
#201697=CARTESIAN_POINT('Ctrl Pts',(-19.4278624395269,-59.8421853116552,
40.10025));
#201698=CARTESIAN_POINT('Ctrl Pts',(-19.4061247292256,-59.7752282754836,
40.10025));
#201699=CARTESIAN_POINT('Origin',(-19.0600454060089,-59.6882395467419,39.92499));
#201700=CARTESIAN_POINT('Origin',(-18.6559403576665,-56.3896289265494,39.6398955069321));
#201701=CARTESIAN_POINT('Origin',(-18.6008891789888,-56.2201988201382,39.92499));
#201702=CARTESIAN_POINT('Origin',(-19.0049943031084,-59.518809673565,39.6398955068274));
#201703=CARTESIAN_POINT('Origin',(-18.949943200106,-59.3493798002279,39.3548010137695));
#201704=CARTESIAN_POINT('Ctrl Pts',(-18.5670586829468,-56.1179479440987,
39.8576902534424));
#201705=CARTESIAN_POINT('Ctrl Pts',(-18.4469743395782,-56.1574782858996,
39.8579948730703));
#201706=CARTESIAN_POINT('Ctrl Pts',(-18.4801050014193,-56.2594439784238,
39.92499));
#201707=CARTESIAN_POINT('Ctrl Pts',(-18.5530176696414,-56.0747358697601,
39.9304020711232));
#201708=CARTESIAN_POINT('Ctrl Pts',(-18.4521518441042,-56.1242410383992,
39.9058915297385));
#201709=CARTESIAN_POINT('Ctrl Pts',(-18.4660639121464,-56.2162299491246,
39.9671523786031));
#201710=CARTESIAN_POINT('Ctrl Pts',(-18.5135050040175,-56.0391722633447,
40.0043257306692));
#201711=CARTESIAN_POINT('Ctrl Pts',(-18.4363793473476,-56.0893377355411,
39.9667894847836));
#201712=CARTESIAN_POINT('Ctrl Pts',(-18.4371504234766,-56.1772247439496,
40.0100138975199));
#201713=CARTESIAN_POINT('Ctrl Pts',(-18.3911086652349,-56.0036796861844,
40.1195533054859));
#201714=CARTESIAN_POINT('Ctrl Pts',(-18.3580919822891,-56.0516449414235,
40.0630813209237));
#201715=CARTESIAN_POINT('Ctrl Pts',(-18.3567819283755,-56.1280773042135,
40.0768265942422));
#201716=CARTESIAN_POINT('Ctrl Pts',(-18.3056594201306,-56.005156302634,
40.1599502027521));
#201717=CARTESIAN_POINT('Ctrl Pts',(-18.2945198471561,-56.0480033886671,
40.1002552791554));
#201718=CARTESIAN_POINT('Ctrl Pts',(-18.3039075553119,-56.1189701685697,
40.10025));
#201719=CARTESIAN_POINT('Ctrl Pts',(-18.2220120550219,-56.032358823839,
40.1599502534424));
#201720=CARTESIAN_POINT('Ctrl Pts',(-18.233549049922,-56.0678348753331,
40.10025));
#201721=CARTESIAN_POINT('Ctrl Pts',(-18.2553202812751,-56.1347810195641,
40.10025));
#201722=CARTESIAN_POINT('Origin',(-18.2553202812751,-56.1347810195641,40.22725));
#201723=CARTESIAN_POINT('Ctrl Pts',(-18.8168143322229,-58.9396512752212,
38.989));
#201724=CARTESIAN_POINT('Ctrl Pts',(-18.9377789661743,-58.9003474831028,
38.989));
#201725=CARTESIAN_POINT('Ctrl Pts',(-18.9375983751891,-58.9004061606709,
39.116189601327));
#201726=CARTESIAN_POINT('Ctrl Pts',(-18.8836520326609,-59.1460772043116,
38.989));
#201727=CARTESIAN_POINT('Ctrl Pts',(-19.0048864565382,-59.1068814887035,
38.988776927543));
#201728=CARTESIAN_POINT('Ctrl Pts',(-18.9912181986571,-59.0654310094269,
39.1161898821828));
#201729=CARTESIAN_POINT('Ctrl Pts',(-18.947282541524,-59.3425907075099,
39.1034967087243));
#201730=CARTESIAN_POINT('Ctrl Pts',(-19.0687550219947,-59.3034471832924,
39.1031720232731));
#201731=CARTESIAN_POINT('Ctrl Pts',(-19.0422633471882,-59.2225318234696,
39.2077529615015));
#201732=CARTESIAN_POINT('Ctrl Pts',(-18.9827025415099,-59.4519788726607,
39.2875012672119));
#201733=CARTESIAN_POINT('Ctrl Pts',(-19.1043350338629,-59.4129503580328,
39.2872087095508));
#201734=CARTESIAN_POINT('Ctrl Pts',(-19.070677448334,-59.3099814352091,
39.354901704823));
#201735=CARTESIAN_POINT('Origin',(-18.8168143322229,-58.9396512752212,39.116));
#201736=CARTESIAN_POINT('Origin',(3.93842937138093E-16,-5.57863568693716E-17,
40.22725));
#201737=CARTESIAN_POINT('Origin',(-18.2263320786585,-56.1441998575527,40.22725));
#201738=CARTESIAN_POINT('Origin',(6.24367625034032,18.1886080242681,39.116));
#201739=CARTESIAN_POINT('Origin',(-18.6927400943499,-58.5579573083284,39.116037328526));
#201740=CARTESIAN_POINT('Ctrl Pts',(-18.1930767435952,-56.0417604764382,
40.1599502534424));
#201741=CARTESIAN_POINT('Ctrl Pts',(-18.2045954185348,-56.0772424804484,
40.10025));
#201742=CARTESIAN_POINT('Ctrl Pts',(-18.2263320786585,-56.1441998575527,
40.10025));
#201743=CARTESIAN_POINT('Ctrl Pts',(-18.1097006409636,-56.0688273470723,
40.159950056604));
#201744=CARTESIAN_POINT('Ctrl Pts',(-18.1438516116611,-56.0969586315449,
40.1002551305372));
#201745=CARTESIAN_POINT('Ctrl Pts',(-18.1778965340257,-56.1599138083632,
40.10025));
#201746=CARTESIAN_POINT('Ctrl Pts',(-18.0401661963854,-56.117216091734,
40.1203070619045));
#201747=CARTESIAN_POINT('Ctrl Pts',(-18.0947679219784,-56.1367924598139,
40.0637098684499));
#201748=CARTESIAN_POINT('Ctrl Pts',(-18.1406818860299,-56.1978007560415,
40.0772636213363));
#201749=CARTESIAN_POINT('Ctrl Pts',(-17.9612165360192,-56.2184352456063,
40.0046102245803));
#201750=CARTESIAN_POINT('Ctrl Pts',(-18.0530423367033,-56.2137528851841,
39.9670001894012));
#201751=CARTESIAN_POINT('Ctrl Pts',(-18.1041286397845,-56.2852436625531,
40.0101788811209));
#201752=CARTESIAN_POINT('Ctrl Pts',(-17.9502021467135,-56.2706228600011,
39.9303710930185));
#201753=CARTESIAN_POINT('Ctrl Pts',(-18.0609092108089,-56.2513800597974,
39.9058663574109));
#201754=CARTESIAN_POINT('Ctrl Pts',(-18.1037173431994,-56.3339837785518,
39.9671344706364));
#201755=CARTESIAN_POINT('Ctrl Pts',(-17.9642361803975,-56.3138168485094,
39.8576902534424));
#201756=CARTESIAN_POINT('Ctrl Pts',(-18.0846218068697,-56.2752137607565,
39.8579948730704));
#201757=CARTESIAN_POINT('Ctrl Pts',(-18.1177524687109,-56.3771794532806,
39.92499));
#201758=CARTESIAN_POINT('Origin',(-17.9969682911414,-56.4164246115663,39.92499));
#201759=CARTESIAN_POINT('Origin',(-18.6791227120623,-58.5158800426268,39.1925554488843));
#201760=CARTESIAN_POINT('Origin',(-18.6538332760107,-58.4380471616454,39.3343017080178));
#201761=CARTESIAN_POINT('Origin',(-18.0520194698702,-56.585854717942,39.6398955069209));
#201762=CARTESIAN_POINT('Origin',(-18.1070706485045,-56.755284824227,39.3548010137695));
#201763=CARTESIAN_POINT('Ctrl Pts',(-18.5518699907153,-58.1242364370956,
39.3978017080178));
#201764=CARTESIAN_POINT('Ctrl Pts',(-18.6726541682848,-58.08499127881,39.3978017080178));
#201765=CARTESIAN_POINT('Ctrl Pts',(-18.6726541682848,-58.08499127881,39.5248017080178));
#201766=CARTESIAN_POINT('Ctrl Pts',(-18.5799074873334,-58.2097691178805,
39.3978017080178));
#201767=CARTESIAN_POINT('Ctrl Pts',(-18.7004428147371,-58.1705159385216,
39.3980355775177));
#201768=CARTESIAN_POINT('Ctrl Pts',(-18.7143758086142,-58.2133972843956,
39.5248015517192));
#201769=CARTESIAN_POINT('Ctrl Pts',(-18.6064173144578,-58.2906472745454,
39.3484893995498));
#201770=CARTESIAN_POINT('Ctrl Pts',(-18.7268501353366,-58.2517893143844,
39.3489438303419));
#201771=CARTESIAN_POINT('Ctrl Pts',(-18.7538265876727,-58.3348142976328,
39.4508333155592));
#201772=CARTESIAN_POINT('Ctrl Pts',(-18.620387828115,-58.3332704847795,
39.2708017080178));
#201773=CARTESIAN_POINT('Ctrl Pts',(-18.7407822670305,-58.2946680067387,
39.2710850691866));
#201774=CARTESIAN_POINT('Ctrl Pts',(-18.7746174535802,-58.3988020033598,
39.3343017080178));
#201775=CARTESIAN_POINT('Origin',(-18.5518699907153,-58.1242364370956,39.5248017080178));
#201776=CARTESIAN_POINT('Ctrl Pts',(-18.0743352474894,-56.6526781108323,
39.2875012672119));
#201777=CARTESIAN_POINT('Ctrl Pts',(-18.1949031876641,-56.614013495596,
39.2878045257519));
#201778=CARTESIAN_POINT('Ctrl Pts',(-18.2279043949852,-56.7161926816715,
39.354901521835));
#201779=CARTESIAN_POINT('Ctrl Pts',(-18.109749103561,-56.7620702268158,
39.1034938540228));
#201780=CARTESIAN_POINT('Ctrl Pts',(-18.2303840130662,-56.7232113603657,
39.103828627881));
#201781=CARTESIAN_POINT('Ctrl Pts',(-18.256319009646,-56.8036438738754,
39.2077506434042));
#201782=CARTESIAN_POINT('Ctrl Pts',(-18.1733695596538,-56.9585888550841,
38.989));
#201783=CARTESIAN_POINT('Ctrl Pts',(-18.2941747571346,-56.9195374698071,
38.9892298954593));
#201784=CARTESIAN_POINT('Ctrl Pts',(-18.307364587184,-56.9607460083102,
39.1161900347276));
#201785=CARTESIAN_POINT('Ctrl Pts',(-18.2401996527048,-57.1650137687746,
38.989));
#201786=CARTESIAN_POINT('Ctrl Pts',(-18.3611647564562,-57.1257098240089,
38.989));
#201787=CARTESIAN_POINT('Ctrl Pts',(-18.3609836949697,-57.1257686544521,
39.116190094565));
#201788=CARTESIAN_POINT('Origin',(-18.2401996527048,-57.1650137687746,39.116));
#201789=CARTESIAN_POINT('Origin',(6.09975091006211,17.7456513739114,39.5248017080178));
#201790=CARTESIAN_POINT('Origin',(-18.5051441132844,-57.9804289733663,39.5248017080178));
#201791=CARTESIAN_POINT('Origin',(6.07721283595922,17.6762863142854,39.116));
#201792=CARTESIAN_POINT('Origin',(-18.3641788932757,-57.5467470426659,39.1160402713847));
#201793=CARTESIAN_POINT('Ctrl Pts',(-18.4366189870675,-57.7713971777986,
39.2708017080178));
#201794=CARTESIAN_POINT('Ctrl Pts',(-18.5581069080663,-57.732451061807,
39.2705119464801));
#201795=CARTESIAN_POINT('Ctrl Pts',(-18.523964983701,-57.6273730232604,
39.3343017080178));
#201796=CARTESIAN_POINT('Ctrl Pts',(-18.4506394153724,-57.8141635875296,
39.3487519301186));
#201797=CARTESIAN_POINT('Ctrl Pts',(-18.5719407253097,-57.7750271733953,
39.348287946398));
#201798=CARTESIAN_POINT('Ctrl Pts',(-18.5448261124702,-57.6915769758401,
39.4512271261624));
#201799=CARTESIAN_POINT('Ctrl Pts',(-18.4772005006362,-57.895184561541,
39.3978017080178));
#201800=CARTESIAN_POINT('Ctrl Pts',(-18.5981804828667,-57.8557848432447,
39.3975673827392));
#201801=CARTESIAN_POINT('Ctrl Pts',(-18.5843471808454,-57.8132103173501,
39.5248015355194));
#201802=CARTESIAN_POINT('Ctrl Pts',(-18.5051441132844,-57.9804289733663,
39.3978017080178));
#201803=CARTESIAN_POINT('Ctrl Pts',(-18.6259282908539,-57.9411838150807,
39.3978017080178));
#201804=CARTESIAN_POINT('Ctrl Pts',(-18.6259282908539,-57.9411838150807,
39.5248017080178));
#201805=CARTESIAN_POINT('Origin',(-18.4031808061315,-57.6666181815461,39.3343017080178));
#201806=CARTESIAN_POINT('Origin',(-18.3780421908663,-57.5892494801765,39.1934008533553));
#201807=CARTESIAN_POINT('Origin',(-25.2734729067959,-55.9845461696115,39.1925554495081));
#201808=CARTESIAN_POINT('Origin',(-25.2915084057485,-56.0249274780511,39.1160373285261));
#201809=CARTESIAN_POINT('Origin',(-25.2401862573144,-55.9097831300745,39.3343017080178));
#201810=CARTESIAN_POINT('Ctrl Pts',(-25.1949317875303,-55.8095395120006,
39.2708017080178));
#201811=CARTESIAN_POINT('Ctrl Pts',(-25.0796311836956,-55.8614118841077,
39.2710850691867));
#201812=CARTESIAN_POINT('Ctrl Pts',(-25.1241659841938,-55.9614386837452,
39.3343017080178));
#201813=CARTESIAN_POINT('Ctrl Pts',(-25.1767321129116,-55.7683775656456,
39.3487519293518));
#201814=CARTESIAN_POINT('Ctrl Pts',(-25.0612313830313,-55.820085255182,
39.3492068662941));
#201815=CARTESIAN_POINT('Ctrl Pts',(-25.0967080045988,-55.8997670518376,
39.451227124875));
#201816=CARTESIAN_POINT('Ctrl Pts',(-25.1422534028251,-55.6903961807894,
39.3978017080178));
#201817=CARTESIAN_POINT('Ctrl Pts',(-25.0264120100489,-55.7418796630205,
39.398034778116));
#201818=CARTESIAN_POINT('Ctrl Pts',(-25.0446893032921,-55.782931135772,
39.5248015355176));
#201819=CARTESIAN_POINT('Ctrl Pts',(-25.1059793847704,-55.60834955903,39.3978017080178));
#201820=CARTESIAN_POINT('Ctrl Pts',(-24.9899591116498,-55.6600051127007,
39.3978017080178));
#201821=CARTESIAN_POINT('Ctrl Pts',(-24.9899591116498,-55.6600051127007,
39.5248017080178));
#201822=CARTESIAN_POINT('Origin',(-25.1059793847704,-55.60834955903,39.5248017080178));
#201823=CARTESIAN_POINT('Origin',(-0.29005068280152,0.129138884176568,39.116));
#201824=CARTESIAN_POINT('Origin',(-25.4547063934086,-56.3916032444849,39.116));
#201825=CARTESIAN_POINT('Origin',(-0.29005068280152,0.129138884176568,39.5248017080178));
#201826=CARTESIAN_POINT('Origin',(-25.044477503395,-55.4702140717966,39.5248017080178));
#201827=CARTESIAN_POINT('Ctrl Pts',(-25.6742415049982,-56.8833377255393,
39.2875012672119));
#201828=CARTESIAN_POINT('Ctrl Pts',(-25.5577357840971,-56.9357219056858,
39.287208709576));
#201829=CARTESIAN_POINT('Ctrl Pts',(-25.5138485805639,-56.8366797759152,
39.3549016990123));
#201830=CARTESIAN_POINT('Ctrl Pts',(-25.6273680143765,-56.7783442778542,
39.1034939173931));
#201831=CARTESIAN_POINT('Ctrl Pts',(-25.5109042502547,-56.8305359187812,
39.1031692336344));
#201832=CARTESIAN_POINT('Ctrl Pts',(-25.4764485929318,-56.7526780286685,
39.2077507202309));
#201833=CARTESIAN_POINT('Ctrl Pts',(-25.543160832995,-56.5897276738852,
38.989));
#201834=CARTESIAN_POINT('Ctrl Pts',(-25.4268390553472,-56.6417212312951,
38.9887769311158));
#201835=CARTESIAN_POINT('Ctrl Pts',(-25.4092610357538,-56.6017723050722,
39.1161898712899));
#201836=CARTESIAN_POINT('Ctrl Pts',(-25.4547063934086,-56.3916032444849,
38.989));
#201837=CARTESIAN_POINT('Ctrl Pts',(-25.3385127913799,-56.4433359691574,
38.989));
#201838=CARTESIAN_POINT('Ctrl Pts',(-25.3386862495673,-56.4432587405967,
39.1161895903856));
#201839=CARTESIAN_POINT('Origin',(-25.6299342604998,-56.7851714777846,39.3548010137695));
#201840=CARTESIAN_POINT('Ctrl Pts',(-25.044477503395,-55.4702140717966,
39.3978017080178));
#201841=CARTESIAN_POINT('Ctrl Pts',(-24.9284572302744,-55.5218696254672,
39.3978017080178));
#201842=CARTESIAN_POINT('Ctrl Pts',(-24.9284572302744,-55.5218696254672,
39.5248017080178));
#201843=CARTESIAN_POINT('Ctrl Pts',(-25.0080814159056,-55.3878899076699,
39.3978017080178));
#201844=CARTESIAN_POINT('Ctrl Pts',(-24.8918114493205,-55.4395618538397,
39.3975666025031));
#201845=CARTESIAN_POINT('Ctrl Pts',(-24.8735420580984,-55.3985281293147,
39.5248015517182));
#201846=CARTESIAN_POINT('Ctrl Pts',(-24.9736678430976,-55.3100454158615,
39.3484894016716));
#201847=CARTESIAN_POINT('Ctrl Pts',(-24.8573359723236,-55.362128664702,
39.3480259000042));
#201848=CARTESIAN_POINT('Ctrl Pts',(-24.8216158475493,-55.2818999508919,
39.4508333188947));
#201849=CARTESIAN_POINT('Ctrl Pts',(-24.9555320242418,-55.2690209153039,
39.2708017080178));
#201850=CARTESIAN_POINT('Ctrl Pts',(-24.8391888661847,-55.3213695969755,
39.27051194648));
#201851=CARTESIAN_POINT('Ctrl Pts',(-24.794250328961,-55.2204359898055,
39.3343017080178));
#201852=CARTESIAN_POINT('Origin',(-24.9102706020816,-55.1687804361349,39.3343017080178));
#201853=CARTESIAN_POINT('Origin',(-25.7023940320537,-56.9479187893842,39.6398955068173));
#201854=CARTESIAN_POINT('Origin',(-25.774853803565,-57.1106661007664,39.92499));
#201855=CARTESIAN_POINT('Origin',(-24.8771824671422,-55.0944632682979,39.1934008539941));
#201856=CARTESIAN_POINT('Origin',(-24.8590452239607,-55.0536014459531,39.1160402713853));
#201857=CARTESIAN_POINT('Ctrl Pts',(-25.61970381813,-57.5052637377731,40.1599502534424));
#201858=CARTESIAN_POINT('Ctrl Pts',(-25.6045223014064,-57.4711877340328,
40.10025));
#201859=CARTESIAN_POINT('Ctrl Pts',(-25.5758735661211,-57.4068835917978,
40.10025));
#201860=CARTESIAN_POINT('Ctrl Pts',(-25.7001924885134,-57.469404346587,
40.1599500538473));
#201861=CARTESIAN_POINT('Ctrl Pts',(-25.663150109512,-57.4450643815409,
40.1002448353499));
#201862=CARTESIAN_POINT('Ctrl Pts',(-25.6224598624455,-57.3861185493457,
40.10025));
#201863=CARTESIAN_POINT('Ctrl Pts',(-25.7642825572405,-57.4134642487751,
40.1202442001039));
#201864=CARTESIAN_POINT('Ctrl Pts',(-25.7077329912392,-57.3998804953991,
40.0633873868018));
#201865=CARTESIAN_POINT('Ctrl Pts',(-25.6552692732808,-57.344105919183,
40.0772271723537));
#201866=CARTESIAN_POINT('Ctrl Pts',(-25.8321626496791,-57.3036982377902,
40.0045995998162));
#201867=CARTESIAN_POINT('Ctrl Pts',(-25.7409042554408,-57.3186021074447,
39.9663485808315));
#201868=CARTESIAN_POINT('Ctrl Pts',(-25.6821129719827,-57.2526112478169,
40.0101727202466));
#201869=CARTESIAN_POINT('Ctrl Pts',(-25.8376543496551,-57.2503778226939,
39.930465434986));
#201870=CARTESIAN_POINT('Ctrl Pts',(-25.7289491719104,-57.2821097063817,
39.9051900162949));
#201871=CARTESIAN_POINT('Ctrl Pts',(-25.677329395237,-57.2038640469266,
39.9671857458174));
#201872=CARTESIAN_POINT('Ctrl Pts',(-25.8191582032623,-57.2088336324698,
39.8576902534424));
#201873=CARTESIAN_POINT('Ctrl Pts',(-25.7028284190336,-57.2611357920724,
39.8573998014387));
#201874=CARTESIAN_POINT('Ctrl Pts',(-25.6588335304443,-57.162321654437,
39.92499));
#201875=CARTESIAN_POINT('Origin',(-25.5758735661211,-57.4068835917978,40.22725));
#201876=CARTESIAN_POINT('Origin',(-0.29005068280152,0.129138884176568,39.116));
#201877=CARTESIAN_POINT('Origin',(-24.695750338031,-54.6869600343296,39.116));
#201878=CARTESIAN_POINT('Origin',(3.68589728140384E-17,1.50634138525679E-16,
40.22725));
#201879=CARTESIAN_POINT('Origin',(-25.5480287005721,-57.4192809246788,40.22725));
#201880=CARTESIAN_POINT('Ctrl Pts',(-24.695750338031,-54.6869600343296,
38.989));
#201881=CARTESIAN_POINT('Ctrl Pts',(-24.5795562613021,-54.7386929703522,
38.989));
#201882=CARTESIAN_POINT('Ctrl Pts',(-24.5797301948983,-54.7386155301259,
39.1161901092322));
#201883=CARTESIAN_POINT('Ctrl Pts',(-24.6072881749585,-54.4888352915933,
38.989));
#201884=CARTESIAN_POINT('Ctrl Pts',(-24.491381933525,-54.540648923419,38.9892298989742));
#201885=CARTESIAN_POINT('Ctrl Pts',(-24.5091541605496,-54.5800991622545,
39.1161900493184));
#201886=CARTESIAN_POINT('Ctrl Pts',(-24.5230714236759,-54.3002245846705,
39.1034966344368));
#201887=CARTESIAN_POINT('Ctrl Pts',(-24.4074205468501,-54.352067335488,
39.1038314102576));
#201888=CARTESIAN_POINT('Ctrl Pts',(-24.4419671033166,-54.4291945615868,
39.2077528789616));
#201889=CARTESIAN_POINT('Ctrl Pts',(-24.4761921430394,-54.1952354911871,
39.2875012672119));
#201890=CARTESIAN_POINT('Ctrl Pts',(-24.3607210114368,-54.247177787347,
39.2878045257868));
#201891=CARTESIAN_POINT('Ctrl Pts',(-24.404567574091,-54.3451938439591,
39.3549015295899));
#201892=CARTESIAN_POINT('Origin',(-24.5205222915154,-54.2933913980362,39.3548010137695));
#201893=CARTESIAN_POINT('Ctrl Pts',(-25.2380597013433,-57.4675553545139,
39.8576902534424));
#201894=CARTESIAN_POINT('Ctrl Pts',(-25.3547675996718,-57.4161024530842,
39.8573998014387));
#201895=CARTESIAN_POINT('Ctrl Pts',(-25.3107727110825,-57.3172883154489,
39.92499));
#201896=CARTESIAN_POINT('Ctrl Pts',(-25.2565651278915,-57.509118023269,
39.9304984902491));
#201897=CARTESIAN_POINT('Ctrl Pts',(-25.352874997054,-57.44956723289,39.9052171569792));
#201898=CARTESIAN_POINT('Ctrl Pts',(-25.3292770036982,-57.3588496371387,
39.9672049726599));
#201899=CARTESIAN_POINT('Ctrl Pts',(-25.2997972770059,-57.5405471770609,
40.0043437678661));
#201900=CARTESIAN_POINT('Ctrl Pts',(-25.3720159720861,-57.4827148996387,
39.9661628577643));
#201901=CARTESIAN_POINT('Ctrl Pts',(-25.3622324578623,-57.3948558336731,
40.0100243556235));
#201902=CARTESIAN_POINT('Ctrl Pts',(-25.4257977880274,-57.5636463159493,
40.1194874821988));
#201903=CARTESIAN_POINT('Ctrl Pts',(-25.4538910783601,-57.5124644612009,
40.0627551483141));
#201904=CARTESIAN_POINT('Ctrl Pts',(-25.4475597357239,-57.4360631077223,
40.0767884282377));
#201905=CARTESIAN_POINT('Ctrl Pts',(-25.5110385513887,-57.553621128909,
40.1599502015387));
#201906=CARTESIAN_POINT('Ctrl Pts',(-25.5177778164707,-57.5097883065925,
40.1002449453854));
#201907=CARTESIAN_POINT('Ctrl Pts',(-25.5012707422378,-57.4400754463039,
40.10025));
#201908=CARTESIAN_POINT('Ctrl Pts',(-25.5918112338797,-57.5176823163887,
40.1599502534424));
#201909=CARTESIAN_POINT('Ctrl Pts',(-25.5766462455179,-57.4835989537476,
40.10025));
#201910=CARTESIAN_POINT('Ctrl Pts',(-25.5480287005721,-57.4192809246788,
40.10025));
#201911=CARTESIAN_POINT('Origin',(-25.1947524379619,-57.3689438691195,39.92499));
#201912=CARTESIAN_POINT('Origin',(-24.4480624203116,-54.1306438627471,39.6398955069335));
#201913=CARTESIAN_POINT('Origin',(-24.3756025490941,-53.9678963272934,39.92499));
#201914=CARTESIAN_POINT('Origin',(-25.1222926664881,-57.2061965577042,39.6398955068267));
#201915=CARTESIAN_POINT('Origin',(-25.0498328948967,-57.0434492461378,39.3548010137695));
#201916=CARTESIAN_POINT('Ctrl Pts',(-24.331269253109,-53.8697418420144,
39.8576902534424));
#201917=CARTESIAN_POINT('Ctrl Pts',(-24.2159747902189,-53.9216078643416,
39.8579948730703));
#201918=CARTESIAN_POINT('Ctrl Pts',(-24.2595822759735,-54.019551880964,
39.92499));
#201919=CARTESIAN_POINT('Ctrl Pts',(-24.3127882662189,-53.8282341734838,
39.930402071123));
#201920=CARTESIAN_POINT('Ctrl Pts',(-24.2176496934291,-53.8880114973683,
39.905891529738));
#201921=CARTESIAN_POINT('Ctrl Pts',(-24.2411010091823,-53.9780422761226,
39.9671523786023));
#201922=CARTESIAN_POINT('Ctrl Pts',(-24.2697746459841,-53.7969955864427,
40.0043257306694));
#201923=CARTESIAN_POINT('Ctrl Pts',(-24.198315211449,-53.854948073304,39.9667894847838));
#201924=CARTESIAN_POINT('Ctrl Pts',(-24.2082687574724,-53.9422730280818,
40.0100138975201));
#201925=CARTESIAN_POINT('Ctrl Pts',(-24.1443388226042,-53.7744913425364,
40.1195533054856));
#201926=CARTESIAN_POINT('Ctrl Pts',(-24.1165167429226,-53.8256450222189,
40.0630813209233));
#201927=CARTESIAN_POINT('Ctrl Pts',(-24.1232032230477,-53.9017956184507,
40.076826594242));
#201928=CARTESIAN_POINT('Ctrl Pts',(-24.0595120258535,-53.7848917482049,
40.1599502027517));
#201929=CARTESIAN_POINT('Ctrl Pts',(-24.0529122166833,-53.828668515861,
40.1002552791541));
#201930=CARTESIAN_POINT('Ctrl Pts',(-24.0696665464382,-53.8982652496117,
40.10025));
#201931=CARTESIAN_POINT('Ctrl Pts',(-23.9791663275016,-53.8206887816835,
40.1599502534424));
#201932=CARTESIAN_POINT('Ctrl Pts',(-23.994348378682,-53.854764547308,40.10025));
#201933=CARTESIAN_POINT('Ctrl Pts',(-24.0229981225299,-53.9190682401994,
40.10025));
#201934=CARTESIAN_POINT('Origin',(-24.0229981225299,-53.9190682401994,40.22725));
#201935=CARTESIAN_POINT('Ctrl Pts',(-24.8746050278055,-56.6498810128381,
38.989));
#201936=CARTESIAN_POINT('Ctrl Pts',(-24.9907986398447,-56.5981482837086,
38.989));
#201937=CARTESIAN_POINT('Ctrl Pts',(-24.9906251716318,-56.598225516733,
39.1161896013271));
#201938=CARTESIAN_POINT('Ctrl Pts',(-24.9626539694736,-56.848189676975,
38.989));
#201939=CARTESIAN_POINT('Ctrl Pts',(-25.0791271905724,-56.7965362315742,
38.9887769275436));
#201940=CARTESIAN_POINT('Ctrl Pts',(-25.0612010539377,-56.7567415443524,
39.1161898821829));
#201941=CARTESIAN_POINT('Ctrl Pts',(-25.0464771582516,-57.036975459333,
39.1034967087243));
#201942=CARTESIAN_POINT('Ctrl Pts',(-25.1631925873323,-56.9853490357247,
39.1031720232723));
#201943=CARTESIAN_POINT('Ctrl Pts',(-25.1283880784746,-56.907646072766,
39.2077529615014));
#201944=CARTESIAN_POINT('Ctrl Pts',(-25.0931373005748,-57.142061986502,
39.2875012672119));
#201945=CARTESIAN_POINT('Ctrl Pts',(-25.2100238867505,-57.0905332166518,
39.2872087095507));
#201946=CARTESIAN_POINT('Ctrl Pts',(-25.1657874977295,-56.9916465440537,
39.354901704823));
#201947=CARTESIAN_POINT('Origin',(-24.8746050278055,-56.6498810128381,39.116));
#201948=CARTESIAN_POINT('Origin',(3.8811097157961E-16,-5.3586061441408E-17,
40.22725));
#201949=CARTESIAN_POINT('Origin',(-23.995153256981,-53.9314655730803,40.22725));
#201950=CARTESIAN_POINT('Origin',(10.5838037820519,22.99100911823,39.116));
#201951=CARTESIAN_POINT('Origin',(-24.7113125977908,-56.2832472948502,39.1160373285277));
#201952=CARTESIAN_POINT('Ctrl Pts',(-23.9513722670367,-53.8330634946837,
40.1599502534424));
#201953=CARTESIAN_POINT('Ctrl Pts',(-23.9665367208226,-53.8671470951729,
40.10025));
#201954=CARTESIAN_POINT('Ctrl Pts',(-23.995153256981,-53.9314655730803,
40.10025));
#201955=CARTESIAN_POINT('Ctrl Pts',(-23.8712821658119,-53.8686972660497,
40.1599500566041));
#201956=CARTESIAN_POINT('Ctrl Pts',(-23.9081865738556,-53.8931046959193,
40.100255130536));
#201957=CARTESIAN_POINT('Ctrl Pts',(-23.9486256024598,-53.9521563342723,
40.10025));
#201958=CARTESIAN_POINT('Ctrl Pts',(-23.8071866393157,-53.9240892607409,
40.1203070619047));
#201959=CARTESIAN_POINT('Ctrl Pts',(-23.8635355386145,-53.9378509529596,
40.0637098684497));
#201960=CARTESIAN_POINT('Ctrl Pts',(-23.915575084618,-53.9937257232526,
40.0772636213363));
#201961=CARTESIAN_POINT('Ctrl Pts',(-23.7392497560571,-54.0330064121714,
40.0046102245801));
#201962=CARTESIAN_POINT('Ctrl Pts',(-23.8300830854579,-54.0187512923762,
39.9670001894015));
#201963=CARTESIAN_POINT('Ctrl Pts',(-23.8883623535218,-54.0845104630312,
40.0101788811209));
#201964=CARTESIAN_POINT('Ctrl Pts',(-23.7337507958619,-54.0860594545422,
39.9303710930186));
#201965=CARTESIAN_POINT('Ctrl Pts',(-23.8418399747443,-54.0553500291285,
39.9058663574115));
#201966=CARTESIAN_POINT('Ctrl Pts',(-23.8930480394871,-54.1330265677743,
39.9671344706369));
#201967=CARTESIAN_POINT('Ctrl Pts',(-23.752222950883,-54.1275498658872,
39.8576902534424));
#201968=CARTESIAN_POINT('Ctrl Pts',(-23.8679139708571,-54.0765745253535,
39.8579948730703));
#201969=CARTESIAN_POINT('Ctrl Pts',(-23.9115214566117,-54.1745185419759,
39.92499));
#201970=CARTESIAN_POINT('Origin',(-23.7955011834911,-54.2261740956465,39.92499));
#201971=CARTESIAN_POINT('Origin',(-24.6933715410276,-56.2428239368544,39.1925554488836));
#201972=CARTESIAN_POINT('Origin',(-24.6600848917114,-56.1680608984277,39.3343017080178));
#201973=CARTESIAN_POINT('Origin',(-23.8679610547539,-54.3889216310586,39.6398955069213));
#201974=CARTESIAN_POINT('Origin',(-23.9404209259123,-54.5516691663894,39.3548010137695));
#201975=CARTESIAN_POINT('Ctrl Pts',(-24.5258780191674,-55.8666273273832,
39.3978017080178));
#201976=CARTESIAN_POINT('Ctrl Pts',(-24.641898292288,-55.8149717737125,
39.3978017080178));
#201977=CARTESIAN_POINT('Ctrl Pts',(-24.641898292288,-55.8149717737125,
39.5248017080178));
#201978=CARTESIAN_POINT('Ctrl Pts',(-24.5627025231283,-55.9487607347574,
39.3978017080178));
#201979=CARTESIAN_POINT('Ctrl Pts',(-24.6784744708792,-55.8971232158788,
39.3980355775163));
#201980=CARTESIAN_POINT('Ctrl Pts',(-24.6968134595441,-55.938313258815,
39.5248015517178));
#201981=CARTESIAN_POINT('Ctrl Pts',(-24.5975211960713,-56.0264248009281,
39.3484893995498));
#201982=CARTESIAN_POINT('Ctrl Pts',(-24.713232510496,-55.9751910510455,
39.3489438303431));
#201983=CARTESIAN_POINT('Ctrl Pts',(-24.7487396569161,-56.0549414076414,
39.4508333155604));
#201984=CARTESIAN_POINT('Ctrl Pts',(-24.6158705164596,-56.0673542004325,
39.2708017080178));
#201985=CARTESIAN_POINT('Ctrl Pts',(-24.7315703643338,-56.0163785451196,
39.2710850691866));
#201986=CARTESIAN_POINT('Ctrl Pts',(-24.776105164832,-56.1164053447571,
39.3343017080178));
#201987=CARTESIAN_POINT('Origin',(-24.5258780191674,-55.8666273273832,39.5248017080178));
#201988=CARTESIAN_POINT('Ctrl Pts',(-23.8971395307771,-54.4530463244691,
39.2875012672119));
#201989=CARTESIAN_POINT('Ctrl Pts',(-24.0130054343468,-54.4019907365348,
39.2878045257519));
#201990=CARTESIAN_POINT('Ctrl Pts',(-24.0565064908996,-54.5001606088507,
39.354901521835));
#201991=CARTESIAN_POINT('Ctrl Pts',(-23.9437939758168,-54.5581374230419,
39.1034938540228));
#201992=CARTESIAN_POINT('Ctrl Pts',(-24.0597061770695,-54.5068816478228,
39.1038286278817));
#201993=CARTESIAN_POINT('Ctrl Pts',(-24.0939065860602,-54.5841625982685,
39.2077506434042));
#201994=CARTESIAN_POINT('Ctrl Pts',(-24.0276077026095,-54.7469293531954,
38.989));
#201995=CARTESIAN_POINT('Ctrl Pts',(-24.1436691352872,-54.6954643138447,
38.9892298954587));
#201996=CARTESIAN_POINT('Ctrl Pts',(-24.1610941752721,-54.7350683949965,
39.1161900347276));
#201997=CARTESIAN_POINT('Ctrl Pts',(-24.1156489724279,-54.9452378026827,
38.989));
#201998=CARTESIAN_POINT('Ctrl Pts',(-24.2318430357375,-54.8935048726347,
38.989));
#201999=CARTESIAN_POINT('Ctrl Pts',(-24.2316691155806,-54.8935823068775,
39.116190094565));
#202000=CARTESIAN_POINT('Origin',(-24.1156489724279,-54.9452378026828,39.116));
#202001=CARTESIAN_POINT('Origin',(10.3344596589369,22.4309730483568,39.5248017080178));
#202002=CARTESIAN_POINT('Origin',(-24.4643761377919,-55.7284918401497,39.5248017080178));
#202003=CARTESIAN_POINT('Origin',(10.2954134679533,22.3432738675267,39.116));
#202004=CARTESIAN_POINT('Origin',(-24.2788510342447,-55.3119205422644,39.1160402713849));
#202005=CARTESIAN_POINT('Ctrl Pts',(-24.3743766270216,-55.5277679687682,
39.2708017080178));
#202006=CARTESIAN_POINT('Ctrl Pts',(-24.4911280468229,-55.4763362579873,
39.27051194648));
#202007=CARTESIAN_POINT('Ctrl Pts',(-24.4461895095991,-55.3754026508174,
39.3343017080178));
#202008=CARTESIAN_POINT('Ctrl Pts',(-24.3927905570426,-55.5688345658066,
39.3487519301186));
#202009=CARTESIAN_POINT('Ctrl Pts',(-24.5093364964831,-55.5172331055199,
39.3482879463987));
#202010=CARTESIAN_POINT('Ctrl Pts',(-24.4736474994194,-55.4370743056912,
39.4512271261644));
#202011=CARTESIAN_POINT('Ctrl Pts',(-24.4276751358079,-55.6466353090196,
39.3978017080178));
#202012=CARTESIAN_POINT('Ctrl Pts',(-24.543873985031,-55.5948055748773,
39.3975673827397));
#202013=CARTESIAN_POINT('Ctrl Pts',(-24.5256662135199,-55.553910250492,
39.5248015355181));
#202014=CARTESIAN_POINT('Ctrl Pts',(-24.4643761377919,-55.7284918401497,
39.3978017080178));
#202015=CARTESIAN_POINT('Ctrl Pts',(-24.5803964109126,-55.6768362864791,
39.3978017080178));
#202016=CARTESIAN_POINT('Ctrl Pts',(-24.5803964109126,-55.6768362864791,
39.5248017080178));
#202017=CARTESIAN_POINT('Origin',(-24.3301692364785,-55.427058204488,39.3343017080178));
#202018=CARTESIAN_POINT('Origin',(-24.2970811017213,-55.3527410377814,39.1934008533551));
#202019=CARTESIAN_POINT('Origin',(-30.9870007556527,-53.0360596835509,39.1925554495085));
#202020=CARTESIAN_POINT('Origin',(-31.0091584503705,-53.0743345559677,39.1160373285265));
#202021=CARTESIAN_POINT('Origin',(-30.9460815882871,-52.9651856060844,39.3343017080178));
#202022=CARTESIAN_POINT('Ctrl Pts',(-30.8905967158739,-52.8702215132214,
39.2708017080178));
#202023=CARTESIAN_POINT('Ctrl Pts',(-30.7813498801535,-52.9338619179794,
39.2710850691866));
#202024=CARTESIAN_POINT('Ctrl Pts',(-30.8360963620065,-53.0286856060844,
39.3343017080178));
#202025=CARTESIAN_POINT('Ctrl Pts',(-30.868194145979,-52.8311874403355,
39.3487519293518));
#202026=CARTESIAN_POINT('Ctrl Pts',(-30.7587310665072,-52.894684983538,
39.3492068662937));
#202027=CARTESIAN_POINT('Ctrl Pts',(-30.8023423591855,-52.9702219582397,
39.4512271248747));
#202028=CARTESIAN_POINT('Ctrl Pts',(-30.8257530395505,-52.7572372522462,
39.3978017080178));
#202029=CARTESIAN_POINT('Ctrl Pts',(-30.7159277273266,-52.8205474253453,
39.398034778116));
#202030=CARTESIAN_POINT('Ctrl Pts',(-30.7383959430076,-52.8594635164577,
39.5248015355176));
#202031=CARTESIAN_POINT('Ctrl Pts',(-30.7811015270746,-52.6794317578286,
39.3978017080178));
#202032=CARTESIAN_POINT('Ctrl Pts',(-30.671116300794,-52.7429317578286,
39.3978017080178));
#202033=CARTESIAN_POINT('Ctrl Pts',(-30.671116300794,-52.7429317578286,
39.5248017080178));
#202034=CARTESIAN_POINT('Origin',(-30.7811015270746,-52.6794317578286,39.5248017080178));
#202035=CARTESIAN_POINT('Origin',(-0.274963065701553,0.158750000000001,
39.116));
#202036=CARTESIAN_POINT('Origin',(-31.2097904767608,-53.4219427993285,39.116));
#202037=CARTESIAN_POINT('Origin',(-0.274963065701553,0.158750000000001,
39.5248017080178));
#202038=CARTESIAN_POINT('Origin',(-30.7054974692372,-52.5484816883958,39.5248017080178));
#202039=CARTESIAN_POINT('Ctrl Pts',(-31.4795232016792,-53.8880358395969,
39.2875012672119));
#202040=CARTESIAN_POINT('Ctrl Pts',(-31.3691313491575,-53.9523112176912,
39.287208709576));
#202041=CARTESIAN_POINT('Ctrl Pts',(-31.3151318426937,-53.8583991130128,
39.3549016990124));
#202042=CARTESIAN_POINT('Ctrl Pts',(-31.4219316852012,-53.7885171709481,
39.1034939173931));
#202043=CARTESIAN_POINT('Ctrl Pts',(-31.3115614337855,-53.8525966788964,
39.1031692336333));
#202044=CARTESIAN_POINT('Ctrl Pts',(-31.2691561625558,-53.7787668993605,
39.2077507202313));
#202045=CARTESIAN_POINT('Ctrl Pts',(-31.3184699958134,-53.6097358757351,
38.989));
#202046=CARTESIAN_POINT('Ctrl Pts',(-31.2082202476906,-53.6736035436587,
38.988776931117));
#202047=CARTESIAN_POINT('Ctrl Pts',(-31.1865627224597,-53.6357108652095,
39.1161898712894));
#202048=CARTESIAN_POINT('Ctrl Pts',(-31.2097904767608,-53.4219427993285,
38.989));
#202049=CARTESIAN_POINT('Ctrl Pts',(-31.0996409376522,-53.485537665384,
38.989));
#202050=CARTESIAN_POINT('Ctrl Pts',(-31.0998053730349,-53.4854427285716,
39.1161895903857));
#202051=CARTESIAN_POINT('Origin',(-31.4251975098795,-53.7950387249977,39.3548010137695));
#202052=CARTESIAN_POINT('Ctrl Pts',(-30.7054974692372,-52.5484816883958,
39.3978017080178));
#202053=CARTESIAN_POINT('Ctrl Pts',(-30.5955122429565,-52.6119816883958,
39.3978017080178));
#202054=CARTESIAN_POINT('Ctrl Pts',(-30.5955122429565,-52.6119816883958,
39.5248017080178));
#202055=CARTESIAN_POINT('Ctrl Pts',(-30.6606955449582,-52.4704129317476,
39.3978017080178));
#202056=CARTESIAN_POINT('Ctrl Pts',(-30.5504637065407,-52.5339553345193,
39.3975666025021));
#202057=CARTESIAN_POINT('Ctrl Pts',(-30.5280052047889,-52.4950560684209,
39.5248015517178));
#202058=CARTESIAN_POINT('Ctrl Pts',(-30.6183335281985,-52.3965920780925,
39.3484894016717));
#202059=CARTESIAN_POINT('Ctrl Pts',(-30.5080831175518,-52.4605500011291,
39.3480259000039));
#202060=CARTESIAN_POINT('Ctrl Pts',(-30.4641724871919,-52.3844945583577,
39.4508333188946));
#202061=CARTESIAN_POINT('Ctrl Pts',(-30.5960088312571,-52.3576880233161,
39.2708017080178));
#202062=CARTESIAN_POINT('Ctrl Pts',(-30.4857749404423,-52.4219111049555,
39.27051194648));
#202063=CARTESIAN_POINT('Ctrl Pts',(-30.4305321463779,-52.326227778884,
39.3343017080178));
#202064=CARTESIAN_POINT('Origin',(-30.5405173726585,-52.262727778884,39.3343017080178));
#202065=CARTESIAN_POINT('Origin',(-31.5142720656056,-53.9493203812217,39.63989550682));
#202066=CARTESIAN_POINT('Origin',(-31.6033466212668,-54.1036020372437,39.92499));
#202067=CARTESIAN_POINT('Origin',(-30.4998422386362,-52.1922763801648,39.1934008539946));
#202068=CARTESIAN_POINT('Origin',(-30.4775331296743,-52.1535342613172,39.1160402713852));
#202069=CARTESIAN_POINT('Ctrl Pts',(-31.490293248291,-54.5122556166609,
40.1599502534424));
#202070=CARTESIAN_POINT('Ctrl Pts',(-31.4716329851992,-54.4799531854478,
40.10025));
#202071=CARTESIAN_POINT('Ctrl Pts',(-31.4364195775137,-54.4189959163062,
40.10025));
#202072=CARTESIAN_POINT('Ctrl Pts',(-31.5665926662616,-54.4681793099457,
40.1599500538464));
#202073=CARTESIAN_POINT('Ctrl Pts',(-31.5272089901454,-54.4478446647266,
40.1002448353503));
#202074=CARTESIAN_POINT('Ctrl Pts',(-31.4805801312539,-54.3934750329625,
40.10025));
#202075=CARTESIAN_POINT('Ctrl Pts',(-31.6244843104275,-54.4058464214485,
40.120244200104));
#202076=CARTESIAN_POINT('Ctrl Pts',(-31.5668246399996,-54.3982481205271,
40.0633873868015));
#202077=CARTESIAN_POINT('Ctrl Pts',(-31.5088182930364,-54.3482630350911,
40.0772271723538));
#202078=CARTESIAN_POINT('Ctrl Pts',(-31.6805188761698,-54.2895863184076,
40.0045995998161));
#202079=CARTESIAN_POINT('Ctrl Pts',(-31.5913182835557,-54.3139476428151,
39.9663485808318));
#202080=CARTESIAN_POINT('Ctrl Pts',(-31.5259511417531,-54.2544636505341,
40.0101727202466));
#202081=CARTESIAN_POINT('Ctrl Pts',(-31.6804069909878,-54.2359839591652,
39.930465434986));
#202082=CARTESIAN_POINT('Ctrl Pts',(-31.5756141966199,-54.2789047974526,
39.9051900162944));
#202083=CARTESIAN_POINT('Ctrl Pts',(-31.5160982999437,-54.2064835118371,
39.9671857458173));
#202084=CARTESIAN_POINT('Ctrl Pts',(-31.6576696180587,-54.1966007261206,
39.8576902534424));
#202085=CARTESIAN_POINT('Ctrl Pts',(-31.5474441649286,-54.2607761425981,
39.8573998014387));
#202086=CARTESIAN_POINT('Ctrl Pts',(-31.4933613949861,-54.1671020372437,
39.92499));
#202087=CARTESIAN_POINT('Origin',(-31.4364195775137,-54.4189959163062,40.22725));
#202088=CARTESIAN_POINT('Origin',(-0.274963065701553,0.158750000000001,
39.116));
#202089=CARTESIAN_POINT('Origin',(-30.2768083268883,-51.8059703131945,39.116));
#202090=CARTESIAN_POINT('Origin',(5.22371297615238E-17,1.42798576194616E-16,
40.22725));
#202091=CARTESIAN_POINT('Origin',(-31.4100231232064,-54.4342359163062,40.22725));
#202092=CARTESIAN_POINT('Ctrl Pts',(-30.2768083268883,-51.8059703131945,
38.989));
#202093=CARTESIAN_POINT('Ctrl Pts',(-30.1666583377715,-51.8695654390623,
38.989));
#202094=CARTESIAN_POINT('Ctrl Pts',(-30.166823223834,-51.8694702420497,
39.1161901092329));
#202095=CARTESIAN_POINT('Ctrl Pts',(-30.1681210939101,-51.6181777324909,
38.989));
#202096=CARTESIAN_POINT('Ctrl Pts',(-30.0582657983061,-51.6818230251232,
38.9892298989718));
#202097=CARTESIAN_POINT('Ctrl Pts',(-30.0800643400517,-51.7191994478448,
39.1161900493191));
#202098=CARTESIAN_POINT('Ctrl Pts',(-30.0646505034512,-51.4394033023488,
39.1034966344368));
#202099=CARTESIAN_POINT('Ctrl Pts',(-29.9550522173005,-51.5030508615808,
39.1038314102583));
#202100=CARTESIAN_POINT('Ctrl Pts',(-29.9974715145359,-51.5761444782056,
39.2077528789608));
#202101=CARTESIAN_POINT('Ctrl Pts',(-30.007053683816,-51.3398895692696,
39.2875012672119));
#202102=CARTESIAN_POINT('Ctrl Pts',(-29.8976445635498,-51.4036173400348,
39.2878045257868));
#202103=CARTESIAN_POINT('Ctrl Pts',(-29.9514963979202,-51.4965132406196,
39.3549015295903));
#202104=CARTESIAN_POINT('Origin',(-30.0614010732039,-51.4328740054941,39.3548010137695));
#202105=CARTESIAN_POINT('Ctrl Pts',(-31.1067982185537,-54.5146464769136,
39.8576902534424));
#202106=CARTESIAN_POINT('Ctrl Pts',(-31.2174884860867,-54.4512761425981,
39.8573998014387));
#202107=CARTESIAN_POINT('Ctrl Pts',(-31.1634057161443,-54.3576020372437,
39.92499));
#202108=CARTESIAN_POINT('Ctrl Pts',(-31.1295467523325,-54.5540471172216,
39.930498490249));
#202109=CARTESIAN_POINT('Ctrl Pts',(-31.2191042733518,-54.4847554296818,
39.9052171569786));
#202110=CARTESIAN_POINT('Ctrl Pts',(-31.1861529813961,-54.3970014563931,
39.9672049726603));
#202111=CARTESIAN_POINT('Ctrl Pts',(-31.1758273123592,-54.5807851087096,
40.0043437678664));
#202112=CARTESIAN_POINT('Ctrl Pts',(-31.2416052667856,-54.515720733339,
39.9661628577646));
#202113=CARTESIAN_POINT('Ctrl Pts',(-31.2226915745266,-54.4293656242362,
40.0100243556236));
#202114=CARTESIAN_POINT('Ctrl Pts',(-31.3035520968882,-54.5905870683101,
40.1194874821985));
#202115=CARTESIAN_POINT('Ctrl Pts',(-31.3261415286127,-54.53674904465,40.0627551483138));
#202116=CARTESIAN_POINT('Ctrl Pts',(-31.3118587536634,-54.4614280312965,
40.0767884282376));
#202117=CARTESIAN_POINT('Ctrl Pts',(-31.3872779850339,-54.5717067142918,
40.1599502015391));
#202118=CARTESIAN_POINT('Ctrl Pts',(-31.3893985541603,-54.5274095677415,
40.1002449453869));
#202119=CARTESIAN_POINT('Ctrl Pts',(-31.3656949292512,-54.459804060898,
40.10025));
#202120=CARTESIAN_POINT('Ctrl Pts',(-31.4638515574743,-54.5275217339718,
40.1599502534424));
#202121=CARTESIAN_POINT('Ctrl Pts',(-31.4452069629856,-54.4952102564864,
40.10025));
#202122=CARTESIAN_POINT('Ctrl Pts',(-31.4100231232064,-54.4342359163062,
40.10025));
#202123=CARTESIAN_POINT('Origin',(-31.0534204898636,-54.4211020372437,39.92499));
#202124=CARTESIAN_POINT('Origin',(-29.9723263949891,-51.278592137217,39.6398955069325));
#202125=CARTESIAN_POINT('Origin',(-29.8832517167489,-51.1243102687783,39.92499));
#202126=CARTESIAN_POINT('Origin',(-30.9643459342343,-54.2668203811893,39.6398955068276));
#202127=CARTESIAN_POINT('Origin',(-30.8752713784764,-54.1125387249977,39.3548010137695));
#202128=CARTESIAN_POINT('Ctrl Pts',(-29.8289013456888,-51.0313275753407,
39.8576902534424));
#202129=CARTESIAN_POINT('Ctrl Pts',(-29.7196599535395,-51.0949610232,39.8579948730704));
#202130=CARTESIAN_POINT('Ctrl Pts',(-29.7732664904682,-51.1878102687783,
39.92499));
#202131=CARTESIAN_POINT('Ctrl Pts',(-29.8061828667729,-50.9919790793207,
39.9304020711232));
#202132=CARTESIAN_POINT('Ctrl Pts',(-29.7178139048428,-51.0613736255828,
39.9058915297387));
#202133=CARTESIAN_POINT('Ctrl Pts',(-29.7505475307855,-51.1484598763128,
39.967152378603));
#202134=CARTESIAN_POINT('Ctrl Pts',(-29.7601395581529,-50.9654077681506,
40.0043257306691));
#202135=CARTESIAN_POINT('Ctrl Pts',(-29.695129270271,-51.030512330103,39.9667894847838));
#202136=CARTESIAN_POINT('Ctrl Pts',(-29.7141562330557,-51.1163184807719,
40.01001389752));
#202137=CARTESIAN_POINT('Ctrl Pts',(-29.6330385513049,-50.9561384187037,
40.1195533054859));
#202138=CARTESIAN_POINT('Ctrl Pts',(-29.6107158994147,-51.0099200724109,
40.0630813209234));
#202139=CARTESIAN_POINT('Ctrl Pts',(-29.6253256551032,-51.0849545802163,
40.076826594242));
#202140=CARTESIAN_POINT('Ctrl Pts',(-29.5497635830448,-50.9753486645701,
40.1599502027514));
#202141=CARTESIAN_POINT('Ctrl Pts',(-29.5477758465707,-51.0195754864248,
40.1002552791554));
#202142=CARTESIAN_POINT('Ctrl Pts',(-29.5717132339809,-51.0870396576426,
40.10025));
#202143=CARTESIAN_POINT('Ctrl Pts',(-29.473599835734,-51.0193480105326,
40.1599502534424));
#202144=CARTESIAN_POINT('Ctrl Pts',(-29.4922606054649,-51.0516501490685,
40.10025));
#202145=CARTESIAN_POINT('Ctrl Pts',(-29.5274749692187,-51.1126068659045,
40.10025));
#202146=CARTESIAN_POINT('Origin',(-29.5274749692187,-51.1126068659046,40.22725));
#202147=CARTESIAN_POINT('Ctrl Pts',(-30.6598643453577,-53.7394427993285,
38.989));
#202148=CARTESIAN_POINT('Ctrl Pts',(-30.7700138939555,-53.6758479277944,
38.989));
#202149=CARTESIAN_POINT('Ctrl Pts',(-30.7698494490696,-53.6759428700936,
39.1161896013264));
#202150=CARTESIAN_POINT('Ctrl Pts',(-30.7681598456261,-53.9274614872887,
38.989));
#202151=CARTESIAN_POINT('Ctrl Pts',(-30.8785957589626,-53.8639162380558,
38.9887769275436));
#202152=CARTESIAN_POINT('Ctrl Pts',(-30.85660814608,-53.8262133418101,39.1161898821822));
#202153=CARTESIAN_POINT('Ctrl Pts',(-30.8712573299222,-54.1064511722687,
39.1034967087243));
#202154=CARTESIAN_POINT('Ctrl Pts',(-30.9819369489432,-54.0429074791677,
39.1031720232731));
#202155=CARTESIAN_POINT('Ctrl Pts',(-30.9392009315176,-53.9692682429941,
39.2077529615022));
#202156=CARTESIAN_POINT('Ctrl Pts',(-30.9286463962981,-54.206084711474,
39.2875012672119));
#202157=CARTESIAN_POINT('Ctrl Pts',(-31.0395064423976,-54.1426202463874,
39.2872087095507));
#202158=CARTESIAN_POINT('Ctrl Pts',(-30.9851759130207,-54.0488992470935,
39.3549017048226));
#202159=CARTESIAN_POINT('Origin',(-30.6598643453577,-53.7394427993285,39.116));
#202160=CARTESIAN_POINT('Origin',(3.8264039982802E-16,-5.07986659106881E-17,
40.22725));
#202161=CARTESIAN_POINT('Origin',(-29.5010785149114,-51.1278468659046,40.22725));
#202162=CARTESIAN_POINT('Origin',(15.8305769983926,26.7843636743469,39.116));
#202163=CARTESIAN_POINT('Origin',(-30.4591427892373,-53.3918862459816,39.1160373285268));
#202164=CARTESIAN_POINT('Ctrl Pts',(-29.4472515437738,-51.0345602039885,
40.1599502534424));
#202165=CARTESIAN_POINT('Ctrl Pts',(-29.4658956314769,-51.0668719738976,
40.10025));
#202166=CARTESIAN_POINT('Ctrl Pts',(-29.5010785149114,-51.1278468659046,
40.10025));
#202167=CARTESIAN_POINT('Ctrl Pts',(-29.3713249278648,-51.0783704650304,
40.1599500566043));
#202168=CARTESIAN_POINT('Ctrl Pts',(-29.4105784408359,-51.098786627384,
40.1002551305372));
#202169=CARTESIAN_POINT('Ctrl Pts',(-29.4569685172211,-51.1532877451684,
40.10025));
#202170=CARTESIAN_POINT('Ctrl Pts',(-29.3133705634514,-51.1401588234662,
40.1203070619046));
#202171=CARTESIAN_POINT('Ctrl Pts',(-29.3708492661238,-51.1479550638448,
40.0637098684497));
#202172=CARTESIAN_POINT('Ctrl Pts',(-29.4284442379234,-51.1980841325266,
40.0772636213363));
#202173=CARTESIAN_POINT('Ctrl Pts',(-29.2571907880104,-51.255580653351,
40.0046102245802));
#202174=CARTESIAN_POINT('Ctrl Pts',(-29.3460364571625,-51.2319089562574,
39.9670001894015));
#202175=CARTESIAN_POINT('Ctrl Pts',(-29.4108701703525,-51.2912160489645,
40.0101788811209));
#202176=CARTESIAN_POINT('Ctrl Pts',(-29.2572675046853,-51.3089178634634,
39.9303710930186));
#202177=CARTESIAN_POINT('Ctrl Pts',(-29.3615545506885,-51.2670782717308,
39.9058663574106));
#202178=CARTESIAN_POINT('Ctrl Pts',(-29.4206015015119,-51.3389765898554,
39.9671344706358));
#202179=CARTESIAN_POINT('Ctrl Pts',(-29.2799753962465,-51.3482501200164,
39.8576902534424));
#202180=CARTESIAN_POINT('Ctrl Pts',(-29.3897042746976,-51.2854610232,39.8579948730703));
#202181=CARTESIAN_POINT('Ctrl Pts',(-29.4433108116264,-51.3783102687783,
39.92499));
#202182=CARTESIAN_POINT('Origin',(-29.3333255853457,-51.4418102687783,39.92499));
#202183=CARTESIAN_POINT('Origin',(-30.4370746239675,-53.3535596824668,39.192555448885));
#202184=CARTESIAN_POINT('Origin',(-30.396155456884,-53.2826856060844,39.3343017080178));
#202185=CARTESIAN_POINT('Origin',(-29.4224002636276,-51.5960921371731,39.6398955069217));
#202186=CARTESIAN_POINT('Origin',(-29.5114749418008,-51.7503740054942,39.3548010137695));
#202187=CARTESIAN_POINT('Ctrl Pts',(-30.2311753956715,-52.9969317578286,
39.3978017080178));
#202188=CARTESIAN_POINT('Ctrl Pts',(-30.3411606219521,-52.9334317578286,
39.3978017080178));
#202189=CARTESIAN_POINT('Ctrl Pts',(-30.3411606219521,-52.9334317578286,
39.5248017080178));
#202190=CARTESIAN_POINT('Ctrl Pts',(-30.2763834500022,-53.074766020994,
39.3978017080178));
#202191=CARTESIAN_POINT('Ctrl Pts',(-30.386123596414,-53.0113099140565,
39.3980355775163));
#202192=CARTESIAN_POINT('Ctrl Pts',(-30.4086676540711,-53.0503573673268,
39.5248015517178));
#202193=CARTESIAN_POINT('Ctrl Pts',(-30.3191294881007,-53.1483650929077,
39.3484893995498));
#202194=CARTESIAN_POINT('Ctrl Pts',(-30.4288515386962,-53.0853168809912,
39.3489438303439));
#202195=CARTESIAN_POINT('Ctrl Pts',(-30.4725003554712,-53.1609188493363,
39.4508333155605));
#202196=CARTESIAN_POINT('Ctrl Pts',(-30.3416565762239,-53.1871522506173,
39.2708017080178));
#202197=CARTESIAN_POINT('Ctrl Pts',(-30.4513942013116,-53.1243619179794,
39.2710850691866));
#202198=CARTESIAN_POINT('Ctrl Pts',(-30.5061406831646,-53.2191856060844,
39.3343017080178));
#202199=CARTESIAN_POINT('Origin',(-30.2311753956715,-52.9969317578286,39.5248017080178));
#202200=CARTESIAN_POINT('Ctrl Pts',(-29.4581217525676,-51.6568155675426,
39.2875012672119));
#202201=CARTESIAN_POINT('Ctrl Pts',(-29.5680161684459,-51.5939283826161,
39.2878045257519));
#202202=CARTESIAN_POINT('Ctrl Pts',(-29.6215404675519,-51.6870133715069,
39.3549015218347));
#202203=CARTESIAN_POINT('Ctrl Pts',(-29.515505630711,-51.756454248638,39.1034938540228));
#202204=CARTESIAN_POINT('Ctrl Pts',(-29.6254251653826,-51.6933631336547,
39.1038286278833));
#202205=CARTESIAN_POINT('Ctrl Pts',(-29.6675162799448,-51.7666458147672,
39.2077506434047));
#202206=CARTESIAN_POINT('Ctrl Pts',(-29.6185943474775,-51.9354510367806,
38.989));
#202207=CARTESIAN_POINT('Ctrl Pts',(-29.7286404220049,-51.8721362050931,
38.9892298954593));
#202208=CARTESIAN_POINT('Ctrl Pts',(-29.7501097595406,-51.9097019182955,
39.116190034727));
#202209=CARTESIAN_POINT('Ctrl Pts',(-29.7268821954852,-52.1234703131945,
38.989));
#202210=CARTESIAN_POINT('Ctrl Pts',(-29.8370321718797,-52.0598751946719,
38.989));
#202211=CARTESIAN_POINT('Ctrl Pts',(-29.8368672985585,-52.0599703843283,
39.1161900945645));
#202212=CARTESIAN_POINT('Origin',(-29.7268821954852,-52.1234703131945,39.116));
#202213=CARTESIAN_POINT('Origin',(15.4537755657018,26.1317244485617,39.5248017080178));
#202214=CARTESIAN_POINT('Origin',(-30.155571337834,-52.8659816883958,39.5248017080178));
#202215=CARTESIAN_POINT('Origin',(15.3947701216595,26.0295240215573,39.116));
#202216=CARTESIAN_POINT('Origin',(-29.9275190026066,-52.4710850656382,39.1160402713848));
#202217=CARTESIAN_POINT('Ctrl Pts',(-30.0450834959839,-52.6757649139394,
39.2708017080178));
#202218=CARTESIAN_POINT('Ctrl Pts',(-30.1558192616004,-52.6124111049555,
39.27051194648));
#202219=CARTESIAN_POINT('Ctrl Pts',(-30.100576467536,-52.516727778884,39.3343017080178));
#202220=CARTESIAN_POINT('Ctrl Pts',(-30.0676891808491,-52.7146817640549,
39.3487519301185));
#202221=CARTESIAN_POINT('Ctrl Pts',(-30.1782028480944,-52.6511806140169,
39.3482879463976));
#202222=CARTESIAN_POINT('Ctrl Pts',(-30.1343304829276,-52.5751914485016,
39.4512271261638));
#202223=CARTESIAN_POINT('Ctrl Pts',(-30.1105150503711,-52.7884098752461,
39.3978017080178));
#202224=CARTESIAN_POINT('Ctrl Pts',(-30.220659667678,-52.7247179826673,
39.3975673827411));
#202225=CARTESIAN_POINT('Ctrl Pts',(-30.1982769148315,-52.6859499175219,
39.5248015355181));
#202226=CARTESIAN_POINT('Ctrl Pts',(-30.155571337834,-52.8659816883958,
39.3978017080178));
#202227=CARTESIAN_POINT('Ctrl Pts',(-30.2655565641147,-52.8024816883958,
39.3978017080178));
#202228=CARTESIAN_POINT('Ctrl Pts',(-30.2655565641147,-52.8024816883958,
39.5248017080178));
#202229=CARTESIAN_POINT('Origin',(-29.9905912412554,-52.580227778884,39.3343017080178));
#202230=CARTESIAN_POINT('Origin',(-29.9499161075309,-52.5097763812719,39.1934008533551));
#202231=CARTESIAN_POINT('Origin',(-36.3610285397812,-49.5064990290886,39.1925554495082));
#202232=CARTESIAN_POINT('Origin',(-36.3870656659254,-49.5422481179707,39.1160373285265));
#202233=CARTESIAN_POINT('Origin',(-36.3129251734945,-49.4402904249164,39.3343017080178));
#202234=CARTESIAN_POINT('Ctrl Pts',(-36.2478178023253,-49.3516463037383,
39.2708017080178));
#202235=CARTESIAN_POINT('Ctrl Pts',(-36.1458216659127,-49.4263574835549,
39.2710850691866));
#202236=CARTESIAN_POINT('Ctrl Pts',(-36.2101800152089,-49.5149391519575,
39.3343017080178));
#202237=CARTESIAN_POINT('Ctrl Pts',(-36.2214577843979,-49.3151677697927,
39.3487519293518));
#202238=CARTESIAN_POINT('Ctrl Pts',(-36.1192316557451,-49.3897594742963,
39.349206866295));
#202239=CARTESIAN_POINT('Ctrl Pts',(-36.1704998050836,-49.4603240281405,
39.4512271248759));
#202240=CARTESIAN_POINT('Ctrl Pts',(-36.1715192752727,-49.2460589922049,
39.3978017080178));
#202241=CARTESIAN_POINT('Ctrl Pts',(-36.0689133127003,-49.3205022166628,
39.3980347781164));
#202242=CARTESIAN_POINT('Ctrl Pts',(-36.0953262843463,-49.3568565532996,
39.5248015355176));
#202243=CARTESIAN_POINT('Ctrl Pts',(-36.1189794796885,-49.1733470784086,
39.3978017080178));
#202244=CARTESIAN_POINT('Ctrl Pts',(-36.0162343214029,-49.2479958054497,
39.3978017080178));
#202245=CARTESIAN_POINT('Ctrl Pts',(-36.0162343214029,-49.2479958054497,
39.5248017080178));
#202246=CARTESIAN_POINT('Origin',(-36.1189794796885,-49.1733470784086,39.5248017080178));
#202247=CARTESIAN_POINT('Origin',(-0.256862895714039,0.186621817602861,
39.116));
#202248=CARTESIAN_POINT('Origin',(-36.6229335645812,-49.8669803696024,39.116));
#202249=CARTESIAN_POINT('Origin',(-0.256862895714039,0.186621817602861,
39.5248017080178));
#202250=CARTESIAN_POINT('Origin',(-36.0301015792679,-49.0510171431402,39.5248017080178));
#202251=CARTESIAN_POINT('Ctrl Pts',(-36.9399086546489,-50.3023253561993,
39.2875012672119));
#202252=CARTESIAN_POINT('Ctrl Pts',(-36.8368401467438,-50.3777877177486,
39.287208709576));
#202253=CARTESIAN_POINT('Ctrl Pts',(-36.7733199672422,-50.2900345588336,
39.3549016990124));
#202254=CARTESIAN_POINT('Ctrl Pts',(-36.8722300970233,-50.2093718139452,
39.1034939173931));
#202255=CARTESIAN_POINT('Ctrl Pts',(-36.7691625978848,-50.2846371204143,
39.103169233635));
#202256=CARTESIAN_POINT('Ctrl Pts',(-36.7192723137706,-50.2156443459718,
39.2077507202315));
#202257=CARTESIAN_POINT('Ctrl Pts',(-36.7506474475454,-50.0423845927726,
38.989));
#202258=CARTESIAN_POINT('Ctrl Pts',(-36.6476776482595,-50.1174266236766,
38.9887769311152));
#202259=CARTESIAN_POINT('Ctrl Pts',(-36.622177901771,-50.0820053531142,
39.1161898712895));
#202260=CARTESIAN_POINT('Ctrl Pts',(-36.6229335645812,-49.8669803696024,
38.989));
#202261=CARTESIAN_POINT('Ctrl Pts',(-36.5200349097933,-49.9417406183803,
38.989));
#202262=CARTESIAN_POINT('Ctrl Pts',(-36.5201885207827,-49.9416290134637,
39.1161895903858));
#202263=CARTESIAN_POINT('Origin',(-36.8761597191957,-50.2155162706042,39.3548010137695));
#202264=CARTESIAN_POINT('Ctrl Pts',(-36.0301015792679,-49.0510171431402,
39.3978017080178));
#202265=CARTESIAN_POINT('Ctrl Pts',(-35.9273564209823,-49.1256658701813,
39.3978017080178));
#202266=CARTESIAN_POINT('Ctrl Pts',(-35.9273564209823,-49.1256658701813,
39.5248017080178));
#202267=CARTESIAN_POINT('Ctrl Pts',(-35.9773846774553,-48.9780591316064,
39.3978017080178));
#202268=CARTESIAN_POINT('Ctrl Pts',(-35.8743986902985,-49.0527758071202,
39.3975666025021));
#202269=CARTESIAN_POINT('Ctrl Pts',(-35.8479971380609,-49.0164371879468,
39.5248015517178));
#202270=CARTESIAN_POINT('Ctrl Pts',(-35.9275383438679,-48.9090707128231,
39.3484894016716));
#202271=CARTESIAN_POINT('Ctrl Pts',(-35.8245773199107,-48.984202573666,
39.3480259000044));
#202272=CARTESIAN_POINT('Ctrl Pts',(-35.7729572780254,-48.9131536812792,
39.4508333188948));
#202273=CARTESIAN_POINT('Ctrl Pts',(-35.9012693628907,-48.8727133447942,
39.2708017080178));
#202274=CARTESIAN_POINT('Ctrl Pts',(-35.7983524848938,-48.9481071848795,
39.27051194648));
#202275=CARTESIAN_POINT('Ctrl Pts',(-35.7334106856009,-48.8587224664499,
39.3343017080178));
#202276=CARTESIAN_POINT('Origin',(-35.8361558438865,-48.7840737394087,39.3343017080178));
#202277=CARTESIAN_POINT('Origin',(-36.980873139623,-50.3596419293452,39.6398955068198));
#202278=CARTESIAN_POINT('Origin',(-37.0855865599605,-50.5037675878943,39.92499));
#202279=CARTESIAN_POINT('Origin',(-35.7883393560614,-48.7182599900754,39.1934008539946));
#202280=CARTESIAN_POINT('Origin',(-35.7621028045852,-48.6820620414863,39.1160402713845));
#202281=CARTESIAN_POINT('Ctrl Pts',(-37.0158684358562,-50.9219998155898,
40.1599502534424));
#202282=CARTESIAN_POINT('Ctrl Pts',(-36.9939338721435,-50.8918248690998,
40.10025));
#202283=CARTESIAN_POINT('Ctrl Pts',(-36.9525415975215,-50.8348823336484,
40.10025));
#202284=CARTESIAN_POINT('Ctrl Pts',(-37.0871426490248,-50.870189502586,
40.1599500538471));
#202285=CARTESIAN_POINT('Ctrl Pts',(-37.0458491715921,-50.8540829678249,
40.100244835349));
#202286=CARTESIAN_POINT('Ctrl Pts',(-36.9937925764114,-50.8048852215559,
40.10025));
#202287=CARTESIAN_POINT('Ctrl Pts',(-37.1382015956602,-50.8021467555732,
40.1202442001038));
#202288=CARTESIAN_POINT('Ctrl Pts',(-37.0800635522215,-50.8006171556814,
40.0633873868017));
#202289=CARTESIAN_POINT('Ctrl Pts',(-37.0171501059293,-50.7569692080812,
40.0772271723537));
#202290=CARTESIAN_POINT('Ctrl Pts',(-37.1817767082789,-50.6806663304942,
40.0045995998163));
#202291=CARTESIAN_POINT('Ctrl Pts',(-37.0956112176475,-50.7142182018864,
39.9663485808314));
#202292=CARTESIAN_POINT('Ctrl Pts',(-37.0243843935851,-50.6618927960199,
40.0101727202466));
#202293=CARTESIAN_POINT('Ctrl Pts',(-37.1760624637761,-50.6273693057704,
39.9304654349858));
#202294=CARTESIAN_POINT('Ctrl Pts',(-37.0763301845679,-50.6810088489693,
39.9051900162958));
#202295=CARTESIAN_POINT('Ctrl Pts',(-37.0095702365079,-50.6152053999548,
39.9671857458184));
#202296=CARTESIAN_POINT('Ctrl Pts',(-37.1493329797263,-50.5905785208482,
39.8576902534424));
#202297=CARTESIAN_POINT('Ctrl Pts',(-37.0464195108255,-50.6659240749081,
39.8573998014387));
#202298=CARTESIAN_POINT('Ctrl Pts',(-36.9828414016749,-50.5784163149355,
39.92499));
#202299=CARTESIAN_POINT('Origin',(-36.9525415975215,-50.8348823336484,40.22725));
#202300=CARTESIAN_POINT('Origin',(-0.256862895714039,0.186621817602861,
39.116));
#202301=CARTESIAN_POINT('Origin',(-35.5261472678868,-48.3573835402117,39.116));
#202302=CARTESIAN_POINT('Origin',(6.67120042669033E-17,1.33398482780241E-16,
40.22725));
#202303=CARTESIAN_POINT('Origin',(-36.9278827595329,-50.8527980281383,40.22725));
#202304=CARTESIAN_POINT('Ctrl Pts',(-35.5261472678868,-48.3573835402117,
38.989));
#202305=CARTESIAN_POINT('Ctrl Pts',(-35.4232481927144,-48.432144094417,
38.989));
#202306=CARTESIAN_POINT('Ctrl Pts',(-35.4234022247158,-48.4320321836172,
39.1161901092323));
#202307=CARTESIAN_POINT('Ctrl Pts',(-35.3984257650695,-48.1819806163539,
38.989));
#202308=CARTESIAN_POINT('Ctrl Pts',(-35.2958250128989,-48.2567602586425,
38.9892298989718));
#202309=CARTESIAN_POINT('Ctrl Pts',(-35.3214110399822,-48.2916533613397,
39.1161900493185));
#202310=CARTESIAN_POINT('Ctrl Pts',(-35.276834980876,-48.0150011530606,
39.1034966344368));
#202311=CARTESIAN_POINT('Ctrl Pts',(-35.1744900671661,-48.0897561847353,
39.1038314102599));
#202312=CARTESIAN_POINT('Ctrl Pts',(-35.2243173504718,-48.1580153629267,
39.2077528789615));
#202313=CARTESIAN_POINT('Ctrl Pts',(-35.209151665053,-47.9220530736685,
39.2875012672119));
#202314=CARTESIAN_POINT('Ctrl Pts',(-35.1070032653413,-47.9968681042462,
39.2878045257868));
#202315=CARTESIAN_POINT('Ctrl Pts',(-35.1702703594596,-48.0836260618767,
39.35490152959));
#202316=CARTESIAN_POINT('Origin',(-35.2729208539817,-48.008847282327,39.3548010137695));
#202317=CARTESIAN_POINT('Ctrl Pts',(-36.6347241449657,-50.9644637245891,
39.8576902534424));
#202318=CARTESIAN_POINT('Ctrl Pts',(-36.7381840359687,-50.8898702560316,
39.8573998014387));
#202319=CARTESIAN_POINT('Ctrl Pts',(-36.674605926818,-50.8023624960589,
39.92499));
#202320=CARTESIAN_POINT('Ctrl Pts',(-36.6614665482806,-51.0012706547885,
39.9304984902489));
#202321=CARTESIAN_POINT('Ctrl Pts',(-36.7432905102115,-50.9229972443173,
39.9052171569796));
#202322=CARTESIAN_POINT('Ctrl Pts',(-36.701346940908,-50.8391683443875,
39.96720497266));
#202323=CARTESIAN_POINT('Ctrl Pts',(-36.710288459717,-51.0230245369437,
40.0043437678665));
#202324=CARTESIAN_POINT('Ctrl Pts',(-36.768904996455,-50.9514409225352,
39.9661628577646));
#202325=CARTESIAN_POINT('Ctrl Pts',(-36.7410683485321,-50.867535894943,
40.0100243556238));
#202326=CARTESIAN_POINT('Ctrl Pts',(-36.8383381382862,-51.0194219249359,
40.1194874821985));
#202327=CARTESIAN_POINT('Ctrl Pts',(-36.8551762168621,-50.9635175930191,
40.0627551483138));
#202328=CARTESIAN_POINT('Ctrl Pts',(-36.8330984946702,-50.8901021525735,
40.0767884282375));
#202329=CARTESIAN_POINT('Ctrl Pts',(-36.9196318328647,-50.9918932610485,
40.1599502015387));
#202330=CARTESIAN_POINT('Ctrl Pts',(-36.9171104726346,-50.9476171190686,
40.1002449453872));
#202331=CARTESIAN_POINT('Ctrl Pts',(-36.8864699989248,-50.8828596657519,
40.10025));
#202332=CARTESIAN_POINT('Ctrl Pts',(-36.991167339171,-50.93994621282,40.1599502534424));
#202333=CARTESIAN_POINT('Ctrl Pts',(-36.9692474126343,-50.9097606317992,
40.10025));
#202334=CARTESIAN_POINT('Ctrl Pts',(-36.9278827595329,-50.8527980281383,
40.10025));
#202335=CARTESIAN_POINT('Origin',(-36.5718607685324,-50.8770112231001,39.92499));
#202336=CARTESIAN_POINT('Origin',(-35.1682072895736,-47.864721425495,39.6398955069317));
#202337=CARTESIAN_POINT('Origin',(-35.0634937251224,-47.7205955685089,39.92499));
#202338=CARTESIAN_POINT('Origin',(-36.467147348224,-50.7328855645163,39.6398955068266));
#202339=CARTESIAN_POINT('Origin',(-36.3624339277676,-50.5887599058099,39.3548010137695));
#202340=CARTESIAN_POINT('Ctrl Pts',(-34.9997217530263,-47.6338034047598,
39.8576902534424));
#202341=CARTESIAN_POINT('Ctrl Pts',(-34.8977303031704,-47.7085070967802,
39.8579948730703));
#202342=CARTESIAN_POINT('Ctrl Pts',(-34.9607485668368,-47.79524429555,39.92499));
#202343=CARTESIAN_POINT('Ctrl Pts',(-34.9730146904946,-47.5970451916066,
39.9304020711231));
#202344=CARTESIAN_POINT('Ctrl Pts',(-34.8923835282626,-47.6752966590742,
39.9058915297382));
#202345=CARTESIAN_POINT('Ctrl Pts',(-34.9340408279395,-47.7584842465951,
39.9671523786036));
#202346=CARTESIAN_POINT('Ctrl Pts',(-34.9244461536127,-47.5754322771534,
40.0043257306692));
#202347=CARTESIAN_POINT('Ctrl Pts',(-34.8665972787028,-47.6469756149919,
39.9667894847835));
#202348=CARTESIAN_POINT('Ctrl Pts',(-34.8944891948624,-47.7303228514091,
40.0100138975201));
#202349=CARTESIAN_POINT('Ctrl Pts',(-34.7970725085258,-47.5794993790984,
40.1195533054858));
#202350=CARTESIAN_POINT('Ctrl Pts',(-34.7804938560721,-47.6353197637777,
40.0630813209237));
#202351=CARTESIAN_POINT('Ctrl Pts',(-34.8028668197836,-47.7084160893873,
40.076826594242));
#202352=CARTESIAN_POINT('Ctrl Pts',(-34.7162617467342,-47.6073089936882,
40.1599502027523));
#202353=CARTESIAN_POINT('Ctrl Pts',(-34.7189078610131,-47.6515013114252,
40.100255279155));
#202354=CARTESIAN_POINT('Ctrl Pts',(-34.7497660430524,-47.7160937685325,
40.10025));
#202355=CARTESIAN_POINT('Ctrl Pts',(-34.6451144164188,-47.6590285860934,
40.1599502534424));
#202356=CARTESIAN_POINT('Ctrl Pts',(-34.667049453402,-47.6892031885512,
40.10025));
#202357=CARTESIAN_POINT('Ctrl Pts',(-34.7084426211234,-47.7461450747863,
40.10025));
#202358=CARTESIAN_POINT('Origin',(-34.7084426211234,-47.7461450747863,40.22725));
#202359=CARTESIAN_POINT('Ctrl Pts',(-36.1092077731531,-50.2402240048081,
38.989));
#202360=CARTESIAN_POINT('Ctrl Pts',(-36.2121064368057,-50.1654637495896,
38.989));
#202361=CARTESIAN_POINT('Ctrl Pts',(-36.2119528169383,-50.1655753609564,
39.1161896013268));
#202362=CARTESIAN_POINT('Ctrl Pts',(-36.2365633238574,-50.4158927445015,
38.989));
#202363=CARTESIAN_POINT('Ctrl Pts',(-36.3397519704563,-50.3411519064829,
38.9887769275436));
#202364=CARTESIAN_POINT('Ctrl Pts',(-36.313943782211,-50.3059538820309,
39.1161898821826));
#202365=CARTESIAN_POINT('Ctrl Pts',(-36.3578055460618,-50.583125283657,
39.1034967087243));
#202366=CARTESIAN_POINT('Ctrl Pts',(-36.4612367259587,-50.5083605190624,
39.1031720232736));
#202367=CARTESIAN_POINT('Ctrl Pts',(-36.4110374247136,-50.4395918165618,
39.2077529615021));
#202368=CARTESIAN_POINT('Ctrl Pts',(-36.4252947698681,-50.6762142289946,
39.2875012672119));
#202369=CARTESIAN_POINT('Ctrl Pts',(-36.5289136700283,-50.6015093986314,
39.2872087095507));
#202370=CARTESIAN_POINT('Ctrl Pts',(-36.4650842569434,-50.513980899522,
39.3549017048229));
#202371=CARTESIAN_POINT('Origin',(-36.1092077731531,-50.2402240048081,39.116));
#202372=CARTESIAN_POINT('Origin',(3.77491158612227E-16,-4.74547095659465E-17,
40.22725));
#202373=CARTESIAN_POINT('Origin',(-34.6837837831348,-47.7640607692761,40.22725));
#202374=CARTESIAN_POINT('Origin',(21.7541926348216,29.4019141737117,39.116));
#202375=CARTESIAN_POINT('Origin',(-35.8732562382988,-49.9155525184322,39.1160373285271));
#202376=CARTESIAN_POINT('Ctrl Pts',(-34.6205005703637,-47.6769115920302,
40.1599502534424));
#202377=CARTESIAN_POINT('Ctrl Pts',(-34.6424200234577,-47.7070975168462,
40.10025));
#202378=CARTESIAN_POINT('Ctrl Pts',(-34.6837837831348,-47.7640607692761,
40.10025));
#202379=CARTESIAN_POINT('Ctrl Pts',(-34.5495693076632,-47.72841834836,40.1599500566044));
#202380=CARTESIAN_POINT('Ctrl Pts',(-34.5907418558587,-47.7446195594503,
40.1002551305372));
#202381=CARTESIAN_POINT('Ctrl Pts',(-34.6425747206407,-47.7939730310144,
40.10025));
#202382=CARTESIAN_POINT('Ctrl Pts',(-34.4983910654766,-47.7959261043554,
40.1203070619047));
#202383=CARTESIAN_POINT('Ctrl Pts',(-34.5563698228278,-47.7976714756522,
40.0637098684499));
#202384=CARTESIAN_POINT('Ctrl Pts',(-34.6188891978597,-47.8415056181563,
40.0772636213362));
#202385=CARTESIAN_POINT('Ctrl Pts',(-34.4545839152296,-47.9165880269726,
40.0046102245801));
#202386=CARTESIAN_POINT('Ctrl Pts',(-34.5404685123898,-47.8837591046485,
39.9670001894012));
#202387=CARTESIAN_POINT('Ctrl Pts',(-34.6111463389772,-47.9359643384887,
40.010178881121));
#202388=CARTESIAN_POINT('Ctrl Pts',(-34.460235468251,-47.9696250311907,
39.9303710930187));
#202389=CARTESIAN_POINT('Ctrl Pts',(-34.559577790676,-47.9171136764605,
39.9058663574101));
#202390=CARTESIAN_POINT('Ctrl Pts',(-34.6258166968299,-47.9824460410472,
39.9671344706361));
#202391=CARTESIAN_POINT('Ctrl Pts',(-34.4869303039399,-48.0063682005185,
39.8576902534424));
#202392=CARTESIAN_POINT('Ctrl Pts',(-34.5894948283136,-47.9324532779036,
39.8579948730704));
#202393=CARTESIAN_POINT('Ctrl Pts',(-34.6525130919799,-48.0191904766735,
39.92499));
#202394=CARTESIAN_POINT('Origin',(-34.5497679336943,-48.0938392037146,39.92499));
#202395=CARTESIAN_POINT('Origin',(-35.8473027479613,-49.8797426632443,39.1925554488848));
#202396=CARTESIAN_POINT('Origin',(-35.7991993820664,-49.8135340601221,39.3343017080178));
#202397=CARTESIAN_POINT('Origin',(-34.6544814981818,-48.237965060654,39.6398955069213));
#202398=CARTESIAN_POINT('Origin',(-34.7591950625536,-48.3820909175328,39.3548010137695));
#202399=CARTESIAN_POINT('Ctrl Pts',(-35.6052536882604,-49.5465907136143,
39.3978017080178));
#202400=CARTESIAN_POINT('Ctrl Pts',(-35.707998846546,-49.4719419865731,
39.3978017080178));
#202401=CARTESIAN_POINT('Ctrl Pts',(-35.707998846546,-49.4719419865731,
39.5248017080178));
#202402=CARTESIAN_POINT('Ctrl Pts',(-35.6583499840584,-49.6192730640951,
39.3978017080178));
#202403=CARTESIAN_POINT('Ctrl Pts',(-35.760855993121,-49.5446936074878,
39.3980355775182));
#202404=CARTESIAN_POINT('Ctrl Pts',(-35.7873581223566,-49.5811706590204,
39.5248015517173));
#202405=CARTESIAN_POINT('Ctrl Pts',(-35.7085550527717,-49.6880007749195,
39.3484893995498));
#202406=CARTESIAN_POINT('Ctrl Pts',(-35.8110857017893,-49.6138288703715,
39.3489438303428));
#202407=CARTESIAN_POINT('Ctrl Pts',(-35.862397963352,-49.6844541394816,
39.4508333155612));
#202408=CARTESIAN_POINT('Ctrl Pts',(-35.7350130971391,-49.7242207306173,
39.2708017080178));
#202409=CARTESIAN_POINT('Ctrl Pts',(-35.8375861910559,-49.6503036646783,
39.2710850691866));
#202410=CARTESIAN_POINT('Ctrl Pts',(-35.9019445403521,-49.738885333081,
39.3343017080178));
#202411=CARTESIAN_POINT('Origin',(-35.6052536882604,-49.5465907136143,39.5248017080178));
#202412=CARTESIAN_POINT('Ctrl Pts',(-34.6963546279287,-48.2946219293745,
39.2875012672119));
#202413=CARTESIAN_POINT('Ctrl Pts',(-34.7990735298985,-48.2205921526137,
39.2878045257519));
#202414=CARTESIAN_POINT('Ctrl Pts',(-34.8620346481358,-48.3075723994624,
39.3549015218345));
#202415=CARTESIAN_POINT('Ctrl Pts',(-34.7638392294011,-48.3877165307503,
39.1034938540228));
#202416=CARTESIAN_POINT('Ctrl Pts',(-34.866561796066,-48.3134813154549,
39.1038286278822));
#202417=CARTESIAN_POINT('Ctrl Pts',(-34.9160824571397,-48.3819628268515,
39.2077506434037));
#202418=CARTESIAN_POINT('Ctrl Pts',(-34.8850734745837,-48.5549570506159,
38.989));
#202419=CARTESIAN_POINT('Ctrl Pts',(-34.9878985031412,-48.4804861171421,
38.9892298954611));
#202420=CARTESIAN_POINT('Ctrl Pts',(-35.0131769156726,-48.5156018845749,
39.1161900347285));
#202421=CARTESIAN_POINT('Ctrl Pts',(-35.0124214764587,-48.7306271754175,
38.989));
#202422=CARTESIAN_POINT('Ctrl Pts',(-35.1153205397465,-48.6558666298469,
38.989));
#202423=CARTESIAN_POINT('Ctrl Pts',(-35.1151665196475,-48.6559785319991,
39.1161900945641));
#202424=CARTESIAN_POINT('Origin',(-35.0124214764587,-48.7306271754175,39.116));
#202425=CARTESIAN_POINT('Origin',(21.2334658618526,28.6851952578919,39.5248017080178));
#202426=CARTESIAN_POINT('Origin',(-35.5163757878398,-49.4242607783459,39.5248017080178));
#202427=CARTESIAN_POINT('Origin',(21.1519223437074,28.5729602337852,39.116));
#202428=CARTESIAN_POINT('Origin',(-35.2482948100398,-49.0553654007524,39.1160402713849));
#202429=CARTESIAN_POINT('Ctrl Pts',(-35.3866101428262,-49.2466351556011,
39.2708017080178));
#202430=CARTESIAN_POINT('Ctrl Pts',(-35.4901170100369,-49.1720533660029,
39.27051194648));
#202431=CARTESIAN_POINT('Ctrl Pts',(-35.425175210744,-49.0826686475733,
39.3343017080178));
#202432=CARTESIAN_POINT('Ctrl Pts',(-35.4131599099205,-49.2829758776409,
39.3487519301186));
#202433=CARTESIAN_POINT('Ctrl Pts',(-35.5164304941039,-49.2082707697416,
39.3482879463972));
#202434=CARTESIAN_POINT('Ctrl Pts',(-35.4648554356498,-49.1372837917339,
39.4512271261637));
#202435=CARTESIAN_POINT('Ctrl Pts',(-35.4634578610141,-49.351823576193,
39.3978017080178));
#202436=CARTESIAN_POINT('Ctrl Pts',(-35.5663414789288,-49.2769673468807,
39.3975673827411));
#202437=CARTESIAN_POINT('Ctrl Pts',(-35.5400289748692,-49.2407512920132,
39.5248015355181));
#202438=CARTESIAN_POINT('Ctrl Pts',(-35.5163757878398,-49.4242607783459,
39.3978017080178));
#202439=CARTESIAN_POINT('Ctrl Pts',(-35.6191209461254,-49.3496120513047,
39.3978017080178));
#202440=CARTESIAN_POINT('Ctrl Pts',(-35.6191209461254,-49.3496120513047,
39.5248017080178));
#202441=CARTESIAN_POINT('Origin',(-35.3224300524584,-49.1573173746145,39.3343017080178));
#202442=CARTESIAN_POINT('Origin',(-35.2746135650462,-49.091503626351,39.1934008533548));
#202443=CARTESIAN_POINT('Origin',(-41.3366772861974,-45.4345348113607,39.1925554495084));
#202444=CARTESIAN_POINT('Origin',(-41.3663085755628,-45.4673664422104,39.1160373285261));
#202445=CARTESIAN_POINT('Origin',(-41.2819167515331,-45.3737170758071,39.3343017080178));
#202446=CARTESIAN_POINT('Ctrl Pts',(-41.2079002115909,-45.2923641298555,
39.2708017080178));
#202447=CARTESIAN_POINT('Ctrl Pts',(-41.1142722655008,-45.3773275334104,
39.2710850691866));
#202448=CARTESIAN_POINT('Ctrl Pts',(-41.1875373586974,-45.4586966628146,
39.3343017080178));
#202449=CARTESIAN_POINT('Ctrl Pts',(-41.1778715515046,-45.2588408013009,
39.3487519293518));
#202450=CARTESIAN_POINT('Ctrl Pts',(-41.0840023845238,-45.3437094247749,
39.3492068662931));
#202451=CARTESIAN_POINT('Ctrl Pts',(-41.1423656859494,-45.4085284377449,
39.4512271248737));
#202452=CARTESIAN_POINT('Ctrl Pts',(-41.1209827764384,-45.1953306044442,
39.3978017080178));
#202453=CARTESIAN_POINT('Ctrl Pts',(-41.0267203359206,-45.2800912647189,
39.3980347781183));
#202454=CARTESIAN_POINT('Ctrl Pts',(-41.0567886774842,-45.3134855411618,
39.5248015355195));
#202455=CARTESIAN_POINT('Ctrl Pts',(-41.0611303347406,-45.1285089182131,
39.3978017080178));
#202456=CARTESIAN_POINT('Ctrl Pts',(-40.966750941905,-45.2134885052206,
39.3978017080178));
#202457=CARTESIAN_POINT('Ctrl Pts',(-40.966750941905,-45.2134885052206,
39.5248017080178));
#202458=CARTESIAN_POINT('Origin',(-41.0611303347406,-45.1285089182131,39.5248017080178));
#202459=CARTESIAN_POINT('Origin',(-0.235948482089066,0.212448967518939,
39.116));
#202460=CARTESIAN_POINT('Origin',(-41.6348281284264,-45.7656648676104,39.116));
#202461=CARTESIAN_POINT('Origin',(-0.235948482089066,0.212448967518939,
39.5248017080178));
#202462=CARTESIAN_POINT('Origin',(-40.9599523566127,-45.0161393894791,39.5248017080178));
#202463=CARTESIAN_POINT('Ctrl Pts',(-41.9955727382253,-46.165492069761,
39.2875012672119));
#202464=CARTESIAN_POINT('Ctrl Pts',(-41.900956815078,-46.2513146333406,
39.287208709576));
#202465=CARTESIAN_POINT('Ctrl Pts',(-41.8286119029177,-46.1706818621615,
39.3549016990125));
#202466=CARTESIAN_POINT('Ctrl Pts',(-41.9185486398931,-46.0801220723616,
39.1034939173931));
#202467=CARTESIAN_POINT('Ctrl Pts',(-41.8239131221214,-46.1657485549032,
39.1031692336336));
#202468=CARTESIAN_POINT('Ctrl Pts',(-41.7670844335159,-46.1023486848317,
39.2077507202291));
#202469=CARTESIAN_POINT('Ctrl Pts',(-41.7801771152787,-45.926758472166,
38.989));
#202470=CARTESIAN_POINT('Ctrl Pts',(-41.6856154234971,-46.0121526898573,
38.9887769311176));
#202471=CARTESIAN_POINT('Ctrl Pts',(-41.6565528363056,-45.9795909100351,
39.116189871292));
#202472=CARTESIAN_POINT('Ctrl Pts',(-41.6348281284264,-45.7656648676104,
38.989));
#202473=CARTESIAN_POINT('Ctrl Pts',(-41.5403077371541,-45.8507714101806,
38.989));
#202474=CARTESIAN_POINT('Ctrl Pts',(-41.5404488407561,-45.8506443599267,
39.1161895903859));
#202475=CARTESIAN_POINT('Origin',(-41.9230990057958,-46.0858221116776,39.3548010137695));
#202476=CARTESIAN_POINT('Ctrl Pts',(-40.9599523566127,-45.0161393894791,
39.3978017080178));
#202477=CARTESIAN_POINT('Ctrl Pts',(-40.8655729637771,-45.1011189764867,
39.3978017080178));
#202478=CARTESIAN_POINT('Ctrl Pts',(-40.8655729637771,-45.1011189764867,
39.5248017080178));
#202479=CARTESIAN_POINT('Ctrl Pts',(-40.8998980546769,-44.9490914662996,
39.3978017080178));
#202480=CARTESIAN_POINT('Ctrl Pts',(-40.8052862548041,-45.0341638030234,
39.3975666025026));
#202481=CARTESIAN_POINT('Ctrl Pts',(-40.7752309130114,-45.000783964291,
39.5248015517178));
#202482=CARTESIAN_POINT('Ctrl Pts',(-40.8431135311195,-44.8856913339442,
39.3484894016717));
#202483=CARTESIAN_POINT('Ctrl Pts',(-40.7485699563835,-44.9711739722012,
39.3480259000039));
#202484=CARTESIAN_POINT('Ctrl Pts',(-40.68980606295,-44.9059100567353,39.4508333188944));
#202485=CARTESIAN_POINT('Ctrl Pts',(-40.8131880745608,-44.8522789915939,
39.2708017080178));
#202486=CARTESIAN_POINT('Ctrl Pts',(-40.7187157882339,-44.938017559436,
39.27051194648));
#202487=CARTESIAN_POINT('Ctrl Pts',(-40.6447864996555,-44.8559107663283,
39.3343017080178));
#202488=CARTESIAN_POINT('Origin',(-40.7391658924911,-44.7709311793208,39.3343017080178));
#202489=CARTESIAN_POINT('Origin',(-42.0423040287729,-46.2182127020652,39.639895506818));
#202490=CARTESIAN_POINT('Origin',(-42.1615090516454,-46.3506032922592,39.92499));
#202491=CARTESIAN_POINT('Origin',(-40.6847319383099,-44.7104761485843,39.1934008539943));
#202492=CARTESIAN_POINT('Origin',(-40.6548553974683,-44.6772189625516,39.1160402713845));
#202493=CARTESIAN_POINT('Ctrl Pts',(-42.1358900227697,-46.7738319284255,
40.1599502534424));
#202494=CARTESIAN_POINT('Ctrl Pts',(-42.1109214781063,-46.746115069687,
40.10025));
#202495=CARTESIAN_POINT('Ctrl Pts',(-42.0638038389703,-46.6938111422602,
40.10025));
#202496=CARTESIAN_POINT('Ctrl Pts',(-42.2013581359409,-46.7148552537637,
40.1599500538459));
#202497=CARTESIAN_POINT('Ctrl Pts',(-42.1586072771693,-46.7031532960222,
40.1002448353478));
#202498=CARTESIAN_POINT('Ctrl Pts',(-42.1016932886507,-46.659666456053,
40.10025));
#202499=CARTESIAN_POINT('Ctrl Pts',(-42.2450249725429,-46.6418481388113,
40.1202442001041));
#202500=CARTESIAN_POINT('Ctrl Pts',(-42.1870455286633,-46.6464039985661,
40.0633873868017));
#202501=CARTESIAN_POINT('Ctrl Pts',(-42.1199142759252,-46.6095714048494,
40.0772271723538));
#202502=CARTESIAN_POINT('Ctrl Pts',(-42.2756632139847,-46.5164783566525,
40.004599599816));
#202503=CARTESIAN_POINT('Ctrl Pts',(-42.1934768724829,-46.5588531737045,
39.9663485808314));
#202504=CARTESIAN_POINT('Ctrl Pts',(-42.1171707421501,-46.5142596423493,
40.0101727202466));
#202505=CARTESIAN_POINT('Ctrl Pts',(-42.2644092166189,-46.4640705998047,
39.9304654349861));
#202506=CARTESIAN_POINT('Ctrl Pts',(-42.1708301402941,-46.527841161857,
39.9051900162953));
#202507=CARTESIAN_POINT('Ctrl Pts',(-42.0975575768116,-46.4693765057998,
39.9671857458178));
#202508=CARTESIAN_POINT('Ctrl Pts',(-42.2339804752703,-46.4302753505423,
39.8576902534424));
#202509=CARTESIAN_POINT('Ctrl Pts',(-42.1395065321001,-46.5159655405273,
39.8573998014387));
#202510=CARTESIAN_POINT('Ctrl Pts',(-42.0671296588098,-46.4355828792668,
39.92499));
#202511=CARTESIAN_POINT('Origin',(-42.0638038389703,-46.6938111422602,40.22725));
#202512=CARTESIAN_POINT('Origin',(-0.235948482089066,0.212448967518939,
39.116));
#202513=CARTESIAN_POINT('Origin',(-40.386254305094,-44.3789831537294,39.116));
#202514=CARTESIAN_POINT('Origin',(8.01250065760356E-17,1.22536847673099E-16,
40.22725));
#202515=CARTESIAN_POINT('Origin',(-42.0411527846897,-46.714206243142,40.22725));
#202516=CARTESIAN_POINT('Ctrl Pts',(-40.386254305094,-44.3789831537294,
38.989));
#202517=CARTESIAN_POINT('Ctrl Pts',(-40.2917335276658,-44.4640900439959,
38.989));
#202518=CARTESIAN_POINT('Ctrl Pts',(-40.2918750180001,-44.4639626455266,
39.1161901092326));
#202519=CARTESIAN_POINT('Ctrl Pts',(-40.2408978759466,-44.2178916378594,
38.989));
#202520=CARTESIAN_POINT('Ctrl Pts',(-40.1466757825259,-44.3029863283988,
38.9892298989778));
#202521=CARTESIAN_POINT('Ctrl Pts',(-40.1757689690818,-44.3350138149348,
39.1161900493206));
#202522=CARTESIAN_POINT('Ctrl Pts',(-40.1025190720984,-44.0645366033543,
39.1034966344368));
#202523=CARTESIAN_POINT('Ctrl Pts',(-40.008548843116,-44.1495800756938,
39.1038314102545));
#202524=CARTESIAN_POINT('Ctrl Pts',(-40.0652381943494,-44.2122569536128,
39.2077528789595));
#202525=CARTESIAN_POINT('Ctrl Pts',(-40.025490812659,-43.9791725362581,
39.2875012672119));
#202526=CARTESIAN_POINT('Ctrl Pts',(-39.9317222927443,-44.0642551375175,
39.2878045257868));
#202527=CARTESIAN_POINT('Ctrl Pts',(-40.003711479089,-44.1439246138549,
39.3549015295901));
#202528=CARTESIAN_POINT('Origin',(-40.0979831325501,-44.0588255818376,39.3548010137695));
#202529=CARTESIAN_POINT('Ctrl Pts',(-41.7612723673365,-46.8559036426983,
39.8576902534424));
#202530=CARTESIAN_POINT('Ctrl Pts',(-41.8563683535933,-46.77090430155,39.8573998014387));
#202531=CARTESIAN_POINT('Ctrl Pts',(-41.7839914803029,-46.6905216402895,
39.92499));
#202532=CARTESIAN_POINT('Ctrl Pts',(-41.7917156448185,-46.8897135983612,
39.9304984902492));
#202533=CARTESIAN_POINT('Ctrl Pts',(-41.8649095672158,-46.8033160448228,
39.9052171569793));
#202534=CARTESIAN_POINT('Ctrl Pts',(-41.8144332630852,-46.7243306652213,
39.96720497266));
#202535=CARTESIAN_POINT('Ctrl Pts',(-41.8425440045879,-46.9062450310967,
40.0043437678661));
#202536=CARTESIAN_POINT('Ctrl Pts',(-41.8933569085957,-46.8289264627104,
39.9661628577639));
#202537=CARTESIAN_POINT('Ctrl Pts',(-41.8569022891475,-46.7483907976685,
40.0100243556234));
#202538=CARTESIAN_POINT('Ctrl Pts',(-41.9695156381237,-46.8892773184516,
40.1194874821988));
#202539=CARTESIAN_POINT('Ctrl Pts',(-41.9804178820376,-46.8319191778366,
40.0627551483143));
#202540=CARTESIAN_POINT('Ctrl Pts',(-41.9507871007486,-46.7612136652284,
40.0767884282378));
#202541=CARTESIAN_POINT('Ctrl Pts',(-42.0474864684053,-46.8534019544983,
40.1599502015396));
#202542=CARTESIAN_POINT('Ctrl Pts',(-42.0403508033715,-46.8096319157686,
40.1002449453872));
#202543=CARTESIAN_POINT('Ctrl Pts',(-42.003109184301,-46.7484320121865,
40.10025));
#202544=CARTESIAN_POINT('Ctrl Pts',(-42.1132001506003,-46.7942619810915,
40.1599502534424));
#202545=CARTESIAN_POINT('Ctrl Pts',(-42.0882450513177,-46.7665330160777,
40.10025));
#202546=CARTESIAN_POINT('Ctrl Pts',(-42.0411527846897,-46.7142062431421,
40.10025));
#202547=CARTESIAN_POINT('Origin',(-41.6896120874673,-46.7755012272971,39.92499));
#202548=CARTESIAN_POINT('Origin',(-39.9787779456718,-43.9264348095002,39.6398955069313));
#202549=CARTESIAN_POINT('Origin',(-39.8595727587357,-43.7940440370142,39.92499));
#202550=CARTESIAN_POINT('Origin',(-41.5704070646213,-46.6431106370585,39.6398955068276));
#202551=CARTESIAN_POINT('Origin',(-41.4512020416176,-46.5107200467155,39.3548010137695));
#202552=CARTESIAN_POINT('Ctrl Pts',(-39.7870778846749,-43.7143933160621,
39.8576902534424));
#202553=CARTESIAN_POINT('Ctrl Pts',(-39.6934538167802,-43.7993487829611,
39.8579948730704));
#202554=CARTESIAN_POINT('Ctrl Pts',(-39.7651933659001,-43.8790236240218,
39.92499));
#202555=CARTESIAN_POINT('Ctrl Pts',(-39.7566748466928,-43.6806281164515,
39.9304020711232));
#202556=CARTESIAN_POINT('Ctrl Pts',(-39.6846648960483,-43.7668791656733,
39.9058915297392));
#202557=CARTESIAN_POINT('Ctrl Pts',(-39.734789463364,-43.8452566693656,
39.9671523786036));
#202558=CARTESIAN_POINT('Ctrl Pts',(-39.7061132086033,-43.6642103943285,
40.0043257306692));
#202559=CARTESIAN_POINT('Ctrl Pts',(-39.6560595510438,-43.7414086642729,
39.9667894847835));
#202560=CARTESIAN_POINT('Ctrl Pts',(-39.692510830909,-43.8213838166742,
40.01001389752));
#202561=CARTESIAN_POINT('Ctrl Pts',(-39.5798624575878,-43.6815693876451,
40.1195533054859));
#202562=CARTESIAN_POINT('Ctrl Pts',(-39.5692094437568,-43.7388169234804,
40.0630813209237));
#202563=CARTESIAN_POINT('Ctrl Pts',(-39.5991004926183,-43.8091742082551,
40.0768265942421));
#202564=CARTESIAN_POINT('Ctrl Pts',(-39.5024012818821,-43.7176736830026,
40.1599502027513));
#202565=CARTESIAN_POINT('Ctrl Pts',(-39.5096522555305,-43.7613473163394,
40.1002552791529));
#202566=CARTESIAN_POINT('Ctrl Pts',(-39.5470931435017,-43.8223603708618,
40.10025));
#202567=CARTESIAN_POINT('Ctrl Pts',(-39.437049873601,-43.776546871172,40.1599502534424));
#202568=CARTESIAN_POINT('Ctrl Pts',(-39.4620188529811,-43.8042633382927,
40.10025));
#202569=CARTESIAN_POINT('Ctrl Pts',(-39.5091373124624,-43.8565665267054,
40.10025));
#202570=CARTESIAN_POINT('Origin',(-39.5091373124624,-43.8565665267054,40.22725));
#202571=CARTESIAN_POINT('Ctrl Pts',(-41.1629311642483,-46.1905628026483,
38.989));
#202572=CARTESIAN_POINT('Ctrl Pts',(-41.2574515636636,-46.1054562527462,
38.989));
#202573=CARTESIAN_POINT('Ctrl Pts',(-41.2573104519064,-46.1055833103429,
39.116189601327));
#202574=CARTESIAN_POINT('Ctrl Pts',(-41.3079514313262,-46.3519569306001,
38.989));
#202575=CARTESIAN_POINT('Ctrl Pts',(-41.4027622547797,-46.2668393800548,
38.9887769275436));
#202576=CARTESIAN_POINT('Ctrl Pts',(-41.373416251083,-46.2345318643232,
39.1161898821827));
#202577=CARTESIAN_POINT('Ctrl Pts',(-41.4460100362725,-46.5056000892427,
39.1034967087243));
#202578=CARTESIAN_POINT('Ctrl Pts',(-41.5410595633946,-46.4204333915663,
39.1031720232727));
#202579=CARTESIAN_POINT('Ctrl Pts',(-41.4839469723849,-46.3572886670234,
39.2077529615019));
#202580=CARTESIAN_POINT('Ctrl Pts',(-41.5228599914565,-46.5911245387428,
39.2875012672119));
#202581=CARTESIAN_POINT('Ctrl Pts',(-41.6181024753233,-46.5059978248574,
39.2872087095508));
#202582=CARTESIAN_POINT('Ctrl Pts',(-41.5454735069377,-46.4256208064855,
39.3549017048229));
#202583=CARTESIAN_POINT('Origin',(-41.1629311642483,-46.1905628026483,39.116));
#202584=CARTESIAN_POINT('Origin',(3.72719664096539E-16,-4.35908294926639E-17,
40.22725));
#202585=CARTESIAN_POINT('Origin',(-39.4864862581819,-43.8769616275872,40.22725));
#202586=CARTESIAN_POINT('Origin',(28.0951675083328,30.7283483363946,39.116));
#202587=CARTESIAN_POINT('Origin',(-40.8943347850526,-45.8923335519886,39.1160373285264));
#202588=CARTESIAN_POINT('Ctrl Pts',(-39.4144401478992,-43.7969047596345,
40.1599502534424));
#202589=CARTESIAN_POINT('Ctrl Pts',(-39.439394812269,-43.8246341160483,
40.10025));
#202590=CARTESIAN_POINT('Ctrl Pts',(-39.4864862581819,-43.8769616275872,
40.10025));
#202591=CARTESIAN_POINT('Ctrl Pts',(-39.3492813761645,-43.8555436924519,
40.159950056604));
#202592=CARTESIAN_POINT('Ctrl Pts',(-39.3919218645327,-43.8673524484222,
40.1002551305372));
#202593=CARTESIAN_POINT('Ctrl Pts',(-39.4486296259963,-43.911017546801,
40.10025));
#202594=CARTESIAN_POINT('Ctrl Pts',(-39.3054399757367,-43.9280312169047,
40.1203070619043));
#202595=CARTESIAN_POINT('Ctrl Pts',(-39.3632835603682,-43.923706596467,
40.0637098684494));
#202596=CARTESIAN_POINT('Ctrl Pts',(-39.4300423632771,-43.9607655567562,
40.0772636213361));
#202597=CARTESIAN_POINT('Ctrl Pts',(-39.2744854109877,-44.0526112349801,
40.0046102245805));
#202598=CARTESIAN_POINT('Ctrl Pts',(-39.3564679665371,-44.0109847679676,
39.9670001894019));
#202599=CARTESIAN_POINT('Ctrl Pts',(-39.4322155454628,-44.0555161714737,
40.0101788811211));
#202600=CARTESIAN_POINT('Ctrl Pts',(-39.285649880758,-44.1047669487876,
39.9303710930184));
#202601=CARTESIAN_POINT('Ctrl Pts',(-39.3789590643341,-44.0421591564532,
39.9058663574109));
#202602=CARTESIAN_POINT('Ctrl Pts',(-39.4516641984998,-44.1002097724415,
39.9671344706356));
#202603=CARTESIAN_POINT('Ctrl Pts',(-39.3160391863692,-44.1385184650374,
39.8576902534424));
#202604=CARTESIAN_POINT('Ctrl Pts',(-39.4103156382734,-44.0542875439838,
39.8579948730703));
#202605=CARTESIAN_POINT('Ctrl Pts',(-39.4820551873932,-44.1339623850445,
39.92499));
#202606=CARTESIAN_POINT('Origin',(-39.3876757945576,-44.2189419720521,39.92499));
#202607=CARTESIAN_POINT('Origin',(-40.8647803215177,-45.8594327453957,39.1925554488843));
#202608=CARTESIAN_POINT('Origin',(-40.8100197873549,-45.7986150108449,39.3343017080178));
#202609=CARTESIAN_POINT('Origin',(-39.5068809815269,-44.351332744487,39.6398955069215));
#202610=CARTESIAN_POINT('Origin',(-39.626086168372,-44.4837235168755,39.3548010137695));
#202611=CARTESIAN_POINT('Ctrl Pts',(-40.5892333705625,-45.553406853251,
39.3978017080178));
#202612=CARTESIAN_POINT('Ctrl Pts',(-40.6836127633981,-45.4684272662434,
39.3978017080178));
#202613=CARTESIAN_POINT('Ctrl Pts',(-40.6836127633981,-45.4684272662434,
39.5248017080178));
#202614=CARTESIAN_POINT('Ctrl Pts',(-40.6496361736976,-45.6201409680071,
39.3978017080178));
#202615=CARTESIAN_POINT('Ctrl Pts',(-40.7437849681275,-45.5352552698635,
39.3980355775177));
#202616=CARTESIAN_POINT('Ctrl Pts',(-40.773954806069,-45.5687622694489,
39.5248015517192));
#202617=CARTESIAN_POINT('Ctrl Pts',(-40.7067502157901,-45.6832443225576,
39.3484893995498));
#202618=CARTESIAN_POINT('Ctrl Pts',(-40.8009661159847,-45.5987613682826,
39.3489438303429));
#202619=CARTESIAN_POINT('Ctrl Pts',(-40.859379634455,-45.6636361529315,
39.4508333155592));
#202620=CARTESIAN_POINT('Ctrl Pts',(-40.7368493365299,-45.7165002428305,
39.2708017080178));
#202621=CARTESIAN_POINT('Ctrl Pts',(-40.8311340869939,-45.6322662944331,
39.2710850691866));
#202622=CARTESIAN_POINT('Ctrl Pts',(-40.9043991801906,-45.7136354238374,
39.3343017080178));
#202623=CARTESIAN_POINT('Origin',(-40.5892333705625,-45.5534068532509,39.5248017080178));
#202624=CARTESIAN_POINT('Ctrl Pts',(-39.5544469813073,-44.4033023070487,
39.2875012672119));
#202625=CARTESIAN_POINT('Ctrl Pts',(-39.6488649595838,-44.3189410241793,
39.2878045257519));
#202626=CARTESIAN_POINT('Ctrl Pts',(-39.7205730817653,-44.3988635552002,
39.3549015218347));
#202627=CARTESIAN_POINT('Ctrl Pts',(-39.6312929306913,-44.4888328647721,
39.1034938540228));
#202628=CARTESIAN_POINT('Ctrl Pts',(-39.7256930794109,-44.404266885711,
39.1038286278806));
#202629=CARTESIAN_POINT('Ctrl Pts',(-39.7821007282717,-44.4671969296246,
39.2077506434033));
#202630=CARTESIAN_POINT('Ctrl Pts',(-39.7693444365328,-44.6424847942257,
38.989));
#202631=CARTESIAN_POINT('Ctrl Pts',(-39.8638218465937,-44.5576736781004,
38.9892298954611));
#202632=CARTESIAN_POINT('Ctrl Pts',(-39.8926323785405,-44.5899547640676,
39.1161900347287));
#202633=CARTESIAN_POINT('Ctrl Pts',(-39.9143573409159,-44.8038810887672,
38.989));
#202634=CARTESIAN_POINT('Ctrl Pts',(-40.0088781074272,-44.7187742083303,
38.989));
#202635=CARTESIAN_POINT('Ctrl Pts',(-40.0087366280261,-44.7189015969553,
39.1161900945644));
#202636=CARTESIAN_POINT('Origin',(-39.9143573409159,-44.8038810887672,39.116));
#202637=CARTESIAN_POINT('Origin',(27.4203375923837,29.9788737863604,39.5248017080178));
#202638=CARTESIAN_POINT('Origin',(-40.4880553924346,-45.441037324517,39.5248017080178));
#202639=CARTESIAN_POINT('Origin',(27.3146622010794,29.8615093742684,39.116));
#202640=CARTESIAN_POINT('Origin',(-40.1828829233543,-45.1021848870409,39.1160402713849));
#202641=CARTESIAN_POINT('Ctrl Pts',(-40.3404336838195,-45.2779489569771,
39.2708017080178));
#202642=CARTESIAN_POINT('Ctrl Pts',(-40.4355776097271,-45.1929563204587,
39.27051194648));
#202643=CARTESIAN_POINT('Ctrl Pts',(-40.3616483211486,-45.1108495273511,
39.3343017080178));
#202644=CARTESIAN_POINT('Ctrl Pts',(-40.3706366483425,-45.3113153943828,
39.3487519301186));
#202645=CARTESIAN_POINT('Ctrl Pts',(-40.4655326953338,-45.226224813414,
39.3482879463985));
#202646=CARTESIAN_POINT('Ctrl Pts',(-40.4068200107203,-45.1610177711054,
39.4512271261638));
#202647=CARTESIAN_POINT('Ctrl Pts',(-40.427855606124,-45.3745283705075,
39.3978017080178));
#202648=CARTESIAN_POINT('Ctrl Pts',(-40.5223510101992,-45.2893279449762,
39.3975673827397));
#202649=CARTESIAN_POINT('Ctrl Pts',(-40.4923970402295,-45.2560606910602,
39.5248015355181));
#202650=CARTESIAN_POINT('Ctrl Pts',(-40.4880553924346,-45.441037324517,
39.3978017080178));
#202651=CARTESIAN_POINT('Ctrl Pts',(-40.5824347852702,-45.3560577375094,
39.3978017080178));
#202652=CARTESIAN_POINT('Ctrl Pts',(-40.5824347852702,-45.3560577375094,
39.5248017080178));
#202653=CARTESIAN_POINT('Origin',(-40.267268928313,-45.1958291143586,39.3343017080178));
#202654=CARTESIAN_POINT('Origin',(-40.2128349746545,-45.1353740846424,39.1934008533546));
#202655=CARTESIAN_POINT('Origin',(-45.8594327460075,-40.864780322453,39.1925554495082));
#202656=CARTESIAN_POINT('Origin',(-45.8923335519897,-40.8943347850517,39.116037328527));
#202657=CARTESIAN_POINT('Origin',(-45.7986150108453,-40.8100197873545,39.3343017080178));
#202658=CARTESIAN_POINT('Ctrl Pts',(-45.7165002428309,-40.7368493365295,
39.2708017080178));
#202659=CARTESIAN_POINT('Ctrl Pts',(-45.6322662944335,-40.8311340869935,
39.2710850691866));
#202660=CARTESIAN_POINT('Ctrl Pts',(-45.7136354238378,-40.9043991801901,
39.3343017080178));
#202661=CARTESIAN_POINT('Ctrl Pts',(-45.6831319408677,-40.7066485019706,
39.3487519293518));
#202662=CARTESIAN_POINT('Ctrl Pts',(-45.5986481857991,-40.8008642060175,
39.3492068662924));
#202663=CARTESIAN_POINT('Ctrl Pts',(-45.663467198768,-40.859227507442,39.4512271248737));
#202664=CARTESIAN_POINT('Ctrl Pts',(-45.6199161851841,-40.6494327168526,
39.3978017080178));
#202665=CARTESIAN_POINT('Ctrl Pts',(-45.5350300257406,-40.7435821574131,
39.3980347781197));
#202666=CARTESIAN_POINT('Ctrl Pts',(-45.5684243021849,-40.7736504989768,
39.5248015355195));
#202667=CARTESIAN_POINT('Ctrl Pts',(-45.5534068532514,-40.589233370562,
39.3978017080178));
#202668=CARTESIAN_POINT('Ctrl Pts',(-45.4684272662438,-40.6836127633977,
39.3978017080178));
#202669=CARTESIAN_POINT('Ctrl Pts',(-45.4684272662438,-40.6836127633977,
39.5248017080178));
#202670=CARTESIAN_POINT('Origin',(-45.5534068532514,-40.589233370562,39.5248017080178));
#202671=CARTESIAN_POINT('Origin',(-0.212448967518931,0.235948482089074,
39.116));
#202672=CARTESIAN_POINT('Origin',(-46.1905628026487,-41.1629311642478,39.116));
#202673=CARTESIAN_POINT('Origin',(-0.212448967518931,0.235948482089074,
39.5248017080178));
#202674=CARTESIAN_POINT('Origin',(-45.4410373245174,-40.4880553924341,39.5248017080178));
#202675=CARTESIAN_POINT('Ctrl Pts',(-46.5911245387432,-41.522859991456,
39.2875012672119));
#202676=CARTESIAN_POINT('Ctrl Pts',(-46.5059978322079,-41.6181024670993,
39.287208709576));
#202677=CARTESIAN_POINT('Ctrl Pts',(-46.4256208133856,-41.5454735131718,
39.3549016990121));
#202678=CARTESIAN_POINT('Ctrl Pts',(-46.5055987918453,-41.4460088704659,
39.103493917393));
#202679=CARTESIAN_POINT('Ctrl Pts',(-46.4204321019767,-41.5410583874205,
39.1031692336335));
#202680=CARTESIAN_POINT('Ctrl Pts',(-46.3572876358789,-41.4839460439595,
39.2077507202298));
#202681=CARTESIAN_POINT('Ctrl Pts',(-46.3519544194668,-41.307949174952,
38.989));
#202682=CARTESIAN_POINT('Ctrl Pts',(-46.2668368728755,-41.4027599825081,
38.9887769311176));
#202683=CARTESIAN_POINT('Ctrl Pts',(-46.2345298607753,-41.3734144471015,
39.1161898712912));
#202684=CARTESIAN_POINT('Ctrl Pts',(-46.1905628026487,-41.1629311642478,
38.989));
#202685=CARTESIAN_POINT('Ctrl Pts',(-46.105456260079,-41.2574515555195,
38.989));
#202686=CARTESIAN_POINT('Ctrl Pts',(-46.1055833103324,-41.2573104519181,
39.1161895903851));
#202687=CARTESIAN_POINT('Origin',(-46.5107200467159,-41.4512020416172,39.3548010137695));
#202688=CARTESIAN_POINT('Ctrl Pts',(-45.4410373245174,-40.4880553924341,
39.3978017080178));
#202689=CARTESIAN_POINT('Ctrl Pts',(-45.3560577375098,-40.5824347852697,
39.3978017080178));
#202690=CARTESIAN_POINT('Ctrl Pts',(-45.3560577375098,-40.5824347852697,
39.5248017080178));
#202691=CARTESIAN_POINT('Ctrl Pts',(-45.3743035899552,-40.4276521486879,
39.3978017080178));
#202692=CARTESIAN_POINT('Ctrl Pts',(-45.2891025640473,-40.5221480762974,
39.3975666025007));
#202693=CARTESIAN_POINT('Ctrl Pts',(-45.2557227253151,-40.492092734505,
39.5248015517178));
#202694=CARTESIAN_POINT('Ctrl Pts',(-45.3112030195551,-40.3705349278739,
39.3484894016716));
#202695=CARTESIAN_POINT('Ctrl Pts',(-45.226112733224,-40.4654317778745,
39.3480259000057));
#202696=CARTESIAN_POINT('Ctrl Pts',(-45.1608488177571,-40.4066678844414,
39.4508333188948));
#202697=CARTESIAN_POINT('Ctrl Pts',(-45.2779489569775,-40.340433683819,
39.2708017080178));
#202698=CARTESIAN_POINT('Ctrl Pts',(-45.1929563204591,-40.4355776097266,
39.27051194648));
#202699=CARTESIAN_POINT('Ctrl Pts',(-45.1108495273515,-40.3616483211481,
39.3343017080178));
#202700=CARTESIAN_POINT('Origin',(-45.1958291143591,-40.2672689283125,39.3343017080178));
#202701=CARTESIAN_POINT('Origin',(-46.6431106370695,-41.5704070646303,39.6398955068187));
#202702=CARTESIAN_POINT('Origin',(-46.7755012272975,-41.6896120874668,39.92499));
#202703=CARTESIAN_POINT('Origin',(-45.1353740836144,-40.2128349741382,39.1934008539952));
#202704=CARTESIAN_POINT('Origin',(-45.1021848870414,-40.1828829233533,39.1160402713854));
#202705=CARTESIAN_POINT('Ctrl Pts',(-46.7942619810919,-42.1132001505999,
40.1599502534424));
#202706=CARTESIAN_POINT('Ctrl Pts',(-46.7665330160781,-42.0882450513173,
40.10025));
#202707=CARTESIAN_POINT('Ctrl Pts',(-46.7142062431425,-42.0411527846893,
40.10025));
#202708=CARTESIAN_POINT('Ctrl Pts',(-46.8532067119186,-42.0477032750701,
40.1599500538469));
#202709=CARTESIAN_POINT('Ctrl Pts',(-46.8094668591651,-42.0405341034489,
40.100244835349));
#202710=CARTESIAN_POINT('Ctrl Pts',(-46.7483190388761,-42.0032346206974,
40.10025));
#202711=CARTESIAN_POINT('Ctrl Pts',(-46.8890030154865,-41.9705316734063,
40.1202442001039));
#202712=CARTESIAN_POINT('Ctrl Pts',(-46.8318174060858,-41.9811230778543,
40.0633873868017));
#202713=CARTESIAN_POINT('Ctrl Pts',(-46.761203850955,-41.9515093836258,
40.0772271723538));
#202714=CARTESIAN_POINT('Ctrl Pts',(-46.906368706767,-41.8426461117366,
40.0045995998162));
#202715=CARTESIAN_POINT('Ctrl Pts',(-46.829061965151,-41.8933796070861,
39.9663485808314));
#202716=CARTESIAN_POINT('Ctrl Pts',(-46.74851255448,-41.8570065263031,40.0101727202465));
#202717=CARTESIAN_POINT('Ctrl Pts',(-46.8896982576908,-41.7917018131131,
39.9304654349859));
#202718=CARTESIAN_POINT('Ctrl Pts',(-46.8032976561895,-41.8649047103977,
39.9051900162951));
#202719=CARTESIAN_POINT('Ctrl Pts',(-46.724315266822,-41.8144193983034,
39.9671857458188));
#202720=CARTESIAN_POINT('Ctrl Pts',(-46.8559036426987,-41.761272367336,
39.8576902534424));
#202721=CARTESIAN_POINT('Ctrl Pts',(-46.7709043015504,-41.8563683535928,
39.8573998014387));
#202722=CARTESIAN_POINT('Ctrl Pts',(-46.6905216402899,-41.7839914803024,
39.92499));
#202723=CARTESIAN_POINT('Origin',(-46.7142062431425,-42.0411527846893,40.22725));
#202724=CARTESIAN_POINT('Origin',(-0.212448967518931,0.235948482089074,
39.116));
#202725=CARTESIAN_POINT('Origin',(-44.8038810887676,-39.9143573409155,39.116));
#202726=CARTESIAN_POINT('Origin',(9.23291810287662E-17,1.10332673220367E-16,
40.22725));
#202727=CARTESIAN_POINT('Origin',(-46.6938111422607,-42.0638038389698,40.22725));
#202728=CARTESIAN_POINT('Ctrl Pts',(-44.8038810887676,-39.9143573409155,
38.989));
#202729=CARTESIAN_POINT('Ctrl Pts',(-44.7187741985013,-40.0088781183435,
38.989));
#202730=CARTESIAN_POINT('Ctrl Pts',(-44.7189015969703,-40.0087366280094,
39.1161901092323));
#202731=CARTESIAN_POINT('Ctrl Pts',(-44.6424822887487,-39.7693421853894,
38.989));
#202732=CARTESIAN_POINT('Ctrl Pts',(-44.5576711710495,-39.8638196089396,
38.9892298989784));
#202733=CARTESIAN_POINT('Ctrl Pts',(-44.589952766033,-39.8926305794718,
39.1161900493203));
#202734=CARTESIAN_POINT('Ctrl Pts',(-44.4888315723759,-39.6312917695239,
39.1034966344368));
#202735=CARTESIAN_POINT('Ctrl Pts',(-44.4042655856137,-39.7256919284549,
39.1038314102544));
#202736=CARTESIAN_POINT('Ctrl Pts',(-44.467195904383,-39.7820998051097,
39.2077528789598));
#202737=CARTESIAN_POINT('Ctrl Pts',(-44.4033023070491,-39.5544469813068,
39.2875012672119));
#202738=CARTESIAN_POINT('Ctrl Pts',(-44.3189410144583,-39.6488649704636,
39.2878045257868));
#202739=CARTESIAN_POINT('Ctrl Pts',(-44.3988635644384,-39.7205730900532,
39.35490152959));
#202740=CARTESIAN_POINT('Origin',(-44.4837235168759,-39.6260861683715,39.3548010137695));
#202741=CARTESIAN_POINT('Ctrl Pts',(-46.4302753505427,-42.2339804752699,
39.8576902534424));
#202742=CARTESIAN_POINT('Ctrl Pts',(-46.5159655405277,-42.1395065320997,
39.8573998014387));
#202743=CARTESIAN_POINT('Ctrl Pts',(-46.4355828792672,-42.0671296588093,
39.92499));
#202744=CARTESIAN_POINT('Ctrl Pts',(-46.4640859592741,-42.264423027446,
39.9304984902493));
#202745=CARTESIAN_POINT('Ctrl Pts',(-46.5278479142027,-42.1708479205167,
39.9052171569797));
#202746=CARTESIAN_POINT('Ctrl Pts',(-46.4693919041982,-42.0975714415909,
39.9672049726614));
#202747=CARTESIAN_POINT('Ctrl Pts',(-46.5163638812298,-42.2755508889259,
40.0043437678659));
#202748=CARTESIAN_POINT('Ctrl Pts',(-46.5588164356976,-42.1933444849778,
39.9661628577643));
#202749=CARTESIAN_POINT('Ctrl Pts',(-46.5141432491634,-42.1170605480847,
40.0100243556235));
#202750=CARTESIAN_POINT('Ctrl Pts',(-46.6408663419437,-42.2454039774545,
40.119487482199));
#202751=CARTESIAN_POINT('Ctrl Pts',(-46.6457133039302,-42.1872204559322,
40.0627551483141));
#202752=CARTESIAN_POINT('Ctrl Pts',(-46.6088541045843,-42.1199995355544,
40.0767884282377));
#202753=CARTESIAN_POINT('Ctrl Pts',(-46.7146600431957,-42.2015749714291,
40.1599502015393));
#202754=CARTESIAN_POINT('Ctrl Pts',(-46.7029882531949,-42.1587905896511,
40.1002449453875));
#202755=CARTESIAN_POINT('Ctrl Pts',(-46.6595535157373,-42.1018187547555,
40.10025));
#202756=CARTESIAN_POINT('Ctrl Pts',(-46.773831928426,-42.1358900227693,
40.1599502534424));
#202757=CARTESIAN_POINT('Ctrl Pts',(-46.7461150696875,-42.1109214781059,
40.10025));
#202758=CARTESIAN_POINT('Ctrl Pts',(-46.6938111422607,-42.0638038389698,
40.10025));
#202759=CARTESIAN_POINT('Origin',(-46.3506032922596,-42.161509051645,39.92499));
#202760=CARTESIAN_POINT('Origin',(-44.3513327445024,-39.5068809815374,39.6398955069331));
#202761=CARTESIAN_POINT('Origin',(-44.2189419720525,-39.3876757945571,39.92499));
#202762=CARTESIAN_POINT('Origin',(-46.2182127020509,-42.0423040287663,39.6398955068274));
#202763=CARTESIAN_POINT('Origin',(-46.085822111678,-41.9230990057953,39.3548010137695));
#202764=CARTESIAN_POINT('Ctrl Pts',(-44.1385184650378,-39.3160391863687,
39.8576902534424));
#202765=CARTESIAN_POINT('Ctrl Pts',(-44.0542875439842,-39.4103156382729,
39.8579948730703));
#202766=CARTESIAN_POINT('Ctrl Pts',(-44.1339623850449,-39.4820551873928,
39.92499));
#202767=CARTESIAN_POINT('Ctrl Pts',(-44.1047525536513,-39.285636938894,
39.9304020711229));
#202768=CARTESIAN_POINT('Ctrl Pts',(-44.0421527706808,-39.3789425853227,
39.9058915297381));
#202769=CARTESIAN_POINT('Ctrl Pts',(-44.100195430388,-39.451651284856,39.9671523786027));
#202770=CARTESIAN_POINT('Ctrl Pts',(-44.0527517782418,-39.2745942850998,
40.0043257306695));
#202771=CARTESIAN_POINT('Ctrl Pts',(-44.0110417363802,-39.3566016867495,
39.9667894847835));
#202772=CARTESIAN_POINT('Ctrl Pts',(-44.0556530121005,-39.4323285306299,
40.01001389752));
#202773=CARTESIAN_POINT('Ctrl Pts',(-43.9290071509458,-39.3050549810249,
40.1195533054855));
#202774=CARTESIAN_POINT('Ctrl Pts',(-43.9243964923857,-39.3631024520341,
40.0630813209236));
#202775=CARTESIAN_POINT('Ctrl Pts',(-43.9614781338111,-39.4299498468377,
40.0768265942421));
#202776=CARTESIAN_POINT('Ctrl Pts',(-43.8557442421763,-39.3490583909339,
40.1599502027517));
#202777=CARTESIAN_POINT('Ctrl Pts',(-43.8675206320097,-39.3917348424039,
40.1002552791553));
#202778=CARTESIAN_POINT('Ctrl Pts',(-43.9111340157071,-39.4485000225468,
40.10025));
#202779=CARTESIAN_POINT('Ctrl Pts',(-43.7969047596348,-39.4144401478987,
40.1599502534424));
#202780=CARTESIAN_POINT('Ctrl Pts',(-43.8246341160487,-39.4393948122686,
40.10025));
#202781=CARTESIAN_POINT('Ctrl Pts',(-43.8769616275876,-39.4864862581814,
40.10025));
#202782=CARTESIAN_POINT('Origin',(-43.8769616275876,-39.4864862581814,40.22725));
#202783=CARTESIAN_POINT('Ctrl Pts',(-45.7656648676108,-41.634828128426,
38.989));
#202784=CARTESIAN_POINT('Ctrl Pts',(-45.8507714175129,-41.5403077290107,
38.989));
#202785=CARTESIAN_POINT('Ctrl Pts',(-45.8506443599162,-41.5404488407678,
39.1161896013269));
#202786=CARTESIAN_POINT('Ctrl Pts',(-45.9267609786668,-41.7801793767981,
38.989));
#202787=CARTESIAN_POINT('Ctrl Pts',(-46.0121552117527,-41.6856176794253,
38.9887769275485));
#202788=CARTESIAN_POINT('Ctrl Pts',(-45.9795929135641,-41.6565546403125,
39.1161898821851));
#202789=CARTESIAN_POINT('Ctrl Pts',(-46.0801233673977,-41.9185498083221,
39.1034967087243));
#202790=CARTESIAN_POINT('Ctrl Pts',(-46.165749859237,-41.8239142817197,
39.1031720232693));
#202791=CARTESIAN_POINT('Ctrl Pts',(-46.1023497159528,-41.7670853619627,
39.2077529614997));
#202792=CARTESIAN_POINT('Ctrl Pts',(-46.1654920697614,-41.9955727382249,
39.2875012672119));
#202793=CARTESIAN_POINT('Ctrl Pts',(-46.2513146407507,-41.9009568069087,
39.2872087095508));
#202794=CARTESIAN_POINT('Ctrl Pts',(-46.1706818552408,-41.8286118967075,
39.3549017048229));
#202795=CARTESIAN_POINT('Origin',(-45.7656648676108,-41.634828128426,39.116));
#202796=CARTESIAN_POINT('Origin',(3.68378193773366E-16,-3.92493591694921E-17,
40.22725));
#202797=CARTESIAN_POINT('Origin',(-43.8565665267058,-39.509137312462,40.22725));
#202798=CARTESIAN_POINT('Origin',(34.5756856720389,30.7048488218244,39.116));
#202799=CARTESIAN_POINT('Origin',(-45.4673664422114,-41.3663085755624,39.116037328527));
#202800=CARTESIAN_POINT('Ctrl Pts',(-43.7765468711724,-39.4370498736006,
40.1599502534424));
#202801=CARTESIAN_POINT('Ctrl Pts',(-43.8042633382931,-39.4620188529807,
40.10025));
#202802=CARTESIAN_POINT('Ctrl Pts',(-43.8565665267058,-39.509137312462,
40.10025));
#202803=CARTESIAN_POINT('Ctrl Pts',(-43.7178744835419,-39.5021785224865,
40.159950056604));
#202804=CARTESIAN_POINT('Ctrl Pts',(-43.7615157339672,-39.5094654441334,
40.1002551305381));
#202805=CARTESIAN_POINT('Ctrl Pts',(-43.8224770900135,-39.5469637653747,
40.10025));
#202806=CARTESIAN_POINT('Ctrl Pts',(-43.6818502604301,-39.5788516269096,
40.1203070619047));
#202807=CARTESIAN_POINT('Ctrl Pts',(-43.7389249259241,-39.5685043961836,
40.0637098684497));
#202808=CARTESIAN_POINT('Ctrl Pts',(-43.8091917332948,-39.598382148533,
40.0772636213364));
#202809=CARTESIAN_POINT('Ctrl Pts',(-43.664087425869,-39.705984815696,40.0046102245801));
#202810=CARTESIAN_POINT('Ctrl Pts',(-43.7412697217731,-39.6560168722791,
39.9670001894016));
#202811=CARTESIAN_POINT('Ctrl Pts',(-43.8212571467115,-39.6923865500761,
40.0101788811207));
#202812=CARTESIAN_POINT('Ctrl Pts',(-43.68064249212,-39.7566878101779,39.9303710930186));
#202813=CARTESIAN_POINT('Ctrl Pts',(-43.7668962219046,-39.6846695243128,
39.9058663574113));
#202814=CARTESIAN_POINT('Ctrl Pts',(-43.84527101142,-39.734802377007,39.9671344706375));
#202815=CARTESIAN_POINT('Ctrl Pts',(-43.7143933160625,-39.7870778846745,
39.8576902534424));
#202816=CARTESIAN_POINT('Ctrl Pts',(-43.7993487829615,-39.6934538167798,
39.8579948730704));
#202817=CARTESIAN_POINT('Ctrl Pts',(-43.8790236240222,-39.7651933658996,
39.92499));
#202818=CARTESIAN_POINT('Origin',(-43.7940440370146,-39.8595727587353,39.92499));
#202819=CARTESIAN_POINT('Origin',(-45.4345348103664,-41.3366772856882,39.192555448885));
#202820=CARTESIAN_POINT('Origin',(-45.3737170758075,-41.2819167515326,39.3343017080178));
#202821=CARTESIAN_POINT('Origin',(-43.9264348094887,-39.9787779456578,39.6398955069202));
#202822=CARTESIAN_POINT('Origin',(-44.058825581838,-40.0979831325497,39.3548010137695));
#202823=CARTESIAN_POINT('Ctrl Pts',(-45.1285089182135,-41.0611303347402,
39.3978017080178));
#202824=CARTESIAN_POINT('Ctrl Pts',(-45.2134885052211,-40.9667509419046,
39.3978017080178));
#202825=CARTESIAN_POINT('Ctrl Pts',(-45.2134885052211,-40.9667509419045,
39.5248017080178));
#202826=CARTESIAN_POINT('Ctrl Pts',(-45.1955564429372,-41.1211850608431,
39.3978017080178));
#202827=CARTESIAN_POINT('Ctrl Pts',(-45.2803165088391,-41.026923146635,
39.3980355775229));
#202828=CARTESIAN_POINT('Ctrl Pts',(-45.3138235084264,-41.0570929845753,
39.5248015517192));
#202829=CARTESIAN_POINT('Ctrl Pts',(-45.2589537050076,-41.1779726855658,
39.3484893995498));
#202830=CARTESIAN_POINT('Ctrl Pts',(-45.3438226072617,-41.0841042944915,
39.3489438303395));
#202831=CARTESIAN_POINT('Ctrl Pts',(-45.4086973919094,-41.1425178129616,
39.4508333155593));
#202832=CARTESIAN_POINT('Ctrl Pts',(-45.2923641298559,-41.2079002115905,
39.2708017080178));
#202833=CARTESIAN_POINT('Ctrl Pts',(-45.3773275334108,-41.1142722655004,
39.2710850691866));
#202834=CARTESIAN_POINT('Ctrl Pts',(-45.4586966628151,-41.187537358697,
39.3343017080178));
#202835=CARTESIAN_POINT('Origin',(-45.1285089182135,-41.0611303347402,39.5248017080178));
#202836=CARTESIAN_POINT('Ctrl Pts',(-43.9791725362585,-40.0254908126586,
39.2875012672119));
#202837=CARTESIAN_POINT('Ctrl Pts',(-44.0642551277132,-39.9317223035495,
39.2878045257519));
#202838=CARTESIAN_POINT('Ctrl Pts',(-44.1439246046466,-40.0037114707676,
39.3549015218347));
#202839=CARTESIAN_POINT('Ctrl Pts',(-44.0645378932555,-40.1025202360368,
39.1034938540228));
#202840=CARTESIAN_POINT('Ctrl Pts',(-44.1495813562482,-40.0085500157871,
39.103828627881));
#202841=CARTESIAN_POINT('Ctrl Pts',(-44.2122579788861,-40.0652391174794,
39.2077506434033));
#202842=CARTESIAN_POINT('Ctrl Pts',(-44.2178941385633,-40.240900132391,
38.989));
#202843=CARTESIAN_POINT('Ctrl Pts',(-44.3029888158476,-40.1466780419424,
38.989229895463));
#202844=CARTESIAN_POINT('Ctrl Pts',(-44.335015812998,-40.1757707681158,
39.1161900347288));
#202845=CARTESIAN_POINT('Ctrl Pts',(-44.3789831537298,-40.3862543050936,
38.989));
#202846=CARTESIAN_POINT('Ctrl Pts',(-44.4640900341667,-40.2917335385823,
38.989));
#202847=CARTESIAN_POINT('Ctrl Pts',(-44.4639626455417,-40.2918750179834,
39.1161900945645));
#202848=CARTESIAN_POINT('Origin',(-44.3789831537298,-40.3862543050936,39.116));
#202849=CARTESIAN_POINT('Origin',(33.743309857225,29.9553742717902,39.5248017080178));
#202850=CARTESIAN_POINT('Origin',(-45.0161393894795,-40.9599523566123,39.5248017080178));
#202851=CARTESIAN_POINT('Origin',(33.61296347236,29.8380098596982,39.116));
#202852=CARTESIAN_POINT('Origin',(-44.6772189625516,-40.654855397468,39.1160402713849));
#202853=CARTESIAN_POINT('Ctrl Pts',(-44.8522789915944,-40.8131880745604,
39.2708017080178));
#202854=CARTESIAN_POINT('Ctrl Pts',(-44.9380175594364,-40.7187157882335,
39.27051194648));
#202855=CARTESIAN_POINT('Ctrl Pts',(-44.8559107663287,-40.644786499655,
39.3343017080178));
#202856=CARTESIAN_POINT('Ctrl Pts',(-44.8858042435438,-40.8432146576637,
39.3487519301186));
#202857=CARTESIAN_POINT('Ctrl Pts',(-44.97128605239,-40.7486708738366,39.3482879464018));
#202858=CARTESIAN_POINT('Ctrl Pts',(-44.906079010081,-40.6899581892249,
39.4512271261645));
#202859=CARTESIAN_POINT('Ctrl Pts',(-44.9493173051404,-40.9001003367645,
39.3978017080178));
#202860=CARTESIAN_POINT('Ctrl Pts',(-45.0343891839553,-40.8054891887082,
39.3975673827364));
#202861=CARTESIAN_POINT('Ctrl Pts',(-45.0011219300394,-40.7755352187373,
39.5248015355181));
#202862=CARTESIAN_POINT('Ctrl Pts',(-45.0161393894795,-40.9599523566123,
39.3978017080178));
#202863=CARTESIAN_POINT('Ctrl Pts',(-45.1011189764871,-40.8655729637766,
39.3978017080178));
#202864=CARTESIAN_POINT('Ctrl Pts',(-45.1011189764871,-40.8655729637766,
39.5248017080178));
#202865=CARTESIAN_POINT('Origin',(-44.7709311793212,-40.7391658924907,39.3343017080178));
#202866=CARTESIAN_POINT('Origin',(-44.7104761492019,-40.6847319392791,39.1934008533549));
#202867=CARTESIAN_POINT('Origin',(-49.8797426639499,-35.8473027488279,39.1925554495084));
#202868=CARTESIAN_POINT('Origin',(-49.9155525184331,-35.8732562382984,39.116037328528));
#202869=CARTESIAN_POINT('Origin',(-49.8135340601225,-35.799199382066,39.3343017080178));
#202870=CARTESIAN_POINT('Ctrl Pts',(-49.7242207306177,-35.7350130971387,
39.2708017080178));
#202871=CARTESIAN_POINT('Ctrl Pts',(-49.6503036646787,-35.8375861910554,
39.2710850691866));
#202872=CARTESIAN_POINT('Ctrl Pts',(-49.7388853330813,-35.9019445403516,
39.3343017080178));
#202873=CARTESIAN_POINT('Ctrl Pts',(-49.6878783768805,-35.7084656432344,
39.3487519293518));
#202874=CARTESIAN_POINT('Ctrl Pts',(-49.6137056554148,-35.8109961808816,
39.3492068662919));
#202875=CARTESIAN_POINT('Ctrl Pts',(-49.6842702092604,-35.8622643302234,
39.4512271248732));
#202876=CARTESIAN_POINT('Ctrl Pts',(-49.6190282456266,-35.6581711379714,
39.3978017080178));
#202877=CARTESIAN_POINT('Ctrl Pts',(-49.5444483977901,-35.7606778378481,
39.3980347781178));
#202878=CARTESIAN_POINT('Ctrl Pts',(-49.5808027344264,-35.7870908094911,
39.5248015355195));
#202879=CARTESIAN_POINT('Ctrl Pts',(-49.5465907136146,-35.6052536882599,
39.3978017080178));
#202880=CARTESIAN_POINT('Ctrl Pts',(-49.4719419865735,-35.7079988465456,
39.3978017080178));
#202881=CARTESIAN_POINT('Ctrl Pts',(-49.4719419865735,-35.7079988465456,
39.5248017080178));
#202882=CARTESIAN_POINT('Origin',(-49.5465907136146,-35.6052536882599,39.5248017080178));
#202883=CARTESIAN_POINT('Origin',(-0.186621817602853,0.256862895714047,
39.116));
#202884=CARTESIAN_POINT('Origin',(-50.2402240048085,-36.1092077731526,39.116));
#202885=CARTESIAN_POINT('Origin',(-0.186621817602853,0.256862895714047,
39.5248017080178));
#202886=CARTESIAN_POINT('Origin',(-49.4242607783462,-35.5163757878393,39.5248017080178));
#202887=CARTESIAN_POINT('Ctrl Pts',(-50.676214228995,-36.4252947698676,
39.2875012672119));
#202888=CARTESIAN_POINT('Ctrl Pts',(-50.6015094050817,-36.5289136610813,
39.287208709576));
#202889=CARTESIAN_POINT('Ctrl Pts',(-50.5139809070357,-36.4650842624219,
39.3549016990122));
#202890=CARTESIAN_POINT('Ctrl Pts',(-50.5831238715085,-36.3578045222543,
39.1034939173931));
#202891=CARTESIAN_POINT('Ctrl Pts',(-50.5083591136198,-36.4612356912225,
39.1031692336333));
#202892=CARTESIAN_POINT('Ctrl Pts',(-50.4395906940211,-36.4110366091596,
39.2077507202295));
#202893=CARTESIAN_POINT('Ctrl Pts',(-50.415890011269,-36.2365613423289,
38.989));
#202894=CARTESIAN_POINT('Ctrl Pts',(-50.3411491755196,-36.339749972703,
38.9887769311182));
#202895=CARTESIAN_POINT('Ctrl Pts',(-50.3059517008894,-36.3139421975384,
39.1161898712915));
#202896=CARTESIAN_POINT('Ctrl Pts',(-50.2402240048085,-36.1092077731526,
38.989));
#202897=CARTESIAN_POINT('Ctrl Pts',(-50.1654637560308,-36.2121064279401,
38.989));
#202898=CARTESIAN_POINT('Ctrl Pts',(-50.1655753609471,-36.2119528169511,
39.1161895903853));
#202899=CARTESIAN_POINT('Origin',(-50.5887599058103,-36.3624339277671,39.3548010137695));
#202900=CARTESIAN_POINT('Ctrl Pts',(-49.4242607783463,-35.5163757878393,
39.3978017080178));
#202901=CARTESIAN_POINT('Ctrl Pts',(-49.3496120513051,-35.619120946125,
39.3978017080178));
#202902=CARTESIAN_POINT('Ctrl Pts',(-49.3496120513051,-35.6191209461249,
39.5248017080178));
#202903=CARTESIAN_POINT('Ctrl Pts',(-49.3515787599185,-35.4632790141053,
39.3978017080178));
#202904=CARTESIAN_POINT('Ctrl Pts',(-49.2767219882448,-35.5661632154432,
39.3975666025054));
#202905=CARTESIAN_POINT('Ctrl Pts',(-49.2403833690709,-35.5397616632038,
39.5248015517178));
#202906=CARTESIAN_POINT('Ctrl Pts',(-49.2828534857277,-35.4130704930583,
39.3484894016716));
#202907=CARTESIAN_POINT('Ctrl Pts',(-49.208148754787,-35.5163418450528,
39.3480259000026));
#202908=CARTESIAN_POINT('Ctrl Pts',(-49.1370998624026,-35.4647218031678,
39.4508333188949));
#202909=CARTESIAN_POINT('Ctrl Pts',(-49.2466351556014,-35.3866101428257,
39.2708017080178));
#202910=CARTESIAN_POINT('Ctrl Pts',(-49.1720533660033,-35.4901170100364,
39.2705119464801));
#202911=CARTESIAN_POINT('Ctrl Pts',(-49.0826686475736,-35.4251752107435,
39.3343017080178));
#202912=CARTESIAN_POINT('Origin',(-49.1573173746148,-35.3224300524579,39.3343017080178));
#202913=CARTESIAN_POINT('Origin',(-50.732885564526,-36.4671473482319,39.6398955068188));
#202914=CARTESIAN_POINT('Origin',(-50.8770112231004,-36.5718607685319,39.92499));
#202915=CARTESIAN_POINT('Origin',(-49.0915036252757,-35.2746135646437,39.1934008539937));
#202916=CARTESIAN_POINT('Origin',(-49.0553654007528,-35.2482948100394,39.1160402713847));
#202917=CARTESIAN_POINT('Ctrl Pts',(-50.9399462128204,-36.9911673391705,
40.1599502534424));
#202918=CARTESIAN_POINT('Ctrl Pts',(-50.9097606317996,-36.9692474126338,
40.10025));
#202919=CARTESIAN_POINT('Ctrl Pts',(-50.8527980281387,-36.9278827595324,
40.10025));
#202920=CARTESIAN_POINT('Ctrl Pts',(-50.9917217504962,-36.9198678602471,
40.1599500538471));
#202921=CARTESIAN_POINT('Ctrl Pts',(-50.9474721267406,-36.9173100216903,
40.100244835349));
#202922=CARTESIAN_POINT('Ctrl Pts',(-50.8827604229961,-36.8866065570947,
40.10025));
#202923=CARTESIAN_POINT('Ctrl Pts',(-51.0192553292378,-36.8393772800889,
40.1202442001037));
#202924=CARTESIAN_POINT('Ctrl Pts',(-50.9634900918192,-36.8558881875865,
40.0633873868015));
#202925=CARTESIAN_POINT('Ctrl Pts',(-50.8901678911824,-36.8338178466772,
40.0772271723538));
#202926=CARTESIAN_POINT('Ctrl Pts',(-51.0231582082091,-36.710377079884,
40.0045995998164));
#202927=CARTESIAN_POINT('Ctrl Pts',(-50.951578055318,-36.7689134067394,
39.9663485808318));
#202928=CARTESIAN_POINT('Ctrl Pts',(-50.8676678805081,-36.7411592876131,
40.0101727202465));
#202929=CARTESIAN_POINT('Ctrl Pts',(-51.0012539523496,-36.6614543958826,
39.9304654349858));
#202930=CARTESIAN_POINT('Ctrl Pts',(-50.922978448743,-36.7432876021378,
39.9051900162949));
#202931=CARTESIAN_POINT('Ctrl Pts',(-50.8391515810792,-36.7013347616509,
39.9671857458173));
#202932=CARTESIAN_POINT('Ctrl Pts',(-50.9644637245895,-36.6347241449652,
39.8576902534424));
#202933=CARTESIAN_POINT('Ctrl Pts',(-50.8898702560319,-36.7381840359682,
39.8573998014387));
#202934=CARTESIAN_POINT('Ctrl Pts',(-50.8023624960593,-36.6746059268175,
39.92499));
#202935=CARTESIAN_POINT('Origin',(-50.8527980281387,-36.9278827595324,40.22725));
#202936=CARTESIAN_POINT('Origin',(-0.186621817602853,0.256862895714047,
39.116));
#202937=CARTESIAN_POINT('Origin',(-48.7306271754178,-35.0124214764582,39.116));
#202938=CARTESIAN_POINT('Origin',(1.03190816135906E-16,9.69196709112357E-17,
40.22725));
#202939=CARTESIAN_POINT('Origin',(-50.8348823336488,-36.9525415975209,40.22725));
#202940=CARTESIAN_POINT('Ctrl Pts',(-48.7306271754178,-35.0124214764582,
38.989));
#202941=CARTESIAN_POINT('Ctrl Pts',(-48.6558666212126,-35.1153205516308,
38.989));
#202942=CARTESIAN_POINT('Ctrl Pts',(-48.6559785320123,-35.1151665196292,
39.1161901092324));
#202943=CARTESIAN_POINT('Ctrl Pts',(-48.5549543235573,-34.8850714976637,
38.989));
#202944=CARTESIAN_POINT('Ctrl Pts',(-48.4804833899316,-34.9878965398047,
38.9892298989778));
#202945=CARTESIAN_POINT('Ctrl Pts',(-48.5155997094345,-35.0131753353128,
39.1161900493204));
#202946=CARTESIAN_POINT('Ctrl Pts',(-48.3877151240598,-34.7638382096857,
39.1034966344368));
#202947=CARTESIAN_POINT('Ctrl Pts',(-48.3134799021657,-34.8665607873099,
39.1038314102547));
#202948=CARTESIAN_POINT('Ctrl Pts',(-48.3819617107265,-34.9160816461997,
39.2077528789594));
#202949=CARTESIAN_POINT('Ctrl Pts',(-48.2946219293748,-34.6963546279283,
39.2875012672119));
#202950=CARTESIAN_POINT('Ctrl Pts',(-48.220592144083,-34.7990735417351,
39.2878045257868));
#202951=CARTESIAN_POINT('Ctrl Pts',(-48.3075724095165,-34.8620346554128,
39.35490152959));
#202952=CARTESIAN_POINT('Origin',(-48.3820909175331,-34.7591950625531,39.3548010137695));
#202953=CARTESIAN_POINT('Ctrl Pts',(-50.5905785208486,-37.1493329797258,
39.8576902534424));
#202954=CARTESIAN_POINT('Ctrl Pts',(-50.6659240749085,-37.046419510825,
39.8573998014387));
#202955=CARTESIAN_POINT('Ctrl Pts',(-50.5784163149359,-36.9828414016744,
39.92499));
#202956=CARTESIAN_POINT('Ctrl Pts',(-50.6273860247248,-37.1760745934426,
39.9304984902492));
#202957=CARTESIAN_POINT('Ctrl Pts',(-50.681017422865,-37.0763471615773,
39.9052171569793));
#202958=CARTESIAN_POINT('Ctrl Pts',(-50.6152221632652,-37.009582415765,
39.9672049726598));
#202959=CARTESIAN_POINT('Ctrl Pts',(-50.6805407410139,-37.1816769644887,
40.0043437678661));
#202960=CARTESIAN_POINT('Ctrl Pts',(-50.7141678268705,-37.0954833955425,
39.9661628577643));
#202961=CARTESIAN_POINT('Ctrl Pts',(-50.6617655220313,-37.024286969575,
40.0100243556235));
#202962=CARTESIAN_POINT('Ctrl Pts',(-50.8012099538927,-37.1386811500609,
40.1194874821989));
#202963=CARTESIAN_POINT('Ctrl Pts',(-50.7999485296224,-37.0803097184694,
40.062755148314));
#202964=CARTESIAN_POINT('Ctrl Pts',(-50.7562647493204,-37.0173098767919,
40.0767884282377));
#202965=CARTESIAN_POINT('Ctrl Pts',(-50.8700180268809,-37.0873787017254,
40.159950201538));
#202966=CARTESIAN_POINT('Ctrl Pts',(-50.8539379904865,-37.0460487315389,
40.100244945386));
#202967=CARTESIAN_POINT('Ctrl Pts',(-50.8047860147144,-36.9939291606747,
40.10025));
#202968=CARTESIAN_POINT('Ctrl Pts',(-50.9219998155902,-37.0158684358557,
40.1599502534424));
#202969=CARTESIAN_POINT('Ctrl Pts',(-50.8918248691002,-36.993933872143,
40.10025));
#202970=CARTESIAN_POINT('Ctrl Pts',(-50.8348823336488,-36.952541597521,
40.10025));
#202971=CARTESIAN_POINT('Origin',(-50.5037675878947,-37.08558655996,39.92499));
#202972=CARTESIAN_POINT('Origin',(-48.2379650606702,-34.6544814981901,39.6398955069326));
#202973=CARTESIAN_POINT('Origin',(-48.093839203715,-34.5497679336938,39.92499));
#202974=CARTESIAN_POINT('Origin',(-50.3596419293373,-36.9808731396128,39.6398955068275));
#202975=CARTESIAN_POINT('Origin',(-50.2155162706046,-36.8761597191952,39.3548010137695));
#202976=CARTESIAN_POINT('Ctrl Pts',(-48.0063682005189,-34.4869303039394,
39.8576902534424));
#202977=CARTESIAN_POINT('Ctrl Pts',(-47.9324532779039,-34.5894948283131,
39.8579948730703));
#202978=CARTESIAN_POINT('Ctrl Pts',(-48.0191904766738,-34.6525130919795,
39.92499));
#202979=CARTESIAN_POINT('Ctrl Pts',(-47.9696093621197,-34.460224101985,
39.9304020711231));
#202980=CARTESIAN_POINT('Ctrl Pts',(-47.9171056031471,-34.559562069433,
39.9058915297378));
#202981=CARTESIAN_POINT('Ctrl Pts',(-47.9824304277179,-34.6258053530815,
39.9671523786028));
#202982=CARTESIAN_POINT('Ctrl Pts',(-47.9167391807674,-34.4546775021463,
40.0043257306692));
#202983=CARTESIAN_POINT('Ctrl Pts',(-47.8838297385504,-34.5405955452482,
39.9667894847832));
#202984=CARTESIAN_POINT('Ctrl Pts',(-47.9361122396534,-34.6112444014587,
40.0100138975199));
#202985=CARTESIAN_POINT('Ctrl Pts',(-47.796856449222,-34.497906166921,40.1195533054858));
#202986=CARTESIAN_POINT('Ctrl Pts',(-47.798338661273,-34.5561175928639,
40.0630813209239));
#202987=CARTESIAN_POINT('Ctrl Pts',(-47.8422046210391,-34.6187227036512,
40.0768265942422));
#202988=CARTESIAN_POINT('Ctrl Pts',(-47.7285944911485,-34.5493265808141,
40.1599502027527));
#202989=CARTESIAN_POINT('Ctrl Pts',(-47.7447672725766,-34.5905382782862,
40.100255279155));
#202990=CARTESIAN_POINT('Ctrl Pts',(-47.7940753146424,-34.6424336528568,
40.10025));
#202991=CARTESIAN_POINT('Ctrl Pts',(-47.6769115920305,-34.6205005703632,
40.1599502534424));
#202992=CARTESIAN_POINT('Ctrl Pts',(-47.7070975168466,-34.6424200234572,
40.10025));
#202993=CARTESIAN_POINT('Ctrl Pts',(-47.7640607692765,-34.6837837831344,
40.10025));
#202994=CARTESIAN_POINT('Origin',(-47.7640607692765,-34.6837837831344,40.22725));
#202995=CARTESIAN_POINT('Ctrl Pts',(-49.8669803696028,-36.6229335645807,
38.989));
#202996=CARTESIAN_POINT('Ctrl Pts',(-49.941740624821,-36.5200349009285,
38.989));
#202997=CARTESIAN_POINT('Ctrl Pts',(-49.9416290134545,-36.5201885207954,
39.1161896013263));
#202998=CARTESIAN_POINT('Ctrl Pts',(-50.0423873219314,-36.7506494346809,
38.989));
#202999=CARTESIAN_POINT('Ctrl Pts',(-50.1174293675647,-36.6476796282247,
38.9887769275478));
#203000=CARTESIAN_POINT('Ctrl Pts',(-50.0820075342382,-36.6221794864698,
39.1161898821845));
#203001=CARTESIAN_POINT('Ctrl Pts',(-50.2093732240197,-36.8722311236853,
39.1034967087243));
#203002=CARTESIAN_POINT('Ctrl Pts',(-50.2846385388084,-36.7691636147926,
39.1031720232704));
#203003=CARTESIAN_POINT('Ctrl Pts',(-50.2156454684932,-36.7192731293496,
39.2077529615001));
#203004=CARTESIAN_POINT('Ctrl Pts',(-50.3023253561997,-36.9399086546484,
39.2875012672119));
#203005=CARTESIAN_POINT('Ctrl Pts',(-50.377787724264,-36.8368401378451,
39.2872087095508));
#203006=CARTESIAN_POINT('Ctrl Pts',(-50.290034551302,-36.7733199617897,
39.3549017048226));
#203007=CARTESIAN_POINT('Origin',(-49.8669803696028,-36.6229335645807,39.116));
#203008=CARTESIAN_POINT('Origin',(3.64514313700082E-16,-3.44778646538029E-17,
40.22725));
#203009=CARTESIAN_POINT('Origin',(-47.7461450747866,-34.7084426211229,40.22725));
#203010=CARTESIAN_POINT('Origin',(40.911747809259,29.3316730956003,39.116));
#203011=CARTESIAN_POINT('Origin',(-49.5422481179709,-36.3870656659258,39.1160373285268));
#203012=CARTESIAN_POINT('Ctrl Pts',(-47.6590285860937,-34.6451144164183,
40.1599502534424));
#203013=CARTESIAN_POINT('Ctrl Pts',(-47.6892031885515,-34.6670494534015,
40.10025));
#203014=CARTESIAN_POINT('Ctrl Pts',(-47.7461450747866,-34.7084426211229,
40.10025));
#203015=CARTESIAN_POINT('Ctrl Pts',(-47.6074854095246,-34.7160192182665,
40.1599500566037));
#203016=CARTESIAN_POINT('Ctrl Pts',(-47.6516492793365,-34.7187044685528,
40.100255130536));
#203017=CARTESIAN_POINT('Ctrl Pts',(-47.7161963245903,-34.7496251732006,
40.10025));
#203018=CARTESIAN_POINT('Ctrl Pts',(-47.5796730526553,-34.7960378560833,
40.1203070619047));
#203019=CARTESIAN_POINT('Ctrl Pts',(-47.6353534770329,-34.7797813814943,
40.0637098684497));
#203020=CARTESIAN_POINT('Ctrl Pts',(-47.7083584310196,-34.8021505789969,
40.0772636213364));
#203021=CARTESIAN_POINT('Ctrl Pts',(-47.5752965616147,-34.9243313177593,
40.0046102245801));
#203022=CARTESIAN_POINT('Ctrl Pts',(-47.6468329724884,-34.8665693571824,
39.9670001894015));
#203023=CARTESIAN_POINT('Ctrl Pts',(-47.7301838844734,-34.8943788354695,
40.0101788811208));
#203024=CARTESIAN_POINT('Ctrl Pts',(-47.5970608435773,-34.9730260802972,
39.9303710930187));
#203025=CARTESIAN_POINT('Ctrl Pts',(-47.675314105656,-34.8923863483126,
39.9058663574112));
#203026=CARTESIAN_POINT('Ctrl Pts',(-47.7584998599245,-34.9340521716866,
39.9671344706364));
#203027=CARTESIAN_POINT('Ctrl Pts',(-47.6338034047601,-34.9997217530258,
39.8576902534424));
#203028=CARTESIAN_POINT('Ctrl Pts',(-47.7085070967805,-34.89773030317,39.8579948730703));
#203029=CARTESIAN_POINT('Ctrl Pts',(-47.7952442955504,-34.9607485668363,
39.92499));
#203030=CARTESIAN_POINT('Origin',(-47.7205955685092,-35.0634937251219,39.92499));
#203031=CARTESIAN_POINT('Origin',(-49.5064990280448,-36.3610285393809,39.1925554488848));
#203032=CARTESIAN_POINT('Origin',(-49.4402904249167,-36.312925173494,39.3343017080178));
#203033=CARTESIAN_POINT('Origin',(-47.8647214254841,-35.1682072895607,39.6398955069214));
#203034=CARTESIAN_POINT('Origin',(-48.0088472823274,-35.2729208539812,39.3548010137695));
#203035=CARTESIAN_POINT('Ctrl Pts',(-49.1733470784089,-36.118979479688,
39.3978017080178));
#203036=CARTESIAN_POINT('Ctrl Pts',(-49.2479958054501,-36.0162343214024,
39.3978017080178));
#203037=CARTESIAN_POINT('Ctrl Pts',(-49.2479958054501,-36.0162343214024,
39.5248017080178));
#203038=CARTESIAN_POINT('Ctrl Pts',(-49.2463047380079,-36.1716968449931,
39.3978017080178));
#203039=CARTESIAN_POINT('Ctrl Pts',(-49.3207474263653,-36.0690914679774,
39.3980355775177));
#203040=CARTESIAN_POINT('Ctrl Pts',(-49.357224477898,-36.0955935972134,
39.5248015517192));
#203041=CARTESIAN_POINT('Ctrl Pts',(-49.3152906263885,-36.2215465627859,
39.3484893995498));
#203042=CARTESIAN_POINT('Ctrl Pts',(-49.3898826892454,-36.1193211766487,
39.348943830343));
#203043=CARTESIAN_POINT('Ctrl Pts',(-49.4605079583576,-36.1706334382077,
39.4508333155595));
#203044=CARTESIAN_POINT('Ctrl Pts',(-49.3516463037387,-36.2478178023248,
39.2708017080178));
#203045=CARTESIAN_POINT('Ctrl Pts',(-49.4263574835553,-36.1458216659123,
39.2710850691867));
#203046=CARTESIAN_POINT('Ctrl Pts',(-49.5149391519579,-36.2101800152084,
39.3343017080178));
#203047=CARTESIAN_POINT('Origin',(-49.1733470784089,-36.118979479688,39.5248017080178));
#203048=CARTESIAN_POINT('Ctrl Pts',(-47.9220530736689,-35.2091516650526,
39.2875012672119));
#203049=CARTESIAN_POINT('Ctrl Pts',(-47.9968680956251,-35.1070032771121,
39.2878045257519));
#203050=CARTESIAN_POINT('Ctrl Pts',(-48.0836260518491,-35.1702703521464,
39.3549015218345));
#203051=CARTESIAN_POINT('Ctrl Pts',(-48.015002557559,-35.2768360036086,
39.1034938540228));
#203052=CARTESIAN_POINT('Ctrl Pts',(-48.0897575808459,-35.1744910995526,
39.1038286278798));
#203053=CARTESIAN_POINT('Ctrl Pts',(-48.1580164790744,-35.2243181613729,
39.2077506434033));
#203054=CARTESIAN_POINT('Ctrl Pts',(-48.181983339224,-35.3984277477545,
38.989));
#203055=CARTESIAN_POINT('Ctrl Pts',(-48.2567629686467,-35.2958269999282,
38.9892298954623));
#203056=CARTESIAN_POINT('Ctrl Pts',(-48.2916555365094,-35.3214126203077,
39.1161900347285));
#203057=CARTESIAN_POINT('Ctrl Pts',(-48.3573835402121,-35.5261472678863,
38.989));
#203058=CARTESIAN_POINT('Ctrl Pts',(-48.4321440857827,-35.4232482045984,
38.989));
#203059=CARTESIAN_POINT('Ctrl Pts',(-48.4320321836305,-35.4234022246976,
39.1161900945642));
#203060=CARTESIAN_POINT('Origin',(-48.3573835402121,-35.5261472678863,39.116));
#203061=CARTESIAN_POINT('Origin',(39.9252688514649,28.6149541797805,39.5248017080178));
#203062=CARTESIAN_POINT('Origin',(-49.0510171431405,-36.0301015792674,39.5248017080178));
#203063=CARTESIAN_POINT('Origin',(39.7707905934409,28.5027191556739,39.116));
#203064=CARTESIAN_POINT('Origin',(-48.6820620414869,-35.7621028045845,39.1160402713842));
#203065=CARTESIAN_POINT('Ctrl Pts',(-48.8727133447945,-35.9012693628902,
39.2708017080178));
#203066=CARTESIAN_POINT('Ctrl Pts',(-48.9481071848799,-35.7983524848933,
39.27051194648));
#203067=CARTESIAN_POINT('Ctrl Pts',(-48.8587224664502,-35.7334106856004,
39.3343017080178));
#203068=CARTESIAN_POINT('Ctrl Pts',(-48.9091935744932,-35.9276271141649,
39.3487519301186));
#203069=CARTESIAN_POINT('Ctrl Pts',(-48.9843245886175,-35.824665968965,
39.3482879464002));
#203070=CARTESIAN_POINT('Ctrl Pts',(-48.9133376106101,-35.7730909105057,
39.4512271261638));
#203071=CARTESIAN_POINT('Ctrl Pts',(-48.978304877513,-35.9775622448352,
39.3978017080178));
#203072=CARTESIAN_POINT('Ctrl Pts',(-49.0530211657568,-35.8745769537837,
39.3975673827364));
#203073=CARTESIAN_POINT('Ctrl Pts',(-49.0168051108907,-35.8482644497259,
39.5248015355181));
#203074=CARTESIAN_POINT('Ctrl Pts',(-49.0510171431405,-36.0301015792674,
39.3978017080178));
#203075=CARTESIAN_POINT('Ctrl Pts',(-49.1256658701817,-35.9273564209818,
39.3978017080178));
#203076=CARTESIAN_POINT('Ctrl Pts',(-49.1256658701817,-35.9273564209818,
39.5248017080178));
#203077=CARTESIAN_POINT('Origin',(-48.7840737394091,-35.836155843886,39.3343017080178));
#203078=CARTESIAN_POINT('Origin',(-48.7182599907933,-35.7883393569604,39.1934008533543));
#203079=CARTESIAN_POINT('Origin',(-53.3535596832587,-30.4370746247561,39.1925554495086));
#203080=CARTESIAN_POINT('Origin',(-53.3918862459828,-30.4591427892365,39.1160373285277));
#203081=CARTESIAN_POINT('Origin',(-53.2826856060847,-30.3961554568834,39.3343017080178));
#203082=CARTESIAN_POINT('Ctrl Pts',(-53.1871522506177,-30.3416565762233,
39.2708017080178));
#203083=CARTESIAN_POINT('Ctrl Pts',(-53.1243619179797,-30.451394201311,
39.2710850691866));
#203084=CARTESIAN_POINT('Ctrl Pts',(-53.2191856060847,-30.506140683164,
39.3343017080178));
#203085=CARTESIAN_POINT('Ctrl Pts',(-53.1482340195362,-30.3190533624374,
39.3487519293518));
#203086=CARTESIAN_POINT('Ctrl Pts',(-53.0851849835388,-30.4287753876648,
39.3492068662924));
#203087=CARTESIAN_POINT('Ctrl Pts',(-53.1607219582406,-30.4723866803434,
39.4512271248735));
#203088=CARTESIAN_POINT('Ctrl Pts',(-53.0745038491603,-30.2762311741509,
39.3978017080178));
#203089=CARTESIAN_POINT('Ctrl Pts',(-53.0110474253452,-30.3859720484844,
39.3980347781178));
#203090=CARTESIAN_POINT('Ctrl Pts',(-53.0499635164576,-30.408440264165,
39.5248015355195));
#203091=CARTESIAN_POINT('Ctrl Pts',(-52.9969317578289,-30.2311753956709,
39.3978017080178));
#203092=CARTESIAN_POINT('Ctrl Pts',(-52.9334317578289,-30.3411606219515,
39.3978017080178));
#203093=CARTESIAN_POINT('Ctrl Pts',(-52.9334317578289,-30.3411606219515,
39.5248017080178));
#203094=CARTESIAN_POINT('Origin',(-52.9969317578289,-30.2311753956709,39.5248017080178));
#203095=CARTESIAN_POINT('Origin',(-0.158749999999993,0.27496306570156,39.116));
#203096=CARTESIAN_POINT('Origin',(-53.7394427993288,-30.6598643453572,39.116));
#203097=CARTESIAN_POINT('Origin',(-0.158749999999993,0.27496306570156,39.5248017080178));
#203098=CARTESIAN_POINT('Origin',(-52.8659816883961,-30.1555713378335,39.5248017080178));
#203099=CARTESIAN_POINT('Ctrl Pts',(-54.2060847114743,-30.9286463962975,
39.2875012672119));
#203100=CARTESIAN_POINT('Ctrl Pts',(-54.1426202518671,-31.0395064328255,
39.287208709576));
#203101=CARTESIAN_POINT('Ctrl Pts',(-54.0488992551384,-30.9851759176836,
39.3549016990122));
#203102=CARTESIAN_POINT('Ctrl Pts',(-54.1064496608377,-30.8712564593355,
39.1034939173931));
#203103=CARTESIAN_POINT('Ctrl Pts',(-54.0429059732646,-30.981936066785,
39.1031692336346));
#203104=CARTESIAN_POINT('Ctrl Pts',(-53.9692670413541,-30.9392002377687,
39.2077507202299));
#203105=CARTESIAN_POINT('Ctrl Pts',(-53.9274585619034,-30.7681581606525,
38.989));
#203106=CARTESIAN_POINT('Ctrl Pts',(-53.8639133132304,-30.8785940576174,
38.9887769311158));
#203107=CARTESIAN_POINT('Ctrl Pts',(-53.8262110069737,-30.8566067980797,
39.1161898712914));
#203108=CARTESIAN_POINT('Ctrl Pts',(-53.7394427993288,-30.6598643453572,
38.989));
#203109=CARTESIAN_POINT('Ctrl Pts',(-53.6758479332735,-30.7700138844655,
38.989));
#203110=CARTESIAN_POINT('Ctrl Pts',(-53.6759428700858,-30.7698494490832,
39.1161895903853));
#203111=CARTESIAN_POINT('Origin',(-54.1125387249981,-30.8752713784759,39.3548010137695));
#203112=CARTESIAN_POINT('Ctrl Pts',(-52.8659816883961,-30.1555713378335,
39.3978017080178));
#203113=CARTESIAN_POINT('Ctrl Pts',(-52.8024816883961,-30.2655565641141,
39.3978017080178));
#203114=CARTESIAN_POINT('Ctrl Pts',(-52.8024816883961,-30.2655565641141,
39.5248017080178));
#203115=CARTESIAN_POINT('Ctrl Pts',(-52.7881477055078,-30.1103627734741,
39.3978017080178));
#203116=CARTESIAN_POINT('Ctrl Pts',(-52.7244553345201,-30.2205080277005,
39.3975666025026));
#203117=CARTESIAN_POINT('Ctrl Pts',(-52.6855560684216,-30.1980495259467,
39.5248015517178));
#203118=CARTESIAN_POINT('Ctrl Pts',(-52.7145506960112,-30.0676130472589,
39.3484894016717));
#203119=CARTESIAN_POINT('Ctrl Pts',(-52.651050001129,-30.1781274387059,
39.3480259000041));
#203120=CARTESIAN_POINT('Ctrl Pts',(-52.5749945583575,-30.1342168083492,
39.4508333188947));
#203121=CARTESIAN_POINT('Ctrl Pts',(-52.6757649139397,-30.0450834959833,
39.2708017080178));
#203122=CARTESIAN_POINT('Ctrl Pts',(-52.6124111049558,-30.1558192615998,
39.27051194648));
#203123=CARTESIAN_POINT('Ctrl Pts',(-52.5167277788843,-30.1005764675355,
39.3343017080178));
#203124=CARTESIAN_POINT('Origin',(-52.5802277788843,-29.9905912412549,39.3343017080178));
#203125=CARTESIAN_POINT('Origin',(-54.2668203812025,-30.9643459342458,39.6398955068168));
#203126=CARTESIAN_POINT('Origin',(-54.421102037244,-31.0534204898631,39.92499));
#203127=CARTESIAN_POINT('Origin',(-52.5097763801588,-29.949916107243,39.1934008539947));
#203128=CARTESIAN_POINT('Origin',(-52.4710850656385,-29.927519002606,39.1160402713848));
#203129=CARTESIAN_POINT('Ctrl Pts',(-54.5275217339721,-31.4638515574737,
40.1599502534424));
#203130=CARTESIAN_POINT('Ctrl Pts',(-54.4952102564867,-31.445206962985,
40.10025));
#203131=CARTESIAN_POINT('Ctrl Pts',(-54.4342359163065,-31.4100231232058,
40.10025));
#203132=CARTESIAN_POINT('Ctrl Pts',(-54.5715608148707,-31.3875306471678,
40.1599500538458));
#203133=CARTESIAN_POINT('Ctrl Pts',(-54.5272862282506,-31.3896121658898,
40.100244835349));
#203134=CARTESIAN_POINT('Ctrl Pts',(-54.4597196360178,-31.3658411130326,
40.10025));
#203135=CARTESIAN_POINT('Ctrl Pts',(-54.5905300051367,-31.3046029601553,
40.1202442001039));
#203136=CARTESIAN_POINT('Ctrl Pts',(-54.5367961153118,-31.3268524737455,
40.0633873868018));
#203137=CARTESIAN_POINT('Ctrl Pts',(-54.4615686025424,-31.312567293429,
40.0772271723537));
#203138=CARTESIAN_POINT('Ctrl Pts',(-54.5809273110395,-31.1759014746041,
40.0045995998163));
#203139=CARTESIAN_POINT('Ctrl Pts',(-54.5158579940067,-31.2415992967182,
39.9663485808315));
#203140=CARTESIAN_POINT('Ctrl Pts',(-54.4295063924929,-31.2227682191857,
40.0101727202466));
#203141=CARTESIAN_POINT('Ctrl Pts',(-54.5540292360078,-31.1295364123889,
39.9304654349859));
#203142=CARTESIAN_POINT('Ctrl Pts',(-54.4847364330945,-31.2191033458793,
39.9051900162955));
#203143=CARTESIAN_POINT('Ctrl Pts',(-54.3969835118368,-31.1861426211009,
39.9671857458175));
#203144=CARTESIAN_POINT('Ctrl Pts',(-54.514646476914,-31.1067982185532,
39.8576902534424));
#203145=CARTESIAN_POINT('Ctrl Pts',(-54.4512761425984,-31.2174884860862,
39.8573998014387));
#203146=CARTESIAN_POINT('Ctrl Pts',(-54.357602037244,-31.1634057161437,
39.92499));
#203147=CARTESIAN_POINT('Origin',(-54.4342359163065,-31.4100231232058,40.22725));
#203148=CARTESIAN_POINT('Origin',(-0.158749999999993,0.27496306570156,39.116));
#203149=CARTESIAN_POINT('Origin',(-52.1234703131948,-29.7268821954847,39.116));
#203150=CARTESIAN_POINT('Origin',(1.12590909550281E-16,8.2444796405856E-17,
40.22725));
#203151=CARTESIAN_POINT('Origin',(-54.4189959163065,-31.4364195775132,40.22725));
#203152=CARTESIAN_POINT('Ctrl Pts',(-52.1234703131948,-29.7268821954847,
38.989));
#203153=CARTESIAN_POINT('Ctrl Pts',(-52.0598751873274,-29.8370321846007,
38.989));
#203154=CARTESIAN_POINT('Ctrl Pts',(-52.0599703843396,-29.8368672985389,
39.1161901092321));
#203155=CARTESIAN_POINT('Ctrl Pts',(-51.9354481180167,-29.6185926664424,
38.989));
#203156=CARTESIAN_POINT('Ctrl Pts',(-51.872133287597,-29.72863875449,38.9892298989754));
#203157=CARTESIAN_POINT('Ctrl Pts',(-51.909699589874,-29.7501084151998,
39.1161900493201));
#203158=CARTESIAN_POINT('Ctrl Pts',(-51.7564527430629,-29.5155047636231,
39.1034966344368));
#203159=CARTESIAN_POINT('Ctrl Pts',(-51.6933616226679,-29.6254243098839,
39.1038314102575));
#203160=CARTESIAN_POINT('Ctrl Pts',(-51.7666446199949,-29.6675155901168,
39.2077528789601));
#203161=CARTESIAN_POINT('Ctrl Pts',(-51.6568155675429,-29.4581217525671,
39.2875012672119));
#203162=CARTESIAN_POINT('Ctrl Pts',(-51.5939283753697,-29.5680161811087,
39.2878045257868));
#203163=CARTESIAN_POINT('Ctrl Pts',(-51.6870133822662,-29.6215404737378,
39.3549015295899));
#203164=CARTESIAN_POINT('Origin',(-51.7503740054945,-29.5114749418002,39.3548010137695));
#203165=CARTESIAN_POINT('Ctrl Pts',(-54.1966007261209,-31.6576696180581,
39.8576902534424));
#203166=CARTESIAN_POINT('Ctrl Pts',(-54.2607761425984,-31.5474441649281,
39.8573998014387));
#203167=CARTESIAN_POINT('Ctrl Pts',(-54.167102037244,-31.4933613949856,
39.92499));
#203168=CARTESIAN_POINT('Ctrl Pts',(-54.2360018544267,-31.6804173066003,
39.9304984902492));
#203169=CARTESIAN_POINT('Ctrl Pts',(-54.2789150989584,-31.5756301844103,
39.9052171569797));
#203170=CARTESIAN_POINT('Ctrl Pts',(-54.2065014563939,-31.5161086602377,
39.9672049726601));
#203171=CARTESIAN_POINT('Ctrl Pts',(-54.2894509908545,-31.6804328064622,
40.0043437678661));
#203172=CARTESIAN_POINT('Ctrl Pts',(-54.3138841827106,-31.5911964272959,
39.9661628577643));
#203173=CARTESIAN_POINT('Ctrl Pts',(-54.2543268901841,-31.5258675551963,
40.0100243556237));
#203174=CARTESIAN_POINT('Ctrl Pts',(-54.4049648787501,-31.6250591602187,
40.1194874821989));
#203175=CARTESIAN_POINT('Ctrl Pts',(-54.3976088886511,-31.5671393481781,
40.062755148314));
#203176=CARTESIAN_POINT('Ctrl Pts',(-54.3475791360314,-31.5090508246492,
40.0767884282375));
#203177=CARTESIAN_POINT('Ctrl Pts',(-54.4680334478296,-31.5668453499336,
40.1599502015396));
#203178=CARTESIAN_POINT('Ctrl Pts',(-54.4477213412895,-31.5274226111431,
40.1002449453875));
#203179=CARTESIAN_POINT('Ctrl Pts',(-54.393390646534,-31.4807263372353,
40.10025));
#203180=CARTESIAN_POINT('Ctrl Pts',(-54.5122556166612,-31.4902932482905,
40.1599502534424));
#203181=CARTESIAN_POINT('Ctrl Pts',(-54.4799531854481,-31.4716329851986,
40.10025));
#203182=CARTESIAN_POINT('Ctrl Pts',(-54.4189959163065,-31.4364195775132,
40.10025));
#203183=CARTESIAN_POINT('Origin',(-54.103602037244,-31.6033466212662,39.92499));
#203184=CARTESIAN_POINT('Origin',(-51.5960921371862,-29.4224002636365,39.6398955069316));
#203185=CARTESIAN_POINT('Origin',(-51.4418102687787,-29.3333255853452,39.92499));
#203186=CARTESIAN_POINT('Origin',(-53.9493203812131,-31.5142720655985,39.6398955068269));
#203187=CARTESIAN_POINT('Origin',(-53.7950387249981,-31.425197509879,39.3548010137695));
#203188=CARTESIAN_POINT('Ctrl Pts',(-51.3482501200167,-29.2799753962459,
39.8576902534424));
#203189=CARTESIAN_POINT('Ctrl Pts',(-51.2854610232003,-29.3897042746971,
39.8579948730703));
#203190=CARTESIAN_POINT('Ctrl Pts',(-51.3783102687786,-29.4433108116258,
39.92499));
#203191=CARTESIAN_POINT('Ctrl Pts',(-51.3089010921303,-29.25725783855,39.9304020711229));
#203192=CARTESIAN_POINT('Ctrl Pts',(-51.2670685993226,-29.3615397594614,
39.9058915297381));
#203193=CARTESIAN_POINT('Ctrl Pts',(-51.3389598763138,-29.4205918519435,
39.9671523786034));
#203194=CARTESIAN_POINT('Ctrl Pts',(-51.2557407616057,-29.2572680623747,
40.0043257306695));
#203195=CARTESIAN_POINT('Ctrl Pts',(-51.231992481769,-29.3461554108685,
39.9667894847835));
#203196=CARTESIAN_POINT('Ctrl Pts',(-51.2913733902316,-29.4109522357565,
40.0100138975202));
#203197=CARTESIAN_POINT('Ctrl Pts',(-51.1410333861058,-29.3127910737011,
40.1195533054855));
#203198=CARTESIAN_POINT('Ctrl Pts',(-51.1485922293426,-29.3705286780142,
40.0630813209236));
#203199=CARTESIAN_POINT('Ctrl Pts',(-51.1987619028147,-29.4282055900899,
40.0768265942419));
#203200=CARTESIAN_POINT('Ctrl Pts',(-51.0785202710257,-29.3710651187643,
40.1599502027521));
#203201=CARTESIAN_POINT('Ctrl Pts',(-51.0989122516715,-29.4103605382566,
40.1002552791547));
#203202=CARTESIAN_POINT('Ctrl Pts',(-51.1533747228767,-29.4568175306708,
40.10025));
#203203=CARTESIAN_POINT('Ctrl Pts',(-51.0345602039888,-29.4472515437732,
40.1599502534424));
#203204=CARTESIAN_POINT('Ctrl Pts',(-51.0668719738979,-29.4658956314764,
40.10025));
#203205=CARTESIAN_POINT('Ctrl Pts',(-51.1278468659049,-29.5010785149108,
40.10025));
#203206=CARTESIAN_POINT('Origin',(-51.1278468659049,-29.5010785149108,40.22725));
#203207=CARTESIAN_POINT('Ctrl Pts',(-53.4219427993288,-31.2097904767603,
38.989));
#203208=CARTESIAN_POINT('Ctrl Pts',(-53.4855376708629,-31.0996409281624,
38.989));
#203209=CARTESIAN_POINT('Ctrl Pts',(-53.4854427285637,-31.0998053730485,
39.1161896013265));
#203210=CARTESIAN_POINT('Ctrl Pts',(-53.6097387976566,-31.3184716867864,
38.989));
#203211=CARTESIAN_POINT('Ctrl Pts',(-53.673606479479,-31.2082219299921,
38.9887769275485));
#203212=CARTESIAN_POINT('Ctrl Pts',(-53.6357132000306,-31.1865640704875,
39.1161898821847));
#203213=CARTESIAN_POINT('Ctrl Pts',(-53.7885186806131,-31.4219325588467,
39.1034967087243));
#203214=CARTESIAN_POINT('Ctrl Pts',(-53.8525981958179,-31.3115622968592,
39.1031720232692));
#203215=CARTESIAN_POINT('Ctrl Pts',(-53.7787681009845,-31.2691568563318,
39.2077529614999));
#203216=CARTESIAN_POINT('Ctrl Pts',(-53.8880358395972,-31.4795232016787,
39.2875012672119));
#203217=CARTESIAN_POINT('Ctrl Pts',(-53.9523112232408,-31.3691313396262,
39.2872087095508));
#203218=CARTESIAN_POINT('Ctrl Pts',(-53.8583991049523,-31.3151318380581,
39.3549017048227));
#203219=CARTESIAN_POINT('Origin',(-53.4219427993288,-31.2097904767603,39.116));
#203220=CARTESIAN_POINT('Origin',(3.61170357355341E-16,-2.93286234380096E-17,
40.22725));
#203221=CARTESIAN_POINT('Origin',(-51.1126068659049,-29.5274749692182,40.22725));
#203222=CARTESIAN_POINT('Origin',(46.8255917980726,26.668150608645,39.116));
#203223=CARTESIAN_POINT('Origin',(-53.0743345559669,-31.0091584503666,39.1160373285225));
#203224=CARTESIAN_POINT('Ctrl Pts',(-51.0193480105329,-29.4735998357335,
40.1599502534424));
#203225=CARTESIAN_POINT('Ctrl Pts',(-51.0516501490688,-29.4922606054643,
40.10025));
#203226=CARTESIAN_POINT('Ctrl Pts',(-51.1126068659049,-29.5274749692182,
40.10025));
#203227=CARTESIAN_POINT('Ctrl Pts',(-50.9754987628538,-29.5495039426968,
40.1599500566034));
#203228=CARTESIAN_POINT('Ctrl Pts',(-51.0197013834521,-29.5475581014576,
40.1002551305372));
#203229=CARTESIAN_POINT('Ctrl Pts',(-51.0871269269763,-29.5715624158004,
40.10025));
#203230=CARTESIAN_POINT('Ctrl Pts',(-50.9562029902289,-29.6319914129669,
40.1203070619047));
#203231=CARTESIAN_POINT('Ctrl Pts',(-51.0098791271085,-29.6100038038525,
40.0637098684499));
#203232=CARTESIAN_POINT('Ctrl Pts',(-51.0848223701588,-29.6246193648993,
40.0772636213362));
#203233=CARTESIAN_POINT('Ctrl Pts',(-50.9652607924606,-29.7600395375188,
40.0046102245802));
#203234=CARTESIAN_POINT('Ctrl Pts',(-51.0303675504166,-29.6951164119093,
39.9670001894012));
#203235=CARTESIAN_POINT('Ctrl Pts',(-51.1161687394136,-29.7140610042229,
40.010178881121));
#203236=CARTESIAN_POINT('Ctrl Pts',(-50.9919958361064,-29.8061925581054,
39.9303710930186));
#203237=CARTESIAN_POINT('Ctrl Pts',(-51.061391271364,-29.71781488578,39.905866357411));
#203238=CARTESIAN_POINT('Ctrl Pts',(-51.1484765898559,-29.7505571803534,
39.967134470636));
#203239=CARTESIAN_POINT('Ctrl Pts',(-51.031327575341,-29.8289013456883,
39.8576902534424));
#203240=CARTESIAN_POINT('Ctrl Pts',(-51.0949610232003,-29.719659953539,
39.8579948730703));
#203241=CARTESIAN_POINT('Ctrl Pts',(-51.1878102687787,-29.7732664904677,
39.92499));
#203242=CARTESIAN_POINT('Origin',(-51.1243102687787,-29.8832517167483,39.92499));
#203243=CARTESIAN_POINT('Origin',(-53.0360596824723,-30.9870007553603,39.1925554488847));
#203244=CARTESIAN_POINT('Origin',(-52.9651856060848,-30.9460815882865,39.3343017080178));
#203245=CARTESIAN_POINT('Origin',(-51.2785921372023,-29.9723263949832,39.6398955069226));
#203246=CARTESIAN_POINT('Origin',(-51.4328740054945,-30.0614010732033,39.3548010137695));
#203247=CARTESIAN_POINT('Ctrl Pts',(-52.6794317578289,-30.781101527074,
39.3978017080178));
#203248=CARTESIAN_POINT('Ctrl Pts',(-52.7429317578289,-30.6711163007934,
39.3978017080178));
#203249=CARTESIAN_POINT('Ctrl Pts',(-52.7429317578289,-30.6711163007934,
39.5248017080178));
#203250=CARTESIAN_POINT('Ctrl Pts',(-52.7575002129172,-30.8259039490956,
39.3978017080178));
#203251=CARTESIAN_POINT('Ctrl Pts',(-52.820809914056,-30.7160792752574,
39.3980355775177));
#203252=CARTESIAN_POINT('Ctrl Pts',(-52.8598573673265,-30.738623332912,
39.5248015517192));
#203253=CARTESIAN_POINT('Ctrl Pts',(-52.8313189037791,-30.8682695960175,
39.3484893995498));
#203254=CARTESIAN_POINT('Ctrl Pts',(-52.8948168809914,-30.7588072175368,
39.3489438303428));
#203255=CARTESIAN_POINT('Ctrl Pts',(-52.9704188493375,-30.8024560343131,
39.4508333155596));
#203256=CARTESIAN_POINT('Ctrl Pts',(-52.8702215132218,-30.8905967158733,
39.2708017080178));
#203257=CARTESIAN_POINT('Ctrl Pts',(-52.9338619179797,-30.7813498801529,
39.2710850691866));
#203258=CARTESIAN_POINT('Ctrl Pts',(-53.0286856060847,-30.8360963620059,
39.3343017080178));
#203259=CARTESIAN_POINT('Origin',(-52.6794317578289,-30.781101527074,39.5248017080178));
#203260=CARTESIAN_POINT('Ctrl Pts',(-51.3398895692699,-30.0070536838155,
39.2875012672119));
#203261=CARTESIAN_POINT('Ctrl Pts',(-51.4036173326911,-29.8976445761577,
39.2878045257519));
#203262=CARTESIAN_POINT('Ctrl Pts',(-51.496513229882,-29.9514963916949,
39.3549015218345));
#203263=CARTESIAN_POINT('Ctrl Pts',(-51.4394048060578,-30.0646513737712,
39.1034938540228));
#203264=CARTESIAN_POINT('Ctrl Pts',(-51.5030523579637,-29.9550530981071,
39.1038286278806));
#203265=CARTESIAN_POINT('Ctrl Pts',(-51.576145673005,-29.9974722043277,
39.2077506434033));
#203266=CARTESIAN_POINT('Ctrl Pts',(-51.6181806476914,-30.168122781117,
38.989));
#203267=CARTESIAN_POINT('Ctrl Pts',(-51.6818259279747,-30.0582674911768,
38.989229895463));
#203268=CARTESIAN_POINT('Ctrl Pts',(-51.7192017762845,-30.0800656843509,
39.1161900347285));
#203269=CARTESIAN_POINT('Ctrl Pts',(-51.8059703131948,-30.2768083268878,
38.989));
#203270=CARTESIAN_POINT('Ctrl Pts',(-51.8695654317172,-30.1666583504936,
38.989));
#203271=CARTESIAN_POINT('Ctrl Pts',(-51.869470242061,-30.1668232238145,
39.1161900945642));
#203272=CARTESIAN_POINT('Origin',(-51.8059703131948,-30.2768083268878,39.116));
#203273=CARTESIAN_POINT('Origin',(45.6951875000003,26.0155113828598,39.5248017080178));
#203274=CARTESIAN_POINT('Origin',(-52.5484816883961,-30.7054974692366,39.5248017080178));
#203275=CARTESIAN_POINT('Origin',(45.5181711678734,25.9133109558554,39.116));
#203276=CARTESIAN_POINT('Origin',(-52.1535342613174,-30.4775331296738,39.1160402713853));
#203277=CARTESIAN_POINT('Ctrl Pts',(-52.3576880233164,-30.5960088312565,
39.2708017080178));
#203278=CARTESIAN_POINT('Ctrl Pts',(-52.4219111049558,-30.4857749404417,
39.2705119464801));
#203279=CARTESIAN_POINT('Ctrl Pts',(-52.3262277788843,-30.4305321463774,
39.3343017080178));
#203280=CARTESIAN_POINT('Ctrl Pts',(-52.3967235457367,-30.6184089696602,
39.3487519301186));
#203281=CARTESIAN_POINT('Ctrl Pts',(-52.4606806140216,-30.5081585269385,
39.3482879463983));
#203282=CARTESIAN_POINT('Ctrl Pts',(-52.3846914485048,-30.4642861617706,
39.4512271261628));
#203283=CARTESIAN_POINT('Ctrl Pts',(-52.4706758922785,-30.6608464521622,
39.3978017080178));
#203284=CARTESIAN_POINT('Ctrl Pts',(-52.5342179826636,-30.5506153465186,
39.3975673827383));
#203285=CARTESIAN_POINT('Ctrl Pts',(-52.49544991752,-30.5282325936716,39.5248015355181));
#203286=CARTESIAN_POINT('Ctrl Pts',(-52.5484816883961,-30.7054974692366,
39.3978017080178));
#203287=CARTESIAN_POINT('Ctrl Pts',(-52.6119816883961,-30.595512242956,
39.3978017080178));
#203288=CARTESIAN_POINT('Ctrl Pts',(-52.6119816883961,-30.595512242956,
39.5248017080178));
#203289=CARTESIAN_POINT('Origin',(-52.2627277788843,-30.540517372658,39.3343017080178));
#203290=CARTESIAN_POINT('Origin',(-52.1922763809707,-30.499842239456,39.193400853355));
#203291=CARTESIAN_POINT('Origin',(-56.242823937725,-24.6933715417292,39.1925554495076));
#203292=CARTESIAN_POINT('Origin',(-56.2832472948486,-24.7113125977911,39.1160373285244));
#203293=CARTESIAN_POINT('Origin',(-56.1680608984279,-24.6600848917108,39.3343017080178));
#203294=CARTESIAN_POINT('Ctrl Pts',(-56.0673542004327,-24.6158705164591,
39.2708017080178));
#203295=CARTESIAN_POINT('Ctrl Pts',(-56.0163785451199,-24.7315703643332,
39.2710850691866));
#203296=CARTESIAN_POINT('Ctrl Pts',(-56.1164053447573,-24.7761051648314,
39.3343017080178));
#203297=CARTESIAN_POINT('Ctrl Pts',(-56.0262864882905,-24.5974591883331,
39.3487519293518));
#203298=CARTESIAN_POINT('Ctrl Pts',(-55.9750519161917,-24.7131705636681,
39.349206866292));
#203299=CARTESIAN_POINT('Ctrl Pts',(-56.0547337128487,-24.7486471852359,
39.4512271248737));
#203300=CARTESIAN_POINT('Ctrl Pts',(-55.9484840819671,-24.5625784858803,
39.3978017080178));
#203301=CARTESIAN_POINT('Ctrl Pts',(-55.8968463240338,-24.6783511906885,
39.3980347781178));
#203302=CARTESIAN_POINT('Ctrl Pts',(-55.937897796785,-24.6966284839301,
39.524801535519));
#203303=CARTESIAN_POINT('Ctrl Pts',(-55.8666273273834,-24.5258780191668,
39.3978017080178));
#203304=CARTESIAN_POINT('Ctrl Pts',(-55.8149717737128,-24.6418982922874,
39.3978017080178));
#203305=CARTESIAN_POINT('Ctrl Pts',(-55.8149717737128,-24.6418982922874,
39.5248017080178));
#203306=CARTESIAN_POINT('Origin',(-55.8666273273834,-24.5258780191668,39.5248017080178));
#203307=CARTESIAN_POINT('Origin',(-0.129138884176559,0.290050682801527,
39.116));
#203308=CARTESIAN_POINT('Origin',(-56.6498810128383,-24.8746050278049,39.116));
#203309=CARTESIAN_POINT('Origin',(-0.129138884176559,0.290050682801527,
39.5248017080178));
#203310=CARTESIAN_POINT('Origin',(-55.7284918401499,-24.4643761377914,39.5248017080178));
#203311=CARTESIAN_POINT('Ctrl Pts',(-57.1420619865023,-25.0931373005742,
39.2875012672119));
#203312=CARTESIAN_POINT('Ctrl Pts',(-57.0905332211012,-25.2100238766575,
39.287208709576));
#203313=CARTESIAN_POINT('Ctrl Pts',(-56.9916465525425,-25.1657875015262,
39.3549016990122));
#203314=CARTESIAN_POINT('Ctrl Pts',(-57.0369738651806,-25.0464764504217,
39.1034939173931));
#203315=CARTESIAN_POINT('Ctrl Pts',(-56.9853474458546,-25.1631918674178,
39.1031692336355));
#203316=CARTESIAN_POINT('Ctrl Pts',(-56.9076448051892,-25.1283875141303,
39.2077507202296));
#203317=CARTESIAN_POINT('Ctrl Pts',(-56.8481865914866,-24.9626525995185,
38.989));
#203318=CARTESIAN_POINT('Ctrl Pts',(-56.7965331449355,-25.0791258042767,
38.9887769311152));
#203319=CARTESIAN_POINT('Ctrl Pts',(-56.7567390814047,-25.06119995738,39.1161898712914));
#203320=CARTESIAN_POINT('Ctrl Pts',(-56.6498810128383,-24.8746050278049,
38.989));
#203321=CARTESIAN_POINT('Ctrl Pts',(-56.5981482881659,-24.9907986298333,
38.989));
#203322=CARTESIAN_POINT('Ctrl Pts',(-56.5982255167266,-24.9906251716462,
39.1161895903852));
#203323=CARTESIAN_POINT('Origin',(-57.043449246138,-25.0498328948962,39.3548010137695));
#203324=CARTESIAN_POINT('Ctrl Pts',(-55.7284918401499,-24.4643761377914,
39.3978017080178));
#203325=CARTESIAN_POINT('Ctrl Pts',(-55.6768362864793,-24.580396410912,
39.3978017080178));
#203326=CARTESIAN_POINT('Ctrl Pts',(-55.6768362864793,-24.580396410912,
39.5248017080178));
#203327=CARTESIAN_POINT('Ctrl Pts',(-55.6463586582056,-24.4275510972974,
39.3978017080178));
#203328=CARTESIAN_POINT('Ctrl Pts',(-55.5945285148507,-24.5437506299579,
39.397566602504));
#203329=CARTESIAN_POINT('Ctrl Pts',(-55.5534947903273,-24.5254812387363,
39.5248015517196));
#203330=CARTESIAN_POINT('Ctrl Pts',(-55.5686962576408,-24.39272854086,39.3484894016716));
#203331=CARTESIAN_POINT('Ctrl Pts',(-55.517095325717,-24.5092751529583,
39.3480259000031));
#203332=CARTESIAN_POINT('Ctrl Pts',(-55.4368666119034,-24.4735550281866,
39.4508333188939));
#203333=CARTESIAN_POINT('Ctrl Pts',(-55.5277679687684,-24.3743766270211,
39.2708017080178));
#203334=CARTESIAN_POINT('Ctrl Pts',(-55.4763362579876,-24.4911280468223,
39.27051194648));
#203335=CARTESIAN_POINT('Ctrl Pts',(-55.3754026508176,-24.4461895095986,
39.3343017080178));
#203336=CARTESIAN_POINT('Origin',(-55.4270582044882,-24.330169236478,39.3343017080178));
#203337=CARTESIAN_POINT('Origin',(-57.206196557715,-25.1222926664907,39.6398955068199));
#203338=CARTESIAN_POINT('Origin',(-57.3689438691197,-25.1947524379613,39.92499));
#203339=CARTESIAN_POINT('Origin',(-55.3527410366459,-24.2970811015516,39.1934008539938));
#203340=CARTESIAN_POINT('Origin',(-55.3119205422647,-24.2788510342449,39.1160402713843));
#203341=CARTESIAN_POINT('Ctrl Pts',(-57.517682316389,-25.5918112338791,
40.1599502534424));
#203342=CARTESIAN_POINT('Ctrl Pts',(-57.4835989537479,-25.5766462455173,
40.10025));
#203343=CARTESIAN_POINT('Ctrl Pts',(-57.419280924679,-25.5480287005715,
40.10025));
#203344=CARTESIAN_POINT('Ctrl Pts',(-57.553502439126,-25.5113050800555,
40.1599500538472));
#203345=CARTESIAN_POINT('Ctrl Pts',(-57.5096879712806,-25.5180031505023,
40.1002448353506));
#203346=CARTESIAN_POINT('Ctrl Pts',(-57.4400067642827,-25.5014249500142,
40.10025));
#203347=CARTESIAN_POINT('Ctrl Pts',(-57.5636994104963,-25.4268488592816,
40.1202442001041));
#203348=CARTESIAN_POINT('Ctrl Pts',(-57.5125855880052,-25.4545932086374,
40.0633873868015));
#203349=CARTESIAN_POINT('Ctrl Pts',(-57.4362769714769,-25.4482497003382,
40.0772271723539));
#203350=CARTESIAN_POINT('Ctrl Pts',(-57.5406963524571,-25.2998561687909,
40.004599599816));
#203351=CARTESIAN_POINT('Ctrl Pts',(-57.4828507843379,-25.3719956870764,
39.9663485808318));
#203352=CARTESIAN_POINT('Ctrl Pts',(-57.395003842335,-25.3622939683644,
40.0101727202465));
#203353=CARTESIAN_POINT('Ctrl Pts',(-57.5090991591924,-25.2565567136861,
39.9304654349861));
#203354=CARTESIAN_POINT('Ctrl Pts',(-57.4495482434214,-25.3528760603493,
39.9051900162944));
#203355=CARTESIAN_POINT('Ctrl Pts',(-57.3588307079386,-25.3292685758746,
39.9671857458173));
#203356=CARTESIAN_POINT('Ctrl Pts',(-57.4675553545142,-25.2380597013427,
39.8576902534424));
#203357=CARTESIAN_POINT('Ctrl Pts',(-57.4161024530845,-25.3547675996712,
39.8573998014387));
#203358=CARTESIAN_POINT('Ctrl Pts',(-57.3172883154491,-25.3107727110819,
39.92499));
#203359=CARTESIAN_POINT('Origin',(-57.419280924679,-25.5480287005715,40.22725));
#203360=CARTESIAN_POINT('Origin',(-0.129138884176559,0.290050682801527,
39.116));
#203361=CARTESIAN_POINT('Origin',(-54.945237802683,-24.1156489724274,39.116));
#203362=CARTESIAN_POINT('Origin',(1.20426471881346E-16,6.70666394583711E-17,
40.22725));
#203363=CARTESIAN_POINT('Origin',(-57.4068835917981,-25.5758735661205,40.22725));
#203364=CARTESIAN_POINT('Ctrl Pts',(-54.945237802683,-24.1156489724274,
38.989));
#203365=CARTESIAN_POINT('Ctrl Pts',(-54.8935048666604,-24.2318430491562,
38.989));
#203366=CARTESIAN_POINT('Ctrl Pts',(-54.8935823068867,-24.23166911556,39.1161901092322));
#203367=CARTESIAN_POINT('Ctrl Pts',(-54.746926274704,-24.027606335879,38.989));
#203368=CARTESIAN_POINT('Ctrl Pts',(-54.6954612380238,-24.1436677818706,
38.9892298989736));
#203369=CARTESIAN_POINT('Ctrl Pts',(-54.7350659388068,-24.1610930816813,
39.1161900493202));
#203370=CARTESIAN_POINT('Ctrl Pts',(-54.5581358350805,-23.9437932708512,
39.1034966344368));
#203371=CARTESIAN_POINT('Ctrl Pts',(-54.5068800556949,-24.0597054841957,
39.1038314102579));
#203372=CARTESIAN_POINT('Ctrl Pts',(-54.5841613379365,-24.0939060248996,
39.20775287896));
#203373=CARTESIAN_POINT('Ctrl Pts',(-54.4530463244694,-23.8971395307765,
39.2875012672119));
#203374=CARTESIAN_POINT('Ctrl Pts',(-54.401990730652,-24.0130054476974,
39.2878045257868));
#203375=CARTESIAN_POINT('Ctrl Pts',(-54.5001606201971,-24.0565064959268,
39.3549015295899));
#203376=CARTESIAN_POINT('Origin',(-54.5516691663896,-23.9404209259118,39.3548010137695));
#203377=CARTESIAN_POINT('Ctrl Pts',(-57.20883363247,-25.8191582032617,39.8576902534424));
#203378=CARTESIAN_POINT('Ctrl Pts',(-57.2611357920726,-25.702828419033,
39.8573998014387));
#203379=CARTESIAN_POINT('Ctrl Pts',(-57.1623216544372,-25.6588335304438,
39.92499));
#203380=CARTESIAN_POINT('Ctrl Pts',(-57.2503966981984,-25.8376627381934,
39.9304984902492));
#203381=CARTESIAN_POINT('Ctrl Pts',(-57.2821216226325,-25.7289639953181,
39.9052171569799));
#203382=CARTESIAN_POINT('Ctrl Pts',(-57.2038829761264,-25.6773378230591,
39.9672049726609));
#203383=CARTESIAN_POINT('Ctrl Pts',(-57.3035546548412,-25.8320911970516,
40.0043437678661));
#203384=CARTESIAN_POINT('Ctrl Pts',(-57.3185262575343,-25.74078970011,39.9661628577643));
#203385=CARTESIAN_POINT('Ctrl Pts',(-57.2524664994798,-25.6820441386712,
40.0100243556236));
#203386=CARTESIAN_POINT('Ctrl Pts',(-57.4126476234253,-25.7649464042479,
40.1194874821989));
#203387=CARTESIAN_POINT('Ctrl Pts',(-57.3992776612641,-25.7081127933386,
40.062755148314));
#203388=CARTESIAN_POINT('Ctrl Pts',(-57.3434500727664,-25.6555720179788,
40.0767884282377));
#203389=CARTESIAN_POINT('Ctrl Pts',(-57.4692856961541,-25.7004590347005,
40.1599502015396));
#203390=CARTESIAN_POINT('Ctrl Pts',(-57.4449640631542,-25.6633754510798,
40.1002449453872));
#203391=CARTESIAN_POINT('Ctrl Pts',(-57.3860499078785,-25.6226140882779,
40.10025));
#203392=CARTESIAN_POINT('Ctrl Pts',(-57.5052637377733,-25.6197038181295,
40.1599502534424));
#203393=CARTESIAN_POINT('Ctrl Pts',(-57.471187734033,-25.6045223014058,
40.10025));
#203394=CARTESIAN_POINT('Ctrl Pts',(-57.4068835917981,-25.5758735661205,
40.10025));
#203395=CARTESIAN_POINT('Origin',(-57.1106661007666,-25.7748538035644,39.92499));
#203396=CARTESIAN_POINT('Origin',(-54.3889216310786,-23.8679610547564,39.6398955069333));
#203397=CARTESIAN_POINT('Origin',(-54.2261740956467,-23.7955011834905,39.92499));
#203398=CARTESIAN_POINT('Origin',(-56.9479187893687,-25.7023940320469,39.6398955068279));
#203399=CARTESIAN_POINT('Origin',(-56.7851714777849,-25.6299342604992,39.3548010137695));
#203400=CARTESIAN_POINT('Ctrl Pts',(-54.1275498658875,-23.7522229508825,
39.8576902534424));
#203401=CARTESIAN_POINT('Ctrl Pts',(-54.0765745253537,-23.8679139708565,
39.8579948730704));
#203402=CARTESIAN_POINT('Ctrl Pts',(-54.1745185419761,-23.9115214566111,
39.92499));
#203403=CARTESIAN_POINT('Ctrl Pts',(-54.0860417646976,-23.7337429357609,
39.9304020711231));
#203404=CARTESIAN_POINT('Ctrl Pts',(-54.0553388636007,-23.8418262755865,
39.9058915297382));
#203405=CARTESIAN_POINT('Ctrl Pts',(-54.1330089371358,-23.8930401898204,
39.9671523786037));
#203406=CARTESIAN_POINT('Ctrl Pts',(-54.0331737207069,-23.7393098712348,
40.0043257306692));
#203407=CARTESIAN_POINT('Ctrl Pts',(-54.018846794374,-23.83019265673,39.9667894847832));
#203408=CARTESIAN_POINT('Ctrl Pts',(-54.0846755205373,-23.888427522722,
40.01001389752));
#203409=CARTESIAN_POINT('Ctrl Pts',(-53.9248984592618,-23.8065189073819,
40.1195533054858));
#203410=CARTESIAN_POINT('Ctrl Pts',(-53.938451117416,-23.8631501047895,
40.0630813209239));
#203411=CARTESIAN_POINT('Ctrl Pts',(-53.9943748351526,-23.9152668978358,
40.0768265942421));
#203412=CARTESIAN_POINT('Ctrl Pts',(-53.8688190939453,-23.8710081209822,
40.1599502027532));
#203413=CARTESIAN_POINT('Ctrl Pts',(-53.8932068549987,-23.9079567336545,
40.1002552791566));
#203414=CARTESIAN_POINT('Ctrl Pts',(-53.9522270531151,-23.9484663513831,
40.10025));
#203415=CARTESIAN_POINT('Ctrl Pts',(-53.8330634946839,-23.9513722670362,
40.1599502534424));
#203416=CARTESIAN_POINT('Ctrl Pts',(-53.8671470951732,-23.9665367208221,
40.10025));
#203417=CARTESIAN_POINT('Ctrl Pts',(-53.9314655730806,-23.9951532569804,
40.10025));
#203418=CARTESIAN_POINT('Origin',(-53.9314655730806,-23.9951532569804,40.22725));
#203419=CARTESIAN_POINT('Ctrl Pts',(-56.3916032444852,-25.454706393408,
38.989));
#203420=CARTESIAN_POINT('Ctrl Pts',(-56.4433359736143,-25.3385127813695,
38.989));
#203421=CARTESIAN_POINT('Ctrl Pts',(-56.4432587405903,-25.3386862495817,
39.1161896013263));
#203422=CARTESIAN_POINT('Ctrl Pts',(-56.5897307565552,-25.5431622092801,
38.989));
#203423=CARTESIAN_POINT('Ctrl Pts',(-56.6417243268827,-25.4268404215574,
38.9887769275485));
#203424=CARTESIAN_POINT('Ctrl Pts',(-56.6017747680112,-25.4092621323421,
39.1161898821845));
#203425=CARTESIAN_POINT('Ctrl Pts',(-56.7783458705719,-25.6273687254288,
39.1034967087244));
#203426=CARTESIAN_POINT('Ctrl Pts',(-56.8305375176085,-25.5109049500324,
39.1031720232701));
#203427=CARTESIAN_POINT('Ctrl Pts',(-56.7526792962279,-25.4764491573029,
39.2077529615002));
#203428=CARTESIAN_POINT('Ctrl Pts',(-56.8833377255396,-25.6742415049977,
39.2875012672119));
#203429=CARTESIAN_POINT('Ctrl Pts',(-56.9357219102086,-25.5577357740381,
39.2872087095508));
#203430=CARTESIAN_POINT('Ctrl Pts',(-56.8366797674145,-25.5138485767964,
39.3549017048226));
#203431=CARTESIAN_POINT('Origin',(-56.3916032444852,-25.454706393408,39.116));
#203432=CARTESIAN_POINT('Origin',(3.58382961824622E-16,-2.38580516864205E-17,
40.22725));
#203433=CARTESIAN_POINT('Origin',(-53.9190682401996,-24.0229981225294,40.22725));
#203434=CARTESIAN_POINT('Origin',(52.0578415156897,22.8300973196046,39.116));
#203435=CARTESIAN_POINT('Origin',(-56.0249274780499,-25.2915084057458,39.1160373285229));
#203436=CARTESIAN_POINT('Ctrl Pts',(-53.8206887816837,-23.9791663275011,
40.1599502534424));
#203437=CARTESIAN_POINT('Ctrl Pts',(-53.8547645473082,-23.9943483786814,
40.10025));
#203438=CARTESIAN_POINT('Ctrl Pts',(-53.9190682401996,-24.0229981225294,
40.10025));
#203439=CARTESIAN_POINT('Ctrl Pts',(-53.7850138844279,-24.0592381182999,
40.1599500566036));
#203440=CARTESIAN_POINT('Ctrl Pts',(-53.8287709626504,-24.052682504579,
40.1002551305357));
#203441=CARTESIAN_POINT('Ctrl Pts',(-53.8983362760846,-24.0695074323273,
40.10025));
#203442=CARTESIAN_POINT('Ctrl Pts',(-53.7744461045708,-24.143290671037,
40.1203070619046));
#203443=CARTESIAN_POINT('Ctrl Pts',(-53.8255298669651,-24.1158128282434,
40.0637098684497));
#203444=CARTESIAN_POINT('Ctrl Pts',(-53.9015903052241,-24.1225146216896,
40.0772636213363));
#203445=CARTESIAN_POINT('Ctrl Pts',(-53.7968389608977,-24.2696905364169,
40.0046102245802));
#203446=CARTESIAN_POINT('Ctrl Pts',(-53.8548027426702,-24.1983175571252,
39.9670001894016));
#203447=CARTESIAN_POINT('Ctrl Pts',(-53.9421141528986,-24.2081897025473,
40.0101788811209));
#203448=CARTESIAN_POINT('Ctrl Pts',(-53.8282518514941,-24.3127961529,39.9303710930186));
#203449=CARTESIAN_POINT('Ctrl Pts',(-53.8880291490215,-24.217648824503,
39.9058663574108));
#203450=CARTESIAN_POINT('Ctrl Pts',(-53.9780599067636,-24.2411088588488,
39.9671344706378));
#203451=CARTESIAN_POINT('Ctrl Pts',(-53.8697418420146,-24.3312692531085,
39.8576902534424));
#203452=CARTESIAN_POINT('Ctrl Pts',(-53.9216078643418,-24.2159747902184,
39.8579948730703));
#203453=CARTESIAN_POINT('Ctrl Pts',(-54.0195518809642,-24.259582275973,
39.92499));
#203454=CARTESIAN_POINT('Origin',(-53.9678963272936,-24.3756025490936,39.92499));
#203455=CARTESIAN_POINT('Origin',(-55.984546168509,-25.2734729066183,39.1925554488849));
#203456=CARTESIAN_POINT('Origin',(-55.9097831300748,-25.2401862573139,39.3343017080178));
#203457=CARTESIAN_POINT('Origin',(-54.1306438627326,-24.4480624203039,39.6398955069233));
#203458=CARTESIAN_POINT('Origin',(-54.2933913980365,-24.5205222915149,39.3548010137695));
#203459=CARTESIAN_POINT('Ctrl Pts',(-55.6083495590303,-25.1059793847698,
39.3978017080178));
#203460=CARTESIAN_POINT('Ctrl Pts',(-55.6600051127009,-24.9899591116492,
39.3978017080178));
#203461=CARTESIAN_POINT('Ctrl Pts',(-55.6600051127009,-24.9899591116492,
39.5248017080178));
#203462=CARTESIAN_POINT('Ctrl Pts',(-55.6906734752781,-25.1423759987951,
39.3978017080178));
#203463=CARTESIAN_POINT('Ctrl Pts',(-55.7421565548654,-25.02653529024,39.3980355775177));
#203464=CARTESIAN_POINT('Ctrl Pts',(-55.7833465978032,-25.0448742789053,
39.5248015517192));
#203465=CARTESIAN_POINT('Ctrl Pts',(-55.7685161955951,-25.1767934079555,
39.3484893995498));
#203466=CARTESIAN_POINT('Ctrl Pts',(-55.8202243900357,-25.0612933298591,
39.3489438303427));
#203467=CARTESIAN_POINT('Ctrl Pts',(-55.89997474663,-25.0968004762774,39.4508333155595));
#203468=CARTESIAN_POINT('Ctrl Pts',(-55.8095395120008,-25.1949317875298,
39.2708017080178));
#203469=CARTESIAN_POINT('Ctrl Pts',(-55.861411884108,-25.079631183695,39.2710850691866));
#203470=CARTESIAN_POINT('Ctrl Pts',(-55.9614386837454,-25.1241659841932,
39.3343017080178));
#203471=CARTESIAN_POINT('Origin',(-55.6083495590303,-25.1059793847698,39.5248017080178));
#203472=CARTESIAN_POINT('Ctrl Pts',(-54.1952354911873,-24.4761921430389,
39.2875012672119));
#203473=CARTESIAN_POINT('Ctrl Pts',(-54.2471777813617,-24.3607210247424,
39.2878045257519));
#203474=CARTESIAN_POINT('Ctrl Pts',(-54.3451938326303,-24.4045675690225,
39.3549015218347));
#203475=CARTESIAN_POINT('Ctrl Pts',(-54.3002261711149,-24.5230721320486,
39.1034938540228));
#203476=CARTESIAN_POINT('Ctrl Pts',(-54.3520689157368,-24.4074212664111,
39.1038286278808));
#203477=CARTESIAN_POINT('Ctrl Pts',(-54.4291958219391,-24.441967664437,
39.2077506434033));
#203478=CARTESIAN_POINT('Ctrl Pts',(-54.4888383671852,-24.6072895482014,
38.989));
#203479=CARTESIAN_POINT('Ctrl Pts',(-54.5406519873274,-24.4913833136928,
38.9892298954611));
#203480=CARTESIAN_POINT('Ctrl Pts',(-54.5801016184605,-24.5091552540984,
39.1161900347287));
#203481=CARTESIAN_POINT('Ctrl Pts',(-54.6869600343299,-24.6957503380304,
38.989));
#203482=CARTESIAN_POINT('Ctrl Pts',(-54.7386929643776,-24.5795562747214,
38.989));
#203483=CARTESIAN_POINT('Ctrl Pts',(-54.7386155301351,-24.5797301948777,
39.1161900945644));
#203484=CARTESIAN_POINT('Origin',(-54.6869600343299,-24.6957503380304,39.116));
#203485=CARTESIAN_POINT('Origin',(50.7999799080417,22.2700612497314,39.5248017080178));
#203486=CARTESIAN_POINT('Origin',(-55.4702140717968,-25.0444775033944,39.5248017080178));
#203487=CARTESIAN_POINT('Origin',(50.603004322856,22.1823620689013,39.116));
#203488=CARTESIAN_POINT('Origin',(-55.0536014459539,-24.8590452239598,39.1160402713848));
#203489=CARTESIAN_POINT('Ctrl Pts',(-55.2690209153042,-24.9555320242412,
39.2708017080178));
#203490=CARTESIAN_POINT('Ctrl Pts',(-55.3213695969757,-24.8391888661841,
39.2705119464801));
#203491=CARTESIAN_POINT('Ctrl Pts',(-55.2204359898058,-24.7942503289604,
39.3343017080178));
#203492=CARTESIAN_POINT('Ctrl Pts',(-55.3101840490925,-24.9737291291718,
39.3487519301186));
#203493=CARTESIAN_POINT('Ctrl Pts',(-55.3622664445122,-24.8573973158467,
39.3482879463976));
#203494=CARTESIAN_POINT('Ctrl Pts',(-55.2821076446841,-24.8217083187827,
39.4512271261631));
#203495=CARTESIAN_POINT('Ctrl Pts',(-55.3881672017734,-25.0082040095644,
39.3978017080178));
#203496=CARTESIAN_POINT('Ctrl Pts',(-55.4398389138625,-24.891934804391,
39.3975673827397));
#203497=CARTESIAN_POINT('Ctrl Pts',(-55.398943589477,-24.8737270328796,
39.5248015355181));
#203498=CARTESIAN_POINT('Ctrl Pts',(-55.4702140717968,-25.0444775033944,
39.3978017080178));
#203499=CARTESIAN_POINT('Ctrl Pts',(-55.5218696254675,-24.9284572302738,
39.3978017080178));
#203500=CARTESIAN_POINT('Ctrl Pts',(-55.5218696254674,-24.9284572302738,
39.5248017080178));
#203501=CARTESIAN_POINT('Origin',(-55.1687804361351,-24.910270602081,39.3343017080178));
#203502=CARTESIAN_POINT('Origin',(-55.094463269184,-24.877182467873,39.1934008533551));
#203503=CARTESIAN_POINT('Origin',(-58.5158800435658,-18.6791227126686,39.1925554495081));
#203504=CARTESIAN_POINT('Origin',(-58.5579573083275,-18.6927400943506,39.116037328525));
#203505=CARTESIAN_POINT('Origin',(-58.4380471616456,-18.6538332760101,39.3343017080178));
#203506=CARTESIAN_POINT('Ctrl Pts',(-58.3332704847797,-18.6203878281144,
39.2708017080178));
#203507=CARTESIAN_POINT('Ctrl Pts',(-58.2946680067389,-18.7407822670299,
39.2710850691866));
#203508=CARTESIAN_POINT('Ctrl Pts',(-58.3988020033599,-18.7746174535796,
39.3343017080178));
#203509=CARTESIAN_POINT('Ctrl Pts',(-58.290503238026,-18.6063701040101,
39.3487519293518));
#203510=CARTESIAN_POINT('Ctrl Pts',(-58.2516444665226,-18.7268030714108,
39.3492068662929));
#203511=CARTESIAN_POINT('Ctrl Pts',(-58.3345980746913,-18.7537563325796,
39.4512271248734));
#203512=CARTESIAN_POINT('Ctrl Pts',(-58.2094810152002,-18.5798130476653,
39.3978017080178));
#203513=CARTESIAN_POINT('Ctrl Pts',(-58.1702276772286,-18.7003491529652,
39.3980347781174));
#203514=CARTESIAN_POINT('Ctrl Pts',(-58.2129647630934,-18.7142352739234,
39.524801535519));
#203515=CARTESIAN_POINT('Ctrl Pts',(-58.1242364370958,-18.5518699907147,
39.3978017080178));
#203516=CARTESIAN_POINT('Ctrl Pts',(-58.0849912788101,-18.6726541682842,
39.3978017080178));
#203517=CARTESIAN_POINT('Ctrl Pts',(-58.0849912788101,-18.6726541682842,
39.5248017080178));
#203518=CARTESIAN_POINT('Origin',(-58.1242364370958,-18.5518699907147,39.5248017080178));
#203519=CARTESIAN_POINT('Origin',(-0.0981128957140385,0.301960443923712,
39.116));
#203520=CARTESIAN_POINT('Origin',(-58.9396512752214,-18.8168143322223,39.116));
#203521=CARTESIAN_POINT('Origin',(-0.0981128957140384,0.301960443923712,
39.5248017080178));
#203522=CARTESIAN_POINT('Origin',(-57.9804289733665,-18.5051441132838,39.5248017080178));
#203523=CARTESIAN_POINT('Ctrl Pts',(-59.4519788726609,-18.9827025415093,
39.2875012672119));
#203524=CARTESIAN_POINT('Ctrl Pts',(-59.4129503614028,-19.1043350233604,
39.287208709576));
#203525=CARTESIAN_POINT('Ctrl Pts',(-59.3099814440481,-19.0706774512225,
39.3549016990122));
#203526=CARTESIAN_POINT('Ctrl Pts',(-59.3425890481023,-18.947282004205,
39.103493917393));
#203527=CARTESIAN_POINT('Ctrl Pts',(-59.3034455268852,-19.0687544722082,
39.103169233633));
#203528=CARTESIAN_POINT('Ctrl Pts',(-59.222530503847,-19.0422629184333,
39.2077507202298));
#203529=CARTESIAN_POINT('Ctrl Pts',(-59.1460739925266,-18.8836509927321,
38.989));
#203530=CARTESIAN_POINT('Ctrl Pts',(-59.1068782740634,-19.0048854004771,
38.9887769311176));
#203531=CARTESIAN_POINT('Ctrl Pts',(-59.0654284453497,-18.9912173655545,
39.1161898712915));
#203532=CARTESIAN_POINT('Ctrl Pts',(-58.9396512752214,-18.8168143322223,
38.989));
#203533=CARTESIAN_POINT('Ctrl Pts',(-58.9003474864892,-18.937778955752,
38.989));
#203534=CARTESIAN_POINT('Ctrl Pts',(-58.900406160666,-18.9375983752041,
39.1161895903854));
#203535=CARTESIAN_POINT('Origin',(-59.3493798002281,-18.9499432001054,39.3548010137695));
#203536=CARTESIAN_POINT('Ctrl Pts',(-57.9804289733665,-18.5051441132838,
39.3978017080178));
#203537=CARTESIAN_POINT('Ctrl Pts',(-57.9411838150808,-18.6259282908533,
39.3978017080178));
#203538=CARTESIAN_POINT('Ctrl Pts',(-57.9411838150808,-18.6259282908533,
39.5248017080178));
#203539=CARTESIAN_POINT('Ctrl Pts',(-57.8948964606935,-18.4771060595081,
39.3978017080178));
#203540=CARTESIAN_POINT('Ctrl Pts',(-57.8554964068714,-18.5980867642071,
39.3975666025045));
#203541=CARTESIAN_POINT('Ctrl Pts',(-57.8127777979941,-18.584206646787,
39.5248015517196));
#203542=CARTESIAN_POINT('Ctrl Pts',(-57.8140195545737,-18.4505921960625,
39.3484894016716));
#203543=CARTESIAN_POINT('Ctrl Pts',(-57.7748837362118,-18.5718941197414,
39.3480259000037));
#203544=CARTESIAN_POINT('Ctrl Pts',(-57.691360753939,-18.5447558577151,
39.4508333188944));
#203545=CARTESIAN_POINT('Ctrl Pts',(-57.7713971777988,-18.4366189870669,
39.2708017080178));
#203546=CARTESIAN_POINT('Ctrl Pts',(-57.7324510618071,-18.5581069080657,
39.27051194648));
#203547=CARTESIAN_POINT('Ctrl Pts',(-57.6273730232606,-18.5239649837004,
39.3343017080178));
#203548=CARTESIAN_POINT('Origin',(-57.6666181815462,-18.403180806131,39.3343017080178));
#203549=CARTESIAN_POINT('Origin',(-59.5188096735778,-19.0049943031116,39.6398955068191));
#203550=CARTESIAN_POINT('Origin',(-59.6882395467421,-19.0600454060083,39.92499));
#203551=CARTESIAN_POINT('Origin',(-57.5892494790283,-18.3780421908171,39.1934008539945));
#203552=CARTESIAN_POINT('Origin',(-57.5467470426661,-18.3641788932745,39.1160402713852));
#203553=CARTESIAN_POINT('Ctrl Pts',(-59.8776671349986,-19.4393816709753,
40.1599502534424));
#203554=CARTESIAN_POINT('Ctrl Pts',(-59.8421853116554,-19.4278624395263,
40.10025));
#203555=CARTESIAN_POINT('Ctrl Pts',(-59.7752282754838,-19.406124729225,
40.10025));
#203556=CARTESIAN_POINT('Ctrl Pts',(-59.9048758468122,-19.3555723159019,
40.1599500538466));
#203557=CARTESIAN_POINT('Ctrl Pts',(-59.8620015382124,-19.3668135526099,
40.1002448353481));
#203558=CARTESIAN_POINT('Ctrl Pts',(-59.7909691583393,-19.3576098387253,
40.10025));
#203559=CARTESIAN_POINT('Ctrl Pts',(-59.9061888791358,-19.270512881395,
40.120244200104));
#203560=CARTESIAN_POINT('Ctrl Pts',(-59.8582551377155,-19.3034480936182,
40.0633873868017));
#203561=CARTESIAN_POINT('Ctrl Pts',(-59.7817014705985,-19.3051157581416,
40.0772271723537));
#203562=CARTESIAN_POINT('Ctrl Pts',(-59.8700374834723,-19.1466203444577,
40.0045995998161));
#203563=CARTESIAN_POINT('Ctrl Pts',(-59.8200494324144,-19.2244111832568,
39.9663485808314));
#203564=CARTESIAN_POINT('Ctrl Pts',(-59.7316696194037,-19.2239451174248,
40.0101727202466));
#203565=CARTESIAN_POINT('Ctrl Pts',(-59.834087357436,-19.1068608943535,
39.930465434986));
#203566=CARTESIAN_POINT('Ctrl Pts',(-59.7849307811025,-19.2088773592673,
39.9051900162943));
#203567=CARTESIAN_POINT('Ctrl Pts',(-59.6922425516964,-19.1948817636404,
39.967185745818));
#203568=CARTESIAN_POINT('Ctrl Pts',(-59.7908376697913,-19.0928077206408,
39.8576902534424));
#203569=CARTESIAN_POINT('Ctrl Pts',(-59.7518659300027,-19.214254573608,
39.8573998014387));
#203570=CARTESIAN_POINT('Ctrl Pts',(-59.6489943884565,-19.1808295835778,
39.92499));
#203571=CARTESIAN_POINT('Origin',(-59.7752282754838,-19.406124729225,40.22725));
#203572=CARTESIAN_POINT('Origin',(-0.0981128957140385,0.301960443923712,
39.116));
#203573=CARTESIAN_POINT('Origin',(-57.1650137687748,-18.2401996527042,39.116));
#203574=CARTESIAN_POINT('Origin',(1.26611655068502E-16,5.09536863743838E-17,
40.22725));
#203575=CARTESIAN_POINT('Origin',(-59.7658094374952,-19.4351129318417,40.22725));
#203576=CARTESIAN_POINT('Ctrl Pts',(-57.1650137687748,-18.2401996527042,
38.989));
#203577=CARTESIAN_POINT('Ctrl Pts',(-57.12570981947,-18.3611647704257,38.989));
#203578=CARTESIAN_POINT('Ctrl Pts',(-57.1257686544591,-18.3609836949483,
39.1161901092321));
#203579=CARTESIAN_POINT('Ctrl Pts',(-56.958585650595,-18.1733685221997,
38.989));
#203580=CARTESIAN_POINT('Ctrl Pts',(-56.9195342693626,-18.2941737326415,
38.989229898976));
#203581=CARTESIAN_POINT('Ctrl Pts',(-56.9607434512643,-18.3073637563258,
39.11619004932));
#203582=CARTESIAN_POINT('Ctrl Pts',(-56.7620685738646,-18.109748568444,
39.1034966344368));
#203583=CARTESIAN_POINT('Ctrl Pts',(-56.72320970454,-18.230383490407,39.103831410257));
#203584=CARTESIAN_POINT('Ctrl Pts',(-56.8036425617902,-18.2563185833,39.2077528789599));
#203585=CARTESIAN_POINT('Ctrl Pts',(-56.6526781108325,-18.0743352474888,
39.2875012672119));
#203586=CARTESIAN_POINT('Ctrl Pts',(-56.6140134911409,-18.1949032015563,
39.2878045257868));
#203587=CARTESIAN_POINT('Ctrl Pts',(-56.7161926934812,-18.2279043987988,
39.3549015295898));
#203588=CARTESIAN_POINT('Origin',(-56.7552848242271,-18.1070706485039,39.3548010137695));
#203589=CARTESIAN_POINT('Ctrl Pts',(-59.5942745858237,-19.6977666881842,
39.8576902534424));
#203590=CARTESIAN_POINT('Ctrl Pts',(-59.6341304551458,-19.5766071063165,
39.8573998014387));
#203591=CARTESIAN_POINT('Ctrl Pts',(-59.5312589135996,-19.5431821162863,
39.92499));
#203592=CARTESIAN_POINT('Ctrl Pts',(-59.6375442153292,-19.7118253299473,
39.9304984902491));
#203593=CARTESIAN_POINT('Ctrl Pts',(-59.6577332347575,-19.6004058925596,
39.9052171569799));
#203594=CARTESIAN_POINT('Ctrl Pts',(-59.5745267832909,-19.557240699363,
39.9672049726607));
#203595=CARTESIAN_POINT('Ctrl Pts',(-59.6898285824899,-19.7007277907731,
40.0043437678662));
#203596=CARTESIAN_POINT('Ctrl Pts',(-59.6951745640074,-19.6083614943628,
39.9661628577642));
#203597=CARTESIAN_POINT('Ctrl Pts',(-59.6233361049588,-19.5568428722495,
40.0100243556236));
#203598=CARTESIAN_POINT('Ctrl Pts',(-59.7913053863691,-19.6225475038108,
40.1194874821987));
#203599=CARTESIAN_POINT('Ctrl Pts',(-59.7720679362494,-19.5674227749672,
40.062755148314));
#203600=CARTESIAN_POINT('Ctrl Pts',(-59.7110541706153,-19.5210053955058,
40.0767884282377));
#203601=CARTESIAN_POINT('Ctrl Pts',(-59.8408924241699,-19.5524931121159,
40.1599502015383));
#203602=CARTESIAN_POINT('Ctrl Pts',(-59.8128277376112,-19.518154979168,
40.1002449453878));
#203603=CARTESIAN_POINT('Ctrl Pts',(-59.7499755976267,-19.4837751174916,
40.10025));
#203604=CARTESIAN_POINT('Ctrl Pts',(-59.8682321556243,-19.4684195516693,
40.1599502534424));
#203605=CARTESIAN_POINT('Ctrl Pts',(-59.8327559231847,-19.456883113188,
40.10025));
#203606=CARTESIAN_POINT('Ctrl Pts',(-59.7658094374952,-19.4351129318417,
40.10025));
#203607=CARTESIAN_POINT('Origin',(-59.492013755314,-19.6639662938558,39.92499));
#203608=CARTESIAN_POINT('Origin',(-56.5858547179577,-18.0520194698753,39.6398955069312));
#203609=CARTESIAN_POINT('Origin',(-56.4164246115664,-17.9969682911408,39.92499));
#203610=CARTESIAN_POINT('Origin',(-59.322583882151,-19.6089151909104,39.6398955068277));
#203611=CARTESIAN_POINT('Origin',(-59.1531540088,-19.5538640879529,39.3548010137695));
#203612=CARTESIAN_POINT('Ctrl Pts',(-56.3138168485096,-17.9642361803969,
39.8576902534424));
#203613=CARTESIAN_POINT('Ctrl Pts',(-56.2752137607567,-18.0846218068692,
39.8579948730704));
#203614=CARTESIAN_POINT('Ctrl Pts',(-56.3771794532808,-18.1177524687103,
39.92499));
#203615=CARTESIAN_POINT('Ctrl Pts',(-56.2706044454594,-17.9501961787622,
39.930402071123));
#203616=CARTESIAN_POINT('Ctrl Pts',(-56.2513675234837,-18.0608967538131,
39.9058915297375));
#203617=CARTESIAN_POINT('Ctrl Pts',(-56.3339654239822,-18.1037113794376,
39.9671523786033));
#203618=CARTESIAN_POINT('Ctrl Pts',(-56.2186079213553,-17.9612588333755,
40.0043257306694));
#203619=CARTESIAN_POINT('Ctrl Pts',(-56.2138593173284,-18.0531413250549,
39.9667894847836));
#203620=CARTESIAN_POINT('Ctrl Pts',(-56.2854146278931,-18.1041761987734,
40.0100138975199));
#203621=CARTESIAN_POINT('Ctrl Pts',(-56.1179510603878,-18.0394175380792,
40.1195533054856));
#203622=CARTESIAN_POINT('Ctrl Pts',(-56.1373490477012,-18.0943218653325,
40.0630813209237));
#203623=CARTESIAN_POINT('Ctrl Pts',(-56.198414097748,-18.1403075368578,
40.0768265942421));
#203624=CARTESIAN_POINT('Ctrl Pts',(-56.0689198620976,-18.1094153628975,
40.1599502027523));
#203625=CARTESIAN_POINT('Ctrl Pts',(-56.0970362061497,-18.1436123520189,
40.1002552791554));
#203626=CARTESIAN_POINT('Ctrl Pts',(-56.1599674935319,-18.1777307632115,
40.10025));
#203627=CARTESIAN_POINT('Ctrl Pts',(-56.0417604764384,-18.1930767435946,
40.1599502534424));
#203628=CARTESIAN_POINT('Ctrl Pts',(-56.0772424804485,-18.2045954185342,
40.10025));
#203629=CARTESIAN_POINT('Ctrl Pts',(-56.1441998575528,-18.2263320786579,
40.10025));
#203630=CARTESIAN_POINT('Origin',(-56.1441998575528,-18.2263320786579,40.22725));
#203631=CARTESIAN_POINT('Ctrl Pts',(-58.7434254837933,-19.4207352200698,
38.989));
#203632=CARTESIAN_POINT('Ctrl Pts',(-58.7827292759115,-19.299770586119,
38.989));
#203633=CARTESIAN_POINT('Ctrl Pts',(-58.7826705983437,-19.2999511771035,
39.1161896013263));
#203634=CARTESIAN_POINT('Ctrl Pts',(-58.9497137831222,-19.4879965013589,
38.989));
#203635=CARTESIAN_POINT('Ctrl Pts',(-58.9892635895143,-19.3668771285525,
38.9887769275485));
#203636=CARTESIAN_POINT('Ctrl Pts',(-58.9476954469492,-19.3535710010441,
39.1161898821845));
#203637=CARTESIAN_POINT('Ctrl Pts',(-59.1460976215389,-19.5520260773857,
39.1034967087243));
#203638=CARTESIAN_POINT('Ctrl Pts',(-59.1858295778064,-19.4307447900771,
39.1031720232694));
#203639=CARTESIAN_POINT('Ctrl Pts',(-59.1047962608419,-19.4046161500177,
39.2077529615002));
#203640=CARTESIAN_POINT('Ctrl Pts',(-59.2554138597572,-19.5876674457075,
39.2875012672119));
#203641=CARTESIAN_POINT('Ctrl Pts',(-59.2953329133625,-19.4663243070093,
39.2872087095508));
#203642=CARTESIAN_POINT('Ctrl Pts',(-59.1922458725047,-19.4330302514111,
39.3549017048226));
#203643=CARTESIAN_POINT('Origin',(-58.7434254837933,-19.4207352200698,39.116));
#203644=CARTESIAN_POINT('Origin',(3.56182666396657E-16,-1.81260861279366E-17,
40.22725));
#203645=CARTESIAN_POINT('Origin',(-56.1347810195643,-18.2553202812746,40.22725));
#203646=CARTESIAN_POINT('Origin',(56.3788528200609,17.9847604760579,39.116));
#203647=CARTESIAN_POINT('Origin',(-58.3616995707157,-19.2967593024458,39.1160373285271));
#203648=CARTESIAN_POINT('Ctrl Pts',(-56.0323588238392,-18.2220120550214,
40.1599502534424));
#203649=CARTESIAN_POINT('Ctrl Pts',(-56.0678348753333,-18.2335490499215,
40.10025));
#203650=CARTESIAN_POINT('Ctrl Pts',(-56.1347810195643,-18.2553202812746,
40.10025));
#203651=CARTESIAN_POINT('Ctrl Pts',(-56.0052491386463,-18.3053742463596,
40.1599500566039));
#203652=CARTESIAN_POINT('Ctrl Pts',(-56.0480812627871,-18.2942806848323,
40.1002551305381));
#203653=CARTESIAN_POINT('Ctrl Pts',(-56.119024173998,-18.3037418885563,
40.10025));
#203654=CARTESIAN_POINT('Ctrl Pts',(-56.0035251343645,-18.3900709842066,
40.1203070619048));
#203655=CARTESIAN_POINT('Ctrl Pts',(-56.0514568378818,-18.3574039607304,
40.0637098684502));
#203656=CARTESIAN_POINT('Ctrl Pts',(-56.1278011372719,-18.3561185603238,
40.0772636213363));
#203657=CARTESIAN_POINT('Ctrl Pts',(-56.039007703967,-18.5134377270389,
40.0046102245801));
#203658=CARTESIAN_POINT('Ctrl Pts',(-56.0891934462345,-18.4363968713614,
39.9670001894009));
#203659=CARTESIAN_POINT('Ctrl Pts',(-56.177058475612,-18.4370884086013,
40.0101788811209));
#203660=CARTESIAN_POINT('Ctrl Pts',(-56.0747542753109,-18.5530236652639,
39.9303710930187));
#203661=CARTESIAN_POINT('Ctrl Pts',(-56.1242585025264,-18.4521491348386,
39.9058663574113));
#203662=CARTESIAN_POINT('Ctrl Pts',(-56.2162483036945,-18.4660698759071,
39.9671344706363));
#203663=CARTESIAN_POINT('Ctrl Pts',(-56.1179479440989,-18.5670586829462,
39.8576902534424));
#203664=CARTESIAN_POINT('Ctrl Pts',(-56.1574782858998,-18.4469743395776,
39.8579948730703));
#203665=CARTESIAN_POINT('Ctrl Pts',(-56.259443978424,-18.4801050014187,
39.92499));
#203666=CARTESIAN_POINT('Origin',(-56.2201988201384,-18.6008891789882,39.92499));
#203667=CARTESIAN_POINT('Origin',(-58.319654251203,-19.2830435998987,39.1925554488847));
#203668=CARTESIAN_POINT('Origin',(-58.2418213702175,-19.2577541638575,39.3343017080178));
#203669=CARTESIAN_POINT('Origin',(-56.3896289265332,-18.6559403576609,39.6398955069214));
#203670=CARTESIAN_POINT('Origin',(-56.559059032799,-18.7109915363514,39.3548010137695));
#203671=CARTESIAN_POINT('Ctrl Pts',(-57.9280106456677,-19.1557908785622,
39.3978017080178));
#203672=CARTESIAN_POINT('Ctrl Pts',(-57.9672558039533,-19.0350067009927,
39.3978017080178));
#203673=CARTESIAN_POINT('Ctrl Pts',(-57.9672558039533,-19.0350067009927,
39.5248017080178));
#203674=CARTESIAN_POINT('Ctrl Pts',(-58.0136880650209,-19.1833829156714,
39.3978017080178));
#203675=CARTESIAN_POINT('Ctrl Pts',(-58.0527804636624,-19.0627953474463,
39.3980355775177));
#203676=CARTESIAN_POINT('Ctrl Pts',(-58.0956618095384,-19.0767283413219,
39.5248015517192));
#203677=CARTESIAN_POINT('Ctrl Pts',(-58.0947019536606,-19.2094750027316,
39.3484893995498));
#203678=CARTESIAN_POINT('Ctrl Pts',(-58.1340538395301,-19.0892026680456,
39.3489438303425));
#203679=CARTESIAN_POINT('Ctrl Pts',(-58.2170788227769,-19.1161791203808,
39.4508333155594));
#203680=CARTESIAN_POINT('Ctrl Pts',(-58.1373965169895,-19.2232259141436,
39.2708017080178));
#203681=CARTESIAN_POINT('Ctrl Pts',(-58.1769325318821,-19.1031347997384,
39.2710850691866));
#203682=CARTESIAN_POINT('Ctrl Pts',(-58.2810665285031,-19.136969986288,
39.3343017080178));
#203683=CARTESIAN_POINT('Origin',(-57.9280106456677,-19.1557908785622,39.5248017080178));
#203684=CARTESIAN_POINT('Ctrl Pts',(-56.4568070719812,-18.6771643191707,
39.2875012672119));
#203685=CARTESIAN_POINT('Ctrl Pts',(-56.4963947983079,-18.5568963159714,
39.2878045257519));
#203686=CARTESIAN_POINT('Ctrl Pts',(-56.5984571192854,-18.5902571970798,
39.3549015218348));
#203687=CARTESIAN_POINT('Ctrl Pts',(-56.566122895188,-18.7128129802652,
39.1034938540228));
#203688=CARTESIAN_POINT('Ctrl Pts',(-56.6055928325706,-18.5923766197444,
39.1038286278815));
#203689=CARTESIAN_POINT('Ctrl Pts',(-56.6859083114046,-18.6186718120036,
39.2077506434028));
#203690=CARTESIAN_POINT('Ctrl Pts',(-56.7625049710037,-18.7768537015935,
38.989));
#203691=CARTESIAN_POINT('Ctrl Pts',(-56.8019192501367,-18.6561664154735,
38.9892298954606));
#203692=CARTESIAN_POINT('Ctrl Pts',(-56.8430104456856,-18.6697173900118,
39.116190034729));
#203693=CARTESIAN_POINT('Ctrl Pts',(-56.9687879773467,-18.8441205405516,
38.989));
#203694=CARTESIAN_POINT('Ctrl Pts',(-57.0080919221123,-18.7231554368005,
38.989));
#203695=CARTESIAN_POINT('Ctrl Pts',(-57.0080330916692,-18.7233364982866,
39.1161900945646));
#203696=CARTESIAN_POINT('Origin',(-56.9687879773467,-18.8441205405516,39.116));
#203697=CARTESIAN_POINT('Origin',(55.0155724295761,17.5418038257013,39.5248017080178));
#203698=CARTESIAN_POINT('Origin',(-57.7842031819384,-19.1090650011312,39.5248017080178));
#203699=CARTESIAN_POINT('Origin',(54.8020887275097,17.4724387660752,39.116));
#203700=CARTESIAN_POINT('Origin',(-57.3504898524412,-18.9681964166827,39.1160402713849));
#203701=CARTESIAN_POINT('Ctrl Pts',(-57.5748148483577,-19.0416371860875,
39.2708017080178));
#203702=CARTESIAN_POINT('Ctrl Pts',(-57.6147155869503,-18.9204594407742,
39.2705119464801));
#203703=CARTESIAN_POINT('Ctrl Pts',(-57.5096375484038,-18.8863175164089,
39.3343017080178));
#203704=CARTESIAN_POINT('Ctrl Pts',(-57.6176546016066,-19.0554318862547,
39.3487519301186));
#203705=CARTESIAN_POINT('Ctrl Pts',(-57.6572916985351,-18.9342932580167,
39.3482879463972));
#203706=CARTESIAN_POINT('Ctrl Pts',(-57.5738415009812,-18.9071786451773,
39.4512271261625));
#203707=CARTESIAN_POINT('Ctrl Pts',(-57.6988141606861,-19.0815664505358,
39.3978017080178));
#203708=CARTESIAN_POINT('Ctrl Pts',(-57.7380493683907,-18.960533015575,
39.3975673827415));
#203709=CARTESIAN_POINT('Ctrl Pts',(-57.6954748424951,-18.9466997135538,
39.5248015355199));
#203710=CARTESIAN_POINT('Ctrl Pts',(-57.7842031819384,-19.1090650011312,
39.3978017080178));
#203711=CARTESIAN_POINT('Ctrl Pts',(-57.823448340224,-18.9882808235617,
39.3978017080178));
#203712=CARTESIAN_POINT('Ctrl Pts',(-57.823448340224,-18.9882808235617,
39.5248017080178));
#203713=CARTESIAN_POINT('Origin',(-57.4703923901182,-19.0071016939784,39.3343017080178));
#203714=CARTESIAN_POINT('Origin',(-57.3930236885614,-18.9819630792891,39.1934008533553));
#203715=CARTESIAN_POINT('Origin',(-60.1478239224126,-12.4602215063121,39.1925554495081));
#203716=CARTESIAN_POINT('Origin',(-60.1910940874976,-12.4693660187259,39.1160373285263));
#203717=CARTESIAN_POINT('Origin',(-60.0677739512127,-12.4432063593718,39.3343017080178));
#203718=CARTESIAN_POINT('Ctrl Pts',(-59.9600752506738,-12.4208962741583,
39.2708017080178));
#203719=CARTESIAN_POINT('Ctrl Pts',(-59.9342688867326,-12.5446662374483,
39.2710850691866));
#203720=CARTESIAN_POINT('Ctrl Pts',(-60.0413691664788,-12.567431104665,
39.3343017080178));
#203721=CARTESIAN_POINT('Ctrl Pts',(-59.9160770362135,-12.4114257351942,
39.3487519293518));
#203722=CARTESIAN_POINT('Ctrl Pts',(-59.890019810135,-12.535260805871,39.3492068662926));
#203723=CARTESIAN_POINT('Ctrl Pts',(-59.9753363727317,-12.5533954010687,
39.4512271248741));
#203724=CARTESIAN_POINT('Ctrl Pts',(-59.8327226933131,-12.3934832896267,
39.3978017080178));
#203725=CARTESIAN_POINT('Ctrl Pts',(-59.8062838430892,-12.517462176626,
39.3980347781178));
#203726=CARTESIAN_POINT('Ctrl Pts',(-59.8502383056086,-12.5268049860494,
39.524801535519));
#203727=CARTESIAN_POINT('Ctrl Pts',(-59.7450242491248,-12.374603792416,
39.3978017080178));
#203728=CARTESIAN_POINT('Ctrl Pts',(-59.718619464391,-12.4988285377092,
39.3978017080178));
#203729=CARTESIAN_POINT('Ctrl Pts',(-59.718619464391,-12.4988285377092,
39.5248017080178));
#203730=CARTESIAN_POINT('Origin',(-59.7450242491248,-12.374603792416,39.5248017080178));
#203731=CARTESIAN_POINT('Origin',(-0.0660119618346311,0.310561863232984,
39.116));
#203732=CARTESIAN_POINT('Origin',(-60.5836663843182,-12.5528626811443,39.116));
#203733=CARTESIAN_POINT('Origin',(-0.0660119618346311,0.310561863232984,
39.5248017080178));
#203734=CARTESIAN_POINT('Origin',(-59.597120393566,-12.3431658574207,39.5248017080178));
#203735=CARTESIAN_POINT('Ctrl Pts',(-61.1105274371642,-12.6642893210138,
39.2875012672119));
#203736=CARTESIAN_POINT('Ctrl Pts',(-61.0844267845857,-12.7893350777081,
39.287208709576));
#203737=CARTESIAN_POINT('Ctrl Pts',(-60.9785037674411,-12.7666250679674,
39.3549016990123));
#203738=CARTESIAN_POINT('Ctrl Pts',(-60.9980344071775,-12.6404971713783,
39.1034939173931));
#203739=CARTESIAN_POINT('Ctrl Pts',(-60.9718026486717,-12.765395812612,
39.1031692336333));
#203740=CARTESIAN_POINT('Ctrl Pts',(-60.8885617651955,-12.7475073053528,
39.2077507202293));
#203741=CARTESIAN_POINT('Ctrl Pts',(-60.7959446297925,-12.5977561540114,
38.989));
#203742=CARTESIAN_POINT('Ctrl Pts',(-60.7696360759153,-12.7224234952044,
38.9887769311182));
#203743=CARTESIAN_POINT('Ctrl Pts',(-60.7269846150103,-12.7131630221038,
39.1161898712916));
#203744=CARTESIAN_POINT('Ctrl Pts',(-60.5836663843182,-12.5528626811443,
38.989));
#203745=CARTESIAN_POINT('Ctrl Pts',(-60.5572221520604,-12.6772730124465,
38.989));
#203746=CARTESIAN_POINT('Ctrl Pts',(-60.5572616290068,-12.677087288016,
39.1161895903855));
#203747=CARTESIAN_POINT('Origin',(-61.0050661295707,-12.6424339620838,39.3548010137695));
#203748=CARTESIAN_POINT('Ctrl Pts',(-59.597120393566,-12.3431658574207,
39.3978017080178));
#203749=CARTESIAN_POINT('Ctrl Pts',(-59.5707156088321,-12.4673906027139,
39.3978017080178));
#203750=CARTESIAN_POINT('Ctrl Pts',(-59.5707156088321,-12.4673906027139,
39.5248017080178));
#203751=CARTESIAN_POINT('Ctrl Pts',(-59.5091256622727,-12.3242219811464,
39.3978017080178));
#203752=CARTESIAN_POINT('Ctrl Pts',(-59.4825873732107,-12.4486583679641,
39.397566602504));
#203753=CARTESIAN_POINT('Ctrl Pts',(-59.4386519140003,-12.439319597819,
39.5248015517196));
#203754=CARTESIAN_POINT('Ctrl Pts',(-59.4259203549057,-12.306307302129,
39.3484894016716));
#203755=CARTESIAN_POINT('Ctrl Pts',(-59.3996784303305,-12.4310355281343,
39.3480259000026));
#203756=CARTESIAN_POINT('Ctrl Pts',(-59.3137762748666,-12.4127764613284,
39.4508333188935));
#203757=CARTESIAN_POINT('Ctrl Pts',(-59.3820708699071,-12.2968658913799,
39.2708017080178));
#203758=CARTESIAN_POINT('Ctrl Pts',(-59.3560370505014,-12.4217592664909,
39.27051194648));
#203759=CARTESIAN_POINT('Ctrl Pts',(-59.2479658375577,-12.398788021052,
39.3343017080178));
#203760=CARTESIAN_POINT('Origin',(-59.2743706222916,-12.2745632757588,39.3343017080178));
#203761=CARTESIAN_POINT('Origin',(-61.1793222555435,-12.6794732450911,39.6398955068204));
#203762=CARTESIAN_POINT('Origin',(-61.3535783813233,-12.7165125280162,39.92499));
#203763=CARTESIAN_POINT('Origin',(-59.1947980527939,-12.25764960399,39.1934008539944));
#203764=CARTESIAN_POINT('Origin',(-59.1510793400371,-12.2483049653992,39.1160402713851));
#203765=CARTESIAN_POINT('Ctrl Pts',(-61.5816197022698,-13.0739701745321,
40.1599502534424));
#203766=CARTESIAN_POINT('Ctrl Pts',(-61.545128164506,-13.0662229071063,
40.10025));
#203767=CARTESIAN_POINT('Ctrl Pts',(-61.4762657165316,-13.0516031943525,
40.10025));
#203768=CARTESIAN_POINT('Ctrl Pts',(-61.5999188988197,-12.9877758510415,
40.1599500538462));
#203769=CARTESIAN_POINT('Ctrl Pts',(-61.558454489368,-13.0034370926705,
40.100244835349));
#203770=CARTESIAN_POINT('Ctrl Pts',(-61.4868491822336,-13.0017087032035,
40.10025));
#203771=CARTESIAN_POINT('Ctrl Pts',(-61.5923336062396,-12.9030451317659,
40.1202442001039));
#203772=CARTESIAN_POINT('Ctrl Pts',(-61.5481051179917,-12.9408103617798,
40.0633873868018));
#203773=CARTESIAN_POINT('Ctrl Pts',(-61.4721451382825,-12.9504709278437,
40.0772271723538));
#203774=CARTESIAN_POINT('Ctrl Pts',(-61.5434299552079,-12.7836101409426,
40.0045995998162));
#203775=CARTESIAN_POINT('Ctrl Pts',(-61.5018471007596,-12.8662000075461,
39.9663485808315));
#203776=CARTESIAN_POINT('Ctrl Pts',(-61.4139027244671,-12.8749747009095,
40.0101727202465));
#203777=CARTESIAN_POINT('Ctrl Pts',(-61.5035207735036,-12.7478263086951,
39.9304654349859));
#203778=CARTESIAN_POINT('Ctrl Pts',(-61.465297106342,-12.8544221781231,
39.9051900162958));
#203779=CARTESIAN_POINT('Ctrl Pts',(-61.3716536946531,-12.8501918100166,
39.9671857458182));
#203780=CARTESIAN_POINT('Ctrl Pts',(-61.4590390555209,-12.7383709431247,
39.8576902534424));
#203781=CARTESIAN_POINT('Ctrl Pts',(-61.43297545991,-12.8632261535951,39.8573998014387));
#203782=CARTESIAN_POINT('Ctrl Pts',(-61.3271735965894,-12.8407372733094,
39.92499));
#203783=CARTESIAN_POINT('Origin',(-61.4762657165316,-13.0516031943525,40.22725));
#203784=CARTESIAN_POINT('Origin',(-0.0660119618346311,0.310561863232984,
39.116));
#203785=CARTESIAN_POINT('Origin',(-58.7584778814677,-12.1649068885788,39.116));
#203786=CARTESIAN_POINT('Origin',(1.31078692950416E-16,3.42824740397342E-17,
40.22725));
#203787=CARTESIAN_POINT('Origin',(-61.4699285681955,-13.0814171332228,40.22725));
#203788=CARTESIAN_POINT('Ctrl Pts',(-58.7584778814677,-12.1649068885788,
38.989));
#203789=CARTESIAN_POINT('Ctrl Pts',(-58.732033541174,-12.28931772815,38.989));
#203790=CARTESIAN_POINT('Ctrl Pts',(-58.7320731263175,-12.2891314946918,
39.1161901092323));
#203791=CARTESIAN_POINT('Ctrl Pts',(-58.5461948427484,-12.1200194799672,
38.989));
#203792=CARTESIAN_POINT('Ctrl Pts',(-58.5199849720729,-12.2442448876955,
38.989229898976));
#203793=CARTESIAN_POINT('Ctrl Pts',(-58.5623471386685,-12.2530551225939,
39.1161900493202));
#203794=CARTESIAN_POINT('Ctrl Pts',(-58.3441042111266,-12.0772896710131,
39.1034966344368));
#203795=CARTESIAN_POINT('Ctrl Pts',(-58.3180679977598,-12.201325600148,
39.1038314102561));
#203796=CARTESIAN_POINT('Ctrl Pts',(-58.4007711908102,-12.2187110949215,
39.2077528789599));
#203797=CARTESIAN_POINT('Ctrl Pts',(-58.2316113004782,-12.0535047649318,
39.2875012672119));
#203798=CARTESIAN_POINT('Ctrl Pts',(-58.2057612725768,-12.1774537884111,
39.2878045257868));
#203799=CARTESIAN_POINT('Ctrl Pts',(-58.3108302909895,-12.1995935666434,
39.3549015295899));
#203800=CARTESIAN_POINT('Origin',(-58.3370777047235,-12.0753355159229,39.3548010137695));
#203801=CARTESIAN_POINT('Ctrl Pts',(-61.3267881959114,-13.3605623192483,
39.8576902534424));
#203802=CARTESIAN_POINT('Ctrl Pts',(-61.3537611057084,-13.2359003894747,
39.8573998014387));
#203803=CARTESIAN_POINT('Ctrl Pts',(-61.2479592423879,-13.213411509189,
39.92499));
#203804=CARTESIAN_POINT('Ctrl Pts',(-61.3712903180782,-13.370021038423,
39.9304984902492));
#203805=CARTESIAN_POINT('Ctrl Pts',(-61.3797222373792,-13.2571016411956,
39.9052171569788));
#203806=CARTESIAN_POINT('Ctrl Pts',(-61.2924596082469,-13.2228703539491,
39.96720497266));
#203807=CARTESIAN_POINT('Ctrl Pts',(-61.4221282572889,-13.3535190881769,
40.0043437678661));
#203808=CARTESIAN_POINT('Ctrl Pts',(-61.4177900459394,-13.26109997677,39.966162857764));
#203809=CARTESIAN_POINT('Ctrl Pts',(-61.3409599630868,-13.2173727427872,
40.0100243556234));
#203810=CARTESIAN_POINT('Ctrl Pts',(-61.514877095365,-13.2651598666396,
40.1194874821989));
#203811=CARTESIAN_POINT('Ctrl Pts',(-61.4899829268154,-13.2123479779266,
40.0627551483143));
#203812=CARTESIAN_POINT('Ctrl Pts',(-61.4244514636294,-13.1725625528864,
40.0767884282378));
#203813=CARTESIAN_POINT('Ctrl Pts',(-61.5568698122754,-13.1903059833733,
40.1599502015386));
#203814=CARTESIAN_POINT('Ctrl Pts',(-61.5253695547376,-13.1590895168684,
40.100244945386));
#203815=CARTESIAN_POINT('Ctrl Pts',(-61.4592680512438,-13.1314678292773,
40.10025));
#203816=CARTESIAN_POINT('Ctrl Pts',(-61.5752716937452,-13.1038352065724,
40.1599502534424));
#203817=CARTESIAN_POINT('Ctrl Pts',(-61.5387839176329,-13.0960702419676,
40.10025));
#203818=CARTESIAN_POINT('Ctrl Pts',(-61.4699285681955,-13.0814171332229,
40.10025));
#203819=CARTESIAN_POINT('Origin',(-61.221554457654,-13.3376362544822,39.92499));
#203820=CARTESIAN_POINT('Origin',(-58.1628213392047,-12.038296182048,39.6398955069332));
#203821=CARTESIAN_POINT('Origin',(-57.988564973546,-12.0012568480856,39.92499));
#203822=CARTESIAN_POINT('Origin',(-61.0472983318727,-13.3005969715127,39.6398955068272));
#203823=CARTESIAN_POINT('Origin',(-60.8730422059014,-13.2635576885498,39.3548010137695));
#203824=CARTESIAN_POINT('Ctrl Pts',(-57.8830978693156,-11.9794294790609,
39.8576902534424));
#203825=CARTESIAN_POINT('Ctrl Pts',(-57.8572899778512,-12.1031907419153,
39.8579948730704));
#203826=CARTESIAN_POINT('Ctrl Pts',(-57.9621601888121,-12.1254815933788,
39.92499));
#203827=CARTESIAN_POINT('Ctrl Pts',(-57.8386546085357,-11.9699833161083,
39.930402071123));
#203828=CARTESIAN_POINT('Ctrl Pts',(-57.8310944294263,-12.0820882677187,
39.9058915297384));
#203829=CARTESIAN_POINT('Ctrl Pts',(-57.9177151970035,-12.1160345187365,
39.9671523786037));
#203830=CARTESIAN_POINT('Ctrl Pts',(-57.7880992891175,-11.9864204851027,
40.0043257306694));
#203831=CARTESIAN_POINT('Ctrl Pts',(-57.7929810340972,-12.0782959991608,
39.9667894847838));
#203832=CARTESIAN_POINT('Ctrl Pts',(-57.8694789541063,-12.1215717318492,
40.0100138975201));
#203833=CARTESIAN_POINT('Ctrl Pts',(-57.6961636462598,-12.0746725352386,
40.1195533054856));
#203834=CARTESIAN_POINT('Ctrl Pts',(-57.7211944343232,-12.1272484490377,
40.0630813209234));
#203835=CARTESIAN_POINT('Ctrl Pts',(-57.7867317752136,-12.1665991704021,
40.0768265942419));
#203836=CARTESIAN_POINT('Ctrl Pts',(-57.6547178110643,-12.1494120604578,
40.1599502027525));
#203837=CARTESIAN_POINT('Ctrl Pts',(-57.6862546895618,-12.1804827566582,
40.1002552791553));
#203838=CARTESIAN_POINT('Ctrl Pts',(-57.7524075778586,-12.2078361528629,
40.10025));
#203839=CARTESIAN_POINT('Ctrl Pts',(-57.6364522029208,-12.2354540642041,
40.1599502534424));
#203840=CARTESIAN_POINT('Ctrl Pts',(-57.6729438621907,-12.2432007592844,
40.10025));
#203841=CARTESIAN_POINT('Ctrl Pts',(-57.7418065394566,-12.2578193919764,
40.10025));
#203842=CARTESIAN_POINT('Origin',(-57.7418065394566,-12.2578193919764,40.22725));
#203843=CARTESIAN_POINT('Ctrl Pts',(-60.451642460649,-13.1739864076103,
38.989));
#203844=CARTESIAN_POINT('Ctrl Pts',(-60.478086695185,-13.0495760655901,
38.989));
#203845=CARTESIAN_POINT('Ctrl Pts',(-60.478047215957,-13.0497618007546,
39.1161896013266));
#203846=CARTESIAN_POINT('Ctrl Pts',(-60.6638314094602,-13.2193162256447,
38.989));
#203847=CARTESIAN_POINT('Ctrl Pts',(-60.6905041359633,-13.0947262769507,
38.988776927546));
#203848=CARTESIAN_POINT('Ctrl Pts',(-60.6477728389708,-13.0858380958632,
39.1161898821847));
#203849=CARTESIAN_POINT('Ctrl Pts',(-60.8658323498479,-13.2624673401139,
39.1034967087243));
#203850=CARTESIAN_POINT('Ctrl Pts',(-60.8926693037164,-13.1376973240559,
39.1031720232711));
#203851=CARTESIAN_POINT('Ctrl Pts',(-60.8093487091498,-13.1201821075162,
39.2077529614998));
#203852=CARTESIAN_POINT('Ctrl Pts',(-60.9782752797349,-13.2864868028992,
39.2875012672119));
#203853=CARTESIAN_POINT('Ctrl Pts',(-61.0052918407716,-13.1616357172824,
39.2872087095508));
#203854=CARTESIAN_POINT('Ctrl Pts',(-60.8992893450419,-13.1392995799683,
39.3549017048227));
#203855=CARTESIAN_POINT('Origin',(-60.451642460649,-13.1739864076103,39.116));
#203856=CARTESIAN_POINT('Origin',(3.54593577968597E-16,-1.21955273767077E-17,
40.22725));
#203857=CARTESIAN_POINT('Origin',(-57.7354693911205,-12.2876333308468,40.22725));
#203858=CARTESIAN_POINT('Origin',(59.5987607253196,12.3435145206982,39.116));
#203859=CARTESIAN_POINT('Origin',(-60.0590486699117,-13.0905908661169,39.1160373285254));
#203860=CARTESIAN_POINT('Ctrl Pts',(-57.6301266171958,-12.2652136052657,
40.1599502534424));
#203861=CARTESIAN_POINT('Ctrl Pts',(-57.6666142715156,-12.2729791421551,
40.10025));
#203862=CARTESIAN_POINT('Ctrl Pts',(-57.7354693911205,-12.2876333308468,
40.10025));
#203863=CARTESIAN_POINT('Ctrl Pts',(-57.6118791634503,-12.3509528635302,
40.1599500566036));
#203864=CARTESIAN_POINT('Ctrl Pts',(-57.6533170557966,-12.3354428975793,
40.100255130536));
#203865=CARTESIAN_POINT('Ctrl Pts',(-57.7248602994014,-12.3374367183504,
40.10025));
#203866=CARTESIAN_POINT('Ctrl Pts',(-57.619017823295,-12.4353658313039,
40.1203070619049));
#203867=CARTESIAN_POINT('Ctrl Pts',(-57.6632723181618,-12.3978675338895,
40.06370986845));
#203868=CARTESIAN_POINT('Ctrl Pts',(-57.7390640345625,-12.3886090227464,
40.0772636213363));
#203869=CARTESIAN_POINT('Ctrl Pts',(-57.6672013517154,-12.5543478197371,
40.00461022458));
#203870=CARTESIAN_POINT('Ctrl Pts',(-57.7090592089829,-12.4724831634111,
39.9670001894012));
#203871=CARTESIAN_POINT('Ctrl Pts',(-57.7965151898611,-12.4639865158418,
40.0101788811209));
#203872=CARTESIAN_POINT('Ctrl Pts',(-57.7068899568908,-12.5899803678811,
39.9303710930188));
#203873=CARTESIAN_POINT('Ctrl Pts',(-57.745578735121,-12.4844838378934,
39.9058663574104));
#203874=CARTESIAN_POINT('Ctrl Pts',(-57.8385197202049,-12.4887127671319,
39.9671344706358));
#203875=CARTESIAN_POINT('Ctrl Pts',(-57.7513140650721,-12.5994235324468,
39.8576902534424));
#203876=CARTESIAN_POINT('Ctrl Pts',(-57.7780756236496,-12.4758649777949,
39.8579948730704));
#203877=CARTESIAN_POINT('Ctrl Pts',(-57.8829458346106,-12.4981558292584,
39.92499));
#203878=CARTESIAN_POINT('Origin',(-57.8565410498767,-12.6223805745516,39.92499));
#203879=CARTESIAN_POINT('Origin',(-60.01579999775,-13.0813452322614,39.1925554488851));
#203880=CARTESIAN_POINT('Origin',(-59.9357500275434,-13.0643300858378,39.3343017080178));
#203881=CARTESIAN_POINT('Origin',(-58.030797415528,-12.6594199084519,39.6398955069206));
#203882=CARTESIAN_POINT('Origin',(-58.2050537810542,-12.6964592423889,39.3548010137695));
#203883=CARTESIAN_POINT('Ctrl Pts',(-59.6130003254556,-12.995727518882,
39.3978017080178));
#203884=CARTESIAN_POINT('Ctrl Pts',(-59.6394051101894,-12.8715027735888,
39.3978017080178));
#203885=CARTESIAN_POINT('Ctrl Pts',(-59.6394051101894,-12.8715027735888,
39.5248017080178));
#203886=CARTESIAN_POINT('Ctrl Pts',(-59.7010925481785,-13.0142126749435,
39.3978017080178));
#203887=CARTESIAN_POINT('Ctrl Pts',(-59.7273659613755,-12.8901994296787,
39.3980355775178));
#203888=CARTESIAN_POINT('Ctrl Pts',(-59.7714687931904,-12.899573775969,
39.5248015517192));
#203889=CARTESIAN_POINT('Ctrl Pts',(-59.7843900000232,-13.0316935695386,
39.3484893995498));
#203890=CARTESIAN_POINT('Ctrl Pts',(-59.810954429825,-12.9079667071265,
39.3489438303421));
#203891=CARTESIAN_POINT('Ctrl Pts',(-59.8963444006333,-12.9261169057235,
39.450833315559));
#203892=CARTESIAN_POINT('Ctrl Pts',(-59.8282880397056,-13.0409063549235,
39.2708017080178));
#203893=CARTESIAN_POINT('Ctrl Pts',(-59.855054532531,-12.9173404733279,
39.2710850691866));
#203894=CARTESIAN_POINT('Ctrl Pts',(-59.9621548122772,-12.9401053405446,
39.3343017080178));
#203895=CARTESIAN_POINT('Origin',(-59.6130003254556,-12.995727518882,39.5248017080178));
#203896=CARTESIAN_POINT('Ctrl Pts',(-58.0998260601481,-12.6735055745737,
39.2875012672119));
#203897=CARTESIAN_POINT('Ctrl Pts',(-58.1266254912132,-12.5497583678825,
39.2878045257519));
#203898=CARTESIAN_POINT('Ctrl Pts',(-58.231615865753,-12.5722680770244,
39.3549015218348));
#203899=CARTESIAN_POINT('Ctrl Pts',(-58.2122693395992,-12.6975323335621,
39.1034938540228));
#203900=CARTESIAN_POINT('Ctrl Pts',(-58.2389340288436,-12.5736300041245,
39.1038286278802));
#203901=CARTESIAN_POINT('Ctrl Pts',(-58.321558127123,-12.5913858949913,
39.2077506434026));
#203902=CARTESIAN_POINT('Ctrl Pts',(-58.4142696920427,-12.7406947165201,
38.989));
#203903=CARTESIAN_POINT('Ctrl Pts',(-58.4408527990799,-12.6165486539543,
38.9892298954605));
#203904=CARTESIAN_POINT('Ctrl Pts',(-58.4831353553018,-12.62573019531,39.1161900347291));
#203905=CARTESIAN_POINT('Ctrl Pts',(-58.6264539577984,-12.7860306150448,
38.989));
#203906=CARTESIAN_POINT('Ctrl Pts',(-58.652898295038,-12.661619789842,38.989));
#203907=CARTESIAN_POINT('Ctrl Pts',(-58.6528587129532,-12.6618060089103,
39.1161900945648));
#203908=CARTESIAN_POINT('Origin',(-58.6264539577984,-12.7860306150448,39.116));
#203909=CARTESIAN_POINT('Origin',(58.1567073854023,12.0369966210207,39.5248017080178));
#203910=CARTESIAN_POINT('Origin',(-59.4650964698967,-12.9642895838867,39.5248017080178));
#203911=CARTESIAN_POINT('Origin',(57.9308881865556,11.9889972685547,39.116));
#203912=CARTESIAN_POINT('Origin',(-59.0190342907425,-12.8695280801153,39.116040271386));
#203913=CARTESIAN_POINT('Ctrl Pts',(-59.249807061628,-12.9191181862042,
39.2708017080178));
#203914=CARTESIAN_POINT('Ctrl Pts',(-59.2768226962999,-12.7944335023704,
39.27051194648));
#203915=CARTESIAN_POINT('Ctrl Pts',(-59.1687514833561,-12.7714622569316,
39.3343017080178));
#203916=CARTESIAN_POINT('Ctrl Pts',(-59.2938540730361,-12.9283593439862,
39.3487519301186));
#203917=CARTESIAN_POINT('Ctrl Pts',(-59.320611599148,-12.8037411209984,
39.3482879463986));
#203918=CARTESIAN_POINT('Ctrl Pts',(-59.2347843016965,-12.7854979657554,
39.4512271261625));
#203919=CARTESIAN_POINT('Ctrl Pts',(-59.3773008374014,-12.9458672564001,
39.3978017080178));
#203920=CARTESIAN_POINT('Ctrl Pts',(-59.4036696715727,-12.8213956592927,
39.3975673827397));
#203921=CARTESIAN_POINT('Ctrl Pts',(-59.3598823995817,-12.8120883873134,
39.5248015355199));
#203922=CARTESIAN_POINT('Ctrl Pts',(-59.4650964698967,-12.9642895838867,
39.3978017080178));
#203923=CARTESIAN_POINT('Ctrl Pts',(-59.4915012546306,-12.8400648385935,
39.3978017080178));
#203924=CARTESIAN_POINT('Ctrl Pts',(-59.4915012546306,-12.8400648385935,
39.5248017080178));
#203925=CARTESIAN_POINT('Origin',(-59.1423466986223,-12.8956870022248,39.3343017080178));
#203926=CARTESIAN_POINT('Origin',(-59.0627741301462,-12.8787733309739,39.1934008533553));
#203927=CARTESIAN_POINT('Origin',(-61.1207756556245,-6.10480350566274,39.1925554495082));
#203928=CARTESIAN_POINT('Origin',(-61.1647646440472,-6.10937495961999,39.1160373285259));
#203929=CARTESIAN_POINT('Origin',(-61.0393856393804,-6.09624906995198,39.3343017080178));
#203930=CARTESIAN_POINT('Ctrl Pts',(-60.9299448846691,-6.0853187813828,
39.2708017080178));
#203931=CARTESIAN_POINT('Ctrl Pts',(-60.9172173747511,-6.21110821942895,
39.2710850691866));
#203932=CARTESIAN_POINT('Ctrl Pts',(-61.0261105245455,-6.22255335066376,
39.3343017080178));
#203933=CARTESIAN_POINT('Ctrl Pts',(-60.885197756147,-6.08049918876655,
39.3487519293518));
#203934=CARTESIAN_POINT('Ctrl Pts',(-60.8722275639182,-6.20637959976686,
39.3492068662932));
#203935=CARTESIAN_POINT('Ctrl Pts',(-60.958972334824,-6.21549684257596,
39.4512271248742));
#203936=CARTESIAN_POINT('Ctrl Pts',(-60.800424540796,-6.07136793516307,
39.3978017080178));
#203937=CARTESIAN_POINT('Ctrl Pts',(-60.7870898478939,-6.19743126523177,
39.3980347781178));
#203938=CARTESIAN_POINT('Ctrl Pts',(-60.8317801127819,-6.20212840134649,
39.524801535519));
#203939=CARTESIAN_POINT('Ctrl Pts',(-60.7112330730304,-6.0617588454153,
39.3978017080178));
#203940=CARTESIAN_POINT('Ctrl Pts',(-60.6979579581954,-6.18806312612707,
39.3978017080178));
#203941=CARTESIAN_POINT('Ctrl Pts',(-60.6979579581954,-6.18806312612707,
39.5248017080178));
#203942=CARTESIAN_POINT('Origin',(-60.7112330730304,-6.0617588454153,39.5248017080178));
#203943=CARTESIAN_POINT('Origin',(-0.0331877870874725,0.315760701779427,
39.116));
#203944=CARTESIAN_POINT('Origin',(-61.5639141665612,-6.15137923967635,39.116));
#203945=CARTESIAN_POINT('Origin',(-0.0331877870874724,0.315760701779427,
39.5248017080178));
#203946=CARTESIAN_POINT('Origin',(-60.5608532912344,-6.04595329345021,39.5248017080178));
#203947=CARTESIAN_POINT('Ctrl Pts',(-62.0995362748659,-6.20712349654423,
39.2875012672119));
#203948=CARTESIAN_POINT('Ctrl Pts',(-62.0866494451786,-6.33421250060381,
39.287208709576));
#203949=CARTESIAN_POINT('Ctrl Pts',(-61.978932842986,-6.32269886887959,
39.3549016990122));
#203950=CARTESIAN_POINT('Ctrl Pts',(-61.9851725366286,-6.19522040634658,
39.1034939173931));
#203951=CARTESIAN_POINT('Ctrl Pts',(-61.9721399414719,-6.32217680516044,
39.1031692336341));
#203952=CARTESIAN_POINT('Ctrl Pts',(-61.8874852020914,-6.31308733464682,
39.2077507202295));
#203953=CARTESIAN_POINT('Ctrl Pts',(-61.7797221753254,-6.17383766261664,
38.989));
#203954=CARTESIAN_POINT('Ctrl Pts',(-61.7665890280543,-6.30057205577826,
38.9887769311176));
#203955=CARTESIAN_POINT('Ctrl Pts',(-61.7232032332924,-6.29582060418315,
39.1161898712914));
#203956=CARTESIAN_POINT('Ctrl Pts',(-61.5639141665612,-6.15137923967635,
38.989));
#203957=CARTESIAN_POINT('Ctrl Pts',(-61.5506192193203,-6.27787221312641,
38.989));
#203958=CARTESIAN_POINT('Ctrl Pts',(-61.5506390665185,-6.27768337964943,
39.1161895903853));
#203959=CARTESIAN_POINT('Origin',(-61.9923681882669,-6.19641157197423,39.3548010137695));
#203960=CARTESIAN_POINT('Ctrl Pts',(-60.5608532912344,-6.04595329345021,
39.3978017080178));
#203961=CARTESIAN_POINT('Ctrl Pts',(-60.5475781763994,-6.17225757416198,
39.3978017080178));
#203962=CARTESIAN_POINT('Ctrl Pts',(-60.5475781763994,-6.17225757416198,
39.5248017080178));
#203963=CARTESIAN_POINT('Ctrl Pts',(-60.4713604300108,-6.03631114775,39.3978017080178));
#203964=CARTESIAN_POINT('Ctrl Pts',(-60.4579746647643,-6.16283986559456,
39.397566602504));
#203965=CARTESIAN_POINT('Ctrl Pts',(-60.4133037213016,-6.15814476024322,
39.5248015517196));
#203966=CARTESIAN_POINT('Ctrl Pts',(-60.3867383361559,-6.02719193013317,
39.3484894016717));
#203967=CARTESIAN_POINT('Ctrl Pts',(-60.3736778173763,-6.15397990991425,
39.3480259000034));
#203968=CARTESIAN_POINT('Ctrl Pts',(-60.2863376507179,-6.14480008848983,
39.4508333188934));
#203969=CARTESIAN_POINT('Ctrl Pts',(-60.3421421670675,-6.02238575970236,
39.2708017080178));
#203970=CARTESIAN_POINT('Ctrl Pts',(-60.3293058762212,-6.14931623097207,
39.2705119464801));
#203971=CARTESIAN_POINT('Ctrl Pts',(-60.2194255397045,-6.13776734223176,
39.3343017080178));
#203972=CARTESIAN_POINT('Origin',(-60.2327006545395,-6.01146306151998,39.3343017080178));
#203973=CARTESIAN_POINT('Origin',(-62.1695413802841,-6.21503322485303,39.6398955068191));
#203974=CARTESIAN_POINT('Origin',(-62.3467145720969,-6.23365487766584,39.92499));
#203975=CARTESIAN_POINT('Origin',(-60.1517960317849,-6.00295964302187,39.1934008539946));
#203976=CARTESIAN_POINT('Origin',(-60.1073400339997,-5.9982360452005,39.116040271385));
#203977=CARTESIAN_POINT('Ctrl Pts',(-62.6108711573006,-6.56531752495261,
40.1599502534424));
#203978=CARTESIAN_POINT('Ctrl Pts',(-62.5737697140402,-6.56142710223311,
40.10025));
#203979=CARTESIAN_POINT('Ctrl Pts',(-62.5037563256535,-6.55408556365905,
40.10025));
#203980=CARTESIAN_POINT('Ctrl Pts',(-62.6200603487601,-6.47768259609045,
40.159950053846));
#203981=CARTESIAN_POINT('Ctrl Pts',(-62.5804601312005,-6.49759225479912,
40.100244835349));
#203982=CARTESIAN_POINT('Ctrl Pts',(-62.5090664195363,-6.50335812634718,
40.10025));
#203983=CARTESIAN_POINT('Ctrl Pts',(-62.603659837329,-6.39420891953715,
40.1202442001038));
#203984=CARTESIAN_POINT('Ctrl Pts',(-62.5636211788254,-6.43639040357905,
40.0633873868018));
#203985=CARTESIAN_POINT('Ctrl Pts',(-62.4890871199581,-6.45393802799988,
40.0772271723538));
#203986=CARTESIAN_POINT('Ctrl Pts',(-62.5425397295636,-6.28054002958106,
40.0045995998164));
#203987=CARTESIAN_POINT('Ctrl Pts',(-62.5098176621807,-6.36702405212743,
39.9663485808315));
#203988=CARTESIAN_POINT('Ctrl Pts',(-62.423272259596,-6.38494336730939,
40.0101727202466));
#203989=CARTESIAN_POINT('Ctrl Pts',(-62.4991087455376,-6.24912387034439,
39.9304654349858));
#203990=CARTESIAN_POINT('Ctrl Pts',(-62.4722367740483,-6.35913125763767,
39.9051900162948));
#203991=CARTESIAN_POINT('Ctrl Pts',(-62.3786641568876,-6.36471246584688,
39.9671857458179));
#203992=CARTESIAN_POINT('Ctrl Pts',(-62.4538823482276,-6.24436990788019,
39.8576902534424));
#203993=CARTESIAN_POINT('Ctrl Pts',(-62.4410124550019,-6.37126553604029,
39.8573998014388));
#203994=CARTESIAN_POINT('Ctrl Pts',(-62.3334394572619,-6.35995915837761,
39.92499));
#203995=CARTESIAN_POINT('Origin',(-62.5037563256535,-6.55408556365905,40.22725));
#203996=CARTESIAN_POINT('Origin',(-0.0331877870874725,0.315760701779427,
39.116));
#203997=CARTESIAN_POINT('Origin',(-59.7081718144893,-5.95633285891171,39.116));
#203998=CARTESIAN_POINT('Origin',(1.33778643725276E-16,1.72356557454365E-17,
40.22725));
#203999=CARTESIAN_POINT('Origin',(-62.5005702980931,-6.58439859102987,40.22725));
#204000=CARTESIAN_POINT('Ctrl Pts',(-59.7081718144893,-5.95633285891171,
38.989));
#204001=CARTESIAN_POINT('Ctrl Pts',(-59.6948768129328,-6.08282634913946,
38.989));
#204002=CARTESIAN_POINT('Ctrl Pts',(-59.6948967145276,-6.08263699811343,
39.1161901092322));
#204003=CARTESIAN_POINT('Ctrl Pts',(-59.4923596726254,-5.93388096803599,
38.989));
#204004=CARTESIAN_POINT('Ctrl Pts',(-59.4792784733316,-6.06016553348717,
38.989229898976));
#204005=CARTESIAN_POINT('Ctrl Pts',(-59.5223294958616,-6.0644994528221,
39.1161900493202));
#204006=CARTESIAN_POINT('Ctrl Pts',(-59.286909633363,-5.91250946061102,
39.1034966344368));
#204007=CARTESIAN_POINT('Ctrl Pts',(-59.2739813341608,-6.03858743332049,
39.1038314102564));
#204008=CARTESIAN_POINT('Ctrl Pts',(-59.3580487495174,-6.04723285085744,
39.20775287896));
#204009=CARTESIAN_POINT('Ctrl Pts',(-59.1725467709678,-5.90061356181218,
39.2875012672119));
#204010=CARTESIAN_POINT('Ctrl Pts',(-59.1597945531718,-6.02658564326377,
39.2878045257868));
#204011=CARTESIAN_POINT('Ctrl Pts',(-59.2666022295037,-6.03762143444266,
39.3549015295899));
#204012=CARTESIAN_POINT('Origin',(-59.2797173540686,-5.91130048050303,39.3548010137695));
#204013=CARTESIAN_POINT('Ctrl Pts',(-62.3873926810692,-6.87697683366523,
39.8576902534424));
#204014=CARTESIAN_POINT('Ctrl Pts',(-62.4011871104969,-6.7501783781756,
39.8573998014387));
#204015=CARTESIAN_POINT('Ctrl Pts',(-62.293614112757,-6.73887200051292,
39.92499));
#204016=CARTESIAN_POINT('Ctrl Pts',(-62.4326397213343,-6.88173199854445,
39.9304984902493));
#204017=CARTESIAN_POINT('Ctrl Pts',(-62.4292221586313,-6.76854981002466,
39.9052171569797));
#204018=CARTESIAN_POINT('Ctrl Pts',(-62.3388594194626,-6.74362747387357,
39.9672049726606));
#204019=CARTESIAN_POINT('Ctrl Pts',(-62.4814742414945,-6.86000643604701,
40.004343767866));
#204020=CARTESIAN_POINT('Ctrl Pts',(-62.4674993676288,-6.768547072768,39.9661628577639));
#204021=CARTESIAN_POINT('Ctrl Pts',(-62.3865194274374,-6.73309031164153,
40.0100243556234));
#204022=CARTESIAN_POINT('Ctrl Pts',(-62.5644789380885,-6.76243636205646,
40.1194874821989));
#204023=CARTESIAN_POINT('Ctrl Pts',(-62.5342007968293,-6.71251593157857,
40.0627551483143));
#204024=CARTESIAN_POINT('Ctrl Pts',(-62.4648696125158,-6.679798358402,40.0767884282379));
#204025=CARTESIAN_POINT('Ctrl Pts',(-62.5984172531147,-6.68360310202781,
40.1599502015393));
#204026=CARTESIAN_POINT('Ctrl Pts',(-62.563826548014,-6.65585031610596,
40.1002449453885));
#204027=CARTESIAN_POINT('Ctrl Pts',(-62.4951999029147,-6.63528943158931,
40.10025));
#204028=CARTESIAN_POINT('Ctrl Pts',(-62.6076796697355,-6.59568250079845,
40.1599502534424));
#204029=CARTESIAN_POINT('Ctrl Pts',(-62.570580117661,-6.59177408464733,
40.10025));
#204030=CARTESIAN_POINT('Ctrl Pts',(-62.5005702980931,-6.58439859102987,
40.10025));
#204031=CARTESIAN_POINT('Origin',(-62.280338997922,-6.86517628122469,39.92499));
#204032=CARTESIAN_POINT('Origin',(-59.1025439185015,-5.89267880207714,39.6398955069327));
#204033=CARTESIAN_POINT('Origin',(-58.925370482788,-5.8740571235783,39.92499));
#204034=CARTESIAN_POINT('Origin',(-62.1031658061012,-6.84655462836385,39.6398955068272));
#204035=CARTESIAN_POINT('Origin',(-61.925992614092,-6.82793297553308,39.3548010137695));
#204036=CARTESIAN_POINT('Ctrl Pts',(-58.8181995570485,-5.86337364149541,
39.8576902534424));
#204037=CARTESIAN_POINT('Ctrl Pts',(-58.8054696185321,-5.98915458643755,
39.8579948730704));
#204038=CARTESIAN_POINT('Ctrl Pts',(-58.912095367953,-6.00036140429007,
39.92499));
#204039=CARTESIAN_POINT('Ctrl Pts',(-58.773012368204,-5.8586248113641,39.9304020711231));
#204040=CARTESIAN_POINT('Ctrl Pts',(-58.7772117628631,-5.97090589422308,
39.9058915297379));
#204041=CARTESIAN_POINT('Ctrl Pts',(-58.8669063622643,-5.99561184840474,
39.967152378603));
#204042=CARTESIAN_POINT('Ctrl Pts',(-58.7244521481309,-5.88025640567524,
40.0043257306693));
#204043=CARTESIAN_POINT('Ctrl Pts',(-58.7389107566976,-5.9711183347532,
39.9667894847842));
#204044=CARTESIAN_POINT('Ctrl Pts',(-58.8195131589313,-6.00616078842852,
40.01001389752));
#204045=CARTESIAN_POINT('Ctrl Pts',(-58.6422449895249,-5.97763489331421,
40.1195533054857));
#204046=CARTESIAN_POINT('Ctrl Pts',(-58.6726343357863,-6.02730636094608,
40.0630813209231));
#204047=CARTESIAN_POINT('Ctrl Pts',(-58.7419259266988,-6.05959099741128,
40.076826594242));
#204048=CARTESIAN_POINT('Ctrl Pts',(-58.6088386066675,-6.05629725705572,
40.1599502027529));
#204049=CARTESIAN_POINT('Ctrl Pts',(-58.6434504949707,-6.08390124328546,
40.1002552791553));
#204050=CARTESIAN_POINT('Ctrl Pts',(-58.7121001992953,-6.10418993496979,
40.10025));
#204051=CARTESIAN_POINT('Ctrl Pts',(-58.5996668978649,-6.14377718965283,
40.1599502534424));
#204052=CARTESIAN_POINT('Ctrl Pts',(-58.6367684021393,-6.14766703046132,
40.10025));
#204053=CARTESIAN_POINT('Ctrl Pts',(-58.7067819056643,-6.15500747092277,
40.10025));
#204054=CARTESIAN_POINT('Origin',(-58.7067819056643,-6.15500747092277,40.22725));
#204055=CARTESIAN_POINT('Ctrl Pts',(-61.4975385923863,-6.7829006432352,
38.989));
#204056=CARTESIAN_POINT('Ctrl Pts',(-61.5108335407726,-6.6564076588874,
38.989));
#204057=CARTESIAN_POINT('Ctrl Pts',(-61.5108136924273,-6.65659650327836,
39.1161896013267));
#204058=CARTESIAN_POINT('Ctrl Pts',(-61.7133034041536,-6.80580235504166,
38.989));
#204059=CARTESIAN_POINT('Ctrl Pts',(-61.7268068187953,-6.67910686401061,
38.988776927546));
#204060=CARTESIAN_POINT('Ctrl Pts',(-61.6833805404074,-6.67473401011687,
39.1161898821849));
#204061=CARTESIAN_POINT('Ctrl Pts',(-61.9187082819379,-6.82760223531334,
39.1034967087243));
#204062=CARTESIAN_POINT('Ctrl Pts',(-61.9323562021234,-6.70071049691222,
39.1031720232715));
#204063=CARTESIAN_POINT('Ctrl Pts',(-61.8476612078244,-6.69200060426958,
39.2077529615));
#204064=CARTESIAN_POINT('Ctrl Pts',(-62.0330459552233,-6.83973663030219,
39.2875012672119));
#204065=CARTESIAN_POINT('Ctrl Pts',(-62.046864024595,-6.71274549238769,
39.2872087095508));
#204066=CARTESIAN_POINT('Ctrl Pts',(-61.9391074595192,-6.70161199275219,
39.3549017048228));
#204067=CARTESIAN_POINT('Origin',(-61.4975385923863,-6.7829006432352,39.116));
#204068=CARTESIAN_POINT('Origin',(3.53633106925806E-16,-6.13135187546137E-18,
40.22725));
#204069=CARTESIAN_POINT('Origin',(-58.7035958781039,-6.1853204982936,40.22725));
#204070=CARTESIAN_POINT('Origin',(61.5757885448748,6.15262728712825,39.116));
#204071=CARTESIAN_POINT('Origin',(-61.0983782637168,-6.74099917687867,39.1160373285262));
#204072=CARTESIAN_POINT('Ctrl Pts',(-58.5964866834551,-6.17403490858981,
40.1599502534424));
#204073=CARTESIAN_POINT('Ctrl Pts',(-58.6335861742242,-6.17794390662133,
40.10025));
#204074=CARTESIAN_POINT('Ctrl Pts',(-58.7035958781039,-6.1853204982936,
40.10025));
#204075=CARTESIAN_POINT('Ctrl Pts',(-58.5873013840787,-6.26121185652503,
40.1599500566034));
#204076=CARTESIAN_POINT('Ctrl Pts',(-58.6268910424087,-6.24145541658243,
40.1002551305363));
#204077=CARTESIAN_POINT('Ctrl Pts',(-58.6982507756617,-6.23596000968369,
40.10025));
#204078=CARTESIAN_POINT('Ctrl Pts',(-58.603224495399,-6.34441620808569,
40.1203070619047));
#204079=CARTESIAN_POINT('Ctrl Pts',(-58.6433169201088,-6.30249747592687,
40.06370986845));
#204080=CARTESIAN_POINT('Ctrl Pts',(-58.7177256636152,-6.28536729223281,
40.0772636213363));
#204081=CARTESIAN_POINT('Ctrl Pts',(-58.6635810738165,-6.45770985055632,
40.0046102245801));
#204082=CARTESIAN_POINT('Ctrl Pts',(-58.6966524426403,-6.37191831988744,
39.9670001894012));
#204083=CARTESIAN_POINT('Ctrl Pts',(-58.7827411889911,-6.35432657855775,
40.0101788811209));
#204084=CARTESIAN_POINT('Ctrl Pts',(-58.7067768761601,-6.4889986109649,
39.9303710930187));
#204085=CARTESIAN_POINT('Ctrl Pts',(-58.7342263230564,-6.38003592347196,
39.9058663574113));
#204086=CARTESIAN_POINT('Ctrl Pts',(-58.8271002111743,-6.37452670784926,
39.967134470637));
#204087=CARTESIAN_POINT('Ctrl Pts',(-58.7519447039089,-6.49374646112702,
39.8576902534424));
#204088=CARTESIAN_POINT('Ctrl Pts',(-58.7656442740271,-6.36806742857287,
39.8579948730703));
#204089=CARTESIAN_POINT('Ctrl Pts',(-58.8722700234481,-6.37927424642539,
39.92499));
#204090=CARTESIAN_POINT('Origin',(-58.8589949086131,-6.50557852713716,39.92499));
#204091=CARTESIAN_POINT('Origin',(-61.054400080406,-6.73632490881056,39.1925554488841));
#204092=CARTESIAN_POINT('Origin',(-60.9730100652055,-6.72777047351084,39.3343017080178));
#204093=CARTESIAN_POINT('Origin',(-59.0361683443172,-6.52420020557848,39.6398955069231));
#204094=CARTESIAN_POINT('Origin',(-59.2133417798937,-6.54282188406189,39.3548010137695));
#204095=CARTESIAN_POINT('Ctrl Pts',(-60.6448574988555,-6.69328024897415,
39.3978017080178));
#204096=CARTESIAN_POINT('Ctrl Pts',(-60.6581326136904,-6.56697596826238,
39.3978017080178));
#204097=CARTESIAN_POINT('Ctrl Pts',(-60.6581326136904,-6.56697596826238,
39.5248017080178));
#204098=CARTESIAN_POINT('Ctrl Pts',(-60.7343993681214,-6.70245599674926,
39.3978017080178));
#204099=CARTESIAN_POINT('Ctrl Pts',(-60.7475659388568,-6.57637578951094,
39.3980355775196));
#204100=CARTESIAN_POINT('Ctrl Pts',(-60.7924070567575,-6.58108878091667,
39.5248015517192));
#204101=CARTESIAN_POINT('Ctrl Pts',(-60.819067758858,-6.71113417453915,
39.3484893995498));
#204102=CARTESIAN_POINT('Ctrl Pts',(-60.8325536871445,-6.58530836180368,
39.3489438303417));
#204103=CARTESIAN_POINT('Ctrl Pts',(-60.919373095124,-6.59443344928389,
39.4508333155595));
#204104=CARTESIAN_POINT('Ctrl Pts',(-60.8636883187845,-6.7157078966937,
39.2708017080178));
#204105=CARTESIAN_POINT('Ctrl Pts',(-60.8773920302461,-6.59002106156426,
39.2710850691866));
#204106=CARTESIAN_POINT('Ctrl Pts',(-60.9862851800405,-6.60146619279907,
39.3343017080178));
#204107=CARTESIAN_POINT('Origin',(-60.6448574988555,-6.69328024897415,39.5248017080178));
#204108=CARTESIAN_POINT('Ctrl Pts',(-59.1062911958297,-6.53099325080016,
39.2875012672119));
#204109=CARTESIAN_POINT('Ctrl Pts',(-59.1200087114582,-6.40512264090962,
39.2878045257519));
#204110=CARTESIAN_POINT('Ctrl Pts',(-59.2267768430461,-6.41653455700086,
39.3549015218348));
#204111=CARTESIAN_POINT('Ctrl Pts',(-59.2206299794252,-6.54313486548303,
39.1034938540228));
#204112=CARTESIAN_POINT('Ctrl Pts',(-59.2341972766252,-6.41712406698078,
39.103828627881));
#204113=CARTESIAN_POINT('Ctrl Pts',(-59.318224747433,-6.42614611919703,
39.2077506434031));
#204114=CARTESIAN_POINT('Ctrl Pts',(-59.426035450364,-6.56494601397012,
38.989));
#204115=CARTESIAN_POINT('Ctrl Pts',(-59.4394961352152,-6.43870134519683,
38.9892298954611));
#204116=CARTESIAN_POINT('Ctrl Pts',(-59.4825067955799,-6.44341285848409,
39.1161900347289));
#204117=CARTESIAN_POINT('Ctrl Pts',(-59.6417962403143,-6.58785426247057,
38.989));
#204118=CARTESIAN_POINT('Ctrl Pts',(-59.6550912403353,-6.46136078685196,
38.989));
#204119=CARTESIAN_POINT('Ctrl Pts',(-59.6550713402783,-6.46155012324701,
39.1161900945646));
#204120=CARTESIAN_POINT('Origin',(-59.6417962403143,-6.58785426247057,39.116));
#204121=CARTESIAN_POINT('Origin',(60.0850508448142,5.99594444118168,39.5248017080178));
#204122=CARTESIAN_POINT('Origin',(-60.4944777170594,-6.67747469700906,39.5248017080178));
#204123=CARTESIAN_POINT('Origin',(59.8516078896891,5.9714085979051,39.116));
#204124=CARTESIAN_POINT('Origin',(-60.0409538388299,-6.62985850077773,39.1160402713847));
#204125=CARTESIAN_POINT('Ctrl Pts',(-60.2756459899119,-6.65505462397356,
39.2708017080178));
#204126=CARTESIAN_POINT('Ctrl Pts',(-60.2894805317162,-6.52822907310738,
39.2705119464801));
#204127=CARTESIAN_POINT('Ctrl Pts',(-60.1796001951996,-6.51668018436707,
39.3343017080178));
#204128=CARTESIAN_POINT('Ctrl Pts',(-60.3204176712045,-6.65964099131245,
39.3487519301186));
#204129=CARTESIAN_POINT('Ctrl Pts',(-60.3340024654448,-6.53290851690434,
39.3482879463971));
#204130=CARTESIAN_POINT('Ctrl Pts',(-60.2467384099268,-6.52373669508308,
39.4512271261623));
#204131=CARTESIAN_POINT('Ctrl Pts',(-60.4052373806432,-6.66833043150608,
39.3978017080178));
#204132=CARTESIAN_POINT('Ctrl Pts',(-60.4184509388156,-6.54178440911727,
39.3975673827415));
#204133=CARTESIAN_POINT('Ctrl Pts',(-60.3739306632446,-6.53710513959975,
39.5248015355199));
#204134=CARTESIAN_POINT('Ctrl Pts',(-60.4944777170594,-6.67747469700906,
39.3978017080178));
#204135=CARTESIAN_POINT('Ctrl Pts',(-60.5077528318944,-6.55117041629729,
39.3978017080178));
#204136=CARTESIAN_POINT('Ctrl Pts',(-60.5077528318944,-6.55117041629729,
39.5248017080178));
#204137=CARTESIAN_POINT('Origin',(-60.1663250803646,-6.64298446507884,39.3343017080178));
#204138=CARTESIAN_POINT('Origin',(-60.0854204586811,-6.63448104699053,39.1934008533548));
#204139=CARTESIAN_POINT('Origin',(-61.4240753804085,0.317499999705897,39.1925554495081));
#204140=CARTESIAN_POINT('Origin',(-61.4683012396063,0.317551690012599,39.1160373285251));
#204141=CARTESIAN_POINT('Origin',(-61.3422370451705,0.3175,39.3343017080178));
#204142=CARTESIAN_POINT('Ctrl Pts',(-61.2322532920972,0.316930737395914,
39.2708017080178));
#204143=CARTESIAN_POINT('Ctrl Pts',(-61.2327440814645,0.1905,39.2710850691866));
#204144=CARTESIAN_POINT('Ctrl Pts',(-61.3422370451705,0.1905,39.3343017080178));
#204145=CARTESIAN_POINT('Ctrl Pts',(-61.1872475084174,0.317046579199636,
39.3487519293518));
#204146=CARTESIAN_POINT('Ctrl Pts',(-61.1875064541755,0.190499999998394,
39.349206866293));
#204147=CARTESIAN_POINT('Ctrl Pts',(-61.274729039531,0.1905,39.4512271248743));
#204148=CARTESIAN_POINT('Ctrl Pts',(-61.1019842137032,0.317266596913493,
39.3978017080178));
#204149=CARTESIAN_POINT('Ctrl Pts',(-61.1018997758111,0.190499999999993,
39.3980347781178));
#204150=CARTESIAN_POINT('Ctrl Pts',(-61.1468362071712,0.1905,39.524801535519));
#204151=CARTESIAN_POINT('Ctrl Pts',(-61.0122769227456,0.3175,39.3978017080178));
#204152=CARTESIAN_POINT('Ctrl Pts',(-61.0122769227456,0.1905,39.3978017080178));
#204153=CARTESIAN_POINT('Ctrl Pts',(-61.0122769227456,0.1905,39.5248017080178));
#204154=CARTESIAN_POINT('Origin',(-61.0122769227456,0.3175,39.5248017080178));
#204155=CARTESIAN_POINT('Origin',(5.50819412990574E-15,0.3175,39.116));
#204156=CARTESIAN_POINT('Origin',(-61.8696548221181,0.3175,39.116));
#204157=CARTESIAN_POINT('Origin',(5.56576032196012E-15,0.3175,39.5248017080178));
#204158=CARTESIAN_POINT('Origin',(-60.8610688070707,0.3175,39.5248017080178));
#204159=CARTESIAN_POINT('Ctrl Pts',(-62.4081695979768,0.318048871877129,
39.2875012672119));
#204160=CARTESIAN_POINT('Ctrl Pts',(-62.4086377819835,0.190309034175427,
39.287208709576));
#204161=CARTESIAN_POINT('Ctrl Pts',(-62.3003077603772,0.190500142125054,
39.3549016990124));
#204162=CARTESIAN_POINT('Ctrl Pts',(-62.2931881445371,0.317932489889954,
39.1034939173931));
#204163=CARTESIAN_POINT('Ctrl Pts',(-62.2934975005749,0.190309294367765,
39.1031692336328));
#204164=CARTESIAN_POINT('Ctrl Pts',(-62.2083564003268,0.190500141995467,
39.2077507202292));
#204165=CARTESIAN_POINT('Ctrl Pts',(-62.0866281564672,0.317722686167411,
38.989));
#204166=CARTESIAN_POINT('Ctrl Pts',(-62.0868143053079,0.190309769569793,
38.9887769311176));
#204167=CARTESIAN_POINT('Ctrl Pts',(-62.0431695205376,0.190500141761866,
39.1161898712917));
#204168=CARTESIAN_POINT('Ctrl Pts',(-61.8696548221181,0.3175,38.989));
#204169=CARTESIAN_POINT('Ctrl Pts',(-61.8696548221181,0.190310267889066,
38.989));
#204170=CARTESIAN_POINT('Ctrl Pts',(-61.8696548221181,0.190500141513915,
39.1161895903856));
#204171=CARTESIAN_POINT('Origin',(-62.3004688883554,0.3175,39.3548010137695));
#204172=CARTESIAN_POINT('Ctrl Pts',(-60.8610688070707,0.3175,39.3978017080178));
#204173=CARTESIAN_POINT('Ctrl Pts',(-60.8610688070707,0.1905,39.3978017080178));
#204174=CARTESIAN_POINT('Ctrl Pts',(-60.8610688070707,0.1905,39.5248017080178));
#204175=CARTESIAN_POINT('Ctrl Pts',(-60.7710583184321,0.317734773760269,
39.3978017080178));
#204176=CARTESIAN_POINT('Ctrl Pts',(-60.7709717342448,0.1905,39.397566602504));
#204177=CARTESIAN_POINT('Ctrl Pts',(-60.7260547307367,0.1905,39.5248015517196));
#204178=CARTESIAN_POINT('Ctrl Pts',(-60.6859465754578,0.317958617919043,
39.3484894016717));
#204179=CARTESIAN_POINT('Ctrl Pts',(-60.6862105562525,0.190499999999993,
39.3480259000038));
#204180=CARTESIAN_POINT('Ctrl Pts',(-60.5983892955396,0.1905,39.4508333188936));
#204181=CARTESIAN_POINT('Ctrl Pts',(-60.6410923272405,0.318076890623366,
39.2708017080178));
#204182=CARTESIAN_POINT('Ctrl Pts',(-60.6415942020421,0.1905,39.2705119464801));
#204183=CARTESIAN_POINT('Ctrl Pts',(-60.5311086139135,0.1905,39.3343017080178));
#204184=CARTESIAN_POINT('Origin',(-60.5311086139134,0.3175,39.3343017080178));
#204185=CARTESIAN_POINT('Origin',(-62.4786179998484,0.317499999976884,39.6398955068187));
#204186=CARTESIAN_POINT('Origin',(-62.6567671111299,0.3175,39.92499));
#204187=CARTESIAN_POINT('Origin',(-60.4497583458796,0.317499999992453,39.1934008539944));
#204188=CARTESIAN_POINT('Origin',(-60.4050521322801,0.317550804320716,39.116040271385));
#204189=CARTESIAN_POINT('Ctrl Pts',(-62.9541448057648,0.0152661173108668,
40.1599502534424));
#204190=CARTESIAN_POINT('Ctrl Pts',(-62.9168399481843,0.0152570710386341,
40.10025));
#204191=CARTESIAN_POINT('Ctrl Pts',(-62.8464427007196,0.01524,40.10025));
#204192=CARTESIAN_POINT('Ctrl Pts',(-62.9541233134297,0.103381504925153,
40.1599500538463));
#204193=CARTESIAN_POINT('Ctrl Pts',(-62.9168211560341,0.0794415635235332,
40.100244835349));
#204194=CARTESIAN_POINT('Ctrl Pts',(-62.8464212442881,0.0662446030559308,
40.10025));
#204195=CARTESIAN_POINT('Ctrl Pts',(-62.9290872705826,0.184683583687856,
40.1202442001037));
#204196=CARTESIAN_POINT('Ctrl Pts',(-62.8936771137448,0.138547994784339,
40.0633873868018));
#204197=CARTESIAN_POINT('Ctrl Pts',(-62.8213855864655,0.113305567451571,
40.0772271723537));
#204198=CARTESIAN_POINT('Ctrl Pts',(-62.8564203507742,0.291340992631635,
40.0045995998164));
#204199=CARTESIAN_POINT('Ctrl Pts',(-62.8329175802742,0.201910351191299,
39.9663485808314));
#204200=CARTESIAN_POINT('Ctrl Pts',(-62.7487193609389,0.175042741957826,
40.0101727202466));
#204201=CARTESIAN_POINT('Ctrl Pts',(-62.8099434033761,0.318045276842632,
39.9304654349858));
#204202=CARTESIAN_POINT('Ctrl Pts',(-62.7947175425018,0.205831635642382,
39.9051900162939));
#204203=CARTESIAN_POINT('Ctrl Pts',(-62.7022409210443,0.190499999999998,
39.9671857458178));
#204204=CARTESIAN_POINT('Ctrl Pts',(-62.7644678366119,0.318045750793045,
39.8576902534424));
#204205=CARTESIAN_POINT('Ctrl Pts',(-62.7649326510149,0.190500000000004,
39.8573998014387));
#204206=CARTESIAN_POINT('Ctrl Pts',(-62.6567671111299,0.1905,39.92499));
#204207=CARTESIAN_POINT('Origin',(5.50819412990574E-15,0.3175,39.116));
#204208=CARTESIAN_POINT('Origin',(-60.003690522373,0.3175,39.116));
#204209=CARTESIAN_POINT('Ctrl Pts',(-60.003690522373,0.3175,38.989));
#204210=CARTESIAN_POINT('Ctrl Pts',(-60.003690522373,0.190309748265386,
38.989));
#204211=CARTESIAN_POINT('Ctrl Pts',(-60.003690522373,0.190500142289529,
39.1161901092319));
#204212=CARTESIAN_POINT('Ctrl Pts',(-59.7867137603524,0.317270385524416,
38.989));
#204213=CARTESIAN_POINT('Ctrl Pts',(-59.7869045527969,0.190310262476459,
38.989229898976));
#204214=CARTESIAN_POINT('Ctrl Pts',(-59.8301727552494,0.190500142032462,
39.1161900493199));
#204215=CARTESIAN_POINT('Ctrl Pts',(-59.5801552670728,0.317049440713614,
39.1034966344368));
#204216=CARTESIAN_POINT('Ctrl Pts',(-59.5804765271871,0.190310761081929,
39.1038314102569));
#204217=CARTESIAN_POINT('Ctrl Pts',(-59.6649871046549,0.190500141785106,
39.20775287896));
#204218=CARTESIAN_POINT('Ctrl Pts',(-59.4651754363832,0.316925998273047,
39.2875012672119));
#204219=CARTESIAN_POINT('Ctrl Pts',(-59.4656607446594,0.190311035335126,
39.2878045257868));
#204220=CARTESIAN_POINT('Ctrl Pts',(-59.5730368716575,0.190500141646902,
39.3549015295898));
#204221=CARTESIAN_POINT('Origin',(-59.5728760150042,0.3175,39.3548010137695));
#204222=CARTESIAN_POINT('Ctrl Pts',(-62.7644678366119,-0.318045750793045,
39.8576902534424));
#204223=CARTESIAN_POINT('Ctrl Pts',(-62.7649326510148,-0.1905,39.8573998014387));
#204224=CARTESIAN_POINT('Ctrl Pts',(-62.6567671111299,-0.1905,39.92499));
#204225=CARTESIAN_POINT('Ctrl Pts',(-62.8099640589335,-0.318045262795181,
39.9304984902491));
#204226=CARTESIAN_POINT('Ctrl Pts',(-62.7947344577634,-0.205840330723031,
39.9052171569785));
#204227=CARTESIAN_POINT('Ctrl Pts',(-62.7022616416339,-0.1905,39.9672049726601));
#204228=CARTESIAN_POINT('Ctrl Pts',(-62.8562601188214,-0.291334117855409,
40.0043437678662));
#204229=CARTESIAN_POINT('Ctrl Pts',(-62.8328016940825,-0.201836550627716,
39.966162857764));
#204230=CARTESIAN_POINT('Ctrl Pts',(-62.7485591297232,-0.1750387340522,
40.0100243556234));
#204231=CARTESIAN_POINT('Ctrl Pts',(-62.9286112571071,-0.185622189560398,
40.1194874821988));
#204232=CARTESIAN_POINT('Ctrl Pts',(-62.8932808767899,-0.139140156000136,
40.0627551483143));
#204233=CARTESIAN_POINT('Ctrl Pts',(-62.8209095783125,-0.113848895265678,
40.0767884282378));
#204234=CARTESIAN_POINT('Ctrl Pts',(-62.9541233349674,-0.103673266462822,
40.1599502015391));
#204235=CARTESIAN_POINT('Ctrl Pts',(-62.9168211653022,-0.0796882264536551,
40.1002449453869));
#204236=CARTESIAN_POINT('Ctrl Pts',(-62.8464212664863,-0.0664134143651546,
40.10025));
#204237=CARTESIAN_POINT('Ctrl Pts',(-62.9541448057648,-0.0152661173108661,
40.1599502534424));
#204238=CARTESIAN_POINT('Ctrl Pts',(-62.9168399481843,-0.0152570710386336,
40.10025));
#204239=CARTESIAN_POINT('Ctrl Pts',(-62.8464427007196,-0.0152399999999996,
40.10025));
#204240=CARTESIAN_POINT('Origin',(-62.6567671111299,-0.3175,39.92499));
#204241=CARTESIAN_POINT('Origin',(-59.3947266586251,0.317499999970926,39.6398955069322));
#204242=CARTESIAN_POINT('Origin',(-59.2165773020941,0.3175,39.92499));
#204243=CARTESIAN_POINT('Origin',(-62.4786179998343,-0.317499999976807,
39.6398955068275));
#204244=CARTESIAN_POINT('Origin',(-62.3004688883554,-0.3175,39.3548010137695));
#204245=CARTESIAN_POINT('Ctrl Pts',(-59.1088767419348,0.316922544675689,
39.8576902534424));
#204246=CARTESIAN_POINT('Ctrl Pts',(-59.1093642282367,0.190499999999994,
39.8579948730703));
#204247=CARTESIAN_POINT('Ctrl Pts',(-59.2165773020941,0.1905,39.92499));
#204248=CARTESIAN_POINT('Ctrl Pts',(-59.063440705323,0.316922012809165,
39.9304020711229));
#204249=CARTESIAN_POINT('Ctrl Pts',(-59.0793536643041,0.205694973741121,
39.9058915297382));
#204250=CARTESIAN_POINT('Ctrl Pts',(-59.1711393827295,0.1905,39.9671523786035));
#204251=CARTESIAN_POINT('Ctrl Pts',(-59.0174076205275,0.290332993454962,
40.0043257306695));
#204252=CARTESIAN_POINT('Ctrl Pts',(-59.0412846811395,0.201480151665867,
39.9667894847835));
#204253=CARTESIAN_POINT('Ctrl Pts',(-59.1251084688121,0.175054909459692,
40.01001389752));
#204254=CARTESIAN_POINT('Ctrl Pts',(-58.9458296250063,0.184894967401607,
40.1195533054855));
#204255=CARTESIAN_POINT('Ctrl Pts',(-58.9812445774292,0.138672156931206,
40.0630813209236));
#204256=CARTESIAN_POINT('Ctrl Pts',(-59.0535312451933,0.113807322597792,
40.076826594242));
#204257=CARTESIAN_POINT('Ctrl Pts',(-58.9208287018089,0.10317160645571,
40.1599502027521));
#204258=CARTESIAN_POINT('Ctrl Pts',(-58.9581363848278,0.0793367652458316,
40.1002552791554));
#204259=CARTESIAN_POINT('Ctrl Pts',(-59.0285307646525,0.0663350652343385,
40.10025));
#204260=CARTESIAN_POINT('Ctrl Pts',(-58.9208513795073,0.0152121934559205,
40.1599502534424));
#204261=CARTESIAN_POINT('Ctrl Pts',(-58.9581562369413,0.0152218248291074,
40.10025));
#204262=CARTESIAN_POINT('Ctrl Pts',(-59.0285534841296,0.0152400000000004,
40.10025));
#204263=CARTESIAN_POINT('Ctrl Pts',(-61.8696548221181,-0.3175,38.989));
#204264=CARTESIAN_POINT('Ctrl Pts',(-61.8696548221181,-0.190310256931795,
38.989));
#204265=CARTESIAN_POINT('Ctrl Pts',(-61.8696548221181,-0.190500141530248,
39.1161896013265));
#204266=CARTESIAN_POINT('Ctrl Pts',(-62.0866315324121,-0.31772268963223,
38.989));
#204267=CARTESIAN_POINT('Ctrl Pts',(-62.0868176889526,-0.190309758576012,
38.988776927546));
#204268=CARTESIAN_POINT('Ctrl Pts',(-62.0431722165666,-0.190500141778232,
39.1161898821847));
#204269=CARTESIAN_POINT('Ctrl Pts',(-62.2931898887681,-0.317932491655698,
39.1034967087244));
#204270=CARTESIAN_POINT('Ctrl Pts',(-62.2934992458057,-0.190309283350195,
39.1031720232705));
#204271=CARTESIAN_POINT('Ctrl Pts',(-62.2083577878507,-0.190500142011858,
39.2077529614999));
#204272=CARTESIAN_POINT('Ctrl Pts',(-62.4081695979768,-0.318048871877129,
39.2875012672119));
#204273=CARTESIAN_POINT('Ctrl Pts',(-62.4086377820239,-0.190309023146872,
39.2872087095507));
#204274=CARTESIAN_POINT('Ctrl Pts',(-62.3003077510788,-0.190500142141458,
39.3549017048227));
#204275=CARTESIAN_POINT('Origin',(-61.8696548221181,-0.3175,39.116));
#204276=CARTESIAN_POINT('Origin',(62.2224557307631,-0.3175,39.116));
#204277=CARTESIAN_POINT('Origin',(-61.4683012396084,-0.317551690014637,
39.1160373285281));
#204278=CARTESIAN_POINT('Ctrl Pts',(-58.9208513795073,-0.0152121934559198,
40.1599502534424));
#204279=CARTESIAN_POINT('Ctrl Pts',(-58.9581562369413,-0.0152218248291069,
40.10025));
#204280=CARTESIAN_POINT('Ctrl Pts',(-59.0285534841296,-0.01524,40.10025));
#204281=CARTESIAN_POINT('Ctrl Pts',(-58.9208288705619,-0.102871702177371,
40.1599500566036));
#204282=CARTESIAN_POINT('Ctrl Pts',(-58.9581365422967,-0.0790852439332833,
40.100255130536));
#204283=CARTESIAN_POINT('Ctrl Pts',(-59.0285309330221,-0.0661608181924982,
40.10025));
#204284=CARTESIAN_POINT('Ctrl Pts',(-58.9453619764183,-0.183955833237535,
40.1203070619047));
#204285=CARTESIAN_POINT('Ctrl Pts',(-58.9808530699758,-0.138075936736132,
40.0637098684499));
#204286=CARTESIAN_POINT('Ctrl Pts',(-59.0530636028226,-0.113261762368167,
40.0772636213363));
#204287=CARTESIAN_POINT('Ctrl Pts',(-59.0172303255293,-0.290319860890624,
40.0046102245802));
#204288=CARTESIAN_POINT('Ctrl Pts',(-59.0411528690725,-0.201541405841779,
39.9670001894012));
#204289=CARTESIAN_POINT('Ctrl Pts',(-59.1249311745757,-0.175047309551177,
40.0101788811209));
#204290=CARTESIAN_POINT('Ctrl Pts',(-59.0634600627912,-0.316922027357334,
39.9303710930186));
#204291=CARTESIAN_POINT('Ctrl Pts',(-59.079369436468,-0.205687000366196,
39.9058663574111));
#204292=CARTESIAN_POINT('Ctrl Pts',(-59.1711586818662,-0.190499999999998,
39.9671344706369));
#204293=CARTESIAN_POINT('Ctrl Pts',(-59.1088767419348,-0.316922544675689,
39.8576902534424));
#204294=CARTESIAN_POINT('Ctrl Pts',(-59.1093642282366,-0.190500000000004,
39.8579948730704));
#204295=CARTESIAN_POINT('Ctrl Pts',(-59.2165773020941,-0.1905,39.92499));
#204296=CARTESIAN_POINT('Origin',(-59.2165773020941,-0.3175,39.92499));
#204297=CARTESIAN_POINT('Origin',(-61.4240753793289,-0.317499999995429,
39.1925554488848));
#204298=CARTESIAN_POINT('Origin',(-61.3422370451705,-0.3175,39.3343017080178));
#204299=CARTESIAN_POINT('Origin',(-59.3947266586079,-0.317499999970831,
39.6398955069215));
#204300=CARTESIAN_POINT('Origin',(-59.5728760150042,-0.3175,39.3548010137695));
#204301=CARTESIAN_POINT('Ctrl Pts',(-61.0122769227456,-0.3175,39.3978017080178));
#204302=CARTESIAN_POINT('Ctrl Pts',(-61.0122769227456,-0.1905,39.3978017080178));
#204303=CARTESIAN_POINT('Ctrl Pts',(-61.0122769227456,-0.1905,39.5248017080178));
#204304=CARTESIAN_POINT('Ctrl Pts',(-61.102287399097,-0.317265808076389,
39.3978017080178));
#204305=CARTESIAN_POINT('Ctrl Pts',(-61.1022028716714,-0.190499999999991,
39.3980355775177));
#204306=CARTESIAN_POINT('Ctrl Pts',(-61.1472909869838,-0.1905,39.5248015517192));
#204307=CARTESIAN_POINT('Ctrl Pts',(-61.1873990841185,-0.317046189129109,
39.3484893995498));
#204308=CARTESIAN_POINT('Ctrl Pts',(-61.1876587562312,-0.190500000000015,
39.3489438303423));
#204309=CARTESIAN_POINT('Ctrl Pts',(-61.2749563897835,-0.1905,39.4508333155593));
#204310=CARTESIAN_POINT('Ctrl Pts',(-61.2322532920972,-0.316930737395914,
39.2708017080178));
#204311=CARTESIAN_POINT('Ctrl Pts',(-61.2327440814645,-0.1905,39.2710850691866));
#204312=CARTESIAN_POINT('Ctrl Pts',(-61.3422370451705,-0.1905,39.3343017080178));
#204313=CARTESIAN_POINT('Origin',(-61.0122769227456,-0.3175,39.5248017080178));
#204314=CARTESIAN_POINT('Ctrl Pts',(-59.4651754363832,-0.316925998273047,
39.2875012672119));
#204315=CARTESIAN_POINT('Ctrl Pts',(-59.4656607446034,-0.190311049925011,
39.2878045257519));
#204316=CARTESIAN_POINT('Ctrl Pts',(-59.5730368592471,-0.190500141625046,
39.3549015218348));
#204317=CARTESIAN_POINT('Ctrl Pts',(-59.5801570044831,-0.317049442579187,
39.1034938540228));
#204318=CARTESIAN_POINT('Ctrl Pts',(-59.5804782634865,-0.190310775687219,
39.1038286278809));
#204319=CARTESIAN_POINT('Ctrl Pts',(-59.6649884842712,-0.190500141763233,
39.2077506434031));
#204320=CARTESIAN_POINT('Ctrl Pts',(-59.7867171285936,-0.317270389088839,
38.989));
#204321=CARTESIAN_POINT('Ctrl Pts',(-59.7869079131825,-0.190310277118105,
38.9892298954611));
#204322=CARTESIAN_POINT('Ctrl Pts',(-59.8301754438929,-0.19050014201055,
39.116190034729));
#204323=CARTESIAN_POINT('Ctrl Pts',(-60.003690522373,-0.3175,38.989));
#204324=CARTESIAN_POINT('Ctrl Pts',(-60.003690522373,-0.190309762954695,
38.989));
#204325=CARTESIAN_POINT('Ctrl Pts',(-60.003690522373,-0.190500142267574,
39.1161900945646));
#204326=CARTESIAN_POINT('Origin',(-60.0036905223731,-0.3175,39.116));
#204327=CARTESIAN_POINT('Origin',(60.71525,-0.3175,39.5248017080178));
#204328=CARTESIAN_POINT('Origin',(-60.8610688070707,-0.3175,39.5248017080178));
#204329=CARTESIAN_POINT('Origin',(60.4792282238308,-0.3175,39.116));
#204330=CARTESIAN_POINT('Origin',(-60.40505213228,-0.317550804320886,39.1160402713852));
#204331=CARTESIAN_POINT('Ctrl Pts',(-60.6410923272405,-0.318076890623366,
39.2708017080178));
#204332=CARTESIAN_POINT('Ctrl Pts',(-60.6415942020421,-0.1905,39.2705119464801));
#204333=CARTESIAN_POINT('Ctrl Pts',(-60.5311086139134,-0.1905,39.3343017080178));
#204334=CARTESIAN_POINT('Ctrl Pts',(-60.6860981505083,-0.317958218318758,
39.3487519301186));
#204335=CARTESIAN_POINT('Ctrl Pts',(-60.68636137503,-0.190499999997976,
39.3482879463971));
#204336=CARTESIAN_POINT('Ctrl Pts',(-60.5986166446964,-0.1905,39.4512271261627));
#204337=CARTESIAN_POINT('Ctrl Pts',(-60.771361502534,-0.317733982967541,
39.3978017080178));
#204338=CARTESIAN_POINT('Ctrl Pts',(-60.771275014198,-0.1905,39.3975673827411));
#204339=CARTESIAN_POINT('Ctrl Pts',(-60.7265095085044,-0.1905,39.5248015355195));
#204340=CARTESIAN_POINT('Ctrl Pts',(-60.8610688070707,-0.3175,39.3978017080178));
#204341=CARTESIAN_POINT('Ctrl Pts',(-60.8610688070707,-0.1905,39.3978017080178));
#204342=CARTESIAN_POINT('Ctrl Pts',(-60.8610688070707,-0.1905,39.5248017080178));
#204343=CARTESIAN_POINT('Origin',(-60.5311086139135,-0.3175,39.3343017080178));
#204344=CARTESIAN_POINT('Origin',(-60.4497583469873,-0.31750000030155,39.1934008533549));
#204345=CARTESIAN_POINT('Origin',(-61.0544000815112,6.73632490863974,39.1925554495085));
#204346=CARTESIAN_POINT('Origin',(-61.0983782637182,6.74099917688121,39.1160373285283));
#204347=CARTESIAN_POINT('Origin',(-60.9730100652054,6.72777047351166,39.3343017080178));
#204348=CARTESIAN_POINT('Ctrl Pts',(-60.8636883187844,6.71570789669452,
39.2708017080178));
#204349=CARTESIAN_POINT('Ctrl Pts',(-60.877392030246,6.59002106156508,39.2710850691866));
#204350=CARTESIAN_POINT('Ctrl Pts',(-60.9862851800404,6.60146619279989,
39.3343017080178));
#204351=CARTESIAN_POINT('Ctrl Pts',(-60.8189169727309,6.71111871849841,
39.3487519293518));
#204352=CARTESIAN_POINT('Ctrl Pts',(-60.8324022194118,6.58529244190258,
39.3492068662932));
#204353=CARTESIAN_POINT('Ctrl Pts',(-60.9191469903167,6.59440968471186,
39.4512271248736));
#204354=CARTESIAN_POINT('Ctrl Pts',(-60.7340977611528,6.70242508976258,
39.3978017080178));
#204355=CARTESIAN_POINT('Ctrl Pts',(-60.7472645033899,6.5763441073677,39.3980347781174));
#204356=CARTESIAN_POINT('Ctrl Pts',(-60.7919547682785,6.5810412434828,39.524801535519));
#204357=CARTESIAN_POINT('Ctrl Pts',(-60.6448574988554,6.69328024897497,
39.3978017080178));
#204358=CARTESIAN_POINT('Ctrl Pts',(-60.6581326136904,6.5669759682632,39.3978017080178));
#204359=CARTESIAN_POINT('Ctrl Pts',(-60.6581326136904,6.5669759682632,39.5248017080178));
#204360=CARTESIAN_POINT('Origin',(-60.6448574988554,6.69328024897497,39.5248017080178));
#204361=CARTESIAN_POINT('Origin',(0.0331877870874877,0.315760701779427,
39.116));
#204362=CARTESIAN_POINT('Origin',(-61.4975385923862,6.78290064323603,39.116));
#204363=CARTESIAN_POINT('Origin',(0.0331877870874878,0.315760701779427,
39.5248017080178));
#204364=CARTESIAN_POINT('Origin',(-60.4944777170593,6.67747469700988,39.5248017080178));
#204365=CARTESIAN_POINT('Ctrl Pts',(-62.0330459552232,6.83973663030303,
39.2875012672119));
#204366=CARTESIAN_POINT('Ctrl Pts',(-62.0468640234019,6.71274550335285,
39.287208709576));
#204367=CARTESIAN_POINT('Ctrl Pts',(-61.9391074687686,6.70161199370869,
39.3549016990123));
#204368=CARTESIAN_POINT('Ctrl Pts',(-61.9187065474464,6.82760205123632,
39.103493917393));
#204369=CARTESIAN_POINT('Ctrl Pts',(-61.9323544653015,6.70071032544359,
39.1031692336337));
#204370=CARTESIAN_POINT('Ctrl Pts',(-61.8476598279006,6.6920004592181,39.2077507202297));
#204371=CARTESIAN_POINT('Ctrl Pts',(-61.7133000470647,6.80580199871487,
38.989));
#204372=CARTESIAN_POINT('Ctrl Pts',(-61.7268034525372,6.67910652125848,
38.9887769311176));
#204373=CARTESIAN_POINT('Ctrl Pts',(-61.6833778591514,6.67473372828989,
39.1161898712915));
#204374=CARTESIAN_POINT('Ctrl Pts',(-61.4975385923862,6.78290064323603,
38.989));
#204375=CARTESIAN_POINT('Ctrl Pts',(-61.5108335396271,6.65640766978589,
38.989));
#204376=CARTESIAN_POINT('Ctrl Pts',(-61.5108136924289,6.65659650326295,
39.1161895903854));
#204377=CARTESIAN_POINT('Origin',(-61.9259926140919,6.82793297553392,39.3548010137695));
#204378=CARTESIAN_POINT('Ctrl Pts',(-60.4944777170593,6.67747469700988,
39.3978017080178));
#204379=CARTESIAN_POINT('Ctrl Pts',(-60.5077528318943,6.55117041629811,
39.3978017080178));
#204380=CARTESIAN_POINT('Ctrl Pts',(-60.5077528318943,6.55117041629811,
39.5248017080178));
#204381=CARTESIAN_POINT('Ctrl Pts',(-60.4049357747551,6.66829952659918,
39.3978017080178));
#204382=CARTESIAN_POINT('Ctrl Pts',(-60.4181493202576,6.54175270773008,
39.397566602504));
#204383=CARTESIAN_POINT('Ctrl Pts',(-60.3734783767973,6.53705760237942,
39.5248015517196));
#204384=CARTESIAN_POINT('Ctrl Pts',(-60.3202668847282,6.65962554481747,
39.3484894016716));
#204385=CARTESIAN_POINT('Ctrl Pts',(-60.3338524728735,6.53289275205061,
39.3480259000029));
#204386=CARTESIAN_POINT('Ctrl Pts',(-60.2465123062119,6.52371293062585,
39.4508333188936));
#204387=CARTESIAN_POINT('Ctrl Pts',(-60.2756459899118,6.65505462397437,
39.2708017080178));
#204388=CARTESIAN_POINT('Ctrl Pts',(-60.2894805317161,6.5282290731082,39.2705119464801));
#204389=CARTESIAN_POINT('Ctrl Pts',(-60.1796001951995,6.51668018436788,
39.3343017080178));
#204390=CARTESIAN_POINT('Origin',(-60.1663250803645,6.64298446507965,39.3343017080178));
#204391=CARTESIAN_POINT('Origin',(-62.1031658061144,6.8465546283679,39.6398955068187));
#204392=CARTESIAN_POINT('Origin',(-62.2803389979219,6.86517628122553,39.92499));
#204393=CARTESIAN_POINT('Origin',(-60.0854204576109,6.63448104656938,39.1934008539947));
#204394=CARTESIAN_POINT('Origin',(-60.0409538388295,6.62985850077888,39.1160402713849));
#204395=CARTESIAN_POINT('Ctrl Pts',(-62.6076796697354,6.59568250079929,
40.1599502534424));
#204396=CARTESIAN_POINT('Ctrl Pts',(-62.5705801176609,6.59177408464818,
40.10025));
#204397=CARTESIAN_POINT('Ctrl Pts',(-62.500570298093,6.58439859103072,40.10025));
#204398=CARTESIAN_POINT('Ctrl Pts',(-62.5984477290795,6.68331293653975,
40.1599500538457));
#204399=CARTESIAN_POINT('Ctrl Pts',(-62.5638523220909,6.65560500345286,
40.1002448353503));
#204400=CARTESIAN_POINT('Ctrl Pts',(-62.495217526425,6.63512154272658,40.10025));
#204401=CARTESIAN_POINT('Ctrl Pts',(-62.5650504549418,6.76155265492316,
40.1202442001039));
#204402=CARTESIAN_POINT('Ctrl Pts',(-62.5346567608586,6.71196843232467,
40.0633873868018));
#204403=CARTESIAN_POINT('Ctrl Pts',(-62.4653998062672,6.67930776339611,
40.0772271723537));
#204404=CARTESIAN_POINT('Ctrl Pts',(-62.48163287707,6.86003002196301,40.0045995998162));
#204405=CARTESIAN_POINT('Ctrl Pts',(-62.4676069047243,6.76863258245075,
39.9663485808315));
#204406=CARTESIAN_POINT('Ctrl Pts',(-62.3866783619498,6.73311104631499,
40.0101727202466));
#204407=CARTESIAN_POINT('Ctrl Pts',(-62.4326191774618,6.88172985342207,
39.930465434986));
#204408=CARTESIAN_POINT('Ctrl Pts',(-62.4292062449178,6.76853939445011,
39.9051900162948));
#204409=CARTESIAN_POINT('Ctrl Pts',(-62.338838812383,6.74362530798309,39.9671857458173));
#204410=CARTESIAN_POINT('Ctrl Pts',(-62.3873926810691,6.87697683366608,
39.8576902534424));
#204411=CARTESIAN_POINT('Ctrl Pts',(-62.4011871104968,6.75017837817646,
39.8573998014387));
#204412=CARTESIAN_POINT('Ctrl Pts',(-62.2936141127569,6.73887200051376,
39.92499));
#204413=CARTESIAN_POINT('Origin',(-62.500570298093,6.58439859103072,40.22725));
#204414=CARTESIAN_POINT('Origin',(0.0331877870874877,0.315760701779427,
39.116));
#204415=CARTESIAN_POINT('Origin',(-59.6417962403142,6.58785426247137,39.116));
#204416=CARTESIAN_POINT('Origin',(1.33778643725275E-16,-1.72356557454387E-17,
40.22725));
#204417=CARTESIAN_POINT('Origin',(-62.5037563256534,6.55408556365989,40.22725));
#204418=CARTESIAN_POINT('Ctrl Pts',(-59.6417962403142,6.58785426247137,
38.989));
#204419=CARTESIAN_POINT('Ctrl Pts',(-59.6550912418707,6.46136077224392,
38.989));
#204420=CARTESIAN_POINT('Ctrl Pts',(-59.6550713402759,6.46155012326965,
39.1161901092319));
#204421=CARTESIAN_POINT('Ctrl Pts',(-59.4260321009469,6.56494565834894,
38.989));
#204422=CARTESIAN_POINT('Ctrl Pts',(-59.43949279477,6.43870097938019,38.989229898976));
#204423=CARTESIAN_POINT('Ctrl Pts',(-59.4825041216627,6.4434125774669,39.1161900493199));
#204424=CARTESIAN_POINT('Ctrl Pts',(-59.2206282517276,6.54313468201949,
39.1034966344368));
#204425=CARTESIAN_POINT('Ctrl Pts',(-59.2341955513627,6.41712387095977,
39.1038314102564));
#204426=CARTESIAN_POINT('Ctrl Pts',(-59.3182233753722,6.42614597501045,
39.2077528789601));
#204427=CARTESIAN_POINT('Ctrl Pts',(-59.1062911958296,6.53099325080096,
39.2875012672119));
#204428=CARTESIAN_POINT('Ctrl Pts',(-59.1200087130388,6.4051226264063,39.2878045257868));
#204429=CARTESIAN_POINT('Ctrl Pts',(-59.2267768553862,6.41653455832064,
39.3549015295898));
#204430=CARTESIAN_POINT('Origin',(-59.2133417798936,6.54282188406269,39.3548010137695));
#204431=CARTESIAN_POINT('Ctrl Pts',(-62.4538823482275,6.24436990788103,
39.8576902534424));
#204432=CARTESIAN_POINT('Ctrl Pts',(-62.4410124550018,6.37126553604114,
39.8573998014387));
#204433=CARTESIAN_POINT('Ctrl Pts',(-62.3334394572618,6.35995915837845,
39.92499));
#204434=CARTESIAN_POINT('Ctrl Pts',(-62.4991292864733,6.24912604340955,
39.9304984902494));
#204435=CARTESIAN_POINT('Ctrl Pts',(-62.4722545055303,6.35912437831612,
39.9052171569796));
#204436=CARTESIAN_POINT('Ctrl Pts',(-62.3786847639677,6.36471463173913,
39.9672049726603));
#204437=CARTESIAN_POINT('Ctrl Pts',(-62.542379656768,6.28053011789782,40.0043437678658));
#204438=CARTESIAN_POINT('Ctrl Pts',(-62.5096946965644,6.36708533499936,
39.966162857764));
#204439=CARTESIAN_POINT('Ctrl Pts',(-62.4231124872028,6.38493060453743,
40.0100243556235));
#204440=CARTESIAN_POINT('Ctrl Pts',(-62.6032845425347,6.39322569848931,
40.1194874821992));
#204441=CARTESIAN_POINT('Ctrl Pts',(-62.5632890102013,6.43576006824499,
40.0627551483143));
#204442=CARTESIAN_POINT('Ctrl Pts',(-62.4886705126495,6.45334792019248,
40.0767884282378));
#204443=CARTESIAN_POINT('Ctrl Pts',(-62.620090867565,6.47739243510536,40.1599502015389));
#204444=CARTESIAN_POINT('Ctrl Pts',(-62.5804859237135,6.49734694408414,
40.1002449453872));
#204445=CARTESIAN_POINT('Ctrl Pts',(-62.5090840872032,6.50319024212558,
40.10025));
#204446=CARTESIAN_POINT('Ctrl Pts',(-62.6108711573005,6.56531752495346,
40.1599502534424));
#204447=CARTESIAN_POINT('Ctrl Pts',(-62.5737697140401,6.56142710223395,
40.10025));
#204448=CARTESIAN_POINT('Ctrl Pts',(-62.5037563256534,6.5540855636599,40.10025));
#204449=CARTESIAN_POINT('Origin',(-62.3467145720969,6.23365487766668,39.92499));
#204450=CARTESIAN_POINT('Origin',(-59.0361683443313,6.52420020558017,39.639895506932));
#204451=CARTESIAN_POINT('Origin',(-58.858994908613,6.50557852713795,39.92499));
#204452=CARTESIAN_POINT('Origin',(-62.1695413802715,6.21503322485432,39.6398955068269));
#204453=CARTESIAN_POINT('Origin',(-61.9923681882668,6.19641157197507,39.3548010137695));
#204454=CARTESIAN_POINT('Ctrl Pts',(-58.7519447039088,6.49374646112781,
39.8576902534424));
#204455=CARTESIAN_POINT('Ctrl Pts',(-58.765644274027,6.36806742857366,39.8579948730703));
#204456=CARTESIAN_POINT('Ctrl Pts',(-58.872270023448,6.37927424642618,39.92499));
#204457=CARTESIAN_POINT('Ctrl Pts',(-58.7067576262547,6.48899657309089,
39.9304020711231));
#204458=CARTESIAN_POINT('Ctrl Pts',(-58.7342098038487,6.38004220452875,
39.9058915297381));
#204459=CARTESIAN_POINT('Ctrl Pts',(-58.8270810177595,6.37452469054088,
39.9671523786032));
#204460=CARTESIAN_POINT('Ctrl Pts',(-58.6637560248473,6.4577414435536,40.0043257306693));
#204461=CARTESIAN_POINT('Ctrl Pts',(-58.6967899354322,6.37187117938164,
39.9667894847835));
#204462=CARTESIAN_POINT('Ctrl Pts',(-58.7829167175845,6.35435266912814,
40.01001389752));
#204463=CARTESIAN_POINT('Ctrl Pts',(-58.603591415908,6.34539908016358,40.1195533054857));
#204464=CARTESIAN_POINT('Ctrl Pts',(-58.6436439608623,6.30313135363892,
40.0630813209236));
#204465=CARTESIAN_POINT('Ctrl Pts',(-58.7181337176194,6.28595874576549,
40.0768265942421));
#204466=CARTESIAN_POINT('Ctrl Pts',(-58.5872698677166,6.26151010025763,
40.1599502027522));
#204467=CARTESIAN_POINT('Ctrl Pts',(-58.6268645946683,6.24170554357573,
40.1002552791554));
#204468=CARTESIAN_POINT('Ctrl Pts',(-58.6982323944355,6.23613328458312,
40.10025));
#204469=CARTESIAN_POINT('Ctrl Pts',(-58.596486683455,6.17403490859061,40.1599502534424));
#204470=CARTESIAN_POINT('Ctrl Pts',(-58.6335861742241,6.17794390662212,
40.10025));
#204471=CARTESIAN_POINT('Ctrl Pts',(-58.7035958781038,6.18532049829439,
40.10025));
#204472=CARTESIAN_POINT('Origin',(-58.7035958781038,6.18532049829439,40.22725));
#204473=CARTESIAN_POINT('Ctrl Pts',(-61.5639141665611,6.15137923967718,
38.989));
#204474=CARTESIAN_POINT('Ctrl Pts',(-61.5506192181748,6.27787222402454,
38.989));
#204475=CARTESIAN_POINT('Ctrl Pts',(-61.5506390665201,6.27768337963402,
39.1161896013263));
#204476=CARTESIAN_POINT('Ctrl Pts',(-61.7797255331385,6.17383801205393,
38.989));
#204477=CARTESIAN_POINT('Ctrl Pts',(-61.766592392013,6.30057242039937,38.988776927546));
#204478=CARTESIAN_POINT('Ctrl Pts',(-61.7232059145547,6.29582088597956,
39.1161898821845));
#204479=CARTESIAN_POINT('Ctrl Pts',(-61.985174271489,6.19522058691287,39.1034967087243));
#204480=CARTESIAN_POINT('Ctrl Pts',(-61.9721416759917,6.32217699854306,
39.1031720232715));
#204481=CARTESIAN_POINT('Ctrl Pts',(-61.8874865820147,6.31308747966697,
39.2077529615005));
#204482=CARTESIAN_POINT('Ctrl Pts',(-62.0995362748658,6.20712349654507,
39.2875012672119));
#204483=CARTESIAN_POINT('Ctrl Pts',(-62.0866494440659,6.33421251157707,
39.2872087095507));
#204484=CARTESIAN_POINT('Ctrl Pts',(-61.9789328337401,6.32269886789217,
39.3549017048226));
#204485=CARTESIAN_POINT('Origin',(-61.5639141665611,6.15137923967718,39.116));
#204486=CARTESIAN_POINT('Origin',(3.53633106925806E-16,6.13135187546216E-18,
40.22725));
#204487=CARTESIAN_POINT('Origin',(-58.7067819056642,6.15500747092357,40.22725));
#204488=CARTESIAN_POINT('Origin',(61.5094129706996,-6.78414869068793,39.116));
#204489=CARTESIAN_POINT('Origin',(-61.1647646440474,6.10937495962054,39.1160373285262));
#204490=CARTESIAN_POINT('Ctrl Pts',(-58.5996668978648,6.14377718965363,
40.1599502534424));
#204491=CARTESIAN_POINT('Ctrl Pts',(-58.6367684021392,6.14766703046211,
40.10025));
#204492=CARTESIAN_POINT('Ctrl Pts',(-58.7067819056642,6.15500747092357,
40.10025));
#204493=CARTESIAN_POINT('Ctrl Pts',(-58.6088074259633,6.05659553606742,
40.1599500566034));
#204494=CARTESIAN_POINT('Ctrl Pts',(-58.6434243604373,6.08415140319827,
40.1002551305372));
#204495=CARTESIAN_POINT('Ctrl Pts',(-58.7120821529693,6.10436324506856,
40.10025));
#204496=CARTESIAN_POINT('Ctrl Pts',(-58.6416817365139,5.97852000021562,
40.1203070619046));
#204497=CARTESIAN_POINT('Ctrl Pts',(-58.6721826510718,6.02785839131309,
40.06370986845));
#204498=CARTESIAN_POINT('Ctrl Pts',(-58.7414038195498,6.06008468706738,
40.0772636213363));
#204499=CARTESIAN_POINT('Ctrl Pts',(-58.7242744516463,5.88025093392509,
40.0046102245803));
#204500=CARTESIAN_POINT('Ctrl Pts',(-58.7387860695146,5.97104363802183,
39.9670001894012));
#204501=CARTESIAN_POINT('Ctrl Pts',(-58.819336041524,6.00614981441059,40.0101788811209));
#204502=CARTESIAN_POINT('Ctrl Pts',(-58.7730316211507,5.85862682030306,
39.9303710930186));
#204503=CARTESIAN_POINT('Ctrl Pts',(-58.77722661518,5.97091547255942,39.9058663574101));
#204504=CARTESIAN_POINT('Ctrl Pts',(-58.866925555679,5.99561386571472,39.9671344706368));
#204505=CARTESIAN_POINT('Ctrl Pts',(-58.8181995570484,5.8633736414962,39.8576902534424));
#204506=CARTESIAN_POINT('Ctrl Pts',(-58.805469618532,5.98915458643835,39.8579948730704));
#204507=CARTESIAN_POINT('Ctrl Pts',(-58.9120953679529,6.00036140429087,
39.92499));
#204508=CARTESIAN_POINT('Origin',(-58.925370482788,5.8740571235791,39.92499));
#204509=CARTESIAN_POINT('Origin',(-61.1207756545813,6.10480350526353,39.1925554488851));
#204510=CARTESIAN_POINT('Origin',(-61.0393856393803,6.09624906995281,39.3343017080178));
#204511=CARTESIAN_POINT('Origin',(-59.1025439184822,5.89267880207721,39.6398955069206));
#204512=CARTESIAN_POINT('Origin',(-59.2797173540685,5.91130048050383,39.3548010137695));
#204513=CARTESIAN_POINT('Ctrl Pts',(-60.7112330730303,6.06175884541612,
39.3978017080178));
#204514=CARTESIAN_POINT('Ctrl Pts',(-60.6979579581953,6.18806312612789,
39.3978017080178));
#204515=CARTESIAN_POINT('Ctrl Pts',(-60.6979579581953,6.18806312612789,
39.5248017080178));
#204516=CARTESIAN_POINT('Ctrl Pts',(-60.8007259828525,6.07140041118273,
39.3978017080178));
#204517=CARTESIAN_POINT('Ctrl Pts',(-60.787391283362,6.19746294737678,39.3980355775177));
#204518=CARTESIAN_POINT('Ctrl Pts',(-60.832232401261,6.20217593878204,39.5248015517192));
#204519=CARTESIAN_POINT('Ctrl Pts',(-60.885348460727,6.08051542067576,39.3484893995498));
#204520=CARTESIAN_POINT('Ctrl Pts',(-60.8723790316489,6.20639551966831,
39.3489438303429));
#204521=CARTESIAN_POINT('Ctrl Pts',(-60.9591984396307,6.2155206071496,39.45083331556));
#204522=CARTESIAN_POINT('Ctrl Pts',(-60.929944884669,6.08531878138363,39.2708017080178));
#204523=CARTESIAN_POINT('Ctrl Pts',(-60.917217374751,6.21110821942976,39.2710850691866));
#204524=CARTESIAN_POINT('Ctrl Pts',(-61.0261105245453,6.22255335066458,
39.3343017080178));
#204525=CARTESIAN_POINT('Origin',(-60.7112330730303,6.06175884541612,39.5248017080178));
#204526=CARTESIAN_POINT('Ctrl Pts',(-59.1725467709677,5.90061356181298,
39.2875012672119));
#204527=CARTESIAN_POINT('Ctrl Pts',(-59.1597945546412,6.02658562874862,
39.2878045257519));
#204528=CARTESIAN_POINT('Ctrl Pts',(-59.2666022171588,6.03762143316794,
39.3549015218348));
#204529=CARTESIAN_POINT('Ctrl Pts',(-59.2869113614504,5.91250964036551,
39.1034938540228));
#204530=CARTESIAN_POINT('Ctrl Pts',(-59.2739830624754,6.03858760028937,
39.1038286278806));
#204531=CARTESIAN_POINT('Ctrl Pts',(-59.3580501215732,6.04723299508913,
39.2077506434029));
#204532=CARTESIAN_POINT('Ctrl Pts',(-59.4923630227875,5.93388131656941,
38.989));
#204533=CARTESIAN_POINT('Ctrl Pts',(-59.4792818168387,6.06016587018228,
38.9892298954611));
#204534=CARTESIAN_POINT('Ctrl Pts',(-59.5223321697741,6.06449973388448,
39.1161900347291));
#204535=CARTESIAN_POINT('Ctrl Pts',(-59.7081718144892,5.95633285891252,
38.989));
#204536=CARTESIAN_POINT('Ctrl Pts',(-59.6948768144682,6.08282633453128,
38.989));
#204537=CARTESIAN_POINT('Ctrl Pts',(-59.6948967145252,6.08263699813607,
39.1161900945648));
#204538=CARTESIAN_POINT('Origin',(-59.7081718144892,5.95633285891252,39.116));
#204539=CARTESIAN_POINT('Origin',(60.0186752706391,-6.62746584474133,39.5248017080178));
#204540=CARTESIAN_POINT('Origin',(-60.5608532912343,6.04595329345103,39.5248017080178));
#204541=CARTESIAN_POINT('Origin',(59.785232315514,-6.60293000146475,39.116));
#204542=CARTESIAN_POINT('Origin',(-60.1073400340001,5.99823604520212,39.1160402713844));
#204543=CARTESIAN_POINT('Ctrl Pts',(-60.3421421670674,6.02238575970317,
39.2708017080178));
#204544=CARTESIAN_POINT('Ctrl Pts',(-60.3293058762211,6.14931623097289,
39.27051194648));
#204545=CARTESIAN_POINT('Ctrl Pts',(-60.2194255397044,6.13776734223257,
39.3343017080178));
#204546=CARTESIAN_POINT('Ctrl Pts',(-60.3868890390927,6.02720817145296,
39.3487519301186));
#204547=CARTESIAN_POINT('Ctrl Pts',(-60.3738278099533,6.15399567477046,
39.3482879463963));
#204548=CARTESIAN_POINT('Ctrl Pts',(-60.2865637544332,6.14482385294874,
39.4512271261618));
#204549=CARTESIAN_POINT('Ctrl Pts',(-60.4716618705782,6.03634362557922,
39.3978017080178));
#204550=CARTESIAN_POINT('Ctrl Pts',(-60.4582762833178,6.1628715669826,39.3975673827415));
#204551=CARTESIAN_POINT('Ctrl Pts',(-60.4137560077483,6.15819229746514,
39.5248015355199));
#204552=CARTESIAN_POINT('Ctrl Pts',(-60.5608532912343,6.04595329345103,
39.3978017080178));
#204553=CARTESIAN_POINT('Ctrl Pts',(-60.5475781763993,6.1722575741628,39.3978017080178));
#204554=CARTESIAN_POINT('Ctrl Pts',(-60.5475781763993,6.1722575741628,39.5248017080178));
#204555=CARTESIAN_POINT('Origin',(-60.2327006545395,6.0114630615208,39.3343017080178));
#204556=CARTESIAN_POINT('Origin',(-60.1517960329186,6.00295964283188,39.1934008533551));
#204557=CARTESIAN_POINT('Origin',(-60.0157999988656,13.0813452322065,39.1925554495085));
#204558=CARTESIAN_POINT('Origin',(-60.0590486699127,13.0905908661204,39.1160373285284));
#204559=CARTESIAN_POINT('Origin',(-59.9357500275432,13.0643300858386,39.3343017080178));
#204560=CARTESIAN_POINT('Ctrl Pts',(-59.8282880397054,13.0409063549243,
39.2708017080178));
#204561=CARTESIAN_POINT('Ctrl Pts',(-59.8550545325308,12.9173404733287,
39.2710850691866));
#204562=CARTESIAN_POINT('Ctrl Pts',(-59.9621548122771,12.9401053405454,
39.3343017080178));
#204563=CARTESIAN_POINT('Ctrl Pts',(-59.7842416555146,13.0316624367251,
39.3487519293518));
#204564=CARTESIAN_POINT('Ctrl Pts',(-59.8108054559344,12.9079350417481,
39.349206866293));
#204565=CARTESIAN_POINT('Ctrl Pts',(-59.8961220185276,12.9260696369486,
39.4512271248735));
#204566=CARTESIAN_POINT('Ctrl Pts',(-59.7007958241042,13.0141504107556,
39.3978017080178));
#204567=CARTESIAN_POINT('Ctrl Pts',(-59.727069488887,12.8901364125065,39.3980347781174));
#204568=CARTESIAN_POINT('Ctrl Pts',(-59.7710239514086,12.8994792219302,
39.524801535519));
#204569=CARTESIAN_POINT('Ctrl Pts',(-59.6130003254554,12.9957275188828,
39.3978017080178));
#204570=CARTESIAN_POINT('Ctrl Pts',(-59.6394051101892,12.8715027735896,
39.3978017080178));
#204571=CARTESIAN_POINT('Ctrl Pts',(-59.6394051101892,12.8715027735896,
39.5248017080178));
#204572=CARTESIAN_POINT('Origin',(-59.6130003254554,12.9957275188828,39.5248017080178));
#204573=CARTESIAN_POINT('Origin',(0.0660119618346463,0.310561863232983,
39.116));
#204574=CARTESIAN_POINT('Origin',(-60.4516424606488,13.1739864076111,39.116));
#204575=CARTESIAN_POINT('Origin',(0.0660119618346464,0.310561863232983,
39.5248017080178));
#204576=CARTESIAN_POINT('Origin',(-59.4650964698965,12.9642895838875,39.5248017080178));
#204577=CARTESIAN_POINT('Ctrl Pts',(-60.9782752797347,13.2864868029,39.2875012672119));
#204578=CARTESIAN_POINT('Ctrl Pts',(-61.0052918384388,13.1616357280628,
39.287208709576));
#204579=CARTESIAN_POINT('Ctrl Pts',(-60.8992893541407,13.1392995818864,
39.3549016990121));
#204580=CARTESIAN_POINT('Ctrl Pts',(-60.8658306440996,13.2624669757409,
39.1034939173931));
#204581=CARTESIAN_POINT('Ctrl Pts',(-60.8926675943332,13.1376969719829,
39.1031692336329));
#204582=CARTESIAN_POINT('Ctrl Pts',(-60.809347351947,13.1201818190179,39.2077507202297));
#204583=CARTESIAN_POINT('Ctrl Pts',(-60.663828108008,13.2193155203584,38.989));
#204584=CARTESIAN_POINT('Ctrl Pts',(-60.6905008239721,13.0947255842063,
38.9887769311176));
#204585=CARTESIAN_POINT('Ctrl Pts',(-60.6477702018622,13.0858375353126,
39.1161898712913));
#204586=CARTESIAN_POINT('Ctrl Pts',(-60.4516424606488,13.1739864076111,
38.989));
#204587=CARTESIAN_POINT('Ctrl Pts',(-60.4780866929065,13.0495760763092,
38.989));
#204588=CARTESIAN_POINT('Ctrl Pts',(-60.4780472159603,13.0497618007394,
39.1161895903852));
#204589=CARTESIAN_POINT('Origin',(-60.8730422059013,13.2635576885506,39.3548010137695));
#204590=CARTESIAN_POINT('Ctrl Pts',(-59.4650964698965,12.9642895838875,
39.3978017080178));
#204591=CARTESIAN_POINT('Ctrl Pts',(-59.4915012546304,12.8400648385943,
39.3978017080178));
#204592=CARTESIAN_POINT('Ctrl Pts',(-59.4915012546304,12.8400648385943,
39.5248017080178));
#204593=CARTESIAN_POINT('Ctrl Pts',(-59.3770041141843,12.9458049943934,
39.3978017080178));
#204594=CARTESIAN_POINT('Ctrl Pts',(-59.4033730190104,12.8213326038441,
39.397566602504));
#204595=CARTESIAN_POINT('Ctrl Pts',(-59.3594375597973,12.8119938336991,
39.5248015517196));
#204596=CARTESIAN_POINT('Ctrl Pts',(-59.2937057271822,12.9283282206303,
39.3484894016716));
#204597=CARTESIAN_POINT('Ctrl Pts',(-59.3204640761271,12.8037097640145,
39.348025900003));
#204598=CARTESIAN_POINT('Ctrl Pts',(-59.2345619206666,12.7854506972091,
39.450833318893));
#204599=CARTESIAN_POINT('Ctrl Pts',(-59.2498070616278,12.919118186205,39.2708017080178));
#204600=CARTESIAN_POINT('Ctrl Pts',(-59.2768226962997,12.7944335023712,
39.2705119464801));
#204601=CARTESIAN_POINT('Ctrl Pts',(-59.168751483356,12.7714622569324,39.3343017080178));
#204602=CARTESIAN_POINT('Origin',(-59.1423466986221,12.8956870022256,39.3343017080178));
#204603=CARTESIAN_POINT('Origin',(-61.0472983318862,13.3005969715151,39.6398955068186));
#204604=CARTESIAN_POINT('Origin',(-61.2215544576538,13.337636254483,39.92499));
#204605=CARTESIAN_POINT('Origin',(-59.0627741291273,12.8787733304436,39.1934008539943));
#204606=CARTESIAN_POINT('Origin',(-59.0190342907434,12.8695280801151,39.1160402713849));
#204607=CARTESIAN_POINT('Ctrl Pts',(-61.575271693745,13.1038352065732,40.1599502534424));
#204608=CARTESIAN_POINT('Ctrl Pts',(-61.5387839176327,13.0960702419685,
40.10025));
#204609=CARTESIAN_POINT('Ctrl Pts',(-61.4699285681953,13.0814171332237,
40.10025));
#204610=CARTESIAN_POINT('Ctrl Pts',(-61.5569304518429,13.1900205930481,
40.1599500538462));
#204611=CARTESIAN_POINT('Ctrl Pts',(-61.5254208297815,13.1588482421897,
40.1002448353506));
#204612=CARTESIAN_POINT('Ctrl Pts',(-61.4593031273755,13.1313027022859,
40.10025));
#204613=CARTESIAN_POINT('Ctrl Pts',(-61.5155378539379,13.2643407403248,
40.120244200104));
#204614=CARTESIAN_POINT('Ctrl Pts',(-61.4904936222817,13.2118511391503,
40.0633873868018));
#204615=CARTESIAN_POINT('Ctrl Pts',(-61.4250300340668,13.1721300657495,
40.0772271723538));
#204616=CARTESIAN_POINT('Ctrl Pts',(-61.4222835584425,13.3535591268197,
40.0045995998161));
#204617=CARTESIAN_POINT('Ctrl Pts',(-61.4178880557396,13.2611962587091,
39.9663485808315));
#204618=CARTESIAN_POINT('Ctrl Pts',(-61.341115859575,13.2174099770542,40.0101727202466));
#204619=CARTESIAN_POINT('Ctrl Pts',(-61.3712701109735,13.3700167576329,
39.930465434986));
#204620=CARTESIAN_POINT('Ctrl Pts',(-61.3797074995629,13.2570896192454,
39.9051900162948));
#204621=CARTESIAN_POINT('Ctrl Pts',(-61.2924393404521,13.2228660458971,
39.9671857458177));
#204622=CARTESIAN_POINT('Ctrl Pts',(-61.3267881959112,13.3605623192491,
39.8576902534424));
#204623=CARTESIAN_POINT('Ctrl Pts',(-61.3537611057082,13.2359003894755,
39.8573998014387));
#204624=CARTESIAN_POINT('Ctrl Pts',(-61.2479592423877,13.2134115091898,
39.92499));
#204625=CARTESIAN_POINT('Origin',(-61.4699285681953,13.0814171332237,40.22725));
#204626=CARTESIAN_POINT('Origin',(0.0660119618346463,0.310561863232983,
39.116));
#204627=CARTESIAN_POINT('Origin',(-58.6264539577983,12.7860306150456,39.116));
#204628=CARTESIAN_POINT('Origin',(1.31078692950418E-16,-3.42824740397364E-17,
40.22725));
#204629=CARTESIAN_POINT('Origin',(-61.4762657165315,13.0516031943533,40.22725));
#204630=CARTESIAN_POINT('Ctrl Pts',(-58.6264539577983,12.7860306150456,
38.989));
#204631=CARTESIAN_POINT('Ctrl Pts',(-58.6528982980921,12.6616197754741,
38.989));
#204632=CARTESIAN_POINT('Ctrl Pts',(-58.6528587129484,12.6618060089325,
39.1161901092325));
#204633=CARTESIAN_POINT('Ctrl Pts',(-58.4142663981466,12.7406940127372,
38.989));
#204634=CARTESIAN_POINT('Ctrl Pts',(-58.4408495151712,12.6165479409689,
38.989229898976));
#204635=CARTESIAN_POINT('Ctrl Pts',(-58.4831327254077,12.625729636332,39.1161900493205));
#204636=CARTESIAN_POINT('Ctrl Pts',(-58.2122676405432,12.6975319705102,
39.1034966344368));
#204637=CARTESIAN_POINT('Ctrl Pts',(-58.2389323335231,12.5736296288405,
39.1038314102556));
#204638=CARTESIAN_POINT('Ctrl Pts',(-58.3215567776493,12.591385608175,39.2077528789596));
#204639=CARTESIAN_POINT('Ctrl Pts',(-58.0998260601479,12.6735055745745,
39.2875012672119));
#204640=CARTESIAN_POINT('Ctrl Pts',(-58.1266254943012,12.5497583536235,
39.2878045257868));
#204641=CARTESIAN_POINT('Ctrl Pts',(-58.2316158778879,12.5722680796269,
39.3549015295901));
#204642=CARTESIAN_POINT('Origin',(-58.2050537810541,12.6964592423897,39.3548010137695));
#204643=CARTESIAN_POINT('Ctrl Pts',(-61.4590390555208,12.7383709431255,
39.8576902534424));
#204644=CARTESIAN_POINT('Ctrl Pts',(-61.4329754599098,12.8632261535959,
39.8573998014387));
#204645=CARTESIAN_POINT('Ctrl Pts',(-61.3271735965892,12.8407372733102,
39.92499));
#204646=CARTESIAN_POINT('Ctrl Pts',(-61.5035409747668,12.7478306169679,
39.9304984902493));
#204647=CARTESIAN_POINT('Ctrl Pts',(-61.4653154597751,12.8544171899343,
39.9052171569796));
#204648=CARTESIAN_POINT('Ctrl Pts',(-61.3716739624481,12.8501961180703,
39.9672049726606));
#204649=CARTESIAN_POINT('Ctrl Pts',(-61.5432717953611,12.7835835513933,
40.004343767866));
#204650=CARTESIAN_POINT('Ctrl Pts',(-61.5017184029588,12.8662481012971,
39.9661628577639));
#204651=CARTESIAN_POINT('Ctrl Pts',(-61.4137451613968,12.8749453072906,
40.0100243556235));
#204652=CARTESIAN_POINT('Ctrl Pts',(-61.5920631419345,12.9020280679176,
40.119487482199));
#204653=CARTESIAN_POINT('Ctrl Pts',(-61.5478406570045,12.9401487584129,
40.0627551483143));
#204654=CARTESIAN_POINT('Ctrl Pts',(-61.4717924962547,12.9498405053867,
40.0767884282377));
#204655=CARTESIAN_POINT('Ctrl Pts',(-61.5999795805214,12.9874904696725,
40.1599502015393));
#204656=CARTESIAN_POINT('Ctrl Pts',(-61.5585057825381,13.0031958218446,
40.1002449453872));
#204657=CARTESIAN_POINT('Ctrl Pts',(-61.4868843017924,13.0015435854429,
40.10025));
#204658=CARTESIAN_POINT('Ctrl Pts',(-61.5816197022697,13.0739701745329,
40.1599502534424));
#204659=CARTESIAN_POINT('Ctrl Pts',(-61.5451281645058,13.0662229071071,
40.10025));
#204660=CARTESIAN_POINT('Ctrl Pts',(-61.4762657165315,13.0516031943533,
40.10025));
#204661=CARTESIAN_POINT('Origin',(-61.3535783813231,12.7165125280171,39.92499));
#204662=CARTESIAN_POINT('Origin',(-58.0307974155445,12.6594199084583,39.6398955069315));
#204663=CARTESIAN_POINT('Origin',(-57.8565410498766,12.6223805745523,39.92499));
#204664=CARTESIAN_POINT('Origin',(-61.1793222555316,12.6794732450921,39.6398955068276));
#204665=CARTESIAN_POINT('Origin',(-61.0050661295705,12.6424339620847,39.3548010137695));
#204666=CARTESIAN_POINT('Ctrl Pts',(-57.7513140650719,12.5994235324476,
39.8576902534424));
#204667=CARTESIAN_POINT('Ctrl Pts',(-57.7780756236494,12.4758649777957,
39.8579948730703));
#204668=CARTESIAN_POINT('Ctrl Pts',(-57.8829458346104,12.4981558292591,
39.92499));
#204669=CARTESIAN_POINT('Ctrl Pts',(-57.7068710254542,12.589976329008,39.9304020711232));
#204670=CARTESIAN_POINT('Ctrl Pts',(-57.7455616498597,12.4844883578133,
39.9058915297387));
#204671=CARTESIAN_POINT('Ctrl Pts',(-57.8385008428012,12.4887087546167,
39.9671523786036));
#204672=CARTESIAN_POINT('Ctrl Pts',(-57.6673720419787,12.5543975270271,
40.0043257306691));
#204673=CARTESIAN_POINT('Ctrl Pts',(-57.7092008760999,12.4724506530563,
39.9667894847835));
#204674=CARTESIAN_POINT('Ctrl Pts',(-57.7966870296831,12.4640308112195,
40.0100138975199));
#204675=CARTESIAN_POINT('Ctrl Pts',(-57.6192799956671,12.4363816727426,
40.119553305486));
#204676=CARTESIAN_POINT('Ctrl Pts',(-57.6635313090883,12.3985321242203,
40.0630813209237));
#204677=CARTESIAN_POINT('Ctrl Pts',(-57.7394080294755,12.3892398894927,
40.0768265942422));
#204678=CARTESIAN_POINT('Ctrl Pts',(-57.611816644779,12.3512461790955,40.1599502027525));
#204679=CARTESIAN_POINT('Ctrl Pts',(-57.6532646075487,12.3356888898089,
40.1002552791541));
#204680=CARTESIAN_POINT('Ctrl Pts',(-57.7248239067135,12.3376071226711,
40.10025));
#204681=CARTESIAN_POINT('Ctrl Pts',(-57.6301266171956,12.2652136052665,
40.1599502534424));
#204682=CARTESIAN_POINT('Ctrl Pts',(-57.6666142715154,12.2729791421559,
40.10025));
#204683=CARTESIAN_POINT('Ctrl Pts',(-57.7354693911204,12.2876333308475,
40.10025));
#204684=CARTESIAN_POINT('Origin',(-57.7354693911203,12.2876333308475,40.22725));
#204685=CARTESIAN_POINT('Ctrl Pts',(-60.5836663843181,12.5528626811452,
38.989));
#204686=CARTESIAN_POINT('Ctrl Pts',(-60.5572221497821,12.677273023165,38.989));
#204687=CARTESIAN_POINT('Ctrl Pts',(-60.55726162901,12.6770872880009,39.1161896013262));
#204688=CARTESIAN_POINT('Ctrl Pts',(-60.7959479326852,12.5977568525207,
38.989));
#204689=CARTESIAN_POINT('Ctrl Pts',(-60.7696393833354,12.7224242094577,
38.9887769275485));
#204690=CARTESIAN_POINT('Ctrl Pts',(-60.7269872521295,12.713163582625,39.1161898821844));
#204691=CARTESIAN_POINT('Ctrl Pts',(-60.99803611366,12.6404975322971,39.1034967087243));
#204692=CARTESIAN_POINT('Ctrl Pts',(-60.9718043534717,12.7653961862424,
39.1031720232704));
#204693=CARTESIAN_POINT('Ctrl Pts',(-60.8885631223998,12.7475075938196,
39.2077529615006));
#204694=CARTESIAN_POINT('Ctrl Pts',(-61.110527437164,12.6642893210146,39.2875012672119));
#204695=CARTESIAN_POINT('Ctrl Pts',(-61.0844267823321,12.7893350885048,
39.2872087095508));
#204696=CARTESIAN_POINT('Ctrl Pts',(-60.9785037583493,12.7666250660189,
39.3549017048226));
#204697=CARTESIAN_POINT('Origin',(-60.5836663843181,12.5528626811452,39.116));
#204698=CARTESIAN_POINT('Origin',(3.545935779686E-16,1.21955273767085E-17,
40.22725));
#204699=CARTESIAN_POINT('Origin',(-57.7418065394565,12.2578193919772,40.22725));
#204700=CARTESIAN_POINT('Origin',(59.4667368016499,-12.964638247165,39.116));
#204701=CARTESIAN_POINT('Origin',(-60.191094087497,12.4693660187274,39.1160373285259));
#204702=CARTESIAN_POINT('Ctrl Pts',(-57.6364522029206,12.2354540642049,
40.1599502534424));
#204703=CARTESIAN_POINT('Ctrl Pts',(-57.6729438621905,12.2432007592851,
40.10025));
#204704=CARTESIAN_POINT('Ctrl Pts',(-57.7418065394565,12.2578193919772,
40.10025));
#204705=CARTESIAN_POINT('Ctrl Pts',(-57.6546556225243,12.1497054461947,
40.1599500566034));
#204706=CARTESIAN_POINT('Ctrl Pts',(-57.6862025493677,12.1807288143667,
40.1002551305381));
#204707=CARTESIAN_POINT('Ctrl Pts',(-57.7523715145536,12.208006627196,40.10025));
#204708=CARTESIAN_POINT('Ctrl Pts',(-57.6955109599434,12.0754939174601,
40.1203070619047));
#204709=CARTESIAN_POINT('Ctrl Pts',(-57.7206875210979,12.1277502414154,
40.0637098684499));
#204710=CARTESIAN_POINT('Ctrl Pts',(-57.7861609236006,12.1670355805166,
40.0772636213362));
#204711=CARTESIAN_POINT('Ctrl Pts',(-57.7879231380266,11.9863964689869,
40.0046102245801));
#204712=CARTESIAN_POINT('Ctrl Pts',(-57.7928648378994,12.0782086782664,
39.9670001894012));
#204713=CARTESIAN_POINT('Ctrl Pts',(-57.8693039540644,12.1215423041377,
40.0101788811209));
#204714=CARTESIAN_POINT('Ctrl Pts',(-57.8386735460213,11.9699873265229,
39.9303710930187));
#204715=CARTESIAN_POINT('Ctrl Pts',(-57.8311081991708,12.0820993460745,
39.9058663574107));
#204716=CARTESIAN_POINT('Ctrl Pts',(-57.9177340744071,12.1160385312533,
39.9671344706365));
#204717=CARTESIAN_POINT('Ctrl Pts',(-57.8830978693155,11.9794294790616,
39.8576902534424));
#204718=CARTESIAN_POINT('Ctrl Pts',(-57.857289977851,12.1031907419161,39.8579948730704));
#204719=CARTESIAN_POINT('Ctrl Pts',(-57.962160188812,12.1254815933796,39.92499));
#204720=CARTESIAN_POINT('Origin',(-57.9885649735458,12.0012568480864,39.92499));
#204721=CARTESIAN_POINT('Origin',(-60.1478239214169,12.460221505806,39.192555448885));
#204722=CARTESIAN_POINT('Origin',(-60.0677739512125,12.4432063593727,39.3343017080178));
#204723=CARTESIAN_POINT('Origin',(-58.1628213391877,12.0382961820444,39.6398955069223));
#204724=CARTESIAN_POINT('Origin',(-58.3370777047234,12.0753355159237,39.3548010137695));
#204725=CARTESIAN_POINT('Ctrl Pts',(-59.7450242491247,12.3746037924168,
39.3978017080178));
#204726=CARTESIAN_POINT('Ctrl Pts',(-59.7186194643908,12.49882853771,39.3978017080178));
#204727=CARTESIAN_POINT('Ctrl Pts',(-59.7186194643908,12.49882853771,39.5248017080178));
#204728=CARTESIAN_POINT('Ctrl Pts',(-59.83301908937,12.3935470970144,39.3978017080178));
#204729=CARTESIAN_POINT('Ctrl Pts',(-59.8065803155741,12.5175251937995,
39.3980355775177));
#204730=CARTESIAN_POINT('Ctrl Pts',(-59.8506831473907,12.52689954009,39.5248015517192));
#204731=CARTESIAN_POINT('Ctrl Pts',(-59.9162252185216,12.411457631101,39.3484893995498));
#204732=CARTESIAN_POINT('Ctrl Pts',(-59.8901687840302,12.5352924712482,
39.3489438303431));
#204733=CARTESIAN_POINT('Ctrl Pts',(-59.9755587548362,12.553442669845,39.4508333155594));
#204734=CARTESIAN_POINT('Ctrl Pts',(-59.9600752506736,12.4208962741591,
39.2708017080178));
#204735=CARTESIAN_POINT('Ctrl Pts',(-59.9342688867324,12.5446662374491,
39.2710850691866));
#204736=CARTESIAN_POINT('Ctrl Pts',(-60.0413691664786,12.5674311046659,
39.3343017080178));
#204737=CARTESIAN_POINT('Origin',(-59.7450242491247,12.3746037924168,39.5248017080178));
#204738=CARTESIAN_POINT('Ctrl Pts',(-58.231611300478,12.0535047649326,39.2875012672119));
#204739=CARTESIAN_POINT('Ctrl Pts',(-58.2057612755554,12.1774537741288,
39.2878045257519));
#204740=CARTESIAN_POINT('Ctrl Pts',(-58.3108302788452,12.1995935640852,
39.3549015218347));
#204741=CARTESIAN_POINT('Ctrl Pts',(-58.3441059109579,12.0772900304171,
39.1034938540228));
#204742=CARTESIAN_POINT('Ctrl Pts',(-58.3180696991556,12.2013259468607,
39.1038286278809));
#204743=CARTESIAN_POINT('Ctrl Pts',(-58.4007725402744,12.2187113817821,
39.2077506434029));
#204744=CARTESIAN_POINT('Ctrl Pts',(-58.5461981381262,12.120020176779,38.989));
#204745=CARTESIAN_POINT('Ctrl Pts',(-58.5199882620682,12.2442455720376,
38.9892298954611));
#204746=CARTESIAN_POINT('Ctrl Pts',(-58.5623497685531,12.2530556816164,
39.1161900347289));
#204747=CARTESIAN_POINT('Ctrl Pts',(-58.7584778814675,12.1649068885796,
38.989));
#204748=CARTESIAN_POINT('Ctrl Pts',(-58.732033544228,12.2893177137821,38.989));
#204749=CARTESIAN_POINT('Ctrl Pts',(-58.7320731263128,12.2891314947141,
39.1161900945645));
#204750=CARTESIAN_POINT('Origin',(-58.7584778814675,12.1649068885796,39.116));
#204751=CARTESIAN_POINT('Origin',(58.0246834617327,-12.6581203474874,39.5248017080178));
#204752=CARTESIAN_POINT('Origin',(-59.5971203935658,12.3431658574215,39.5248017080178));
#204753=CARTESIAN_POINT('Origin',(57.798864262886,-12.6101209950214,39.116));
#204754=CARTESIAN_POINT('Origin',(-59.1510793400376,12.2483049654019,39.1160402713836));
#204755=CARTESIAN_POINT('Ctrl Pts',(-59.382070869907,12.2968658913807,39.2708017080178));
#204756=CARTESIAN_POINT('Ctrl Pts',(-59.3560370505013,12.4217592664917,
39.27051194648));
#204757=CARTESIAN_POINT('Ctrl Pts',(-59.2479658375575,12.3987880210528,
39.3343017080178));
#204758=CARTESIAN_POINT('Ctrl Pts',(-59.4260685345959,12.3063392072229,
39.3487519301185));
#204759=CARTESIAN_POINT('Ctrl Pts',(-59.3998259533518,12.4310668851203,
39.3482879463966));
#204760=CARTESIAN_POINT('Ctrl Pts',(-59.3139986558985,12.4128237298768,
39.4512271261623));
#204761=CARTESIAN_POINT('Ctrl Pts',(-59.5094220566594,12.3242857901781,
39.3978017080178));
#204762=CARTESIAN_POINT('Ctrl Pts',(-59.4828840257723,12.4487214234132,
39.3975673827415));
#204763=CARTESIAN_POINT('Ctrl Pts',(-59.4390967537827,12.4394141514345,
39.5248015355199));
#204764=CARTESIAN_POINT('Ctrl Pts',(-59.5971203935658,12.3431658574215,
39.3978017080178));
#204765=CARTESIAN_POINT('Ctrl Pts',(-59.570715608832,12.4673906027147,39.3978017080178));
#204766=CARTESIAN_POINT('Ctrl Pts',(-59.570715608832,12.4673906027147,39.5248017080178));
#204767=CARTESIAN_POINT('Origin',(-59.2743706222914,12.2745632757596,39.3343017080178));
#204768=CARTESIAN_POINT('Origin',(-59.1947980539414,12.2576496039199,39.1934008533547));
#204769=CARTESIAN_POINT('Origin',(-58.3196542523184,19.2830435999574,39.1925554495077));
#204770=CARTESIAN_POINT('Origin',(-58.3616995707146,19.2967593024446,39.1160373285253));
#204771=CARTESIAN_POINT('Origin',(-58.2418213702172,19.2577541638583,39.3343017080178));
#204772=CARTESIAN_POINT('Ctrl Pts',(-58.1373965169892,19.2232259141444,
39.2708017080178));
#204773=CARTESIAN_POINT('Ctrl Pts',(-58.1769325318818,19.1031347997392,
39.2710850691866));
#204774=CARTESIAN_POINT('Ctrl Pts',(-58.2810665285028,19.1369699862888,
39.3343017080178));
#204775=CARTESIAN_POINT('Ctrl Pts',(-58.0945576760634,19.2094285342449,
39.3487519293518));
#204776=CARTESIAN_POINT('Ctrl Pts',(-58.1339089916615,19.0891556041209,
39.349206866292));
#204777=CARTESIAN_POINT('Ctrl Pts',(-58.2168625998337,19.1161088652887,
39.4512271248733));
#204778=CARTESIAN_POINT('Ctrl Pts',(-58.0133994748122,19.1832899764614,
39.3978017080178));
#204779=CARTESIAN_POINT('Ctrl Pts',(-58.0524922023739,19.0627016856755,
39.3980347781174));
#204780=CARTESIAN_POINT('Ctrl Pts',(-58.0952292882366,19.0765878066328,
39.524801535519));
#204781=CARTESIAN_POINT('Ctrl Pts',(-57.9280106456674,19.155790878563,39.3978017080178));
#204782=CARTESIAN_POINT('Ctrl Pts',(-57.967255803953,19.0350067009935,39.3978017080178));
#204783=CARTESIAN_POINT('Ctrl Pts',(-57.967255803953,19.0350067009935,39.5248017080178));
#204784=CARTESIAN_POINT('Origin',(-57.9280106456674,19.1557908785629,39.5248017080178));
#204785=CARTESIAN_POINT('Origin',(0.0981128957140535,0.301960443923711,
39.116));
#204786=CARTESIAN_POINT('Origin',(-58.7434254837931,19.4207352200705,39.116));
#204787=CARTESIAN_POINT('Origin',(0.0981128957140536,0.301960443923711,
39.5248017080178));
#204788=CARTESIAN_POINT('Origin',(-57.7842031819381,19.109065001132,39.5248017080178));
#204789=CARTESIAN_POINT('Ctrl Pts',(-59.255413859757,19.5876674457083,39.2875012672119));
#204790=CARTESIAN_POINT('Ctrl Pts',(-59.2953329099158,19.4663243174863,
39.287208709576));
#204791=CARTESIAN_POINT('Ctrl Pts',(-59.1922458813527,19.4330302542696,
39.3549016990123));
#204792=CARTESIAN_POINT('Ctrl Pts',(-59.1460959632216,19.5520255367114,
39.1034939173931));
#204793=CARTESIAN_POINT('Ctrl Pts',(-59.1858279145868,19.4307442612513,
39.1031692336319));
#204794=CARTESIAN_POINT('Ctrl Pts',(-59.1047949412326,19.4046157212343,
39.2077507202296));
#204795=CARTESIAN_POINT('Ctrl Pts',(-58.949710573478,19.4879954548411,38.989));
#204796=CARTESIAN_POINT('Ctrl Pts',(-58.9892603680799,19.3668760934068,
38.98877693112));
#204797=CARTESIAN_POINT('Ctrl Pts',(-58.9476928828783,19.3535701679106,
39.1161898712916));
#204798=CARTESIAN_POINT('Ctrl Pts',(-58.7434254837931,19.4207352200705,
38.989));
#204799=CARTESIAN_POINT('Ctrl Pts',(-58.7827292725253,19.2997705965407,
38.989));
#204800=CARTESIAN_POINT('Ctrl Pts',(-58.7826705983485,19.2999511770888,
39.1161895903855));
#204801=CARTESIAN_POINT('Origin',(-59.1531540087997,19.5538640879537,39.3548010137695));
#204802=CARTESIAN_POINT('Ctrl Pts',(-57.7842031819381,19.109065001132,39.3978017080178));
#204803=CARTESIAN_POINT('Ctrl Pts',(-57.8234483402237,18.9882808235625,
39.3978017080178));
#204804=CARTESIAN_POINT('Ctrl Pts',(-57.8234483402237,18.9882808235625,
39.5248017080178));
#204805=CARTESIAN_POINT('Ctrl Pts',(-57.6985255711015,19.0814735135857,
39.3978017080178));
#204806=CARTESIAN_POINT('Ctrl Pts',(-57.7377609320107,18.9604392969153,
39.3975666025021));
#204807=CARTESIAN_POINT('Ctrl Pts',(-57.6950423231344,18.9465591794954,
39.5248015517196));
#204808=CARTESIAN_POINT('Ctrl Pts',(-57.6175103216837,19.0553854270309,
39.3484894016717));
#204809=CARTESIAN_POINT('Ctrl Pts',(-57.6571482613595,18.9342466524521,
39.3480259000043));
#204810=CARTESIAN_POINT('Ctrl Pts',(-57.5736252790853,18.9071083904254,
39.4508333188935));
#204811=CARTESIAN_POINT('Ctrl Pts',(-57.5748148483574,19.0416371860882,
39.2708017080178));
#204812=CARTESIAN_POINT('Ctrl Pts',(-57.61471558695,18.920459440775,39.27051194648));
#204813=CARTESIAN_POINT('Ctrl Pts',(-57.5096375484035,18.8863175164097,
39.3343017080178));
#204814=CARTESIAN_POINT('Origin',(-57.4703923901179,19.0071016939792,39.3343017080178));
#204815=CARTESIAN_POINT('Origin',(-59.322583882164,19.6089151909166,39.6398955068188));
#204816=CARTESIAN_POINT('Origin',(-59.4920137553138,19.6639662938566,39.92499));
#204817=CARTESIAN_POINT('Origin',(-57.393023687604,18.9819630786532,39.1934008539945));
#204818=CARTESIAN_POINT('Origin',(-57.3504898524412,18.9681964166833,39.1160402713845));
#204819=CARTESIAN_POINT('Ctrl Pts',(-59.868232155624,19.4684195516701,40.1599502534424));
#204820=CARTESIAN_POINT('Ctrl Pts',(-59.8327559231845,19.4568831131889,
40.10025));
#204821=CARTESIAN_POINT('Ctrl Pts',(-59.765809437495,19.4351129318425,40.10025));
#204822=CARTESIAN_POINT('Ctrl Pts',(-59.8409825629598,19.5522156237499,
40.1599500538463));
#204823=CARTESIAN_POINT('Ctrl Pts',(-59.8129039518352,19.5179203859182,
40.100244835349));
#204824=CARTESIAN_POINT('Ctrl Pts',(-59.750027742079,19.4836145615375,40.10025));
#204825=CARTESIAN_POINT('Ctrl Pts',(-59.7920481472522,19.6218019328335,
40.1202442001036));
#204826=CARTESIAN_POINT('Ctrl Pts',(-59.7726277678653,19.5669820401376,
40.0633873868015));
#204827=CARTESIAN_POINT('Ctrl Pts',(-59.7116747787978,19.5206357546568,
40.0772271723537));
#204828=CARTESIAN_POINT('Ctrl Pts',(-59.6899788477097,19.7007838434714,
40.0045995998165));
#204829=CARTESIAN_POINT('Ctrl Pts',(-59.6952619726975,19.6084674936735,
39.9663485808317));
#204830=CARTESIAN_POINT('Ctrl Pts',(-59.6234872553903,19.5568961981642,
40.0101727202466));
#204831=CARTESIAN_POINT('Ctrl Pts',(-59.6375245663854,19.7118189603904,
39.9304654349857));
#204832=CARTESIAN_POINT('Ctrl Pts',(-59.6577198343148,19.6003923959452,
39.9051900162946));
#204833=CARTESIAN_POINT('Ctrl Pts',(-59.5745070768387,19.5572342963495,
39.9671857458178));
#204834=CARTESIAN_POINT('Ctrl Pts',(-59.5942745858234,19.697766688185,39.8576902534424));
#204835=CARTESIAN_POINT('Ctrl Pts',(-59.6341304551456,19.5766071063173,
39.8573998014387));
#204836=CARTESIAN_POINT('Ctrl Pts',(-59.5312589135994,19.5431821162871,
39.92499));
#204837=CARTESIAN_POINT('Origin',(-59.765809437495,19.4351129318425,40.22725));
#204838=CARTESIAN_POINT('Origin',(0.0981128957140535,0.301960443923711,
39.116));
#204839=CARTESIAN_POINT('Origin',(-56.9687879773464,18.8441205405524,39.116));
#204840=CARTESIAN_POINT('Origin',(1.26611655068499E-16,-5.09536863743859E-17,
40.22725));
#204841=CARTESIAN_POINT('Origin',(-59.7752282754835,19.4061247292258,40.22725));
#204842=CARTESIAN_POINT('Ctrl Pts',(-56.9687879773464,18.8441205405524,
38.989));
#204843=CARTESIAN_POINT('Ctrl Pts',(-57.0080919266514,18.7231554228306,
38.989));
#204844=CARTESIAN_POINT('Ctrl Pts',(-57.0080330916622,18.7233364983083,
39.1161901092323));
#204845=CARTESIAN_POINT('Ctrl Pts',(-56.762501768717,18.776852657361,38.989));
#204846=CARTESIAN_POINT('Ctrl Pts',(-56.801916058748,18.6561653631345,38.989229898976));
#204847=CARTESIAN_POINT('Ctrl Pts',(-56.8430078886277,18.6697165591972,
39.1161900493203));
#204848=CARTESIAN_POINT('Ctrl Pts',(-56.5661212433882,18.7128124416044,
39.1034966344368));
#204849=CARTESIAN_POINT('Ctrl Pts',(-56.60559118576,18.5923760693073,39.1038314102556));
#204850=CARTESIAN_POINT('Ctrl Pts',(-56.6859069993035,18.6186713857,39.2077528789596));
#204851=CARTESIAN_POINT('Ctrl Pts',(-56.456807071981,18.6771643191714,39.2875012672119));
#204852=CARTESIAN_POINT('Ctrl Pts',(-56.4963948028695,18.5568963021134,
39.2878045257868));
#204853=CARTESIAN_POINT('Ctrl Pts',(-56.5984571310817,18.5902572009365,
39.35490152959));
#204854=CARTESIAN_POINT('Origin',(-56.5590590327988,18.7109915363521,39.3548010137695));
#204855=CARTESIAN_POINT('Ctrl Pts',(-59.790837669791,19.0928077206416,39.8576902534424));
#204856=CARTESIAN_POINT('Ctrl Pts',(-59.7518659300024,19.2142545736088,
39.8573998014387));
#204857=CARTESIAN_POINT('Ctrl Pts',(-59.6489943884562,19.1808295835786,
39.92499));
#204858=CARTESIAN_POINT('Ctrl Pts',(-59.834106997697,19.1068672906329,39.9304984902492));
#204859=CARTESIAN_POINT('Ctrl Pts',(-59.7849495554007,19.2088743168613,
39.9052171569785));
#204860=CARTESIAN_POINT('Ctrl Pts',(-59.6922622581482,19.1948881666556,
39.9672049726599));
#204861=CARTESIAN_POINT('Ctrl Pts',(-59.8698829694066,19.146577368363,40.0043437678661));
#204862=CARTESIAN_POINT('Ctrl Pts',(-59.8199164124675,19.2244455609614,
39.9661628577646));
#204863=CARTESIAN_POINT('Ctrl Pts',(-59.7315159919505,19.2238994150017,
40.0100243556235));
#204864=CARTESIAN_POINT('Ctrl Pts',(-59.9060262085834,19.2694731179107,
40.1194874821988));
#204865=CARTESIAN_POINT('Ctrl Pts',(-59.8580612818569,19.3027624708837,
40.0627551483138));
#204866=CARTESIAN_POINT('Ctrl Pts',(-59.7814166574708,19.3044519280755,
40.0767884282377));
#204867=CARTESIAN_POINT('Ctrl Pts',(-59.9049660265685,19.3552948408467,
40.1599502015386));
#204868=CARTESIAN_POINT('Ctrl Pts',(-59.8620777700628,19.3665789650872,
40.1002449453863));
#204869=CARTESIAN_POINT('Ctrl Pts',(-59.791021345013,19.3574492964898,40.10025));
#204870=CARTESIAN_POINT('Ctrl Pts',(-59.8776671349984,19.4393816709761,
40.1599502534424));
#204871=CARTESIAN_POINT('Ctrl Pts',(-59.8421853116551,19.4278624395271,
40.10025));
#204872=CARTESIAN_POINT('Ctrl Pts',(-59.7752282754835,19.4061247292258,
40.10025));
#204873=CARTESIAN_POINT('Origin',(-59.6882395467419,19.0600454060092,39.92499));
#204874=CARTESIAN_POINT('Origin',(-56.3896289265485,18.655940357667,39.6398955069316));
#204875=CARTESIAN_POINT('Origin',(-56.2201988201381,18.600889178989,39.92499));
#204876=CARTESIAN_POINT('Origin',(-59.5188096735653,19.004994303108,39.6398955068273));
#204877=CARTESIAN_POINT('Origin',(-59.3493798002278,18.9499432001062,39.3548010137695));
#204878=CARTESIAN_POINT('Ctrl Pts',(-56.1179479440987,18.567058682947,39.8576902534424));
#204879=CARTESIAN_POINT('Ctrl Pts',(-56.1574782858996,18.4469743395784,
39.8579948730703));
#204880=CARTESIAN_POINT('Ctrl Pts',(-56.2594439784237,18.4801050014195,
39.92499));
#204881=CARTESIAN_POINT('Ctrl Pts',(-56.0747358697602,18.5530176696414,
39.930402071123));
#204882=CARTESIAN_POINT('Ctrl Pts',(-56.1242410384002,18.4521518441034,
39.9058915297388));
#204883=CARTESIAN_POINT('Ctrl Pts',(-56.2162299491246,18.4660639121466,
39.967152378603));
#204884=CARTESIAN_POINT('Ctrl Pts',(-56.0391722633446,18.5135050040176,
40.0043257306694));
#204885=CARTESIAN_POINT('Ctrl Pts',(-56.0893377355407,18.4363793473478,
39.9667894847842));
#204886=CARTESIAN_POINT('Ctrl Pts',(-56.1772247439496,18.4371504234765,
40.0100138975201));
#204887=CARTESIAN_POINT('Ctrl Pts',(-56.0036796861844,18.3911086652353,
40.1195533054856));
#204888=CARTESIAN_POINT('Ctrl Pts',(-56.0516449414237,18.3580919822893,
40.0630813209231));
#204889=CARTESIAN_POINT('Ctrl Pts',(-56.1280773042134,18.3567819283759,
40.076826594242));
#204890=CARTESIAN_POINT('Ctrl Pts',(-56.0051563026338,18.3056594201307,
40.1599502027523));
#204891=CARTESIAN_POINT('Ctrl Pts',(-56.0480033886678,18.2945198471566,
40.1002552791563));
#204892=CARTESIAN_POINT('Ctrl Pts',(-56.1189701685705,18.3039075553122,
40.10025));
#204893=CARTESIAN_POINT('Ctrl Pts',(-56.032358823839,18.2220120550221,40.1599502534424));
#204894=CARTESIAN_POINT('Ctrl Pts',(-56.0678348753331,18.2335490499222,
40.10025));
#204895=CARTESIAN_POINT('Ctrl Pts',(-56.134781019564,18.2553202812753,40.10025));
#204896=CARTESIAN_POINT('Origin',(-56.1347810195641,18.2553202812753,40.22725));
#204897=CARTESIAN_POINT('Ctrl Pts',(-58.9396512752212,18.8168143322231,
38.989));
#204898=CARTESIAN_POINT('Ctrl Pts',(-58.9003474831028,18.9377789661744,
38.989));
#204899=CARTESIAN_POINT('Ctrl Pts',(-58.9004061606708,18.9375983751893,
39.1161896013269));
#204900=CARTESIAN_POINT('Ctrl Pts',(-59.1460772043116,18.8836520326607,
38.989));
#204901=CARTESIAN_POINT('Ctrl Pts',(-59.1068814887041,19.0048864565377,
38.988776927546));
#204902=CARTESIAN_POINT('Ctrl Pts',(-59.0654310094273,18.9912181986575,
39.116189882185));
#204903=CARTESIAN_POINT('Ctrl Pts',(-59.3425907075095,18.947282541525,39.1034967087243));
#204904=CARTESIAN_POINT('Ctrl Pts',(-59.3034471832914,19.0687550219954,
39.103172023271));
#204905=CARTESIAN_POINT('Ctrl Pts',(-59.222531823469,19.0422633471882,39.2077529614998));
#204906=CARTESIAN_POINT('Ctrl Pts',(-59.4519788726606,18.9827025415101,
39.2875012672119));
#204907=CARTESIAN_POINT('Ctrl Pts',(-59.4129503580328,19.104335033863,39.2872087095507));
#204908=CARTESIAN_POINT('Ctrl Pts',(-59.3099814352091,19.0706774483342,
39.3549017048229));
#204909=CARTESIAN_POINT('Origin',(-58.9396512752212,18.8168143322231,39.116));
#204910=CARTESIAN_POINT('Origin',(3.56182666396656E-16,1.81260861279374E-17,
40.22725));
#204911=CARTESIAN_POINT('Origin',(-56.1441998575526,18.2263320786586,40.22725));
#204912=CARTESIAN_POINT('Origin',(56.1826270286323,-18.588681363906,39.116));
#204913=CARTESIAN_POINT('Origin',(-58.5579573083284,18.6927400943502,39.116037328526));
#204914=CARTESIAN_POINT('Ctrl Pts',(-56.0417604764382,18.1930767435953,
40.1599502534424));
#204915=CARTESIAN_POINT('Ctrl Pts',(-56.0772424804483,18.204595418535,40.10025));
#204916=CARTESIAN_POINT('Ctrl Pts',(-56.1441998575526,18.2263320786586,
40.10025));
#204917=CARTESIAN_POINT('Ctrl Pts',(-56.0688273470725,18.1097006409638,
40.1599500566036));
#204918=CARTESIAN_POINT('Ctrl Pts',(-56.0969586315472,18.1438516116619,
40.1002551305369));
#204919=CARTESIAN_POINT('Ctrl Pts',(-56.1599138083641,18.1778965340261,
40.10025));
#204920=CARTESIAN_POINT('Ctrl Pts',(-56.1172160917338,18.0401661963856,
40.1203070619047));
#204921=CARTESIAN_POINT('Ctrl Pts',(-56.136792459813,18.0947679219786,40.0637098684496));
#204922=CARTESIAN_POINT('Ctrl Pts',(-56.1978007560409,18.14068188603,40.0772636213364));
#204923=CARTESIAN_POINT('Ctrl Pts',(-56.2184352456064,17.9612165360194,
40.0046102245801));
#204924=CARTESIAN_POINT('Ctrl Pts',(-56.2137528851849,18.0530423367035,
39.9670001894015));
#204925=CARTESIAN_POINT('Ctrl Pts',(-56.2852436625537,18.1041286397848,
40.0101788811208));
#204926=CARTESIAN_POINT('Ctrl Pts',(-56.2706228600015,17.9502021467121,
39.9303710930187));
#204927=CARTESIAN_POINT('Ctrl Pts',(-56.2513800597996,18.0609092108084,
39.9058663574117));
#204928=CARTESIAN_POINT('Ctrl Pts',(-56.3339837785519,18.1037173431996,
39.9671344706371));
#204929=CARTESIAN_POINT('Ctrl Pts',(-56.3138168485093,17.9642361803977,
39.8576902534424));
#204930=CARTESIAN_POINT('Ctrl Pts',(-56.2752137607564,18.0846218068699,
39.8579948730703));
#204931=CARTESIAN_POINT('Ctrl Pts',(-56.3771794532806,18.117752468711,39.92499));
#204932=CARTESIAN_POINT('Origin',(-56.4164246115662,17.9969682911416,39.92499));
#204933=CARTESIAN_POINT('Origin',(-58.5158800426271,18.6791227120623,39.1925554488845));
#204934=CARTESIAN_POINT('Origin',(-58.4380471616453,18.6538332760109,39.3343017080178));
#204935=CARTESIAN_POINT('Origin',(-56.5858547179449,18.0520194698678,39.6398955069221));
#204936=CARTESIAN_POINT('Origin',(-56.7552848242269,18.1070706485047,39.3548010137695));
#204937=CARTESIAN_POINT('Ctrl Pts',(-58.1242364370955,18.5518699907155,
39.3978017080178));
#204938=CARTESIAN_POINT('Ctrl Pts',(-58.0849912788099,18.672654168285,39.3978017080178));
#204939=CARTESIAN_POINT('Ctrl Pts',(-58.0849912788099,18.672654168285,39.5248017080178));
#204940=CARTESIAN_POINT('Ctrl Pts',(-58.2097691178803,18.5799074873342,
39.3978017080178));
#204941=CARTESIAN_POINT('Ctrl Pts',(-58.1705159385189,18.7004428147377,
39.3980355775196));
#204942=CARTESIAN_POINT('Ctrl Pts',(-58.213397284395,18.7143758086142,39.5248015517192));
#204943=CARTESIAN_POINT('Ctrl Pts',(-58.2906472745457,18.6064173144569,
39.3484893995498));
#204944=CARTESIAN_POINT('Ctrl Pts',(-58.2517893143875,18.7268501353373,
39.3489438303413));
#204945=CARTESIAN_POINT('Ctrl Pts',(-58.3348142976334,18.7538265876731,
39.4508333155594));
#204946=CARTESIAN_POINT('Ctrl Pts',(-58.3332704847794,18.6203878281152,
39.2708017080178));
#204947=CARTESIAN_POINT('Ctrl Pts',(-58.2946680067386,18.7407822670307,
39.2710850691867));
#204948=CARTESIAN_POINT('Ctrl Pts',(-58.3988020033597,18.7746174535804,
39.3343017080178));
#204949=CARTESIAN_POINT('Origin',(-58.1242364370955,18.5518699907155,39.5248017080178));
#204950=CARTESIAN_POINT('Ctrl Pts',(-56.6526781108322,18.0743352474896,
39.2875012672119));
#204951=CARTESIAN_POINT('Ctrl Pts',(-56.6140134955961,18.1949031876638,
39.2878045257519));
#204952=CARTESIAN_POINT('Ctrl Pts',(-56.716192681671,18.2279043949852,39.3549015218347));
#204953=CARTESIAN_POINT('Ctrl Pts',(-56.7620702268159,18.1097491035606,
39.1034938540228));
#204954=CARTESIAN_POINT('Ctrl Pts',(-56.7232113603681,18.2303840130666,
39.1038286278784));
#204955=CARTESIAN_POINT('Ctrl Pts',(-56.8036438738767,18.2563190096466,
39.207750643403));
#204956=CARTESIAN_POINT('Ctrl Pts',(-56.958588855084,18.1733695596541,38.989));
#204957=CARTESIAN_POINT('Ctrl Pts',(-56.9195374698056,18.2941747571335,
38.9892298954636));
#204958=CARTESIAN_POINT('Ctrl Pts',(-56.9607460083086,18.3073645871837,
39.1161900347288));
#204959=CARTESIAN_POINT('Ctrl Pts',(-57.1650137687746,18.240199652705,38.989));
#204960=CARTESIAN_POINT('Ctrl Pts',(-57.125709824009,18.3611647564559,38.989));
#204961=CARTESIAN_POINT('Ctrl Pts',(-57.125768654452,18.3609836949699,39.1161900945645));
#204962=CARTESIAN_POINT('Origin',(-57.1650137687745,18.240199652705,39.116));
#204963=CARTESIAN_POINT('Origin',(54.8193466381475,-18.1457247135494,39.5248017080178));
#204964=CARTESIAN_POINT('Origin',(-57.9804289733662,18.5051441132846,39.5248017080178));
#204965=CARTESIAN_POINT('Origin',(54.6058629360811,-18.0763596539233,39.116));
#204966=CARTESIAN_POINT('Origin',(-57.5467470426658,18.3641788932756,39.116040271385));
#204967=CARTESIAN_POINT('Ctrl Pts',(-57.7713971777985,18.4366189870677,
39.2708017080178));
#204968=CARTESIAN_POINT('Ctrl Pts',(-57.7324510618069,18.5581069080665,
39.27051194648));
#204969=CARTESIAN_POINT('Ctrl Pts',(-57.6273730232604,18.5239649837012,
39.3343017080178));
#204970=CARTESIAN_POINT('Ctrl Pts',(-57.8141635875298,18.450639415372,39.3487519301186));
#204971=CARTESIAN_POINT('Ctrl Pts',(-57.7750271733919,18.5719407253113,
39.3482879463966));
#204972=CARTESIAN_POINT('Ctrl Pts',(-57.6915769758397,18.5448261124702,
39.4512271261621));
#204973=CARTESIAN_POINT('Ctrl Pts',(-57.8951845615401,18.477200500639,39.3978017080178));
#204974=CARTESIAN_POINT('Ctrl Pts',(-57.8557848432464,18.5981804828681,
39.397567382742));
#204975=CARTESIAN_POINT('Ctrl Pts',(-57.8132103173504,18.5843471808457,
39.5248015355199));
#204976=CARTESIAN_POINT('Ctrl Pts',(-57.9804289733662,18.5051441132846,
39.3978017080178));
#204977=CARTESIAN_POINT('Ctrl Pts',(-57.9411838150806,18.6259282908541,
39.3978017080178));
#204978=CARTESIAN_POINT('Ctrl Pts',(-57.9411838150806,18.6259282908541,
39.5248017080178));
#204979=CARTESIAN_POINT('Origin',(-57.666618181546,18.4031808061317,39.3343017080178));
#204980=CARTESIAN_POINT('Origin',(-57.5892494801772,18.3780421908681,39.1934008533546));
#204981=CARTESIAN_POINT('Origin',(-55.9845461696107,25.273472906794,39.1925554495072));
#204982=CARTESIAN_POINT('Origin',(-56.0249274780501,25.2915084057467,39.1160373285231));
#204983=CARTESIAN_POINT('Origin',(-55.9097831300745,25.2401862573146,39.3343017080178));
#204984=CARTESIAN_POINT('Ctrl Pts',(-55.8095395120005,25.1949317875305,
39.2708017080178));
#204985=CARTESIAN_POINT('Ctrl Pts',(-55.8614118841076,25.0796311836958,
39.2710850691866));
#204986=CARTESIAN_POINT('Ctrl Pts',(-55.9614386837451,25.124165984194,39.3343017080178));
#204987=CARTESIAN_POINT('Ctrl Pts',(-55.7683775656457,25.1767321129114,
39.3487519293518));
#204988=CARTESIAN_POINT('Ctrl Pts',(-55.8200852551826,25.0612313830313,
39.3492068662946));
#204989=CARTESIAN_POINT('Ctrl Pts',(-55.8997670518381,25.0967080045992,
39.4512271248741));
#204990=CARTESIAN_POINT('Ctrl Pts',(-55.6903961807893,25.1422534028253,
39.3978017080178));
#204991=CARTESIAN_POINT('Ctrl Pts',(-55.7418796630199,25.0264120100489,
39.3980347781155));
#204992=CARTESIAN_POINT('Ctrl Pts',(-55.7829311357716,25.0446893032921,
39.524801535519));
#204993=CARTESIAN_POINT('Ctrl Pts',(-55.6083495590299,25.1059793847706,
39.3978017080178));
#204994=CARTESIAN_POINT('Ctrl Pts',(-55.6600051127006,24.98995911165,39.3978017080178));
#204995=CARTESIAN_POINT('Ctrl Pts',(-55.6600051127006,24.98995911165,39.5248017080178));
#204996=CARTESIAN_POINT('Origin',(-55.6083495590299,25.1059793847706,39.5248017080178));
#204997=CARTESIAN_POINT('Origin',(0.129138884176574,0.290050682801525,39.116));
#204998=CARTESIAN_POINT('Origin',(-56.3916032444848,25.4547063934087,39.116));
#204999=CARTESIAN_POINT('Origin',(0.129138884176574,0.290050682801525,39.5248017080178));
#205000=CARTESIAN_POINT('Origin',(-55.4702140717965,25.0444775033952,39.5248017080178));
#205001=CARTESIAN_POINT('Ctrl Pts',(-56.8833377255392,25.6742415049984,
39.2875012672119));
#205002=CARTESIAN_POINT('Ctrl Pts',(-56.9357219056856,25.5577357840976,
39.287208709576));
#205003=CARTESIAN_POINT('Ctrl Pts',(-56.8366797759153,25.5138485805642,
39.3549016990122));
#205004=CARTESIAN_POINT('Ctrl Pts',(-56.7783442778555,25.6273680143737,
39.1034939173931));
#205005=CARTESIAN_POINT('Ctrl Pts',(-56.8305359187831,25.5109042502482,
39.1031692336329));
#205006=CARTESIAN_POINT('Ctrl Pts',(-56.7526780286664,25.4764485929311,
39.2077507202299));
#205007=CARTESIAN_POINT('Ctrl Pts',(-56.5897276738849,25.5431608329955,
38.989));
#205008=CARTESIAN_POINT('Ctrl Pts',(-56.6417212312953,25.4268390553483,
38.9887769311182));
#205009=CARTESIAN_POINT('Ctrl Pts',(-56.6017723050738,25.4092610357547,
39.1161898712914));
#205010=CARTESIAN_POINT('Ctrl Pts',(-56.3916032444848,25.4547063934087,
38.989));
#205011=CARTESIAN_POINT('Ctrl Pts',(-56.4433359691572,25.3385127913803,
38.989));
#205012=CARTESIAN_POINT('Ctrl Pts',(-56.4432587405966,25.3386862495675,
39.1161895903853));
#205013=CARTESIAN_POINT('Origin',(-56.7851714777845,25.6299342605,39.3548010137695));
#205014=CARTESIAN_POINT('Ctrl Pts',(-55.4702140717965,25.0444775033952,
39.3978017080178));
#205015=CARTESIAN_POINT('Ctrl Pts',(-55.5218696254671,24.9284572302746,
39.3978017080178));
#205016=CARTESIAN_POINT('Ctrl Pts',(-55.5218696254671,24.9284572302746,
39.5248017080178));
#205017=CARTESIAN_POINT('Ctrl Pts',(-55.3878899076691,25.0080814159073,
39.3978017080178));
#205018=CARTESIAN_POINT('Ctrl Pts',(-55.4395618538405,24.8918114493237,
39.3975666025045));
#205019=CARTESIAN_POINT('Ctrl Pts',(-55.3985281293149,24.8735420580987,
39.5248015517196));
#205020=CARTESIAN_POINT('Ctrl Pts',(-55.3100454158619,24.9736678430968,
39.3484894016716));
#205021=CARTESIAN_POINT('Ctrl Pts',(-55.3621286647,24.8573359723215,39.3480259000037));
#205022=CARTESIAN_POINT('Ctrl Pts',(-55.2818999508914,24.8216158475493,
39.4508333188938));
#205023=CARTESIAN_POINT('Ctrl Pts',(-55.2690209153038,24.9555320242419,
39.2708017080178));
#205024=CARTESIAN_POINT('Ctrl Pts',(-55.3213695969754,24.8391888661849,
39.27051194648));
#205025=CARTESIAN_POINT('Ctrl Pts',(-55.2204359898054,24.7942503289611,
39.3343017080178));
#205026=CARTESIAN_POINT('Origin',(-55.1687804361348,24.9102706020818,39.3343017080178));
#205027=CARTESIAN_POINT('Origin',(-56.9479187893799,25.7023940320541,39.6398955068197));
#205028=CARTESIAN_POINT('Origin',(-57.1106661007663,25.7748538035651,39.92499));
#205029=CARTESIAN_POINT('Origin',(-55.0944632682976,24.8771824671432,39.1934008539939));
#205030=CARTESIAN_POINT('Origin',(-55.0536014459533,24.8590452239608,39.1160402713851));
#205031=CARTESIAN_POINT('Ctrl Pts',(-57.505263737773,25.6197038181302,40.1599502534424));
#205032=CARTESIAN_POINT('Ctrl Pts',(-57.4711877340327,25.6045223014066,
40.10025));
#205033=CARTESIAN_POINT('Ctrl Pts',(-57.4068835917977,25.5758735661212,
40.10025));
#205034=CARTESIAN_POINT('Ctrl Pts',(-57.4694043465862,25.7001924885134,
40.1599500538462));
#205035=CARTESIAN_POINT('Ctrl Pts',(-57.4450643815399,25.6631501095118,
40.1002448353478));
#205036=CARTESIAN_POINT('Ctrl Pts',(-57.3861185493425,25.6224598624443,
40.10025));
#205037=CARTESIAN_POINT('Ctrl Pts',(-57.413464248775,25.7642825572405,40.1202442001038));
#205038=CARTESIAN_POINT('Ctrl Pts',(-57.3998804953985,25.7077329912391,
40.0633873868015));
#205039=CARTESIAN_POINT('Ctrl Pts',(-57.3441059191826,25.6552692732808,
40.0772271723537));
#205040=CARTESIAN_POINT('Ctrl Pts',(-57.3036982377901,25.8321626496794,
40.0045995998164));
#205041=CARTESIAN_POINT('Ctrl Pts',(-57.3186021074453,25.7409042554413,
39.9663485808318));
#205042=CARTESIAN_POINT('Ctrl Pts',(-57.2526112478171,25.6821129719831,
40.0101727202466));
#205043=CARTESIAN_POINT('Ctrl Pts',(-57.2503778226939,25.8376543496548,
39.9304654349858));
#205044=CARTESIAN_POINT('Ctrl Pts',(-57.2821097063785,25.728949171911,39.9051900162956));
#205045=CARTESIAN_POINT('Ctrl Pts',(-57.2038640469252,25.6773293952367,
39.9671857458187));
#205046=CARTESIAN_POINT('Ctrl Pts',(-57.2088336324697,25.8191582032625,
39.8576902534424));
#205047=CARTESIAN_POINT('Ctrl Pts',(-57.2611357920723,25.7028284190338,
39.8573998014387));
#205048=CARTESIAN_POINT('Ctrl Pts',(-57.1623216544369,25.6588335304445,
39.92499));
#205049=CARTESIAN_POINT('Origin',(-57.4068835917977,25.5758735661212,40.22725));
#205050=CARTESIAN_POINT('Origin',(0.129138884176574,0.290050682801525,39.116));
#205051=CARTESIAN_POINT('Origin',(-54.6869600343295,24.6957503380312,39.116));
#205052=CARTESIAN_POINT('Origin',(1.20426471881346E-16,-6.70666394583731E-17,
40.22725));
#205053=CARTESIAN_POINT('Origin',(-57.4192809246787,25.5480287005723,40.22725));
#205054=CARTESIAN_POINT('Ctrl Pts',(-54.6869600343295,24.6957503380312,
38.989));
#205055=CARTESIAN_POINT('Ctrl Pts',(-54.7386929703522,24.5795562613022,
38.989));
#205056=CARTESIAN_POINT('Ctrl Pts',(-54.7386155301258,24.5797301948985,
39.1161901092324));
#205057=CARTESIAN_POINT('Ctrl Pts',(-54.4888352915933,24.6072881749587,
38.989));
#205058=CARTESIAN_POINT('Ctrl Pts',(-54.5406489234191,24.4913819335262,
38.989229898976));
#205059=CARTESIAN_POINT('Ctrl Pts',(-54.5800991622559,24.5091541605505,
39.1161900493204));
#205060=CARTESIAN_POINT('Ctrl Pts',(-54.3002245846697,24.5230714236777,
39.1034966344368));
#205061=CARTESIAN_POINT('Ctrl Pts',(-54.3520673354865,24.4074205468518,
39.103831410256));
#205062=CARTESIAN_POINT('Ctrl Pts',(-54.4291945615849,24.441967103316,39.2077528789598));
#205063=CARTESIAN_POINT('Ctrl Pts',(-54.195235491187,24.4761921430396,39.2875012672119));
#205064=CARTESIAN_POINT('Ctrl Pts',(-54.247177787347,24.3607210114368,39.2878045257868));
#205065=CARTESIAN_POINT('Ctrl Pts',(-54.3451938439591,24.4045675740912,
39.35490152959));
#205066=CARTESIAN_POINT('Origin',(-54.2933913980362,24.5205222915156,39.3548010137695));
#205067=CARTESIAN_POINT('Ctrl Pts',(-57.4675553545138,25.2380597013435,
39.8576902534424));
#205068=CARTESIAN_POINT('Ctrl Pts',(-57.4161024530841,25.354767599672,39.8573998014387));
#205069=CARTESIAN_POINT('Ctrl Pts',(-57.3172883154488,25.3107727110827,
39.92499));
#205070=CARTESIAN_POINT('Ctrl Pts',(-57.5091180232691,25.2565651278913,
39.9304984902492));
#205071=CARTESIAN_POINT('Ctrl Pts',(-57.4495672328895,25.3528749970536,
39.9052171569797));
#205072=CARTESIAN_POINT('Ctrl Pts',(-57.358849637138,25.3292770036981,39.9672049726607));
#205073=CARTESIAN_POINT('Ctrl Pts',(-57.5405471770606,25.2997972770063,
40.004343767866));
#205074=CARTESIAN_POINT('Ctrl Pts',(-57.482714899638,25.3720159720864,39.9661628577643));
#205075=CARTESIAN_POINT('Ctrl Pts',(-57.3948558336728,25.3622324578625,
40.0100243556236));
#205076=CARTESIAN_POINT('Ctrl Pts',(-57.5636463159494,25.4257977880274,
40.1194874821989));
#205077=CARTESIAN_POINT('Ctrl Pts',(-57.5124644612013,25.4538910783601,
40.062755148314));
#205078=CARTESIAN_POINT('Ctrl Pts',(-57.4360631077225,25.4475597357241,
40.0767884282376));
#205079=CARTESIAN_POINT('Ctrl Pts',(-57.5536211289088,25.511038551389,40.1599502015387));
#205080=CARTESIAN_POINT('Ctrl Pts',(-57.509788306592,25.517777816471,40.1002449453875));
#205081=CARTESIAN_POINT('Ctrl Pts',(-57.4400754463037,25.5012707422381,
40.10025));
#205082=CARTESIAN_POINT('Ctrl Pts',(-57.5176823163886,25.5918112338799,
40.1599502534424));
#205083=CARTESIAN_POINT('Ctrl Pts',(-57.4835989537475,25.5766462455181,
40.10025));
#205084=CARTESIAN_POINT('Ctrl Pts',(-57.4192809246787,25.5480287005723,
40.10025));
#205085=CARTESIAN_POINT('Origin',(-57.3689438691194,25.1947524379621,39.92499));
#205086=CARTESIAN_POINT('Origin',(-54.1306438627472,24.4480624203115,39.6398955069335));
#205087=CARTESIAN_POINT('Origin',(-53.9678963272933,24.3756025490943,39.92499));
#205088=CARTESIAN_POINT('Origin',(-57.2061965577014,25.1222926664875,39.6398955068285));
#205089=CARTESIAN_POINT('Origin',(-57.0434492461377,25.0498328948969,39.3548010137695));
#205090=CARTESIAN_POINT('Ctrl Pts',(-53.8697418420143,24.3312692531092,
39.8576902534424));
#205091=CARTESIAN_POINT('Ctrl Pts',(-53.9216078643415,24.2159747902191,
39.8579948730703));
#205092=CARTESIAN_POINT('Ctrl Pts',(-54.0195518809639,24.2595822759737,
39.92499));
#205093=CARTESIAN_POINT('Ctrl Pts',(-53.8282341734838,24.3127882662188,
39.9304020711231));
#205094=CARTESIAN_POINT('Ctrl Pts',(-53.8880114973681,24.2176496934286,
39.9058915297379));
#205095=CARTESIAN_POINT('Ctrl Pts',(-53.9780422761229,24.2411010091827,
39.9671523786028));
#205096=CARTESIAN_POINT('Ctrl Pts',(-53.7969955864425,24.2697746459846,
40.0043257306693));
#205097=CARTESIAN_POINT('Ctrl Pts',(-53.8549480733036,24.1983152114492,
39.9667894847835));
#205098=CARTESIAN_POINT('Ctrl Pts',(-53.9422730280817,24.2082687574727,
40.0100138975199));
#205099=CARTESIAN_POINT('Ctrl Pts',(-53.7744913425364,24.1443388226041,
40.1195533054857));
#205100=CARTESIAN_POINT('Ctrl Pts',(-53.8256450222191,24.1165167429228,
40.0630813209236));
#205101=CARTESIAN_POINT('Ctrl Pts',(-53.9017956184507,24.1232032230478,
40.0768265942421));
#205102=CARTESIAN_POINT('Ctrl Pts',(-53.7848917482045,24.0595120258538,
40.1599502027521));
#205103=CARTESIAN_POINT('Ctrl Pts',(-53.8286685158632,24.0529122166846,
40.1002552791554));
#205104=CARTESIAN_POINT('Ctrl Pts',(-53.8982652496121,24.0696665464387,
40.10025));
#205105=CARTESIAN_POINT('Ctrl Pts',(-53.8206887816834,23.9791663275018,
40.1599502534424));
#205106=CARTESIAN_POINT('Ctrl Pts',(-53.8547645473079,23.9943483786821,
40.10025));
#205107=CARTESIAN_POINT('Ctrl Pts',(-53.9190682401993,24.0229981225301,
40.10025));
#205108=CARTESIAN_POINT('Origin',(-53.9190682401993,24.0229981225301,40.22725));
#205109=CARTESIAN_POINT('Ctrl Pts',(-56.649881012838,24.8746050278057,38.989));
#205110=CARTESIAN_POINT('Ctrl Pts',(-56.5981482837086,24.9907986398447,
38.989));
#205111=CARTESIAN_POINT('Ctrl Pts',(-56.5982255167329,24.990625171632,39.1161896013268));
#205112=CARTESIAN_POINT('Ctrl Pts',(-56.8481896769747,24.9626539694743,
38.989));
#205113=CARTESIAN_POINT('Ctrl Pts',(-56.7965362315768,25.0791271905752,
38.9887769275485));
#205114=CARTESIAN_POINT('Ctrl Pts',(-56.7567415443537,25.0612010539385,
39.116189882185));
#205115=CARTESIAN_POINT('Ctrl Pts',(-57.036975459333,25.0464771582517,39.1034967087243));
#205116=CARTESIAN_POINT('Ctrl Pts',(-56.9853490357206,25.1631925873301,
39.10317202327));
#205117=CARTESIAN_POINT('Ctrl Pts',(-56.9076460727643,25.1283880784741,
39.2077529614999));
#205118=CARTESIAN_POINT('Ctrl Pts',(-57.1420619865019,25.093137300575,39.2875012672119));
#205119=CARTESIAN_POINT('Ctrl Pts',(-57.0905332166518,25.2100238867504,
39.2872087095507));
#205120=CARTESIAN_POINT('Ctrl Pts',(-56.9916465440539,25.1657874977298,
39.3549017048228));
#205121=CARTESIAN_POINT('Origin',(-56.649881012838,24.8746050278057,39.116));
#205122=CARTESIAN_POINT('Origin',(3.58382961824623E-16,2.38580516864212E-17,
40.22725));
#205123=CARTESIAN_POINT('Origin',(-53.9314655730802,23.9951532569811,40.22725));
#205124=CARTESIAN_POINT('Origin',(51.799563747336,-23.4101986852082,39.116));
#205125=CARTESIAN_POINT('Origin',(-56.2832472948488,24.7113125977917,39.1160373285251));
#205126=CARTESIAN_POINT('Ctrl Pts',(-53.8330634946836,23.9513722670369,
40.1599502534424));
#205127=CARTESIAN_POINT('Ctrl Pts',(-53.8671470951728,23.9665367208228,
40.10025));
#205128=CARTESIAN_POINT('Ctrl Pts',(-53.9314655730802,23.9951532569811,
40.10025));
#205129=CARTESIAN_POINT('Ctrl Pts',(-53.8686972660497,23.871282165812,40.159950056604));
#205130=CARTESIAN_POINT('Ctrl Pts',(-53.8931046959165,23.9081865738544,
40.1002551305369));
#205131=CARTESIAN_POINT('Ctrl Pts',(-53.9521563342718,23.9486256024597,
40.10025));
#205132=CARTESIAN_POINT('Ctrl Pts',(-53.9240892607408,23.807186639316,40.1203070619047));
#205133=CARTESIAN_POINT('Ctrl Pts',(-53.9378509529599,23.863535538615,40.0637098684499));
#205134=CARTESIAN_POINT('Ctrl Pts',(-53.9937257232526,23.9155750846183,
40.0772636213364));
#205135=CARTESIAN_POINT('Ctrl Pts',(-54.0330064121714,23.7392497560572,
40.0046102245801));
#205136=CARTESIAN_POINT('Ctrl Pts',(-54.0187512923758,23.8300830854577,
39.9670001894012));
#205137=CARTESIAN_POINT('Ctrl Pts',(-54.0845104630311,23.8883623535219,
40.0101788811208));
#205138=CARTESIAN_POINT('Ctrl Pts',(-54.0860594545419,23.7337507958625,
39.9303710930187));
#205139=CARTESIAN_POINT('Ctrl Pts',(-54.0553500291278,23.8418399747429,
39.9058663574104));
#205140=CARTESIAN_POINT('Ctrl Pts',(-54.1330265677735,23.8930480394869,
39.9671344706359));
#205141=CARTESIAN_POINT('Ctrl Pts',(-54.1275498658872,23.7522229508832,
39.8576902534424));
#205142=CARTESIAN_POINT('Ctrl Pts',(-54.0765745253534,23.8679139708573,
39.8579948730703));
#205143=CARTESIAN_POINT('Ctrl Pts',(-54.1745185419758,23.9115214566119,
39.92499));
#205144=CARTESIAN_POINT('Origin',(-54.2261740956464,23.7955011834913,39.92499));
#205145=CARTESIAN_POINT('Origin',(-56.2428239368561,24.6933715410274,39.1925554488845));
#205146=CARTESIAN_POINT('Origin',(-56.1680608984276,24.6600848917116,39.3343017080178));
#205147=CARTESIAN_POINT('Origin',(-54.3889216310588,23.8679610547526,39.639895506921));
#205148=CARTESIAN_POINT('Origin',(-54.5516691663893,23.9404209259125,39.3548010137695));
#205149=CARTESIAN_POINT('Ctrl Pts',(-55.8666273273831,24.5258780191675,
39.3978017080178));
#205150=CARTESIAN_POINT('Ctrl Pts',(-55.8149717737125,24.6418982922882,
39.3978017080178));
#205151=CARTESIAN_POINT('Ctrl Pts',(-55.8149717737125,24.6418982922882,
39.5248017080178));
#205152=CARTESIAN_POINT('Ctrl Pts',(-55.9487607347574,24.5627025231283,
39.3978017080178));
#205153=CARTESIAN_POINT('Ctrl Pts',(-55.8971232158786,24.6784744708797,
39.3980355775182));
#205154=CARTESIAN_POINT('Ctrl Pts',(-55.9383132588147,24.6968134595443,
39.5248015517192));
#205155=CARTESIAN_POINT('Ctrl Pts',(-56.0264248009273,24.597521196073,39.3484893995498));
#205156=CARTESIAN_POINT('Ctrl Pts',(-55.9751910510454,24.7132325104962,
39.3489438303417));
#205157=CARTESIAN_POINT('Ctrl Pts',(-56.0549414076415,24.7487396569164,
39.4508333155595));
#205158=CARTESIAN_POINT('Ctrl Pts',(-56.0673542004324,24.6158705164598,
39.2708017080178));
#205159=CARTESIAN_POINT('Ctrl Pts',(-56.0163785451196,24.731570364334,39.2710850691866));
#205160=CARTESIAN_POINT('Ctrl Pts',(-56.116405344757,24.7761051648322,39.3343017080178));
#205161=CARTESIAN_POINT('Origin',(-55.8666273273831,24.5258780191675,39.5248017080178));
#205162=CARTESIAN_POINT('Ctrl Pts',(-54.4530463244691,23.8971395307773,
39.2875012672119));
#205163=CARTESIAN_POINT('Ctrl Pts',(-54.401990736535,24.0130054343465,39.2878045257519));
#205164=CARTESIAN_POINT('Ctrl Pts',(-54.5001606088501,24.0565064908996,
39.3549015218347));
#205165=CARTESIAN_POINT('Ctrl Pts',(-54.5581374230423,23.9437939758161,
39.1034938540228));
#205166=CARTESIAN_POINT('Ctrl Pts',(-54.506881647828,24.0597061770709,39.1038286278813));
#205167=CARTESIAN_POINT('Ctrl Pts',(-54.5841625982711,24.0939065860615,
39.2077506434033));
#205168=CARTESIAN_POINT('Ctrl Pts',(-54.7469293531953,24.0276077026093,
38.989));
#205169=CARTESIAN_POINT('Ctrl Pts',(-54.6954643138415,24.1436691352846,
38.9892298954611));
#205170=CARTESIAN_POINT('Ctrl Pts',(-54.735068394994,24.1610941752712,39.1161900347288));
#205171=CARTESIAN_POINT('Ctrl Pts',(-54.9452378026827,24.1156489724281,
38.989));
#205172=CARTESIAN_POINT('Ctrl Pts',(-54.8935048726349,24.2318430357372,
38.989));
#205173=CARTESIAN_POINT('Ctrl Pts',(-54.8935823068775,24.2316691155808,
39.1161900945645));
#205174=CARTESIAN_POINT('Origin',(-54.9452378026827,24.1156489724281,39.116));
#205175=CARTESIAN_POINT('Origin',(50.541702139688,-22.850162615335,39.5248017080178));
#205176=CARTESIAN_POINT('Origin',(-55.7284918401496,24.4643761377921,39.5248017080178));
#205177=CARTESIAN_POINT('Origin',(50.3447265545023,-22.7624634345049,39.116));
#205178=CARTESIAN_POINT('Origin',(-55.3119205422643,24.2788510342452,39.1160402713846));
#205179=CARTESIAN_POINT('Ctrl Pts',(-55.5277679687681,24.3743766270218,
39.2708017080178));
#205180=CARTESIAN_POINT('Ctrl Pts',(-55.4763362579872,24.491128046823,39.2705119464801));
#205181=CARTESIAN_POINT('Ctrl Pts',(-55.3754026508173,24.4461895095993,
39.3343017080178));
#205182=CARTESIAN_POINT('Ctrl Pts',(-55.5688345658067,24.3927905570423,
39.3487519301186));
#205183=CARTESIAN_POINT('Ctrl Pts',(-55.5172331055191,24.5093364964835,
39.3482879463986));
#205184=CARTESIAN_POINT('Ctrl Pts',(-55.4370743056935,24.4736474994206,
39.4512271261638));
#205185=CARTESIAN_POINT('Ctrl Pts',(-55.6466353090197,24.4276751358079,
39.3978017080178));
#205186=CARTESIAN_POINT('Ctrl Pts',(-55.5948055748778,24.543873985031,39.3975673827401));
#205187=CARTESIAN_POINT('Ctrl Pts',(-55.5539102504902,24.5256662135193,
39.5248015355181));
#205188=CARTESIAN_POINT('Ctrl Pts',(-55.7284918401496,24.4643761377921,
39.3978017080178));
#205189=CARTESIAN_POINT('Ctrl Pts',(-55.676836286479,24.5803964109127,39.3978017080178));
#205190=CARTESIAN_POINT('Ctrl Pts',(-55.676836286479,24.5803964109127,39.5248017080178));
#205191=CARTESIAN_POINT('Origin',(-55.4270582044879,24.3301692364787,39.3343017080178));
#205192=CARTESIAN_POINT('Origin',(-55.3527410377818,24.2970811017172,39.1934008533559));
#205193=CARTESIAN_POINT('Origin',(-53.0360596835504,30.9870007556532,39.1925554495084));
#205194=CARTESIAN_POINT('Origin',(-53.0743345559671,31.0091584503694,39.1160373285251));
#205195=CARTESIAN_POINT('Origin',(-52.9651856060843,30.9460815882873,39.3343017080178));
#205196=CARTESIAN_POINT('Ctrl Pts',(-52.8702215132213,30.8905967158741,
39.2708017080178));
#205197=CARTESIAN_POINT('Ctrl Pts',(-52.9338619179793,30.7813498801536,
39.2710850691866));
#205198=CARTESIAN_POINT('Ctrl Pts',(-53.0286856060843,30.8360963620066,
39.3343017080178));
#205199=CARTESIAN_POINT('Ctrl Pts',(-52.8311874403355,30.868194145979,39.3487519293518));
#205200=CARTESIAN_POINT('Ctrl Pts',(-52.8946849835385,30.7587310665085,
39.3492068662926));
#205201=CARTESIAN_POINT('Ctrl Pts',(-52.9702219582401,30.802342359186,39.4512271248735));
#205202=CARTESIAN_POINT('Ctrl Pts',(-52.7572372522463,30.8257530395504,
39.3978017080178));
#205203=CARTESIAN_POINT('Ctrl Pts',(-52.8205474253443,30.7159277273269,
39.3980347781178));
#205204=CARTESIAN_POINT('Ctrl Pts',(-52.8594635164572,30.7383959430076,
39.5248015355195));
#205205=CARTESIAN_POINT('Ctrl Pts',(-52.6794317578285,30.7811015270748,
39.3978017080178));
#205206=CARTESIAN_POINT('Ctrl Pts',(-52.7429317578285,30.6711163007942,
39.3978017080178));
#205207=CARTESIAN_POINT('Ctrl Pts',(-52.7429317578285,30.6711163007942,
39.5248017080178));
#205208=CARTESIAN_POINT('Origin',(-52.6794317578285,30.7811015270748,39.5248017080178));
#205209=CARTESIAN_POINT('Origin',(0.158750000000008,0.274963065701558,39.116));
#205210=CARTESIAN_POINT('Origin',(-53.4219427993284,31.209790476761,39.116));
#205211=CARTESIAN_POINT('Origin',(0.158750000000008,0.274963065701558,39.5248017080178));
#205212=CARTESIAN_POINT('Origin',(-52.5484816883957,30.7054974692373,39.5248017080178));
#205213=CARTESIAN_POINT('Ctrl Pts',(-53.8880358395968,31.4795232016794,
39.2875012672119));
#205214=CARTESIAN_POINT('Ctrl Pts',(-53.9523112176908,31.3691313491582,
39.287208709576));
#205215=CARTESIAN_POINT('Ctrl Pts',(-53.8583991130131,31.3151318426941,
39.3549016990121));
#205216=CARTESIAN_POINT('Ctrl Pts',(-53.7885171709481,31.4219316852012,
39.1034939173931));
#205217=CARTESIAN_POINT('Ctrl Pts',(-53.8525966788897,31.3115614337837,
39.1031692336348));
#205218=CARTESIAN_POINT('Ctrl Pts',(-53.7787668993583,31.2691561625547,
39.2077507202298));
#205219=CARTESIAN_POINT('Ctrl Pts',(-53.6097358757354,31.3184699958127,
38.989));
#205220=CARTESIAN_POINT('Ctrl Pts',(-53.6736035436633,31.2082202476928,
38.9887769311176));
#205221=CARTESIAN_POINT('Ctrl Pts',(-53.6357108652113,31.186562722461,39.1161898712912));
#205222=CARTESIAN_POINT('Ctrl Pts',(-53.4219427993284,31.209790476761,38.989));
#205223=CARTESIAN_POINT('Ctrl Pts',(-53.4855376653836,31.0996409376529,
38.989));
#205224=CARTESIAN_POINT('Ctrl Pts',(-53.4854427285714,31.0998053730351,
39.1161895903851));
#205225=CARTESIAN_POINT('Origin',(-53.7950387249976,31.4251975098797,39.3548010137695));
#205226=CARTESIAN_POINT('Ctrl Pts',(-52.5484816883957,30.7054974692373,
39.3978017080178));
#205227=CARTESIAN_POINT('Ctrl Pts',(-52.6119816883957,30.5955122429567,
39.3978017080178));
#205228=CARTESIAN_POINT('Ctrl Pts',(-52.6119816883957,30.5955122429567,
39.5248017080178));
#205229=CARTESIAN_POINT('Ctrl Pts',(-52.4704129317472,30.6606955449589,
39.3978017080178));
#205230=CARTESIAN_POINT('Ctrl Pts',(-52.5339553345217,30.5504637065431,
39.3975666025022));
#205231=CARTESIAN_POINT('Ctrl Pts',(-52.4950560684217,30.5280052047896,
39.5248015517178));
#205232=CARTESIAN_POINT('Ctrl Pts',(-52.3965920780924,30.6183335281986,
39.3484894016716));
#205233=CARTESIAN_POINT('Ctrl Pts',(-52.4605500011258,30.5080831175487,
39.348025900005));
#205234=CARTESIAN_POINT('Ctrl Pts',(-52.3844945583563,30.4641724871913,
39.450833318895));
#205235=CARTESIAN_POINT('Ctrl Pts',(-52.357688023316,30.5960088312573,39.2708017080178));
#205236=CARTESIAN_POINT('Ctrl Pts',(-52.4219111049554,30.4857749404424,
39.2705119464801));
#205237=CARTESIAN_POINT('Ctrl Pts',(-52.3262277788839,30.4305321463781,
39.3343017080178));
#205238=CARTESIAN_POINT('Origin',(-52.2627277788839,30.5405173726587,39.3343017080178));
#205239=CARTESIAN_POINT('Origin',(-53.9493203812208,31.5142720656068,39.6398955068201));
#205240=CARTESIAN_POINT('Origin',(-54.1036020372436,31.603346621267,39.92499));
#205241=CARTESIAN_POINT('Origin',(-52.1922763801643,30.4998422386362,39.1934008539949));
#205242=CARTESIAN_POINT('Origin',(-52.1535342613176,30.4775331296743,39.1160402713847));
#205243=CARTESIAN_POINT('Ctrl Pts',(-54.5122556166608,31.4902932482912,
40.1599502534424));
#205244=CARTESIAN_POINT('Ctrl Pts',(-54.4799531854476,31.4716329851994,
40.10025));
#205245=CARTESIAN_POINT('Ctrl Pts',(-54.4189959163061,31.4364195775139,
40.10025));
#205246=CARTESIAN_POINT('Ctrl Pts',(-54.4681793099456,31.5665926662618,
40.1599500538464));
#205247=CARTESIAN_POINT('Ctrl Pts',(-54.4478446647269,31.5272089901459,
40.100244835349));
#205248=CARTESIAN_POINT('Ctrl Pts',(-54.3934750329619,31.4805801312537,
40.10025));
#205249=CARTESIAN_POINT('Ctrl Pts',(-54.4058464214484,31.6244843104277,
40.120244200104));
#205250=CARTESIAN_POINT('Ctrl Pts',(-54.398248120527,31.5668246399998,40.0633873868015));
#205251=CARTESIAN_POINT('Ctrl Pts',(-54.3482630350909,31.5088182930366,
40.0772271723538));
#205252=CARTESIAN_POINT('Ctrl Pts',(-54.2895863184075,31.68051887617,40.0045995998161));
#205253=CARTESIAN_POINT('Ctrl Pts',(-54.313947642815,31.5913182835559,39.9663485808318));
#205254=CARTESIAN_POINT('Ctrl Pts',(-54.254463650534,31.5259511417533,40.0101727202466));
#205255=CARTESIAN_POINT('Ctrl Pts',(-54.2359839591645,31.680406990989,39.930465434986));
#205256=CARTESIAN_POINT('Ctrl Pts',(-54.278904797451,31.5756141966208,39.9051900162946));
#205257=CARTESIAN_POINT('Ctrl Pts',(-54.2064835118365,31.5160982999436,
39.9671857458179));
#205258=CARTESIAN_POINT('Ctrl Pts',(-54.1966007261205,31.6576696180589,
39.8576902534424));
#205259=CARTESIAN_POINT('Ctrl Pts',(-54.260776142598,31.5474441649288,39.8573998014387));
#205260=CARTESIAN_POINT('Ctrl Pts',(-54.1671020372436,31.4933613949863,
39.92499));
#205261=CARTESIAN_POINT('Origin',(-54.4189959163061,31.4364195775139,40.22725));
#205262=CARTESIAN_POINT('Origin',(0.158750000000008,0.274963065701558,39.116));
#205263=CARTESIAN_POINT('Origin',(-51.8059703131944,30.2768083268885,39.116));
#205264=CARTESIAN_POINT('Origin',(1.12590909550281E-16,-8.24447964058581E-17,
40.22725));
#205265=CARTESIAN_POINT('Origin',(-54.4342359163061,31.4100231232066,40.22725));
#205266=CARTESIAN_POINT('Ctrl Pts',(-51.8059703131944,30.2768083268885,
38.989));
#205267=CARTESIAN_POINT('Ctrl Pts',(-51.8695654390618,30.1666583377723,
38.989));
#205268=CARTESIAN_POINT('Ctrl Pts',(-51.8694702420496,30.1668232238342,
39.1161901092323));
#205269=CARTESIAN_POINT('Ctrl Pts',(-51.6181777324919,30.1681210939084,
38.989));
#205270=CARTESIAN_POINT('Ctrl Pts',(-51.6818230251198,30.0582657983037,
38.989229898976));
#205271=CARTESIAN_POINT('Ctrl Pts',(-51.7191994478421,30.0800643400504,
39.1161900493203));
#205272=CARTESIAN_POINT('Ctrl Pts',(-51.43940330235,30.0646505034491,39.1034966344368));
#205273=CARTESIAN_POINT('Ctrl Pts',(-51.5030508615843,29.9550522173057,
39.1038314102567));
#205274=CARTESIAN_POINT('Ctrl Pts',(-51.5761444782083,29.9974715145378,
39.2077528789599));
#205275=CARTESIAN_POINT('Ctrl Pts',(-51.3398895692694,30.0070536838162,
39.2875012672119));
#205276=CARTESIAN_POINT('Ctrl Pts',(-51.4036173400344,29.8976445635505,
39.2878045257868));
#205277=CARTESIAN_POINT('Ctrl Pts',(-51.496513240619,29.9514963979201,39.35490152959));
#205278=CARTESIAN_POINT('Origin',(-51.432874005494,30.0614010732041,39.3548010137695));
#205279=CARTESIAN_POINT('Ctrl Pts',(-54.5146464769135,31.1067982185539,
39.8576902534424));
#205280=CARTESIAN_POINT('Ctrl Pts',(-54.451276142598,31.2174884860869,39.8573998014387));
#205281=CARTESIAN_POINT('Ctrl Pts',(-54.3576020372436,31.1634057161445,
39.92499));
#205282=CARTESIAN_POINT('Ctrl Pts',(-54.5540471172209,31.1295467523339,
39.9304984902491));
#205283=CARTESIAN_POINT('Ctrl Pts',(-54.4847554296815,31.2191042733502,
39.9052171569793));
#205284=CARTESIAN_POINT('Ctrl Pts',(-54.3970014563939,31.1861529813968,
39.9672049726597));
#205285=CARTESIAN_POINT('Ctrl Pts',(-54.5807851087093,31.1758273123595,
40.0043437678661));
#205286=CARTESIAN_POINT('Ctrl Pts',(-54.515720733338,31.2416052667855,39.9661628577646));
#205287=CARTESIAN_POINT('Ctrl Pts',(-54.4293656242355,31.2226915745265,
40.0100243556237));
#205288=CARTESIAN_POINT('Ctrl Pts',(-54.5905870683102,31.3035520968883,
40.1194874821988));
#205289=CARTESIAN_POINT('Ctrl Pts',(-54.5367490446508,31.3261415286131,
40.0627551483138));
#205290=CARTESIAN_POINT('Ctrl Pts',(-54.461428031297,31.311858753664,40.0767884282376));
#205291=CARTESIAN_POINT('Ctrl Pts',(-54.5717067142918,31.3872779850343,
40.1599502015394));
#205292=CARTESIAN_POINT('Ctrl Pts',(-54.5274095677426,31.3893985541613,
40.1002449453872));
#205293=CARTESIAN_POINT('Ctrl Pts',(-54.4598040608988,31.3656949292519,
40.10025));
#205294=CARTESIAN_POINT('Ctrl Pts',(-54.5275217339717,31.4638515574745,
40.1599502534424));
#205295=CARTESIAN_POINT('Ctrl Pts',(-54.4952102564863,31.4452069629858,
40.10025));
#205296=CARTESIAN_POINT('Ctrl Pts',(-54.4342359163061,31.4100231232066,
40.10025));
#205297=CARTESIAN_POINT('Origin',(-54.4211020372436,31.0534204898638,39.92499));
#205298=CARTESIAN_POINT('Origin',(-51.2785921372153,29.9723263949871,39.6398955069309));
#205299=CARTESIAN_POINT('Origin',(-51.1243102687782,29.883251716749,39.92499));
#205300=CARTESIAN_POINT('Origin',(-54.2668203811871,30.9643459342335,39.639895506829));
#205301=CARTESIAN_POINT('Origin',(-54.1125387249976,30.8752713784766,39.3548010137695));
#205302=CARTESIAN_POINT('Ctrl Pts',(-51.0313275753406,29.828901345689,39.8576902534424));
#205303=CARTESIAN_POINT('Ctrl Pts',(-51.0949610231999,29.7196599535397,
39.8579948730704));
#205304=CARTESIAN_POINT('Ctrl Pts',(-51.1878102687782,29.7732664904684,
39.92499));
#205305=CARTESIAN_POINT('Ctrl Pts',(-50.9919790793206,29.8061828667735,
39.9304020711229));
#205306=CARTESIAN_POINT('Ctrl Pts',(-51.0613736255811,29.7178139048431,
39.9058915297375));
#205307=CARTESIAN_POINT('Ctrl Pts',(-51.1484598763126,29.7505475307857,
39.9671523786024));
#205308=CARTESIAN_POINT('Ctrl Pts',(-50.9654077681504,29.7601395581529,
40.0043257306695));
#205309=CARTESIAN_POINT('Ctrl Pts',(-51.0305123301025,29.6951292702712,
39.9667894847838));
#205310=CARTESIAN_POINT('Ctrl Pts',(-51.1163184807716,29.7141562330556,
40.0100138975202));
#205311=CARTESIAN_POINT('Ctrl Pts',(-50.9561384187038,29.6330385513053,
40.1195533054855));
#205312=CARTESIAN_POINT('Ctrl Pts',(-51.0099200724111,29.6107158994149,
40.0630813209233));
#205313=CARTESIAN_POINT('Ctrl Pts',(-51.0849545802164,29.6253256551036,
40.0768265942419));
#205314=CARTESIAN_POINT('Ctrl Pts',(-50.9753486645695,29.5497635830446,
40.1599502027523));
#205315=CARTESIAN_POINT('Ctrl Pts',(-51.0195754864236,29.5477758465704,
40.100255279156));
#205316=CARTESIAN_POINT('Ctrl Pts',(-51.087039657642,29.5717132339807,40.10025));
#205317=CARTESIAN_POINT('Ctrl Pts',(-51.0193480105325,29.4735998357342,
40.1599502534424));
#205318=CARTESIAN_POINT('Ctrl Pts',(-51.0516501490684,29.492260605465,40.10025));
#205319=CARTESIAN_POINT('Ctrl Pts',(-51.1126068659044,29.5274749692189,
40.10025));
#205320=CARTESIAN_POINT('Origin',(-51.1126068659044,29.5274749692189,40.22725));
#205321=CARTESIAN_POINT('Ctrl Pts',(-53.7394427993284,30.6598643453579,
38.989));
#205322=CARTESIAN_POINT('Ctrl Pts',(-53.6758479277944,30.7700138939557,
38.989));
#205323=CARTESIAN_POINT('Ctrl Pts',(-53.6759428700935,30.7698494490698,
39.1161896013264));
#205324=CARTESIAN_POINT('Ctrl Pts',(-53.9274614872882,30.7681598456269,
38.989));
#205325=CARTESIAN_POINT('Ctrl Pts',(-53.8639162380569,30.8785957589629,
38.9887769275479));
#205326=CARTESIAN_POINT('Ctrl Pts',(-53.8262133418093,30.8566081460798,
39.1161898821845));
#205327=CARTESIAN_POINT('Ctrl Pts',(-54.1064511722685,30.8712573299225,
39.1034967087244));
#205328=CARTESIAN_POINT('Ctrl Pts',(-54.0429074791663,30.9819369489427,
39.1031720232703));
#205329=CARTESIAN_POINT('Ctrl Pts',(-53.9692682429949,30.9392009315184,
39.2077529615001));
#205330=CARTESIAN_POINT('Ctrl Pts',(-54.2060847114739,30.9286463962983,
39.2875012672119));
#205331=CARTESIAN_POINT('Ctrl Pts',(-54.1426202463873,31.0395064423977,
39.2872087095508));
#205332=CARTESIAN_POINT('Ctrl Pts',(-54.0488992470934,30.9851759130209,
39.3549017048226));
#205333=CARTESIAN_POINT('Origin',(-53.7394427993284,30.6598643453579,39.116));
#205334=CARTESIAN_POINT('Origin',(3.61170357355341E-16,2.93286234380104E-17,
40.22725));
#205335=CARTESIAN_POINT('Origin',(-51.1278468659044,29.5010785149116,40.22725));
#205336=CARTESIAN_POINT('Origin',(46.5080917980719,-27.2180767400485,39.116));
#205337=CARTESIAN_POINT('Origin',(-53.3918862459816,30.4591427892373,39.1160373285273));
#205338=CARTESIAN_POINT('Ctrl Pts',(-51.0345602039884,29.447251543774,40.1599502534424));
#205339=CARTESIAN_POINT('Ctrl Pts',(-51.0668719738975,29.4658956314771,
40.10025));
#205340=CARTESIAN_POINT('Ctrl Pts',(-51.1278468659044,29.5010785149116,
40.10025));
#205341=CARTESIAN_POINT('Ctrl Pts',(-51.0783704650304,29.3713249278651,
40.159950056604));
#205342=CARTESIAN_POINT('Ctrl Pts',(-51.0987866273836,29.4105784408359,
40.100255130536));
#205343=CARTESIAN_POINT('Ctrl Pts',(-51.1532877451691,29.4569685172218,
40.10025));
#205344=CARTESIAN_POINT('Ctrl Pts',(-51.1401588234662,29.3133705634516,
40.1203070619044));
#205345=CARTESIAN_POINT('Ctrl Pts',(-51.1479550638447,29.3708492661242,
40.0637098684497));
#205346=CARTESIAN_POINT('Ctrl Pts',(-51.198084132527,29.4284442379238,40.0772636213363));
#205347=CARTESIAN_POINT('Ctrl Pts',(-51.2555806533507,29.2571907880105,
40.0046102245804));
#205348=CARTESIAN_POINT('Ctrl Pts',(-51.2319089562573,29.3460364571625,
39.9670001894016));
#205349=CARTESIAN_POINT('Ctrl Pts',(-51.2912160489638,29.4108701703525,
40.0101788811209));
#205350=CARTESIAN_POINT('Ctrl Pts',(-51.3089178634635,29.2572675046854,
39.9303710930185));
#205351=CARTESIAN_POINT('Ctrl Pts',(-51.2670782717317,29.3615545506876,
39.9058663574103));
#205352=CARTESIAN_POINT('Ctrl Pts',(-51.3389765898556,29.4206015015123,
39.9671344706357));
#205353=CARTESIAN_POINT('Ctrl Pts',(-51.3482501200163,29.2799753962467,
39.8576902534424));
#205354=CARTESIAN_POINT('Ctrl Pts',(-51.2854610231999,29.3897042746978,
39.8579948730704));
#205355=CARTESIAN_POINT('Ctrl Pts',(-51.3783102687782,29.4433108116265,
39.92499));
#205356=CARTESIAN_POINT('Origin',(-51.4418102687782,29.3333255853459,39.92499));
#205357=CARTESIAN_POINT('Origin',(-53.3535596824659,30.437074623968,39.1925554488847));
#205358=CARTESIAN_POINT('Origin',(-53.2826856060843,30.3961554568841,39.3343017080178));
#205359=CARTESIAN_POINT('Origin',(-51.5960921371744,29.4224002636274,39.6398955069223));
#205360=CARTESIAN_POINT('Origin',(-51.750374005494,29.5114749418009,39.3548010137695));
#205361=CARTESIAN_POINT('Ctrl Pts',(-52.9969317578285,30.2311753956717,
39.3978017080178));
#205362=CARTESIAN_POINT('Ctrl Pts',(-52.9334317578285,30.3411606219523,
39.3978017080178));
#205363=CARTESIAN_POINT('Ctrl Pts',(-52.9334317578285,30.3411606219523,
39.5248017080178));
#205364=CARTESIAN_POINT('Ctrl Pts',(-53.0747660209932,30.2763834500036,
39.3978017080178));
#205365=CARTESIAN_POINT('Ctrl Pts',(-53.0113099140572,30.3861235964154,
39.3980355775173));
#205366=CARTESIAN_POINT('Ctrl Pts',(-53.0503573673261,30.4086676540709,
39.5248015517192));
#205367=CARTESIAN_POINT('Ctrl Pts',(-53.1483650929077,30.3191294881006,
39.3484893995498));
#205368=CARTESIAN_POINT('Ctrl Pts',(-53.0853168809894,30.4288515386957,
39.3489438303427));
#205369=CARTESIAN_POINT('Ctrl Pts',(-53.1609188493371,30.472500355472,39.4508333155597));
#205370=CARTESIAN_POINT('Ctrl Pts',(-53.1871522506172,30.3416565762241,
39.2708017080178));
#205371=CARTESIAN_POINT('Ctrl Pts',(-53.1243619179793,30.4513942013118,
39.2710850691866));
#205372=CARTESIAN_POINT('Ctrl Pts',(-53.2191856060843,30.5061406831648,
39.3343017080178));
#205373=CARTESIAN_POINT('Origin',(-52.9969317578285,30.2311753956717,39.5248017080178));
#205374=CARTESIAN_POINT('Ctrl Pts',(-51.6568155675425,29.4581217525678,
39.2875012672119));
#205375=CARTESIAN_POINT('Ctrl Pts',(-51.5939283826159,29.5680161684461,
39.2878045257519));
#205376=CARTESIAN_POINT('Ctrl Pts',(-51.6870133715069,29.6215404675521,
39.3549015218347));
#205377=CARTESIAN_POINT('Ctrl Pts',(-51.7564542486366,29.5155056307134,
39.1034938540228));
#205378=CARTESIAN_POINT('Ctrl Pts',(-51.6933631336501,29.6254251653837,
39.1038286278814));
#205379=CARTESIAN_POINT('Ctrl Pts',(-51.7666458147666,29.6675162799448,
39.2077506434032));
#205380=CARTESIAN_POINT('Ctrl Pts',(-51.9354510367808,29.6185943474771,
38.989));
#205381=CARTESIAN_POINT('Ctrl Pts',(-51.8721362050962,29.7286404220048,
38.9892298954605));
#205382=CARTESIAN_POINT('Ctrl Pts',(-51.9097019182958,29.750109759541,39.1161900347289));
#205383=CARTESIAN_POINT('Ctrl Pts',(-52.1234703131944,29.7268821954854,
38.989));
#205384=CARTESIAN_POINT('Ctrl Pts',(-52.0598751946718,29.8370321718799,
38.989));
#205385=CARTESIAN_POINT('Ctrl Pts',(-52.0599703843282,29.8368672985587,
39.1161900945646));
#205386=CARTESIAN_POINT('Origin',(-52.1234703131944,29.7268821954854,39.116));
#205387=CARTESIAN_POINT('Origin',(45.3776874999996,-26.5654375142634,39.5248017080178));
#205388=CARTESIAN_POINT('Origin',(-52.8659816883957,30.1555713378342,39.5248017080178));
#205389=CARTESIAN_POINT('Origin',(45.2006711678726,-26.4632370872589,39.116));
#205390=CARTESIAN_POINT('Origin',(-52.4710850656381,29.9275190026063,39.1160402713852));
#205391=CARTESIAN_POINT('Ctrl Pts',(-52.6757649139393,30.0450834959841,
39.2708017080178));
#205392=CARTESIAN_POINT('Ctrl Pts',(-52.6124111049554,30.1558192616006,
39.27051194648));
#205393=CARTESIAN_POINT('Ctrl Pts',(-52.5167277788839,30.1005764675362,
39.3343017080178));
#205394=CARTESIAN_POINT('Ctrl Pts',(-52.7146817640547,30.0676891808493,
39.3487519301185));
#205395=CARTESIAN_POINT('Ctrl Pts',(-52.6511806140165,30.1782028480957,
39.3482879463988));
#205396=CARTESIAN_POINT('Ctrl Pts',(-52.5751914484999,30.1343304829268,
39.4512271261642));
#205397=CARTESIAN_POINT('Ctrl Pts',(-52.788409875246,30.1105150503713,39.3978017080178));
#205398=CARTESIAN_POINT('Ctrl Pts',(-52.7247179826667,30.2206596676787,
39.3975673827392));
#205399=CARTESIAN_POINT('Ctrl Pts',(-52.685949917523,30.1982769148324,39.5248015355181));
#205400=CARTESIAN_POINT('Ctrl Pts',(-52.8659816883957,30.1555713378342,
39.3978017080178));
#205401=CARTESIAN_POINT('Ctrl Pts',(-52.8024816883957,30.2655565641149,
39.3978017080178));
#205402=CARTESIAN_POINT('Ctrl Pts',(-52.8024816883957,30.2655565641149,
39.5248017080178));
#205403=CARTESIAN_POINT('Origin',(-52.5802277788839,29.9905912412556,39.3343017080178));
#205404=CARTESIAN_POINT('Origin',(-52.509776381272,29.9499161075316,39.1934008533548));
#205405=CARTESIAN_POINT('Origin',(-49.5064990290873,36.3610285397835,39.1925554495084));
#205406=CARTESIAN_POINT('Origin',(-49.5422481179704,36.3870656659293,39.1160373285299));
#205407=CARTESIAN_POINT('Origin',(-49.4402904249163,36.3129251734947,39.3343017080178));
#205408=CARTESIAN_POINT('Ctrl Pts',(-49.3516463037382,36.2478178023255,
39.2708017080178));
#205409=CARTESIAN_POINT('Ctrl Pts',(-49.4263574835548,36.1458216659129,
39.2710850691866));
#205410=CARTESIAN_POINT('Ctrl Pts',(-49.5149391519574,36.2101800152091,
39.3343017080178));
#205411=CARTESIAN_POINT('Ctrl Pts',(-49.3151677697924,36.2214577843983,
39.3487519293518));
#205412=CARTESIAN_POINT('Ctrl Pts',(-49.3897594742873,36.1192316557419,
39.3492068662902));
#205413=CARTESIAN_POINT('Ctrl Pts',(-49.4603240281357,36.1704998050804,
39.451227124873));
#205414=CARTESIAN_POINT('Ctrl Pts',(-49.2460589922052,36.1715192752722,
39.3978017080178));
#205415=CARTESIAN_POINT('Ctrl Pts',(-49.3205022166676,36.0689133127054,
39.3980347781197));
#205416=CARTESIAN_POINT('Ctrl Pts',(-49.356856553303,36.0953262843491,39.5248015355195));
#205417=CARTESIAN_POINT('Ctrl Pts',(-49.1733470784084,36.1189794796887,
39.3978017080178));
#205418=CARTESIAN_POINT('Ctrl Pts',(-49.2479958054496,36.0162343214031,
39.3978017080178));
#205419=CARTESIAN_POINT('Ctrl Pts',(-49.2479958054496,36.0162343214031,
39.5248017080178));
#205420=CARTESIAN_POINT('Origin',(-49.1733470784084,36.1189794796887,39.5248017080178));
#205421=CARTESIAN_POINT('Origin',(0.186621817602868,0.256862895714044,39.116));
#205422=CARTESIAN_POINT('Origin',(-49.8669803696023,36.6229335645814,39.116));
#205423=CARTESIAN_POINT('Origin',(0.186621817602868,0.256862895714044,39.5248017080178));
#205424=CARTESIAN_POINT('Origin',(-49.05101714314,36.0301015792681,39.5248017080178));
#205425=CARTESIAN_POINT('Ctrl Pts',(-50.3023253561992,36.939908654649,39.2875012672119));
#205426=CARTESIAN_POINT('Ctrl Pts',(-50.377787717748,36.8368401467448,39.287208709576));
#205427=CARTESIAN_POINT('Ctrl Pts',(-50.2900345588341,36.7733199672428,
39.354901699012));
#205428=CARTESIAN_POINT('Ctrl Pts',(-50.2093718139431,36.8722300970262,
39.1034939173931));
#205429=CARTESIAN_POINT('Ctrl Pts',(-50.2846371204121,36.7691625978866,
39.1031692336331));
#205430=CARTESIAN_POINT('Ctrl Pts',(-50.2156443459689,36.7192723137688,
39.2077507202301));
#205431=CARTESIAN_POINT('Ctrl Pts',(-50.0423845927714,36.750647447547,38.989));
#205432=CARTESIAN_POINT('Ctrl Pts',(-50.1174266236757,36.6476776482617,
38.9887769311182));
#205433=CARTESIAN_POINT('Ctrl Pts',(-50.0820053531167,36.6221779017731,
39.116189871291));
#205434=CARTESIAN_POINT('Ctrl Pts',(-49.8669803696023,36.6229335645814,
38.989));
#205435=CARTESIAN_POINT('Ctrl Pts',(-49.9417406183797,36.5200349097942,
38.989));
#205436=CARTESIAN_POINT('Ctrl Pts',(-49.9416290134636,36.5201885207829,
39.1161895903849));
#205437=CARTESIAN_POINT('Origin',(-50.2155162706041,36.8761597191958,39.3548010137695));
#205438=CARTESIAN_POINT('Ctrl Pts',(-49.05101714314,36.0301015792681,39.3978017080178));
#205439=CARTESIAN_POINT('Ctrl Pts',(-49.1256658701812,35.9273564209825,
39.3978017080178));
#205440=CARTESIAN_POINT('Ctrl Pts',(-49.1256658701812,35.9273564209825,
39.5248017080178));
#205441=CARTESIAN_POINT('Ctrl Pts',(-48.9780591316057,35.9773846774561,
39.3978017080178));
#205442=CARTESIAN_POINT('Ctrl Pts',(-49.0527758071224,35.874398690299,39.3975666025017));
#205443=CARTESIAN_POINT('Ctrl Pts',(-49.016437187947,35.8479971380613,39.5248015517178));
#205444=CARTESIAN_POINT('Ctrl Pts',(-48.9090707128232,35.9275383438678,
39.3484894016716));
#205445=CARTESIAN_POINT('Ctrl Pts',(-48.9842025736629,35.8245773199103,
39.3480259000054));
#205446=CARTESIAN_POINT('Ctrl Pts',(-48.9131536812787,35.7729572780253,
39.4508333188949));
#205447=CARTESIAN_POINT('Ctrl Pts',(-48.872713344794,35.9012693628909,39.2708017080178));
#205448=CARTESIAN_POINT('Ctrl Pts',(-48.9481071848794,35.7983524848939,
39.27051194648));
#205449=CARTESIAN_POINT('Ctrl Pts',(-48.8587224664497,35.733410685601,39.3343017080178));
#205450=CARTESIAN_POINT('Origin',(-48.7840737394086,35.8361558438867,39.3343017080178));
#205451=CARTESIAN_POINT('Origin',(-50.3596419293478,36.9808731396215,39.6398955068191));
#205452=CARTESIAN_POINT('Origin',(-50.5037675878942,37.0855865599607,39.92499));
#205453=CARTESIAN_POINT('Origin',(-48.7182599900743,35.7883393560622,39.1934008539949));
#205454=CARTESIAN_POINT('Origin',(-48.6820620414858,35.7621028045855,39.1160402713848));
#205455=CARTESIAN_POINT('Ctrl Pts',(-50.9219998155897,37.0158684358564,
40.1599502534424));
#205456=CARTESIAN_POINT('Ctrl Pts',(-50.8918248690997,36.9939338721437,
40.10025));
#205457=CARTESIAN_POINT('Ctrl Pts',(-50.8348823336483,36.9525415975216,
40.10025));
#205458=CARTESIAN_POINT('Ctrl Pts',(-50.8701895025857,37.0871426490249,
40.1599500538467));
#205459=CARTESIAN_POINT('Ctrl Pts',(-50.8540829678241,37.0458491715919,
40.100244835349));
#205460=CARTESIAN_POINT('Ctrl Pts',(-50.8048852215546,36.9937925764108,
40.10025));
#205461=CARTESIAN_POINT('Ctrl Pts',(-50.8021467555731,37.1382015956604,
40.1202442001038));
#205462=CARTESIAN_POINT('Ctrl Pts',(-50.8006171556815,37.0800635522217,
40.0633873868018));
#205463=CARTESIAN_POINT('Ctrl Pts',(-50.756969208081,37.0171501059292,40.0772271723538));
#205464=CARTESIAN_POINT('Ctrl Pts',(-50.6806663304941,37.1817767082791,
40.0045995998163));
#205465=CARTESIAN_POINT('Ctrl Pts',(-50.7142182018859,37.0956112176477,
39.9663485808315));
#205466=CARTESIAN_POINT('Ctrl Pts',(-50.6618927960199,37.0243843935855,
40.0101727202465));
#205467=CARTESIAN_POINT('Ctrl Pts',(-50.6273693057704,37.1760624637761,
39.9304654349858));
#205468=CARTESIAN_POINT('Ctrl Pts',(-50.6810088489711,37.0763301845675,
39.9051900162956));
#205469=CARTESIAN_POINT('Ctrl Pts',(-50.6152053999548,37.0095702365081,
39.9671857458182));
#205470=CARTESIAN_POINT('Ctrl Pts',(-50.5905785208481,37.1493329797265,
39.8576902534424));
#205471=CARTESIAN_POINT('Ctrl Pts',(-50.665924074908,37.0464195108257,39.8573998014387));
#205472=CARTESIAN_POINT('Ctrl Pts',(-50.5784163149354,36.9828414016751,
39.92499));
#205473=CARTESIAN_POINT('Origin',(-50.8348823336483,36.9525415975216,40.22725));
#205474=CARTESIAN_POINT('Origin',(0.186621817602868,0.256862895714044,39.116));
#205475=CARTESIAN_POINT('Origin',(-48.3573835402116,35.526147267887,39.116));
#205476=CARTESIAN_POINT('Origin',(1.03190816135906E-16,-9.69196709112375E-17,
40.22725));
#205477=CARTESIAN_POINT('Origin',(-50.8527980281382,36.9278827595331,40.22725));
#205478=CARTESIAN_POINT('Ctrl Pts',(-48.3573835402116,35.526147267887,38.989));
#205479=CARTESIAN_POINT('Ctrl Pts',(-48.4321440944166,35.4232481927149,
38.989));
#205480=CARTESIAN_POINT('Ctrl Pts',(-48.4320321836171,35.423402224716,39.1161901092319));
#205481=CARTESIAN_POINT('Ctrl Pts',(-48.1819806163548,35.3984257650683,
38.989));
#205482=CARTESIAN_POINT('Ctrl Pts',(-48.2567602586406,35.2958250128989,
38.989229898976));
#205483=CARTESIAN_POINT('Ctrl Pts',(-48.2916533613388,35.3214110399818,
39.1161900493199));
#205484=CARTESIAN_POINT('Ctrl Pts',(-48.0150011530602,35.2768349808766,
39.1034966344368));
#205485=CARTESIAN_POINT('Ctrl Pts',(-48.0897561847363,35.1744900671682,
39.1038314102573));
#205486=CARTESIAN_POINT('Ctrl Pts',(-48.1580153629271,35.2243173504724,
39.2077528789601));
#205487=CARTESIAN_POINT('Ctrl Pts',(-47.9220530736684,35.2091516650532,
39.2875012672119));
#205488=CARTESIAN_POINT('Ctrl Pts',(-47.9968681042458,35.1070032653419,
39.2878045257868));
#205489=CARTESIAN_POINT('Ctrl Pts',(-48.0836260618763,35.1702703594596,
39.3549015295897));
#205490=CARTESIAN_POINT('Origin',(-48.0088472823269,35.2729208539819,39.3548010137695));
#205491=CARTESIAN_POINT('Ctrl Pts',(-50.964463724589,36.6347241449659,39.8576902534424));
#205492=CARTESIAN_POINT('Ctrl Pts',(-50.8898702560315,36.7381840359688,
39.8573998014387));
#205493=CARTESIAN_POINT('Ctrl Pts',(-50.8023624960588,36.6746059268182,
39.92499));
#205494=CARTESIAN_POINT('Ctrl Pts',(-51.0012706547886,36.6614665482809,
39.9304984902493));
#205495=CARTESIAN_POINT('Ctrl Pts',(-50.9229972443165,36.7432905102103,
39.9052171569806));
#205496=CARTESIAN_POINT('Ctrl Pts',(-50.8391683443882,36.7013469409088,
39.9672049726601));
#205497=CARTESIAN_POINT('Ctrl Pts',(-51.0230245369435,36.7102884597167,
40.004343767866));
#205498=CARTESIAN_POINT('Ctrl Pts',(-50.9514409225344,36.7689049964548,
39.9661628577642));
#205499=CARTESIAN_POINT('Ctrl Pts',(-50.867535894942,36.7410683485313,40.0100243556235));
#205500=CARTESIAN_POINT('Ctrl Pts',(-51.0194219249358,36.8383381382868,
40.119487482199));
#205501=CARTESIAN_POINT('Ctrl Pts',(-50.9635175930195,36.8551762168625,
40.062755148314));
#205502=CARTESIAN_POINT('Ctrl Pts',(-50.8901021525742,36.8330984946713,
40.0767884282377));
#205503=CARTESIAN_POINT('Ctrl Pts',(-50.9918932610483,36.9196318328646,
40.1599502015384));
#205504=CARTESIAN_POINT('Ctrl Pts',(-50.9476171190676,36.9171104726342,
40.1002449453869));
#205505=CARTESIAN_POINT('Ctrl Pts',(-50.882859665751,36.8864699989243,40.10025));
#205506=CARTESIAN_POINT('Ctrl Pts',(-50.9399462128199,36.9911673391712,
40.1599502534424));
#205507=CARTESIAN_POINT('Ctrl Pts',(-50.9097606317991,36.9692474126344,
40.10025));
#205508=CARTESIAN_POINT('Ctrl Pts',(-50.8527980281382,36.9278827595331,
40.10025));
#205509=CARTESIAN_POINT('Origin',(-50.8770112230999,36.5718607685326,39.92499));
#205510=CARTESIAN_POINT('Origin',(-47.864721425496,35.1682072895758,39.6398955069329));
#205511=CARTESIAN_POINT('Origin',(-47.7205955685088,35.0634937251226,39.92499));
#205512=CARTESIAN_POINT('Origin',(-50.7328855645153,36.4671473482232,39.6398955068274));
#205513=CARTESIAN_POINT('Origin',(-50.5887599058098,36.3624339277678,39.3548010137695));
#205514=CARTESIAN_POINT('Ctrl Pts',(-47.6338034047597,34.9997217530264,
39.8576902534424));
#205515=CARTESIAN_POINT('Ctrl Pts',(-47.7085070967801,34.8977303031706,
39.8579948730704));
#205516=CARTESIAN_POINT('Ctrl Pts',(-47.7952442955499,34.960748566837,39.92499));
#205517=CARTESIAN_POINT('Ctrl Pts',(-47.597045191607,34.9730146904941,39.9304020711231));
#205518=CARTESIAN_POINT('Ctrl Pts',(-47.675296659073,34.8923835282623,39.9058915297375));
#205519=CARTESIAN_POINT('Ctrl Pts',(-47.7584842465943,34.9340408279391,
39.9671523786028));
#205520=CARTESIAN_POINT('Ctrl Pts',(-47.5754322771533,34.9244461536127,
40.0043257306693));
#205521=CARTESIAN_POINT('Ctrl Pts',(-47.6469756149924,34.8665972787026,
39.9667894847838));
#205522=CARTESIAN_POINT('Ctrl Pts',(-47.7303228514092,34.8944891948627,
40.0100138975202));
#205523=CARTESIAN_POINT('Ctrl Pts',(-47.5794993790982,34.7970725085261,
40.1195533054857));
#205524=CARTESIAN_POINT('Ctrl Pts',(-47.635319763777,34.7804938560726,40.0630813209234));
#205525=CARTESIAN_POINT('Ctrl Pts',(-47.708416089387,34.8028668197837,40.0768265942419));
#205526=CARTESIAN_POINT('Ctrl Pts',(-47.6073089936885,34.7162617467345,
40.1599502027516));
#205527=CARTESIAN_POINT('Ctrl Pts',(-47.651501311427,34.7189078610141,40.1002552791553));
#205528=CARTESIAN_POINT('Ctrl Pts',(-47.7160937685338,34.7497660430534,
40.10025));
#205529=CARTESIAN_POINT('Ctrl Pts',(-47.6590285860933,34.645114416419,40.1599502534424));
#205530=CARTESIAN_POINT('Ctrl Pts',(-47.689203188551,34.6670494534022,40.10025));
#205531=CARTESIAN_POINT('Ctrl Pts',(-47.7461450747862,34.7084426211235,
40.10025));
#205532=CARTESIAN_POINT('Origin',(-47.7461450747862,34.7084426211235,40.22725));
#205533=CARTESIAN_POINT('Ctrl Pts',(-50.240224004808,36.1092077731533,38.989));
#205534=CARTESIAN_POINT('Ctrl Pts',(-50.1654637495897,36.2121064368056,
38.989));
#205535=CARTESIAN_POINT('Ctrl Pts',(-50.1655753609562,36.2119528169385,
39.1161896013264));
#205536=CARTESIAN_POINT('Ctrl Pts',(-50.4158927445024,36.2365633238561,
38.989));
#205537=CARTESIAN_POINT('Ctrl Pts',(-50.3411519064795,36.339751970454,38.988776927543));
#205538=CARTESIAN_POINT('Ctrl Pts',(-50.3059538820317,36.3139437822118,
39.1161898821846));
#205539=CARTESIAN_POINT('Ctrl Pts',(-50.5831252836573,36.3578055460614,
39.1034967087244));
#205540=CARTESIAN_POINT('Ctrl Pts',(-50.5083605190661,36.4612367259627,
39.1031720232725));
#205541=CARTESIAN_POINT('Ctrl Pts',(-50.4395918165607,36.4110374247131,
39.2077529615003));
#205542=CARTESIAN_POINT('Ctrl Pts',(-50.6762142289945,36.4252947698683,
39.2875012672119));
#205543=CARTESIAN_POINT('Ctrl Pts',(-50.6015093986314,36.5289136700281,
39.2872087095508));
#205544=CARTESIAN_POINT('Ctrl Pts',(-50.5139808995221,36.4650842569438,
39.3549017048227));
#205545=CARTESIAN_POINT('Origin',(-50.240224004808,36.1092077731533,39.116));
#205546=CARTESIAN_POINT('Origin',(3.64514313700083E-16,3.44778646538036E-17,
40.22725));
#205547=CARTESIAN_POINT('Origin',(-47.764060769276,34.683783783135,40.22725));
#205548=CARTESIAN_POINT('Origin',(40.5385041740525,-29.8453988870287,39.116));
#205549=CARTESIAN_POINT('Origin',(-49.9155525184323,35.8732562382991,39.1160373285273));
#205550=CARTESIAN_POINT('Ctrl Pts',(-47.6769115920301,34.6205005703638,
40.1599502534424));
#205551=CARTESIAN_POINT('Ctrl Pts',(-47.7070975168461,34.6424200234579,
40.10025));
#205552=CARTESIAN_POINT('Ctrl Pts',(-47.764060769276,34.683783783135,40.10025));
#205553=CARTESIAN_POINT('Ctrl Pts',(-47.7284183483602,34.5495693076633,
40.1599500566042));
#205554=CARTESIAN_POINT('Ctrl Pts',(-47.7446195594519,34.5907418558602,
40.100255130536));
#205555=CARTESIAN_POINT('Ctrl Pts',(-47.7939730310155,34.6425747206417,
40.10025));
#205556=CARTESIAN_POINT('Ctrl Pts',(-47.7959261043552,34.498391065477,40.1203070619046));
#205557=CARTESIAN_POINT('Ctrl Pts',(-47.7976714756521,34.556369822828,40.0637098684497));
#205558=CARTESIAN_POINT('Ctrl Pts',(-47.8415056181568,34.6188891978604,
40.0772636213363));
#205559=CARTESIAN_POINT('Ctrl Pts',(-47.9165880269726,34.4545839152295,
40.0046102245802));
#205560=CARTESIAN_POINT('Ctrl Pts',(-47.8837591046483,34.54046851239,39.9670001894016));
#205561=CARTESIAN_POINT('Ctrl Pts',(-47.9359643384879,34.6111463389768,
40.0101788811209));
#205562=CARTESIAN_POINT('Ctrl Pts',(-47.9696250311905,34.4602354682514,
39.9303710930186));
#205563=CARTESIAN_POINT('Ctrl Pts',(-47.9171136764619,34.5595777906768,
39.9058663574108));
#205564=CARTESIAN_POINT('Ctrl Pts',(-47.982446041048,34.6258166968307,39.9671344706366));
#205565=CARTESIAN_POINT('Ctrl Pts',(-48.0063682005184,34.4869303039401,
39.8576902534424));
#205566=CARTESIAN_POINT('Ctrl Pts',(-47.9324532779035,34.5894948283137,
39.8579948730703));
#205567=CARTESIAN_POINT('Ctrl Pts',(-48.0191904766733,34.6525130919801,
39.92499));
#205568=CARTESIAN_POINT('Origin',(-48.0938392037145,34.5497679336945,39.92499));
#205569=CARTESIAN_POINT('Origin',(-49.8797426632439,35.8473027479618,39.1925554488847));
#205570=CARTESIAN_POINT('Origin',(-49.813534060122,35.7991993820666,39.3343017080178));
#205571=CARTESIAN_POINT('Origin',(-48.2379650606559,34.6544814981802,39.6398955069217));
#205572=CARTESIAN_POINT('Origin',(-48.3820909175326,34.7591950625538,39.3548010137695));
#205573=CARTESIAN_POINT('Ctrl Pts',(-49.5465907136142,35.6052536882606,
39.3978017080178));
#205574=CARTESIAN_POINT('Ctrl Pts',(-49.471941986573,35.7079988465462,39.3978017080178));
#205575=CARTESIAN_POINT('Ctrl Pts',(-49.471941986573,35.7079988465462,39.5248017080178));
#205576=CARTESIAN_POINT('Ctrl Pts',(-49.6192730640965,35.6583499840564,
39.3978017080178));
#205577=CARTESIAN_POINT('Ctrl Pts',(-49.5446936074929,35.7608559931221,
39.3980355775182));
#205578=CARTESIAN_POINT('Ctrl Pts',(-49.5811706590224,35.7873581223583,
39.5248015517192));
#205579=CARTESIAN_POINT('Ctrl Pts',(-49.6880007749199,35.7085550527711,
39.3484893995498));
#205580=CARTESIAN_POINT('Ctrl Pts',(-49.6138288703648,35.8110857017878,
39.3489438303412));
#205581=CARTESIAN_POINT('Ctrl Pts',(-49.6844541394787,35.8623979633502,
39.4508333155589));
#205582=CARTESIAN_POINT('Ctrl Pts',(-49.7242207306172,35.7350130971393,
39.2708017080178));
#205583=CARTESIAN_POINT('Ctrl Pts',(-49.6503036646782,35.8375861910561,
39.2710850691866));
#205584=CARTESIAN_POINT('Ctrl Pts',(-49.7388853330808,35.9019445403522,
39.3343017080178));
#205585=CARTESIAN_POINT('Origin',(-49.5465907136142,35.6052536882606,39.5248017080178));
#205586=CARTESIAN_POINT('Ctrl Pts',(-48.2946219293743,34.6963546279289,
39.2875012672119));
#205587=CARTESIAN_POINT('Ctrl Pts',(-48.2205921526132,34.7990735298992,
39.2878045257519));
#205588=CARTESIAN_POINT('Ctrl Pts',(-48.3075723994626,34.8620346481363,
39.3549015218348));
#205589=CARTESIAN_POINT('Ctrl Pts',(-48.3877165307502,34.7638392294012,
39.1034938540228));
#205590=CARTESIAN_POINT('Ctrl Pts',(-48.3134813154478,34.8665617960639,
39.1038286278799));
#205591=CARTESIAN_POINT('Ctrl Pts',(-48.3819628268478,34.9160824571373,
39.2077506434029));
#205592=CARTESIAN_POINT('Ctrl Pts',(-48.5549570506144,34.8850734745857,
38.989));
#205593=CARTESIAN_POINT('Ctrl Pts',(-48.480486117147,34.9878985031432,38.9892298954618));
#205594=CARTESIAN_POINT('Ctrl Pts',(-48.5156018845779,35.0131769156751,
39.1161900347291));
#205595=CARTESIAN_POINT('Ctrl Pts',(-48.7306271754173,35.0124214764589,
38.989));
#205596=CARTESIAN_POINT('Ctrl Pts',(-48.6558666298464,35.1153205397472,
38.989));
#205597=CARTESIAN_POINT('Ctrl Pts',(-48.655978531999,35.1151665196476,39.1161900945647));
#205598=CARTESIAN_POINT('Origin',(-48.7306271754173,35.0124214764589,39.116));
#205599=CARTESIAN_POINT('Origin',(39.5520252162584,-29.1286799712089,39.5248017080178));
#205600=CARTESIAN_POINT('Origin',(-49.4242607783458,35.51637578784,39.5248017080178));
#205601=CARTESIAN_POINT('Origin',(39.3975469582344,-29.0164449471022,39.116));
#205602=CARTESIAN_POINT('Origin',(-49.0553654007523,35.2482948100397,39.1160402713849));
#205603=CARTESIAN_POINT('Ctrl Pts',(-49.246635155601,35.3866101428264,39.2708017080178));
#205604=CARTESIAN_POINT('Ctrl Pts',(-49.1720533660028,35.4901170100371,
39.27051194648));
#205605=CARTESIAN_POINT('Ctrl Pts',(-49.0826686475732,35.4251752107442,
39.3343017080178));
#205606=CARTESIAN_POINT('Ctrl Pts',(-49.2829758776396,35.4131599099222,
39.3487519301186));
#205607=CARTESIAN_POINT('Ctrl Pts',(-49.2082707697373,35.5164304941041,
39.3482879463997));
#205608=CARTESIAN_POINT('Ctrl Pts',(-49.1372837917323,35.4648554356489,
39.4512271261641));
#205609=CARTESIAN_POINT('Ctrl Pts',(-49.3518235761942,35.4634578610125,
39.3978017080178));
#205610=CARTESIAN_POINT('Ctrl Pts',(-49.276967346883,35.5663414789297,39.3975673827387));
#205611=CARTESIAN_POINT('Ctrl Pts',(-49.2407512920142,35.5400289748701,
39.5248015355181));
#205612=CARTESIAN_POINT('Ctrl Pts',(-49.4242607783458,35.51637578784,39.3978017080178));
#205613=CARTESIAN_POINT('Ctrl Pts',(-49.3496120513046,35.6191209461256,
39.3978017080178));
#205614=CARTESIAN_POINT('Ctrl Pts',(-49.3496120513046,35.6191209461256,
39.5248017080178));
#205615=CARTESIAN_POINT('Origin',(-49.1573173746143,35.3224300524586,39.3343017080178));
#205616=CARTESIAN_POINT('Origin',(-49.0915036263502,35.2746135650466,39.1934008533551));
#205617=CARTESIAN_POINT('Origin',(-45.4345348113613,41.3366772861953,39.1925554495078));
#205618=CARTESIAN_POINT('Origin',(-45.4673664422111,41.3663085755596,39.1160373285232));
#205619=CARTESIAN_POINT('Origin',(-45.3737170758069,41.2819167515332,39.3343017080178));
#205620=CARTESIAN_POINT('Ctrl Pts',(-45.2923641298554,41.2079002115911,
39.2708017080178));
#205621=CARTESIAN_POINT('Ctrl Pts',(-45.3773275334102,41.114272265501,39.2710850691866));
#205622=CARTESIAN_POINT('Ctrl Pts',(-45.4586966628145,41.1875373586976,
39.3343017080178));
#205623=CARTESIAN_POINT('Ctrl Pts',(-45.2588408013008,41.1778715515047,
39.3487519293518));
#205624=CARTESIAN_POINT('Ctrl Pts',(-45.3437094247727,41.0840023845234,
39.3492068662929));
#205625=CARTESIAN_POINT('Ctrl Pts',(-45.4085284377449,41.1423656859497,
39.4512271248738));
#205626=CARTESIAN_POINT('Ctrl Pts',(-45.1953306044444,41.1209827764383,
39.3978017080178));
#205627=CARTESIAN_POINT('Ctrl Pts',(-45.280091264719,41.0267203359225,39.3980347781178));
#205628=CARTESIAN_POINT('Ctrl Pts',(-45.3134855411615,41.0567886774842,
39.5248015355195));
#205629=CARTESIAN_POINT('Ctrl Pts',(-45.1285089182129,41.0611303347408,
39.3978017080178));
#205630=CARTESIAN_POINT('Ctrl Pts',(-45.2134885052205,40.9667509419051,
39.3978017080178));
#205631=CARTESIAN_POINT('Ctrl Pts',(-45.2134885052205,40.9667509419051,
39.5248017080178));
#205632=CARTESIAN_POINT('Origin',(-45.1285089182129,41.0611303347408,39.5248017080178));
#205633=CARTESIAN_POINT('Origin',(0.212448967518945,0.235948482089071,39.116));
#205634=CARTESIAN_POINT('Origin',(-45.7656648676103,41.6348281284266,39.116));
#205635=CARTESIAN_POINT('Origin',(0.212448967518945,0.235948482089071,39.5248017080178));
#205636=CARTESIAN_POINT('Origin',(-45.016139389479,40.9599523566129,39.5248017080178));
#205637=CARTESIAN_POINT('Ctrl Pts',(-46.1654920697608,41.9955727382255,
39.2875012672119));
#205638=CARTESIAN_POINT('Ctrl Pts',(-46.2513146333399,41.9009568150788,
39.287208709576));
#205639=CARTESIAN_POINT('Ctrl Pts',(-46.1706818621619,41.8286119029183,
39.354901699012));
#205640=CARTESIAN_POINT('Ctrl Pts',(-46.0801220723621,41.9185486398925,
39.1034939173931));
#205641=CARTESIAN_POINT('Ctrl Pts',(-46.1657485549033,41.8239131221199,
39.1031692336338));
#205642=CARTESIAN_POINT('Ctrl Pts',(-46.1023486848284,41.7670844335132,
39.2077507202299));
#205643=CARTESIAN_POINT('Ctrl Pts',(-45.9267584721682,41.7801771152764,
38.989));
#205644=CARTESIAN_POINT('Ctrl Pts',(-46.0121526898595,41.6856154234958,
38.9887769311176));
#205645=CARTESIAN_POINT('Ctrl Pts',(-45.9795909100378,41.6565528363084,
39.1161898712912));
#205646=CARTESIAN_POINT('Ctrl Pts',(-45.7656648676103,41.6348281284266,
38.989));
#205647=CARTESIAN_POINT('Ctrl Pts',(-45.8507714101799,41.5403077371549,
38.989));
#205648=CARTESIAN_POINT('Ctrl Pts',(-45.8506443599266,41.5404488407563,
39.1161895903851));
#205649=CARTESIAN_POINT('Origin',(-46.0858221116775,41.9230990057959,39.3548010137695));
#205650=CARTESIAN_POINT('Ctrl Pts',(-45.016139389479,40.9599523566129,39.3978017080178));
#205651=CARTESIAN_POINT('Ctrl Pts',(-45.1011189764865,40.8655729637772,
39.3978017080178));
#205652=CARTESIAN_POINT('Ctrl Pts',(-45.1011189764865,40.8655729637772,
39.5248017080178));
#205653=CARTESIAN_POINT('Ctrl Pts',(-44.9490914662995,40.8998980546771,
39.3978017080178));
#205654=CARTESIAN_POINT('Ctrl Pts',(-45.0341638030233,40.8052862548047,
39.3975666025003));
#205655=CARTESIAN_POINT('Ctrl Pts',(-45.0007839642914,40.7752309130121,
39.5248015517178));
#205656=CARTESIAN_POINT('Ctrl Pts',(-44.885691333944,40.8431135311197,39.3484894016716));
#205657=CARTESIAN_POINT('Ctrl Pts',(-44.9711739722005,40.7485699563835,
39.3480259000058));
#205658=CARTESIAN_POINT('Ctrl Pts',(-44.9059100567345,40.6898060629495,
39.4508333188946));
#205659=CARTESIAN_POINT('Ctrl Pts',(-44.8522789915938,40.813188074561,39.2708017080178));
#205660=CARTESIAN_POINT('Ctrl Pts',(-44.9380175594359,40.7187157882341,
39.27051194648));
#205661=CARTESIAN_POINT('Ctrl Pts',(-44.8559107663282,40.6447864996556,
39.3343017080178));
#205662=CARTESIAN_POINT('Origin',(-44.7709311793206,40.7391658924913,39.3343017080178));
#205663=CARTESIAN_POINT('Origin',(-46.2182127020652,42.0423040287734,39.6398955068177));
#205664=CARTESIAN_POINT('Origin',(-46.3506032922591,42.1615090516456,39.92499));
#205665=CARTESIAN_POINT('Origin',(-44.7104761485858,40.684731938309,39.193400853994));
#205666=CARTESIAN_POINT('Origin',(-44.6772189625514,40.6548553974684,39.1160402713846));
#205667=CARTESIAN_POINT('Ctrl Pts',(-46.7738319284254,42.1358900227699,
40.1599502534424));
#205668=CARTESIAN_POINT('Ctrl Pts',(-46.7461150696869,42.1109214781065,
40.10025));
#205669=CARTESIAN_POINT('Ctrl Pts',(-46.6938111422601,42.0638038389704,
40.10025));
#205670=CARTESIAN_POINT('Ctrl Pts',(-46.714855253764,42.2013581359417,40.1599500538471));
#205671=CARTESIAN_POINT('Ctrl Pts',(-46.7031532960251,42.1586072771723,
40.1002448353478));
#205672=CARTESIAN_POINT('Ctrl Pts',(-46.6596664560547,42.1016932886526,
40.10025));
#205673=CARTESIAN_POINT('Ctrl Pts',(-46.6418481388114,42.245024972543,40.1202442001042));
#205674=CARTESIAN_POINT('Ctrl Pts',(-46.6464039985657,42.1870455286632,
40.0633873868017));
#205675=CARTESIAN_POINT('Ctrl Pts',(-46.609571404849,42.1199142759251,40.0772271723538));
#205676=CARTESIAN_POINT('Ctrl Pts',(-46.5164783566522,42.275663213985,40.0045995998159));
#205677=CARTESIAN_POINT('Ctrl Pts',(-46.5588531737047,42.1934768724834,
39.9663485808314));
#205678=CARTESIAN_POINT('Ctrl Pts',(-46.5142596423495,42.1171707421506,
40.0101727202466));
#205679=CARTESIAN_POINT('Ctrl Pts',(-46.4640705998041,42.2644092166196,
39.9304654349861));
#205680=CARTESIAN_POINT('Ctrl Pts',(-46.5278411618548,42.1708301402928,
39.9051900162966));
#205681=CARTESIAN_POINT('Ctrl Pts',(-46.4693765057993,42.0975575768115,
39.9671857458179));
#205682=CARTESIAN_POINT('Ctrl Pts',(-46.4302753505421,42.2339804752705,
39.8576902534424));
#205683=CARTESIAN_POINT('Ctrl Pts',(-46.5159655405271,42.1395065321003,
39.8573998014387));
#205684=CARTESIAN_POINT('Ctrl Pts',(-46.4355828792667,42.06712965881,39.92499));
#205685=CARTESIAN_POINT('Origin',(-46.6938111422601,42.0638038389704,40.22725));
#205686=CARTESIAN_POINT('Origin',(0.212448967518945,0.235948482089071,39.116));
#205687=CARTESIAN_POINT('Origin',(-44.3789831537292,40.3862543050942,39.116));
#205688=CARTESIAN_POINT('Origin',(9.23291810287646E-17,-1.10332673220368E-16,
40.22725));
#205689=CARTESIAN_POINT('Origin',(-46.7142062431419,42.0411527846899,40.22725));
#205690=CARTESIAN_POINT('Ctrl Pts',(-44.3789831537292,40.3862543050942,
38.989));
#205691=CARTESIAN_POINT('Ctrl Pts',(-44.4640900439955,40.2917335276662,
38.989));
#205692=CARTESIAN_POINT('Ctrl Pts',(-44.4639626455265,40.2918750180003,
39.1161901092322));
#205693=CARTESIAN_POINT('Ctrl Pts',(-44.2178916378592,40.2408978759468,
38.989));
#205694=CARTESIAN_POINT('Ctrl Pts',(-44.3029863283978,40.1466757825274,
38.9892298989754));
#205695=CARTESIAN_POINT('Ctrl Pts',(-44.3350138149328,40.1757689690803,
39.1161900493202));
#205696=CARTESIAN_POINT('Ctrl Pts',(-44.0645366033547,40.1025190720979,
39.1034966344368));
#205697=CARTESIAN_POINT('Ctrl Pts',(-44.1495800756942,40.0085488431148,
39.1038314102563));
#205698=CARTESIAN_POINT('Ctrl Pts',(-44.2122569536148,40.0652381943514,
39.20775287896));
#205699=CARTESIAN_POINT('Ctrl Pts',(-43.9791725362579,40.0254908126592,
39.2875012672119));
#205700=CARTESIAN_POINT('Ctrl Pts',(-44.0642551375171,39.9317222927448,
39.2878045257868));
#205701=CARTESIAN_POINT('Ctrl Pts',(-44.1439246138545,40.0037114790889,
39.3549015295899));
#205702=CARTESIAN_POINT('Origin',(-44.0588255818374,40.0979831325503,39.3548010137695));
#205703=CARTESIAN_POINT('Ctrl Pts',(-46.8559036426982,41.7612723673367,
39.8576902534424));
#205704=CARTESIAN_POINT('Ctrl Pts',(-46.7709043015499,41.8563683535934,
39.8573998014387));
#205705=CARTESIAN_POINT('Ctrl Pts',(-46.6905216402894,41.7839914803031,
39.92499));
#205706=CARTESIAN_POINT('Ctrl Pts',(-46.8897135983598,41.7917156448197,
39.9304984902488));
#205707=CARTESIAN_POINT('Ctrl Pts',(-46.8033160448216,41.8649095672156,
39.9052171569791));
#205708=CARTESIAN_POINT('Ctrl Pts',(-46.7243306652211,41.8144332630853,
39.9672049726598));
#205709=CARTESIAN_POINT('Ctrl Pts',(-46.9062450310964,41.8425440045886,
40.0043437678665));
#205710=CARTESIAN_POINT('Ctrl Pts',(-46.8289264627112,41.8933569085961,
39.9661628577649));
#205711=CARTESIAN_POINT('Ctrl Pts',(-46.7483907976682,41.8569022891479,
40.0100243556237));
#205712=CARTESIAN_POINT('Ctrl Pts',(-46.8892773184515,41.9695156381233,
40.1194874821984));
#205713=CARTESIAN_POINT('Ctrl Pts',(-46.8319191778356,41.9804178820375,
40.0627551483134));
#205714=CARTESIAN_POINT('Ctrl Pts',(-46.7612136652285,41.9507871007485,
40.0767884282375));
#205715=CARTESIAN_POINT('Ctrl Pts',(-46.8534019544973,42.0474864684051,
40.1599502015382));
#205716=CARTESIAN_POINT('Ctrl Pts',(-46.8096319157665,42.0403508033695,
40.1002449453869));
#205717=CARTESIAN_POINT('Ctrl Pts',(-46.7484320121836,42.003109184299,40.10025));
#205718=CARTESIAN_POINT('Ctrl Pts',(-46.7942619810913,42.1132001506005,
40.1599502534424));
#205719=CARTESIAN_POINT('Ctrl Pts',(-46.7665330160776,42.0882450513179,
40.10025));
#205720=CARTESIAN_POINT('Ctrl Pts',(-46.7142062431419,42.0411527846899,
40.10025));
#205721=CARTESIAN_POINT('Origin',(-46.7755012272969,41.6896120874674,39.92499));
#205722=CARTESIAN_POINT('Origin',(-43.9264348094991,39.9787779456715,39.6398955069307));
#205723=CARTESIAN_POINT('Origin',(-43.7940440370141,39.8595727587359,39.92499));
#205724=CARTESIAN_POINT('Origin',(-46.6431106370596,41.5704070646253,39.6398955068254));
#205725=CARTESIAN_POINT('Origin',(-46.5107200467153,41.4512020416178,39.3548010137695));
#205726=CARTESIAN_POINT('Ctrl Pts',(-43.714393316062,39.7870778846751,39.8576902534424));
#205727=CARTESIAN_POINT('Ctrl Pts',(-43.799348782961,39.6934538167804,39.8579948730704));
#205728=CARTESIAN_POINT('Ctrl Pts',(-43.8790236240217,39.7651933659002,
39.92499));
#205729=CARTESIAN_POINT('Ctrl Pts',(-43.6806281164518,39.7566748466926,
39.9304020711229));
#205730=CARTESIAN_POINT('Ctrl Pts',(-43.7668791656724,39.6846648960486,
39.9058915297384));
#205731=CARTESIAN_POINT('Ctrl Pts',(-43.8452566693655,39.7347894633642,
39.9671523786037));
#205732=CARTESIAN_POINT('Ctrl Pts',(-43.6642103943284,39.7061132086031,
40.0043257306695));
#205733=CARTESIAN_POINT('Ctrl Pts',(-43.7414086642728,39.656059551044,39.9667894847838));
#205734=CARTESIAN_POINT('Ctrl Pts',(-43.8213838166742,39.6925108309093,
40.01001389752));
#205735=CARTESIAN_POINT('Ctrl Pts',(-43.681569387645,39.5798624575882,40.1195533054856));
#205736=CARTESIAN_POINT('Ctrl Pts',(-43.7388169234803,39.569209443757,40.0630813209234));
#205737=CARTESIAN_POINT('Ctrl Pts',(-43.8091742082548,39.5991004926183,
40.076826594242));
#205738=CARTESIAN_POINT('Ctrl Pts',(-43.7176736830024,39.502401281882,40.1599502027517));
#205739=CARTESIAN_POINT('Ctrl Pts',(-43.7613473163384,39.50965225553,40.1002552791541));
#205740=CARTESIAN_POINT('Ctrl Pts',(-43.8223603708606,39.5470931435009,
40.10025));
#205741=CARTESIAN_POINT('Ctrl Pts',(-43.7765468711719,39.4370498736012,
40.1599502534424));
#205742=CARTESIAN_POINT('Ctrl Pts',(-43.8042633382926,39.4620188529813,
40.10025));
#205743=CARTESIAN_POINT('Ctrl Pts',(-43.8565665267053,39.5091373124626,
40.10025));
#205744=CARTESIAN_POINT('Origin',(-43.8565665267053,39.5091373124626,40.22725));
#205745=CARTESIAN_POINT('Ctrl Pts',(-46.1905628026481,41.1629311642484,
38.989));
#205746=CARTESIAN_POINT('Ctrl Pts',(-46.1054562527463,41.2574515636633,
38.989));
#205747=CARTESIAN_POINT('Ctrl Pts',(-46.1055833103428,41.2573104519066,
39.1161896013265));
#205748=CARTESIAN_POINT('Ctrl Pts',(-46.3519569306006,41.3079514313256,
38.989));
#205749=CARTESIAN_POINT('Ctrl Pts',(-46.2668393800556,41.4027622547787,
38.988776927546));
#205750=CARTESIAN_POINT('Ctrl Pts',(-46.2345318643238,41.3734162510838,
39.1161898821846));
#205751=CARTESIAN_POINT('Ctrl Pts',(-46.5056000892403,41.4460100362752,
39.1034967087244));
#205752=CARTESIAN_POINT('Ctrl Pts',(-46.420433391565,41.541059563396,39.103172023271));
#205753=CARTESIAN_POINT('Ctrl Pts',(-46.3572886670226,41.4839469723845,
39.2077529615));
#205754=CARTESIAN_POINT('Ctrl Pts',(-46.5911245387426,41.5228599914567,
39.2875012672119));
#205755=CARTESIAN_POINT('Ctrl Pts',(-46.5059978248576,41.6181024753231,
39.2872087095508));
#205756=CARTESIAN_POINT('Ctrl Pts',(-46.4256208064857,41.5454735069382,
39.3549017048227));
#205757=CARTESIAN_POINT('Origin',(-46.1905628026481,41.1629311642484,39.116));
#205758=CARTESIAN_POINT('Origin',(3.68378193773366E-16,3.92493591694927E-17,
40.22725));
#205759=CARTESIAN_POINT('Origin',(-43.8769616275871,39.486486258182,40.22725));
#205760=CARTESIAN_POINT('Origin',(34.1507877370002,-31.1767457860026,39.116));
#205761=CARTESIAN_POINT('Origin',(-45.892333551989,40.8943347850521,39.1160373285266));
#205762=CARTESIAN_POINT('Ctrl Pts',(-43.7969047596343,39.4144401478993,
40.1599502534424));
#205763=CARTESIAN_POINT('Ctrl Pts',(-43.8246341160482,39.4393948122691,
40.10025));
#205764=CARTESIAN_POINT('Ctrl Pts',(-43.8769616275871,39.486486258182,40.10025));
#205765=CARTESIAN_POINT('Ctrl Pts',(-43.8555436924522,39.3492813761649,
40.1599500566032));
#205766=CARTESIAN_POINT('Ctrl Pts',(-43.8673524484236,39.3919218645342,
40.1002551305372));
#205767=CARTESIAN_POINT('Ctrl Pts',(-43.9110175468025,39.4486296259977,
40.10025));
#205768=CARTESIAN_POINT('Ctrl Pts',(-43.9280312169043,39.3054399757369,
40.1203070619046));
#205769=CARTESIAN_POINT('Ctrl Pts',(-43.9237065964667,39.3632835603681,
40.0637098684499));
#205770=CARTESIAN_POINT('Ctrl Pts',(-43.9607655567554,39.430042363277,40.0772636213363));
#205771=CARTESIAN_POINT('Ctrl Pts',(-44.0526112349802,39.2744854109879,
40.0046102245802));
#205772=CARTESIAN_POINT('Ctrl Pts',(-44.0109847679678,39.3564679665376,
39.9670001894012));
#205773=CARTESIAN_POINT('Ctrl Pts',(-44.0555161714742,39.4322155454632,
40.0101788811209));
#205774=CARTESIAN_POINT('Ctrl Pts',(-44.1047669487885,39.2856498807568,
39.9303710930186));
#205775=CARTESIAN_POINT('Ctrl Pts',(-44.0421591564523,39.3789590643314,
39.9058663574094));
#205776=CARTESIAN_POINT('Ctrl Pts',(-44.1002097724411,39.4516641984998,
39.967134470636));
#205777=CARTESIAN_POINT('Ctrl Pts',(-44.1385184650372,39.3160391863694,
39.8576902534424));
#205778=CARTESIAN_POINT('Ctrl Pts',(-44.0542875439837,39.4103156382735,
39.8579948730703));
#205779=CARTESIAN_POINT('Ctrl Pts',(-44.1339623850444,39.4820551873934,
39.92499));
#205780=CARTESIAN_POINT('Origin',(-44.218941972052,39.3876757945577,39.92499));
#205781=CARTESIAN_POINT('Origin',(-45.8594327453955,40.8647803215178,39.1925554488843));
#205782=CARTESIAN_POINT('Origin',(-45.7986150108448,40.8100197873551,39.3343017080178));
#205783=CARTESIAN_POINT('Origin',(-44.3513327444881,39.5068809815262,39.6398955069218));
#205784=CARTESIAN_POINT('Origin',(-44.4837235168753,39.6260861683721,39.3548010137695));
#205785=CARTESIAN_POINT('Ctrl Pts',(-45.5534068532508,40.5892333705626,
39.3978017080178));
#205786=CARTESIAN_POINT('Ctrl Pts',(-45.4684272662432,40.6836127633983,
39.3978017080178));
#205787=CARTESIAN_POINT('Ctrl Pts',(-45.4684272662432,40.6836127633983,
39.5248017080178));
#205788=CARTESIAN_POINT('Ctrl Pts',(-45.6201409680064,40.6496361736984,
39.3978017080178));
#205789=CARTESIAN_POINT('Ctrl Pts',(-45.5352552698605,40.7437849681284,
39.3980355775196));
#205790=CARTESIAN_POINT('Ctrl Pts',(-45.5687622694472,40.7739548060677,
39.5248015517192));
#205791=CARTESIAN_POINT('Ctrl Pts',(-45.6832443225586,40.7067502157891,
39.3484893995498));
#205792=CARTESIAN_POINT('Ctrl Pts',(-45.5987613682854,40.800966115985,39.3489438303422));
#205793=CARTESIAN_POINT('Ctrl Pts',(-45.6636361529334,40.859379634457,39.45083331556));
#205794=CARTESIAN_POINT('Ctrl Pts',(-45.7165002428303,40.7368493365301,
39.2708017080178));
#205795=CARTESIAN_POINT('Ctrl Pts',(-45.6322662944329,40.8311340869941,
39.2710850691866));
#205796=CARTESIAN_POINT('Ctrl Pts',(-45.7136354238372,40.9043991801907,
39.3343017080178));
#205797=CARTESIAN_POINT('Origin',(-45.5534068532508,40.5892333705626,39.5248017080178));
#205798=CARTESIAN_POINT('Ctrl Pts',(-44.4033023070486,39.5544469813075,
39.2875012672119));
#205799=CARTESIAN_POINT('Ctrl Pts',(-44.3189410241787,39.6488649595845,
39.2878045257519));
#205800=CARTESIAN_POINT('Ctrl Pts',(-44.3988635552005,39.7205730817659,
39.3549015218351));
#205801=CARTESIAN_POINT('Ctrl Pts',(-44.4888328647704,39.6312929306932,
39.1034938540228));
#205802=CARTESIAN_POINT('Ctrl Pts',(-44.4042668857084,39.7256930794085,
39.1038286278778));
#205803=CARTESIAN_POINT('Ctrl Pts',(-44.4671969296207,39.7821007282684,
39.2077506434024));
#205804=CARTESIAN_POINT('Ctrl Pts',(-44.6424847942264,39.769344436532,38.989));
#205805=CARTESIAN_POINT('Ctrl Pts',(-44.5576736781015,39.8638218465963,
38.9892298954636));
#205806=CARTESIAN_POINT('Ctrl Pts',(-44.5899547640708,39.8926323785438,
39.1161900347295));
#205807=CARTESIAN_POINT('Ctrl Pts',(-44.8038810887671,39.9143573409161,
38.989));
#205808=CARTESIAN_POINT('Ctrl Pts',(-44.7187742083296,40.0088781074279,
38.989));
#205809=CARTESIAN_POINT('Ctrl Pts',(-44.7189015969551,40.0087366280263,
39.1161900945652));
#205810=CARTESIAN_POINT('Origin',(-44.8038810887671,39.9143573409161,39.116));
#205811=CARTESIAN_POINT('Origin',(33.3184119221863,-30.4272712359684,39.5248017080178));
#205812=CARTESIAN_POINT('Origin',(-45.4410373245168,40.4880553924347,39.5248017080178));
#205813=CARTESIAN_POINT('Origin',(33.1880655373213,-30.3099068238764,39.116));
#205814=CARTESIAN_POINT('Origin',(-45.1021848870407,40.1828829233541,39.1160402713851));
#205815=CARTESIAN_POINT('Ctrl Pts',(-45.2779489569769,40.3404336838196,
39.2708017080178));
#205816=CARTESIAN_POINT('Ctrl Pts',(-45.1929563204586,40.4355776097272,
39.2705119464801));
#205817=CARTESIAN_POINT('Ctrl Pts',(-45.1108495273509,40.3616483211487,
39.3343017080178));
#205818=CARTESIAN_POINT('Ctrl Pts',(-45.3113153943826,40.3706366483427,
39.3487519301185));
#205819=CARTESIAN_POINT('Ctrl Pts',(-45.2262248134191,40.4655326953387,
39.3482879463977));
#205820=CARTESIAN_POINT('Ctrl Pts',(-45.1610177711094,40.4068200107242,
39.4512271261624));
#205821=CARTESIAN_POINT('Ctrl Pts',(-45.3745283705082,40.4278556061232,
39.3978017080178));
#205822=CARTESIAN_POINT('Ctrl Pts',(-45.2893279449732,40.5223510101947,
39.3975673827383));
#205823=CARTESIAN_POINT('Ctrl Pts',(-45.2560606910569,40.4923970402268,
39.5248015355181));
#205824=CARTESIAN_POINT('Ctrl Pts',(-45.4410373245168,40.4880553924347,
39.3978017080178));
#205825=CARTESIAN_POINT('Ctrl Pts',(-45.3560577375092,40.5824347852704,
39.3978017080178));
#205826=CARTESIAN_POINT('Ctrl Pts',(-45.3560577375093,40.5824347852704,
39.5248017080178));
#205827=CARTESIAN_POINT('Origin',(-45.1958291143585,40.2672689283131,39.3343017080178));
#205828=CARTESIAN_POINT('Origin',(-45.1353740846424,40.2128349746537,39.193400853355));
#205829=CARTESIAN_POINT('Origin',(-40.8647803224532,45.8594327460079,39.1925554495084));
#205830=CARTESIAN_POINT('Origin',(-40.8943347850518,45.8923335519894,39.1160373285266));
#205831=CARTESIAN_POINT('Origin',(-40.8100197873543,45.7986150108455,39.3343017080178));
#205832=CARTESIAN_POINT('Ctrl Pts',(-40.7368493365293,45.716500242831,39.2708017080178));
#205833=CARTESIAN_POINT('Ctrl Pts',(-40.8311340869933,45.6322662944336,
39.2710850691866));
#205834=CARTESIAN_POINT('Ctrl Pts',(-40.9043991801899,45.7136354238379,
39.3343017080178));
#205835=CARTESIAN_POINT('Ctrl Pts',(-40.7066485019697,45.6831319408686,
39.3487519293518));
#205836=CARTESIAN_POINT('Ctrl Pts',(-40.8008642060156,45.5986481857975,
39.3492068662932));
#205837=CARTESIAN_POINT('Ctrl Pts',(-40.8592275074407,45.6634671987668,
39.4512271248733));
#205838=CARTESIAN_POINT('Ctrl Pts',(-40.649432716852,45.6199161851846,39.3978017080178));
#205839=CARTESIAN_POINT('Ctrl Pts',(-40.7435821574136,45.5350300257427,
39.3980347781178));
#205840=CARTESIAN_POINT('Ctrl Pts',(-40.7736504989776,45.5684243021861,
39.5248015355195));
#205841=CARTESIAN_POINT('Ctrl Pts',(-40.5892333705618,45.5534068532515,
39.3978017080178));
#205842=CARTESIAN_POINT('Ctrl Pts',(-40.6836127633975,45.4684272662439,
39.3978017080178));
#205843=CARTESIAN_POINT('Ctrl Pts',(-40.6836127633975,45.4684272662439,
39.5248017080178));
#205844=CARTESIAN_POINT('Origin',(-40.5892333705618,45.5534068532515,39.5248017080178));
#205845=CARTESIAN_POINT('Origin',(0.23594848208908,0.212448967518935,39.116));
#205846=CARTESIAN_POINT('Origin',(-41.1629311642476,46.1905628026488,39.116));
#205847=CARTESIAN_POINT('Origin',(0.23594848208908,0.212448967518935,39.5248017080178));
#205848=CARTESIAN_POINT('Origin',(-40.4880553924339,45.4410373245175,39.5248017080178));
#205849=CARTESIAN_POINT('Ctrl Pts',(-41.5228599914559,46.5911245387433,
39.2875012672119));
#205850=CARTESIAN_POINT('Ctrl Pts',(-41.6181024670991,46.5059978322081,
39.287208709576));
#205851=CARTESIAN_POINT('Ctrl Pts',(-41.5454735131716,46.4256208133857,
39.3549016990121));
#205852=CARTESIAN_POINT('Ctrl Pts',(-41.4460088704665,46.5055987918449,
39.1034939173931));
#205853=CARTESIAN_POINT('Ctrl Pts',(-41.5410583874207,46.4204321019766,
39.1031692336335));
#205854=CARTESIAN_POINT('Ctrl Pts',(-41.4839460439595,46.3572876358793,
39.2077507202297));
#205855=CARTESIAN_POINT('Ctrl Pts',(-41.3079491749511,46.3519544194674,
38.989));
#205856=CARTESIAN_POINT('Ctrl Pts',(-41.4027599825073,46.2668368728761,
38.9887769311176));
#205857=CARTESIAN_POINT('Ctrl Pts',(-41.3734144471011,46.2345298607752,
39.1161898712913));
#205858=CARTESIAN_POINT('Ctrl Pts',(-41.1629311642476,46.1905628026488,
38.989));
#205859=CARTESIAN_POINT('Ctrl Pts',(-41.2574515555194,46.1054562600791,
38.989));
#205860=CARTESIAN_POINT('Ctrl Pts',(-41.2573104519179,46.1055833103326,
39.1161895903852));
#205861=CARTESIAN_POINT('Origin',(-41.451202041617,46.510720046716,39.3548010137695));
#205862=CARTESIAN_POINT('Ctrl Pts',(-40.4880553924339,45.4410373245175,
39.3978017080178));
#205863=CARTESIAN_POINT('Ctrl Pts',(-40.5824347852696,45.3560577375099,
39.3978017080178));
#205864=CARTESIAN_POINT('Ctrl Pts',(-40.5824347852696,45.3560577375099,
39.5248017080178));
#205865=CARTESIAN_POINT('Ctrl Pts',(-40.427652148688,45.3743035899551,39.3978017080178));
#205866=CARTESIAN_POINT('Ctrl Pts',(-40.5221480762998,45.2891025640498,
39.3975666025003));
#205867=CARTESIAN_POINT('Ctrl Pts',(-40.4920927345059,45.2557227253165,
39.5248015517178));
#205868=CARTESIAN_POINT('Ctrl Pts',(-40.3705349278749,45.3112030195542,
39.3484894016716));
#205869=CARTESIAN_POINT('Ctrl Pts',(-40.4654317778737,45.2261127332184,
39.3480259000072));
#205870=CARTESIAN_POINT('Ctrl Pts',(-40.4066678844398,45.1608488177557,
39.4508333188954));
#205871=CARTESIAN_POINT('Ctrl Pts',(-40.3404336838189,45.2779489569776,
39.2708017080178));
#205872=CARTESIAN_POINT('Ctrl Pts',(-40.4355776097265,45.1929563204593,
39.27051194648));
#205873=CARTESIAN_POINT('Ctrl Pts',(-40.361648321148,45.1108495273516,39.3343017080178));
#205874=CARTESIAN_POINT('Origin',(-40.2672689283123,45.1958291143592,39.3343017080178));
#205875=CARTESIAN_POINT('Origin',(-41.5704070646319,46.6431106370705,39.6398955068176));
#205876=CARTESIAN_POINT('Origin',(-41.6896120874666,46.7755012272977,39.92499));
#205877=CARTESIAN_POINT('Origin',(-40.2128349741375,45.1353740836144,39.1934008539954));
#205878=CARTESIAN_POINT('Origin',(-40.1828829233547,45.1021848870412,39.116040271384));
#205879=CARTESIAN_POINT('Ctrl Pts',(-42.1132001505997,46.794261981092,40.1599502534424));
#205880=CARTESIAN_POINT('Ctrl Pts',(-42.0882450513171,46.7665330160783,
40.10025));
#205881=CARTESIAN_POINT('Ctrl Pts',(-42.0411527846891,46.7142062431426,
40.10025));
#205882=CARTESIAN_POINT('Ctrl Pts',(-42.0477032750704,46.8532067119191,
40.1599500538478));
#205883=CARTESIAN_POINT('Ctrl Pts',(-42.0405341034509,46.8094668591674,
40.100244835349));
#205884=CARTESIAN_POINT('Ctrl Pts',(-42.0032346206984,46.7483190388774,
40.10025));
#205885=CARTESIAN_POINT('Ctrl Pts',(-41.9705316734061,46.8890030154868,
40.120244200104));
#205886=CARTESIAN_POINT('Ctrl Pts',(-41.9811230778539,46.831817406086,40.0633873868017));
#205887=CARTESIAN_POINT('Ctrl Pts',(-41.9515093836254,46.761203850955,40.0772271723537));
#205888=CARTESIAN_POINT('Ctrl Pts',(-41.8426461117365,46.906368706767,40.0045995998161));
#205889=CARTESIAN_POINT('Ctrl Pts',(-41.8933796070862,46.8290619651512,
39.9663485808314));
#205890=CARTESIAN_POINT('Ctrl Pts',(-41.8570065263032,46.7485125544803,
40.0101727202466));
#205891=CARTESIAN_POINT('Ctrl Pts',(-41.7917018131136,46.8896982576904,
39.930465434986));
#205892=CARTESIAN_POINT('Ctrl Pts',(-41.8649047103985,46.8032976561882,
39.9051900162957));
#205893=CARTESIAN_POINT('Ctrl Pts',(-41.8144193983037,46.7243152668227,
39.9671857458179));
#205894=CARTESIAN_POINT('Ctrl Pts',(-41.7612723673359,46.8559036426989,
39.8576902534424));
#205895=CARTESIAN_POINT('Ctrl Pts',(-41.8563683535926,46.7709043015506,
39.8573998014387));
#205896=CARTESIAN_POINT('Ctrl Pts',(-41.7839914803023,46.6905216402901,
39.92499));
#205897=CARTESIAN_POINT('Origin',(-42.0411527846891,46.7142062431426,40.22725));
#205898=CARTESIAN_POINT('Origin',(0.23594848208908,0.212448967518935,39.116));
#205899=CARTESIAN_POINT('Origin',(-39.9143573409153,44.8038810887678,39.116));
#205900=CARTESIAN_POINT('Origin',(8.0125006576031E-17,-1.22536847673101E-16,
40.22725));
#205901=CARTESIAN_POINT('Origin',(-42.0638038389696,46.6938111422608,40.22725));
#205902=CARTESIAN_POINT('Ctrl Pts',(-39.9143573409153,44.8038810887678,
38.989));
#205903=CARTESIAN_POINT('Ctrl Pts',(-40.0088781183431,44.7187741985016,
38.989));
#205904=CARTESIAN_POINT('Ctrl Pts',(-40.0087366280092,44.7189015969705,
39.116190109232));
#205905=CARTESIAN_POINT('Ctrl Pts',(-39.7693421853879,44.6424822887502,
38.989));
#205906=CARTESIAN_POINT('Ctrl Pts',(-39.863819608937,44.5576711710514,38.9892298989736));
#205907=CARTESIAN_POINT('Ctrl Pts',(-39.8926305794711,44.5899527660325,
39.11619004932));
#205908=CARTESIAN_POINT('Ctrl Pts',(-39.6312917695235,44.4888315723763,
39.1034966344368));
#205909=CARTESIAN_POINT('Ctrl Pts',(-39.7256919284545,44.4042655856146,
39.1038314102582));
#205910=CARTESIAN_POINT('Ctrl Pts',(-39.7820998051101,44.4671959043838,
39.2077528789599));
#205911=CARTESIAN_POINT('Ctrl Pts',(-39.5544469813067,44.4033023070493,
39.2875012672119));
#205912=CARTESIAN_POINT('Ctrl Pts',(-39.6488649704632,44.3189410144587,
39.2878045257868));
#205913=CARTESIAN_POINT('Ctrl Pts',(-39.7205730900529,44.3988635644383,
39.3549015295898));
#205914=CARTESIAN_POINT('Origin',(-39.6260861683714,44.483723516876,39.3548010137695));
#205915=CARTESIAN_POINT('Ctrl Pts',(-42.2339804752697,46.4302753505428,
39.8576902534424));
#205916=CARTESIAN_POINT('Ctrl Pts',(-42.1395065320995,46.5159655405278,
39.8573998014387));
#205917=CARTESIAN_POINT('Ctrl Pts',(-42.0671296588092,46.4355828792674,
39.92499));
#205918=CARTESIAN_POINT('Ctrl Pts',(-42.2644230274451,46.4640859592749,
39.9304984902493));
#205919=CARTESIAN_POINT('Ctrl Pts',(-42.1708479205184,46.5278479142039,
39.9052171569784));
#205920=CARTESIAN_POINT('Ctrl Pts',(-42.0975714415917,46.4693919041994,
39.9672049726596));
#205921=CARTESIAN_POINT('Ctrl Pts',(-42.2755508889257,46.5163638812299,
40.0043437678659));
#205922=CARTESIAN_POINT('Ctrl Pts',(-42.1933444849776,46.5588164356977,
39.966162857764));
#205923=CARTESIAN_POINT('Ctrl Pts',(-42.1170605480848,46.5141432491636,
40.0100243556234));
#205924=CARTESIAN_POINT('Ctrl Pts',(-42.2454039774543,46.6408663419438,
40.119487482199));
#205925=CARTESIAN_POINT('Ctrl Pts',(-42.187220455932,46.6457133039303,40.0627551483144));
#205926=CARTESIAN_POINT('Ctrl Pts',(-42.1199995355541,46.6088541045844,
40.0767884282378));
#205927=CARTESIAN_POINT('Ctrl Pts',(-42.2015749714289,46.7146600431958,
40.1599502015393));
#205928=CARTESIAN_POINT('Ctrl Pts',(-42.1587905896512,46.7029882531954,
40.1002449453881));
#205929=CARTESIAN_POINT('Ctrl Pts',(-42.1018187547561,46.6595535157382,
40.10025));
#205930=CARTESIAN_POINT('Ctrl Pts',(-42.1358900227691,46.7738319284261,
40.1599502534424));
#205931=CARTESIAN_POINT('Ctrl Pts',(-42.1109214781057,46.7461150696876,
40.10025));
#205932=CARTESIAN_POINT('Ctrl Pts',(-42.0638038389696,46.6938111422608,
40.10025));
#205933=CARTESIAN_POINT('Origin',(-42.1615090516448,46.3506032922598,39.92499));
#205934=CARTESIAN_POINT('Origin',(-39.5068809815375,44.3513327445023,39.6398955069331));
#205935=CARTESIAN_POINT('Origin',(-39.387675794557,44.2189419720526,39.92499));
#205936=CARTESIAN_POINT('Origin',(-42.0423040287649,46.2182127020538,39.6398955068266));
#205937=CARTESIAN_POINT('Origin',(-41.9230990057951,46.0858221116782,39.3548010137695));
#205938=CARTESIAN_POINT('Ctrl Pts',(-39.3160391863686,44.1385184650379,
39.8576902534424));
#205939=CARTESIAN_POINT('Ctrl Pts',(-39.4103156382728,44.0542875439844,
39.8579948730703));
#205940=CARTESIAN_POINT('Ctrl Pts',(-39.4820551873926,44.1339623850451,
39.92499));
#205941=CARTESIAN_POINT('Ctrl Pts',(-39.2856369388936,44.1047525536515,
39.9304020711232));
#205942=CARTESIAN_POINT('Ctrl Pts',(-39.3789425853219,44.0421527706803,
39.9058915297377));
#205943=CARTESIAN_POINT('Ctrl Pts',(-39.4516512848558,44.100195430388,39.9671523786027));
#205944=CARTESIAN_POINT('Ctrl Pts',(-39.2745942850996,44.0527517782423,
40.0043257306692));
#205945=CARTESIAN_POINT('Ctrl Pts',(-39.3566016867499,44.0110417363804,
39.9667894847835));
#205946=CARTESIAN_POINT('Ctrl Pts',(-39.43232853063,44.0556530121007,40.0100138975201));
#205947=CARTESIAN_POINT('Ctrl Pts',(-39.3050549810248,43.9290071509457,
40.1195533054858));
#205948=CARTESIAN_POINT('Ctrl Pts',(-39.3631024520333,43.9243964923859,
40.0630813209236));
#205949=CARTESIAN_POINT('Ctrl Pts',(-39.4299498468374,43.9614781338112,
40.0768265942419));
#205950=CARTESIAN_POINT('Ctrl Pts',(-39.3490583909335,43.8557442421763,
40.1599502027522));
#205951=CARTESIAN_POINT('Ctrl Pts',(-39.3917348424042,43.8675206320098,
40.1002552791541));
#205952=CARTESIAN_POINT('Ctrl Pts',(-39.4485000225464,43.9111340157069,
40.10025));
#205953=CARTESIAN_POINT('Ctrl Pts',(-39.4144401478986,43.796904759635,40.1599502534424));
#205954=CARTESIAN_POINT('Ctrl Pts',(-39.4393948122684,43.8246341160488,
40.10025));
#205955=CARTESIAN_POINT('Ctrl Pts',(-39.4864862581813,43.8769616275878,
40.10025));
#205956=CARTESIAN_POINT('Origin',(-39.4864862581813,43.8769616275878,40.22725));
#205957=CARTESIAN_POINT('Ctrl Pts',(-41.6348281284258,45.765664867611,38.989));
#205958=CARTESIAN_POINT('Ctrl Pts',(-41.5403077290107,45.8507714175129,
38.989));
#205959=CARTESIAN_POINT('Ctrl Pts',(-41.5404488407676,45.8506443599163,
39.1161896013267));
#205960=CARTESIAN_POINT('Ctrl Pts',(-41.7801793767997,45.9267609786653,
38.989));
#205961=CARTESIAN_POINT('Ctrl Pts',(-41.6856176794227,46.012155211749,38.988776927543));
#205962=CARTESIAN_POINT('Ctrl Pts',(-41.6565546403132,45.9795929135653,
39.1161898821824));
#205963=CARTESIAN_POINT('Ctrl Pts',(-41.9185498083232,46.0801233673967,
39.1034967087243));
#205964=CARTESIAN_POINT('Ctrl Pts',(-41.8239142817226,46.1657498592425,
39.1031720232716));
#205965=CARTESIAN_POINT('Ctrl Pts',(-41.7670853619614,46.1023497159518,
39.2077529615019));
#205966=CARTESIAN_POINT('Ctrl Pts',(-41.9955727382247,46.1654920697616,
39.2875012672119));
#205967=CARTESIAN_POINT('Ctrl Pts',(-41.9009568069087,46.2513146407507,
39.2872087095508));
#205968=CARTESIAN_POINT('Ctrl Pts',(-41.8286118967075,46.1706818552411,
39.3549017048228));
#205969=CARTESIAN_POINT('Origin',(-41.6348281284258,45.765664867611,39.116));
#205970=CARTESIAN_POINT('Origin',(3.72719664096538E-16,4.35908294926644E-17,
40.22725));
#205971=CARTESIAN_POINT('Origin',(-39.5091373124618,43.856566526706,40.22725));
#205972=CARTESIAN_POINT('Origin',(27.6232705441538,-31.1532462714324,39.116));
#205973=CARTESIAN_POINT('Origin',(-41.3663085755636,45.4673664422112,39.1160373285278));
#205974=CARTESIAN_POINT('Ctrl Pts',(-39.4370498736004,43.7765468711726,
40.1599502534424));
#205975=CARTESIAN_POINT('Ctrl Pts',(-39.4620188529806,43.8042633382933,
40.10025));
#205976=CARTESIAN_POINT('Ctrl Pts',(-39.5091373124618,43.856566526706,40.10025));
#205977=CARTESIAN_POINT('Ctrl Pts',(-39.5021785224862,43.7178744835423,
40.159950056604));
#205978=CARTESIAN_POINT('Ctrl Pts',(-39.5094654441321,43.761515733967,40.1002551305381));
#205979=CARTESIAN_POINT('Ctrl Pts',(-39.5469637653738,43.8224770900129,
40.10025));
#205980=CARTESIAN_POINT('Ctrl Pts',(-39.5788516269098,43.6818502604299,
40.1203070619047));
#205981=CARTESIAN_POINT('Ctrl Pts',(-39.5685043961838,43.7389249259234,
40.06370986845));
#205982=CARTESIAN_POINT('Ctrl Pts',(-39.5983821485328,43.8091917332947,
40.0772636213363));
#205983=CARTESIAN_POINT('Ctrl Pts',(-39.7059848156956,43.6640874258694,
40.0046102245801));
#205984=CARTESIAN_POINT('Ctrl Pts',(-39.6560168722787,43.7412697217741,
39.9670001894012));
#205985=CARTESIAN_POINT('Ctrl Pts',(-39.692386550076,43.8212571467119,40.0101788811208));
#205986=CARTESIAN_POINT('Ctrl Pts',(-39.7566878101776,43.6806424921203,
39.9303710930186));
#205987=CARTESIAN_POINT('Ctrl Pts',(-39.6846695243124,43.7668962219029,
39.9058663574106));
#205988=CARTESIAN_POINT('Ctrl Pts',(-39.7348023770063,43.8452710114195,
39.9671344706368));
#205989=CARTESIAN_POINT('Ctrl Pts',(-39.7870778846743,43.7143933160627,
39.8576902534424));
#205990=CARTESIAN_POINT('Ctrl Pts',(-39.6934538167797,43.7993487829616,
39.8579948730704));
#205991=CARTESIAN_POINT('Ctrl Pts',(-39.7651933658995,43.8790236240223,
39.92499));
#205992=CARTESIAN_POINT('Origin',(-39.8595727587351,43.7940440370148,39.92499));
#205993=CARTESIAN_POINT('Origin',(-41.3366772856866,45.434534810366,39.1925554488842));
#205994=CARTESIAN_POINT('Origin',(-41.2819167515325,45.3737170758076,39.3343017080178));
#205995=CARTESIAN_POINT('Origin',(-39.9787779456617,43.9264348094905,39.6398955069226));
#205996=CARTESIAN_POINT('Origin',(-40.0979831325495,44.0588255818381,39.3548010137695));
#205997=CARTESIAN_POINT('Ctrl Pts',(-41.06113033474,45.1285089182136,39.3978017080178));
#205998=CARTESIAN_POINT('Ctrl Pts',(-40.9667509419044,45.2134885052212,
39.3978017080178));
#205999=CARTESIAN_POINT('Ctrl Pts',(-40.9667509419044,45.2134885052212,
39.5248017080178));
#206000=CARTESIAN_POINT('Ctrl Pts',(-41.1211850608437,45.1955564429366,
39.3978017080178));
#206001=CARTESIAN_POINT('Ctrl Pts',(-41.0269231466371,45.28031650884,39.3980355775177));
#206002=CARTESIAN_POINT('Ctrl Pts',(-41.0570929845756,45.3138235084271,
39.5248015517192));
#206003=CARTESIAN_POINT('Ctrl Pts',(-41.1779726855659,45.2589537050075,
39.3484893995498));
#206004=CARTESIAN_POINT('Ctrl Pts',(-41.0841042944899,45.3438226072592,
39.3489438303425));
#206005=CARTESIAN_POINT('Ctrl Pts',(-41.1425178129608,45.4086973919089,
39.4508333155591));
#206006=CARTESIAN_POINT('Ctrl Pts',(-41.2079002115903,45.2923641298561,
39.2708017080178));
#206007=CARTESIAN_POINT('Ctrl Pts',(-41.1142722655002,45.3773275334109,
39.2710850691866));
#206008=CARTESIAN_POINT('Ctrl Pts',(-41.1875373586968,45.4586966628152,
39.3343017080178));
#206009=CARTESIAN_POINT('Origin',(-41.06113033474,45.1285089182136,39.5248017080178));
#206010=CARTESIAN_POINT('Ctrl Pts',(-40.0254908126584,43.9791725362586,
39.2875012672119));
#206011=CARTESIAN_POINT('Ctrl Pts',(-39.9317223035497,44.064255127713,39.2878045257519));
#206012=CARTESIAN_POINT('Ctrl Pts',(-40.0037114707672,44.1439246046464,
39.3549015218344));
#206013=CARTESIAN_POINT('Ctrl Pts',(-40.1025202360379,44.0645378932545,
39.1034938540228));
#206014=CARTESIAN_POINT('Ctrl Pts',(-40.0085500157897,44.1495813562492,
39.1038286278834));
#206015=CARTESIAN_POINT('Ctrl Pts',(-40.0652391174805,44.2122579788877,
39.2077506434036));
#206016=CARTESIAN_POINT('Ctrl Pts',(-40.2409001323909,44.2178941385634,
38.989));
#206017=CARTESIAN_POINT('Ctrl Pts',(-40.1466780419426,44.3029888158449,
38.9892298954605));
#206018=CARTESIAN_POINT('Ctrl Pts',(-40.1757707681144,44.3350158129969,
39.1161900347283));
#206019=CARTESIAN_POINT('Ctrl Pts',(-40.3862543050934,44.3789831537299,
38.989));
#206020=CARTESIAN_POINT('Ctrl Pts',(-40.2917335385825,44.4640900341665,
38.989));
#206021=CARTESIAN_POINT('Ctrl Pts',(-40.2918750179832,44.4639626455419,
39.116190094564));
#206022=CARTESIAN_POINT('Origin',(-40.3862543050934,44.3789831537299,39.116));
#206023=CARTESIAN_POINT('Origin',(26.9484406282047,-30.4037717213982,39.5248017080178));
#206024=CARTESIAN_POINT('Origin',(-40.9599523566121,45.0161393894797,39.5248017080178));
#206025=CARTESIAN_POINT('Origin',(26.8427652369004,-30.2864073093061,39.116));
#206026=CARTESIAN_POINT('Origin',(-40.6548553974679,44.6772189625514,39.1160402713853));
#206027=CARTESIAN_POINT('Ctrl Pts',(-40.8131880745603,44.8522789915945,
39.2708017080178));
#206028=CARTESIAN_POINT('Ctrl Pts',(-40.7187157882333,44.9380175594366,
39.27051194648));
#206029=CARTESIAN_POINT('Ctrl Pts',(-40.6447864996549,44.8559107663289,
39.3343017080178));
#206030=CARTESIAN_POINT('Ctrl Pts',(-40.8432146576646,44.8858042435429,
39.3487519301185));
#206031=CARTESIAN_POINT('Ctrl Pts',(-40.748670873839,44.9712860523926,39.3482879463985));
#206032=CARTESIAN_POINT('Ctrl Pts',(-40.6899581892264,44.906079010083,39.4512271261639));
#206033=CARTESIAN_POINT('Ctrl Pts',(-40.9001003367641,44.9493173051408,
39.3978017080178));
#206034=CARTESIAN_POINT('Ctrl Pts',(-40.8054891887044,45.0343891839552,
39.3975673827397));
#206035=CARTESIAN_POINT('Ctrl Pts',(-40.7755352187359,45.0011219300382,
39.5248015355181));
#206036=CARTESIAN_POINT('Ctrl Pts',(-40.9599523566121,45.0161393894797,
39.3978017080178));
#206037=CARTESIAN_POINT('Ctrl Pts',(-40.8655729637765,45.1011189764872,
39.3978017080178));
#206038=CARTESIAN_POINT('Ctrl Pts',(-40.8655729637765,45.1011189764872,
39.5248017080178));
#206039=CARTESIAN_POINT('Origin',(-40.7391658924905,44.7709311793213,39.3343017080178));
#206040=CARTESIAN_POINT('Origin',(-40.6847319392783,44.7104761492014,39.1934008533554));
#206041=CARTESIAN_POINT('Origin',(-35.8473027488275,49.8797426639498,39.1925554495083));
#206042=CARTESIAN_POINT('Origin',(-35.8732562382978,49.9155525184337,39.1160373285282));
#206043=CARTESIAN_POINT('Origin',(-35.7991993820658,49.8135340601226,39.3343017080178));
#206044=CARTESIAN_POINT('Ctrl Pts',(-35.7350130971385,49.7242207306178,
39.2708017080178));
#206045=CARTESIAN_POINT('Ctrl Pts',(-35.8375861910552,49.6503036646788,
39.2710850691866));
#206046=CARTESIAN_POINT('Ctrl Pts',(-35.9019445403514,49.7388853330815,
39.3343017080178));
#206047=CARTESIAN_POINT('Ctrl Pts',(-35.7084656432366,49.6878783768789,
39.3487519293518));
#206048=CARTESIAN_POINT('Ctrl Pts',(-35.8109961808828,49.6137056554138,
39.3492068662929));
#206049=CARTESIAN_POINT('Ctrl Pts',(-35.8622643302213,49.6842702092578,
39.4512271248737));
#206050=CARTESIAN_POINT('Ctrl Pts',(-35.6581711379707,49.6190282456271,
39.3978017080178));
#206051=CARTESIAN_POINT('Ctrl Pts',(-35.7606778378473,49.5444483977908,
39.3980347781164));
#206052=CARTESIAN_POINT('Ctrl Pts',(-35.7870908094924,49.5808027344285,
39.5248015355176));
#206053=CARTESIAN_POINT('Ctrl Pts',(-35.6052536882598,49.5465907136148,
39.3978017080178));
#206054=CARTESIAN_POINT('Ctrl Pts',(-35.7079988465454,49.4719419865736,
39.3978017080178));
#206055=CARTESIAN_POINT('Ctrl Pts',(-35.7079988465454,49.4719419865736,
39.5248017080178));
#206056=CARTESIAN_POINT('Origin',(-35.6052536882598,49.5465907136148,39.5248017080178));
#206057=CARTESIAN_POINT('Origin',(0.256862895714053,0.186621817602858,39.116));
#206058=CARTESIAN_POINT('Origin',(-36.1092077731524,50.2402240048086,39.116));
#206059=CARTESIAN_POINT('Origin',(0.256862895714053,0.186621817602858,39.5248017080178));
#206060=CARTESIAN_POINT('Origin',(-35.5163757878391,49.4242607783464,39.5248017080178));
#206061=CARTESIAN_POINT('Ctrl Pts',(-36.4252947698674,50.6762142289951,
39.2875012672119));
#206062=CARTESIAN_POINT('Ctrl Pts',(-36.5289136610809,50.601509405082,39.287208709576));
#206063=CARTESIAN_POINT('Ctrl Pts',(-36.4650842624219,50.513980907036,39.3549016990121));
#206064=CARTESIAN_POINT('Ctrl Pts',(-36.3578045222537,50.5831238715089,
39.103493917393));
#206065=CARTESIAN_POINT('Ctrl Pts',(-36.4612356912194,50.5083591136189,
39.1031692336376));
#206066=CARTESIAN_POINT('Ctrl Pts',(-36.4110366091576,50.4395906940187,
39.2077507202321));
#206067=CARTESIAN_POINT('Ctrl Pts',(-36.2365613423287,50.4158900112692,
38.989));
#206068=CARTESIAN_POINT('Ctrl Pts',(-36.3397499727032,50.3411491755218,
38.9887769311134));
#206069=CARTESIAN_POINT('Ctrl Pts',(-36.3139421975398,50.3059517008917,
39.1161898712888));
#206070=CARTESIAN_POINT('Ctrl Pts',(-36.1092077731524,50.2402240048086,
38.989));
#206071=CARTESIAN_POINT('Ctrl Pts',(-36.2121064279397,50.1654637560311,
38.989));
#206072=CARTESIAN_POINT('Ctrl Pts',(-36.2119528169509,50.1655753609473,
39.1161895903851));
#206073=CARTESIAN_POINT('Origin',(-36.3624339277669,50.5887599058104,39.3548010137695));
#206074=CARTESIAN_POINT('Ctrl Pts',(-35.5163757878391,49.4242607783464,
39.3978017080178));
#206075=CARTESIAN_POINT('Ctrl Pts',(-35.6191209461248,49.3496120513052,
39.3978017080178));
#206076=CARTESIAN_POINT('Ctrl Pts',(-35.6191209461248,49.3496120513052,
39.5248017080178));
#206077=CARTESIAN_POINT('Ctrl Pts',(-35.4632790141033,49.3515787599201,
39.3978017080178));
#206078=CARTESIAN_POINT('Ctrl Pts',(-35.5661632154413,49.276721988248,39.3975666025022));
#206079=CARTESIAN_POINT('Ctrl Pts',(-35.5397616632048,49.2403833690727,
39.5248015517178));
#206080=CARTESIAN_POINT('Ctrl Pts',(-35.4130704930569,49.2828534857288,
39.3484894016717));
#206081=CARTESIAN_POINT('Ctrl Pts',(-35.5163418450511,49.2081487547859,
39.3480259000055));
#206082=CARTESIAN_POINT('Ctrl Pts',(-35.464721803166,49.1370998624006,39.4508333188956));
#206083=CARTESIAN_POINT('Ctrl Pts',(-35.3866101428255,49.2466351556016,
39.2708017080178));
#206084=CARTESIAN_POINT('Ctrl Pts',(-35.4901170100363,49.1720533660034,
39.2705119464801));
#206085=CARTESIAN_POINT('Ctrl Pts',(-35.4251752107434,49.0826686475738,
39.3343017080178));
#206086=CARTESIAN_POINT('Origin',(-35.3224300524577,49.1573173746149,39.3343017080178));
#206087=CARTESIAN_POINT('Origin',(-36.4671473482338,50.7328855645276,39.6398955068173));
#206088=CARTESIAN_POINT('Origin',(-36.5718607685317,50.8770112231006,39.92499));
#206089=CARTESIAN_POINT('Origin',(-35.2746135646439,49.0915036252753,39.1934008539938));
#206090=CARTESIAN_POINT('Origin',(-35.2482948100384,49.055365400753,39.1160402713854));
#206091=CARTESIAN_POINT('Ctrl Pts',(-36.9911673391703,50.9399462128205,
40.1599502534424));
#206092=CARTESIAN_POINT('Ctrl Pts',(-36.9692474126336,50.9097606317997,
40.10025));
#206093=CARTESIAN_POINT('Ctrl Pts',(-36.9278827595322,50.8527980281388,
40.10025));
#206094=CARTESIAN_POINT('Ctrl Pts',(-36.9198678602466,50.991721750496,40.1599500538463));
#206095=CARTESIAN_POINT('Ctrl Pts',(-36.9173100216895,50.9474721267403,
40.100244835349));
#206096=CARTESIAN_POINT('Ctrl Pts',(-36.8866065570935,50.8827604229949,
40.10025));
#206097=CARTESIAN_POINT('Ctrl Pts',(-36.8393772800889,51.0192553292381,
40.1202442001041));
#206098=CARTESIAN_POINT('Ctrl Pts',(-36.8558881875866,50.9634900918193,
40.0633873868015));
#206099=CARTESIAN_POINT('Ctrl Pts',(-36.8338178466773,50.8901678911828,
40.0772271723539));
#206100=CARTESIAN_POINT('Ctrl Pts',(-36.7103770798836,51.0231582082091,
40.004599599816));
#206101=CARTESIAN_POINT('Ctrl Pts',(-36.7689134067389,50.9515780553181,
39.9663485808318));
#206102=CARTESIAN_POINT('Ctrl Pts',(-36.7411592876127,50.8676678805079,
40.0101727202465));
#206103=CARTESIAN_POINT('Ctrl Pts',(-36.6614543958819,51.0012539523503,
39.9304654349861));
#206104=CARTESIAN_POINT('Ctrl Pts',(-36.7432876021362,50.9229784487436,
39.9051900162947));
#206105=CARTESIAN_POINT('Ctrl Pts',(-36.7013347616503,50.8391515810788,
39.9671857458184));
#206106=CARTESIAN_POINT('Ctrl Pts',(-36.634724144965,50.9644637245896,39.8576902534424));
#206107=CARTESIAN_POINT('Ctrl Pts',(-36.738184035968,50.8898702560321,39.8573998014387));
#206108=CARTESIAN_POINT('Ctrl Pts',(-36.6746059268174,50.8023624960594,
39.92499));
#206109=CARTESIAN_POINT('Origin',(-36.9278827595322,50.8527980281388,40.22725));
#206110=CARTESIAN_POINT('Origin',(0.256862895714053,0.186621817602858,39.116));
#206111=CARTESIAN_POINT('Origin',(-35.0124214764581,48.7306271754179,39.116));
#206112=CARTESIAN_POINT('Origin',(6.67120042669018E-17,-1.33398482780243E-16,
40.22725));
#206113=CARTESIAN_POINT('Origin',(-36.9525415975208,50.8348823336489,40.22725));
#206114=CARTESIAN_POINT('Ctrl Pts',(-35.0124214764581,48.7306271754179,
38.989));
#206115=CARTESIAN_POINT('Ctrl Pts',(-35.1153205516305,48.6558666212127,
38.989));
#206116=CARTESIAN_POINT('Ctrl Pts',(-35.115166519629,48.6559785320125,39.1161901092323));
#206117=CARTESIAN_POINT('Ctrl Pts',(-34.8850714976646,48.5549543235566,
38.989));
#206118=CARTESIAN_POINT('Ctrl Pts',(-34.9878965398059,48.4804833899298,
38.9892298989718));
#206119=CARTESIAN_POINT('Ctrl Pts',(-35.0131753353115,48.515599709433,39.1161900493185));
#206120=CARTESIAN_POINT('Ctrl Pts',(-34.7638382096882,48.3877151240579,
39.1034966344368));
#206121=CARTESIAN_POINT('Ctrl Pts',(-34.8665607873115,48.3134799021656,
39.1038314102594));
#206122=CARTESIAN_POINT('Ctrl Pts',(-34.916081646201,48.3819617107287,39.2077528789615));
#206123=CARTESIAN_POINT('Ctrl Pts',(-34.6963546279281,48.2946219293749,
39.2875012672119));
#206124=CARTESIAN_POINT('Ctrl Pts',(-34.7990735417349,48.2205921440832,
39.2878045257868));
#206125=CARTESIAN_POINT('Ctrl Pts',(-34.8620346554126,48.3075724095165,
39.35490152959));
#206126=CARTESIAN_POINT('Origin',(-34.759195062553,48.3820909175332,39.3548010137695));
#206127=CARTESIAN_POINT('Ctrl Pts',(-37.1493329797256,50.5905785208487,
39.8576902534424));
#206128=CARTESIAN_POINT('Ctrl Pts',(-37.0464195108248,50.6659240749087,
39.8573998014387));
#206129=CARTESIAN_POINT('Ctrl Pts',(-36.9828414016742,50.578416314936,39.92499));
#206130=CARTESIAN_POINT('Ctrl Pts',(-37.1760745934428,50.6273860247245,
39.930498490249));
#206131=CARTESIAN_POINT('Ctrl Pts',(-37.0763471615787,50.6810174228644,
39.905217156979));
#206132=CARTESIAN_POINT('Ctrl Pts',(-37.0095824157651,50.6152221632658,
39.9672049726596));
#206133=CARTESIAN_POINT('Ctrl Pts',(-37.1816769644883,50.6805407410144,
40.0043437678663));
#206134=CARTESIAN_POINT('Ctrl Pts',(-37.0954833955414,50.7141678268705,
39.9661628577642));
#206135=CARTESIAN_POINT('Ctrl Pts',(-37.0242869695743,50.661765522031,40.0100243556237));
#206136=CARTESIAN_POINT('Ctrl Pts',(-37.1386811500609,50.8012099538924,
40.1194874821986));
#206137=CARTESIAN_POINT('Ctrl Pts',(-37.08030971847,50.7999485296225,40.062755148314));
#206138=CARTESIAN_POINT('Ctrl Pts',(-37.0173098767922,50.7562647493209,
40.0767884282375));
#206139=CARTESIAN_POINT('Ctrl Pts',(-37.0873787017255,50.8700180268819,
40.1599502015394));
#206140=CARTESIAN_POINT('Ctrl Pts',(-37.0460487315402,50.8539379904895,
40.1002449453872));
#206141=CARTESIAN_POINT('Ctrl Pts',(-36.9939291606758,50.8047860147164,
40.10025));
#206142=CARTESIAN_POINT('Ctrl Pts',(-37.0158684358555,50.9219998155903,
40.1599502534424));
#206143=CARTESIAN_POINT('Ctrl Pts',(-36.9939338721428,50.8918248691003,
40.10025));
#206144=CARTESIAN_POINT('Ctrl Pts',(-36.9525415975208,50.8348823336489,
40.10025));
#206145=CARTESIAN_POINT('Origin',(-37.0855865599598,50.5037675878948,39.92499));
#206146=CARTESIAN_POINT('Origin',(-34.6544814981902,48.2379650606699,39.6398955069325));
#206147=CARTESIAN_POINT('Origin',(-34.5497679336937,48.0938392037151,39.92499));
#206148=CARTESIAN_POINT('Origin',(-36.980873139614,50.3596419293373,39.6398955068271));
#206149=CARTESIAN_POINT('Origin',(-36.876159719195,50.2155162706047,39.3548010137695));
#206150=CARTESIAN_POINT('Ctrl Pts',(-34.4869303039392,48.006368200519,39.8576902534424));
#206151=CARTESIAN_POINT('Ctrl Pts',(-34.5894948283129,47.9324532779041,
39.8579948730703));
#206152=CARTESIAN_POINT('Ctrl Pts',(-34.6525130919793,48.0191904766739,
39.92499));
#206153=CARTESIAN_POINT('Ctrl Pts',(-34.4602241019849,47.9696093621198,
39.930402071123));
#206154=CARTESIAN_POINT('Ctrl Pts',(-34.559562069435,47.9171056031468,39.9058915297386));
#206155=CARTESIAN_POINT('Ctrl Pts',(-34.6258053530817,47.9824304277186,
39.9671523786034));
#206156=CARTESIAN_POINT('Ctrl Pts',(-34.4546775021463,47.9167391807674,
40.0043257306694));
#206157=CARTESIAN_POINT('Ctrl Pts',(-34.5405955452481,47.8838297385506,
39.9667894847838));
#206158=CARTESIAN_POINT('Ctrl Pts',(-34.6112444014586,47.9361122396534,
40.01001389752));
#206159=CARTESIAN_POINT('Ctrl Pts',(-34.4979061669207,47.7968564492224,
40.1195533054857));
#206160=CARTESIAN_POINT('Ctrl Pts',(-34.5561175928638,47.7983386612732,
40.0630813209234));
#206161=CARTESIAN_POINT('Ctrl Pts',(-34.6187227036509,47.8422046210393,
40.076826594242));
#206162=CARTESIAN_POINT('Ctrl Pts',(-34.5493265808147,47.7285944911493,
40.1599502027511));
#206163=CARTESIAN_POINT('Ctrl Pts',(-34.5905382782876,47.7447672725789,
40.1002552791554));
#206164=CARTESIAN_POINT('Ctrl Pts',(-34.6424336528575,47.7940753146434,
40.10025));
#206165=CARTESIAN_POINT('Ctrl Pts',(-34.620500570363,47.6769115920307,40.1599502534424));
#206166=CARTESIAN_POINT('Ctrl Pts',(-34.642420023457,47.7070975168467,40.10025));
#206167=CARTESIAN_POINT('Ctrl Pts',(-34.6837837831342,47.7640607692766,
40.10025));
#206168=CARTESIAN_POINT('Origin',(-34.6837837831342,47.7640607692766,40.22725));
#206169=CARTESIAN_POINT('Ctrl Pts',(-36.6229335645805,49.8669803696029,
38.989));
#206170=CARTESIAN_POINT('Ctrl Pts',(-36.5200349009277,49.9417406248216,
38.989));
#206171=CARTESIAN_POINT('Ctrl Pts',(-36.5201885207953,49.9416290134547,
39.1161896013271));
#206172=CARTESIAN_POINT('Ctrl Pts',(-36.7506494346786,50.042387321933,38.989));
#206173=CARTESIAN_POINT('Ctrl Pts',(-36.6476796282208,50.1174293675617,
38.9887769275442));
#206174=CARTESIAN_POINT('Ctrl Pts',(-36.6221794864683,50.0820075342366,
39.1161898821828));
#206175=CARTESIAN_POINT('Ctrl Pts',(-36.8722311236856,50.2093732240195,
39.1034967087243));
#206176=CARTESIAN_POINT('Ctrl Pts',(-36.7691636147928,50.284638538816,39.1031720232712));
#206177=CARTESIAN_POINT('Ctrl Pts',(-36.7192731293507,50.2156454684951,
39.2077529615018));
#206178=CARTESIAN_POINT('Ctrl Pts',(-36.9399086546482,50.3023253561999,
39.2875012672119));
#206179=CARTESIAN_POINT('Ctrl Pts',(-36.8368401378443,50.3777877242645,
39.2872087095508));
#206180=CARTESIAN_POINT('Ctrl Pts',(-36.7733199617892,50.2900345513016,
39.354901704823));
#206181=CARTESIAN_POINT('Origin',(-36.6229335645805,49.8669803696029,39.116));
#206182=CARTESIAN_POINT('Origin',(3.77491158612227E-16,4.74547095659469E-17,
40.22725));
#206183=CARTESIAN_POINT('Origin',(-34.7084426211227,47.7461450747867,40.22725));
#206184=CARTESIAN_POINT('Origin',(21.2404668433927,-29.7751578089172,39.116));
#206185=CARTESIAN_POINT('Origin',(-36.3870656659264,49.5422481179711,39.116037328528));
#206186=CARTESIAN_POINT('Ctrl Pts',(-34.6451144164181,47.6590285860939,
40.1599502534424));
#206187=CARTESIAN_POINT('Ctrl Pts',(-34.6670494534013,47.6892031885516,
40.10025));
#206188=CARTESIAN_POINT('Ctrl Pts',(-34.7084426211227,47.7461450747867,
40.10025));
#206189=CARTESIAN_POINT('Ctrl Pts',(-34.7160192182661,47.6074854095251,
40.1599500566034));
#206190=CARTESIAN_POINT('Ctrl Pts',(-34.7187044685518,47.6516492793364,
40.1002551305369));
#206191=CARTESIAN_POINT('Ctrl Pts',(-34.7496251732003,47.7161963245905,
40.10025));
#206192=CARTESIAN_POINT('Ctrl Pts',(-34.7960378560837,47.5796730526554,
40.1203070619043));
#206193=CARTESIAN_POINT('Ctrl Pts',(-34.7797813814947,47.6353534770327,
40.0637098684494));
#206194=CARTESIAN_POINT('Ctrl Pts',(-34.802150578997,47.7083584310198,40.0772636213361));
#206195=CARTESIAN_POINT('Ctrl Pts',(-34.9243313177586,47.5752965616149,
40.0046102245805));
#206196=CARTESIAN_POINT('Ctrl Pts',(-34.8665693571816,47.6468329724888,
39.9670001894019));
#206197=CARTESIAN_POINT('Ctrl Pts',(-34.894378835469,47.7301838844735,40.0101788811211));
#206198=CARTESIAN_POINT('Ctrl Pts',(-34.9730260802977,47.5970608435772,
39.9303710930184));
#206199=CARTESIAN_POINT('Ctrl Pts',(-34.8923863483135,47.6753141056551,
39.9058663574106));
#206200=CARTESIAN_POINT('Ctrl Pts',(-34.934052171687,47.7584998599255,39.9671344706371));
#206201=CARTESIAN_POINT('Ctrl Pts',(-34.9997217530256,47.6338034047603,
39.8576902534424));
#206202=CARTESIAN_POINT('Ctrl Pts',(-34.8977303031698,47.7085070967806,
39.8579948730703));
#206203=CARTESIAN_POINT('Ctrl Pts',(-34.9607485668361,47.7952442955505,
39.92499));
#206204=CARTESIAN_POINT('Origin',(-35.0634937251217,47.7205955685094,39.92499));
#206205=CARTESIAN_POINT('Origin',(-36.3610285393802,49.5064990280449,39.1925554488846));
#206206=CARTESIAN_POINT('Origin',(-36.3129251734939,49.4402904249169,39.3343017080178));
#206207=CARTESIAN_POINT('Origin',(-35.1682072895617,47.8647214254821,39.6398955069207));
#206208=CARTESIAN_POINT('Origin',(-35.2729208539811,48.0088472823275,39.3548010137695));
#206209=CARTESIAN_POINT('Ctrl Pts',(-36.1189794796879,49.1733470784091,
39.3978017080178));
#206210=CARTESIAN_POINT('Ctrl Pts',(-36.0162343214022,49.2479958054502,
39.3978017080178));
#206211=CARTESIAN_POINT('Ctrl Pts',(-36.0162343214022,49.2479958054502,
39.5248017080178));
#206212=CARTESIAN_POINT('Ctrl Pts',(-36.1716968449934,49.2463047380077,
39.3978017080178));
#206213=CARTESIAN_POINT('Ctrl Pts',(-36.0690914679777,49.3207474263656,
39.3980355775191));
#206214=CARTESIAN_POINT('Ctrl Pts',(-36.0955935972134,49.3572244778984,
39.5248015517192));
#206215=CARTESIAN_POINT('Ctrl Pts',(-36.2215465627857,49.3152906263886,
39.3484893995498));
#206216=CARTESIAN_POINT('Ctrl Pts',(-36.1193211766481,49.3898826892451,
39.3489438303418));
#206217=CARTESIAN_POINT('Ctrl Pts',(-36.1706334382073,49.4605079583574,
39.4508333155594));
#206218=CARTESIAN_POINT('Ctrl Pts',(-36.2478178023246,49.3516463037388,
39.2708017080178));
#206219=CARTESIAN_POINT('Ctrl Pts',(-36.1458216659121,49.4263574835554,
39.2710850691866));
#206220=CARTESIAN_POINT('Ctrl Pts',(-36.2101800152082,49.514939151958,39.3343017080178));
#206221=CARTESIAN_POINT('Origin',(-36.1189794796879,49.1733470784091,39.5248017080178));
#206222=CARTESIAN_POINT('Ctrl Pts',(-35.2091516650524,47.922053073669,39.2875012672119));
#206223=CARTESIAN_POINT('Ctrl Pts',(-35.1070032771116,47.9968680956254,
39.2878045257519));
#206224=CARTESIAN_POINT('Ctrl Pts',(-35.1702703521464,48.0836260518495,
39.3549015218347));
#206225=CARTESIAN_POINT('Ctrl Pts',(-35.2768360036062,48.0150025575607,
39.1034938540228));
#206226=CARTESIAN_POINT('Ctrl Pts',(-35.1744910995566,48.0897575808481,
39.1038286278809));
#206227=CARTESIAN_POINT('Ctrl Pts',(-35.2243181613712,48.1580164790724,
39.2077506434028));
#206228=CARTESIAN_POINT('Ctrl Pts',(-35.398427747753,48.181983339225,38.989));
#206229=CARTESIAN_POINT('Ctrl Pts',(-35.2958269999255,48.2567629686449,
38.9892298954624));
#206230=CARTESIAN_POINT('Ctrl Pts',(-35.3214126203088,48.2916555365114,
39.1161900347289));
#206231=CARTESIAN_POINT('Ctrl Pts',(-35.5261472678861,48.3573835402122,
38.989));
#206232=CARTESIAN_POINT('Ctrl Pts',(-35.4232482045979,48.432144085783,38.989));
#206233=CARTESIAN_POINT('Ctrl Pts',(-35.4234022246974,48.4320321836306,
39.1161900945646));
#206234=CARTESIAN_POINT('Origin',(-35.5261472678861,48.3573835402122,39.116));
#206235=CARTESIAN_POINT('Origin',(20.7197400704237,-29.0584388930974,39.5248017080178));
#206236=CARTESIAN_POINT('Origin',(-36.0301015792672,49.0510171431407,39.5248017080178));
#206237=CARTESIAN_POINT('Origin',(20.6381965522785,-28.9462038689907,39.116));
#206238=CARTESIAN_POINT('Origin',(-35.7621028045848,48.6820620414861,39.1160402713851));
#206239=CARTESIAN_POINT('Ctrl Pts',(-35.90126936289,48.8727133447947,39.2708017080178));
#206240=CARTESIAN_POINT('Ctrl Pts',(-35.7983524848931,48.94810718488,39.27051194648));
#206241=CARTESIAN_POINT('Ctrl Pts',(-35.7334106856002,48.8587224664504,
39.3343017080178));
#206242=CARTESIAN_POINT('Ctrl Pts',(-35.9276271141638,48.909193574494,39.3487519301185));
#206243=CARTESIAN_POINT('Ctrl Pts',(-35.8246659689621,48.9843245886183,
39.3482879463976));
#206244=CARTESIAN_POINT('Ctrl Pts',(-35.7730909105055,48.9133376106103,
39.4512271261638));
#206245=CARTESIAN_POINT('Ctrl Pts',(-35.9775622448353,48.978304877513,39.3978017080178));
#206246=CARTESIAN_POINT('Ctrl Pts',(-35.8745769537837,49.0530211657577,
39.3975673827401));
#206247=CARTESIAN_POINT('Ctrl Pts',(-35.8482644497257,49.0168051108908,
39.5248015355181));
#206248=CARTESIAN_POINT('Ctrl Pts',(-36.0301015792672,49.0510171431407,
39.3978017080178));
#206249=CARTESIAN_POINT('Ctrl Pts',(-35.9273564209816,49.1256658701818,
39.3978017080178));
#206250=CARTESIAN_POINT('Ctrl Pts',(-35.9273564209816,49.1256658701818,
39.5248017080178));
#206251=CARTESIAN_POINT('Origin',(-35.8361558438858,48.7840737394092,39.3343017080178));
#206252=CARTESIAN_POINT('Origin',(-35.7883393569606,48.7182599907915,39.193400853355));
#206253=CARTESIAN_POINT('Origin',(-30.437074624756,53.3535596832575,39.192555449508));
#206254=CARTESIAN_POINT('Origin',(-30.4591427892374,53.3918862459807,39.1160373285255));
#206255=CARTESIAN_POINT('Origin',(-30.3961554568832,53.2826856060848,39.3343017080178));
#206256=CARTESIAN_POINT('Ctrl Pts',(-30.3416565762231,53.1871522506178,
39.2708017080178));
#206257=CARTESIAN_POINT('Ctrl Pts',(-30.4513942013108,53.1243619179798,
39.2710850691867));
#206258=CARTESIAN_POINT('Ctrl Pts',(-30.5061406831638,53.2191856060848,
39.3343017080178));
#206259=CARTESIAN_POINT('Ctrl Pts',(-30.3190533624385,53.1482340195356,
39.3487519293518));
#206260=CARTESIAN_POINT('Ctrl Pts',(-30.4287753876661,53.0851849835386,
39.3492068662939));
#206261=CARTESIAN_POINT('Ctrl Pts',(-30.4723866803431,53.1607219582405,
39.4512271248748));
#206262=CARTESIAN_POINT('Ctrl Pts',(-30.2762311741509,53.0745038491602,
39.3978017080178));
#206263=CARTESIAN_POINT('Ctrl Pts',(-30.3859720484835,53.0110474253453,
39.398034778116));
#206264=CARTESIAN_POINT('Ctrl Pts',(-30.4084402641648,53.0499635164578,
39.5248015355176));
#206265=CARTESIAN_POINT('Ctrl Pts',(-30.2311753956707,52.996931757829,39.3978017080178));
#206266=CARTESIAN_POINT('Ctrl Pts',(-30.3411606219514,52.933431757829,39.3978017080178));
#206267=CARTESIAN_POINT('Ctrl Pts',(-30.3411606219514,52.933431757829,39.5248017080178));
#206268=CARTESIAN_POINT('Origin',(-30.2311753956707,52.996931757829,39.5248017080178));
#206269=CARTESIAN_POINT('Origin',(0.274963065701566,0.158749999999997,39.116));
#206270=CARTESIAN_POINT('Origin',(-30.659864345357,53.7394427993289,39.116));
#206271=CARTESIAN_POINT('Origin',(0.274963065701566,0.158749999999997,39.5248017080178));
#206272=CARTESIAN_POINT('Origin',(-30.1555713378333,52.8659816883962,39.5248017080178));
#206273=CARTESIAN_POINT('Ctrl Pts',(-30.9286463962973,54.2060847114744,
39.2875012672119));
#206274=CARTESIAN_POINT('Ctrl Pts',(-31.039506432826,54.1426202518668,39.287208709576));
#206275=CARTESIAN_POINT('Ctrl Pts',(-30.9851759176831,54.048899255138,39.3549016990126));
#206276=CARTESIAN_POINT('Ctrl Pts',(-30.8712564593345,54.1064496608383,
39.1034939173931));
#206277=CARTESIAN_POINT('Ctrl Pts',(-30.9819360667873,54.0429059732653,
39.1031692336345));
#206278=CARTESIAN_POINT('Ctrl Pts',(-30.9392002377703,53.9692670413573,
39.2077507202313));
#206279=CARTESIAN_POINT('Ctrl Pts',(-30.7681581606534,53.9274585619029,
38.989));
#206280=CARTESIAN_POINT('Ctrl Pts',(-30.8785940576184,53.8639133132283,
38.9887769311152));
#206281=CARTESIAN_POINT('Ctrl Pts',(-30.8566067980778,53.8262110069709,
39.1161898712897));
#206282=CARTESIAN_POINT('Ctrl Pts',(-30.659864345357,53.7394427993289,38.989));
#206283=CARTESIAN_POINT('Ctrl Pts',(-30.7700138844659,53.6758479332733,
38.989));
#206284=CARTESIAN_POINT('Ctrl Pts',(-30.769849449083,53.6759428700859,39.116189590386));
#206285=CARTESIAN_POINT('Origin',(-30.8752713784757,54.1125387249982,39.3548010137695));
#206286=CARTESIAN_POINT('Ctrl Pts',(-30.1555713378333,52.8659816883962,
39.3978017080178));
#206287=CARTESIAN_POINT('Ctrl Pts',(-30.2655565641139,52.8024816883962,
39.3978017080178));
#206288=CARTESIAN_POINT('Ctrl Pts',(-30.2655565641139,52.8024816883962,
39.5248017080178));
#206289=CARTESIAN_POINT('Ctrl Pts',(-30.1103627734739,52.7881477055079,
39.3978017080178));
#206290=CARTESIAN_POINT('Ctrl Pts',(-30.2205080276998,52.7244553345187,
39.3975666025021));
#206291=CARTESIAN_POINT('Ctrl Pts',(-30.1980495259467,52.685556068422,39.5248015517178));
#206292=CARTESIAN_POINT('Ctrl Pts',(-30.0676130472578,52.7145506960118,
39.3484894016716));
#206293=CARTESIAN_POINT('Ctrl Pts',(-30.1781274387052,52.6510500011318,
39.3480259000039));
#206294=CARTESIAN_POINT('Ctrl Pts',(-30.1342168083487,52.5749945583572,
39.4508333188949));
#206295=CARTESIAN_POINT('Ctrl Pts',(-30.0450834959832,52.6757649139399,
39.2708017080178));
#206296=CARTESIAN_POINT('Ctrl Pts',(-30.1558192615997,52.6124111049559,
39.27051194648));
#206297=CARTESIAN_POINT('Ctrl Pts',(-30.1005764675353,52.5167277788844,
39.3343017080178));
#206298=CARTESIAN_POINT('Origin',(-29.9905912412547,52.5802277788844,39.3343017080178));
#206299=CARTESIAN_POINT('Origin',(-30.9643459342459,54.2668203812029,39.6398955068166));
#206300=CARTESIAN_POINT('Origin',(-31.0534204898629,54.4211020372441,39.92499));
#206301=CARTESIAN_POINT('Origin',(-29.9499161072434,52.5097763801591,39.1934008539945));
#206302=CARTESIAN_POINT('Origin',(-29.9275190026058,52.4710850656386,39.1160402713848));
#206303=CARTESIAN_POINT('Ctrl Pts',(-31.4638515574735,54.5275217339722,
40.1599502534424));
#206304=CARTESIAN_POINT('Ctrl Pts',(-31.4452069629848,54.4952102564868,
40.10025));
#206305=CARTESIAN_POINT('Ctrl Pts',(-31.4100231232056,54.4342359163066,
40.10025));
#206306=CARTESIAN_POINT('Ctrl Pts',(-31.3875306471679,54.5715608148717,
40.1599500538472));
#206307=CARTESIAN_POINT('Ctrl Pts',(-31.3896121658909,54.5272862282532,
40.100244835349));
#206308=CARTESIAN_POINT('Ctrl Pts',(-31.365841113034,54.4597196360208,40.10025));
#206309=CARTESIAN_POINT('Ctrl Pts',(-31.3046029601553,54.5905300051369,
40.1202442001041));
#206310=CARTESIAN_POINT('Ctrl Pts',(-31.3268524737456,54.5367961153122,
40.0633873868015));
#206311=CARTESIAN_POINT('Ctrl Pts',(-31.3125672934291,54.4615686025428,
40.0772271723538));
#206312=CARTESIAN_POINT('Ctrl Pts',(-31.1759014746037,54.5809273110396,
40.0045995998161));
#206313=CARTESIAN_POINT('Ctrl Pts',(-31.2415992967176,54.5158579940065,
39.9663485808318));
#206314=CARTESIAN_POINT('Ctrl Pts',(-31.2227682191853,54.4295063924926,
40.0101727202466));
#206315=CARTESIAN_POINT('Ctrl Pts',(-31.1295364123884,54.5540292360083,
39.9304654349861));
#206316=CARTESIAN_POINT('Ctrl Pts',(-31.2191033458797,54.4847364330961,
39.9051900162944));
#206317=CARTESIAN_POINT('Ctrl Pts',(-31.1861426211014,54.3969835118379,
39.9671857458167));
#206318=CARTESIAN_POINT('Ctrl Pts',(-31.106798218553,54.5146464769141,39.8576902534424));
#206319=CARTESIAN_POINT('Ctrl Pts',(-31.217488486086,54.4512761425985,39.8573998014387));
#206320=CARTESIAN_POINT('Ctrl Pts',(-31.1634057161435,54.3576020372441,
39.92499));
#206321=CARTESIAN_POINT('Origin',(-31.4100231232056,54.4342359163066,40.22725));
#206322=CARTESIAN_POINT('Origin',(0.274963065701566,0.158749999999997,39.116));
#206323=CARTESIAN_POINT('Origin',(-29.7268821954845,52.1234703131949,39.116));
#206324=CARTESIAN_POINT('Origin',(5.22371297615222E-17,-1.42798576194617E-16,
40.22725));
#206325=CARTESIAN_POINT('Origin',(-31.436419577513,54.4189959163066,40.22725));
#206326=CARTESIAN_POINT('Ctrl Pts',(-29.7268821954845,52.1234703131949,
38.989));
#206327=CARTESIAN_POINT('Ctrl Pts',(-29.8370321846011,52.0598751873272,
38.989));
#206328=CARTESIAN_POINT('Ctrl Pts',(-29.8368672985388,52.0599703843397,
39.1161901092328));
#206329=CARTESIAN_POINT('Ctrl Pts',(-29.6185926664413,51.9354481180173,
38.989));
#206330=CARTESIAN_POINT('Ctrl Pts',(-29.7286387544932,51.8721332876001,
38.9892298989718));
#206331=CARTESIAN_POINT('Ctrl Pts',(-29.7501084152017,51.9096995898778,
39.116190049319));
#206332=CARTESIAN_POINT('Ctrl Pts',(-29.5155047636231,51.7564527430629,
39.1034966344368));
#206333=CARTESIAN_POINT('Ctrl Pts',(-29.6254243098796,51.6933616226636,
39.1038314102586));
#206334=CARTESIAN_POINT('Ctrl Pts',(-29.6675155901142,51.7666446199909,
39.2077528789606));
#206335=CARTESIAN_POINT('Ctrl Pts',(-29.4581217525669,51.656815567543,39.2875012672119));
#206336=CARTESIAN_POINT('Ctrl Pts',(-29.5680161811092,51.5939283753695,
39.2878045257868));
#206337=CARTESIAN_POINT('Ctrl Pts',(-29.6215404737379,51.6870133822668,
39.3549015295902));
#206338=CARTESIAN_POINT('Origin',(-29.5114749418,51.7503740054946,39.3548010137695));
#206339=CARTESIAN_POINT('Ctrl Pts',(-31.6576696180579,54.196600726121,39.8576902534424));
#206340=CARTESIAN_POINT('Ctrl Pts',(-31.5474441649279,54.2607761425985,
39.8573998014387));
#206341=CARTESIAN_POINT('Ctrl Pts',(-31.4933613949854,54.1671020372441,
39.92499));
#206342=CARTESIAN_POINT('Ctrl Pts',(-31.6804173066001,54.2360018544268,
39.9304984902494));
#206343=CARTESIAN_POINT('Ctrl Pts',(-31.5756301844101,54.2789150989593,
39.9052171569796));
#206344=CARTESIAN_POINT('Ctrl Pts',(-31.5161086602375,54.2065014563941,
39.96720497266));
#206345=CARTESIAN_POINT('Ctrl Pts',(-31.6804328064619,54.2894509908545,
40.0043437678659));
#206346=CARTESIAN_POINT('Ctrl Pts',(-31.5911964272957,54.313884182711,39.966162857764));
#206347=CARTESIAN_POINT('Ctrl Pts',(-31.5258675551963,54.2543268901841,
40.0100243556235));
#206348=CARTESIAN_POINT('Ctrl Pts',(-31.6250591602186,54.4049648787503,
40.1194874821991));
#206349=CARTESIAN_POINT('Ctrl Pts',(-31.5671393481779,54.397608888651,40.0627551483143));
#206350=CARTESIAN_POINT('Ctrl Pts',(-31.5090508246489,54.3475791360316,
40.0767884282377));
#206351=CARTESIAN_POINT('Ctrl Pts',(-31.5668453499335,54.4680334478298,
40.1599502015398));
#206352=CARTESIAN_POINT('Ctrl Pts',(-31.5274226111428,54.4477213412897,
40.100244945386));
#206353=CARTESIAN_POINT('Ctrl Pts',(-31.4807263372351,54.3933906465338,
40.10025));
#206354=CARTESIAN_POINT('Ctrl Pts',(-31.4902932482903,54.5122556166614,
40.1599502534424));
#206355=CARTESIAN_POINT('Ctrl Pts',(-31.4716329851984,54.4799531854482,
40.10025));
#206356=CARTESIAN_POINT('Ctrl Pts',(-31.436419577513,54.4189959163066,40.10025));
#206357=CARTESIAN_POINT('Origin',(-31.603346621266,54.1036020372441,39.92499));
#206358=CARTESIAN_POINT('Origin',(-29.4224002636351,51.596092137187,39.6398955069316));
#206359=CARTESIAN_POINT('Origin',(-29.333325585345,51.4418102687788,39.92499));
#206360=CARTESIAN_POINT('Origin',(-31.5142720655972,53.9493203812116,39.6398955068281));
#206361=CARTESIAN_POINT('Origin',(-31.4251975098788,53.7950387249982,39.3548010137695));
#206362=CARTESIAN_POINT('Ctrl Pts',(-29.2799753962458,51.3482501200168,
39.8576902534424));
#206363=CARTESIAN_POINT('Ctrl Pts',(-29.3897042746969,51.2854610232004,
39.8579948730703));
#206364=CARTESIAN_POINT('Ctrl Pts',(-29.4433108116256,51.3783102687788,
39.92499));
#206365=CARTESIAN_POINT('Ctrl Pts',(-29.2572578385493,51.3089010921306,
39.9304020711231));
#206366=CARTESIAN_POINT('Ctrl Pts',(-29.3615397594605,51.2670685993242,
39.9058915297385));
#206367=CARTESIAN_POINT('Ctrl Pts',(-29.4205918519431,51.3389598763134,
39.9671523786034));
#206368=CARTESIAN_POINT('Ctrl Pts',(-29.2572680623744,51.255740761606,40.0043257306693));
#206369=CARTESIAN_POINT('Ctrl Pts',(-29.3461554108688,51.2319924817694,
39.9667894847835));
#206370=CARTESIAN_POINT('Ctrl Pts',(-29.4109522357566,51.2913733902323,
40.0100138975201));
#206371=CARTESIAN_POINT('Ctrl Pts',(-29.312791073701,51.1410333861057,40.1195533054858));
#206372=CARTESIAN_POINT('Ctrl Pts',(-29.3705286780136,51.1485922293424,
40.0630813209236));
#206373=CARTESIAN_POINT('Ctrl Pts',(-29.4282055900895,51.1987619028143,
40.076826594242));
#206374=CARTESIAN_POINT('Ctrl Pts',(-29.3710651187643,51.0785202710265,
40.159950202751));
#206375=CARTESIAN_POINT('Ctrl Pts',(-29.4103605382572,51.0989122516725,
40.1002552791547));
#206376=CARTESIAN_POINT('Ctrl Pts',(-29.4568175306711,51.1533747228777,
40.10025));
#206377=CARTESIAN_POINT('Ctrl Pts',(-29.4472515437731,51.0345602039889,
40.1599502534424));
#206378=CARTESIAN_POINT('Ctrl Pts',(-29.4658956314762,51.066871973898,40.10025));
#206379=CARTESIAN_POINT('Ctrl Pts',(-29.5010785149107,51.127846865905,40.10025));
#206380=CARTESIAN_POINT('Origin',(-29.5010785149107,51.127846865905,40.22725));
#206381=CARTESIAN_POINT('Ctrl Pts',(-31.2097904767601,53.4219427993289,
38.989));
#206382=CARTESIAN_POINT('Ctrl Pts',(-31.0996409281616,53.4855376708634,
38.989));
#206383=CARTESIAN_POINT('Ctrl Pts',(-31.0998053730483,53.4854427285638,
39.1161896013272));
#206384=CARTESIAN_POINT('Ctrl Pts',(-31.3184716867872,53.6097387976561,
38.989));
#206385=CARTESIAN_POINT('Ctrl Pts',(-31.2082219299917,53.6736064794776,
38.9887769275436));
#206386=CARTESIAN_POINT('Ctrl Pts',(-31.1865640704865,53.6357132000293,
39.1161898821829));
#206387=CARTESIAN_POINT('Ctrl Pts',(-31.4219325588441,53.7885186806146,
39.1034967087243));
#206388=CARTESIAN_POINT('Ctrl Pts',(-31.3115622968571,53.8525981958214,
39.1031720232723));
#206389=CARTESIAN_POINT('Ctrl Pts',(-31.2691568563324,53.7787681009859,
39.2077529615016));
#206390=CARTESIAN_POINT('Ctrl Pts',(-31.4795232016785,53.8880358395973,
39.2875012672119));
#206391=CARTESIAN_POINT('Ctrl Pts',(-31.3691313396255,53.9523112232412,
39.2872087095508));
#206392=CARTESIAN_POINT('Ctrl Pts',(-31.3151318380577,53.8583991049519,
39.354901704823));
#206393=CARTESIAN_POINT('Origin',(-31.2097904767601,53.4219427993289,39.116));
#206394=CARTESIAN_POINT('Origin',(3.82640399828021E-16,5.07986659106885E-17,
40.22725));
#206395=CARTESIAN_POINT('Origin',(-29.527474969218,51.112606865905,40.22725));
#206396=CARTESIAN_POINT('Origin',(15.2806508669887,-27.1018636743464,39.116));
#206397=CARTESIAN_POINT('Origin',(-31.0091584503668,53.0743345559679,39.1160373285238));
#206398=CARTESIAN_POINT('Ctrl Pts',(-29.4735998357333,51.019348010533,40.1599502534424));
#206399=CARTESIAN_POINT('Ctrl Pts',(-29.4922606054642,51.0516501490689,
40.10025));
#206400=CARTESIAN_POINT('Ctrl Pts',(-29.527474969218,51.112606865905,40.10025));
#206401=CARTESIAN_POINT('Ctrl Pts',(-29.5495039426964,50.9754987628535,
40.1599500566041));
#206402=CARTESIAN_POINT('Ctrl Pts',(-29.5475581014565,51.0197013834509,
40.100255130536));
#206403=CARTESIAN_POINT('Ctrl Pts',(-29.5715624158006,51.0871269269771,
40.10025));
#206404=CARTESIAN_POINT('Ctrl Pts',(-29.6319914129668,50.9562029902291,
40.1203070619046));
#206405=CARTESIAN_POINT('Ctrl Pts',(-29.6100038038524,51.0098791271086,
40.0637098684499));
#206406=CARTESIAN_POINT('Ctrl Pts',(-29.6246193648992,51.0848223701589,
40.0772636213362));
#206407=CARTESIAN_POINT('Ctrl Pts',(-29.7600395375186,50.9652607924608,
40.0046102245801));
#206408=CARTESIAN_POINT('Ctrl Pts',(-29.695116411909,51.0303675504167,39.9670001894012));
#206409=CARTESIAN_POINT('Ctrl Pts',(-29.7140610042227,51.1161687394137,
40.010178881121));
#206410=CARTESIAN_POINT('Ctrl Pts',(-29.8061925581062,50.9919958361059,
39.9303710930186));
#206411=CARTESIAN_POINT('Ctrl Pts',(-29.7178148857793,51.0613912713645,
39.9058663574112));
#206412=CARTESIAN_POINT('Ctrl Pts',(-29.7505571803535,51.1484765898565,
39.9671344706366));
#206413=CARTESIAN_POINT('Ctrl Pts',(-29.8289013456881,51.0313275753412,
39.8576902534424));
#206414=CARTESIAN_POINT('Ctrl Pts',(-29.7196599535388,51.0949610232004,
39.8579948730704));
#206415=CARTESIAN_POINT('Ctrl Pts',(-29.7732664904675,51.1878102687788,
39.92499));
#206416=CARTESIAN_POINT('Origin',(-29.8832517167481,51.1243102687788,39.92499));
#206417=CARTESIAN_POINT('Origin',(-30.9870007553615,53.0360596824725,39.1925554488852));
#206418=CARTESIAN_POINT('Origin',(-30.9460815882863,52.9651856060848,39.3343017080178));
#206419=CARTESIAN_POINT('Origin',(-29.9723263949791,51.2785921372021,39.6398955069213));
#206420=CARTESIAN_POINT('Origin',(-30.0614010732032,51.4328740054946,39.3548010137695));
#206421=CARTESIAN_POINT('Ctrl Pts',(-30.7811015270739,52.679431757829,39.3978017080178));
#206422=CARTESIAN_POINT('Ctrl Pts',(-30.6711163007932,52.742931757829,39.3978017080178));
#206423=CARTESIAN_POINT('Ctrl Pts',(-30.6711163007932,52.742931757829,39.5248017080178));
#206424=CARTESIAN_POINT('Ctrl Pts',(-30.8259039490945,52.7575002129179,
39.3978017080178));
#206425=CARTESIAN_POINT('Ctrl Pts',(-30.7160792752572,52.8208099140567,
39.3980355775187));
#206426=CARTESIAN_POINT('Ctrl Pts',(-30.7386233329133,52.8598573673291,
39.5248015517178));
#206427=CARTESIAN_POINT('Ctrl Pts',(-30.868269596017,52.8313189037794,39.3484893995498));
#206428=CARTESIAN_POINT('Ctrl Pts',(-30.7588072175368,52.8948168809906,
39.3489438303419));
#206429=CARTESIAN_POINT('Ctrl Pts',(-30.802456034311,52.9704188493343,39.4508333155597));
#206430=CARTESIAN_POINT('Ctrl Pts',(-30.8905967158731,52.8702215132219,
39.2708017080178));
#206431=CARTESIAN_POINT('Ctrl Pts',(-30.7813498801527,52.9338619179798,
39.2710850691866));
#206432=CARTESIAN_POINT('Ctrl Pts',(-30.8360963620057,53.0286856060849,
39.3343017080178));
#206433=CARTESIAN_POINT('Origin',(-30.7811015270739,52.679431757829,39.5248017080178));
#206434=CARTESIAN_POINT('Ctrl Pts',(-30.0070536838153,51.33988956927,39.2875012672119));
#206435=CARTESIAN_POINT('Ctrl Pts',(-29.897644576157,51.4036173326915,39.2878045257519));
#206436=CARTESIAN_POINT('Ctrl Pts',(-29.9514963916949,51.4965132298826,
39.3549015218349));
#206437=CARTESIAN_POINT('Ctrl Pts',(-30.0646513737685,51.4394048060594,
39.1034938540228));
#206438=CARTESIAN_POINT('Ctrl Pts',(-29.9550530981037,51.5030523579604,
39.103828627882));
#206439=CARTESIAN_POINT('Ctrl Pts',(-29.9974722043259,51.5761456730022,
39.2077506434042));
#206440=CARTESIAN_POINT('Ctrl Pts',(-30.1681227811168,51.6181806476915,
38.989));
#206441=CARTESIAN_POINT('Ctrl Pts',(-30.058267491178,51.6818259279779,38.9892298954593));
#206442=CARTESIAN_POINT('Ctrl Pts',(-30.0800656843523,51.7192017762872,
39.1161900347273));
#206443=CARTESIAN_POINT('Ctrl Pts',(-30.2768083268876,51.8059703131949,
38.989));
#206444=CARTESIAN_POINT('Ctrl Pts',(-30.1666583504929,51.8695654317176,
38.989));
#206445=CARTESIAN_POINT('Ctrl Pts',(-30.1668232238143,51.8694702420611,
39.1161900945648));
#206446=CARTESIAN_POINT('Origin',(-30.2768083268876,51.8059703131949,39.116));
#206447=CARTESIAN_POINT('Origin',(14.903849434298,-26.4492244485613,39.5248017080178));
#206448=CARTESIAN_POINT('Origin',(-30.7054974692364,52.5484816883962,39.5248017080178));
#206449=CARTESIAN_POINT('Origin',(14.8448439902557,-26.3470240215568,39.116));
#206450=CARTESIAN_POINT('Origin',(-30.4775331296737,52.1535342613176,39.1160402713853));
#206451=CARTESIAN_POINT('Ctrl Pts',(-30.5960088312564,52.3576880233165,
39.2708017080178));
#206452=CARTESIAN_POINT('Ctrl Pts',(-30.4857749404415,52.4219111049559,
39.2705119464801));
#206453=CARTESIAN_POINT('Ctrl Pts',(-30.4305321463772,52.3262277788844,
39.3343017080178));
#206454=CARTESIAN_POINT('Ctrl Pts',(-30.6184089696597,52.396723545737,39.3487519301186));
#206455=CARTESIAN_POINT('Ctrl Pts',(-30.5081585269339,52.4606806140172,
39.3482879463988));
#206456=CARTESIAN_POINT('Ctrl Pts',(-30.4642861617682,52.384691448501,39.451227126164));
#206457=CARTESIAN_POINT('Ctrl Pts',(-30.660846452162,52.4706758922786,39.3978017080178));
#206458=CARTESIAN_POINT('Ctrl Pts',(-30.5506153465205,52.5342179826678,
39.3975673827397));
#206459=CARTESIAN_POINT('Ctrl Pts',(-30.528232593673,52.4954499175231,39.5248015355181));
#206460=CARTESIAN_POINT('Ctrl Pts',(-30.7054974692364,52.5484816883962,
39.3978017080178));
#206461=CARTESIAN_POINT('Ctrl Pts',(-30.5955122429558,52.6119816883962,
39.3978017080178));
#206462=CARTESIAN_POINT('Ctrl Pts',(-30.5955122429558,52.6119816883962,
39.5248017080178));
#206463=CARTESIAN_POINT('Origin',(-30.5405173726578,52.2627277788844,39.3343017080178));
#206464=CARTESIAN_POINT('Origin',(-30.4998422394556,52.1922763809708,39.193400853355));
#206465=CARTESIAN_POINT('Origin',(-24.6933715417274,56.2428239377275,39.1925554495085));
#206466=CARTESIAN_POINT('Origin',(-24.7113125977903,56.2832472948513,39.1160373285287));
#206467=CARTESIAN_POINT('Origin',(-24.6600848917106,56.168060898428,39.3343017080178));
#206468=CARTESIAN_POINT('Ctrl Pts',(-24.6158705164589,56.0673542004328,
39.2708017080178));
#206469=CARTESIAN_POINT('Ctrl Pts',(-24.731570364333,56.01637854512,39.2710850691866));
#206470=CARTESIAN_POINT('Ctrl Pts',(-24.7761051648312,56.1164053447574,
39.3343017080178));
#206471=CARTESIAN_POINT('Ctrl Pts',(-24.5974591883321,56.0262864882909,
39.3487519293518));
#206472=CARTESIAN_POINT('Ctrl Pts',(-24.7131705636667,55.9750519161912,
39.3492068662931));
#206473=CARTESIAN_POINT('Ctrl Pts',(-24.7486471852354,56.0547337128479,
39.4512271248745));
#206474=CARTESIAN_POINT('Ctrl Pts',(-24.5625784858788,55.9484840819677,
39.3978017080178));
#206475=CARTESIAN_POINT('Ctrl Pts',(-24.6783511906864,55.8968463240355,
39.398034778116));
#206476=CARTESIAN_POINT('Ctrl Pts',(-24.6966284839301,55.9378977967857,
39.5248015355176));
#206477=CARTESIAN_POINT('Ctrl Pts',(-24.5258780191666,55.8666273273835,
39.3978017080178));
#206478=CARTESIAN_POINT('Ctrl Pts',(-24.6418982922872,55.8149717737129,
39.3978017080178));
#206479=CARTESIAN_POINT('Ctrl Pts',(-24.6418982922872,55.8149717737129,
39.5248017080178));
#206480=CARTESIAN_POINT('Origin',(-24.5258780191666,55.8666273273835,39.5248017080178));
#206481=CARTESIAN_POINT('Origin',(0.290050682801532,0.129138884176564,39.116));
#206482=CARTESIAN_POINT('Origin',(-24.8746050278048,56.6498810128384,39.116));
#206483=CARTESIAN_POINT('Origin',(0.290050682801533,0.129138884176564,39.5248017080178));
#206484=CARTESIAN_POINT('Origin',(-24.4643761377912,55.72849184015,39.5248017080178));
#206485=CARTESIAN_POINT('Ctrl Pts',(-25.0931373005741,57.1420619865023,
39.2875012672119));
#206486=CARTESIAN_POINT('Ctrl Pts',(-25.2100238766574,57.0905332211013,
39.287208709576));
#206487=CARTESIAN_POINT('Ctrl Pts',(-25.165787501526,56.9916465525425,39.3549016990122));
#206488=CARTESIAN_POINT('Ctrl Pts',(-25.0464764504208,57.0369738651811,
39.1034939173931));
#206489=CARTESIAN_POINT('Ctrl Pts',(-25.1631918674125,56.9853474458547,
39.103169233632));
#206490=CARTESIAN_POINT('Ctrl Pts',(-25.1283875141299,56.9076448051888,
39.2077507202312));
#206491=CARTESIAN_POINT('Ctrl Pts',(-24.9626525995179,56.8481865914869,
38.989));
#206492=CARTESIAN_POINT('Ctrl Pts',(-25.0791258042768,56.7965331449371,
38.9887769311206));
#206493=CARTESIAN_POINT('Ctrl Pts',(-25.0611999573799,56.7567390814052,
39.1161898712896));
#206494=CARTESIAN_POINT('Ctrl Pts',(-24.8746050278048,56.6498810128384,
38.989));
#206495=CARTESIAN_POINT('Ctrl Pts',(-24.9907986298332,56.598148288166,38.989));
#206496=CARTESIAN_POINT('Ctrl Pts',(-24.990625171646,56.5982255167267,39.1161895903853));
#206497=CARTESIAN_POINT('Origin',(-25.049832894896,57.0434492461381,39.3548010137695));
#206498=CARTESIAN_POINT('Ctrl Pts',(-24.4643761377912,55.72849184015,39.3978017080178));
#206499=CARTESIAN_POINT('Ctrl Pts',(-24.5803964109118,55.6768362864794,
39.3978017080178));
#206500=CARTESIAN_POINT('Ctrl Pts',(-24.5803964109118,55.6768362864794,
39.5248017080178));
#206501=CARTESIAN_POINT('Ctrl Pts',(-24.4275510972981,55.6463586582053,
39.3978017080178));
#206502=CARTESIAN_POINT('Ctrl Pts',(-24.5437506299587,55.5945285148505,
39.3975666025031));
#206503=CARTESIAN_POINT('Ctrl Pts',(-24.5254812387358,55.5534947903269,
39.5248015517182));
#206504=CARTESIAN_POINT('Ctrl Pts',(-24.3927285408598,55.5686962576409,
39.3484894016716));
#206505=CARTESIAN_POINT('Ctrl Pts',(-24.5092751529634,55.5170953257147,
39.3480259000038));
#206506=CARTESIAN_POINT('Ctrl Pts',(-24.4735550281868,55.4368666119041,
39.4508333188947));
#206507=CARTESIAN_POINT('Ctrl Pts',(-24.3743766270209,55.5277679687685,
39.2708017080178));
#206508=CARTESIAN_POINT('Ctrl Pts',(-24.4911280468221,55.4763362579877,
39.27051194648));
#206509=CARTESIAN_POINT('Ctrl Pts',(-24.4461895095984,55.3754026508177,
39.3343017080178));
#206510=CARTESIAN_POINT('Origin',(-24.3301692364778,55.4270582044883,39.3343017080178));
#206511=CARTESIAN_POINT('Origin',(-25.1222926664929,57.2061965577165,39.6398955068185));
#206512=CARTESIAN_POINT('Origin',(-25.1947524379611,57.3689438691198,39.92499));
#206513=CARTESIAN_POINT('Origin',(-24.2970811015489,55.3527410366449,39.193400853995));
#206514=CARTESIAN_POINT('Origin',(-24.2788510342437,55.3119205422647,39.1160402713851));
#206515=CARTESIAN_POINT('Ctrl Pts',(-25.5918112338789,57.5176823163891,
40.1599502534424));
#206516=CARTESIAN_POINT('Ctrl Pts',(-25.5766462455171,57.483598953748,40.10025));
#206517=CARTESIAN_POINT('Ctrl Pts',(-25.5480287005713,57.4192809246791,
40.10025));
#206518=CARTESIAN_POINT('Ctrl Pts',(-25.5113050800551,57.5535024391257,
40.1599500538466));
#206519=CARTESIAN_POINT('Ctrl Pts',(-25.5180031505006,57.509687971276,40.1002448353478));
#206520=CARTESIAN_POINT('Ctrl Pts',(-25.501424950013,57.4400067642803,40.10025));
#206521=CARTESIAN_POINT('Ctrl Pts',(-25.4268488592814,57.5636994104962,
40.1202442001039));
#206522=CARTESIAN_POINT('Ctrl Pts',(-25.4545932086369,57.5125855880061,
40.0633873868018));
#206523=CARTESIAN_POINT('Ctrl Pts',(-25.4482497003379,57.436276971477,40.0772271723538));
#206524=CARTESIAN_POINT('Ctrl Pts',(-25.2998561687908,57.5406963524573,
40.0045995998162));
#206525=CARTESIAN_POINT('Ctrl Pts',(-25.3719956870765,57.482850784337,39.9663485808315));
#206526=CARTESIAN_POINT('Ctrl Pts',(-25.3622939683643,57.3950038423351,
40.0101727202465));
#206527=CARTESIAN_POINT('Ctrl Pts',(-25.2565567136854,57.5090991591925,
39.9304654349859));
#206528=CARTESIAN_POINT('Ctrl Pts',(-25.3528760603481,57.4495482434222,
39.9051900162946));
#206529=CARTESIAN_POINT('Ctrl Pts',(-25.3292685758745,57.3588307079389,
39.9671857458169));
#206530=CARTESIAN_POINT('Ctrl Pts',(-25.2380597013425,57.4675553545143,
39.8576902534424));
#206531=CARTESIAN_POINT('Ctrl Pts',(-25.354767599671,57.4161024530845,39.8573998014387));
#206532=CARTESIAN_POINT('Ctrl Pts',(-25.3107727110817,57.3172883154492,
39.92499));
#206533=CARTESIAN_POINT('Origin',(-25.5480287005713,57.4192809246791,40.22725));
#206534=CARTESIAN_POINT('Origin',(0.290050682801532,0.129138884176564,39.116));
#206535=CARTESIAN_POINT('Origin',(-24.1156489724272,54.9452378026831,39.116));
#206536=CARTESIAN_POINT('Origin',(3.68589728140376E-17,-1.5063413852568E-16,
40.22725));
#206537=CARTESIAN_POINT('Origin',(-25.5758735661203,57.4068835917982,40.22725));
#206538=CARTESIAN_POINT('Ctrl Pts',(-24.1156489724272,54.9452378026831,
38.989));
#206539=CARTESIAN_POINT('Ctrl Pts',(-24.2318430491562,54.8935048666604,
38.989));
#206540=CARTESIAN_POINT('Ctrl Pts',(-24.2316691155599,54.8935823068868,
39.1161901092324));
#206541=CARTESIAN_POINT('Ctrl Pts',(-24.0276063358803,54.7469262747034,
38.989));
#206542=CARTESIAN_POINT('Ctrl Pts',(-24.1436677818718,54.695461238022,38.9892298989742));
#206543=CARTESIAN_POINT('Ctrl Pts',(-24.1610930816816,54.7350659388079,
39.1161900493186));
#206544=CARTESIAN_POINT('Ctrl Pts',(-23.9437932708526,54.55813583508,39.1034966344368));
#206545=CARTESIAN_POINT('Ctrl Pts',(-24.0597054841957,54.5068800556966,
39.1038314102578));
#206546=CARTESIAN_POINT('Ctrl Pts',(-24.0939060248989,54.5841613379354,
39.2077528789611));
#206547=CARTESIAN_POINT('Ctrl Pts',(-23.8971395307763,54.4530463244695,
39.2875012672119));
#206548=CARTESIAN_POINT('Ctrl Pts',(-24.0130054476974,54.401990730652,39.2878045257868));
#206549=CARTESIAN_POINT('Ctrl Pts',(-24.0565064959267,54.5001606201974,
39.35490152959));
#206550=CARTESIAN_POINT('Origin',(-23.9404209259116,54.5516691663897,39.3548010137695));
#206551=CARTESIAN_POINT('Ctrl Pts',(-25.8191582032616,57.2088336324701,
39.8576902534424));
#206552=CARTESIAN_POINT('Ctrl Pts',(-25.7028284190329,57.2611357920727,
39.8573998014387));
#206553=CARTESIAN_POINT('Ctrl Pts',(-25.6588335304436,57.1623216544373,
39.92499));
#206554=CARTESIAN_POINT('Ctrl Pts',(-25.837662738193,57.2503966981984,39.930498490249));
#206555=CARTESIAN_POINT('Ctrl Pts',(-25.7289639953175,57.2821216226318,
39.9052171569806));
#206556=CARTESIAN_POINT('Ctrl Pts',(-25.6773378230588,57.2038829761261,
39.9672049726605));
#206557=CARTESIAN_POINT('Ctrl Pts',(-25.8320911970515,57.3035546548414,
40.0043437678664));
#206558=CARTESIAN_POINT('Ctrl Pts',(-25.7407897001101,57.3185262575347,
39.966162857764));
#206559=CARTESIAN_POINT('Ctrl Pts',(-25.6820441386713,57.2524664994808,
40.0100243556236));
#206560=CARTESIAN_POINT('Ctrl Pts',(-25.7649464042476,57.4126476234252,
40.1194874821986));
#206561=CARTESIAN_POINT('Ctrl Pts',(-25.7081127933381,57.3992776612639,
40.0627551483143));
#206562=CARTESIAN_POINT('Ctrl Pts',(-25.6555720179783,57.3434500727656,
40.0767884282376));
#206563=CARTESIAN_POINT('Ctrl Pts',(-25.7004590347003,57.4692856961542,
40.1599502015394));
#206564=CARTESIAN_POINT('Ctrl Pts',(-25.6633754510794,57.4449640631536,
40.1002449453872));
#206565=CARTESIAN_POINT('Ctrl Pts',(-25.6226140882776,57.3860499078786,
40.10025));
#206566=CARTESIAN_POINT('Ctrl Pts',(-25.6197038181293,57.5052637377734,
40.1599502534424));
#206567=CARTESIAN_POINT('Ctrl Pts',(-25.6045223014057,57.4711877340331,
40.10025));
#206568=CARTESIAN_POINT('Ctrl Pts',(-25.5758735661203,57.4068835917982,
40.10025));
#206569=CARTESIAN_POINT('Origin',(-25.7748538035642,57.1106661007667,39.92499));
#206570=CARTESIAN_POINT('Origin',(-23.8679610547577,54.3889216310751,39.6398955069317));
#206571=CARTESIAN_POINT('Origin',(-23.7955011834904,54.2261740956468,39.92499));
#206572=CARTESIAN_POINT('Origin',(-25.7023940320476,56.9479187893687,39.6398955068277));
#206573=CARTESIAN_POINT('Origin',(-25.629934260499,56.785171477785,39.3548010137695));
#206574=CARTESIAN_POINT('Ctrl Pts',(-23.7522229508823,54.1275498658876,
39.8576902534424));
#206575=CARTESIAN_POINT('Ctrl Pts',(-23.8679139708563,54.0765745253538,
39.8579948730703));
#206576=CARTESIAN_POINT('Ctrl Pts',(-23.911521456611,54.1745185419762,39.92499));
#206577=CARTESIAN_POINT('Ctrl Pts',(-23.7337429357603,54.0860417646979,
39.930402071123));
#206578=CARTESIAN_POINT('Ctrl Pts',(-23.841826275586,54.0553388636023,39.9058915297381));
#206579=CARTESIAN_POINT('Ctrl Pts',(-23.8930401898202,54.1330089371358,
39.9671523786038));
#206580=CARTESIAN_POINT('Ctrl Pts',(-23.7393098712344,54.033173720707,40.0043257306694));
#206581=CARTESIAN_POINT('Ctrl Pts',(-23.8301926567295,54.018846794374,39.9667894847838));
#206582=CARTESIAN_POINT('Ctrl Pts',(-23.8884275227219,54.0846755205375,
40.01001389752));
#206583=CARTESIAN_POINT('Ctrl Pts',(-23.806518907382,53.9248984592618,40.1195533054857));
#206584=CARTESIAN_POINT('Ctrl Pts',(-23.8631501047896,53.938451117416,40.0630813209234));
#206585=CARTESIAN_POINT('Ctrl Pts',(-23.9152668978355,53.9943748351525,
40.076826594242));
#206586=CARTESIAN_POINT('Ctrl Pts',(-23.8710081209824,53.8688190939466,
40.1599502027512));
#206587=CARTESIAN_POINT('Ctrl Pts',(-23.9079567336554,53.8932068550015,
40.1002552791541));
#206588=CARTESIAN_POINT('Ctrl Pts',(-23.948466351384,53.9522270531176,40.10025));
#206589=CARTESIAN_POINT('Ctrl Pts',(-23.951372267036,53.833063494684,40.1599502534424));
#206590=CARTESIAN_POINT('Ctrl Pts',(-23.9665367208219,53.8671470951733,
40.10025));
#206591=CARTESIAN_POINT('Ctrl Pts',(-23.9951532569802,53.9314655730806,
40.10025));
#206592=CARTESIAN_POINT('Origin',(-23.9951532569802,53.9314655730806,40.22725));
#206593=CARTESIAN_POINT('Ctrl Pts',(-25.4547063934078,56.3916032444853,
38.989));
#206594=CARTESIAN_POINT('Ctrl Pts',(-25.3385127813683,56.4433359736149,
38.989));
#206595=CARTESIAN_POINT('Ctrl Pts',(-25.3386862495815,56.4432587405904,
39.1161896013274));
#206596=CARTESIAN_POINT('Ctrl Pts',(-25.5431622092821,56.5897307565543,
38.989));
#206597=CARTESIAN_POINT('Ctrl Pts',(-25.426840421553,56.6417243268743,38.988776927543));
#206598=CARTESIAN_POINT('Ctrl Pts',(-25.4092621323401,56.6017747680072,
39.1161898821832));
#206599=CARTESIAN_POINT('Ctrl Pts',(-25.627368725429,56.7783458705718,39.1034967087243));
#206600=CARTESIAN_POINT('Ctrl Pts',(-25.5109049500366,56.8305375176205,
39.1031720232707));
#206601=CARTESIAN_POINT('Ctrl Pts',(-25.4764491573047,56.7526792962324,
39.2077529615013));
#206602=CARTESIAN_POINT('Ctrl Pts',(-25.6742415049975,56.8833377255396,
39.2875012672119));
#206603=CARTESIAN_POINT('Ctrl Pts',(-25.5577357740368,56.9357219102092,
39.2872087095508));
#206604=CARTESIAN_POINT('Ctrl Pts',(-25.5138485767958,56.8366797674136,
39.3549017048232));
#206605=CARTESIAN_POINT('Origin',(-25.4547063934078,56.3916032444853,39.116));
#206606=CARTESIAN_POINT('Origin',(3.88110971579612E-16,5.35860614414083E-17,
40.22725));
#206607=CARTESIAN_POINT('Origin',(-24.0229981225292,53.9190682401997,40.22725));
#206608=CARTESIAN_POINT('Origin',(10.0037024164483,-23.2492868865826,39.116));
#206609=CARTESIAN_POINT('Origin',(-25.2915084057502,56.0249274780519,39.1160373285286));
#206610=CARTESIAN_POINT('Ctrl Pts',(-23.9791663275009,53.8206887816838,
40.1599502534424));
#206611=CARTESIAN_POINT('Ctrl Pts',(-23.9943483786813,53.8547645473083,
40.10025));
#206612=CARTESIAN_POINT('Ctrl Pts',(-24.0229981225292,53.9190682401997,
40.10025));
#206613=CARTESIAN_POINT('Ctrl Pts',(-24.0592381182997,53.785013884428,40.1599500566034));
#206614=CARTESIAN_POINT('Ctrl Pts',(-24.0526825045793,53.8287709626519,
40.100255130536));
#206615=CARTESIAN_POINT('Ctrl Pts',(-24.0695074323274,53.8983362760852,
40.10025));
#206616=CARTESIAN_POINT('Ctrl Pts',(-24.1432906710367,53.7744461045707,
40.1203070619049));
#206617=CARTESIAN_POINT('Ctrl Pts',(-24.115812828243,53.8255298669644,40.06370986845));
#206618=CARTESIAN_POINT('Ctrl Pts',(-24.1225146216891,53.9015903052236,
40.0772636213363));
#206619=CARTESIAN_POINT('Ctrl Pts',(-24.2696905364168,53.796838960898,40.0046102245799));
#206620=CARTESIAN_POINT('Ctrl Pts',(-24.1983175571254,53.8548027426712,
39.9670001894012));
#206621=CARTESIAN_POINT('Ctrl Pts',(-24.2081897025474,53.9421141528993,
40.0101788811208));
#206622=CARTESIAN_POINT('Ctrl Pts',(-24.3127961528998,53.8282518514941,
39.9303710930188));
#206623=CARTESIAN_POINT('Ctrl Pts',(-24.2176488245027,53.8880291490223,
39.9058663574119));
#206624=CARTESIAN_POINT('Ctrl Pts',(-24.2411088588481,53.9780599067625,
39.967134470637));
#206625=CARTESIAN_POINT('Ctrl Pts',(-24.3312692531083,53.8697418420147,
39.8576902534424));
#206626=CARTESIAN_POINT('Ctrl Pts',(-24.2159747902182,53.9216078643419,
39.8579948730703));
#206627=CARTESIAN_POINT('Ctrl Pts',(-24.2595822759728,54.0195518809643,
39.92499));
#206628=CARTESIAN_POINT('Origin',(-24.3756025490934,53.9678963272937,39.92499));
#206629=CARTESIAN_POINT('Origin',(-25.273472906618,55.984546168508,39.1925554488842));
#206630=CARTESIAN_POINT('Origin',(-25.2401862573137,55.9097831300749,39.3343017080178));
#206631=CARTESIAN_POINT('Origin',(-24.4480624203039,54.1306438627321,39.639895506923));
#206632=CARTESIAN_POINT('Origin',(-24.5205222915147,54.2933913980366,39.3548010137695));
#206633=CARTESIAN_POINT('Ctrl Pts',(-25.1059793847697,55.6083495590304,
39.3978017080178));
#206634=CARTESIAN_POINT('Ctrl Pts',(-24.9899591116491,55.660005112701,39.3978017080178));
#206635=CARTESIAN_POINT('Ctrl Pts',(-24.9899591116491,55.660005112701,39.5248017080178));
#206636=CARTESIAN_POINT('Ctrl Pts',(-25.1423759987949,55.6906734752782,
39.3978017080178));
#206637=CARTESIAN_POINT('Ctrl Pts',(-25.0265352902402,55.7421565548672,
39.3980355775163));
#206638=CARTESIAN_POINT('Ctrl Pts',(-25.0448742789051,55.7833465978032,
39.5248015517178));
#206639=CARTESIAN_POINT('Ctrl Pts',(-25.1767934079549,55.7685161955953,
39.3484893995498));
#206640=CARTESIAN_POINT('Ctrl Pts',(-25.0612933298573,55.820224390034,39.3489438303431));
#206641=CARTESIAN_POINT('Ctrl Pts',(-25.0968004762773,55.8999747466301,
39.4508333155605));
#206642=CARTESIAN_POINT('Ctrl Pts',(-25.1949317875296,55.8095395120009,
39.2708017080178));
#206643=CARTESIAN_POINT('Ctrl Pts',(-25.0796311836949,55.8614118841081,
39.2710850691866));
#206644=CARTESIAN_POINT('Ctrl Pts',(-25.1241659841931,55.9614386837455,
39.3343017080178));
#206645=CARTESIAN_POINT('Origin',(-25.1059793847697,55.6083495590304,39.5248017080178));
#206646=CARTESIAN_POINT('Ctrl Pts',(-24.4761921430387,54.1952354911874,
39.2875012672119));
#206647=CARTESIAN_POINT('Ctrl Pts',(-24.3607210247419,54.247177781362,39.2878045257519));
#206648=CARTESIAN_POINT('Ctrl Pts',(-24.4045675690225,54.3451938326307,
39.3549015218349));
#206649=CARTESIAN_POINT('Ctrl Pts',(-24.523072132049,54.3002261711148,39.1034938540228));
#206650=CARTESIAN_POINT('Ctrl Pts',(-24.4074212664148,54.3520689157386,
39.1038286278812));
#206651=CARTESIAN_POINT('Ctrl Pts',(-24.4419676644362,54.4291958219377,
39.2077506434045));
#206652=CARTESIAN_POINT('Ctrl Pts',(-24.6072895482032,54.4888383671844,
38.989));
#206653=CARTESIAN_POINT('Ctrl Pts',(-24.4913833136934,54.5406519873246,
38.9892298954618));
#206654=CARTESIAN_POINT('Ctrl Pts',(-24.5091552540989,54.580101618462,39.1161900347274));
#206655=CARTESIAN_POINT('Ctrl Pts',(-24.6957503380303,54.6869600343299,
38.989));
#206656=CARTESIAN_POINT('Ctrl Pts',(-24.5795562747208,54.7386929643778,
38.989));
#206657=CARTESIAN_POINT('Ctrl Pts',(-24.5797301948775,54.7386155301351,
39.1161900945648));
#206658=CARTESIAN_POINT('Origin',(-24.6957503380303,54.6869600343299,39.116));
#206659=CARTESIAN_POINT('Origin',(9.75435829333325,-22.6892508167094,39.5248017080178));
#206660=CARTESIAN_POINT('Origin',(-25.0444775033943,55.4702140717969,39.5248017080178));
#206661=CARTESIAN_POINT('Origin',(9.71531210234964,-22.6015516358793,39.116));
#206662=CARTESIAN_POINT('Origin',(-24.8590452239599,55.0536014459538,39.1160402713851));
#206663=CARTESIAN_POINT('Ctrl Pts',(-24.955532024241,55.2690209153042,39.2708017080178));
#206664=CARTESIAN_POINT('Ctrl Pts',(-24.839188866184,55.3213695969758,39.27051194648));
#206665=CARTESIAN_POINT('Ctrl Pts',(-24.7942503289602,55.2204359898058,
39.3343017080178));
#206666=CARTESIAN_POINT('Ctrl Pts',(-24.9737291291715,55.3101840490926,
39.3487519301186));
#206667=CARTESIAN_POINT('Ctrl Pts',(-24.8573973158448,55.362266444506,39.3482879463992));
#206668=CARTESIAN_POINT('Ctrl Pts',(-24.8217083187807,55.2821076446801,
39.4512271261643));
#206669=CARTESIAN_POINT('Ctrl Pts',(-25.0082040095649,55.3881672017732,
39.3978017080178));
#206670=CARTESIAN_POINT('Ctrl Pts',(-24.8919348043934,55.4398389138667,
39.3975673827397));
#206671=CARTESIAN_POINT('Ctrl Pts',(-24.8737270328808,55.3989435894802,
39.5248015355181));
#206672=CARTESIAN_POINT('Ctrl Pts',(-25.0444775033943,55.4702140717969,
39.3978017080178));
#206673=CARTESIAN_POINT('Ctrl Pts',(-24.9284572302737,55.5218696254675,
39.3978017080178));
#206674=CARTESIAN_POINT('Ctrl Pts',(-24.9284572302736,55.5218696254675,
39.5248017080178));
#206675=CARTESIAN_POINT('Origin',(-24.9102706020808,55.1687804361352,39.3343017080178));
#206676=CARTESIAN_POINT('Origin',(-24.8771824678736,55.0944632691849,39.1934008533545));
#206677=CARTESIAN_POINT('Origin',(-18.6791227126682,58.5158800435661,39.1925554495081));
#206678=CARTESIAN_POINT('Origin',(-18.6927400943481,58.5579573083294,39.1160373285272));
#206679=CARTESIAN_POINT('Origin',(-18.6538332760099,58.4380471616456,39.3343017080178));
#206680=CARTESIAN_POINT('Ctrl Pts',(-18.6203878281142,58.3332704847798,
39.2708017080178));
#206681=CARTESIAN_POINT('Ctrl Pts',(-18.7407822670297,58.294668006739,39.2710850691866));
#206682=CARTESIAN_POINT('Ctrl Pts',(-18.7746174535794,58.39880200336,39.3343017080178));
#206683=CARTESIAN_POINT('Ctrl Pts',(-18.6063701040097,58.2905032380261,
39.3487519293518));
#206684=CARTESIAN_POINT('Ctrl Pts',(-18.7268030714138,58.2516444665218,
39.3492068662926));
#206685=CARTESIAN_POINT('Ctrl Pts',(-18.7537563325798,58.3345980746928,
39.4512271248738));
#206686=CARTESIAN_POINT('Ctrl Pts',(-18.5798130476652,58.2094810152003,
39.3978017080178));
#206687=CARTESIAN_POINT('Ctrl Pts',(-18.7003491529649,58.1702276772286,
39.3980347781178));
#206688=CARTESIAN_POINT('Ctrl Pts',(-18.7142352739229,58.2129647630925,
39.524801535519));
#206689=CARTESIAN_POINT('Ctrl Pts',(-18.5518699907145,58.1242364370958,
39.3978017080178));
#206690=CARTESIAN_POINT('Ctrl Pts',(-18.672654168284,58.0849912788102,39.3978017080178));
#206691=CARTESIAN_POINT('Ctrl Pts',(-18.672654168284,58.0849912788102,39.5248017080178));
#206692=CARTESIAN_POINT('Origin',(-18.5518699907145,58.1242364370958,39.5248017080178));
#206693=CARTESIAN_POINT('Origin',(0.301960443923718,0.0981128957140429,
39.116));
#206694=CARTESIAN_POINT('Origin',(-18.8168143322221,58.9396512752215,39.116));
#206695=CARTESIAN_POINT('Origin',(0.301960443923718,0.0981128957140429,
39.5248017080178));
#206696=CARTESIAN_POINT('Origin',(-18.5051441132836,57.9804289733665,39.5248017080178));
#206697=CARTESIAN_POINT('Ctrl Pts',(-18.9827025415091,59.4519788726609,
39.2875012672119));
#206698=CARTESIAN_POINT('Ctrl Pts',(-19.1043350233607,59.4129503614027,
39.287208709576));
#206699=CARTESIAN_POINT('Ctrl Pts',(-19.0706774512221,59.3099814440477,
39.3549016990125));
#206700=CARTESIAN_POINT('Ctrl Pts',(-18.9472820042043,59.3425890481026,
39.1034939173931));
#206701=CARTESIAN_POINT('Ctrl Pts',(-19.0687544722108,59.3034455268866,
39.1031692336336));
#206702=CARTESIAN_POINT('Ctrl Pts',(-19.042262918434,59.2225305038497,39.2077507202307));
#206703=CARTESIAN_POINT('Ctrl Pts',(-18.8836509927328,59.1460739925263,
38.989));
#206704=CARTESIAN_POINT('Ctrl Pts',(-19.0048854004771,59.1068782740618,
38.9887769311158));
#206705=CARTESIAN_POINT('Ctrl Pts',(-18.9912173655535,59.0654284453474,
39.1161898712903));
#206706=CARTESIAN_POINT('Ctrl Pts',(-18.8168143322221,58.9396512752215,
38.989));
#206707=CARTESIAN_POINT('Ctrl Pts',(-18.9377789557524,58.9003474864891,
38.989));
#206708=CARTESIAN_POINT('Ctrl Pts',(-18.9375983752039,58.9004061606661,
39.116189590386));
#206709=CARTESIAN_POINT('Origin',(-18.9499432001052,59.3493798002282,39.3548010137695));
#206710=CARTESIAN_POINT('Ctrl Pts',(-18.5051441132836,57.9804289733665,
39.3978017080178));
#206711=CARTESIAN_POINT('Ctrl Pts',(-18.6259282908531,57.9411838150809,
39.3978017080178));
#206712=CARTESIAN_POINT('Ctrl Pts',(-18.6259282908531,57.9411838150809,
39.5248017080178));
#206713=CARTESIAN_POINT('Ctrl Pts',(-18.477106059507,57.8948964606938,39.3978017080178));
#206714=CARTESIAN_POINT('Ctrl Pts',(-18.5980867642062,57.8554964068695,
39.3975666025045));
#206715=CARTESIAN_POINT('Ctrl Pts',(-18.5842066467862,57.8127777979925,
39.5248015517196));
#206716=CARTESIAN_POINT('Ctrl Pts',(-18.4505921960625,57.8140195545737,
39.3484894016716));
#206717=CARTESIAN_POINT('Ctrl Pts',(-18.5718941197448,57.7748837362136,
39.348025900003));
#206718=CARTESIAN_POINT('Ctrl Pts',(-18.5447558577156,57.6913607539413,
39.4508333188939));
#206719=CARTESIAN_POINT('Ctrl Pts',(-18.4366189870667,57.7713971777989,
39.2708017080178));
#206720=CARTESIAN_POINT('Ctrl Pts',(-18.5581069080655,57.7324510618072,
39.27051194648));
#206721=CARTESIAN_POINT('Ctrl Pts',(-18.5239649837002,57.6273730232607,
39.3343017080178));
#206722=CARTESIAN_POINT('Origin',(-18.4031808061308,57.6666181815463,39.3343017080178));
#206723=CARTESIAN_POINT('Origin',(-19.0049943031126,59.5188096735815,39.6398955068167));
#206724=CARTESIAN_POINT('Origin',(-19.0600454060081,59.6882395467422,39.92499));
#206725=CARTESIAN_POINT('Origin',(-18.3780421908181,57.5892494790287,39.1934008539941));
#206726=CARTESIAN_POINT('Origin',(-18.3641788932749,57.5467470426663,39.1160402713848));
#206727=CARTESIAN_POINT('Ctrl Pts',(-19.4393816709751,59.8776671349987,
40.1599502534424));
#206728=CARTESIAN_POINT('Ctrl Pts',(-19.4278624395261,59.8421853116554,
40.10025));
#206729=CARTESIAN_POINT('Ctrl Pts',(-19.4061247292248,59.7752282754839,
40.10025));
#206730=CARTESIAN_POINT('Ctrl Pts',(-19.3555723159017,59.9048758468123,
40.1599500538465));
#206731=CARTESIAN_POINT('Ctrl Pts',(-19.3668135526094,59.8620015382124,
40.100244835349));
#206732=CARTESIAN_POINT('Ctrl Pts',(-19.357609838725,59.7909691583393,40.10025));
#206733=CARTESIAN_POINT('Ctrl Pts',(-19.2705128813948,59.9061888791357,
40.1202442001037));
#206734=CARTESIAN_POINT('Ctrl Pts',(-19.3034480936183,59.8582551377153,
40.0633873868015));
#206735=CARTESIAN_POINT('Ctrl Pts',(-19.3051157581413,59.7817014705981,
40.0772271723539));
#206736=CARTESIAN_POINT('Ctrl Pts',(-19.1466203444575,59.8700374834727,
40.0045995998165));
#206737=CARTESIAN_POINT('Ctrl Pts',(-19.2244111832563,59.8200494324148,
39.9663485808318));
#206738=CARTESIAN_POINT('Ctrl Pts',(-19.2239451174246,59.7316696194043,
40.0101727202464));
#206739=CARTESIAN_POINT('Ctrl Pts',(-19.1068608943535,59.8340873574358,
39.9304654349858));
#206740=CARTESIAN_POINT('Ctrl Pts',(-19.2088773592686,59.7849307811033,
39.9051900162937));
#206741=CARTESIAN_POINT('Ctrl Pts',(-19.1948817636402,59.6922425516967,
39.9671857458174));
#206742=CARTESIAN_POINT('Ctrl Pts',(-19.0928077206406,59.7908376697913,
39.8576902534424));
#206743=CARTESIAN_POINT('Ctrl Pts',(-19.2142545736078,59.7518659300027,
39.8573998014387));
#206744=CARTESIAN_POINT('Ctrl Pts',(-19.1808295835776,59.6489943884566,
39.92499));
#206745=CARTESIAN_POINT('Origin',(-19.4061247292248,59.7752282754839,40.22725));
#206746=CARTESIAN_POINT('Origin',(0.301960443923718,0.0981128957140429,
39.116));
#206747=CARTESIAN_POINT('Origin',(-18.240199652704,57.1650137687749,39.116));
#206748=CARTESIAN_POINT('Origin',(2.07460197300492E-17,-1.56819321712836E-16,
40.22725));
#206749=CARTESIAN_POINT('Origin',(-19.4351129318415,59.7658094374953,40.22725));
#206750=CARTESIAN_POINT('Ctrl Pts',(-18.240199652704,57.1650137687749,38.989));
#206751=CARTESIAN_POINT('Ctrl Pts',(-18.3611647704257,57.12570981947,38.989));
#206752=CARTESIAN_POINT('Ctrl Pts',(-18.3609836949481,57.1257686544591,
39.1161901092322));
#206753=CARTESIAN_POINT('Ctrl Pts',(-18.1733685221997,56.958585650595,38.989));
#206754=CARTESIAN_POINT('Ctrl Pts',(-18.2941737326416,56.9195342693631,
38.9892298989724));
#206755=CARTESIAN_POINT('Ctrl Pts',(-18.3073637563256,56.9607434512644,
39.1161900493184));
#206756=CARTESIAN_POINT('Ctrl Pts',(-18.1097485684441,56.7620685738645,
39.1034966344368));
#206757=CARTESIAN_POINT('Ctrl Pts',(-18.2303834904091,56.7232097045386,
39.1038314102595));
#206758=CARTESIAN_POINT('Ctrl Pts',(-18.2563185832998,56.8036425617904,
39.2077528789613));
#206759=CARTESIAN_POINT('Ctrl Pts',(-18.0743352474886,56.6526781108325,
39.2875012672119));
#206760=CARTESIAN_POINT('Ctrl Pts',(-18.1949032015563,56.6140134911409,
39.2878045257868));
#206761=CARTESIAN_POINT('Ctrl Pts',(-18.2279043987986,56.7161926934814,
39.3549015295899));
#206762=CARTESIAN_POINT('Origin',(-18.1070706485037,56.7552848242272,39.3548010137695));
#206763=CARTESIAN_POINT('Ctrl Pts',(-19.697766688184,59.5942745858238,39.8576902534424));
#206764=CARTESIAN_POINT('Ctrl Pts',(-19.5766071063163,59.6341304551459,
39.8573998014387));
#206765=CARTESIAN_POINT('Ctrl Pts',(-19.5431821162861,59.5312589135997,
39.92499));
#206766=CARTESIAN_POINT('Ctrl Pts',(-19.7118253299475,59.6375442153291,
39.9304984902489));
#206767=CARTESIAN_POINT('Ctrl Pts',(-19.6004058925609,59.6577332347567,
39.9052171569792));
#206768=CARTESIAN_POINT('Ctrl Pts',(-19.5572406993628,59.574526783291,39.9672049726606));
#206769=CARTESIAN_POINT('Ctrl Pts',(-19.700727790773,59.6898285824901,40.0043437678664));
#206770=CARTESIAN_POINT('Ctrl Pts',(-19.6083614943627,59.6951745640082,
39.9661628577646));
#206771=CARTESIAN_POINT('Ctrl Pts',(-19.5568428722492,59.6233361049589,
40.0100243556237));
#206772=CARTESIAN_POINT('Ctrl Pts',(-19.6225475038105,59.791305386369,40.1194874821985));
#206773=CARTESIAN_POINT('Ctrl Pts',(-19.5674227749668,59.7720679362489,
40.0627551483138));
#206774=CARTESIAN_POINT('Ctrl Pts',(-19.5210053955057,59.7110541706153,
40.0767884282375));
#206775=CARTESIAN_POINT('Ctrl Pts',(-19.5524931121158,59.8408924241704,
40.1599502015391));
#206776=CARTESIAN_POINT('Ctrl Pts',(-19.5181549791682,59.8128277376128,
40.1002449453872));
#206777=CARTESIAN_POINT('Ctrl Pts',(-19.4837751174919,59.7499755976288,
40.10025));
#206778=CARTESIAN_POINT('Ctrl Pts',(-19.4684195516691,59.8682321556243,
40.1599502534424));
#206779=CARTESIAN_POINT('Ctrl Pts',(-19.4568831131878,59.8327559231848,
40.10025));
#206780=CARTESIAN_POINT('Ctrl Pts',(-19.4351129318415,59.7658094374953,
40.10025));
#206781=CARTESIAN_POINT('Origin',(-19.6639662938556,59.4920137553141,39.92499));
#206782=CARTESIAN_POINT('Origin',(-18.0520194698729,56.5858547179589,39.6398955069315));
#206783=CARTESIAN_POINT('Origin',(-17.9969682911406,56.4164246115665,39.92499));
#206784=CARTESIAN_POINT('Origin',(-19.6089151909109,59.3225838821518,39.6398955068272));
#206785=CARTESIAN_POINT('Origin',(-19.5538640879527,59.1531540088001,39.3548010137695));
#206786=CARTESIAN_POINT('Ctrl Pts',(-17.9642361803967,56.3138168485097,
39.8576902534424));
#206787=CARTESIAN_POINT('Ctrl Pts',(-18.084621806869,56.2752137607567,39.8579948730703));
#206788=CARTESIAN_POINT('Ctrl Pts',(-18.1177524687101,56.3771794532809,
39.92499));
#206789=CARTESIAN_POINT('Ctrl Pts',(-17.9501961787623,56.2706044454594,
39.930402071123));
#206790=CARTESIAN_POINT('Ctrl Pts',(-18.060896753812,56.2513675234857,39.9058915297379));
#206791=CARTESIAN_POINT('Ctrl Pts',(-18.1037113794371,56.3339654239813,
39.9671523786023));
#206792=CARTESIAN_POINT('Ctrl Pts',(-17.9612588333752,56.2186079213554,
40.0043257306694));
#206793=CARTESIAN_POINT('Ctrl Pts',(-18.0531413250546,56.2138593173285,
39.9667894847835));
#206794=CARTESIAN_POINT('Ctrl Pts',(-18.1041761987731,56.2854146278932,
40.0100138975199));
#206795=CARTESIAN_POINT('Ctrl Pts',(-18.0394175380792,56.1179510603878,
40.1195533054856));
#206796=CARTESIAN_POINT('Ctrl Pts',(-18.0943218653324,56.1373490477013,
40.0630813209237));
#206797=CARTESIAN_POINT('Ctrl Pts',(-18.1403075368577,56.1984140977481,
40.0768265942422));
#206798=CARTESIAN_POINT('Ctrl Pts',(-18.1094153628975,56.0689198620986,
40.1599502027507));
#206799=CARTESIAN_POINT('Ctrl Pts',(-18.1436123520187,56.0970362061498,
40.1002552791544));
#206800=CARTESIAN_POINT('Ctrl Pts',(-18.1777307632117,56.1599674935332,
40.10025));
#206801=CARTESIAN_POINT('Ctrl Pts',(-18.1930767435944,56.0417604764385,
40.1599502534424));
#206802=CARTESIAN_POINT('Ctrl Pts',(-18.204595418534,56.0772424804486,40.10025));
#206803=CARTESIAN_POINT('Ctrl Pts',(-18.2263320786577,56.1441998575529,
40.10025));
#206804=CARTESIAN_POINT('Origin',(-18.2263320786577,56.1441998575529,40.22725));
#206805=CARTESIAN_POINT('Ctrl Pts',(-19.4207352200695,58.7434254837934,
38.989));
#206806=CARTESIAN_POINT('Ctrl Pts',(-19.2997705861184,58.7827292759117,
38.989));
#206807=CARTESIAN_POINT('Ctrl Pts',(-19.2999511771033,58.7826705983438,
39.1161896013267));
#206808=CARTESIAN_POINT('Ctrl Pts',(-19.4879965013594,58.9497137831221,
38.989));
#206809=CARTESIAN_POINT('Ctrl Pts',(-19.3668771285512,58.9892635895131,
38.9887769275436));
#206810=CARTESIAN_POINT('Ctrl Pts',(-19.3535710010434,58.947695446948,39.1161898821825));
#206811=CARTESIAN_POINT('Ctrl Pts',(-19.5520260773864,59.1460976215386,
39.1034967087243));
#206812=CARTESIAN_POINT('Ctrl Pts',(-19.4307447900772,59.1858295778086,
39.1031720232724));
#206813=CARTESIAN_POINT('Ctrl Pts',(-19.4046161500179,59.1047962608432,
39.2077529615019));
#206814=CARTESIAN_POINT('Ctrl Pts',(-19.5876674457073,59.2554138597573,
39.2875012672119));
#206815=CARTESIAN_POINT('Ctrl Pts',(-19.4663243070086,59.2953329133627,
39.2872087095508));
#206816=CARTESIAN_POINT('Ctrl Pts',(-19.4330302514108,59.1922458725044,
39.3549017048228));
#206817=CARTESIAN_POINT('Origin',(-19.4207352200695,58.7434254837934,39.116));
#206818=CARTESIAN_POINT('Origin',(3.93842937138094E-16,5.57863568693718E-17,
40.22725));
#206819=CARTESIAN_POINT('Origin',(-18.2553202812744,56.1347810195644,40.22725));
#206820=CARTESIAN_POINT('Origin',(5.6397553624924,-18.3848338156955,39.116));
#206821=CARTESIAN_POINT('Origin',(-19.2967593024422,58.3616995707148,39.1160373285237));
#206822=CARTESIAN_POINT('Ctrl Pts',(-18.2220120550212,56.0323588238393,
40.1599502534424));
#206823=CARTESIAN_POINT('Ctrl Pts',(-18.2335490499213,56.0678348753334,
40.10025));
#206824=CARTESIAN_POINT('Ctrl Pts',(-18.2553202812744,56.1347810195644,
40.10025));
#206825=CARTESIAN_POINT('Ctrl Pts',(-18.3053742463592,56.0052491386463,
40.1599500566041));
#206826=CARTESIAN_POINT('Ctrl Pts',(-18.2942806848318,56.0480812627856,
40.1002551305372));
#206827=CARTESIAN_POINT('Ctrl Pts',(-18.3037418885554,56.1190241739962,
40.10025));
#206828=CARTESIAN_POINT('Ctrl Pts',(-18.3900709842067,56.0035251343648,
40.1203070619042));
#206829=CARTESIAN_POINT('Ctrl Pts',(-18.3574039607301,56.051456837883,40.0637098684494));
#206830=CARTESIAN_POINT('Ctrl Pts',(-18.3561185603239,56.1278011372725,
40.0772636213361));
#206831=CARTESIAN_POINT('Ctrl Pts',(-18.5134377270384,56.0390077039668,
40.0046102245806));
#206832=CARTESIAN_POINT('Ctrl Pts',(-18.4363968713612,56.0891934462333,
39.9670001894019));
#206833=CARTESIAN_POINT('Ctrl Pts',(-18.4370884086008,56.1770584756116,
40.010178881121));
#206834=CARTESIAN_POINT('Ctrl Pts',(-18.5530236652643,56.0747542753111,
39.9303710930183));
#206835=CARTESIAN_POINT('Ctrl Pts',(-18.452149134841,56.1242585025261,39.9058663574096));
#206836=CARTESIAN_POINT('Ctrl Pts',(-18.466069875907,56.2162483036951,39.9671344706363));
#206837=CARTESIAN_POINT('Ctrl Pts',(-18.567058682946,56.117947944099,39.8576902534424));
#206838=CARTESIAN_POINT('Ctrl Pts',(-18.4469743395774,56.1574782858999,
39.8579948730704));
#206839=CARTESIAN_POINT('Ctrl Pts',(-18.4801050014185,56.259443978424,39.92499));
#206840=CARTESIAN_POINT('Origin',(-18.600889178988,56.2201988201384,39.92499));
#206841=CARTESIAN_POINT('Origin',(-19.2830435998994,58.3196542512046,39.1925554488857));
#206842=CARTESIAN_POINT('Origin',(-19.2577541638573,58.2418213702175,39.3343017080178));
#206843=CARTESIAN_POINT('Origin',(-18.6559403576601,56.3896289265348,39.6398955069222));
#206844=CARTESIAN_POINT('Origin',(-18.7109915363512,56.5590590327991,39.3548010137695));
#206845=CARTESIAN_POINT('Ctrl Pts',(-19.155790878562,57.9280106456677,39.3978017080178));
#206846=CARTESIAN_POINT('Ctrl Pts',(-19.0350067009925,57.9672558039534,
39.3978017080178));
#206847=CARTESIAN_POINT('Ctrl Pts',(-19.0350067009925,57.9672558039534,
39.5248017080178));
#206848=CARTESIAN_POINT('Ctrl Pts',(-19.1833829156718,58.0136880650208,
39.3978017080178));
#206849=CARTESIAN_POINT('Ctrl Pts',(-19.0627953474461,58.0527804636625,
39.3980355775177));
#206850=CARTESIAN_POINT('Ctrl Pts',(-19.0767283413218,58.0956618095388,
39.5248015517192));
#206851=CARTESIAN_POINT('Ctrl Pts',(-19.2094750027316,58.0947019536606,
39.3484893995498));
#206852=CARTESIAN_POINT('Ctrl Pts',(-19.089202668042,58.1340538395312,39.3489438303425));
#206853=CARTESIAN_POINT('Ctrl Pts',(-19.1161791203805,58.2170788227765,
39.4508333155592));
#206854=CARTESIAN_POINT('Ctrl Pts',(-19.2232259141434,58.1373965169895,
39.2708017080178));
#206855=CARTESIAN_POINT('Ctrl Pts',(-19.1031347997382,58.1769325318821,
39.2710850691866));
#206856=CARTESIAN_POINT('Ctrl Pts',(-19.1369699862878,58.2810665285032,
39.3343017080178));
#206857=CARTESIAN_POINT('Origin',(-19.155790878562,57.9280106456677,39.5248017080178));
#206858=CARTESIAN_POINT('Ctrl Pts',(-18.6771643191705,56.4568070719813,
39.2875012672119));
#206859=CARTESIAN_POINT('Ctrl Pts',(-18.5568963159711,56.4963947983081,
39.2878045257519));
#206860=CARTESIAN_POINT('Ctrl Pts',(-18.5902571970796,56.5984571192857,
39.3549015218349));
#206861=CARTESIAN_POINT('Ctrl Pts',(-18.7128129802632,56.5661228951886,
39.1034938540228));
#206862=CARTESIAN_POINT('Ctrl Pts',(-18.5923766197454,56.6055928325716,
39.1038286278827));
#206863=CARTESIAN_POINT('Ctrl Pts',(-18.6186718120038,56.6859083114056,
39.2077506434045));
#206864=CARTESIAN_POINT('Ctrl Pts',(-18.7768537015926,56.7625049710039,
38.989));
#206865=CARTESIAN_POINT('Ctrl Pts',(-18.6561664154737,56.8019192501357,
38.9892298954593));
#206866=CARTESIAN_POINT('Ctrl Pts',(-18.6697173900114,56.843010445685,39.1161900347273));
#206867=CARTESIAN_POINT('Ctrl Pts',(-18.8441205405514,56.9687879773468,
38.989));
#206868=CARTESIAN_POINT('Ctrl Pts',(-18.7231554368002,57.0080919221124,
38.989));
#206869=CARTESIAN_POINT('Ctrl Pts',(-18.7233364982864,57.0080330916693,
39.1161900945648));
#206870=CARTESIAN_POINT('Origin',(-18.8441205405514,56.9687879773468,39.116));
#206871=CARTESIAN_POINT('Origin',(5.49583002221419,-17.9418771653389,39.5248017080178));
#206872=CARTESIAN_POINT('Origin',(-19.109065001131,57.7842031819385,39.5248017080178));
#206873=CARTESIAN_POINT('Origin',(5.4732919481113,-17.8725121057128,39.116));
#206874=CARTESIAN_POINT('Origin',(-18.9681964166823,57.3504898524415,39.1160402713845));
#206875=CARTESIAN_POINT('Ctrl Pts',(-19.0416371860872,57.5748148483578,
39.2708017080178));
#206876=CARTESIAN_POINT('Ctrl Pts',(-18.920459440774,57.6147155869504,39.27051194648));
#206877=CARTESIAN_POINT('Ctrl Pts',(-18.8863175164087,57.5096375484038,
39.3343017080178));
#206878=CARTESIAN_POINT('Ctrl Pts',(-19.0554318862554,57.6176546016064,
39.3487519301186));
#206879=CARTESIAN_POINT('Ctrl Pts',(-18.9342932580167,57.6572916985375,
39.3482879463984));
#206880=CARTESIAN_POINT('Ctrl Pts',(-18.907178645177,57.5738415009809,39.4512271261631));
#206881=CARTESIAN_POINT('Ctrl Pts',(-19.0815664505357,57.6988141606861,
39.3978017080178));
#206882=CARTESIAN_POINT('Ctrl Pts',(-18.9605330155739,57.7380493683893,
39.3975673827392));
#206883=CARTESIAN_POINT('Ctrl Pts',(-18.9466997135537,57.6954748424955,
39.5248015355194));
#206884=CARTESIAN_POINT('Ctrl Pts',(-19.109065001131,57.7842031819385,39.3978017080178));
#206885=CARTESIAN_POINT('Ctrl Pts',(-18.9882808235615,57.8234483402241,
39.3978017080178));
#206886=CARTESIAN_POINT('Ctrl Pts',(-18.9882808235615,57.8234483402241,
39.5248017080178));
#206887=CARTESIAN_POINT('Origin',(-19.0071016939782,57.4703923901182,39.3343017080178));
#206888=CARTESIAN_POINT('Origin',(-18.9819630792879,57.393023688563,39.1934008533546));
#206889=CARTESIAN_POINT('Origin',(-12.4602215063111,60.1478239224134,39.1925554495084));
#206890=CARTESIAN_POINT('Origin',(-12.4693660187272,60.1910940874968,39.1160373285258));
#206891=CARTESIAN_POINT('Origin',(-12.4432063593716,60.0677739512127,39.3343017080178));
#206892=CARTESIAN_POINT('Ctrl Pts',(-12.420896274158,59.9600752506738,39.2708017080178));
#206893=CARTESIAN_POINT('Ctrl Pts',(-12.544666237448,59.9342688867326,39.2710850691866));
#206894=CARTESIAN_POINT('Ctrl Pts',(-12.5674311046648,60.0413691664789,
39.3343017080178));
#206895=CARTESIAN_POINT('Ctrl Pts',(-12.4114257351939,59.9160770362136,
39.3487519293518));
#206896=CARTESIAN_POINT('Ctrl Pts',(-12.5352608058714,59.8900198101348,
39.3492068662926));
#206897=CARTESIAN_POINT('Ctrl Pts',(-12.5533954010684,59.9753363727317,
39.4512271248741));
#206898=CARTESIAN_POINT('Ctrl Pts',(-12.3934832896268,59.832722693313,39.3978017080178));
#206899=CARTESIAN_POINT('Ctrl Pts',(-12.5174621766263,59.8062838430892,
39.3980347781178));
#206900=CARTESIAN_POINT('Ctrl Pts',(-12.5268049860492,59.8502383056087,
39.524801535519));
#206901=CARTESIAN_POINT('Ctrl Pts',(-12.3746037924158,59.7450242491249,
39.3978017080178));
#206902=CARTESIAN_POINT('Ctrl Pts',(-12.498828537709,59.718619464391,39.3978017080178));
#206903=CARTESIAN_POINT('Ctrl Pts',(-12.498828537709,59.718619464391,39.5248017080178));
#206904=CARTESIAN_POINT('Origin',(-12.3746037924158,59.7450242491249,39.5248017080178));
#206905=CARTESIAN_POINT('Origin',(0.31056186323299,0.0660119618346354,39.116));
#206906=CARTESIAN_POINT('Origin',(-12.5528626811441,60.5836663843183,39.116));
#206907=CARTESIAN_POINT('Origin',(0.31056186323299,0.0660119618346354,39.5248017080178));
#206908=CARTESIAN_POINT('Origin',(-12.3431658574205,59.597120393566,39.5248017080178));
#206909=CARTESIAN_POINT('Ctrl Pts',(-12.6642893210135,61.1105274371642,
39.2875012672119));
#206910=CARTESIAN_POINT('Ctrl Pts',(-12.7893350777075,61.0844267845858,
39.287208709576));
#206911=CARTESIAN_POINT('Ctrl Pts',(-12.7666250679672,60.9785037674415,
39.3549016990121));
#206912=CARTESIAN_POINT('Ctrl Pts',(-12.6404971713777,60.9980344071776,
39.1034939173931));
#206913=CARTESIAN_POINT('Ctrl Pts',(-12.7653958126085,60.9718026486694,
39.1031692336342));
#206914=CARTESIAN_POINT('Ctrl Pts',(-12.747507305352,60.888561765193,39.2077507202298));
#206915=CARTESIAN_POINT('Ctrl Pts',(-12.5977561540109,60.7959446297927,
38.989));
#206916=CARTESIAN_POINT('Ctrl Pts',(-12.7224234952038,60.7696360759178,
38.9887769311182));
#206917=CARTESIAN_POINT('Ctrl Pts',(-12.7131630221041,60.7269846150126,
39.1161898712912));
#206918=CARTESIAN_POINT('Ctrl Pts',(-12.5528626811441,60.5836663843183,
38.989));
#206919=CARTESIAN_POINT('Ctrl Pts',(-12.6772730124459,60.5572221520606,
38.989));
#206920=CARTESIAN_POINT('Ctrl Pts',(-12.6770872880158,60.5572616290068,
39.1161895903851));
#206921=CARTESIAN_POINT('Origin',(-12.6424339620836,61.0050661295708,39.3548010137695));
#206922=CARTESIAN_POINT('Ctrl Pts',(-12.3431658574205,59.597120393566,39.3978017080178));
#206923=CARTESIAN_POINT('Ctrl Pts',(-12.4673906027137,59.5707156088322,
39.3978017080178));
#206924=CARTESIAN_POINT('Ctrl Pts',(-12.4673906027137,59.5707156088322,
39.5248017080178));
#206925=CARTESIAN_POINT('Ctrl Pts',(-12.3242219811461,59.5091256622727,
39.3978017080178));
#206926=CARTESIAN_POINT('Ctrl Pts',(-12.448658367964,59.4825873732114,39.397566602504));
#206927=CARTESIAN_POINT('Ctrl Pts',(-12.4393195978188,59.4386519140005,
39.5248015517196));
#206928=CARTESIAN_POINT('Ctrl Pts',(-12.3063073021287,59.4259203549058,
39.3484894016716));
#206929=CARTESIAN_POINT('Ctrl Pts',(-12.4310355281329,59.3996784303299,
39.3480259000028));
#206930=CARTESIAN_POINT('Ctrl Pts',(-12.4127764613281,59.3137762748665,
39.4508333188936));
#206931=CARTESIAN_POINT('Ctrl Pts',(-12.2968658913797,59.3820708699072,
39.2708017080178));
#206932=CARTESIAN_POINT('Ctrl Pts',(-12.4217592664906,59.3560370505015,
39.27051194648));
#206933=CARTESIAN_POINT('Ctrl Pts',(-12.3987880210518,59.2479658375578,
39.3343017080178));
#206934=CARTESIAN_POINT('Origin',(-12.2745632757586,59.2743706222916,39.3343017080178));
#206935=CARTESIAN_POINT('Origin',(-12.6794732450919,61.1793222555445,39.6398955068197));
#206936=CARTESIAN_POINT('Origin',(-12.716512528016,61.3535783813233,39.92499));
#206937=CARTESIAN_POINT('Origin',(-12.25764960399,59.1947980527935,39.1934008539946));
#206938=CARTESIAN_POINT('Origin',(-12.2483049653994,59.1510793400374,39.1160402713848));
#206939=CARTESIAN_POINT('Ctrl Pts',(-13.0739701745318,61.5816197022699,
40.1599502534424));
#206940=CARTESIAN_POINT('Ctrl Pts',(-13.066222907106,61.545128164506,40.10025));
#206941=CARTESIAN_POINT('Ctrl Pts',(-13.0516031943522,61.4762657165317,
40.10025));
#206942=CARTESIAN_POINT('Ctrl Pts',(-12.9877758510414,61.5999188988203,
40.1599500538471));
#206943=CARTESIAN_POINT('Ctrl Pts',(-13.0034370926704,61.5584544893691,
40.100244835349));
#206944=CARTESIAN_POINT('Ctrl Pts',(-13.0017087032037,61.4868491822358,
40.10025));
#206945=CARTESIAN_POINT('Ctrl Pts',(-12.9030451317656,61.5923336062397,
40.1202442001039));
#206946=CARTESIAN_POINT('Ctrl Pts',(-12.9408103617797,61.5481051179917,
40.0633873868017));
#206947=CARTESIAN_POINT('Ctrl Pts',(-12.9504709278434,61.4721451382826,
40.0772271723538));
#206948=CARTESIAN_POINT('Ctrl Pts',(-12.7836101409423,61.543429955208,40.0045995998162));
#206949=CARTESIAN_POINT('Ctrl Pts',(-12.8662000075457,61.5018471007596,
39.9663485808314));
#206950=CARTESIAN_POINT('Ctrl Pts',(-12.8749747009092,61.4139027244671,
40.0101727202465));
#206951=CARTESIAN_POINT('Ctrl Pts',(-12.7478263086949,61.5035207735037,
39.9304654349859));
#206952=CARTESIAN_POINT('Ctrl Pts',(-12.8544221781243,61.4652971063446,
39.9051900162944));
#206953=CARTESIAN_POINT('Ctrl Pts',(-12.8501918100166,61.3716536946544,
39.9671857458169));
#206954=CARTESIAN_POINT('Ctrl Pts',(-12.7383709431244,61.459039055521,39.8576902534424));
#206955=CARTESIAN_POINT('Ctrl Pts',(-12.8632261535949,61.43297545991,39.8573998014387));
#206956=CARTESIAN_POINT('Ctrl Pts',(-12.8407372733092,61.3271735965895,
39.92499));
#206957=CARTESIAN_POINT('Origin',(-13.0516031943522,61.4762657165317,40.22725));
#206958=CARTESIAN_POINT('Origin',(0.31056186323299,0.0660119618346354,39.116));
#206959=CARTESIAN_POINT('Origin',(-12.1649068885786,58.7584778814678,39.116));
#206960=CARTESIAN_POINT('Origin',(4.07480739539809E-18,-1.61286359594752E-16,
40.22725));
#206961=CARTESIAN_POINT('Origin',(-13.0814171332226,61.4699285681956,40.22725));
#206962=CARTESIAN_POINT('Ctrl Pts',(-12.1649068885786,58.7584778814678,
38.989));
#206963=CARTESIAN_POINT('Ctrl Pts',(-12.28931772815,58.732033541174,38.989));
#206964=CARTESIAN_POINT('Ctrl Pts',(-12.2891314946916,58.7320731263176,
39.1161901092324));
#206965=CARTESIAN_POINT('Ctrl Pts',(-12.1200194799675,58.5461948427483,
38.989));
#206966=CARTESIAN_POINT('Ctrl Pts',(-12.2442448876963,58.5199849720741,
38.9892298989736));
#206967=CARTESIAN_POINT('Ctrl Pts',(-12.2530551225939,58.5623471386696,
39.1161900493204));
#206968=CARTESIAN_POINT('Ctrl Pts',(-12.0772896710125,58.3441042111268,
39.1034966344368));
#206969=CARTESIAN_POINT('Ctrl Pts',(-12.2013256001473,58.3180679977581,
39.1038314102574));
#206970=CARTESIAN_POINT('Ctrl Pts',(-12.218711094921,58.4007711908091,39.2077528789597));
#206971=CARTESIAN_POINT('Ctrl Pts',(-12.0535047649316,58.2316113004782,
39.2875012672119));
#206972=CARTESIAN_POINT('Ctrl Pts',(-12.1774537884111,58.2057612725768,
39.2878045257868));
#206973=CARTESIAN_POINT('Ctrl Pts',(-12.1995935666432,58.3108302909897,
39.3549015295901));
#206974=CARTESIAN_POINT('Origin',(-12.0753355159227,58.3370777047236,39.3548010137695));
#206975=CARTESIAN_POINT('Ctrl Pts',(-13.360562319248,61.3267881959114,39.8576902534424));
#206976=CARTESIAN_POINT('Ctrl Pts',(-13.2359003894744,61.3537611057084,
39.8573998014387));
#206977=CARTESIAN_POINT('Ctrl Pts',(-13.2134115091888,61.2479592423879,
39.92499));
#206978=CARTESIAN_POINT('Ctrl Pts',(-13.3700210384232,61.3712903180781,
39.9304984902491));
#206979=CARTESIAN_POINT('Ctrl Pts',(-13.2571016411962,61.3797222373784,
39.9052171569785));
#206980=CARTESIAN_POINT('Ctrl Pts',(-13.2228703539489,61.2924596082476,
39.9672049726597));
#206981=CARTESIAN_POINT('Ctrl Pts',(-13.3535190881765,61.4221282572892,
40.0043437678663));
#206982=CARTESIAN_POINT('Ctrl Pts',(-13.2610999767698,61.4177900459397,
39.9661628577642));
#206983=CARTESIAN_POINT('Ctrl Pts',(-13.2173727427866,61.3409599630863,
40.0100243556236));
#206984=CARTESIAN_POINT('Ctrl Pts',(-13.2651598666396,61.5148770953649,
40.1194874821987));
#206985=CARTESIAN_POINT('Ctrl Pts',(-13.2123479779264,61.4899829268152,
40.062755148314));
#206986=CARTESIAN_POINT('Ctrl Pts',(-13.1725625528865,61.42445146363,40.0767884282376));
#206987=CARTESIAN_POINT('Ctrl Pts',(-13.1903059833729,61.5568698122756,
40.1599502015388));
#206988=CARTESIAN_POINT('Ctrl Pts',(-13.1590895168684,61.5253695547385,
40.1002449453881));
#206989=CARTESIAN_POINT('Ctrl Pts',(-13.1314678292774,61.4592680512459,
40.10025));
#206990=CARTESIAN_POINT('Ctrl Pts',(-13.1038352065721,61.5752716937453,
40.1599502534424));
#206991=CARTESIAN_POINT('Ctrl Pts',(-13.0960702419674,61.5387839176329,
40.10025));
#206992=CARTESIAN_POINT('Ctrl Pts',(-13.0814171332226,61.4699285681956,
40.10025));
#206993=CARTESIAN_POINT('Origin',(-13.3376362544819,61.221554457654,39.92499));
#206994=CARTESIAN_POINT('Origin',(-12.0382961820468,58.1628213392039,39.6398955069326));
#206995=CARTESIAN_POINT('Origin',(-12.0012568480854,57.9885649735461,39.92499));
#206996=CARTESIAN_POINT('Origin',(-13.300596971511,61.0472983318734,39.6398955068269));
#206997=CARTESIAN_POINT('Origin',(-13.2635576885496,60.8730422059015,39.3548010137695));
#206998=CARTESIAN_POINT('Ctrl Pts',(-11.9794294790606,57.8830978693157,
39.8576902534424));
#206999=CARTESIAN_POINT('Ctrl Pts',(-12.1031907419151,57.8572899778512,
39.8579948730703));
#207000=CARTESIAN_POINT('Ctrl Pts',(-12.1254815933786,57.9621601888122,
39.92499));
#207001=CARTESIAN_POINT('Ctrl Pts',(-11.9699833161084,57.8386546085356,
39.9304020711231));
#207002=CARTESIAN_POINT('Ctrl Pts',(-12.0820882677171,57.8310944294267,
39.9058915297383));
#207003=CARTESIAN_POINT('Ctrl Pts',(-12.1160345187361,57.9177151970029,
39.9671523786031));
#207004=CARTESIAN_POINT('Ctrl Pts',(-11.9864204851024,57.7880992891177,
40.0043257306692));
#207005=CARTESIAN_POINT('Ctrl Pts',(-12.0782959991605,57.7929810340973,
39.9667894847835));
#207006=CARTESIAN_POINT('Ctrl Pts',(-12.1215717318488,57.8694789541064,
40.0100138975199));
#207007=CARTESIAN_POINT('Ctrl Pts',(-12.0746725352384,57.6961636462597,
40.1195533054858));
#207008=CARTESIAN_POINT('Ctrl Pts',(-12.1272484490375,57.7211944343233,
40.0630813209236));
#207009=CARTESIAN_POINT('Ctrl Pts',(-12.1665991704021,57.7867317752136,
40.0768265942421));
#207010=CARTESIAN_POINT('Ctrl Pts',(-12.1494120604577,57.6547178110651,
40.1599502027512));
#207011=CARTESIAN_POINT('Ctrl Pts',(-12.180482756658,57.6862546895627,40.100255279155));
#207012=CARTESIAN_POINT('Ctrl Pts',(-12.2078361528627,57.7524075778595,
40.10025));
#207013=CARTESIAN_POINT('Ctrl Pts',(-12.2354540642039,57.6364522029208,
40.1599502534424));
#207014=CARTESIAN_POINT('Ctrl Pts',(-12.2432007592841,57.6729438621907,
40.10025));
#207015=CARTESIAN_POINT('Ctrl Pts',(-12.2578193919762,57.7418065394567,
40.10025));
#207016=CARTESIAN_POINT('Origin',(-12.2578193919762,57.7418065394567,40.22725));
#207017=CARTESIAN_POINT('Ctrl Pts',(-13.1739864076101,60.451642460649,38.989));
#207018=CARTESIAN_POINT('Ctrl Pts',(-13.0495760655898,60.478086695185,38.989));
#207019=CARTESIAN_POINT('Ctrl Pts',(-13.0497618007543,60.4780472159571,
39.1161896013266));
#207020=CARTESIAN_POINT('Ctrl Pts',(-13.2193162256439,60.6638314094604,
38.989));
#207021=CARTESIAN_POINT('Ctrl Pts',(-13.0947262769505,60.6905041359636,
38.988776927546));
#207022=CARTESIAN_POINT('Ctrl Pts',(-13.085838095863,60.647772838971,39.1161898821848));
#207023=CARTESIAN_POINT('Ctrl Pts',(-13.2624673401135,60.8658323498479,
39.1034967087243));
#207024=CARTESIAN_POINT('Ctrl Pts',(-13.1376973240554,60.8926693037162,
39.1031720232711));
#207025=CARTESIAN_POINT('Ctrl Pts',(-13.1201821075158,60.8093487091495,
39.2077529615));
#207026=CARTESIAN_POINT('Ctrl Pts',(-13.2864868028989,60.9782752797349,
39.2875012672119));
#207027=CARTESIAN_POINT('Ctrl Pts',(-13.161635717282,61.0052918407716,39.2872087095508));
#207028=CARTESIAN_POINT('Ctrl Pts',(-13.139299579968,60.8992893450419,39.3549017048228));
#207029=CARTESIAN_POINT('Origin',(-13.1739864076101,60.451642460649,39.116));
#207030=CARTESIAN_POINT('Origin',(3.9977349588932E-16,5.73754452974297E-17,
40.22725));
#207031=CARTESIAN_POINT('Origin',(-12.2876333308465,57.7354693911206,40.22725));
#207032=CARTESIAN_POINT('Origin',(2.37914510404509,-12.7200883457656,39.116));
#207033=CARTESIAN_POINT('Origin',(-13.0905908661173,60.0590486699123,39.1160373285265));
#207034=CARTESIAN_POINT('Ctrl Pts',(-12.2652136052655,57.6301266171959,
40.1599502534424));
#207035=CARTESIAN_POINT('Ctrl Pts',(-12.2729791421549,57.6666142715156,
40.10025));
#207036=CARTESIAN_POINT('Ctrl Pts',(-12.2876333308465,57.7354693911206,
40.10025));
#207037=CARTESIAN_POINT('Ctrl Pts',(-12.3509528635302,57.6118791634504,
40.1599500566036));
#207038=CARTESIAN_POINT('Ctrl Pts',(-12.3354428975791,57.6533170557961,
40.1002551305363));
#207039=CARTESIAN_POINT('Ctrl Pts',(-12.3374367183502,57.7248602994012,
40.10025));
#207040=CARTESIAN_POINT('Ctrl Pts',(-12.4353658313035,57.6190178232954,
40.1203070619044));
#207041=CARTESIAN_POINT('Ctrl Pts',(-12.3978675338892,57.6632723181628,
40.0637098684499));
#207042=CARTESIAN_POINT('Ctrl Pts',(-12.3886090227463,57.7390640345635,
40.0772636213363));
#207043=CARTESIAN_POINT('Ctrl Pts',(-12.5543478197371,57.6672013517152,
40.0046102245803));
#207044=CARTESIAN_POINT('Ctrl Pts',(-12.4724831634109,57.709059208982,39.9670001894012));
#207045=CARTESIAN_POINT('Ctrl Pts',(-12.4639865158414,57.7965151898603,
40.0101788811208));
#207046=CARTESIAN_POINT('Ctrl Pts',(-12.5899803678808,57.7068899568911,
39.9303710930185));
#207047=CARTESIAN_POINT('Ctrl Pts',(-12.4844838378932,57.7455787351226,
39.905866357411));
#207048=CARTESIAN_POINT('Ctrl Pts',(-12.4887127671319,57.838519720206,39.9671344706364));
#207049=CARTESIAN_POINT('Ctrl Pts',(-12.5994235324466,57.7513140650721,
39.8576902534424));
#207050=CARTESIAN_POINT('Ctrl Pts',(-12.4758649777947,57.7780756236497,
39.8579948730703));
#207051=CARTESIAN_POINT('Ctrl Pts',(-12.4981558292581,57.8829458346106,
39.92499));
#207052=CARTESIAN_POINT('Origin',(-12.6223805745513,57.8565410498768,39.92499));
#207053=CARTESIAN_POINT('Origin',(-13.0813452322613,60.01579999775,39.192555448885));
#207054=CARTESIAN_POINT('Origin',(-13.0643300858376,59.9357500275434,39.3343017080178));
#207055=CARTESIAN_POINT('Origin',(-12.6594199084536,58.03079741553,39.639895506922));
#207056=CARTESIAN_POINT('Origin',(-12.6964592423886,58.2050537810543,39.3548010137695));
#207057=CARTESIAN_POINT('Ctrl Pts',(-12.9957275188818,59.6130003254556,
39.3978017080178));
#207058=CARTESIAN_POINT('Ctrl Pts',(-12.8715027735886,59.6394051101895,
39.3978017080178));
#207059=CARTESIAN_POINT('Ctrl Pts',(-12.8715027735886,59.6394051101895,
39.5248017080178));
#207060=CARTESIAN_POINT('Ctrl Pts',(-13.0142126749433,59.7010925481785,
39.3978017080178));
#207061=CARTESIAN_POINT('Ctrl Pts',(-12.8901994296779,59.727365961373,39.3980355775177));
#207062=CARTESIAN_POINT('Ctrl Pts',(-12.8995737759685,59.7714687931892,
39.5248015517192));
#207063=CARTESIAN_POINT('Ctrl Pts',(-13.0316935695382,59.7843900000233,
39.3484893995498));
#207064=CARTESIAN_POINT('Ctrl Pts',(-12.9079667071272,59.8109544298284,
39.348943830343));
#207065=CARTESIAN_POINT('Ctrl Pts',(-12.9261169057236,59.896344400635,39.4508333155594));
#207066=CARTESIAN_POINT('Ctrl Pts',(-13.0409063549232,59.8282880397056,
39.2708017080178));
#207067=CARTESIAN_POINT('Ctrl Pts',(-12.9173404733276,59.855054532531,39.2710850691866));
#207068=CARTESIAN_POINT('Ctrl Pts',(-12.9401053405444,59.9621548122773,
39.3343017080178));
#207069=CARTESIAN_POINT('Origin',(-12.9957275188818,59.6130003254556,39.5248017080178));
#207070=CARTESIAN_POINT('Ctrl Pts',(-12.6735055745735,58.0998260601481,
39.2875012672119));
#207071=CARTESIAN_POINT('Ctrl Pts',(-12.5497583678825,58.1266254912132,
39.2878045257519));
#207072=CARTESIAN_POINT('Ctrl Pts',(-12.5722680770241,58.2316158657529,
39.3549015218347));
#207073=CARTESIAN_POINT('Ctrl Pts',(-12.697532333562,58.2122693395992,39.1034938540228));
#207074=CARTESIAN_POINT('Ctrl Pts',(-12.5736300041235,58.2389340288477,
39.1038286278794));
#207075=CARTESIAN_POINT('Ctrl Pts',(-12.5913858949916,58.3215581271253,
39.2077506434031));
#207076=CARTESIAN_POINT('Ctrl Pts',(-12.7406947165199,58.4142696920427,
38.989));
#207077=CARTESIAN_POINT('Ctrl Pts',(-12.6165486539538,58.4408527990771,
38.9892298954629));
#207078=CARTESIAN_POINT('Ctrl Pts',(-12.6257301953094,58.4831353553,39.1161900347289));
#207079=CARTESIAN_POINT('Ctrl Pts',(-12.7860306150445,58.6264539577985,
38.989));
#207080=CARTESIAN_POINT('Ctrl Pts',(-12.6616197898419,58.6528982950381,
38.989));
#207081=CARTESIAN_POINT('Ctrl Pts',(-12.66180600891,58.6528587129533,39.1161900945646));
#207082=CARTESIAN_POINT('Origin',(-12.7860306150445,58.6264539577985,39.116));
#207083=CARTESIAN_POINT('Origin',(2.31399271319931,-12.4135704460881,39.5248017080178));
#207084=CARTESIAN_POINT('Origin',(-12.9642895838864,59.4650964698968,39.5248017080178));
#207085=CARTESIAN_POINT('Origin',(2.30379013587677,-12.3655710936221,39.116));
#207086=CARTESIAN_POINT('Origin',(-12.8695280801141,59.0190342907435,39.1160402713851));
#207087=CARTESIAN_POINT('Ctrl Pts',(-12.9191181862039,59.2498070616281,
39.2708017080178));
#207088=CARTESIAN_POINT('Ctrl Pts',(-12.7944335023702,59.2768226962999,
39.27051194648));
#207089=CARTESIAN_POINT('Ctrl Pts',(-12.7714622569314,59.1687514833562,
39.3343017080178));
#207090=CARTESIAN_POINT('Ctrl Pts',(-12.9283593439867,59.293854073036,39.3487519301186));
#207091=CARTESIAN_POINT('Ctrl Pts',(-12.8037411210015,59.3206115991496,
39.3482879463984));
#207092=CARTESIAN_POINT('Ctrl Pts',(-12.7854979657552,59.2347843016968,
39.4512271261627));
#207093=CARTESIAN_POINT('Ctrl Pts',(-12.9458672563998,59.3773008374015,
39.3978017080178));
#207094=CARTESIAN_POINT('Ctrl Pts',(-12.821395659292,59.4036696715712,39.3975673827392));
#207095=CARTESIAN_POINT('Ctrl Pts',(-12.8120883873131,59.3598823995816,
39.5248015355194));
#207096=CARTESIAN_POINT('Ctrl Pts',(-12.9642895838864,59.4650964698968,
39.3978017080178));
#207097=CARTESIAN_POINT('Ctrl Pts',(-12.8400648385932,59.4915012546306,
39.3978017080178));
#207098=CARTESIAN_POINT('Ctrl Pts',(-12.8400648385932,59.4915012546306,
39.5248017080178));
#207099=CARTESIAN_POINT('Origin',(-12.8956870022246,59.1423466986223,39.3343017080178));
#207100=CARTESIAN_POINT('Origin',(-12.8787733309733,59.0627741301469,39.193400853355));
#207101=CARTESIAN_POINT('Origin',(-6.10480350566275,61.1207756556245,39.1925554495081));
#207102=CARTESIAN_POINT('Origin',(-6.10937495962055,61.1647646440466,39.116037328525));
#207103=CARTESIAN_POINT('Origin',(-6.09624906995176,61.0393856393804,39.3343017080178));
#207104=CARTESIAN_POINT('Ctrl Pts',(-6.08531878138258,60.9299448846691,
39.2708017080178));
#207105=CARTESIAN_POINT('Ctrl Pts',(-6.21110821942872,60.9172173747511,
39.2710850691866));
#207106=CARTESIAN_POINT('Ctrl Pts',(-6.22255335066354,61.0261105245455,
39.3343017080178));
#207107=CARTESIAN_POINT('Ctrl Pts',(-6.08049918876613,60.885197756147,39.3487519293518));
#207108=CARTESIAN_POINT('Ctrl Pts',(-6.20637959976764,60.8722275639175,
39.349206866293));
#207109=CARTESIAN_POINT('Ctrl Pts',(-6.2154968425757,60.9589723348237,39.4512271248741));
#207110=CARTESIAN_POINT('Ctrl Pts',(-6.0713679351625,60.800424540796,39.3978017080178));
#207111=CARTESIAN_POINT('Ctrl Pts',(-6.19743126523124,60.7870898478945,
39.3980347781178));
#207112=CARTESIAN_POINT('Ctrl Pts',(-6.2021284013463,60.8317801127822,39.524801535519));
#207113=CARTESIAN_POINT('Ctrl Pts',(-6.06175884541508,60.7112330730304,
39.3978017080178));
#207114=CARTESIAN_POINT('Ctrl Pts',(-6.18806312612685,60.6979579581955,
39.3978017080178));
#207115=CARTESIAN_POINT('Ctrl Pts',(-6.18806312612685,60.6979579581955,
39.5248017080178));
#207116=CARTESIAN_POINT('Origin',(-6.06175884541508,60.7112330730304,39.5248017080178));
#207117=CARTESIAN_POINT('Origin',(0.315760701779433,0.0331877870874769,
39.116));
#207118=CARTESIAN_POINT('Origin',(-6.15137923967613,61.5639141665612,39.116));
#207119=CARTESIAN_POINT('Origin',(0.315760701779433,0.0331877870874769,
39.5248017080178));
#207120=CARTESIAN_POINT('Origin',(-6.04595329344999,60.5608532912344,39.5248017080178));
#207121=CARTESIAN_POINT('Ctrl Pts',(-6.207123496544,62.0995362748659,39.2875012672119));
#207122=CARTESIAN_POINT('Ctrl Pts',(-6.33421250060359,62.0866494451786,
39.287208709576));
#207123=CARTESIAN_POINT('Ctrl Pts',(-6.32269886887937,61.978932842986,39.3549016990122));
#207124=CARTESIAN_POINT('Ctrl Pts',(-6.19522040634688,61.9851725366286,
39.1034939173931));
#207125=CARTESIAN_POINT('Ctrl Pts',(-6.32217680516144,61.9721399414732,
39.1031692336336));
#207126=CARTESIAN_POINT('Ctrl Pts',(-6.31308733464659,61.8874852020914,
39.2077507202295));
#207127=CARTESIAN_POINT('Ctrl Pts',(-6.17383766261612,61.7797221753254,
38.989));
#207128=CARTESIAN_POINT('Ctrl Pts',(-6.30057205577764,61.7665890280533,
38.9887769311176));
#207129=CARTESIAN_POINT('Ctrl Pts',(-6.29582060418292,61.7232032332924,
39.1161898712914));
#207130=CARTESIAN_POINT('Ctrl Pts',(-6.15137923967613,61.5639141665612,
38.989));
#207131=CARTESIAN_POINT('Ctrl Pts',(-6.2778722131262,61.5506192193203,38.989));
#207132=CARTESIAN_POINT('Ctrl Pts',(-6.27768337964921,61.5506390665185,
39.1161895903853));
#207133=CARTESIAN_POINT('Origin',(-6.19641157197401,61.9923681882669,39.3548010137695));
#207134=CARTESIAN_POINT('Ctrl Pts',(-6.04595329344999,60.5608532912344,
39.3978017080178));
#207135=CARTESIAN_POINT('Ctrl Pts',(-6.17225757416176,60.5475781763994,
39.3978017080178));
#207136=CARTESIAN_POINT('Ctrl Pts',(-6.17225757416176,60.5475781763994,
39.5248017080178));
#207137=CARTESIAN_POINT('Ctrl Pts',(-6.03631114774952,60.4713604300109,
39.3978017080178));
#207138=CARTESIAN_POINT('Ctrl Pts',(-6.16283986559437,60.4579746647649,
39.397566602504));
#207139=CARTESIAN_POINT('Ctrl Pts',(-6.158144760243,60.4133037213017,39.5248015517196));
#207140=CARTESIAN_POINT('Ctrl Pts',(-6.0271919301333,60.3867383361559,39.3484894016716));
#207141=CARTESIAN_POINT('Ctrl Pts',(-6.15397990991402,60.3736778173757,
39.3480259000036));
#207142=CARTESIAN_POINT('Ctrl Pts',(-6.14480008848961,60.286337650718,39.4508333188934));
#207143=CARTESIAN_POINT('Ctrl Pts',(-6.02238575970214,60.3421421670676,
39.2708017080178));
#207144=CARTESIAN_POINT('Ctrl Pts',(-6.14931623097185,60.3293058762212,
39.27051194648));
#207145=CARTESIAN_POINT('Ctrl Pts',(-6.13776734223154,60.2194255397046,
39.3343017080178));
#207146=CARTESIAN_POINT('Origin',(-6.01146306151977,60.2327006545396,39.3343017080178));
#207147=CARTESIAN_POINT('Origin',(-6.21503322485447,62.169541380285,39.6398955068184));
#207148=CARTESIAN_POINT('Origin',(-6.23365487766561,62.346714572097,39.92499));
#207149=CARTESIAN_POINT('Origin',(-6.00295964302103,60.1517960317845,39.1934008539949));
#207150=CARTESIAN_POINT('Origin',(-5.99823604520081,60.107340034,39.1160402713845));
#207151=CARTESIAN_POINT('Ctrl Pts',(-6.56531752495238,62.6108711573006,
40.1599502534424));
#207152=CARTESIAN_POINT('Ctrl Pts',(-6.56142710223288,62.5737697140403,
40.10025));
#207153=CARTESIAN_POINT('Ctrl Pts',(-6.55408556365883,62.5037563256535,
40.10025));
#207154=CARTESIAN_POINT('Ctrl Pts',(-6.47768259609018,62.6200603487606,
40.1599500538468));
#207155=CARTESIAN_POINT('Ctrl Pts',(-6.49759225479899,62.5804601312023,
40.100244835349));
#207156=CARTESIAN_POINT('Ctrl Pts',(-6.50335812634711,62.5090664195381,
40.10025));
#207157=CARTESIAN_POINT('Ctrl Pts',(-6.39420891953703,62.603659837329,40.1202442001038));
#207158=CARTESIAN_POINT('Ctrl Pts',(-6.43639040357899,62.5636211788254,
40.0633873868015));
#207159=CARTESIAN_POINT('Ctrl Pts',(-6.45393802799966,62.4890871199578,
40.0772271723538));
#207160=CARTESIAN_POINT('Ctrl Pts',(-6.28054002958072,62.5425397295636,
40.0045995998163));
#207161=CARTESIAN_POINT('Ctrl Pts',(-6.36702405212707,62.5098176621808,
39.9663485808318));
#207162=CARTESIAN_POINT('Ctrl Pts',(-6.38494336730917,62.4232722595963,
40.0101727202465));
#207163=CARTESIAN_POINT('Ctrl Pts',(-6.24912387034407,62.4991087455376,
39.9304654349858));
#207164=CARTESIAN_POINT('Ctrl Pts',(-6.35913125763593,62.4722367740482,
39.9051900162944));
#207165=CARTESIAN_POINT('Ctrl Pts',(-6.36471246584663,62.3786641568873,
39.967185745818));
#207166=CARTESIAN_POINT('Ctrl Pts',(-6.24436990787996,62.4538823482276,
39.8576902534424));
#207167=CARTESIAN_POINT('Ctrl Pts',(-6.37126553604008,62.4410124550019,
39.8573998014387));
#207168=CARTESIAN_POINT('Ctrl Pts',(-6.35995915837738,62.333439457262,39.92499));
#207169=CARTESIAN_POINT('Origin',(-6.55408556365882,62.5037563256535,40.22725));
#207170=CARTESIAN_POINT('Origin',(0.315760701779433,0.0331877870874769,
39.116));
#207171=CARTESIAN_POINT('Origin',(-5.9563328589115,59.7081718144893,39.116));
#207172=CARTESIAN_POINT('Origin',(-1.29720108988958E-17,-1.63986310369608E-16,
40.22725));
#207173=CARTESIAN_POINT('Origin',(-6.58439859102965,62.5005702980931,40.22725));
#207174=CARTESIAN_POINT('Ctrl Pts',(-5.9563328589115,59.7081718144893,38.989));
#207175=CARTESIAN_POINT('Ctrl Pts',(-6.08282634913902,59.6948768129328,
38.989));
#207176=CARTESIAN_POINT('Ctrl Pts',(-6.08263699811321,59.6948967145276,
39.116190109232));
#207177=CARTESIAN_POINT('Ctrl Pts',(-5.93388096803544,59.4923596726254,
38.989));
#207178=CARTESIAN_POINT('Ctrl Pts',(-6.06016553348636,59.4792784733305,
38.9892298989736));
#207179=CARTESIAN_POINT('Ctrl Pts',(-6.06449945282174,59.5223294958602,
39.11619004932));
#207180=CARTESIAN_POINT('Ctrl Pts',(-5.91250946061117,59.286909633363,39.1034966344368));
#207181=CARTESIAN_POINT('Ctrl Pts',(-6.03858743331817,59.2739813341626,
39.1038314102587));
#207182=CARTESIAN_POINT('Ctrl Pts',(-6.0472328508574,59.358048749519,39.2077528789603));
#207183=CARTESIAN_POINT('Ctrl Pts',(-5.90061356181196,59.1725467709678,
39.2875012672119));
#207184=CARTESIAN_POINT('Ctrl Pts',(-6.02658564326333,59.1597945531718,
39.2878045257868));
#207185=CARTESIAN_POINT('Ctrl Pts',(-6.03762143444243,59.2666022295036,
39.3549015295898));
#207186=CARTESIAN_POINT('Origin',(-5.91130048050282,59.2797173540686,39.3548010137695));
#207187=CARTESIAN_POINT('Ctrl Pts',(-6.87697683366501,62.3873926810692,
39.8576902534424));
#207188=CARTESIAN_POINT('Ctrl Pts',(-6.75017837817539,62.4011871104969,
39.8573998014387));
#207189=CARTESIAN_POINT('Ctrl Pts',(-6.7388720005127,62.293614112757,39.92499));
#207190=CARTESIAN_POINT('Ctrl Pts',(-6.88173199854425,62.4326397213343,
39.9304984902493));
#207191=CARTESIAN_POINT('Ctrl Pts',(-6.76854981002517,62.4292221586323,
39.9052171569784));
#207192=CARTESIAN_POINT('Ctrl Pts',(-6.7436274738735,62.338859419464,39.9672049726588));
#207193=CARTESIAN_POINT('Ctrl Pts',(-6.86000643604672,62.4814742414946,
40.004343767866));
#207194=CARTESIAN_POINT('Ctrl Pts',(-6.76854707276804,62.4674993676295,
39.966162857764));
#207195=CARTESIAN_POINT('Ctrl Pts',(-6.73309031164129,62.3865194274377,
40.0100243556234));
#207196=CARTESIAN_POINT('Ctrl Pts',(-6.76243636205631,62.5644789380885,
40.1194874821989));
#207197=CARTESIAN_POINT('Ctrl Pts',(-6.71251593157802,62.5342007968288,
40.0627551483144));
#207198=CARTESIAN_POINT('Ctrl Pts',(-6.6797983584018,62.4648696125156,40.0767884282378));
#207199=CARTESIAN_POINT('Ctrl Pts',(-6.68360310202759,62.5984172531152,
40.1599502015401));
#207200=CARTESIAN_POINT('Ctrl Pts',(-6.65585031610573,62.5638265480135,
40.1002449453869));
#207201=CARTESIAN_POINT('Ctrl Pts',(-6.63528943158898,62.4951999029141,
40.10025));
#207202=CARTESIAN_POINT('Ctrl Pts',(-6.59568250079822,62.6076796697355,
40.1599502534424));
#207203=CARTESIAN_POINT('Ctrl Pts',(-6.5917740846471,62.570580117661,40.10025));
#207204=CARTESIAN_POINT('Ctrl Pts',(-6.58439859102965,62.5005702980932,
40.10025));
#207205=CARTESIAN_POINT('Origin',(-6.86517628122447,62.280338997922,39.92499));
#207206=CARTESIAN_POINT('Origin',(-5.89267880207669,59.102543918501,39.6398955069323));
#207207=CARTESIAN_POINT('Origin',(-5.87405712357809,58.9253704827881,39.92499));
#207208=CARTESIAN_POINT('Origin',(-6.84655462836599,62.1031658061002,39.6398955068277));
#207209=CARTESIAN_POINT('Origin',(-6.82793297553286,61.925992614092,39.3548010137695));
#207210=CARTESIAN_POINT('Ctrl Pts',(-5.8633736414952,58.8181995570485,39.8576902534424));
#207211=CARTESIAN_POINT('Ctrl Pts',(-5.98915458643735,58.8054696185321,
39.8579948730703));
#207212=CARTESIAN_POINT('Ctrl Pts',(-6.00036140428986,58.9120953679531,
39.92499));
#207213=CARTESIAN_POINT('Ctrl Pts',(-5.85862481136388,58.773012368204,39.9304020711231));
#207214=CARTESIAN_POINT('Ctrl Pts',(-5.97090589422178,58.7772117628642,
39.9058915297384));
#207215=CARTESIAN_POINT('Ctrl Pts',(-5.99561184840459,58.8669063622649,
39.9671523786036));
#207216=CARTESIAN_POINT('Ctrl Pts',(-5.8802564056751,58.7244521481309,40.0043257306693));
#207217=CARTESIAN_POINT('Ctrl Pts',(-5.97111833475339,58.7389107566976,
39.9667894847838));
#207218=CARTESIAN_POINT('Ctrl Pts',(-6.00616078842833,58.8195131589313,
40.0100138975201));
#207219=CARTESIAN_POINT('Ctrl Pts',(-5.97763489331393,58.642244989525,40.1195533054857));
#207220=CARTESIAN_POINT('Ctrl Pts',(-6.02730636094545,58.6726343357863,
40.0630813209234));
#207221=CARTESIAN_POINT('Ctrl Pts',(-6.05959099741105,58.7419259266988,
40.076826594242));
#207222=CARTESIAN_POINT('Ctrl Pts',(-6.05629725705567,58.6088386066683,
40.1599502027516));
#207223=CARTESIAN_POINT('Ctrl Pts',(-6.08390124328572,58.6434504949722,
40.1002552791541));
#207224=CARTESIAN_POINT('Ctrl Pts',(-6.1041899349697,58.7121001992962,40.10025));
#207225=CARTESIAN_POINT('Ctrl Pts',(-6.14377718965262,58.5996668978649,
40.1599502534424));
#207226=CARTESIAN_POINT('Ctrl Pts',(-6.14766703046111,58.6367684021393,
40.10025));
#207227=CARTESIAN_POINT('Ctrl Pts',(-6.15500747092256,58.7067819056643,
40.10025));
#207228=CARTESIAN_POINT('Origin',(-6.15500747092256,58.7067819056643,40.22725));
#207229=CARTESIAN_POINT('Ctrl Pts',(-6.78290064323498,61.4975385923863,
38.989));
#207230=CARTESIAN_POINT('Ctrl Pts',(-6.65640765888762,61.5108335407726,
38.989));
#207231=CARTESIAN_POINT('Ctrl Pts',(-6.65659650327814,61.5108136924273,
39.1161896013263));
#207232=CARTESIAN_POINT('Ctrl Pts',(-6.80580235504196,61.7133034041536,
38.989));
#207233=CARTESIAN_POINT('Ctrl Pts',(-6.67910686401144,61.7268068187953,
38.988776927546));
#207234=CARTESIAN_POINT('Ctrl Pts',(-6.67473401011693,61.6833805404101,
39.1161898821844));
#207235=CARTESIAN_POINT('Ctrl Pts',(-6.82760223531305,61.9187082819379,
39.1034967087243));
#207236=CARTESIAN_POINT('Ctrl Pts',(-6.70071049691168,61.9323562021233,
39.1031720232714));
#207237=CARTESIAN_POINT('Ctrl Pts',(-6.69200060426903,61.8476612078213,
39.2077529615005));
#207238=CARTESIAN_POINT('Ctrl Pts',(-6.83973663030197,62.0330459552233,
39.2875012672119));
#207239=CARTESIAN_POINT('Ctrl Pts',(-6.71274549238791,62.046864024595,39.2872087095508));
#207240=CARTESIAN_POINT('Ctrl Pts',(-6.701611992752,61.9391074595196,39.3549017048226));
#207241=CARTESIAN_POINT('Origin',(-6.78290064323498,61.4975385923863,39.116));
#207242=CARTESIAN_POINT('Origin',(4.0583767139057E-16,5.83359163402242E-17,
40.22725));
#207243=CARTESIAN_POINT('Origin',(-6.18532049829339,58.7035958781039,40.22725));
#207244=CARTESIAN_POINT('Origin',(0.364094271196318,-6.50157577599494,39.116));
#207245=CARTESIAN_POINT('Origin',(-6.74099917687859,61.0983782637168,39.1160373285255));
#207246=CARTESIAN_POINT('Ctrl Pts',(-6.17403490858961,58.5964866834551,
40.1599502534424));
#207247=CARTESIAN_POINT('Ctrl Pts',(-6.17794390662112,58.6335861742242,
40.10025));
#207248=CARTESIAN_POINT('Ctrl Pts',(-6.18532049829339,58.7035958781039,
40.10025));
#207249=CARTESIAN_POINT('Ctrl Pts',(-6.2612118565248,58.5873013840788,40.1599500566034));
#207250=CARTESIAN_POINT('Ctrl Pts',(-6.24145541658216,58.6268910424085,
40.1002551305381));
#207251=CARTESIAN_POINT('Ctrl Pts',(-6.23596000968337,58.6982507756608,
40.10025));
#207252=CARTESIAN_POINT('Ctrl Pts',(-6.34441620808552,58.6032244953991,
40.1203070619047));
#207253=CARTESIAN_POINT('Ctrl Pts',(-6.30249747592673,58.6433169201089,
40.0637098684497));
#207254=CARTESIAN_POINT('Ctrl Pts',(-6.28536729223264,58.7177256636153,
40.0772636213362));
#207255=CARTESIAN_POINT('Ctrl Pts',(-6.45770985055608,58.6635810738165,
40.0046102245801));
#207256=CARTESIAN_POINT('Ctrl Pts',(-6.37191831988716,58.6966524426404,
39.9670001894015));
#207257=CARTESIAN_POINT('Ctrl Pts',(-6.35432657855751,58.7827411889911,
40.0101788811209));
#207258=CARTESIAN_POINT('Ctrl Pts',(-6.48899861096501,58.7067768761601,
39.9303710930187));
#207259=CARTESIAN_POINT('Ctrl Pts',(-6.38003592347278,58.7342263230558,
39.9058663574104));
#207260=CARTESIAN_POINT('Ctrl Pts',(-6.37452670784895,58.8271002111734,
39.967134470636));
#207261=CARTESIAN_POINT('Ctrl Pts',(-6.49374646112681,58.7519447039089,
39.8576902534424));
#207262=CARTESIAN_POINT('Ctrl Pts',(-6.36806742857265,58.7656442740271,
39.8579948730703));
#207263=CARTESIAN_POINT('Ctrl Pts',(-6.37927424642518,58.8722700234481,
39.92499));
#207264=CARTESIAN_POINT('Origin',(-6.50557852713695,58.8589949086131,39.92499));
#207265=CARTESIAN_POINT('Origin',(-6.73632490881093,61.0544000804071,39.1925554488848));
#207266=CARTESIAN_POINT('Origin',(-6.72777047351062,60.9730100652055,39.3343017080178));
#207267=CARTESIAN_POINT('Origin',(-6.52420020557747,59.0361683443156,39.639895506922));
#207268=CARTESIAN_POINT('Origin',(-6.54282188406168,59.2133417798937,39.3548010137695));
#207269=CARTESIAN_POINT('Ctrl Pts',(-6.69328024897394,60.6448574988555,
39.3978017080178));
#207270=CARTESIAN_POINT('Ctrl Pts',(-6.56697596826217,60.6581326136905,
39.3978017080178));
#207271=CARTESIAN_POINT('Ctrl Pts',(-6.56697596826216,60.6581326136905,
39.5248017080178));
#207272=CARTESIAN_POINT('Ctrl Pts',(-6.70245599674905,60.7343993681215,
39.3978017080178));
#207273=CARTESIAN_POINT('Ctrl Pts',(-6.5763757895108,60.7475659388583,39.3980355775177));
#207274=CARTESIAN_POINT('Ctrl Pts',(-6.58108878091646,60.7924070567576,
39.5248015517192));
#207275=CARTESIAN_POINT('Ctrl Pts',(-6.7111341745387,60.819067758858,39.3484893995498));
#207276=CARTESIAN_POINT('Ctrl Pts',(-6.58530836180002,60.8325536871429,
39.3489438303426));
#207277=CARTESIAN_POINT('Ctrl Pts',(-6.59443344928367,60.919373095124,39.4508333155595));
#207278=CARTESIAN_POINT('Ctrl Pts',(-6.71570789669348,60.8636883187845,
39.2708017080178));
#207279=CARTESIAN_POINT('Ctrl Pts',(-6.59002106156404,60.8773920302461,
39.2710850691866));
#207280=CARTESIAN_POINT('Ctrl Pts',(-6.60146619279885,60.9862851800405,
39.3343017080178));
#207281=CARTESIAN_POINT('Origin',(-6.69328024897394,60.6448574988555,39.5248017080178));
#207282=CARTESIAN_POINT('Ctrl Pts',(-6.53099325079995,59.1062911958297,
39.2875012672119));
#207283=CARTESIAN_POINT('Ctrl Pts',(-6.40512264090925,59.1200087114583,
39.2878045257519));
#207284=CARTESIAN_POINT('Ctrl Pts',(-6.41653455700066,59.2267768430462,
39.3549015218348));
#207285=CARTESIAN_POINT('Ctrl Pts',(-6.54313486548275,59.2206299794252,
39.1034938540228));
#207286=CARTESIAN_POINT('Ctrl Pts',(-6.41712406698103,59.2341972766234,
39.1038286278805));
#207287=CARTESIAN_POINT('Ctrl Pts',(-6.4261461191967,59.3182247474318,39.2077506434029));
#207288=CARTESIAN_POINT('Ctrl Pts',(-6.56494601396936,59.426035450364,38.989));
#207289=CARTESIAN_POINT('Ctrl Pts',(-6.43870134519624,59.4394961352166,
38.9892298954611));
#207290=CARTESIAN_POINT('Ctrl Pts',(-6.44341285848398,59.482506795581,39.1161900347291));
#207291=CARTESIAN_POINT('Ctrl Pts',(-6.58785426247035,59.6417962403143,
38.989));
#207292=CARTESIAN_POINT('Ctrl Pts',(-6.46136078685158,59.6550912403354,
38.989));
#207293=CARTESIAN_POINT('Ctrl Pts',(-6.4615501232468,59.6550713402783,39.1161900945648));
#207294=CARTESIAN_POINT('Origin',(-6.58785426247035,59.6417962403143,39.116));
#207295=CARTESIAN_POINT('Origin',(0.347626240493858,-6.34489293004837,39.5248017080178));
#207296=CARTESIAN_POINT('Origin',(-6.67747469700884,60.4944777170594,39.5248017080178));
#207297=CARTESIAN_POINT('Origin',(0.345047419449677,-6.32035708677179,39.116));
#207298=CARTESIAN_POINT('Origin',(-6.62985850077849,60.0409538388293,39.1160402713855));
#207299=CARTESIAN_POINT('Ctrl Pts',(-6.65505462397334,60.2756459899119,
39.2708017080178));
#207300=CARTESIAN_POINT('Ctrl Pts',(-6.52822907310717,60.2894805317162,
39.27051194648));
#207301=CARTESIAN_POINT('Ctrl Pts',(-6.51668018436685,60.1796001951996,
39.3343017080178));
#207302=CARTESIAN_POINT('Ctrl Pts',(-6.65964099131221,60.3204176712045,
39.3487519301185));
#207303=CARTESIAN_POINT('Ctrl Pts',(-6.53290851690289,60.334002465445,39.3482879464));
#207304=CARTESIAN_POINT('Ctrl Pts',(-6.52373669508281,60.2467384099263,
39.4512271261638));
#207305=CARTESIAN_POINT('Ctrl Pts',(-6.6683304315061,60.4052373806432,39.3978017080178));
#207306=CARTESIAN_POINT('Ctrl Pts',(-6.54178440911703,60.4184509388156,
39.3975673827378));
#207307=CARTESIAN_POINT('Ctrl Pts',(-6.53710513959958,60.373930663245,39.5248015355181));
#207308=CARTESIAN_POINT('Ctrl Pts',(-6.67747469700884,60.4944777170594,
39.3978017080178));
#207309=CARTESIAN_POINT('Ctrl Pts',(-6.55117041629707,60.5077528318944,
39.3978017080178));
#207310=CARTESIAN_POINT('Ctrl Pts',(-6.55117041629707,60.5077528318944,
39.5248017080178));
#207311=CARTESIAN_POINT('Origin',(-6.64298446507862,60.1663250803646,39.3343017080178));
#207312=CARTESIAN_POINT('Origin',(-6.63448104698998,60.0854204586817,39.1934008533545));
#207313=CARTESIAN_POINT('Origin',(0.317499999708719,61.4240753804094,39.1925554495086));
#207314=CARTESIAN_POINT('Origin',(0.317551690014633,61.4683012396074,39.1160373285273));
#207315=CARTESIAN_POINT('Origin',(0.317500000000648,61.3422370451705,39.3343017080178));
#207316=CARTESIAN_POINT('Ctrl Pts',(0.316930737396561,61.2322532920972,
39.2708017080178));
#207317=CARTESIAN_POINT('Ctrl Pts',(0.190500000000648,61.2327440814646,
39.2710850691866));
#207318=CARTESIAN_POINT('Ctrl Pts',(0.190500000000648,61.3422370451705,
39.3343017080178));
#207319=CARTESIAN_POINT('Ctrl Pts',(0.317046579200286,61.1872475084174,
39.3487519293518));
#207320=CARTESIAN_POINT('Ctrl Pts',(0.190500000000646,61.1875064541748,
39.3492068662925));
#207321=CARTESIAN_POINT('Ctrl Pts',(0.190500000000647,61.2747290395312,
39.451227124874));
#207322=CARTESIAN_POINT('Ctrl Pts',(0.317266596914152,61.1019842137032,
39.3978017080178));
#207323=CARTESIAN_POINT('Ctrl Pts',(0.19050000000065,61.1018997758116,39.3980347781183));
#207324=CARTESIAN_POINT('Ctrl Pts',(0.190500000000646,61.146836207171,39.5248015355195));
#207325=CARTESIAN_POINT('Ctrl Pts',(0.317500000000645,61.0122769227456,
39.3978017080178));
#207326=CARTESIAN_POINT('Ctrl Pts',(0.190500000000645,61.0122769227456,
39.3978017080178));
#207327=CARTESIAN_POINT('Ctrl Pts',(0.190500000000645,61.0122769227456,
39.5248017080178));
#207328=CARTESIAN_POINT('Origin',(0.317500000000645,61.0122769227456,39.5248017080178));
#207329=CARTESIAN_POINT('Origin',(0.317500000000006,-3.32563597524808E-15,
39.116));
#207330=CARTESIAN_POINT('Origin',(0.317500000000654,61.8696548221181,39.116));
#207331=CARTESIAN_POINT('Origin',(0.317500000000006,-3.32563597524808E-15,
39.5248017080178));
#207332=CARTESIAN_POINT('Origin',(0.317500000000643,60.8610688070707,39.5248017080178));
#207333=CARTESIAN_POINT('Ctrl Pts',(0.318048871877788,62.4081695979768,
39.2875012672119));
#207334=CARTESIAN_POINT('Ctrl Pts',(0.19030903417629,62.4086377819835,39.287208709576));
#207335=CARTESIAN_POINT('Ctrl Pts',(0.190500142125712,62.3003077603774,
39.3549016990122));
#207336=CARTESIAN_POINT('Ctrl Pts',(0.317932489890632,62.2931881445371,
39.1034939173931));
#207337=CARTESIAN_POINT('Ctrl Pts',(0.190309294369134,62.2934975005705,
39.103169233634));
#207338=CARTESIAN_POINT('Ctrl Pts',(0.190500141996123,62.2083564003244,
39.2077507202297));
#207339=CARTESIAN_POINT('Ctrl Pts',(0.317722686168063,62.0866281564673,
38.989));
#207340=CARTESIAN_POINT('Ctrl Pts',(0.190309769570643,62.0868143053113,
38.9887769311176));
#207341=CARTESIAN_POINT('Ctrl Pts',(0.190500141762521,62.0431695205396,
39.1161898712915));
#207342=CARTESIAN_POINT('Ctrl Pts',(0.317500000000654,61.8696548221181,
38.989));
#207343=CARTESIAN_POINT('Ctrl Pts',(0.190310267889922,61.8696548221181,
38.989));
#207344=CARTESIAN_POINT('Ctrl Pts',(0.190500141514568,61.8696548221181,
39.1161895903854));
#207345=CARTESIAN_POINT('Origin',(0.317500000000658,62.3004688883554,39.3548010137695));
#207346=CARTESIAN_POINT('Ctrl Pts',(0.317500000000643,60.8610688070707,
39.3978017080178));
#207347=CARTESIAN_POINT('Ctrl Pts',(0.190500000000643,60.8610688070707,
39.3978017080178));
#207348=CARTESIAN_POINT('Ctrl Pts',(0.190500000000643,60.8610688070707,
39.5248017080178));
#207349=CARTESIAN_POINT('Ctrl Pts',(0.317734773760909,60.7710583184321,
39.3978017080178));
#207350=CARTESIAN_POINT('Ctrl Pts',(0.190500000000643,60.7709717342408,
39.3975666025021));
#207351=CARTESIAN_POINT('Ctrl Pts',(0.190500000000642,60.7260547307358,
39.5248015517178));
#207352=CARTESIAN_POINT('Ctrl Pts',(0.317958617919677,60.6859465754578,
39.3484894016716));
#207353=CARTESIAN_POINT('Ctrl Pts',(0.190500000001051,60.6862105562579,
39.3480259000038));
#207354=CARTESIAN_POINT('Ctrl Pts',(0.19050000000064,60.5983892955408,39.4508333188947));
#207355=CARTESIAN_POINT('Ctrl Pts',(0.318076890624007,60.6410923272405,
39.2708017080178));
#207356=CARTESIAN_POINT('Ctrl Pts',(0.19050000000064,60.6415942020421,39.27051194648));
#207357=CARTESIAN_POINT('Ctrl Pts',(0.19050000000064,60.5311086139135,39.3343017080178));
#207358=CARTESIAN_POINT('Origin',(0.317500000000639,60.5311086139135,39.3343017080178));
#207359=CARTESIAN_POINT('Origin',(0.317499999979629,62.4786179998468,39.6398955068197));
#207360=CARTESIAN_POINT('Origin',(0.317500000000662,62.6567671111299,39.92499));
#207361=CARTESIAN_POINT('Origin',(0.317499999994473,60.4497583458796,39.1934008539944));
#207362=CARTESIAN_POINT('Origin',(0.317550804321697,60.4050521322799,39.1160402713852));
#207363=CARTESIAN_POINT('Ctrl Pts',(0.0152661173115319,62.9541448057648,
40.1599502534424));
#207364=CARTESIAN_POINT('Ctrl Pts',(0.0152570710392988,62.9168399481843,
40.10025));
#207365=CARTESIAN_POINT('Ctrl Pts',(0.0152400000006639,62.8464427007196,
40.10025));
#207366=CARTESIAN_POINT('Ctrl Pts',(0.103381504925819,62.9541233134297,
40.1599500538463));
#207367=CARTESIAN_POINT('Ctrl Pts',(0.0794415635241996,62.9168211560341,
40.100244835349));
#207368=CARTESIAN_POINT('Ctrl Pts',(0.0662446030565934,62.8464212442881,
40.10025));
#207369=CARTESIAN_POINT('Ctrl Pts',(0.184683583688528,62.9290872705826,
40.1202442001037));
#207370=CARTESIAN_POINT('Ctrl Pts',(0.138547994785008,62.8936771137448,
40.0633873868015));
#207371=CARTESIAN_POINT('Ctrl Pts',(0.11330556745224,62.8213855864655,40.0772271723537));
#207372=CARTESIAN_POINT('Ctrl Pts',(0.29134099263231,62.8564203507742,40.0045995998164));
#207373=CARTESIAN_POINT('Ctrl Pts',(0.201910351191971,62.8329175802742,
39.9663485808318));
#207374=CARTESIAN_POINT('Ctrl Pts',(0.175042741958496,62.7487193609389,
40.0101727202466));
#207375=CARTESIAN_POINT('Ctrl Pts',(0.318045276843284,62.8099434033761,
39.9304654349858));
#207376=CARTESIAN_POINT('Ctrl Pts',(0.205831635643775,62.7947175424999,
39.9051900162947));
#207377=CARTESIAN_POINT('Ctrl Pts',(0.190500000000664,62.7022409210443,
39.9671857458178));
#207378=CARTESIAN_POINT('Ctrl Pts',(0.318045750793708,62.7644678366119,
39.8576902534424));
#207379=CARTESIAN_POINT('Ctrl Pts',(0.190500000000658,62.7649326510149,
39.8573998014387));
#207380=CARTESIAN_POINT('Ctrl Pts',(0.190500000000662,62.6567671111299,
39.92499));
#207381=CARTESIAN_POINT('Origin',(0.317500000000006,-3.32563597524808E-15,
39.116));
#207382=CARTESIAN_POINT('Origin',(0.317500000000634,60.0036905223731,39.116));
#207383=CARTESIAN_POINT('Ctrl Pts',(0.317500000000634,60.0036905223731,
38.989));
#207384=CARTESIAN_POINT('Ctrl Pts',(0.190309748265858,60.003690522373,38.989));
#207385=CARTESIAN_POINT('Ctrl Pts',(0.190500142290163,60.0036905223731,
39.1161901092321));
#207386=CARTESIAN_POINT('Ctrl Pts',(0.31727038552505,59.7867137603524,38.989));
#207387=CARTESIAN_POINT('Ctrl Pts',(0.190310262476932,59.7869045527987,
38.989229898976));
#207388=CARTESIAN_POINT('Ctrl Pts',(0.190500142033094,59.8301727552495,
39.1161900493201));
#207389=CARTESIAN_POINT('Ctrl Pts',(0.317049440714262,59.5801552670728,
39.1034966344368));
#207390=CARTESIAN_POINT('Ctrl Pts',(0.190310761082396,59.5804765271847,
39.1038314102561));
#207391=CARTESIAN_POINT('Ctrl Pts',(0.190500141785737,59.664987104655,39.2077528789601));
#207392=CARTESIAN_POINT('Ctrl Pts',(0.316925998273675,59.4651754363832,
39.2875012672119));
#207393=CARTESIAN_POINT('Ctrl Pts',(0.190311035335595,59.4656607446593,
39.2878045257868));
#207394=CARTESIAN_POINT('Ctrl Pts',(0.190500141647532,59.5730368716576,
39.3549015295899));
#207395=CARTESIAN_POINT('Origin',(0.31750000000063,59.5728760150042,39.3548010137695));
#207396=CARTESIAN_POINT('Ctrl Pts',(-0.318045750792382,62.7644678366119,
39.8576902534424));
#207397=CARTESIAN_POINT('Ctrl Pts',(-0.190499999999334,62.7649326510149,
39.8573998014387));
#207398=CARTESIAN_POINT('Ctrl Pts',(-0.190499999999338,62.6567671111299,
39.92499));
#207399=CARTESIAN_POINT('Ctrl Pts',(-0.318045262794513,62.8099640589335,
39.9304984902491));
#207400=CARTESIAN_POINT('Ctrl Pts',(-0.20584033072329,62.7947344577613,
39.9052171569794));
#207401=CARTESIAN_POINT('Ctrl Pts',(-0.190499999999339,62.7022616416333,
39.9672049726608));
#207402=CARTESIAN_POINT('Ctrl Pts',(-0.291334117854747,62.8562601188214,
40.0043437678662));
#207403=CARTESIAN_POINT('Ctrl Pts',(-0.201836550627054,62.8328016940825,
39.9661628577639));
#207404=CARTESIAN_POINT('Ctrl Pts',(-0.175038734051537,62.7485591297232,
40.0100243556234));
#207405=CARTESIAN_POINT('Ctrl Pts',(-0.185622189559732,62.9286112571071,
40.1194874821987));
#207406=CARTESIAN_POINT('Ctrl Pts',(-0.139140155999468,62.8932808767899,
40.0627551483143));
#207407=CARTESIAN_POINT('Ctrl Pts',(-0.113848895265012,62.8209095783125,
40.0767884282378));
#207408=CARTESIAN_POINT('Ctrl Pts',(-0.103673266462164,62.9541233349674,
40.1599502015391));
#207409=CARTESIAN_POINT('Ctrl Pts',(-0.0796882264529957,62.9168211653022,
40.1002449453869));
#207410=CARTESIAN_POINT('Ctrl Pts',(-0.0664134143644937,62.8464212664863,
40.10025));
#207411=CARTESIAN_POINT('Ctrl Pts',(-0.0152661173102017,62.9541448057648,
40.1599502534424));
#207412=CARTESIAN_POINT('Ctrl Pts',(-0.0152570710379694,62.9168399481843,
40.10025));
#207413=CARTESIAN_POINT('Ctrl Pts',(-0.015239999999336,62.8464427007196,
40.10025));
#207414=CARTESIAN_POINT('Origin',(-0.317499999999338,62.6567671111299,39.92499));
#207415=CARTESIAN_POINT('Origin',(0.317499999970736,59.3947266586226,39.6398955069306));
#207416=CARTESIAN_POINT('Origin',(0.317500000000626,59.2165773020941,39.92499));
#207417=CARTESIAN_POINT('Origin',(-0.317499999976485,62.4786179998354,39.6398955068269));
#207418=CARTESIAN_POINT('Origin',(-0.317499999999342,62.3004688883555,39.3548010137695));
#207419=CARTESIAN_POINT('Ctrl Pts',(0.316922544676314,59.1088767419348,
39.8576902534424));
#207420=CARTESIAN_POINT('Ctrl Pts',(0.190500000000626,59.1093642282366,
39.8579948730703));
#207421=CARTESIAN_POINT('Ctrl Pts',(0.190500000000626,59.2165773020941,
39.92499));
#207422=CARTESIAN_POINT('Ctrl Pts',(0.316922012809789,59.0634407053228,
39.9304020711232));
#207423=CARTESIAN_POINT('Ctrl Pts',(0.205694973741221,59.0793536643037,
39.9058915297385));
#207424=CARTESIAN_POINT('Ctrl Pts',(0.190500000000625,59.1711393827287,
39.9671523786031));
#207425=CARTESIAN_POINT('Ctrl Pts',(0.290332993455678,59.0174076205277,
40.0043257306692));
#207426=CARTESIAN_POINT('Ctrl Pts',(0.201480151666502,59.0412846811398,
39.9667894847832));
#207427=CARTESIAN_POINT('Ctrl Pts',(0.175054909460471,59.1251084688124,
40.0100138975199));
#207428=CARTESIAN_POINT('Ctrl Pts',(0.184894967402138,58.9458296250061,
40.1195533054858));
#207429=CARTESIAN_POINT('Ctrl Pts',(0.138672156931825,58.9812445774289,
40.0630813209239));
#207430=CARTESIAN_POINT('Ctrl Pts',(0.113807322598262,59.053531245193,40.0768265942422));
#207431=CARTESIAN_POINT('Ctrl Pts',(0.103171606456398,58.9208287018091,
40.1599502027518));
#207432=CARTESIAN_POINT('Ctrl Pts',(0.0793367652464492,58.9581363848269,
40.1002552791538));
#207433=CARTESIAN_POINT('Ctrl Pts',(0.0663350652350921,59.0285307646513,
40.10025));
#207434=CARTESIAN_POINT('Ctrl Pts',(0.015212193456543,58.9208513795073,
40.1599502534424));
#207435=CARTESIAN_POINT('Ctrl Pts',(0.0152218248297303,58.9581562369413,
40.10025));
#207436=CARTESIAN_POINT('Ctrl Pts',(0.0152400000006241,59.0285534841296,
40.10025));
#207437=CARTESIAN_POINT('Ctrl Pts',(-0.317499999999346,61.8696548221181,
38.989));
#207438=CARTESIAN_POINT('Ctrl Pts',(-0.190310256931028,61.8696548221181,
38.989));
#207439=CARTESIAN_POINT('Ctrl Pts',(-0.190500141529595,61.8696548221181,
39.1161896013266));
#207440=CARTESIAN_POINT('Ctrl Pts',(-0.317722689631595,62.0866315324121,
38.989));
#207441=CARTESIAN_POINT('Ctrl Pts',(-0.190309758575247,62.0868176889541,
38.988776927546));
#207442=CARTESIAN_POINT('Ctrl Pts',(-0.190500141777577,62.0431722165661,
39.1161898821848));
#207443=CARTESIAN_POINT('Ctrl Pts',(-0.317932491655033,62.2931898887681,
39.1034967087243));
#207444=CARTESIAN_POINT('Ctrl Pts',(-0.190309283349939,62.2934992458037,
39.103172023271));
#207445=CARTESIAN_POINT('Ctrl Pts',(-0.1905001420112,62.2083577878513,39.2077529614998));
#207446=CARTESIAN_POINT('Ctrl Pts',(-0.31804887187647,62.4081695979768,
39.2875012672119));
#207447=CARTESIAN_POINT('Ctrl Pts',(-0.1903090231461,62.4086377820239,39.2872087095508));
#207448=CARTESIAN_POINT('Ctrl Pts',(-0.1905001421408,62.3003077510787,39.3549017048228));
#207449=CARTESIAN_POINT('Origin',(-0.317499999999346,61.8696548221181,39.116));
#207450=CARTESIAN_POINT('Origin',(-0.317499999999998,6.55071265098105E-13,
39.116));
#207451=CARTESIAN_POINT('Origin',(-0.317551690012418,61.4683012396066,39.1160373285255));
#207452=CARTESIAN_POINT('Ctrl Pts',(-0.015212193455297,58.9208513795073,
40.1599502534424));
#207453=CARTESIAN_POINT('Ctrl Pts',(-0.0152218248284836,58.9581562369413,
40.10025));
#207454=CARTESIAN_POINT('Ctrl Pts',(-0.0152399999993761,59.0285534841296,
40.10025));
#207455=CARTESIAN_POINT('Ctrl Pts',(-0.102871702176771,58.9208288705618,
40.1599500566038));
#207456=CARTESIAN_POINT('Ctrl Pts',(-0.0790852439327617,58.9581365422965,
40.100255130536));
#207457=CARTESIAN_POINT('Ctrl Pts',(-0.0661608181918845,59.0285309330218,
40.10025));
#207458=CARTESIAN_POINT('Ctrl Pts',(-0.183955833236888,58.9453619764183,
40.1203070619046));
#207459=CARTESIAN_POINT('Ctrl Pts',(-0.138075936735343,58.9808530699761,
40.0637098684499));
#207460=CARTESIAN_POINT('Ctrl Pts',(-0.113261762367537,59.0530636028226,
40.0772636213363));
#207461=CARTESIAN_POINT('Ctrl Pts',(-0.290319860890038,59.0172303255294,
40.0046102245801));
#207462=CARTESIAN_POINT('Ctrl Pts',(-0.201541405841316,59.0411528690721,
39.9670001894012));
#207463=CARTESIAN_POINT('Ctrl Pts',(-0.175047309550564,59.1249311745757,
40.0101788811209));
#207464=CARTESIAN_POINT('Ctrl Pts',(-0.316922027356722,59.0634600627912,
39.9303710930187));
#207465=CARTESIAN_POINT('Ctrl Pts',(-0.20568700036667,59.0793694364685,
39.9058663574109));
#207466=CARTESIAN_POINT('Ctrl Pts',(-0.190499999999374,59.1711586818658,
39.9671344706364));
#207467=CARTESIAN_POINT('Ctrl Pts',(-0.316922544675064,59.1088767419348,
39.8576902534424));
#207468=CARTESIAN_POINT('Ctrl Pts',(-0.190499999999374,59.1093642282366,
39.8579948730703));
#207469=CARTESIAN_POINT('Ctrl Pts',(-0.190499999999374,59.2165773020941,
39.92499));
#207470=CARTESIAN_POINT('Origin',(-0.317499999999374,59.2165773020941,39.92499));
#207471=CARTESIAN_POINT('Origin',(-0.317499999993373,61.4240753793279,39.1925554488842));
#207472=CARTESIAN_POINT('Origin',(-0.317499999999352,61.3422370451705,39.3343017080178));
#207473=CARTESIAN_POINT('Origin',(-0.317499999969898,59.3947266586074,39.6398955069212));
#207474=CARTESIAN_POINT('Origin',(-0.31749999999937,59.5728760150042,39.3548010137695));
#207475=CARTESIAN_POINT('Ctrl Pts',(-0.317499999999355,61.0122769227456,
39.3978017080178));
#207476=CARTESIAN_POINT('Ctrl Pts',(-0.190499999999355,61.0122769227456,
39.3978017080178));
#207477=CARTESIAN_POINT('Ctrl Pts',(-0.190499999999355,61.0122769227456,
39.5248017080178));
#207478=CARTESIAN_POINT('Ctrl Pts',(-0.317265808075748,61.1022873990971,
39.3978017080178));
#207479=CARTESIAN_POINT('Ctrl Pts',(-0.190499999999328,61.1022028716704,
39.3980355775177));
#207480=CARTESIAN_POINT('Ctrl Pts',(-0.190499999999354,61.1472909869838,
39.5248015517192));
#207481=CARTESIAN_POINT('Ctrl Pts',(-0.317046189128453,61.1873990841185,
39.3484893995498));
#207482=CARTESIAN_POINT('Ctrl Pts',(-0.190500000000547,61.1876587562325,
39.3489438303426));
#207483=CARTESIAN_POINT('Ctrl Pts',(-0.190499999999353,61.2749563897836,
39.4508333155593));
#207484=CARTESIAN_POINT('Ctrl Pts',(-0.316930737395267,61.2322532920972,
39.2708017080178));
#207485=CARTESIAN_POINT('Ctrl Pts',(-0.190499999999346,61.2327440814646,
39.2710850691866));
#207486=CARTESIAN_POINT('Ctrl Pts',(-0.190499999999352,61.3422370451705,
39.3343017080178));
#207487=CARTESIAN_POINT('Origin',(-0.317499999999355,61.0122769227456,39.5248017080178));
#207488=CARTESIAN_POINT('Ctrl Pts',(-0.316925998272419,59.4651754363832,
39.2875012672119));
#207489=CARTESIAN_POINT('Ctrl Pts',(-0.190311049924531,59.4656607446034,
39.2878045257519));
#207490=CARTESIAN_POINT('Ctrl Pts',(-0.190500141624416,59.5730368592469,
39.3549015218347));
#207491=CARTESIAN_POINT('Ctrl Pts',(-0.31704944257856,59.5801570044831,
39.1034938540228));
#207492=CARTESIAN_POINT('Ctrl Pts',(-0.190310775688781,59.5804782634853,
39.1038286278806));
#207493=CARTESIAN_POINT('Ctrl Pts',(-0.190500141762599,59.664988484272,
39.2077506434032));
#207494=CARTESIAN_POINT('Ctrl Pts',(-0.317270389088207,59.7867171285936,
38.989));
#207495=CARTESIAN_POINT('Ctrl Pts',(-0.190310277117612,59.7869079131834,
38.9892298954611));
#207496=CARTESIAN_POINT('Ctrl Pts',(-0.190500142009918,59.8301754438923,
39.1161900347288));
#207497=CARTESIAN_POINT('Ctrl Pts',(-0.317499999999366,60.0036905223731,
38.989));
#207498=CARTESIAN_POINT('Ctrl Pts',(-0.190309762954212,60.0036905223731,
38.989));
#207499=CARTESIAN_POINT('Ctrl Pts',(-0.19050014226694,60.0036905223731,
39.1161900945645));
#207500=CARTESIAN_POINT('Origin',(-0.317499999999366,60.0036905223731,39.116));
#207501=CARTESIAN_POINT('Origin',(-0.317499999999991,6.39284123049835E-13,
39.5248017080178));
#207502=CARTESIAN_POINT('Origin',(-0.317499999999357,60.8610688070707,39.5248017080178));
#207503=CARTESIAN_POINT('Origin',(-0.317499999999991,6.36811926168668E-13,
39.116));
#207504=CARTESIAN_POINT('Origin',(-0.317550804320187,60.4050521322801,39.116040271385));
#207505=CARTESIAN_POINT('Ctrl Pts',(-0.318076890622726,60.6410923272405,
39.2708017080178));
#207506=CARTESIAN_POINT('Ctrl Pts',(-0.190499999999366,60.6415942020422,
39.27051194648));
#207507=CARTESIAN_POINT('Ctrl Pts',(-0.19049999999936,60.5311086139135,
39.3343017080178));
#207508=CARTESIAN_POINT('Ctrl Pts',(-0.317958218318119,60.6860981505084,
39.3487519301186));
#207509=CARTESIAN_POINT('Ctrl Pts',(-0.190499999998138,60.6863613750267,
39.348287946399));
#207510=CARTESIAN_POINT('Ctrl Pts',(-0.19049999999936,60.598616644694,39.4512271261644));
#207511=CARTESIAN_POINT('Ctrl Pts',(-0.317733982966902,60.771361502534,
39.3978017080178));
#207512=CARTESIAN_POINT('Ctrl Pts',(-0.190499999999357,60.7712750142006,
39.3975673827397));
#207513=CARTESIAN_POINT('Ctrl Pts',(-0.190499999999358,60.7265095085063,
39.5248015355181));
#207514=CARTESIAN_POINT('Ctrl Pts',(-0.317499999999357,60.8610688070707,
39.3978017080178));
#207515=CARTESIAN_POINT('Ctrl Pts',(-0.190499999999357,60.8610688070707,
39.3978017080178));
#207516=CARTESIAN_POINT('Ctrl Pts',(-0.190499999999357,60.8610688070707,
39.5248017080178));
#207517=CARTESIAN_POINT('Origin',(-0.31749999999936,60.5311086139135,39.3343017080178));
#207518=CARTESIAN_POINT('Origin',(-0.317500000299763,60.4497583469878,39.1934008533546));
#207519=CARTESIAN_POINT('Origin',(6.73632490863968,61.054400081511,39.1925554495083));
#207520=CARTESIAN_POINT('Origin',(6.74099917688,61.0983782637173,39.1160373285268));
#207521=CARTESIAN_POINT('Origin',(6.72777047351185,60.9730100652054,39.3343017080178));
#207522=CARTESIAN_POINT('Ctrl Pts',(6.71570789669471,60.8636883187844,39.2708017080178));
#207523=CARTESIAN_POINT('Ctrl Pts',(6.59002106156527,60.877392030246,39.2710850691866));
#207524=CARTESIAN_POINT('Ctrl Pts',(6.60146619280008,60.9862851800404,39.3343017080178));
#207525=CARTESIAN_POINT('Ctrl Pts',(6.71111871849892,60.8189169727308,39.3487519293518));
#207526=CARTESIAN_POINT('Ctrl Pts',(6.58529244190356,60.8324022194127,39.3492068662927));
#207527=CARTESIAN_POINT('Ctrl Pts',(6.59440968471234,60.9191469903194,39.451227124874));
#207528=CARTESIAN_POINT('Ctrl Pts',(6.70242508976313,60.7340977611528,39.3978017080178));
#207529=CARTESIAN_POINT('Ctrl Pts',(6.57634410736793,60.7472645033892,39.3980347781183));
#207530=CARTESIAN_POINT('Ctrl Pts',(6.58104124348278,60.7919547682765,39.5248015355195));
#207531=CARTESIAN_POINT('Ctrl Pts',(6.69328024897516,60.6448574988554,39.3978017080178));
#207532=CARTESIAN_POINT('Ctrl Pts',(6.56697596826339,60.6581326136904,39.3978017080178));
#207533=CARTESIAN_POINT('Ctrl Pts',(6.56697596826339,60.6581326136904,39.5248017080178));
#207534=CARTESIAN_POINT('Origin',(6.69328024897516,60.6448574988554,39.5248017080178));
#207535=CARTESIAN_POINT('Origin',(0.315760701779432,-0.0331877870874832,
39.116));
#207536=CARTESIAN_POINT('Origin',(6.78290064323623,61.4975385923861,39.116));
#207537=CARTESIAN_POINT('Origin',(0.315760701779432,-0.0331877870874832,
39.5248017080178));
#207538=CARTESIAN_POINT('Origin',(6.67747469701007,60.4944777170593,39.5248017080178));
#207539=CARTESIAN_POINT('Ctrl Pts',(6.83973663030323,62.0330459552232,39.2875012672119));
#207540=CARTESIAN_POINT('Ctrl Pts',(6.71274550335304,62.0468640234019,39.287208709576));
#207541=CARTESIAN_POINT('Ctrl Pts',(6.70161199370888,61.9391074687686,39.3549016990123));
#207542=CARTESIAN_POINT('Ctrl Pts',(6.82760205123604,61.9187065474465,39.1034939173931));
#207543=CARTESIAN_POINT('Ctrl Pts',(6.70071032544346,61.932354465302,39.1031692336335));
#207544=CARTESIAN_POINT('Ctrl Pts',(6.69200045921829,61.8476598279005,39.2077507202298));
#207545=CARTESIAN_POINT('Ctrl Pts',(6.80580199871536,61.7133000470645,38.989));
#207546=CARTESIAN_POINT('Ctrl Pts',(6.67910652125894,61.7268034525369,38.9887769311176));
#207547=CARTESIAN_POINT('Ctrl Pts',(6.67473372829009,61.6833778591514,39.1161898712915));
#207548=CARTESIAN_POINT('Ctrl Pts',(6.78290064323623,61.4975385923861,38.989));
#207549=CARTESIAN_POINT('Ctrl Pts',(6.65640766978607,61.5108335396271,38.989));
#207550=CARTESIAN_POINT('Ctrl Pts',(6.65659650326314,61.5108136924289,39.1161895903854));
#207551=CARTESIAN_POINT('Origin',(6.82793297553411,61.9259926140919,39.3548010137695));
#207552=CARTESIAN_POINT('Ctrl Pts',(6.67747469701007,60.4944777170593,39.3978017080178));
#207553=CARTESIAN_POINT('Ctrl Pts',(6.5511704162983,60.5077528318943,39.3978017080178));
#207554=CARTESIAN_POINT('Ctrl Pts',(6.5511704162983,60.5077528318943,39.5248017080178));
#207555=CARTESIAN_POINT('Ctrl Pts',(6.66829952659994,60.404935774755,39.3978017080178));
#207556=CARTESIAN_POINT('Ctrl Pts',(6.54175270773074,60.4181493202563,39.3975666025021));
#207557=CARTESIAN_POINT('Ctrl Pts',(6.53705760237946,60.3734783767959,39.5248015517178));
#207558=CARTESIAN_POINT('Ctrl Pts',(6.65962554481765,60.3202668847282,39.3484894016717));
#207559=CARTESIAN_POINT('Ctrl Pts',(6.53289275204912,60.3338524728754,39.3480259000038));
#207560=CARTESIAN_POINT('Ctrl Pts',(6.52371293062624,60.2465123062138,39.4508333188945));
#207561=CARTESIAN_POINT('Ctrl Pts',(6.65505462397456,60.2756459899118,39.2708017080178));
#207562=CARTESIAN_POINT('Ctrl Pts',(6.52822907310839,60.2894805317161,39.27051194648));
#207563=CARTESIAN_POINT('Ctrl Pts',(6.51668018436807,60.1796001951995,39.3343017080178));
#207564=CARTESIAN_POINT('Origin',(6.64298446507984,60.1663250803645,39.3343017080178));
#207565=CARTESIAN_POINT('Origin',(6.84655462836781,62.1031658061145,39.6398955068186));
#207566=CARTESIAN_POINT('Origin',(6.86517628122572,62.2803389979219,39.92499));
#207567=CARTESIAN_POINT('Origin',(6.63448104656917,60.0854204576121,39.193400853994));
#207568=CARTESIAN_POINT('Origin',(6.62985850077975,60.040953838829,39.1160402713856));
#207569=CARTESIAN_POINT('Ctrl Pts',(6.59568250079948,62.6076796697354,40.1599502534424));
#207570=CARTESIAN_POINT('Ctrl Pts',(6.59177408464837,62.5705801176609,40.10025));
#207571=CARTESIAN_POINT('Ctrl Pts',(6.58439859103091,62.500570298093,40.10025));
#207572=CARTESIAN_POINT('Ctrl Pts',(6.68331293653994,62.5984477290793,40.1599500538453));
#207573=CARTESIAN_POINT('Ctrl Pts',(6.6556050034532,62.5638523220915,40.1002448353493));
#207574=CARTESIAN_POINT('Ctrl Pts',(6.63512154272685,62.4952175264256,40.10025));
#207575=CARTESIAN_POINT('Ctrl Pts',(6.76155265492332,62.5650504549417,40.1202442001039));
#207576=CARTESIAN_POINT('Ctrl Pts',(6.71196843232468,62.534656760858,40.0633873868015));
#207577=CARTESIAN_POINT('Ctrl Pts',(6.67930776339633,62.4653998062675,40.0772271723537));
#207578=CARTESIAN_POINT('Ctrl Pts',(6.86003002196325,62.48163287707,40.0045995998162));
#207579=CARTESIAN_POINT('Ctrl Pts',(6.76863258245113,62.4676069047249,39.9663485808318));
#207580=CARTESIAN_POINT('Ctrl Pts',(6.73311104631518,62.3866783619495,40.0101727202466));
#207581=CARTESIAN_POINT('Ctrl Pts',(6.88172985342223,62.4326191774618,39.9304654349859));
#207582=CARTESIAN_POINT('Ctrl Pts',(6.76853939445079,62.4292062449162,39.905190016295));
#207583=CARTESIAN_POINT('Ctrl Pts',(6.74362530798325,62.3388388123827,39.9671857458179));
#207584=CARTESIAN_POINT('Ctrl Pts',(6.87697683366627,62.387392681069,39.8576902534424));
#207585=CARTESIAN_POINT('Ctrl Pts',(6.75017837817664,62.4011871104968,39.8573998014387));
#207586=CARTESIAN_POINT('Ctrl Pts',(6.73887200051396,62.2936141127569,39.92499));
#207587=CARTESIAN_POINT('Origin',(6.58439859103091,62.500570298093,40.22725));
#207588=CARTESIAN_POINT('Origin',(0.315760701779432,-0.0331877870874832,
39.116));
#207589=CARTESIAN_POINT('Origin',(6.58785426247156,59.6417962403142,39.116));
#207590=CARTESIAN_POINT('Origin',(5.64744126194171E-15,5.53089827396188E-15,
40.22725));
#207591=CARTESIAN_POINT('Origin',(6.55408556366009,62.5037563256534,40.22725));
#207592=CARTESIAN_POINT('Ctrl Pts',(6.58785426247156,59.6417962403142,38.989));
#207593=CARTESIAN_POINT('Ctrl Pts',(6.4613607722442,59.6550912418706,38.989));
#207594=CARTESIAN_POINT('Ctrl Pts',(6.46155012326984,59.6550713402759,39.1161901092318));
#207595=CARTESIAN_POINT('Ctrl Pts',(6.56494565834935,59.4260321009468,38.989));
#207596=CARTESIAN_POINT('Ctrl Pts',(6.43870097938069,59.4394927947694,38.989229898976));
#207597=CARTESIAN_POINT('Ctrl Pts',(6.44341257746704,59.4825041216622,39.1161900493198));
#207598=CARTESIAN_POINT('Ctrl Pts',(6.54313468201973,59.2206282517276,39.1034966344368));
#207599=CARTESIAN_POINT('Ctrl Pts',(6.41712387096456,59.2341955513628,39.1038314102566));
#207600=CARTESIAN_POINT('Ctrl Pts',(6.42614597501067,59.3182233753726,39.2077528789601));
#207601=CARTESIAN_POINT('Ctrl Pts',(6.53099325080115,59.1062911958296,39.2875012672119));
#207602=CARTESIAN_POINT('Ctrl Pts',(6.40512262640657,59.1200087130388,39.2878045257868));
#207603=CARTESIAN_POINT('Ctrl Pts',(6.41653455832081,59.2267768553861,39.3549015295897));
#207604=CARTESIAN_POINT('Origin',(6.54282188406287,59.2133417798936,39.3548010137695));
#207605=CARTESIAN_POINT('Ctrl Pts',(6.24436990788122,62.4538823482275,39.8576902534424));
#207606=CARTESIAN_POINT('Ctrl Pts',(6.37126553604133,62.4410124550017,39.8573998014387));
#207607=CARTESIAN_POINT('Ctrl Pts',(6.35995915837864,62.3334394572618,39.92499));
#207608=CARTESIAN_POINT('Ctrl Pts',(6.24912604340989,62.4991292864732,39.9304984902492));
#207609=CARTESIAN_POINT('Ctrl Pts',(6.35912437831703,62.4722545055303,39.9052171569795));
#207610=CARTESIAN_POINT('Ctrl Pts',(6.36471463173929,62.3786847639674,39.9672049726605));
#207611=CARTESIAN_POINT('Ctrl Pts',(6.28053011789799,62.5423796567681,40.004343767866));
#207612=CARTESIAN_POINT('Ctrl Pts',(6.3670853349994,62.5096946965644,39.9661628577643));
#207613=CARTESIAN_POINT('Ctrl Pts',(6.38493060453772,62.4231124872027,40.0100243556236));
#207614=CARTESIAN_POINT('Ctrl Pts',(6.39322569848953,62.6032845425346,40.1194874821989));
#207615=CARTESIAN_POINT('Ctrl Pts',(6.43576006824533,62.5632890102012,40.062755148314));
#207616=CARTESIAN_POINT('Ctrl Pts',(6.45334792019258,62.4886705126495,40.0767884282376));
#207617=CARTESIAN_POINT('Ctrl Pts',(6.47739243510552,62.620090867565,40.1599502015389));
#207618=CARTESIAN_POINT('Ctrl Pts',(6.49734694408422,62.5804859237135,40.1002449453872));
#207619=CARTESIAN_POINT('Ctrl Pts',(6.50319024212585,62.5090840872032,40.10025));
#207620=CARTESIAN_POINT('Ctrl Pts',(6.56531752495365,62.6108711573005,40.1599502534424));
#207621=CARTESIAN_POINT('Ctrl Pts',(6.56142710223415,62.5737697140401,40.10025));
#207622=CARTESIAN_POINT('Ctrl Pts',(6.55408556366009,62.5037563256534,40.10025));
#207623=CARTESIAN_POINT('Origin',(6.23365487766687,62.3467145720968,39.92499));
#207624=CARTESIAN_POINT('Origin',(6.52420020557921,59.0361683443322,39.6398955069324));
#207625=CARTESIAN_POINT('Origin',(6.50557852713814,58.858994908613,39.92499));
#207626=CARTESIAN_POINT('Origin',(6.2150332248537,62.1695413802714,39.639895506827));
#207627=CARTESIAN_POINT('Origin',(6.19641157197526,61.9923681882668,39.3548010137695));
#207628=CARTESIAN_POINT('Ctrl Pts',(6.493746461128,58.7519447039088,39.8576902534424));
#207629=CARTESIAN_POINT('Ctrl Pts',(6.36806742857384,58.765644274027,39.8579948730703));
#207630=CARTESIAN_POINT('Ctrl Pts',(6.37927424642637,58.872270023448,39.92499));
#207631=CARTESIAN_POINT('Ctrl Pts',(6.48899657309109,58.7067576262548,39.9304020711229));
#207632=CARTESIAN_POINT('Ctrl Pts',(6.38004220453006,58.7342098038497,39.9058915297385));
#207633=CARTESIAN_POINT('Ctrl Pts',(6.37452469054112,58.82708101776,39.9671523786039));
#207634=CARTESIAN_POINT('Ctrl Pts',(6.45774144355365,58.6637560248471,40.0043257306696));
#207635=CARTESIAN_POINT('Ctrl Pts',(6.37187117938174,58.6967899354329,39.9667894847838));
#207636=CARTESIAN_POINT('Ctrl Pts',(6.35435266912822,58.7829167175848,40.0100138975201));
#207637=CARTESIAN_POINT('Ctrl Pts',(6.34539908016389,58.6035914159082,40.1195533054854));
#207638=CARTESIAN_POINT('Ctrl Pts',(6.30313135363918,58.6436439608617,40.0630813209233));
#207639=CARTESIAN_POINT('Ctrl Pts',(6.28595874576577,58.7181337176191,40.076826594242));
#207640=CARTESIAN_POINT('Ctrl Pts',(6.26151010025777,58.587269867717,40.1599502027514));
#207641=CARTESIAN_POINT('Ctrl Pts',(6.24170554357575,58.6268645946676,40.1002552791553));
#207642=CARTESIAN_POINT('Ctrl Pts',(6.23613328458318,58.6982323944352,40.10025));
#207643=CARTESIAN_POINT('Ctrl Pts',(6.17403490859079,58.596486683455,40.1599502534424));
#207644=CARTESIAN_POINT('Ctrl Pts',(6.17794390662231,58.6335861742241,40.10025));
#207645=CARTESIAN_POINT('Ctrl Pts',(6.18532049829458,58.7035958781038,40.10025));
#207646=CARTESIAN_POINT('Origin',(6.18532049829458,58.7035958781038,40.22725));
#207647=CARTESIAN_POINT('Ctrl Pts',(6.15137923967737,61.5639141665611,38.989));
#207648=CARTESIAN_POINT('Ctrl Pts',(6.27787222402492,61.5506192181748,38.989));
#207649=CARTESIAN_POINT('Ctrl Pts',(6.27768337963421,61.5506390665201,39.1161896013264));
#207650=CARTESIAN_POINT('Ctrl Pts',(6.17383801205405,61.7797255331385,38.989));
#207651=CARTESIAN_POINT('Ctrl Pts',(6.3005724203996,61.7665923920118,38.988776927546));
#207652=CARTESIAN_POINT('Ctrl Pts',(6.29582088597955,61.7232059145528,39.1161898821846));
#207653=CARTESIAN_POINT('Ctrl Pts',(6.19522058691312,61.985174271489,39.1034967087243));
#207654=CARTESIAN_POINT('Ctrl Pts',(6.3221769985456,61.972141675993,39.103172023271));
#207655=CARTESIAN_POINT('Ctrl Pts',(6.31308747966742,61.8874865820171,39.2077529615));
#207656=CARTESIAN_POINT('Ctrl Pts',(6.20712349654526,62.0995362748658,39.2875012672119));
#207657=CARTESIAN_POINT('Ctrl Pts',(6.33421251157745,62.0866494440659,39.2872087095508));
#207658=CARTESIAN_POINT('Ctrl Pts',(6.32269886789234,61.9789328337399,39.3549017048227));
#207659=CARTESIAN_POINT('Origin',(6.15137923967737,61.5639141665611,39.116));
#207660=CARTESIAN_POINT('Origin',(5.67080826956262E-15,5.31104381076135E-15,
40.22725));
#207661=CARTESIAN_POINT('Origin',(6.15500747092375,58.7067819056642,40.22725));
#207662=CARTESIAN_POINT('Origin',(0.364094271196581,6.50157577599617,39.116));
#207663=CARTESIAN_POINT('Origin',(6.10937495962157,61.1647646440465,39.116037328525));
#207664=CARTESIAN_POINT('Ctrl Pts',(6.14377718965381,58.5996668978648,40.1599502534424));
#207665=CARTESIAN_POINT('Ctrl Pts',(6.1476670304623,58.6367684021392,40.10025));
#207666=CARTESIAN_POINT('Ctrl Pts',(6.15500747092375,58.7067819056642,40.10025));
#207667=CARTESIAN_POINT('Ctrl Pts',(6.05659553606757,58.6088074259629,40.1599500566041));
#207668=CARTESIAN_POINT('Ctrl Pts',(6.08415140319854,58.6434243604373,40.1002551305372));
#207669=CARTESIAN_POINT('Ctrl Pts',(6.10436324506862,58.712082152968,40.10025));
#207670=CARTESIAN_POINT('Ctrl Pts',(5.97852000021575,58.6416817365139,40.1203070619047));
#207671=CARTESIAN_POINT('Ctrl Pts',(6.02785839131313,58.6721826510715,40.06370986845));
#207672=CARTESIAN_POINT('Ctrl Pts',(6.06008468706751,58.7414038195495,40.0772636213363));
#207673=CARTESIAN_POINT('Ctrl Pts',(5.88025093392533,58.7242744516464,40.0046102245801));
#207674=CARTESIAN_POINT('Ctrl Pts',(5.97104363802217,58.7387860695149,39.9670001894012));
#207675=CARTESIAN_POINT('Ctrl Pts',(6.00614981441082,58.8193360415243,40.0101788811209));
#207676=CARTESIAN_POINT('Ctrl Pts',(5.85862682030321,58.7730316211506,39.9303710930187));
#207677=CARTESIAN_POINT('Ctrl Pts',(5.97091547255935,58.777226615181,39.9058663574108));
#207678=CARTESIAN_POINT('Ctrl Pts',(5.99561386571491,58.866925555679,39.967134470637));
#207679=CARTESIAN_POINT('Ctrl Pts',(5.86337364149639,58.8181995570484,39.8576902534424));
#207680=CARTESIAN_POINT('Ctrl Pts',(5.98915458643854,58.805469618532,39.8579948730703));
#207681=CARTESIAN_POINT('Ctrl Pts',(6.00036140429106,58.9120953679529,39.92499));
#207682=CARTESIAN_POINT('Origin',(5.87405712357929,58.9253704827879,39.92499));
#207683=CARTESIAN_POINT('Origin',(6.10480350526343,61.1207756545817,39.1925554488853));
#207684=CARTESIAN_POINT('Origin',(6.096249069953,61.0393856393803,39.3343017080178));
#207685=CARTESIAN_POINT('Origin',(5.89267880207684,59.1025439184842,39.6398955069219));
#207686=CARTESIAN_POINT('Origin',(5.91130048050402,59.2797173540685,39.3548010137695));
#207687=CARTESIAN_POINT('Ctrl Pts',(6.06175884541631,60.7112330730303,39.3978017080178));
#207688=CARTESIAN_POINT('Ctrl Pts',(6.18806312612808,60.6979579581953,39.3978017080178));
#207689=CARTESIAN_POINT('Ctrl Pts',(6.18806312612808,60.6979579581953,39.5248017080178));
#207690=CARTESIAN_POINT('Ctrl Pts',(6.07140041118295,60.8007259828525,39.3978017080178));
#207691=CARTESIAN_POINT('Ctrl Pts',(6.19746294737696,60.7873912833615,39.3980355775177));
#207692=CARTESIAN_POINT('Ctrl Pts',(6.20217593878221,60.8322324012609,39.5248015517192));
#207693=CARTESIAN_POINT('Ctrl Pts',(6.08051542067653,60.8853484607269,39.3484893995498));
#207694=CARTESIAN_POINT('Ctrl Pts',(6.206395519668,60.8723790316496,39.3489438303431));
#207695=CARTESIAN_POINT('Ctrl Pts',(6.21552060714981,60.9591984396309,39.45083331556));
#207696=CARTESIAN_POINT('Ctrl Pts',(6.08531878138382,60.929944884669,39.2708017080178));
#207697=CARTESIAN_POINT('Ctrl Pts',(6.21110821942996,60.917217374751,39.2710850691866));
#207698=CARTESIAN_POINT('Ctrl Pts',(6.22255335066477,61.0261105245453,39.3343017080178));
#207699=CARTESIAN_POINT('Origin',(6.06175884541631,60.7112330730303,39.5248017080178));
#207700=CARTESIAN_POINT('Ctrl Pts',(5.90061356181316,59.1725467709677,39.2875012672119));
#207701=CARTESIAN_POINT('Ctrl Pts',(6.02658562874881,59.1597945546411,39.2878045257519));
#207702=CARTESIAN_POINT('Ctrl Pts',(6.03762143316813,59.2666022171588,39.3549015218348));
#207703=CARTESIAN_POINT('Ctrl Pts',(5.91250964036517,59.2869113614504,39.1034938540228));
#207704=CARTESIAN_POINT('Ctrl Pts',(6.03858760028819,59.2739830624739,39.1038286278801));
#207705=CARTESIAN_POINT('Ctrl Pts',(6.04723299508931,59.3580501215732,39.2077506434029));
#207706=CARTESIAN_POINT('Ctrl Pts',(5.93388131656935,59.4923630227874,38.989));
#207707=CARTESIAN_POINT('Ctrl Pts',(6.06016587018271,59.4792818168399,38.9892298954611));
#207708=CARTESIAN_POINT('Ctrl Pts',(6.06449973388467,59.5223321697741,39.1161900347291));
#207709=CARTESIAN_POINT('Ctrl Pts',(5.95633285891271,59.7081718144892,38.989));
#207710=CARTESIAN_POINT('Ctrl Pts',(6.08282633453148,59.6948768144682,38.989));
#207711=CARTESIAN_POINT('Ctrl Pts',(6.08263699813626,59.6948967145252,39.1161900945648));
#207712=CARTESIAN_POINT('Origin',(5.95633285891271,59.7081718144892,39.116));
#207713=CARTESIAN_POINT('Origin',(0.347626240494121,6.34489293004957,39.5248017080178));
#207714=CARTESIAN_POINT('Origin',(6.04595329345122,60.5608532912343,39.5248017080178));
#207715=CARTESIAN_POINT('Origin',(0.345047419449927,6.32035708677299,39.116));
#207716=CARTESIAN_POINT('Origin',(5.99823604520107,60.1073400339994,39.1160402713854));
#207717=CARTESIAN_POINT('Ctrl Pts',(6.02238575970336,60.3421421670674,39.2708017080178));
#207718=CARTESIAN_POINT('Ctrl Pts',(6.14931623097308,60.3293058762211,39.27051194648));
#207719=CARTESIAN_POINT('Ctrl Pts',(6.13776734223276,60.2194255397044,39.3343017080178));
#207720=CARTESIAN_POINT('Ctrl Pts',(6.02720817145297,60.3868890390927,39.3487519301186));
#207721=CARTESIAN_POINT('Ctrl Pts',(6.15399567476866,60.3738278099515,39.3482879463982));
#207722=CARTESIAN_POINT('Ctrl Pts',(6.14482385294874,60.2865637544314,39.4512271261636));
#207723=CARTESIAN_POINT('Ctrl Pts',(6.03634362557985,60.4716618705781,39.3978017080178));
#207724=CARTESIAN_POINT('Ctrl Pts',(6.16287156698308,60.4582762833192,39.3975673827397));
#207725=CARTESIAN_POINT('Ctrl Pts',(6.15819229746547,60.4137560077496,39.5248015355181));
#207726=CARTESIAN_POINT('Ctrl Pts',(6.04595329345122,60.5608532912343,39.3978017080178));
#207727=CARTESIAN_POINT('Ctrl Pts',(6.17225757416299,60.5475781763993,39.3978017080178));
#207728=CARTESIAN_POINT('Ctrl Pts',(6.17225757416299,60.5475781763993,39.5248017080178));
#207729=CARTESIAN_POINT('Origin',(6.01146306152099,60.2327006545394,39.3343017080178));
#207730=CARTESIAN_POINT('Origin',(6.00295964283411,60.1517960329196,39.1934008533544));
#207731=CARTESIAN_POINT('Origin',(13.0813452322048,60.0157999988651,39.192555449508));
#207732=CARTESIAN_POINT('Origin',(13.0905908661203,60.0590486699119,39.1160373285273));
#207733=CARTESIAN_POINT('Origin',(13.0643300858388,59.9357500275432,39.3343017080178));
#207734=CARTESIAN_POINT('Ctrl Pts',(13.0409063549245,59.8282880397053,39.2708017080178));
#207735=CARTESIAN_POINT('Ctrl Pts',(12.9173404733289,59.8550545325308,39.2710850691866));
#207736=CARTESIAN_POINT('Ctrl Pts',(12.9401053405456,59.962154812277,39.3343017080178));
#207737=CARTESIAN_POINT('Ctrl Pts',(13.0316624367254,59.7842416555145,39.3487519293518));
#207738=CARTESIAN_POINT('Ctrl Pts',(12.9079350417484,59.8108054559338,39.3492068662936));
#207739=CARTESIAN_POINT('Ctrl Pts',(12.926069636949,59.8961220185284,39.4512271248748));
#207740=CARTESIAN_POINT('Ctrl Pts',(13.0141504107554,59.7007958241043,39.3978017080178));
#207741=CARTESIAN_POINT('Ctrl Pts',(12.8901364125069,59.7270694888874,39.3980347781164));
#207742=CARTESIAN_POINT('Ctrl Pts',(12.8994792219303,59.771023951408,39.5248015355176));
#207743=CARTESIAN_POINT('Ctrl Pts',(12.995727518883,59.6130003254553,39.3978017080178));
#207744=CARTESIAN_POINT('Ctrl Pts',(12.8715027735898,59.6394051101892,39.3978017080178));
#207745=CARTESIAN_POINT('Ctrl Pts',(12.8715027735898,59.6394051101892,39.5248017080178));
#207746=CARTESIAN_POINT('Origin',(12.995727518883,59.6130003254553,39.5248017080178));
#207747=CARTESIAN_POINT('Origin',(0.310561863232988,-0.0660119618346419,
39.116));
#207748=CARTESIAN_POINT('Origin',(13.1739864076113,60.4516424606487,39.116));
#207749=CARTESIAN_POINT('Origin',(0.310561863232988,-0.0660119618346419,
39.5248017080178));
#207750=CARTESIAN_POINT('Origin',(12.9642895838877,59.4650964698965,39.5248017080178));
#207751=CARTESIAN_POINT('Ctrl Pts',(13.2864868029002,60.9782752797347,39.2875012672119));
#207752=CARTESIAN_POINT('Ctrl Pts',(13.1616357280628,61.0052918384388,39.287208709576));
#207753=CARTESIAN_POINT('Ctrl Pts',(13.1392995818866,60.8992893541404,39.3549016990123));
#207754=CARTESIAN_POINT('Ctrl Pts',(13.2624669757413,60.8658306440995,39.103493917393));
#207755=CARTESIAN_POINT('Ctrl Pts',(13.1376969719802,60.8926675943325,39.1031692336351));
#207756=CARTESIAN_POINT('Ctrl Pts',(13.1201818190182,60.8093473519472,39.2077507202316));
#207757=CARTESIAN_POINT('Ctrl Pts',(13.2193155203587,60.663828108008,38.989));
#207758=CARTESIAN_POINT('Ctrl Pts',(13.0947255842066,60.690500823973,38.9887769311152));
#207759=CARTESIAN_POINT('Ctrl Pts',(13.0858375353127,60.6477702018618,39.1161898712892));
#207760=CARTESIAN_POINT('Ctrl Pts',(13.1739864076113,60.4516424606487,38.989));
#207761=CARTESIAN_POINT('Ctrl Pts',(13.0495760763092,60.4780866929065,38.989));
#207762=CARTESIAN_POINT('Ctrl Pts',(13.0497618007396,60.4780472159602,39.1161895903854));
#207763=CARTESIAN_POINT('Origin',(13.2635576885508,60.8730422059012,39.3548010137695));
#207764=CARTESIAN_POINT('Ctrl Pts',(12.9642895838877,59.4650964698965,39.3978017080178));
#207765=CARTESIAN_POINT('Ctrl Pts',(12.8400648385945,59.4915012546304,39.3978017080178));
#207766=CARTESIAN_POINT('Ctrl Pts',(12.8400648385945,59.4915012546304,39.5248017080178));
#207767=CARTESIAN_POINT('Ctrl Pts',(12.9458049943937,59.3770041141843,39.3978017080178));
#207768=CARTESIAN_POINT('Ctrl Pts',(12.8213326038448,59.4033730190106,39.3975666025021));
#207769=CARTESIAN_POINT('Ctrl Pts',(12.8119938336996,59.3594375597987,39.5248015517178));
#207770=CARTESIAN_POINT('Ctrl Pts',(12.92832822063,59.2937057271823,39.3484894016716));
#207771=CARTESIAN_POINT('Ctrl Pts',(12.803709764015,59.3204640761266,39.3480259000045));
#207772=CARTESIAN_POINT('Ctrl Pts',(12.785450697209,59.2345619206646,39.4508333188949));
#207773=CARTESIAN_POINT('Ctrl Pts',(12.9191181862052,59.2498070616278,39.2708017080178));
#207774=CARTESIAN_POINT('Ctrl Pts',(12.7944335023714,59.2768226962997,39.27051194648));
#207775=CARTESIAN_POINT('Ctrl Pts',(12.7714622569326,59.1687514833559,39.3343017080178));
#207776=CARTESIAN_POINT('Origin',(12.8956870022258,59.1423466986221,39.3343017080178));
#207777=CARTESIAN_POINT('Origin',(13.300596971516,61.0472983318851,39.6398955068192));
#207778=CARTESIAN_POINT('Origin',(13.3376362544832,61.2215544576538,39.92499));
#207779=CARTESIAN_POINT('Origin',(12.8787733304445,59.0627741291271,39.1934008539943));
#207780=CARTESIAN_POINT('Origin',(12.869528080115,59.0190342907435,39.1160402713846));
#207781=CARTESIAN_POINT('Ctrl Pts',(13.1038352065734,61.575271693745,40.1599502534424));
#207782=CARTESIAN_POINT('Ctrl Pts',(13.0960702419687,61.5387839176326,40.10025));
#207783=CARTESIAN_POINT('Ctrl Pts',(13.0814171332239,61.4699285681953,40.10025));
#207784=CARTESIAN_POINT('Ctrl Pts',(13.1900205930483,61.5569304518429,40.1599500538461));
#207785=CARTESIAN_POINT('Ctrl Pts',(13.1588482421898,61.5254208297812,40.1002448353481));
#207786=CARTESIAN_POINT('Ctrl Pts',(13.1313027022863,61.4593031273767,40.10025));
#207787=CARTESIAN_POINT('Ctrl Pts',(13.2643407403251,61.5155378539378,40.1202442001038));
#207788=CARTESIAN_POINT('Ctrl Pts',(13.2118511391503,61.4904936222811,40.0633873868015));
#207789=CARTESIAN_POINT('Ctrl Pts',(13.1721300657497,61.4250300340665,40.0772271723537));
#207790=CARTESIAN_POINT('Ctrl Pts',(13.3535591268199,61.4222835584426,40.0045995998163));
#207791=CARTESIAN_POINT('Ctrl Pts',(13.2611962587095,61.4178880557402,39.9663485808318));
#207792=CARTESIAN_POINT('Ctrl Pts',(13.2174099770544,61.3411158595752,40.0101727202466));
#207793=CARTESIAN_POINT('Ctrl Pts',(13.3700167576327,61.3712701109735,39.9304654349859));
#207794=CARTESIAN_POINT('Ctrl Pts',(13.2570896192449,61.3797074995622,39.905190016295));
#207795=CARTESIAN_POINT('Ctrl Pts',(13.2228660458972,61.2924393404512,39.9671857458184));
#207796=CARTESIAN_POINT('Ctrl Pts',(13.3605623192493,61.3267881959111,39.8576902534424));
#207797=CARTESIAN_POINT('Ctrl Pts',(13.2359003894757,61.3537611057082,39.8573998014387));
#207798=CARTESIAN_POINT('Ctrl Pts',(13.21341150919,61.2479592423876,39.92499));
#207799=CARTESIAN_POINT('Origin',(13.0814171332239,61.4699285681953,40.22725));
#207800=CARTESIAN_POINT('Origin',(0.310561863232988,-0.0660119618346419,
39.116));
#207801=CARTESIAN_POINT('Origin',(12.7860306150458,58.6264539577982,39.116));
#207802=CARTESIAN_POINT('Origin',(5.63039444364742E-15,5.53359822473674E-15,
40.22725));
#207803=CARTESIAN_POINT('Origin',(13.0516031943535,61.4762657165314,40.22725));
#207804=CARTESIAN_POINT('Ctrl Pts',(12.7860306150458,58.6264539577982,38.989));
#207805=CARTESIAN_POINT('Ctrl Pts',(12.6616197754744,58.652898298092,38.989));
#207806=CARTESIAN_POINT('Ctrl Pts',(12.6618060089327,58.6528587129484,39.1161901092324));
#207807=CARTESIAN_POINT('Ctrl Pts',(12.7406940127379,58.4142663981465,38.989));
#207808=CARTESIAN_POINT('Ctrl Pts',(12.6165479409694,58.4408495151684,38.9892298989742));
#207809=CARTESIAN_POINT('Ctrl Pts',(12.6257296363319,58.4831327254061,39.1161900493186));
#207810=CARTESIAN_POINT('Ctrl Pts',(12.6975319705105,58.2122676405432,39.1034966344368));
#207811=CARTESIAN_POINT('Ctrl Pts',(12.5736296288419,58.2389323335264,39.1038314102579));
#207812=CARTESIAN_POINT('Ctrl Pts',(12.5913856081756,58.3215567776513,39.2077528789614));
#207813=CARTESIAN_POINT('Ctrl Pts',(12.6735055745747,58.0998260601478,39.2875012672119));
#207814=CARTESIAN_POINT('Ctrl Pts',(12.5497583536238,58.1266254943011,39.2878045257868));
#207815=CARTESIAN_POINT('Ctrl Pts',(12.5722680796271,58.2316158778877,39.35490152959));
#207816=CARTESIAN_POINT('Origin',(12.6964592423899,58.205053781054,39.3548010137695));
#207817=CARTESIAN_POINT('Ctrl Pts',(12.7383709431257,61.4590390555207,39.8576902534424));
#207818=CARTESIAN_POINT('Ctrl Pts',(12.8632261535962,61.4329754599097,39.8573998014387));
#207819=CARTESIAN_POINT('Ctrl Pts',(12.8407372733105,61.3271735965892,39.92499));
#207820=CARTESIAN_POINT('Ctrl Pts',(12.7478306169683,61.5035409747666,39.9304984902492));
#207821=CARTESIAN_POINT('Ctrl Pts',(12.8544171899353,61.4653154597758,39.905217156979));
#207822=CARTESIAN_POINT('Ctrl Pts',(12.8501961180706,61.3716739624487,39.9672049726598));
#207823=CARTESIAN_POINT('Ctrl Pts',(12.7835835513936,61.5432717953611,40.004343767866));
#207824=CARTESIAN_POINT('Ctrl Pts',(12.866248101297,61.5017184029585,39.9661628577646));
#207825=CARTESIAN_POINT('Ctrl Pts',(12.874945307291,61.413745161397,40.0100243556235));
#207826=CARTESIAN_POINT('Ctrl Pts',(12.9020280679178,61.5920631419344,40.1194874821989));
#207827=CARTESIAN_POINT('Ctrl Pts',(12.9401487584136,61.5478406570048,40.0627551483138));
#207828=CARTESIAN_POINT('Ctrl Pts',(12.9498405053869,61.4717924962544,40.0767884282377));
#207829=CARTESIAN_POINT('Ctrl Pts',(12.9874904696727,61.5999795805214,40.1599502015394));
#207830=CARTESIAN_POINT('Ctrl Pts',(13.0031958218447,61.5585057825384,40.1002449453869));
#207831=CARTESIAN_POINT('Ctrl Pts',(13.0015435854432,61.4868843017929,40.10025));
#207832=CARTESIAN_POINT('Ctrl Pts',(13.0739701745332,61.5816197022696,40.1599502534424));
#207833=CARTESIAN_POINT('Ctrl Pts',(13.0662229071073,61.5451281645058,40.10025));
#207834=CARTESIAN_POINT('Ctrl Pts',(13.0516031943535,61.4762657165314,40.10025));
#207835=CARTESIAN_POINT('Origin',(12.7165125280173,61.353578381323,39.92499));
#207836=CARTESIAN_POINT('Origin',(12.659419908459,58.0307974155464,39.6398955069327));
#207837=CARTESIAN_POINT('Origin',(12.6223805745526,57.8565410498765,39.92499));
#207838=CARTESIAN_POINT('Origin',(12.6794732450915,61.1793222555321,39.6398955068273));
#207839=CARTESIAN_POINT('Origin',(12.6424339620849,61.0050661295705,39.3548010137695));
#207840=CARTESIAN_POINT('Ctrl Pts',(12.5994235324478,57.7513140650719,39.8576902534424));
#207841=CARTESIAN_POINT('Ctrl Pts',(12.4758649777959,57.7780756236494,39.8579948730703));
#207842=CARTESIAN_POINT('Ctrl Pts',(12.4981558292594,57.8829458346104,39.92499));
#207843=CARTESIAN_POINT('Ctrl Pts',(12.5899763290081,57.7068710254543,39.930402071123));
#207844=CARTESIAN_POINT('Ctrl Pts',(12.4844883578143,57.7455616498591,39.9058915297379));
#207845=CARTESIAN_POINT('Ctrl Pts',(12.4887087546169,57.8385008428011,39.967152378603));
#207846=CARTESIAN_POINT('Ctrl Pts',(12.5543975270271,57.6673720419785,40.0043257306694));
#207847=CARTESIAN_POINT('Ctrl Pts',(12.4724506530562,57.7092008760995,39.9667894847838));
#207848=CARTESIAN_POINT('Ctrl Pts',(12.4640308112194,57.7966870296828,40.0100138975201));
#207849=CARTESIAN_POINT('Ctrl Pts',(12.436381672743,57.6192799956673,40.1195533054856));
#207850=CARTESIAN_POINT('Ctrl Pts',(12.3985321242208,57.6635313090886,40.0630813209233));
#207851=CARTESIAN_POINT('Ctrl Pts',(12.3892398894932,57.7394080294758,40.076826594242));
#207852=CARTESIAN_POINT('Ctrl Pts',(12.3512461790957,57.6118166447793,40.1599502027519));
#207853=CARTESIAN_POINT('Ctrl Pts',(12.3356888898087,57.6532646075471,40.1002552791541));
#207854=CARTESIAN_POINT('Ctrl Pts',(12.3376071226711,57.7248239067128,40.10025));
#207855=CARTESIAN_POINT('Ctrl Pts',(12.2652136052667,57.6301266171956,40.1599502534424));
#207856=CARTESIAN_POINT('Ctrl Pts',(12.2729791421561,57.6666142715154,40.10025));
#207857=CARTESIAN_POINT('Ctrl Pts',(12.2876333308477,57.7354693911203,40.10025));
#207858=CARTESIAN_POINT('Origin',(12.2876333308477,57.7354693911203,40.22725));
#207859=CARTESIAN_POINT('Ctrl Pts',(12.5528626811454,60.583666384318,38.989));
#207860=CARTESIAN_POINT('Ctrl Pts',(12.6772730231654,60.5572221497821,38.989));
#207861=CARTESIAN_POINT('Ctrl Pts',(12.6770872880011,60.55726162901,39.1161896013264));
#207862=CARTESIAN_POINT('Ctrl Pts',(12.5977568525216,60.795947932685,38.989));
#207863=CARTESIAN_POINT('Ctrl Pts',(12.7224242094588,60.7696393833351,38.9887769275436));
#207864=CARTESIAN_POINT('Ctrl Pts',(12.713163582625,60.7269872521286,39.1161898821822));
#207865=CARTESIAN_POINT('Ctrl Pts',(12.6404975322983,60.9980361136597,39.1034967087243));
#207866=CARTESIAN_POINT('Ctrl Pts',(12.7653961862444,60.9718043534714,39.103172023274));
#207867=CARTESIAN_POINT('Ctrl Pts',(12.74750759382,60.8885631224008,39.2077529615022));
#207868=CARTESIAN_POINT('Ctrl Pts',(12.6642893210148,61.110527437164,39.2875012672119));
#207869=CARTESIAN_POINT('Ctrl Pts',(12.7893350885052,61.084426782332,39.2872087095507));
#207870=CARTESIAN_POINT('Ctrl Pts',(12.7666250660191,60.9785037583491,39.3549017048226));
#207871=CARTESIAN_POINT('Origin',(12.5528626811454,60.583666384318,39.116));
#207872=CARTESIAN_POINT('Origin',(5.67687244506386E-15,5.31008333971855E-15,
40.22725));
#207873=CARTESIAN_POINT('Origin',(12.2578193919774,57.7418065394565,40.22725));
#207874=CARTESIAN_POINT('Origin',(2.3791451040456,12.7200883457668,39.116));
#207875=CARTESIAN_POINT('Origin',(12.4693660187268,60.1910940874971,39.1160373285255));
#207876=CARTESIAN_POINT('Ctrl Pts',(12.2354540642051,57.6364522029206,40.1599502534424));
#207877=CARTESIAN_POINT('Ctrl Pts',(12.2432007592853,57.6729438621905,40.10025));
#207878=CARTESIAN_POINT('Ctrl Pts',(12.2578193919774,57.7418065394565,40.10025));
#207879=CARTESIAN_POINT('Ctrl Pts',(12.1497054461948,57.6546556225243,40.1599500566034));
#207880=CARTESIAN_POINT('Ctrl Pts',(12.1807288143669,57.6862025493687,40.1002551305369));
#207881=CARTESIAN_POINT('Ctrl Pts',(12.2080066271962,57.7523715145536,40.10025));
#207882=CARTESIAN_POINT('Ctrl Pts',(12.0754939174604,57.6955109599433,40.1203070619046));
#207883=CARTESIAN_POINT('Ctrl Pts',(12.127750241416,57.7206875210984,40.0637098684496));
#207884=CARTESIAN_POINT('Ctrl Pts',(12.1670355805169,57.7861609236006,40.0772636213363));
#207885=CARTESIAN_POINT('Ctrl Pts',(11.9863964689869,57.7879231380266,40.0046102245801));
#207886=CARTESIAN_POINT('Ctrl Pts',(12.0782086782662,57.7928648378987,39.9670001894015));
#207887=CARTESIAN_POINT('Ctrl Pts',(12.1215423041379,57.8693039540644,40.0101788811209));
#207888=CARTESIAN_POINT('Ctrl Pts',(11.9699873265234,57.8386735460213,39.9303710930186));
#207889=CARTESIAN_POINT('Ctrl Pts',(12.0820993460723,57.8311081991742,39.9058663574109));
#207890=CARTESIAN_POINT('Ctrl Pts',(12.1160385312535,57.917734074407,39.9671344706364));
#207891=CARTESIAN_POINT('Ctrl Pts',(11.9794294790618,57.8830978693154,39.8576902534424));
#207892=CARTESIAN_POINT('Ctrl Pts',(12.1031907419163,57.857289977851,39.8579948730703));
#207893=CARTESIAN_POINT('Ctrl Pts',(12.1254815933798,57.9621601888119,39.92499));
#207894=CARTESIAN_POINT('Origin',(12.0012568480866,57.9885649735458,39.92499));
#207895=CARTESIAN_POINT('Origin',(12.4602215058074,60.1478239214161,39.1925554488847));
#207896=CARTESIAN_POINT('Origin',(12.4432063593729,60.0677739512124,39.3343017080178));
#207897=CARTESIAN_POINT('Origin',(12.0382961820458,58.1628213391881,39.6398955069227));
#207898=CARTESIAN_POINT('Origin',(12.0753355159239,58.3370777047233,39.3548010137695));
#207899=CARTESIAN_POINT('Ctrl Pts',(12.3746037924171,59.7450242491246,39.3978017080178));
#207900=CARTESIAN_POINT('Ctrl Pts',(12.4988285377102,59.7186194643908,39.3978017080178));
#207901=CARTESIAN_POINT('Ctrl Pts',(12.4988285377102,59.7186194643908,39.5248017080178));
#207902=CARTESIAN_POINT('Ctrl Pts',(12.3935470970145,59.8330190893699,39.3978017080178));
#207903=CARTESIAN_POINT('Ctrl Pts',(12.5175251937997,59.8065803155747,39.3980355775177));
#207904=CARTESIAN_POINT('Ctrl Pts',(12.5268995400901,59.8506831473904,39.5248015517192));
#207905=CARTESIAN_POINT('Ctrl Pts',(12.4114576311024,59.9162252185214,39.3484893995498));
#207906=CARTESIAN_POINT('Ctrl Pts',(12.5352924712502,59.8901687840289,39.3489438303428));
#207907=CARTESIAN_POINT('Ctrl Pts',(12.5534426698453,59.9755587548363,39.4508333155594));
#207908=CARTESIAN_POINT('Ctrl Pts',(12.4208962741593,59.9600752506736,39.2708017080178));
#207909=CARTESIAN_POINT('Ctrl Pts',(12.5446662374493,59.9342688867323,39.2710850691866));
#207910=CARTESIAN_POINT('Ctrl Pts',(12.5674311046661,60.0413691664786,39.3343017080178));
#207911=CARTESIAN_POINT('Origin',(12.3746037924171,59.7450242491246,39.5248017080178));
#207912=CARTESIAN_POINT('Ctrl Pts',(12.0535047649328,58.231611300478,39.2875012672119));
#207913=CARTESIAN_POINT('Ctrl Pts',(12.177453774129,58.2057612755554,39.2878045257519));
#207914=CARTESIAN_POINT('Ctrl Pts',(12.1995935640854,58.3108302788451,39.3549015218347));
#207915=CARTESIAN_POINT('Ctrl Pts',(12.077290030418,58.3441059109578,39.1034938540228));
#207916=CARTESIAN_POINT('Ctrl Pts',(12.2013259468594,58.318069699157,39.1038286278812));
#207917=CARTESIAN_POINT('Ctrl Pts',(12.2187113817826,58.4007725402757,39.2077506434032));
#207918=CARTESIAN_POINT('Ctrl Pts',(12.1200201767774,58.5461981381265,38.989));
#207919=CARTESIAN_POINT('Ctrl Pts',(12.2442455720365,58.5199882620676,38.9892298954612));
#207920=CARTESIAN_POINT('Ctrl Pts',(12.2530556816164,58.5623497685521,39.1161900347288));
#207921=CARTESIAN_POINT('Ctrl Pts',(12.1649068885798,58.7584778814675,38.989));
#207922=CARTESIAN_POINT('Ctrl Pts',(12.2893177137823,58.7320335442279,38.989));
#207923=CARTESIAN_POINT('Ctrl Pts',(12.2891314947143,58.7320731263127,39.1161900945645));
#207924=CARTESIAN_POINT('Origin',(12.1649068885798,58.7584778814675,39.116));
#207925=CARTESIAN_POINT('Origin',(2.31399271319982,12.4135704460892,39.5248017080178));
#207926=CARTESIAN_POINT('Origin',(12.3431658574217,59.5971203935658,39.5248017080178));
#207927=CARTESIAN_POINT('Origin',(2.30379013587727,12.3655710936233,39.116));
#207928=CARTESIAN_POINT('Origin',(12.2483049654007,59.1510793400371,39.1160402713848));
#207929=CARTESIAN_POINT('Ctrl Pts',(12.296865891381,59.3820708699069,39.2708017080178));
#207930=CARTESIAN_POINT('Ctrl Pts',(12.4217592664919,59.3560370505013,39.27051194648));
#207931=CARTESIAN_POINT('Ctrl Pts',(12.398788021053,59.2479658375575,39.3343017080178));
#207932=CARTESIAN_POINT('Ctrl Pts',(12.3063392072231,59.4260685345959,39.3487519301186));
#207933=CARTESIAN_POINT('Ctrl Pts',(12.4310668851193,59.3998259533523,39.3482879463979));
#207934=CARTESIAN_POINT('Ctrl Pts',(12.4128237298768,59.3139986558978,39.4512271261639));
#207935=CARTESIAN_POINT('Ctrl Pts',(12.3242857901782,59.5094220566594,39.3978017080178));
#207936=CARTESIAN_POINT('Ctrl Pts',(12.4487214234133,59.4828840257721,39.3975673827397));
#207937=CARTESIAN_POINT('Ctrl Pts',(12.4394141514348,59.4390967537832,39.5248015355181));
#207938=CARTESIAN_POINT('Ctrl Pts',(12.3431658574217,59.5971203935658,39.3978017080178));
#207939=CARTESIAN_POINT('Ctrl Pts',(12.4673906027149,59.5707156088319,39.3978017080178));
#207940=CARTESIAN_POINT('Ctrl Pts',(12.4673906027149,59.5707156088319,39.5248017080178));
#207941=CARTESIAN_POINT('Origin',(12.2745632757598,59.2743706222914,39.3343017080178));
#207942=CARTESIAN_POINT('Origin',(12.2576496039196,59.194798053941,39.193400853355));
#207943=CARTESIAN_POINT('Origin',(19.2830435999582,58.3196542523187,39.1925554495079));
#207944=CARTESIAN_POINT('Origin',(19.2967593024445,58.3616995707149,39.1160373285249));
#207945=CARTESIAN_POINT('Origin',(19.2577541638585,58.2418213702172,39.3343017080178));
#207946=CARTESIAN_POINT('Ctrl Pts',(19.2232259141446,58.1373965169891,39.2708017080178));
#207947=CARTESIAN_POINT('Ctrl Pts',(19.1031347997394,58.1769325318817,39.2710850691866));
#207948=CARTESIAN_POINT('Ctrl Pts',(19.136969986289,58.2810665285028,39.3343017080178));
#207949=CARTESIAN_POINT('Ctrl Pts',(19.2094285342446,58.0945576760635,39.3487519293518));
#207950=CARTESIAN_POINT('Ctrl Pts',(19.0891556041211,58.1339089916632,39.3492068662935));
#207951=CARTESIAN_POINT('Ctrl Pts',(19.1161088652894,58.2168625998353,39.4512271248748));
#207952=CARTESIAN_POINT('Ctrl Pts',(19.1832899764616,58.0133994748122,39.3978017080178));
#207953=CARTESIAN_POINT('Ctrl Pts',(19.0627016856753,58.0524922023727,39.398034778116));
#207954=CARTESIAN_POINT('Ctrl Pts',(19.0765878066325,58.0952292882353,39.5248015355176));
#207955=CARTESIAN_POINT('Ctrl Pts',(19.1557908785631,57.9280106456674,39.3978017080178));
#207956=CARTESIAN_POINT('Ctrl Pts',(19.0350067009936,57.967255803953,39.3978017080178));
#207957=CARTESIAN_POINT('Ctrl Pts',(19.0350067009936,57.967255803953,39.5248017080178));
#207958=CARTESIAN_POINT('Origin',(19.1557908785631,57.9280106456674,39.5248017080178));
#207959=CARTESIAN_POINT('Origin',(0.301960443923716,-0.098112895714049,
39.116));
#207960=CARTESIAN_POINT('Origin',(19.4207352200707,58.743425483793,39.116));
#207961=CARTESIAN_POINT('Origin',(0.301960443923716,-0.098112895714049,
39.5248017080178));
#207962=CARTESIAN_POINT('Origin',(19.1090650011322,57.7842031819381,39.5248017080178));
#207963=CARTESIAN_POINT('Ctrl Pts',(19.5876674457085,59.2554138597569,39.2875012672119));
#207964=CARTESIAN_POINT('Ctrl Pts',(19.4663243174862,59.2953329099158,39.287208709576));
#207965=CARTESIAN_POINT('Ctrl Pts',(19.4330302542698,59.1922458813525,39.3549016990124));
#207966=CARTESIAN_POINT('Ctrl Pts',(19.5520255367116,59.1460959632215,39.1034939173931));
#207967=CARTESIAN_POINT('Ctrl Pts',(19.4307442612541,59.1858279145874,39.1031692336328));
#207968=CARTESIAN_POINT('Ctrl Pts',(19.4046157212346,59.1047949412331,39.207750720231));
#207969=CARTESIAN_POINT('Ctrl Pts',(19.4879954548418,58.9497105734778,38.989));
#207970=CARTESIAN_POINT('Ctrl Pts',(19.366876093407,58.9892603680788,38.9887769311182));
#207971=CARTESIAN_POINT('Ctrl Pts',(19.3535701679106,58.9476928828777,39.11618987129));
#207972=CARTESIAN_POINT('Ctrl Pts',(19.4207352200707,58.743425483793,38.989));
#207973=CARTESIAN_POINT('Ctrl Pts',(19.2997705965407,58.7827292725253,38.989));
#207974=CARTESIAN_POINT('Ctrl Pts',(19.299951177089,58.7826705983484,39.1161895903857));
#207975=CARTESIAN_POINT('Origin',(19.5538640879539,59.1531540087997,39.3548010137695));
#207976=CARTESIAN_POINT('Ctrl Pts',(19.1090650011322,57.7842031819381,39.3978017080178));
#207977=CARTESIAN_POINT('Ctrl Pts',(18.9882808235627,57.8234483402237,39.3978017080178));
#207978=CARTESIAN_POINT('Ctrl Pts',(18.9882808235627,57.8234483402237,39.5248017080178));
#207979=CARTESIAN_POINT('Ctrl Pts',(19.0814735135856,57.6985255711016,39.3978017080178));
#207980=CARTESIAN_POINT('Ctrl Pts',(18.9604392969159,57.7377609320109,39.3975666025035));
#207981=CARTESIAN_POINT('Ctrl Pts',(18.9465591794953,57.6950423231336,39.5248015517178));
#207982=CARTESIAN_POINT('Ctrl Pts',(19.0553854270312,57.6175103216836,39.3484894016716));
#207983=CARTESIAN_POINT('Ctrl Pts',(18.9342466524546,57.6571482613582,39.3480259000032));
#207984=CARTESIAN_POINT('Ctrl Pts',(18.9071083904259,57.5736252790862,39.4508333188947));
#207985=CARTESIAN_POINT('Ctrl Pts',(19.0416371860884,57.5748148483574,39.2708017080178));
#207986=CARTESIAN_POINT('Ctrl Pts',(18.9204594407751,57.61471558695,39.2705119464801));
#207987=CARTESIAN_POINT('Ctrl Pts',(18.8863175164099,57.5096375484035,39.3343017080178));
#207988=CARTESIAN_POINT('Origin',(19.0071016939793,57.4703923901179,39.3343017080178));
#207989=CARTESIAN_POINT('Origin',(19.6089151909165,59.3225838821656,39.6398955068179));
#207990=CARTESIAN_POINT('Origin',(19.6639662938568,59.4920137553137,39.92499));
#207991=CARTESIAN_POINT('Origin',(18.9819630786535,57.3930236876039,39.1934008539944));
#207992=CARTESIAN_POINT('Origin',(18.9681964166836,57.350489852441,39.1160402713847));
#207993=CARTESIAN_POINT('Ctrl Pts',(19.4684195516703,59.868232155624,40.1599502534424));
#207994=CARTESIAN_POINT('Ctrl Pts',(19.456883113189,59.8327559231844,40.10025));
#207995=CARTESIAN_POINT('Ctrl Pts',(19.4351129318427,59.7658094374949,40.10025));
#207996=CARTESIAN_POINT('Ctrl Pts',(19.55221562375,59.8409825629602,40.159950053847));
#207997=CARTESIAN_POINT('Ctrl Pts',(19.5179203859198,59.8129039518391,40.1002448353493));
#207998=CARTESIAN_POINT('Ctrl Pts',(19.4836145615386,59.7500277420817,40.10025));
#207999=CARTESIAN_POINT('Ctrl Pts',(19.621801932834,59.7920481472521,40.1202442001036));
#208000=CARTESIAN_POINT('Ctrl Pts',(19.5669820401376,59.7726277678653,40.0633873868015));
#208001=CARTESIAN_POINT('Ctrl Pts',(19.520635754657,59.7116747787977,40.0772271723537));
#208002=CARTESIAN_POINT('Ctrl Pts',(19.7007838434713,59.6899788477097,40.0045995998165));
#208003=CARTESIAN_POINT('Ctrl Pts',(19.6084674936738,59.6952619726975,39.9663485808318));
#208004=CARTESIAN_POINT('Ctrl Pts',(19.5568961981644,59.6234872553903,40.0101727202466));
#208005=CARTESIAN_POINT('Ctrl Pts',(19.7118189603907,59.6375245663853,39.9304654349857));
#208006=CARTESIAN_POINT('Ctrl Pts',(19.6003923959459,59.6577198343137,39.9051900162949));
#208007=CARTESIAN_POINT('Ctrl Pts',(19.5572342963496,59.5745070768387,39.9671857458178));
#208008=CARTESIAN_POINT('Ctrl Pts',(19.6977666881852,59.5942745858234,39.8576902534424));
#208009=CARTESIAN_POINT('Ctrl Pts',(19.5766071063175,59.6341304551455,39.8573998014387));
#208010=CARTESIAN_POINT('Ctrl Pts',(19.5431821162873,59.5312589135993,39.92499));
#208011=CARTESIAN_POINT('Origin',(19.4351129318427,59.7658094374949,40.22725));
#208012=CARTESIAN_POINT('Origin',(0.301960443923716,-0.098112895714049,
39.116));
#208013=CARTESIAN_POINT('Origin',(18.8441205405526,56.9687879773464,39.116));
#208014=CARTESIAN_POINT('Origin',(5.61372323131277E-15,5.53806526261865E-15,
40.22725));
#208015=CARTESIAN_POINT('Origin',(19.406124729226,59.7752282754835,40.22725));
#208016=CARTESIAN_POINT('Ctrl Pts',(18.8441205405526,56.9687879773464,38.989));
#208017=CARTESIAN_POINT('Ctrl Pts',(18.7231554228307,57.0080919266514,38.989));
#208018=CARTESIAN_POINT('Ctrl Pts',(18.7233364983085,57.0080330916621,39.1161901092324));
#208019=CARTESIAN_POINT('Ctrl Pts',(18.7768526573605,56.7625017687172,38.989));
#208020=CARTESIAN_POINT('Ctrl Pts',(18.656165363134,56.8019160587468,38.9892298989742));
#208021=CARTESIAN_POINT('Ctrl Pts',(18.6697165591974,56.8430078886276,39.1161900493186));
#208022=CARTESIAN_POINT('Ctrl Pts',(18.712812441602,56.566121243389,39.1034966344368));
#208023=CARTESIAN_POINT('Ctrl Pts',(18.5923760693066,56.605591185762,39.1038314102574));
#208024=CARTESIAN_POINT('Ctrl Pts',(18.6186713857003,56.6859069993037,39.2077528789611));
#208025=CARTESIAN_POINT('Ctrl Pts',(18.6771643191716,56.4568070719809,39.2875012672119));
#208026=CARTESIAN_POINT('Ctrl Pts',(18.5568963021134,56.4963948028695,39.2878045257868));
#208027=CARTESIAN_POINT('Ctrl Pts',(18.5902572009367,56.5984571310818,39.35490152959));
#208028=CARTESIAN_POINT('Origin',(18.7109915363523,56.5590590327987,39.3548010137695));
#208029=CARTESIAN_POINT('Ctrl Pts',(19.0928077206418,59.7908376697909,39.8576902534424));
#208030=CARTESIAN_POINT('Ctrl Pts',(19.214254573609,59.7518659300023,39.8573998014387));
#208031=CARTESIAN_POINT('Ctrl Pts',(19.1808295835788,59.6489943884562,39.92499));
#208032=CARTESIAN_POINT('Ctrl Pts',(19.1068672906319,59.8341069976972,39.9304984902491));
#208033=CARTESIAN_POINT('Ctrl Pts',(19.2088743168593,59.7849495554005,39.9052171569788));
#208034=CARTESIAN_POINT('Ctrl Pts',(19.1948881666556,59.6922622581476,39.9672049726605));
#208035=CARTESIAN_POINT('Ctrl Pts',(19.1465773683635,59.8698829694065,40.0043437678661));
#208036=CARTESIAN_POINT('Ctrl Pts',(19.224445560962,59.8199164124671,39.9661628577643));
#208037=CARTESIAN_POINT('Ctrl Pts',(19.2238994150019,59.7315159919506,40.0100243556235));
#208038=CARTESIAN_POINT('Ctrl Pts',(19.2694731179107,59.9060262085834,40.1194874821988));
#208039=CARTESIAN_POINT('Ctrl Pts',(19.3027624708836,59.8580612818571,40.0627551483141));
#208040=CARTESIAN_POINT('Ctrl Pts',(19.3044519280757,59.7814166574707,40.0767884282377));
#208041=CARTESIAN_POINT('Ctrl Pts',(19.3552948408472,59.9049660265687,40.1599502015391));
#208042=CARTESIAN_POINT('Ctrl Pts',(19.3665789650881,59.862077770064,40.1002449453885));
#208043=CARTESIAN_POINT('Ctrl Pts',(19.3574492964906,59.7910213450152,40.10025));
#208044=CARTESIAN_POINT('Ctrl Pts',(19.4393816709763,59.8776671349983,40.1599502534424));
#208045=CARTESIAN_POINT('Ctrl Pts',(19.4278624395273,59.842185311655,40.10025));
#208046=CARTESIAN_POINT('Ctrl Pts',(19.406124729226,59.7752282754835,40.10025));
#208047=CARTESIAN_POINT('Origin',(19.0600454060093,59.6882395467418,39.92499));
#208048=CARTESIAN_POINT('Origin',(18.6559403576659,56.3896289265475,39.6398955069309));
#208049=CARTESIAN_POINT('Origin',(18.6008891789892,56.2201988201381,39.92499));
#208050=CARTESIAN_POINT('Origin',(19.0049943031095,59.5188096735647,39.6398955068273));
#208051=CARTESIAN_POINT('Origin',(18.9499432001064,59.3493798002278,39.3548010137695));
#208052=CARTESIAN_POINT('Ctrl Pts',(18.5670586829472,56.1179479440986,39.8576902534424));
#208053=CARTESIAN_POINT('Ctrl Pts',(18.4469743395785,56.1574782858995,39.8579948730703));
#208054=CARTESIAN_POINT('Ctrl Pts',(18.4801050014197,56.2594439784237,39.92499));
#208055=CARTESIAN_POINT('Ctrl Pts',(18.5530176696416,56.0747358697601,39.9304020711231));
#208056=CARTESIAN_POINT('Ctrl Pts',(18.4521518441046,56.1242410383984,39.9058915297382));
#208057=CARTESIAN_POINT('Ctrl Pts',(18.4660639121468,56.2162299491245,39.9671523786031));
#208058=CARTESIAN_POINT('Ctrl Pts',(18.5135050040178,56.0391722633446,40.0043257306692));
#208059=CARTESIAN_POINT('Ctrl Pts',(18.4363793473476,56.0893377355413,39.9667894847835));
#208060=CARTESIAN_POINT('Ctrl Pts',(18.4371504234769,56.1772247439498,40.01001389752));
#208061=CARTESIAN_POINT('Ctrl Pts',(18.3911086652354,56.0036796861842,40.1195533054858));
#208062=CARTESIAN_POINT('Ctrl Pts',(18.3580919822899,56.0516449414231,40.0630813209236));
#208063=CARTESIAN_POINT('Ctrl Pts',(18.3567819283759,56.1280773042131,40.0768265942421));
#208064=CARTESIAN_POINT('Ctrl Pts',(18.305659420131,56.0051563026342,40.1599502027515));
#208065=CARTESIAN_POINT('Ctrl Pts',(18.2945198471564,56.0480033886679,40.1002552791541));
#208066=CARTESIAN_POINT('Ctrl Pts',(18.3039075553125,56.1189701685706,40.10025));
#208067=CARTESIAN_POINT('Ctrl Pts',(18.2220120550223,56.0323588238389,40.1599502534424));
#208068=CARTESIAN_POINT('Ctrl Pts',(18.2335490499224,56.067834875333,40.10025));
#208069=CARTESIAN_POINT('Ctrl Pts',(18.2553202812755,56.134781019564,40.10025));
#208070=CARTESIAN_POINT('Origin',(18.2553202812755,56.134781019564,40.22725));
#208071=CARTESIAN_POINT('Ctrl Pts',(18.8168143322233,58.9396512752211,38.989));
#208072=CARTESIAN_POINT('Ctrl Pts',(18.9377789661745,58.9003474831028,38.989));
#208073=CARTESIAN_POINT('Ctrl Pts',(18.9375983751895,58.9004061606707,39.1161896013268));
#208074=CARTESIAN_POINT('Ctrl Pts',(18.8836520326613,59.1460772043115,38.989));
#208075=CARTESIAN_POINT('Ctrl Pts',(19.004886456538,59.1068814887034,38.9887769275436));
#208076=CARTESIAN_POINT('Ctrl Pts',(18.9912181986579,59.0654310094279,39.1161898821825));
#208077=CARTESIAN_POINT('Ctrl Pts',(18.9472825415237,59.3425907075099,39.1034967087243));
#208078=CARTESIAN_POINT('Ctrl Pts',(19.0687550219952,59.3034471832925,39.1031720232725));
#208079=CARTESIAN_POINT('Ctrl Pts',(19.0422633471881,59.2225318234682,39.2077529615018));
#208080=CARTESIAN_POINT('Ctrl Pts',(18.9827025415103,59.4519788726605,39.2875012672119));
#208081=CARTESIAN_POINT('Ctrl Pts',(19.1043350338631,59.4129503580328,39.2872087095507));
#208082=CARTESIAN_POINT('Ctrl Pts',(19.0706774483344,59.3099814352091,39.3549017048228));
#208083=CARTESIAN_POINT('Origin',(18.8168143322233,58.9396512752211,39.116));
#208084=CARTESIAN_POINT('Origin',(5.68280300381509E-15,5.3084942512905E-15,
40.22725));
#208085=CARTESIAN_POINT('Origin',(18.2263320786588,56.1441998575526,40.22725));
#208086=CARTESIAN_POINT('Origin',(5.63975536249314,18.3848338156965,39.116));
#208087=CARTESIAN_POINT('Origin',(18.6927400943511,58.557957308326,39.1160373285235));
#208088=CARTESIAN_POINT('Ctrl Pts',(18.1930767435955,56.0417604764381,40.1599502534424));
#208089=CARTESIAN_POINT('Ctrl Pts',(18.2045954185351,56.0772424804482,40.10025));
#208090=CARTESIAN_POINT('Ctrl Pts',(18.2263320786588,56.1441998575526,40.10025));
#208091=CARTESIAN_POINT('Ctrl Pts',(18.109700640964,56.0688273470721,40.1599500566042));
#208092=CARTESIAN_POINT('Ctrl Pts',(18.1438516116619,56.0969586315456,40.1002551305369));
#208093=CARTESIAN_POINT('Ctrl Pts',(18.1778965340261,56.1599138083631,40.10025));
#208094=CARTESIAN_POINT('Ctrl Pts',(18.0401661963857,56.1172160917338,40.1203070619046));
#208095=CARTESIAN_POINT('Ctrl Pts',(18.0947679219785,56.1367924598132,40.0637098684499));
#208096=CARTESIAN_POINT('Ctrl Pts',(18.1406818860301,56.1978007560411,40.0772636213362));
#208097=CARTESIAN_POINT('Ctrl Pts',(17.9612165360197,56.2184352456062,40.0046102245802));
#208098=CARTESIAN_POINT('Ctrl Pts',(18.053042336704,56.2137528851846,39.9670001894012));
#208099=CARTESIAN_POINT('Ctrl Pts',(18.104128639785,56.2852436625533,40.0101788811209));
#208100=CARTESIAN_POINT('Ctrl Pts',(17.9502021467132,56.2706228600011,39.9303710930186));
#208101=CARTESIAN_POINT('Ctrl Pts',(18.0609092108094,56.2513800597966,39.9058663574109));
#208102=CARTESIAN_POINT('Ctrl Pts',(18.1037173431996,56.3339837785513,39.9671344706363));
#208103=CARTESIAN_POINT('Ctrl Pts',(17.9642361803979,56.3138168485093,39.8576902534424));
#208104=CARTESIAN_POINT('Ctrl Pts',(18.0846218068701,56.2752137607564,39.8579948730703));
#208105=CARTESIAN_POINT('Ctrl Pts',(18.1177524687112,56.3771794532805,39.92499));
#208106=CARTESIAN_POINT('Origin',(17.9969682911417,56.4164246115661,39.92499));
#208107=CARTESIAN_POINT('Origin',(18.6791227120638,58.5158800426259,39.1925554488841));
#208108=CARTESIAN_POINT('Origin',(18.6538332760111,58.4380471616453,39.3343017080178));
#208109=CARTESIAN_POINT('Origin',(18.0520194698704,56.5858547179429,39.6398955069215));
#208110=CARTESIAN_POINT('Origin',(18.1070706485049,56.7552848242268,39.3548010137695));
#208111=CARTESIAN_POINT('Ctrl Pts',(18.5518699907157,58.1242364370955,39.3978017080178));
#208112=CARTESIAN_POINT('Ctrl Pts',(18.6726541682852,58.0849912788098,39.3978017080178));
#208113=CARTESIAN_POINT('Ctrl Pts',(18.6726541682852,58.0849912788098,39.5248017080178));
#208114=CARTESIAN_POINT('Ctrl Pts',(18.5799074873344,58.2097691178802,39.3978017080178));
#208115=CARTESIAN_POINT('Ctrl Pts',(18.7004428147375,58.1705159385202,39.3980355775163));
#208116=CARTESIAN_POINT('Ctrl Pts',(18.7143758086146,58.2133972843955,39.5248015517178));
#208117=CARTESIAN_POINT('Ctrl Pts',(18.6064173144583,58.2906472745453,39.3484893995498));
#208118=CARTESIAN_POINT('Ctrl Pts',(18.7268501353397,58.2517893143851,39.3489438303433));
#208119=CARTESIAN_POINT('Ctrl Pts',(18.7538265876731,58.3348142976327,39.4508333155602));
#208120=CARTESIAN_POINT('Ctrl Pts',(18.6203878281154,58.3332704847794,39.2708017080178));
#208121=CARTESIAN_POINT('Ctrl Pts',(18.7407822670309,58.2946680067386,39.2710850691866));
#208122=CARTESIAN_POINT('Ctrl Pts',(18.7746174535806,58.3988020033596,39.3343017080178));
#208123=CARTESIAN_POINT('Origin',(18.5518699907157,58.1242364370955,39.5248017080178));
#208124=CARTESIAN_POINT('Ctrl Pts',(18.0743352474898,56.6526781108321,39.2875012672119));
#208125=CARTESIAN_POINT('Ctrl Pts',(18.1949031876639,56.614013495596,39.2878045257519));
#208126=CARTESIAN_POINT('Ctrl Pts',(18.2279043949854,56.7161926816709,39.3549015218347));
#208127=CARTESIAN_POINT('Ctrl Pts',(18.1097491035613,56.7620702268156,39.1034938540228));
#208128=CARTESIAN_POINT('Ctrl Pts',(18.2303840130663,56.7232113603676,39.1038286278797));
#208129=CARTESIAN_POINT('Ctrl Pts',(18.2563190096467,56.8036438738764,39.2077506434024));
#208130=CARTESIAN_POINT('Ctrl Pts',(18.1733695596542,56.9585888550839,38.989));
#208131=CARTESIAN_POINT('Ctrl Pts',(18.2941747571336,56.919537469806,38.9892298954617));
#208132=CARTESIAN_POINT('Ctrl Pts',(18.307364587184,56.9607460083087,39.1161900347294));
#208133=CARTESIAN_POINT('Ctrl Pts',(18.2401996527051,57.1650137687745,38.989));
#208134=CARTESIAN_POINT('Ctrl Pts',(18.361164756456,57.125709824009,38.989));
#208135=CARTESIAN_POINT('Ctrl Pts',(18.3609836949701,57.125768654452,39.1161900945644));
#208136=CARTESIAN_POINT('Origin',(18.2401996527051,57.1650137687745,39.116));
#208137=CARTESIAN_POINT('Origin',(5.49583002221492,17.9418771653399,39.5248017080178));
#208138=CARTESIAN_POINT('Origin',(18.5051441132848,57.9804289733662,39.5248017080178));
#208139=CARTESIAN_POINT('Origin',(5.47329194811203,17.8725121057138,39.116));
#208140=CARTESIAN_POINT('Origin',(18.3641788932758,57.5467470426658,39.116040271385));
#208141=CARTESIAN_POINT('Ctrl Pts',(18.4366189870679,57.7713971777985,39.2708017080178));
#208142=CARTESIAN_POINT('Ctrl Pts',(18.5581069080667,57.7324510618068,39.27051194648));
#208143=CARTESIAN_POINT('Ctrl Pts',(18.5239649837014,57.6273730232603,39.3343017080178));
#208144=CARTESIAN_POINT('Ctrl Pts',(18.4506394153725,57.8141635875296,39.3487519301186));
#208145=CARTESIAN_POINT('Ctrl Pts',(18.5719407253098,57.7750271733906,39.3482879463984));
#208146=CARTESIAN_POINT('Ctrl Pts',(18.5448261124699,57.6915769758379,39.451227126164));
#208147=CARTESIAN_POINT('Ctrl Pts',(18.4772005006382,57.8951845615404,39.3978017080178));
#208148=CARTESIAN_POINT('Ctrl Pts',(18.5981804828681,57.8557848432477,39.3975673827401));
#208149=CARTESIAN_POINT('Ctrl Pts',(18.5843471808463,57.8132103173516,39.5248015355181));
#208150=CARTESIAN_POINT('Ctrl Pts',(18.5051441132848,57.9804289733662,39.3978017080178));
#208151=CARTESIAN_POINT('Ctrl Pts',(18.6259282908542,57.9411838150805,39.3978017080178));
#208152=CARTESIAN_POINT('Ctrl Pts',(18.6259282908542,57.9411838150805,39.5248017080178));
#208153=CARTESIAN_POINT('Origin',(18.4031808061319,57.666618181546,39.3343017080178));
#208154=CARTESIAN_POINT('Origin',(18.3780421908675,57.5892494801764,39.1934008533551));
#208155=CARTESIAN_POINT('Origin',(25.273472906796,55.9845461696116,39.1925554495081));
#208156=CARTESIAN_POINT('Origin',(25.2915084057467,56.0249274780509,39.1160373285247));
#208157=CARTESIAN_POINT('Origin',(25.2401862573148,55.9097831300744,39.3343017080178));
#208158=CARTESIAN_POINT('Ctrl Pts',(25.1949317875307,55.8095395120004,39.2708017080178));
#208159=CARTESIAN_POINT('Ctrl Pts',(25.079631183696,55.8614118841076,39.2710850691866));
#208160=CARTESIAN_POINT('Ctrl Pts',(25.1241659841942,55.961438683745,39.3343017080178));
#208161=CARTESIAN_POINT('Ctrl Pts',(25.1767321129116,55.7683775656456,39.3487519293517));
#208162=CARTESIAN_POINT('Ctrl Pts',(25.0612313830309,55.8200852551827,39.3492068662942));
#208163=CARTESIAN_POINT('Ctrl Pts',(25.0967080045995,55.8997670518382,39.4512271248752));
#208164=CARTESIAN_POINT('Ctrl Pts',(25.1422534028249,55.6903961807895,39.3978017080178));
#208165=CARTESIAN_POINT('Ctrl Pts',(25.0264120100491,55.74187966302,39.398034778116));
#208166=CARTESIAN_POINT('Ctrl Pts',(25.0446893032922,55.7829311357713,39.5248015355176));
#208167=CARTESIAN_POINT('Ctrl Pts',(25.1059793847708,55.6083495590299,39.3978017080178));
#208168=CARTESIAN_POINT('Ctrl Pts',(24.9899591116502,55.6600051127005,39.3978017080178));
#208169=CARTESIAN_POINT('Ctrl Pts',(24.9899591116502,55.6600051127005,39.5248017080178));
#208170=CARTESIAN_POINT('Origin',(25.1059793847708,55.6083495590299,39.5248017080178));
#208171=CARTESIAN_POINT('Origin',(0.29005068280153,-0.12913888417657,39.116));
#208172=CARTESIAN_POINT('Origin',(25.454706393409,56.3916032444848,39.116));
#208173=CARTESIAN_POINT('Origin',(0.29005068280153,-0.12913888417657,39.5248017080178));
#208174=CARTESIAN_POINT('Origin',(25.0444775033954,55.4702140717964,39.5248017080178));
#208175=CARTESIAN_POINT('Ctrl Pts',(25.6742415049986,56.8833377255391,39.2875012672119));
#208176=CARTESIAN_POINT('Ctrl Pts',(25.5577357840972,56.9357219056858,39.287208709576));
#208177=CARTESIAN_POINT('Ctrl Pts',(25.5138485805642,56.8366797759148,39.3549016990125));
#208178=CARTESIAN_POINT('Ctrl Pts',(25.627368014374,56.7783442778554,39.1034939173931));
#208179=CARTESIAN_POINT('Ctrl Pts',(25.510904250253,56.8305359187817,39.1031692336344));
#208180=CARTESIAN_POINT('Ctrl Pts',(25.4764485929327,56.7526780286695,39.2077507202307));
#208181=CARTESIAN_POINT('Ctrl Pts',(25.5431608329957,56.5897276738848,38.989));
#208182=CARTESIAN_POINT('Ctrl Pts',(25.4268390553479,56.6417212312948,38.9887769311158));
#208183=CARTESIAN_POINT('Ctrl Pts',(25.4092610357536,56.6017723050709,39.1161898712902));
#208184=CARTESIAN_POINT('Ctrl Pts',(25.454706393409,56.3916032444848,38.989));
#208185=CARTESIAN_POINT('Ctrl Pts',(25.33851279138,56.4433359691574,38.989));
#208186=CARTESIAN_POINT('Ctrl Pts',(25.3386862495677,56.4432587405965,39.1161895903859));
#208187=CARTESIAN_POINT('Origin',(25.6299342605002,56.7851714777844,39.3548010137695));
#208188=CARTESIAN_POINT('Ctrl Pts',(25.0444775033954,55.4702140717964,39.3978017080178));
#208189=CARTESIAN_POINT('Ctrl Pts',(24.9284572302748,55.521869625467,39.3978017080178));
#208190=CARTESIAN_POINT('Ctrl Pts',(24.9284572302748,55.521869625467,39.5248017080178));
#208191=CARTESIAN_POINT('Ctrl Pts',(25.0080814159069,55.3878899076694,39.3978017080178));
#208192=CARTESIAN_POINT('Ctrl Pts',(24.891811449322,55.4395618538376,39.3975666025031));
#208193=CARTESIAN_POINT('Ctrl Pts',(24.8735420580987,55.3985281293144,39.5248015517182));
#208194=CARTESIAN_POINT('Ctrl Pts',(24.9736678430993,55.3100454158607,39.3484894016716));
#208195=CARTESIAN_POINT('Ctrl Pts',(24.857335972326,55.362128664703,39.3480259000036));
#208196=CARTESIAN_POINT('Ctrl Pts',(24.8216158475498,55.281899950892,39.4508333188946));
#208197=CARTESIAN_POINT('Ctrl Pts',(24.9555320242421,55.2690209153037,39.2708017080178));
#208198=CARTESIAN_POINT('Ctrl Pts',(24.8391888661851,55.3213695969753,39.27051194648));
#208199=CARTESIAN_POINT('Ctrl Pts',(24.7942503289613,55.2204359898053,39.3343017080178));
#208200=CARTESIAN_POINT('Origin',(24.910270602082,55.1687804361347,39.3343017080178));
#208201=CARTESIAN_POINT('Origin',(25.7023940320534,56.9479187893822,39.6398955068185));
#208202=CARTESIAN_POINT('Origin',(25.7748538035653,57.1106661007662,39.92499));
#208203=CARTESIAN_POINT('Origin',(24.877182467142,55.0944632682965,39.1934008539949));
#208204=CARTESIAN_POINT('Origin',(24.8590452239608,55.0536014459534,39.1160402713848));
#208205=CARTESIAN_POINT('Ctrl Pts',(25.6197038181304,57.5052637377729,40.1599502534424));
#208206=CARTESIAN_POINT('Ctrl Pts',(25.6045223014068,57.4711877340326,40.10025));
#208207=CARTESIAN_POINT('Ctrl Pts',(25.5758735661215,57.4068835917977,40.10025));
#208208=CARTESIAN_POINT('Ctrl Pts',(25.7001924885135,57.4694043465857,40.1599500538455));
#208209=CARTESIAN_POINT('Ctrl Pts',(25.6631501095111,57.4450643815376,40.1002448353481));
#208210=CARTESIAN_POINT('Ctrl Pts',(25.622459862445,57.3861185493433,40.10025));
#208211=CARTESIAN_POINT('Ctrl Pts',(25.7642825572406,57.413464248775,40.1202442001039));
#208212=CARTESIAN_POINT('Ctrl Pts',(25.7077329912395,57.399880495399,40.0633873868017));
#208213=CARTESIAN_POINT('Ctrl Pts',(25.6552692732811,57.3441059191828,40.0772271723538));
#208214=CARTESIAN_POINT('Ctrl Pts',(25.8321626496797,57.3036982377899,40.0045995998162));
#208215=CARTESIAN_POINT('Ctrl Pts',(25.7409042554413,57.3186021074446,39.9663485808314));
#208216=CARTESIAN_POINT('Ctrl Pts',(25.6821129719832,57.2526112478168,40.0101727202466));
#208217=CARTESIAN_POINT('Ctrl Pts',(25.8376543496551,57.2503778226938,39.9304654349859));
#208218=CARTESIAN_POINT('Ctrl Pts',(25.7289491719115,57.28210970638,39.9051900162952));
#208219=CARTESIAN_POINT('Ctrl Pts',(25.6773293952371,57.2038640469256,39.9671857458183));
#208220=CARTESIAN_POINT('Ctrl Pts',(25.8191582032627,57.2088336324696,39.8576902534424));
#208221=CARTESIAN_POINT('Ctrl Pts',(25.702828419034,57.2611357920722,39.8573998014387));
#208222=CARTESIAN_POINT('Ctrl Pts',(25.6588335304447,57.1623216544368,39.92499));
#208223=CARTESIAN_POINT('Origin',(25.5758735661215,57.4068835917977,40.22725));
#208224=CARTESIAN_POINT('Origin',(0.29005068280153,-0.12913888417657,39.116));
#208225=CARTESIAN_POINT('Origin',(24.6957503380314,54.6869600343295,39.116));
#208226=CARTESIAN_POINT('Origin',(5.59761027822878E-15,5.54425044580581E-15,
40.22725));
#208227=CARTESIAN_POINT('Origin',(25.5480287005725,57.4192809246786,40.22725));
#208228=CARTESIAN_POINT('Ctrl Pts',(24.6957503380314,54.6869600343295,38.989));
#208229=CARTESIAN_POINT('Ctrl Pts',(24.5795562613026,54.738692970352,38.989));
#208230=CARTESIAN_POINT('Ctrl Pts',(24.5797301948987,54.7386155301257,39.1161901092321));
#208231=CARTESIAN_POINT('Ctrl Pts',(24.6072881749609,54.4888352915923,38.989));
#208232=CARTESIAN_POINT('Ctrl Pts',(24.4913819335275,54.540648923418,38.989229898976));
#208233=CARTESIAN_POINT('Ctrl Pts',(24.5091541605501,54.5800991622545,39.1161900493183));
#208234=CARTESIAN_POINT('Ctrl Pts',(24.5230714236775,54.3002245846698,39.1034966344368));
#208235=CARTESIAN_POINT('Ctrl Pts',(24.4074205468513,54.3520673354873,39.1038314102562));
#208236=CARTESIAN_POINT('Ctrl Pts',(24.4419671033168,54.4291945615862,39.2077528789614));
#208237=CARTESIAN_POINT('Ctrl Pts',(24.4761921430398,54.1952354911869,39.2875012672119));
#208238=CARTESIAN_POINT('Ctrl Pts',(24.3607210114372,54.2471777873468,39.2878045257868));
#208239=CARTESIAN_POINT('Ctrl Pts',(24.4045675740913,54.3451938439588,39.3549015295899));
#208240=CARTESIAN_POINT('Origin',(24.5205222915158,54.2933913980361,39.3548010137695));
#208241=CARTESIAN_POINT('Ctrl Pts',(25.2380597013437,57.4675553545137,39.8576902534424));
#208242=CARTESIAN_POINT('Ctrl Pts',(25.3547675996722,57.416102453084,39.8573998014387));
#208243=CARTESIAN_POINT('Ctrl Pts',(25.3107727110829,57.3172883154487,39.92499));
#208244=CARTESIAN_POINT('Ctrl Pts',(25.2565651278917,57.5091180232689,39.9304984902492));
#208245=CARTESIAN_POINT('Ctrl Pts',(25.3528749970543,57.44956723289,39.905217156979));
#208246=CARTESIAN_POINT('Ctrl Pts',(25.3292770036986,57.3588496371387,39.9672049726596));
#208247=CARTESIAN_POINT('Ctrl Pts',(25.2997972770066,57.5405471770605,40.0043437678661));
#208248=CARTESIAN_POINT('Ctrl Pts',(25.3720159720868,57.4827148996386,39.9661628577646));
#208249=CARTESIAN_POINT('Ctrl Pts',(25.3622324578628,57.3948558336727,40.0100243556237));
#208250=CARTESIAN_POINT('Ctrl Pts',(25.4257977880274,57.5636463159493,40.1194874821989));
#208251=CARTESIAN_POINT('Ctrl Pts',(25.4538910783602,57.5124644612007,40.0627551483138));
#208252=CARTESIAN_POINT('Ctrl Pts',(25.4475597357242,57.4360631077224,40.0767884282375));
#208253=CARTESIAN_POINT('Ctrl Pts',(25.5110385513892,57.5536211289084,40.1599502015382));
#208254=CARTESIAN_POINT('Ctrl Pts',(25.517777816472,57.509788306594,40.1002449453885));
#208255=CARTESIAN_POINT('Ctrl Pts',(25.5012707422386,57.4400754463044,40.10025));
#208256=CARTESIAN_POINT('Ctrl Pts',(25.5918112338801,57.5176823163886,40.1599502534424));
#208257=CARTESIAN_POINT('Ctrl Pts',(25.5766462455183,57.4835989537475,40.10025));
#208258=CARTESIAN_POINT('Ctrl Pts',(25.5480287005725,57.4192809246786,40.10025));
#208259=CARTESIAN_POINT('Origin',(25.1947524379623,57.3689438691193,39.92499));
#208260=CARTESIAN_POINT('Origin',(24.4480624203082,54.1306438627435,39.6398955069306));
#208261=CARTESIAN_POINT('Origin',(24.3756025490945,53.9678963272932,39.92499));
#208262=CARTESIAN_POINT('Origin',(25.1222926664914,57.2061965577052,39.6398955068253));
#208263=CARTESIAN_POINT('Origin',(25.0498328948971,57.0434492461376,39.3548010137695));
#208264=CARTESIAN_POINT('Ctrl Pts',(24.3312692531094,53.8697418420142,39.8576902534424));
#208265=CARTESIAN_POINT('Ctrl Pts',(24.2159747902193,53.9216078643414,39.8579948730703));
#208266=CARTESIAN_POINT('Ctrl Pts',(24.2595822759739,54.0195518809638,39.92499));
#208267=CARTESIAN_POINT('Ctrl Pts',(24.3127882662185,53.828234173484,39.930402071123));
#208268=CARTESIAN_POINT('Ctrl Pts',(24.2176496934292,53.8880114973686,39.9058915297383));
#208269=CARTESIAN_POINT('Ctrl Pts',(24.241101009183,53.9780422761231,39.9671523786034));
#208270=CARTESIAN_POINT('Ctrl Pts',(24.2697746459846,53.7969955864425,40.0043257306694));
#208271=CARTESIAN_POINT('Ctrl Pts',(24.1983152114497,53.8549480733036,39.9667894847835));
#208272=CARTESIAN_POINT('Ctrl Pts',(24.2082687574729,53.9422730280819,40.0100138975201));
#208273=CARTESIAN_POINT('Ctrl Pts',(24.1443388226044,53.7744913425363,40.1195533054856));
#208274=CARTESIAN_POINT('Ctrl Pts',(24.1165167429227,53.825645022219,40.0630813209236));
#208275=CARTESIAN_POINT('Ctrl Pts',(24.123203223048,53.9017956184502,40.076826594242));
#208276=CARTESIAN_POINT('Ctrl Pts',(24.0595120258541,53.7848917482049,40.1599502027513));
#208277=CARTESIAN_POINT('Ctrl Pts',(24.0529122166853,53.8286685158639,40.100255279155));
#208278=CARTESIAN_POINT('Ctrl Pts',(24.069666546439,53.8982652496125,40.10025));
#208279=CARTESIAN_POINT('Ctrl Pts',(23.979166327502,53.8206887816833,40.1599502534424));
#208280=CARTESIAN_POINT('Ctrl Pts',(23.9943483786823,53.8547645473078,40.10025));
#208281=CARTESIAN_POINT('Ctrl Pts',(24.0229981225303,53.9190682401992,40.10025));
#208282=CARTESIAN_POINT('Origin',(24.0229981225303,53.9190682401992,40.22725));
#208283=CARTESIAN_POINT('Ctrl Pts',(24.8746050278059,56.6498810128379,38.989));
#208284=CARTESIAN_POINT('Ctrl Pts',(24.9907986398451,56.5981482837085,38.989));
#208285=CARTESIAN_POINT('Ctrl Pts',(24.9906251716322,56.5982255167328,39.1161896013271));
#208286=CARTESIAN_POINT('Ctrl Pts',(24.9626539694757,56.8481896769742,38.989));
#208287=CARTESIAN_POINT('Ctrl Pts',(25.079127190575,56.7965362315748,38.9887769275466));
#208288=CARTESIAN_POINT('Ctrl Pts',(25.0612010539382,56.7567415443525,39.1161898821828));
#208289=CARTESIAN_POINT('Ctrl Pts',(25.046477158254,57.0369754593319,39.1034967087243));
#208290=CARTESIAN_POINT('Ctrl Pts',(25.1631925873332,56.985349035722,39.1031720232705));
#208291=CARTESIAN_POINT('Ctrl Pts',(25.1283880784749,56.9076460727655,39.2077529615015));
#208292=CARTESIAN_POINT('Ctrl Pts',(25.0931373005752,57.1420619865018,39.2875012672119));
#208293=CARTESIAN_POINT('Ctrl Pts',(25.2100238867509,57.0905332166516,39.2872087095507));
#208294=CARTESIAN_POINT('Ctrl Pts',(25.1657874977299,56.9916465440536,39.354901704823));
#208295=CARTESIAN_POINT('Origin',(24.8746050278059,56.6498810128379,39.116));
#208296=CARTESIAN_POINT('Origin',(5.68853496937358E-15,5.30629395586253E-15,
40.22725));
#208297=CARTESIAN_POINT('Origin',(23.9951532569813,53.9314655730802,40.22725));
#208298=CARTESIAN_POINT('Origin',(10.0037024164492,23.2492868865834,39.116));
#208299=CARTESIAN_POINT('Origin',(24.7113125977913,56.2832472948504,39.1160373285276));
#208300=CARTESIAN_POINT('Ctrl Pts',(23.9513722670371,53.8330634946835,40.1599502534424));
#208301=CARTESIAN_POINT('Ctrl Pts',(23.966536720823,53.8671470951728,40.10025));
#208302=CARTESIAN_POINT('Ctrl Pts',(23.9951532569813,53.9314655730802,40.10025));
#208303=CARTESIAN_POINT('Ctrl Pts',(23.8712821658127,53.8686972660498,40.1599500566034));
#208304=CARTESIAN_POINT('Ctrl Pts',(23.9081865738562,53.8931046959194,40.1002551305381));
#208305=CARTESIAN_POINT('Ctrl Pts',(23.9486256024605,53.9521563342729,40.10025));
#208306=CARTESIAN_POINT('Ctrl Pts',(23.8071866393158,53.9240892607409,40.1203070619045));
#208307=CARTESIAN_POINT('Ctrl Pts',(23.8635355386149,53.9378509529598,40.0637098684499));
#208308=CARTESIAN_POINT('Ctrl Pts',(23.9155750846183,53.9937257232524,40.0772636213362));
#208309=CARTESIAN_POINT('Ctrl Pts',(23.7392497560577,54.033006412171,40.0046102245802));
#208310=CARTESIAN_POINT('Ctrl Pts',(23.8300830854582,54.0187512923757,39.9670001894012));
#208311=CARTESIAN_POINT('Ctrl Pts',(23.8883623535222,54.0845104630311,40.0101788811209));
#208312=CARTESIAN_POINT('Ctrl Pts',(23.7337507958623,54.0860594545421,39.9303710930186));
#208313=CARTESIAN_POINT('Ctrl Pts',(23.8418399747433,54.0553500291283,39.9058663574109));
#208314=CARTESIAN_POINT('Ctrl Pts',(23.8930480394874,54.1330265677739,39.9671344706365));
#208315=CARTESIAN_POINT('Ctrl Pts',(23.7522229508834,54.1275498658871,39.8576902534424));
#208316=CARTESIAN_POINT('Ctrl Pts',(23.8679139708575,54.0765745253533,39.8579948730703));
#208317=CARTESIAN_POINT('Ctrl Pts',(23.9115214566121,54.1745185419757,39.92499));
#208318=CARTESIAN_POINT('Origin',(23.7955011834915,54.2261740956463,39.92499));
#208319=CARTESIAN_POINT('Origin',(24.6933715410276,56.2428239368548,39.1925554488838));
#208320=CARTESIAN_POINT('Origin',(24.6600848917118,56.1680608984275,39.3343017080178));
#208321=CARTESIAN_POINT('Origin',(23.8679610547522,54.388921631059,39.6398955069211));
#208322=CARTESIAN_POINT('Origin',(23.9404209259127,54.5516691663892,39.3548010137695));
#208323=CARTESIAN_POINT('Ctrl Pts',(24.5258780191677,55.866627327383,39.3978017080178));
#208324=CARTESIAN_POINT('Ctrl Pts',(24.6418982922884,55.8149717737124,39.3978017080178));
#208325=CARTESIAN_POINT('Ctrl Pts',(24.6418982922884,55.8149717737124,39.5248017080178));
#208326=CARTESIAN_POINT('Ctrl Pts',(24.5627025231295,55.9487607347569,39.3978017080178));
#208327=CARTESIAN_POINT('Ctrl Pts',(24.6784744708811,55.8971232158781,39.3980355775159));
#208328=CARTESIAN_POINT('Ctrl Pts',(24.6968134595448,55.9383132588155,39.5248015517178));
#208329=CARTESIAN_POINT('Ctrl Pts',(24.5975211960713,56.026424800928,39.3484893995498));
#208330=CARTESIAN_POINT('Ctrl Pts',(24.7132325104948,55.9751910510458,39.3489438303434));
#208331=CARTESIAN_POINT('Ctrl Pts',(24.7487396569161,56.0549414076403,39.4508333155602));
#208332=CARTESIAN_POINT('Ctrl Pts',(24.61587051646,56.0673542004323,39.2708017080178));
#208333=CARTESIAN_POINT('Ctrl Pts',(24.7315703643342,56.0163785451195,39.2710850691866));
#208334=CARTESIAN_POINT('Ctrl Pts',(24.7761051648324,56.1164053447569,39.3343017080178));
#208335=CARTESIAN_POINT('Origin',(24.5258780191677,55.866627327383,39.5248017080178));
#208336=CARTESIAN_POINT('Ctrl Pts',(23.8971395307774,54.453046324469,39.2875012672119));
#208337=CARTESIAN_POINT('Ctrl Pts',(24.0130054343475,54.4019907365345,39.2878045257519));
#208338=CARTESIAN_POINT('Ctrl Pts',(24.0565064909001,54.5001606088507,39.3549015218351));
#208339=CARTESIAN_POINT('Ctrl Pts',(23.9437939758161,54.5581374230423,39.1034938540228));
#208340=CARTESIAN_POINT('Ctrl Pts',(24.059706177069,54.5068816478247,39.1038286278798));
#208341=CARTESIAN_POINT('Ctrl Pts',(24.0939065860597,54.5841625982665,39.2077506434038));
#208342=CARTESIAN_POINT('Ctrl Pts',(24.0276077026109,54.7469293531947,38.989));
#208343=CARTESIAN_POINT('Ctrl Pts',(24.1436691352865,54.6954643138438,38.9892298954617));
#208344=CARTESIAN_POINT('Ctrl Pts',(24.1610941752732,54.735068394998,39.1161900347279));
#208345=CARTESIAN_POINT('Ctrl Pts',(24.1156489724283,54.9452378026826,38.989));
#208346=CARTESIAN_POINT('Ctrl Pts',(24.2318430357382,54.8935048726345,38.989));
#208347=CARTESIAN_POINT('Ctrl Pts',(24.231669115581,54.8935823068774,39.1161900945654));
#208348=CARTESIAN_POINT('Origin',(24.1156489724283,54.9452378026826,39.116));
#208349=CARTESIAN_POINT('Origin',(9.75435829333415,22.6892508167102,39.5248017080178));
#208350=CARTESIAN_POINT('Origin',(24.4643761377923,55.7284918401495,39.5248017080178));
#208351=CARTESIAN_POINT('Origin',(9.71531210235053,22.6015516358801,39.116));
#208352=CARTESIAN_POINT('Origin',(24.278851034245,55.3119205422642,39.1160402713849));
#208353=CARTESIAN_POINT('Ctrl Pts',(24.374376627022,55.527767968768,39.2708017080178));
#208354=CARTESIAN_POINT('Ctrl Pts',(24.4911280468232,55.4763362579872,39.27051194648));
#208355=CARTESIAN_POINT('Ctrl Pts',(24.4461895095995,55.3754026508172,39.3343017080178));
#208356=CARTESIAN_POINT('Ctrl Pts',(24.3927905570414,55.5688345658071,39.3487519301186));
#208357=CARTESIAN_POINT('Ctrl Pts',(24.5093364964834,55.5172331055225,39.3482879463981));
#208358=CARTESIAN_POINT('Ctrl Pts',(24.4736474994209,55.4370743056936,39.4512271261637));
#208359=CARTESIAN_POINT('Ctrl Pts',(24.4276751358087,55.6466353090193,39.3978017080178));
#208360=CARTESIAN_POINT('Ctrl Pts',(24.543873985031,55.5948055748752,39.3975673827397));
#208361=CARTESIAN_POINT('Ctrl Pts',(24.5256662135194,55.5539102504899,39.5248015355181));
#208362=CARTESIAN_POINT('Ctrl Pts',(24.4643761377923,55.7284918401495,39.3978017080178));
#208363=CARTESIAN_POINT('Ctrl Pts',(24.5803964109129,55.6768362864789,39.3978017080178));
#208364=CARTESIAN_POINT('Ctrl Pts',(24.5803964109129,55.6768362864789,39.5248017080178));
#208365=CARTESIAN_POINT('Origin',(24.3301692364789,55.4270582044878,39.3343017080178));
#208366=CARTESIAN_POINT('Origin',(24.2970811017216,55.3527410377811,39.1934008533552));
#208367=CARTESIAN_POINT('Origin',(30.9870007556516,53.0360596835508,39.1925554495081));
#208368=CARTESIAN_POINT('Origin',(31.0091584503715,53.0743345559674,39.1160373285272));
#208369=CARTESIAN_POINT('Origin',(30.9460815882875,52.9651856060842,39.3343017080178));
#208370=CARTESIAN_POINT('Ctrl Pts',(30.8905967158742,52.8702215132212,39.2708017080178));
#208371=CARTESIAN_POINT('Ctrl Pts',(30.7813498801538,52.9338619179792,39.2710850691866));
#208372=CARTESIAN_POINT('Ctrl Pts',(30.8360963620068,53.0286856060842,39.3343017080178));
#208373=CARTESIAN_POINT('Ctrl Pts',(30.8681941459793,52.8311874403353,39.3487519293517));
#208374=CARTESIAN_POINT('Ctrl Pts',(30.7587310665105,52.8946849835399,39.3492068662932));
#208375=CARTESIAN_POINT('Ctrl Pts',(30.8023423591876,52.9702219582425,39.4512271248746));
#208376=CARTESIAN_POINT('Ctrl Pts',(30.8257530395504,52.7572372522463,39.3978017080178));
#208377=CARTESIAN_POINT('Ctrl Pts',(30.715927727326,52.8205474253429,39.3980347781178));
#208378=CARTESIAN_POINT('Ctrl Pts',(30.7383959430067,52.8594635164552,39.524801535519));
#208379=CARTESIAN_POINT('Ctrl Pts',(30.781101527075,52.6794317578284,39.3978017080178));
#208380=CARTESIAN_POINT('Ctrl Pts',(30.6711163007943,52.7429317578284,39.3978017080178));
#208381=CARTESIAN_POINT('Ctrl Pts',(30.6711163007943,52.7429317578284,39.5248017080178));
#208382=CARTESIAN_POINT('Origin',(30.781101527075,52.6794317578284,39.5248017080178));
#208383=CARTESIAN_POINT('Origin',(0.274963065701563,-0.158750000000003,
39.116));
#208384=CARTESIAN_POINT('Origin',(31.2097904767612,53.4219427993283,39.116));
#208385=CARTESIAN_POINT('Origin',(0.274963065701563,-0.158750000000003,
39.5248017080178));
#208386=CARTESIAN_POINT('Origin',(30.7054974692375,52.5484816883956,39.5248017080178));
#208387=CARTESIAN_POINT('Ctrl Pts',(31.4795232016796,53.8880358395966,39.2875012672119));
#208388=CARTESIAN_POINT('Ctrl Pts',(31.369131349158,53.9523112176909,39.287208709576));
#208389=CARTESIAN_POINT('Ctrl Pts',(31.3151318426941,53.8583991130126,39.3549016990123));
#208390=CARTESIAN_POINT('Ctrl Pts',(31.4219316852027,53.7885171709472,39.1034939173931));
#208391=CARTESIAN_POINT('Ctrl Pts',(31.3115614337849,53.8525966788984,39.1031692336334));
#208392=CARTESIAN_POINT('Ctrl Pts',(31.269156162556,53.7787668993601,39.2077507202308));
#208393=CARTESIAN_POINT('Ctrl Pts',(31.3184699958138,53.6097358757348,38.989));
#208394=CARTESIAN_POINT('Ctrl Pts',(31.2082202476905,53.6736035436575,38.9887769311164));
#208395=CARTESIAN_POINT('Ctrl Pts',(31.1865627224602,53.6357108652095,39.1161898712899));
#208396=CARTESIAN_POINT('Ctrl Pts',(31.2097904767612,53.4219427993283,38.989));
#208397=CARTESIAN_POINT('Ctrl Pts',(31.0996409376526,53.4855376653837,38.989));
#208398=CARTESIAN_POINT('Ctrl Pts',(31.0998053730352,53.4854427285713,39.1161895903856));
#208399=CARTESIAN_POINT('Origin',(31.4251975098799,53.7950387249975,39.3548010137695));
#208400=CARTESIAN_POINT('Ctrl Pts',(30.7054974692375,52.5484816883955,39.3978017080178));
#208401=CARTESIAN_POINT('Ctrl Pts',(30.5955122429569,52.6119816883956,39.3978017080178));
#208402=CARTESIAN_POINT('Ctrl Pts',(30.5955122429569,52.6119816883956,39.5248017080178));
#208403=CARTESIAN_POINT('Ctrl Pts',(30.6606955449583,52.4704129317475,39.3978017080178));
#208404=CARTESIAN_POINT('Ctrl Pts',(30.5504637065433,52.5339553345216,39.397566602504));
#208405=CARTESIAN_POINT('Ctrl Pts',(30.5280052047894,52.4950560684209,39.5248015517196));
#208406=CARTESIAN_POINT('Ctrl Pts',(30.618333528198,52.3965920780928,39.3484894016716));
#208407=CARTESIAN_POINT('Ctrl Pts',(30.5080831175492,52.4605500011255,39.3480259000037));
#208408=CARTESIAN_POINT('Ctrl Pts',(30.4641724871921,52.3844945583571,39.4508333188932));
#208409=CARTESIAN_POINT('Ctrl Pts',(30.5960088312575,52.3576880233159,39.2708017080178));
#208410=CARTESIAN_POINT('Ctrl Pts',(30.4857749404426,52.4219111049553,39.27051194648));
#208411=CARTESIAN_POINT('Ctrl Pts',(30.4305321463783,52.3262277788838,39.3343017080178));
#208412=CARTESIAN_POINT('Origin',(30.5405173726589,52.2627277788838,39.3343017080178));
#208413=CARTESIAN_POINT('Origin',(31.5142720656045,53.9493203812239,39.6398955068191));
#208414=CARTESIAN_POINT('Origin',(31.6033466212672,54.1036020372434,39.92499));
#208415=CARTESIAN_POINT('Origin',(30.499842238637,52.1922763801646,39.1934008539944));
#208416=CARTESIAN_POINT('Origin',(30.4775331296744,52.1535342613176,39.1160402713846));
#208417=CARTESIAN_POINT('Ctrl Pts',(31.4902932482914,54.5122556166607,40.1599502534424));
#208418=CARTESIAN_POINT('Ctrl Pts',(31.4716329851996,54.4799531854475,40.10025));
#208419=CARTESIAN_POINT('Ctrl Pts',(31.4364195775141,54.4189959163059,40.10025));
#208420=CARTESIAN_POINT('Ctrl Pts',(31.5665926662623,54.4681793099456,40.1599500538468));
#208421=CARTESIAN_POINT('Ctrl Pts',(31.5272089901464,54.4478446647271,40.100244835349));
#208422=CARTESIAN_POINT('Ctrl Pts',(31.4805801312546,54.3934750329631,40.10025));
#208423=CARTESIAN_POINT('Ctrl Pts',(31.6244843104276,54.4058464214482,40.1202442001037));
#208424=CARTESIAN_POINT('Ctrl Pts',(31.5668246399994,54.3982481205263,40.0633873868012));
#208425=CARTESIAN_POINT('Ctrl Pts',(31.5088182930364,54.3482630350898,40.0772271723536));
#208426=CARTESIAN_POINT('Ctrl Pts',(31.6805188761705,54.2895863184075,40.0045995998164));
#208427=CARTESIAN_POINT('Ctrl Pts',(31.5913182835567,54.3139476428155,39.9663485808321));
#208428=CARTESIAN_POINT('Ctrl Pts',(31.5259511417539,54.2544636505349,40.0101727202467));
#208429=CARTESIAN_POINT('Ctrl Pts',(31.6804069909882,54.2359839591648,39.9304654349857));
#208430=CARTESIAN_POINT('Ctrl Pts',(31.5756141966203,54.2789047974524,39.9051900162937));
#208431=CARTESIAN_POINT('Ctrl Pts',(31.5160982999439,54.2064835118364,39.9671857458168));
#208432=CARTESIAN_POINT('Ctrl Pts',(31.6576696180591,54.1966007261204,39.8576902534424));
#208433=CARTESIAN_POINT('Ctrl Pts',(31.547444164929,54.2607761425979,39.8573998014387));
#208434=CARTESIAN_POINT('Ctrl Pts',(31.4933613949865,54.1671020372435,39.92499));
#208435=CARTESIAN_POINT('Origin',(31.4364195775141,54.4189959163059,40.22725));
#208436=CARTESIAN_POINT('Origin',(0.274963065701563,-0.158750000000003,
39.116));
#208437=CARTESIAN_POINT('Origin',(30.2768083268887,51.8059703131943,39.116));
#208438=CARTESIAN_POINT('Origin',(5.58223212128129E-15,5.55208600813687E-15,
40.22725));
#208439=CARTESIAN_POINT('Origin',(31.4100231232068,54.4342359163059,40.22725));
#208440=CARTESIAN_POINT('Ctrl Pts',(30.2768083268887,51.8059703131943,38.989));
#208441=CARTESIAN_POINT('Ctrl Pts',(30.1666583377722,51.8695654390619,38.989));
#208442=CARTESIAN_POINT('Ctrl Pts',(30.1668232238344,51.8694702420495,39.1161901092326));
#208443=CARTESIAN_POINT('Ctrl Pts',(30.1681210939104,51.6181777324908,38.989));
#208444=CARTESIAN_POINT('Ctrl Pts',(30.0582657983062,51.6818230251226,38.9892298989718));
#208445=CARTESIAN_POINT('Ctrl Pts',(30.0800643400511,51.7191994478429,39.1161900493188));
#208446=CARTESIAN_POINT('Ctrl Pts',(30.0646505034505,51.4394033023492,39.1034966344368));
#208447=CARTESIAN_POINT('Ctrl Pts',(29.9550522173037,51.5030508615797,39.1038314102585));
#208448=CARTESIAN_POINT('Ctrl Pts',(29.9974715145374,51.5761444782073,39.2077528789611));
#208449=CARTESIAN_POINT('Ctrl Pts',(30.0070536838164,51.3398895692694,39.2875012672119));
#208450=CARTESIAN_POINT('Ctrl Pts',(29.8976445635504,51.4036173400345,39.2878045257868));
#208451=CARTESIAN_POINT('Ctrl Pts',(29.9514963979204,51.4965132406191,39.3549015295901));
#208452=CARTESIAN_POINT('Origin',(30.0614010732043,51.4328740054939,39.3548010137695));
#208453=CARTESIAN_POINT('Ctrl Pts',(31.1067982185541,54.5146464769134,39.8576902534424));
#208454=CARTESIAN_POINT('Ctrl Pts',(31.2174884860871,54.4512761425979,39.8573998014387));
#208455=CARTESIAN_POINT('Ctrl Pts',(31.1634057161447,54.3576020372435,39.92499));
#208456=CARTESIAN_POINT('Ctrl Pts',(31.1295467523335,54.5540471172212,39.9304984902491));
#208457=CARTESIAN_POINT('Ctrl Pts',(31.2191042733517,54.4847554296812,39.9052171569791));
#208458=CARTESIAN_POINT('Ctrl Pts',(31.1861529813963,54.3970014563925,39.9672049726606));
#208459=CARTESIAN_POINT('Ctrl Pts',(31.1758273123594,54.5807851087095,40.0043437678663));
#208460=CARTESIAN_POINT('Ctrl Pts',(31.241605266786,54.5157207333391,39.966162857764));
#208461=CARTESIAN_POINT('Ctrl Pts',(31.2226915745269,54.4293656242364,40.0100243556234));
#208462=CARTESIAN_POINT('Ctrl Pts',(31.3035520968889,54.5905870683099,40.1194874821986));
#208463=CARTESIAN_POINT('Ctrl Pts',(31.326141528613,54.5367490446495,40.0627551483143));
#208464=CARTESIAN_POINT('Ctrl Pts',(31.3118587536639,54.461428031296,40.0767884282378));
#208465=CARTESIAN_POINT('Ctrl Pts',(31.3872779850339,54.5717067142911,40.1599502015381));
#208466=CARTESIAN_POINT('Ctrl Pts',(31.3893985541595,54.5274095677394,40.100244945386));
#208467=CARTESIAN_POINT('Ctrl Pts',(31.3656949292504,54.459804060896,40.10025));
#208468=CARTESIAN_POINT('Ctrl Pts',(31.4638515574747,54.5275217339716,40.1599502534424));
#208469=CARTESIAN_POINT('Ctrl Pts',(31.445206962986,54.4952102564862,40.10025));
#208470=CARTESIAN_POINT('Ctrl Pts',(31.4100231232068,54.434235916306,40.10025));
#208471=CARTESIAN_POINT('Origin',(31.053420489864,54.4211020372435,39.92499));
#208472=CARTESIAN_POINT('Origin',(29.9723263949888,51.278592137215,39.6398955069312));
#208473=CARTESIAN_POINT('Origin',(29.8832517167492,51.1243102687781,39.92499));
#208474=CARTESIAN_POINT('Origin',(30.9643459342367,54.2668203811885,39.6398955068273));
#208475=CARTESIAN_POINT('Origin',(30.8752713784768,54.1125387249975,39.3548010137695));
#208476=CARTESIAN_POINT('Ctrl Pts',(29.8289013456892,51.0313275753405,39.8576902534424));
#208477=CARTESIAN_POINT('Ctrl Pts',(29.7196599535399,51.0949610231998,39.8579948730703));
#208478=CARTESIAN_POINT('Ctrl Pts',(29.7732664904686,51.1878102687781,39.92499));
#208479=CARTESIAN_POINT('Ctrl Pts',(29.8061828667731,50.9919790793207,39.930402071123));
#208480=CARTESIAN_POINT('Ctrl Pts',(29.7178139048433,51.0613736255825,39.9058915297388));
#208481=CARTESIAN_POINT('Ctrl Pts',(29.7505475307862,51.1484598763131,39.9671523786037));
#208482=CARTESIAN_POINT('Ctrl Pts',(29.7601395581531,50.9654077681504,40.0043257306694));
#208483=CARTESIAN_POINT('Ctrl Pts',(29.6951292702712,51.0305123301031,39.9667894847838));
#208484=CARTESIAN_POINT('Ctrl Pts',(29.7141562330561,51.1163184807718,40.01001389752));
#208485=CARTESIAN_POINT('Ctrl Pts',(29.6330385513055,50.9561384187036,40.1195533054856));
#208486=CARTESIAN_POINT('Ctrl Pts',(29.6107158994153,51.0099200724104,40.0630813209234));
#208487=CARTESIAN_POINT('Ctrl Pts',(29.6253256551034,51.0849545802161,40.0768265942421));
#208488=CARTESIAN_POINT('Ctrl Pts',(29.5497635830449,50.9753486645696,40.1599502027521));
#208489=CARTESIAN_POINT('Ctrl Pts',(29.5477758465702,51.0195754864235,40.1002552791541));
#208490=CARTESIAN_POINT('Ctrl Pts',(29.5717132339806,51.0870396576411,40.10025));
#208491=CARTESIAN_POINT('Ctrl Pts',(29.4735998357344,51.0193480105324,40.1599502534424));
#208492=CARTESIAN_POINT('Ctrl Pts',(29.4922606054652,51.0516501490683,40.10025));
#208493=CARTESIAN_POINT('Ctrl Pts',(29.5274749692191,51.1126068659043,40.10025));
#208494=CARTESIAN_POINT('Origin',(29.5274749692191,51.1126068659043,40.22725));
#208495=CARTESIAN_POINT('Ctrl Pts',(30.6598643453581,53.7394427993283,38.989));
#208496=CARTESIAN_POINT('Ctrl Pts',(30.7700138939565,53.6758479277939,38.989));
#208497=CARTESIAN_POINT('Ctrl Pts',(30.7698494490699,53.6759428700934,39.1161896013271));
#208498=CARTESIAN_POINT('Ctrl Pts',(30.7681598456269,53.9274614872883,38.989));
#208499=CARTESIAN_POINT('Ctrl Pts',(30.8785957589617,53.8639162380512,38.9887769275436));
#208500=CARTESIAN_POINT('Ctrl Pts',(30.8566081460784,53.8262133418065,39.1161898821829));
#208501=CARTESIAN_POINT('Ctrl Pts',(30.8712573299201,54.1064511722699,39.1034967087243));
#208502=CARTESIAN_POINT('Ctrl Pts',(30.9819369489468,54.0429074791724,39.1031720232714));
#208503=CARTESIAN_POINT('Ctrl Pts',(30.9392009315203,53.9692682429977,39.2077529615014));
#208504=CARTESIAN_POINT('Ctrl Pts',(30.9286463962985,54.2060847114738,39.2875012672119));
#208505=CARTESIAN_POINT('Ctrl Pts',(31.0395064423985,54.1426202463868,39.2872087095507));
#208506=CARTESIAN_POINT('Ctrl Pts',(30.9851759130208,54.0488992470928,39.354901704823));
#208507=CARTESIAN_POINT('Origin',(30.6598643453581,53.7394427993283,39.116));
#208508=CARTESIAN_POINT('Origin',(5.69400554112517E-15,5.30350656033181E-15,
40.22725));
#208509=CARTESIAN_POINT('Origin',(29.5010785149117,51.1278468659043,40.22725));
#208510=CARTESIAN_POINT('Origin',(15.2806508669898,27.1018636743471,39.116));
#208511=CARTESIAN_POINT('Origin',(30.4591427892375,53.3918862459818,39.1160373285273));
#208512=CARTESIAN_POINT('Ctrl Pts',(29.4472515437741,51.0345602039883,40.1599502534424));
#208513=CARTESIAN_POINT('Ctrl Pts',(29.4658956314773,51.0668719738974,40.10025));
#208514=CARTESIAN_POINT('Ctrl Pts',(29.5010785149117,51.1278468659044,40.10025));
#208515=CARTESIAN_POINT('Ctrl Pts',(29.3713249278651,51.0783704650302,40.1599500566043));
#208516=CARTESIAN_POINT('Ctrl Pts',(29.410578440836,51.0987866273836,40.100255130536));
#208517=CARTESIAN_POINT('Ctrl Pts',(29.4569685172211,51.1532877451675,40.10025));
#208518=CARTESIAN_POINT('Ctrl Pts',(29.3133705634517,51.1401588234659,40.1203070619047));
#208519=CARTESIAN_POINT('Ctrl Pts',(29.3708492661241,51.1479550638441,40.0637098684496));
#208520=CARTESIAN_POINT('Ctrl Pts',(29.4284442379235,51.198084132526,40.0772636213363));
#208521=CARTESIAN_POINT('Ctrl Pts',(29.2571907880108,51.2555806533508,40.0046102245801));
#208522=CARTESIAN_POINT('Ctrl Pts',(29.346036457163,51.2319089562579,39.9670001894015));
#208523=CARTESIAN_POINT('Ctrl Pts',(29.4108701703532,51.2912160489646,40.0101788811209));
#208524=CARTESIAN_POINT('Ctrl Pts',(29.2572675046855,51.3089178634633,39.9303710930187));
#208525=CARTESIAN_POINT('Ctrl Pts',(29.3615545506891,51.2670782717306,39.9058663574108));
#208526=CARTESIAN_POINT('Ctrl Pts',(29.4206015015128,51.338976589856,39.9671344706372));
#208527=CARTESIAN_POINT('Ctrl Pts',(29.2799753962468,51.3482501200162,39.8576902534424));
#208528=CARTESIAN_POINT('Ctrl Pts',(29.389704274698,51.2854610231998,39.8579948730703));
#208529=CARTESIAN_POINT('Ctrl Pts',(29.4433108116267,51.3783102687781,39.92499));
#208530=CARTESIAN_POINT('Origin',(29.3333255853461,51.4418102687781,39.92499));
#208531=CARTESIAN_POINT('Origin',(30.4370746239673,53.3535596824664,39.1925554488847));
#208532=CARTESIAN_POINT('Origin',(30.3961554568843,53.2826856060842,39.3343017080178));
#208533=CARTESIAN_POINT('Origin',(29.4224002636289,51.5960921371705,39.6398955069207));
#208534=CARTESIAN_POINT('Origin',(29.5114749418011,51.750374005494,39.3548010137695));
#208535=CARTESIAN_POINT('Ctrl Pts',(30.2311753956719,52.9969317578284,39.3978017080178));
#208536=CARTESIAN_POINT('Ctrl Pts',(30.3411606219525,52.9334317578284,39.3978017080178));
#208537=CARTESIAN_POINT('Ctrl Pts',(30.3411606219525,52.9334317578284,39.5248017080178));
#208538=CARTESIAN_POINT('Ctrl Pts',(30.2763834500039,53.0747660209931,39.3978017080178));
#208539=CARTESIAN_POINT('Ctrl Pts',(30.3861235964158,53.0113099140559,39.3980355775196));
#208540=CARTESIAN_POINT('Ctrl Pts',(30.4086676540716,53.0503573673268,39.5248015517192));
#208541=CARTESIAN_POINT('Ctrl Pts',(30.319129488101,53.1483650929075,39.3484893995498));
#208542=CARTESIAN_POINT('Ctrl Pts',(30.4288515386952,53.0853168809912,39.3489438303413));
#208543=CARTESIAN_POINT('Ctrl Pts',(30.4725003554715,53.1609188493359,39.4508333155594));
#208544=CARTESIAN_POINT('Ctrl Pts',(30.3416565762243,53.1871522506172,39.2708017080178));
#208545=CARTESIAN_POINT('Ctrl Pts',(30.451394201312,53.1243619179792,39.2710850691866));
#208546=CARTESIAN_POINT('Ctrl Pts',(30.506140683165,53.2191856060842,39.3343017080178));
#208547=CARTESIAN_POINT('Origin',(30.2311753956718,52.9969317578284,39.5248017080178));
#208548=CARTESIAN_POINT('Ctrl Pts',(29.458121752568,51.6568155675424,39.2875012672119));
#208549=CARTESIAN_POINT('Ctrl Pts',(29.5680161684464,51.5939283826158,39.2878045257519));
#208550=CARTESIAN_POINT('Ctrl Pts',(29.6215404675523,51.6870133715069,39.3549015218348));
#208551=CARTESIAN_POINT('Ctrl Pts',(29.5155056307115,51.7564542486377,39.1034938540228));
#208552=CARTESIAN_POINT('Ctrl Pts',(29.625425165382,51.6933631336519,39.1038286278807));
#208553=CARTESIAN_POINT('Ctrl Pts',(29.6675162799446,51.7666458147659,39.2077506434044));
#208554=CARTESIAN_POINT('Ctrl Pts',(29.6185943474785,51.93545103678,38.989));
#208555=CARTESIAN_POINT('Ctrl Pts',(29.7286404220058,51.872136205095,38.9892298954617));
#208556=CARTESIAN_POINT('Ctrl Pts',(29.7501097595415,51.9097019182962,39.1161900347272));
#208557=CARTESIAN_POINT('Ctrl Pts',(29.7268821954856,52.1234703131943,38.989));
#208558=CARTESIAN_POINT('Ctrl Pts',(29.8370321718802,52.0598751946716,38.989));
#208559=CARTESIAN_POINT('Ctrl Pts',(29.8368672985589,52.0599703843281,39.1161900945647));
#208560=CARTESIAN_POINT('Origin',(29.7268821954856,52.1234703131943,39.116));
#208561=CARTESIAN_POINT('Origin',(14.9038494342991,26.4492244485619,39.5248017080178));
#208562=CARTESIAN_POINT('Origin',(30.1555713378344,52.8659816883956,39.5248017080178));
#208563=CARTESIAN_POINT('Origin',(14.8448439902567,26.3470240215575,39.116));
#208564=CARTESIAN_POINT('Origin',(29.9275190026064,52.471085065638,39.1160402713852));
#208565=CARTESIAN_POINT('Ctrl Pts',(30.0450834959843,52.6757649139392,39.2708017080178));
#208566=CARTESIAN_POINT('Ctrl Pts',(30.1558192616008,52.6124111049553,39.27051194648));
#208567=CARTESIAN_POINT('Ctrl Pts',(30.1005764675364,52.5167277788838,39.3343017080178));
#208568=CARTESIAN_POINT('Ctrl Pts',(30.0676891808479,52.7146817640556,39.3487519301186));
#208569=CARTESIAN_POINT('Ctrl Pts',(30.1782028480943,52.6511806140172,39.3482879463985));
#208570=CARTESIAN_POINT('Ctrl Pts',(30.1343304829269,52.5751914484995,39.4512271261632));
#208571=CARTESIAN_POINT('Ctrl Pts',(30.1105150503725,52.7884098752453,39.3978017080178));
#208572=CARTESIAN_POINT('Ctrl Pts',(30.2206596676791,52.7247179826666,39.3975673827397));
#208573=CARTESIAN_POINT('Ctrl Pts',(30.1982769148327,52.6859499175231,39.5248015355194));
#208574=CARTESIAN_POINT('Ctrl Pts',(30.1555713378344,52.8659816883956,39.3978017080178));
#208575=CARTESIAN_POINT('Ctrl Pts',(30.265556564115,52.8024816883956,39.3978017080178));
#208576=CARTESIAN_POINT('Ctrl Pts',(30.265556564115,52.8024816883956,39.5248017080178));
#208577=CARTESIAN_POINT('Origin',(29.9905912412558,52.5802277788838,39.3343017080178));
#208578=CARTESIAN_POINT('Origin',(29.9499161075313,52.5097763812713,39.1934008533552));
#208579=CARTESIAN_POINT('Origin',(36.361028539783,49.5064990290875,39.1925554495082));
#208580=CARTESIAN_POINT('Origin',(36.3870656659288,49.5422481179703,39.1160373285292));
#208581=CARTESIAN_POINT('Origin',(36.3129251734949,49.4402904249162,39.3343017080178));
#208582=CARTESIAN_POINT('Ctrl Pts',(36.2478178023256,49.3516463037381,39.2708017080178));
#208583=CARTESIAN_POINT('Ctrl Pts',(36.1458216659131,49.4263574835547,39.2710850691866));
#208584=CARTESIAN_POINT('Ctrl Pts',(36.2101800152093,49.5149391519573,39.3343017080178));
#208585=CARTESIAN_POINT('Ctrl Pts',(36.2214577843992,49.3151677697917,39.3487519293518));
#208586=CARTESIAN_POINT('Ctrl Pts',(36.1192316557432,49.389759474291,39.3492068662919));
#208587=CARTESIAN_POINT('Ctrl Pts',(36.1704998050828,49.4603240281388,39.4512271248743));
#208588=CARTESIAN_POINT('Ctrl Pts',(36.1715192752727,49.246058992205,39.3978017080178));
#208589=CARTESIAN_POINT('Ctrl Pts',(36.068913312703,49.3205022166658,39.3980347781187));
#208590=CARTESIAN_POINT('Ctrl Pts',(36.0953262843475,49.3568565533005,39.524801535519));
#208591=CARTESIAN_POINT('Ctrl Pts',(36.1189794796889,49.1733470784083,39.3978017080178));
#208592=CARTESIAN_POINT('Ctrl Pts',(36.0162343214032,49.2479958054495,39.3978017080178));
#208593=CARTESIAN_POINT('Ctrl Pts',(36.0162343214032,49.2479958054495,39.5248017080178));
#208594=CARTESIAN_POINT('Origin',(36.1189794796889,49.1733470784083,39.5248017080178));
#208595=CARTESIAN_POINT('Origin',(0.256862895714049,-0.186621817602863,
39.116));
#208596=CARTESIAN_POINT('Origin',(36.6229335645815,49.8669803696022,39.116));
#208597=CARTESIAN_POINT('Origin',(0.256862895714049,-0.186621817602863,
39.5248017080178));
#208598=CARTESIAN_POINT('Origin',(36.0301015792682,49.0510171431399,39.5248017080178));
#208599=CARTESIAN_POINT('Ctrl Pts',(36.9399086546492,50.3023253561991,39.2875012672119));
#208600=CARTESIAN_POINT('Ctrl Pts',(36.8368401467444,50.3777877177482,39.287208709576));
#208601=CARTESIAN_POINT('Ctrl Pts',(36.7733199672427,50.2900345588335,39.3549016990123));
#208602=CARTESIAN_POINT('Ctrl Pts',(36.8722300970248,50.2093718139441,39.1034939173931));
#208603=CARTESIAN_POINT('Ctrl Pts',(36.7691625978877,50.2846371204152,39.1031692336321));
#208604=CARTESIAN_POINT('Ctrl Pts',(36.7192723137716,50.2156443459724,39.2077507202293));
#208605=CARTESIAN_POINT('Ctrl Pts',(36.7506474475478,50.0423845927708,38.989));
#208606=CARTESIAN_POINT('Ctrl Pts',(36.6476776482611,50.1174266236732,38.9887769311182));
#208607=CARTESIAN_POINT('Ctrl Pts',(36.622177901771,50.0820053531135,39.1161898712916));
#208608=CARTESIAN_POINT('Ctrl Pts',(36.6229335645815,49.8669803696022,38.989));
#208609=CARTESIAN_POINT('Ctrl Pts',(36.5200349097939,49.9417406183799,38.989));
#208610=CARTESIAN_POINT('Ctrl Pts',(36.5201885207831,49.9416290134635,39.1161895903855));
#208611=CARTESIAN_POINT('Origin',(36.876159719196,50.215516270604,39.3548010137695));
#208612=CARTESIAN_POINT('Ctrl Pts',(36.0301015792682,49.0510171431399,39.3978017080178));
#208613=CARTESIAN_POINT('Ctrl Pts',(35.9273564209826,49.1256658701811,39.3978017080178));
#208614=CARTESIAN_POINT('Ctrl Pts',(35.9273564209826,49.1256658701811,39.5248017080178));
#208615=CARTESIAN_POINT('Ctrl Pts',(35.9773846774565,48.9780591316055,39.3978017080178));
#208616=CARTESIAN_POINT('Ctrl Pts',(35.8743986903,49.0527758071216,39.3975666025035));
#208617=CARTESIAN_POINT('Ctrl Pts',(35.8479971380625,49.0164371879483,39.5248015517196));
#208618=CARTESIAN_POINT('Ctrl Pts',(35.9275383438686,48.9090707128226,39.3484894016716));
#208619=CARTESIAN_POINT('Ctrl Pts',(35.8245773199098,48.9842025736633,39.348025900004));
#208620=CARTESIAN_POINT('Ctrl Pts',(35.772957278024,48.9131536812767,39.4508333188941));
#208621=CARTESIAN_POINT('Ctrl Pts',(35.901269362891,48.8727133447939,39.2708017080178));
#208622=CARTESIAN_POINT('Ctrl Pts',(35.7983524848941,48.9481071848793,39.27051194648));
#208623=CARTESIAN_POINT('Ctrl Pts',(35.7334106856012,48.8587224664496,39.3343017080178));
#208624=CARTESIAN_POINT('Origin',(35.8361558438868,48.7840737394085,39.3343017080178));
#208625=CARTESIAN_POINT('Origin',(36.9808731396208,50.3596419293477,39.6398955068193));
#208626=CARTESIAN_POINT('Origin',(37.0855865599608,50.5037675878941,39.92499));
#208627=CARTESIAN_POINT('Origin',(35.7883393560629,48.7182599900743,39.1934008539946));
#208628=CARTESIAN_POINT('Origin',(35.7621028045855,48.682062041486,39.1160402713846));
#208629=CARTESIAN_POINT('Ctrl Pts',(37.0158684358566,50.9219998155896,40.1599502534424));
#208630=CARTESIAN_POINT('Ctrl Pts',(36.9939338721439,50.8918248690996,40.10025));
#208631=CARTESIAN_POINT('Ctrl Pts',(36.9525415975218,50.8348823336482,40.10025));
#208632=CARTESIAN_POINT('Ctrl Pts',(37.087142649025,50.8701895025857,40.1599500538468));
#208633=CARTESIAN_POINT('Ctrl Pts',(37.0458491715926,50.8540829678248,40.100244835349));
#208634=CARTESIAN_POINT('Ctrl Pts',(36.993792576411,50.8048852215546,40.10025));
#208635=CARTESIAN_POINT('Ctrl Pts',(37.1382015956606,50.802146755573,40.120244200104));
#208636=CARTESIAN_POINT('Ctrl Pts',(37.0800635522221,50.8006171556817,40.0633873868018));
#208637=CARTESIAN_POINT('Ctrl Pts',(37.0171501059297,50.7569692080812,40.0772271723538));
#208638=CARTESIAN_POINT('Ctrl Pts',(37.1817767082791,50.6806663304939,40.0045995998161));
#208639=CARTESIAN_POINT('Ctrl Pts',(37.0956112176475,50.7142182018855,39.9663485808314));
#208640=CARTESIAN_POINT('Ctrl Pts',(37.0243843935853,50.6618927960195,40.0101727202465));
#208641=CARTESIAN_POINT('Ctrl Pts',(37.1760624637757,50.6273693057707,39.9304654349859));
#208642=CARTESIAN_POINT('Ctrl Pts',(37.0763301845697,50.6810088489719,39.9051900162942));
#208643=CARTESIAN_POINT('Ctrl Pts',(37.009570236509,50.6152053999557,39.9671857458172));
#208644=CARTESIAN_POINT('Ctrl Pts',(37.1493329797266,50.590578520848,39.8576902534424));
#208645=CARTESIAN_POINT('Ctrl Pts',(37.0464195108259,50.6659240749079,39.8573998014387));
#208646=CARTESIAN_POINT('Ctrl Pts',(36.9828414016752,50.5784163149353,39.92499));
#208647=CARTESIAN_POINT('Origin',(36.9525415975218,50.8348823336482,40.22725));
#208648=CARTESIAN_POINT('Origin',(0.256862895714049,-0.186621817602863,
39.116));
#208649=CARTESIAN_POINT('Origin',(35.5261472678871,48.3573835402115,39.116));
#208650=CARTESIAN_POINT('Origin',(5.56775724677591E-15,5.56148610155125E-15,
40.22725));
#208651=CARTESIAN_POINT('Origin',(36.9278827595332,50.8527980281381,40.22725));
#208652=CARTESIAN_POINT('Ctrl Pts',(35.5261472678871,48.3573835402115,38.989));
#208653=CARTESIAN_POINT('Ctrl Pts',(35.4232481927143,48.432144094417,38.989));
#208654=CARTESIAN_POINT('Ctrl Pts',(35.4234022247162,48.432032183617,39.1161901092328));
#208655=CARTESIAN_POINT('Ctrl Pts',(35.3984257650696,48.1819806163539,38.989));
#208656=CARTESIAN_POINT('Ctrl Pts',(35.2958250128997,48.2567602586438,38.9892298989718));
#208657=CARTESIAN_POINT('Ctrl Pts',(35.3214110399842,48.2916533613418,39.116190049319));
#208658=CARTESIAN_POINT('Ctrl Pts',(35.2768349808764,48.0150011530603,39.1034966344368));
#208659=CARTESIAN_POINT('Ctrl Pts',(35.1744900671637,48.0897561847345,39.1038314102594));
#208660=CARTESIAN_POINT('Ctrl Pts',(35.2243173504702,48.1580153629237,39.2077528789609));
#208661=CARTESIAN_POINT('Ctrl Pts',(35.2091516650533,47.9220530736683,39.2875012672119));
#208662=CARTESIAN_POINT('Ctrl Pts',(35.1070032653412,47.9968681042462,39.2878045257868));
#208663=CARTESIAN_POINT('Ctrl Pts',(35.1702703594602,48.0836260618768,39.3549015295903));
#208664=CARTESIAN_POINT('Origin',(35.272920853982,48.0088472823268,39.3548010137695));
#208665=CARTESIAN_POINT('Ctrl Pts',(36.634724144966,50.9644637245889,39.8576902534424));
#208666=CARTESIAN_POINT('Ctrl Pts',(36.738184035969,50.8898702560314,39.8573998014387));
#208667=CARTESIAN_POINT('Ctrl Pts',(36.6746059268184,50.8023624960587,39.92499));
#208668=CARTESIAN_POINT('Ctrl Pts',(36.6614665482798,51.0012706547895,39.9304984902494));
#208669=CARTESIAN_POINT('Ctrl Pts',(36.7432905102111,50.9229972443178,39.9052171569795));
#208670=CARTESIAN_POINT('Ctrl Pts',(36.7013469409089,50.839168344388,39.96720497266));
#208671=CARTESIAN_POINT('Ctrl Pts',(36.710288459717,51.0230245369432,40.0043437678658));
#208672=CARTESIAN_POINT('Ctrl Pts',(36.7689049964553,50.951440922535,39.966162857764));
#208673=CARTESIAN_POINT('Ctrl Pts',(36.7410683485316,50.8675358949423,40.0100243556234));
#208674=CARTESIAN_POINT('Ctrl Pts',(36.8383381382869,51.0194219249359,40.1194874821991));
#208675=CARTESIAN_POINT('Ctrl Pts',(36.8551762168624,50.9635175930189,40.0627551483143));
#208676=CARTESIAN_POINT('Ctrl Pts',(36.8330984946713,50.8901021525737,40.0767884282378));
#208677=CARTESIAN_POINT('Ctrl Pts',(36.9196318328649,50.9918932610482,40.1599502015385));
#208678=CARTESIAN_POINT('Ctrl Pts',(36.9171104726343,50.9476171190675,40.1002449453875));
#208679=CARTESIAN_POINT('Ctrl Pts',(36.8864699989244,50.8828596657509,40.10025));
#208680=CARTESIAN_POINT('Ctrl Pts',(36.9911673391713,50.9399462128198,40.1599502534424));
#208681=CARTESIAN_POINT('Ctrl Pts',(36.9692474126346,50.909760631799,40.10025));
#208682=CARTESIAN_POINT('Ctrl Pts',(36.9278827595333,50.8527980281381,40.10025));
#208683=CARTESIAN_POINT('Origin',(36.5718607685328,50.8770112230998,39.92499));
#208684=CARTESIAN_POINT('Origin',(35.1682072895768,47.8647214254969,39.6398955069337));
#208685=CARTESIAN_POINT('Origin',(35.0634937251227,47.7205955685087,39.92499));
#208686=CARTESIAN_POINT('Origin',(36.4671473482256,50.7328855645163,39.6398955068261));
#208687=CARTESIAN_POINT('Origin',(36.3624339277679,50.5887599058097,39.3548010137695));
#208688=CARTESIAN_POINT('Ctrl Pts',(34.9997217530266,47.6338034047596,39.8576902534424));
#208689=CARTESIAN_POINT('Ctrl Pts',(34.8977303031707,47.70850709678,39.8579948730703));
#208690=CARTESIAN_POINT('Ctrl Pts',(34.9607485668371,47.7952442955498,39.92499));
#208691=CARTESIAN_POINT('Ctrl Pts',(34.9730146904946,47.5970451916066,39.930402071123));
#208692=CARTESIAN_POINT('Ctrl Pts',(34.8923835282618,47.6752966590737,39.9058915297377));
#208693=CARTESIAN_POINT('Ctrl Pts',(34.9340408279394,47.7584842465943,39.9671523786032));
#208694=CARTESIAN_POINT('Ctrl Pts',(34.9244461536129,47.5754322771532,40.0043257306693));
#208695=CARTESIAN_POINT('Ctrl Pts',(34.8665972787031,47.6469756149917,39.9667894847838));
#208696=CARTESIAN_POINT('Ctrl Pts',(34.894489194863,47.7303228514092,40.01001389752));
#208697=CARTESIAN_POINT('Ctrl Pts',(34.7970725085263,47.5794993790981,40.1195533054857));
#208698=CARTESIAN_POINT('Ctrl Pts',(34.7804938560725,47.6353197637775,40.0630813209234));
#208699=CARTESIAN_POINT('Ctrl Pts',(34.8028668197837,47.7084160893868,40.076826594242));
#208700=CARTESIAN_POINT('Ctrl Pts',(34.716261746735,47.607308993689,40.1599502027505));
#208701=CARTESIAN_POINT('Ctrl Pts',(34.7189078610147,47.6515013114269,40.1002552791544));
#208702=CARTESIAN_POINT('Ctrl Pts',(34.7497660430541,47.7160937685343,40.10025));
#208703=CARTESIAN_POINT('Ctrl Pts',(34.6451144164191,47.6590285860932,40.1599502534424));
#208704=CARTESIAN_POINT('Ctrl Pts',(34.6670494534023,47.6892031885509,40.10025));
#208705=CARTESIAN_POINT('Ctrl Pts',(34.7084426211237,47.746145074786,40.10025));
#208706=CARTESIAN_POINT('Origin',(34.7084426211237,47.7461450747861,40.22725));
#208707=CARTESIAN_POINT('Ctrl Pts',(36.1092077731534,50.2402240048079,38.989));
#208708=CARTESIAN_POINT('Ctrl Pts',(36.2121064368061,50.1654637495893,38.989));
#208709=CARTESIAN_POINT('Ctrl Pts',(36.2119528169387,50.1655753609561,39.1161896013269));
#208710=CARTESIAN_POINT('Ctrl Pts',(36.2365633238594,50.4158927445001,38.989));
#208711=CARTESIAN_POINT('Ctrl Pts',(36.3397519704551,50.3411519064778,38.9887769275466));
#208712=CARTESIAN_POINT('Ctrl Pts',(36.3139437822104,50.3059538820295,39.116189882185));
#208713=CARTESIAN_POINT('Ctrl Pts',(36.3578055460604,50.5831252836579,39.1034967087243));
#208714=CARTESIAN_POINT('Ctrl Pts',(36.4612367259619,50.5083605190678,39.1031720232695));
#208715=CARTESIAN_POINT('Ctrl Pts',(36.411037424715,50.439591816563,39.2077529614998));
#208716=CARTESIAN_POINT('Ctrl Pts',(36.4252947698684,50.6762142289944,39.2875012672119));
#208717=CARTESIAN_POINT('Ctrl Pts',(36.5289136700287,50.6015093986311,39.2872087095508));
#208718=CARTESIAN_POINT('Ctrl Pts',(36.4650842569437,50.5139808995218,39.3549017048229));
#208719=CARTESIAN_POINT('Origin',(36.1092077731534,50.2402240048079,39.116));
#208720=CARTESIAN_POINT('Origin',(5.69915478234096E-15,5.30016260398707E-15,
40.22725));
#208721=CARTESIAN_POINT('Origin',(34.6837837831351,47.7640607692759,40.22725));
#208722=CARTESIAN_POINT('Origin',(21.2404668433939,29.7751578089175,39.116));
#208723=CARTESIAN_POINT('Origin',(35.873256238299,49.9155525184323,39.1160373285273));
#208724=CARTESIAN_POINT('Ctrl Pts',(34.620500570364,47.67691159203,40.1599502534424));
#208725=CARTESIAN_POINT('Ctrl Pts',(34.642420023458,47.707097516846,40.10025));
#208726=CARTESIAN_POINT('Ctrl Pts',(34.6837837831352,47.7640607692759,40.10025));
#208727=CARTESIAN_POINT('Ctrl Pts',(34.5495693076632,47.7284183483598,40.1599500566048));
#208728=CARTESIAN_POINT('Ctrl Pts',(34.5907418558588,47.7446195594498,40.1002551305351));
#208729=CARTESIAN_POINT('Ctrl Pts',(34.6425747206411,47.7939730310143,40.10025));
#208730=CARTESIAN_POINT('Ctrl Pts',(34.4983910654774,47.7959261043552,40.1203070619042));
#208731=CARTESIAN_POINT('Ctrl Pts',(34.5563698228282,47.797671475652,40.0637098684499));
#208732=CARTESIAN_POINT('Ctrl Pts',(34.6188891978606,47.8415056181567,40.0772636213362));
#208733=CARTESIAN_POINT('Ctrl Pts',(34.4545839152295,47.9165880269723,40.0046102245806));
#208734=CARTESIAN_POINT('Ctrl Pts',(34.5404685123901,47.8837591046483,39.9670001894012));
#208735=CARTESIAN_POINT('Ctrl Pts',(34.6111463389769,47.9359643384878,40.0101788811209));
#208736=CARTESIAN_POINT('Ctrl Pts',(34.4602354682508,47.9696250311912,39.9303710930183));
#208737=CARTESIAN_POINT('Ctrl Pts',(34.5595777906775,47.9171136764607,39.905866357411));
#208738=CARTESIAN_POINT('Ctrl Pts',(34.625816696831,47.9824460410481,39.9671344706369));
#208739=CARTESIAN_POINT('Ctrl Pts',(34.4869303039402,48.0063682005183,39.8576902534424));
#208740=CARTESIAN_POINT('Ctrl Pts',(34.5894948283139,47.9324532779034,39.8579948730703));
#208741=CARTESIAN_POINT('Ctrl Pts',(34.6525130919802,48.0191904766733,39.92499));
#208742=CARTESIAN_POINT('Origin',(34.5497679336946,48.0938392037144,39.92499));
#208743=CARTESIAN_POINT('Origin',(35.8473027479618,49.8797426632445,39.192555448885));
#208744=CARTESIAN_POINT('Origin',(35.7991993820668,49.8135340601219,39.3343017080178));
#208745=CARTESIAN_POINT('Origin',(34.6544814981813,48.2379650606536,39.6398955069209));
#208746=CARTESIAN_POINT('Origin',(34.759195062554,48.3820909175325,39.3548010137695));
#208747=CARTESIAN_POINT('Ctrl Pts',(35.6052536882608,49.5465907136141,39.3978017080178));
#208748=CARTESIAN_POINT('Ctrl Pts',(35.7079988465464,49.4719419865729,39.3978017080178));
#208749=CARTESIAN_POINT('Ctrl Pts',(35.7079988465464,49.4719419865729,39.5248017080178));
#208750=CARTESIAN_POINT('Ctrl Pts',(35.6583499840587,49.6192730640949,39.3978017080178));
#208751=CARTESIAN_POINT('Ctrl Pts',(35.7608559931214,49.5446936074884,39.3980355775201));
#208752=CARTESIAN_POINT('Ctrl Pts',(35.7873581223574,49.5811706590209,39.5248015517192));
#208753=CARTESIAN_POINT('Ctrl Pts',(35.7085550527699,49.6880007749208,39.3484893995498));
#208754=CARTESIAN_POINT('Ctrl Pts',(35.8110857017869,49.6138288703721,39.3489438303412));
#208755=CARTESIAN_POINT('Ctrl Pts',(35.8623979633517,49.6844541394804,39.4508333155595));
#208756=CARTESIAN_POINT('Ctrl Pts',(35.7350130971395,49.7242207306171,39.2708017080178));
#208757=CARTESIAN_POINT('Ctrl Pts',(35.8375861910562,49.6503036646781,39.2710850691866));
#208758=CARTESIAN_POINT('Ctrl Pts',(35.9019445403524,49.7388853330807,39.3343017080178));
#208759=CARTESIAN_POINT('Origin',(35.6052536882608,49.5465907136141,39.5248017080178));
#208760=CARTESIAN_POINT('Ctrl Pts',(34.6963546279291,48.2946219293742,39.2875012672119));
#208761=CARTESIAN_POINT('Ctrl Pts',(34.7990735298991,48.2205921526132,39.2878045257519));
#208762=CARTESIAN_POINT('Ctrl Pts',(34.8620346481364,48.3075723994624,39.3549015218347));
#208763=CARTESIAN_POINT('Ctrl Pts',(34.7638392294029,48.387716530749,39.1034938540228));
#208764=CARTESIAN_POINT('Ctrl Pts',(34.8665617960674,48.3134813154523,39.1038286278818));
#208765=CARTESIAN_POINT('Ctrl Pts',(34.916082457139,48.3819628268498,39.2077506434048));
#208766=CARTESIAN_POINT('Ctrl Pts',(34.885073474582,48.5549570506171,38.989));
#208767=CARTESIAN_POINT('Ctrl Pts',(34.9878985031391,48.4804861171447,38.9892298954611));
#208768=CARTESIAN_POINT('Ctrl Pts',(35.013176915674,48.515601884576,39.1161900347271));
#208769=CARTESIAN_POINT('Ctrl Pts',(35.012421476459,48.7306271754172,38.989));
#208770=CARTESIAN_POINT('Ctrl Pts',(35.1153205397472,48.6558666298465,38.989));
#208771=CARTESIAN_POINT('Ctrl Pts',(35.1151665196478,48.6559785319989,39.1161900945645));
#208772=CARTESIAN_POINT('Origin',(35.012421476459,48.7306271754172,39.116));
#208773=CARTESIAN_POINT('Origin',(20.7197400704249,29.0584388930977,39.5248017080178));
#208774=CARTESIAN_POINT('Origin',(35.5163757878401,49.4242607783457,39.5248017080178));
#208775=CARTESIAN_POINT('Origin',(20.6381965522797,28.9462038689911,39.116));
#208776=CARTESIAN_POINT('Origin',(35.2482948100405,49.0553654007522,39.1160402713845));
#208777=CARTESIAN_POINT('Ctrl Pts',(35.3866101428265,49.2466351556009,39.2708017080178));
#208778=CARTESIAN_POINT('Ctrl Pts',(35.4901170100373,49.1720533660027,39.27051194648));
#208779=CARTESIAN_POINT('Ctrl Pts',(35.4251752107443,49.0826686475731,39.3343017080178));
#208780=CARTESIAN_POINT('Ctrl Pts',(35.4131599099226,49.2829758776393,39.3487519301185));
#208781=CARTESIAN_POINT('Ctrl Pts',(35.5164304941056,49.2082707697385,39.3482879463972));
#208782=CARTESIAN_POINT('Ctrl Pts',(35.4648554356505,49.1372837917341,39.4512271261624));
#208783=CARTESIAN_POINT('Ctrl Pts',(35.4634578610134,49.3518235761936,39.3978017080178));
#208784=CARTESIAN_POINT('Ctrl Pts',(35.5663414789288,49.2769673468819,39.3975673827415));
#208785=CARTESIAN_POINT('Ctrl Pts',(35.5400289748693,49.2407512920126,39.5248015355194));
#208786=CARTESIAN_POINT('Ctrl Pts',(35.5163757878401,49.4242607783457,39.3978017080178));
#208787=CARTESIAN_POINT('Ctrl Pts',(35.6191209461258,49.3496120513045,39.3978017080178));
#208788=CARTESIAN_POINT('Ctrl Pts',(35.6191209461258,49.3496120513045,39.5248017080178));
#208789=CARTESIAN_POINT('Origin',(35.3224300524587,49.1573173746142,39.3343017080178));
#208790=CARTESIAN_POINT('Origin',(35.274613565047,49.0915036263512,39.1934008533544));
#208791=CARTESIAN_POINT('Origin',(41.3366772861977,45.4345348113602,39.1925554495083));
#208792=CARTESIAN_POINT('Origin',(41.366308575564,45.4673664422105,39.1160373285273));
#208793=CARTESIAN_POINT('Origin',(41.2819167515334,45.3737170758068,39.3343017080178));
#208794=CARTESIAN_POINT('Ctrl Pts',(41.2079002115913,45.2923641298552,39.2708017080178));
#208795=CARTESIAN_POINT('Ctrl Pts',(41.1142722655012,45.3773275334101,39.2710850691866));
#208796=CARTESIAN_POINT('Ctrl Pts',(41.1875373586978,45.4586966628144,39.3343017080178));
#208797=CARTESIAN_POINT('Ctrl Pts',(41.1778715515039,45.2588408013016,39.3487519293518));
#208798=CARTESIAN_POINT('Ctrl Pts',(41.0840023845219,45.343709424771,39.349206866291));
#208799=CARTESIAN_POINT('Ctrl Pts',(41.1423656859486,45.4085284377433,39.4512271248737));
#208800=CARTESIAN_POINT('Ctrl Pts',(41.1209827764384,45.1953306044442,39.3978017080178));
#208801=CARTESIAN_POINT('Ctrl Pts',(41.026720335924,45.2800912647201,39.3980347781197));
#208802=CARTESIAN_POINT('Ctrl Pts',(41.0567886774853,45.3134855411624,39.524801535519));
#208803=CARTESIAN_POINT('Ctrl Pts',(41.0611303347409,45.1285089182128,39.3978017080178));
#208804=CARTESIAN_POINT('Ctrl Pts',(40.9667509419053,45.2134885052204,39.3978017080178));
#208805=CARTESIAN_POINT('Ctrl Pts',(40.9667509419053,45.2134885052204,39.5248017080178));
#208806=CARTESIAN_POINT('Origin',(41.0611303347409,45.1285089182128,39.5248017080178));
#208807=CARTESIAN_POINT('Origin',(0.235948482089076,-0.21244896751894,39.116));
#208808=CARTESIAN_POINT('Origin',(41.6348281284267,45.7656648676101,39.116));
#208809=CARTESIAN_POINT('Origin',(0.235948482089076,-0.21244896751894,39.5248017080178));
#208810=CARTESIAN_POINT('Origin',(40.959952356613,45.0161393894788,39.5248017080178));
#208811=CARTESIAN_POINT('Ctrl Pts',(41.9955727382256,46.1654920697607,39.2875012672119));
#208812=CARTESIAN_POINT('Ctrl Pts',(41.9009568150788,46.2513146333399,39.287208709576));
#208813=CARTESIAN_POINT('Ctrl Pts',(41.8286119029184,46.1706818621616,39.3549016990121));
#208814=CARTESIAN_POINT('Ctrl Pts',(41.9185486398962,46.0801220723588,39.1034939173931));
#208815=CARTESIAN_POINT('Ctrl Pts',(41.8239131221214,46.165748554905,39.1031692336345));
#208816=CARTESIAN_POINT('Ctrl Pts',(41.7670844335144,46.1023486848294,39.2077507202296));
#208817=CARTESIAN_POINT('Ctrl Pts',(41.7801771152788,45.926758472166,38.989));
#208818=CARTESIAN_POINT('Ctrl Pts',(41.6856154234981,46.0121526898551,38.9887769311158));
#208819=CARTESIAN_POINT('Ctrl Pts',(41.6565528363077,45.9795909100367,39.1161898712914));
#208820=CARTESIAN_POINT('Ctrl Pts',(41.6348281284267,45.7656648676101,38.989));
#208821=CARTESIAN_POINT('Ctrl Pts',(41.5403077371549,45.8507714101799,38.989));
#208822=CARTESIAN_POINT('Ctrl Pts',(41.5404488407565,45.8506443599264,39.1161895903853));
#208823=CARTESIAN_POINT('Origin',(41.9230990057961,46.0858221116773,39.3548010137695));
#208824=CARTESIAN_POINT('Ctrl Pts',(40.959952356613,45.0161393894788,39.3978017080178));
#208825=CARTESIAN_POINT('Ctrl Pts',(40.8655729637774,45.1011189764864,39.3978017080178));
#208826=CARTESIAN_POINT('Ctrl Pts',(40.8655729637774,45.1011189764864,39.5248017080178));
#208827=CARTESIAN_POINT('Ctrl Pts',(40.899898054678,44.9490914662986,39.3978017080178));
#208828=CARTESIAN_POINT('Ctrl Pts',(40.8052862548051,45.0341638030236,39.3975666025031));
#208829=CARTESIAN_POINT('Ctrl Pts',(40.7752309130129,45.000783964292,39.5248015517196));
#208830=CARTESIAN_POINT('Ctrl Pts',(40.8431135311188,44.8856913339448,39.3484894016716));
#208831=CARTESIAN_POINT('Ctrl Pts',(40.7485699563816,44.9711739722015,39.3480259000038));
#208832=CARTESIAN_POINT('Ctrl Pts',(40.6898060629487,44.9059100567333,39.4508333188935));
#208833=CARTESIAN_POINT('Ctrl Pts',(40.8131880745612,44.8522789915937,39.2708017080178));
#208834=CARTESIAN_POINT('Ctrl Pts',(40.7187157882343,44.9380175594357,39.27051194648));
#208835=CARTESIAN_POINT('Ctrl Pts',(40.6447864996558,44.8559107663281,39.3343017080178));
#208836=CARTESIAN_POINT('Origin',(40.7391658924914,44.7709311793205,39.3343017080178));
#208837=CARTESIAN_POINT('Origin',(42.0423040287729,46.218212702065,39.639895506818));
#208838=CARTESIAN_POINT('Origin',(42.1615090516458,46.3506032922589,39.92499));
#208839=CARTESIAN_POINT('Origin',(40.6847319383107,44.7104761485831,39.1934008539946));
#208840=CARTESIAN_POINT('Origin',(40.6548553974685,44.6772189625516,39.1160402713843));
#208841=CARTESIAN_POINT('Ctrl Pts',(42.1358900227701,46.7738319284252,40.1599502534424));
#208842=CARTESIAN_POINT('Ctrl Pts',(42.1109214781067,46.7461150696867,40.10025));
#208843=CARTESIAN_POINT('Ctrl Pts',(42.0638038389706,46.6938111422599,40.10025));
#208844=CARTESIAN_POINT('Ctrl Pts',(42.2013581359415,46.7148552537629,40.1599500538455));
#208845=CARTESIAN_POINT('Ctrl Pts',(42.1586072771699,46.7031532960216,40.100244835349));
#208846=CARTESIAN_POINT('Ctrl Pts',(42.1016932886506,46.6596664560519,40.10025));
#208847=CARTESIAN_POINT('Ctrl Pts',(42.2450249725429,46.6418481388115,40.1202442001042));
#208848=CARTESIAN_POINT('Ctrl Pts',(42.187045528663,46.6464039985659,40.0633873868017));
#208849=CARTESIAN_POINT('Ctrl Pts',(42.1199142759252,46.6095714048492,40.0772271723541));
#208850=CARTESIAN_POINT('Ctrl Pts',(42.2756632139854,46.5164783566517,40.0045995998159));
#208851=CARTESIAN_POINT('Ctrl Pts',(42.1934768724838,46.5588531737043,39.9663485808314));
#208852=CARTESIAN_POINT('Ctrl Pts',(42.1171707421508,46.514259642349,40.0101727202462));
#208853=CARTESIAN_POINT('Ctrl Pts',(42.2644092166203,46.4640705998035,39.9304654349861));
#208854=CARTESIAN_POINT('Ctrl Pts',(42.1708301402944,46.5278411618565,39.9051900162951));
#208855=CARTESIAN_POINT('Ctrl Pts',(42.0975575768118,46.4693765057994,39.967185745818));
#208856=CARTESIAN_POINT('Ctrl Pts',(42.2339804752707,46.430275350542,39.8576902534424));
#208857=CARTESIAN_POINT('Ctrl Pts',(42.1395065321005,46.515965540527,39.8573998014387));
#208858=CARTESIAN_POINT('Ctrl Pts',(42.0671296588101,46.4355828792665,39.92499));
#208859=CARTESIAN_POINT('Origin',(42.0638038389706,46.6938111422599,40.22725));
#208860=CARTESIAN_POINT('Origin',(0.235948482089076,-0.21244896751894,39.116));
#208861=CARTESIAN_POINT('Origin',(40.3862543050944,44.3789831537291,39.116));
#208862=CARTESIAN_POINT('Origin',(5.55434424446678E-15,5.57234773665839E-15,
40.22725));
#208863=CARTESIAN_POINT('Origin',(42.0411527846901,46.7142062431418,40.22725));
#208864=CARTESIAN_POINT('Ctrl Pts',(40.3862543050944,44.3789831537291,38.989));
#208865=CARTESIAN_POINT('Ctrl Pts',(40.2917335276659,44.4640900439958,38.989));
#208866=CARTESIAN_POINT('Ctrl Pts',(40.2918750180005,44.4639626455264,39.1161901092328));
#208867=CARTESIAN_POINT('Ctrl Pts',(40.240897875948,44.2178916378582,38.989));
#208868=CARTESIAN_POINT('Ctrl Pts',(40.1466757825285,44.3029863283993,38.9892298989778));
#208869=CARTESIAN_POINT('Ctrl Pts',(40.1757689690828,44.3350138149353,39.1161900493208));
#208870=CARTESIAN_POINT('Ctrl Pts',(40.1025190720977,44.0645366033549,39.1034966344368));
#208871=CARTESIAN_POINT('Ctrl Pts',(40.0085488431135,44.1495800756922,39.1038314102538));
#208872=CARTESIAN_POINT('Ctrl Pts',(40.0652381943489,44.2122569536116,39.2077528789592));
#208873=CARTESIAN_POINT('Ctrl Pts',(40.0254908126594,43.9791725362578,39.2875012672119));
#208874=CARTESIAN_POINT('Ctrl Pts',(39.9317222927445,44.0642551375174,39.2878045257868));
#208875=CARTESIAN_POINT('Ctrl Pts',(40.0037114790895,44.1439246138547,39.3549015295903));
#208876=CARTESIAN_POINT('Origin',(40.0979831325504,44.0588255818373,39.3548010137695));
#208877=CARTESIAN_POINT('Ctrl Pts',(41.7612723673368,46.855903642698,39.8576902534424));
#208878=CARTESIAN_POINT('Ctrl Pts',(41.8563683535936,46.7709043015497,39.8573998014387));
#208879=CARTESIAN_POINT('Ctrl Pts',(41.7839914803032,46.6905216402892,39.92499));
#208880=CARTESIAN_POINT('Ctrl Pts',(41.7917156448194,46.8897135983604,39.9304984902491));
#208881=CARTESIAN_POINT('Ctrl Pts',(41.8649095672154,46.8033160448216,39.90521715698));
#208882=CARTESIAN_POINT('Ctrl Pts',(41.8144332630849,46.7243306652203,39.9672049726612));
#208883=CARTESIAN_POINT('Ctrl Pts',(41.8425440045886,46.9062450310961,40.0043437678661));
#208884=CARTESIAN_POINT('Ctrl Pts',(41.8933569085963,46.8289264627101,39.9661628577639));
#208885=CARTESIAN_POINT('Ctrl Pts',(41.8569022891477,46.7483907976678,40.0100243556236));
#208886=CARTESIAN_POINT('Ctrl Pts',(41.9695156381237,46.8892773184516,40.1194874821988));
#208887=CARTESIAN_POINT('Ctrl Pts',(41.9804178820376,46.8319191778363,40.0627551483143));
#208888=CARTESIAN_POINT('Ctrl Pts',(41.9507871007491,46.7612136652286,40.0767884282376));
#208889=CARTESIAN_POINT('Ctrl Pts',(42.0474864684053,46.8534019544971,40.1599502015382));
#208890=CARTESIAN_POINT('Ctrl Pts',(42.0403508033701,46.8096319157661,40.1002449453869));
#208891=CARTESIAN_POINT('Ctrl Pts',(42.0031091842997,46.7484320121841,40.10025));
#208892=CARTESIAN_POINT('Ctrl Pts',(42.1132001506006,46.7942619810912,40.1599502534424));
#208893=CARTESIAN_POINT('Ctrl Pts',(42.0882450513181,46.7665330160774,40.10025));
#208894=CARTESIAN_POINT('Ctrl Pts',(42.0411527846901,46.7142062431418,40.10025));
#208895=CARTESIAN_POINT('Origin',(41.6896120874676,46.7755012272968,39.92499));
#208896=CARTESIAN_POINT('Origin',(39.9787779456735,43.9264348094991,39.6398955069315));
#208897=CARTESIAN_POINT('Origin',(39.859572758736,43.794044037014,39.92499));
#208898=CARTESIAN_POINT('Origin',(41.5704070646205,46.6431106370574,39.6398955068284));
#208899=CARTESIAN_POINT('Origin',(41.451202041618,46.5107200467152,39.3548010137695));
#208900=CARTESIAN_POINT('Ctrl Pts',(39.7870778846752,43.7143933160618,39.8576902534424));
#208901=CARTESIAN_POINT('Ctrl Pts',(39.6934538167806,43.7993487829608,39.8579948730703));
#208902=CARTESIAN_POINT('Ctrl Pts',(39.7651933659004,43.8790236240215,39.92499));
#208903=CARTESIAN_POINT('Ctrl Pts',(39.7566748466922,43.6806281164521,39.9304020711231));
#208904=CARTESIAN_POINT('Ctrl Pts',(39.6846648960476,43.7668791656722,39.9058915297384));
#208905=CARTESIAN_POINT('Ctrl Pts',(39.7347894633641,43.845256669365,39.9671523786032));
#208906=CARTESIAN_POINT('Ctrl Pts',(39.7061132086034,43.6642103943284,40.0043257306692));
#208907=CARTESIAN_POINT('Ctrl Pts',(39.6560595510438,43.7414086642726,39.9667894847835));
#208908=CARTESIAN_POINT('Ctrl Pts',(39.6925108309094,43.8213838166739,40.01001389752));
#208909=CARTESIAN_POINT('Ctrl Pts',(39.5798624575883,43.6815693876447,40.1195533054858));
#208910=CARTESIAN_POINT('Ctrl Pts',(39.5692094437574,43.7388169234802,40.0630813209236));
#208911=CARTESIAN_POINT('Ctrl Pts',(39.5991004926186,43.8091742082548,40.0768265942421));
#208912=CARTESIAN_POINT('Ctrl Pts',(39.5024012818823,43.7176736830024,40.1599502027513));
#208913=CARTESIAN_POINT('Ctrl Pts',(39.5096522555304,43.7613473163387,40.1002552791553));
#208914=CARTESIAN_POINT('Ctrl Pts',(39.5470931435016,43.8223603708611,40.10025));
#208915=CARTESIAN_POINT('Ctrl Pts',(39.4370498736014,43.7765468711718,40.1599502534424));
#208916=CARTESIAN_POINT('Ctrl Pts',(39.4620188529815,43.8042633382925,40.10025));
#208917=CARTESIAN_POINT('Ctrl Pts',(39.5091373124628,43.8565665267052,40.10025));
#208918=CARTESIAN_POINT('Origin',(39.5091373124628,43.8565665267052,40.22725));
#208919=CARTESIAN_POINT('Ctrl Pts',(41.1629311642486,46.190562802648,38.989));
#208920=CARTESIAN_POINT('Ctrl Pts',(41.2574515636637,46.1054562527461,38.989));
#208921=CARTESIAN_POINT('Ctrl Pts',(41.2573104519068,46.1055833103427,39.1161896013266));
#208922=CARTESIAN_POINT('Ctrl Pts',(41.3079514313265,46.3519569305998,38.989));
#208923=CARTESIAN_POINT('Ctrl Pts',(41.4027622547802,46.2668393800551,38.9887769275466));
#208924=CARTESIAN_POINT('Ctrl Pts',(41.3734162510838,46.2345318643235,39.1161898821848));
#208925=CARTESIAN_POINT('Ctrl Pts',(41.4460100362754,46.5056000892402,39.1034967087243));
#208926=CARTESIAN_POINT('Ctrl Pts',(41.5410595633975,46.4204333915625,39.1031720232707));
#208927=CARTESIAN_POINT('Ctrl Pts',(41.4839469723848,46.3572886670227,39.2077529615));
#208928=CARTESIAN_POINT('Ctrl Pts',(41.5228599914568,46.5911245387425,39.2875012672119));
#208929=CARTESIAN_POINT('Ctrl Pts',(41.6181024753234,46.5059978248573,39.2872087095507));
#208930=CARTESIAN_POINT('Ctrl Pts',(41.5454735069382,46.4256208064854,39.3549017048228));
#208931=CARTESIAN_POINT('Origin',(41.1629311642486,46.190562802648,39.116));
#208932=CARTESIAN_POINT('Origin',(5.70392627685665E-15,5.29629872391379E-15,
40.22725));
#208933=CARTESIAN_POINT('Origin',(39.4864862581822,43.876961627587,40.22725));
#208934=CARTESIAN_POINT('Origin',(27.6232705441551,31.1532462714325,39.116));
#208935=CARTESIAN_POINT('Origin',(40.8943347850524,45.8923335519894,39.1160373285266));
#208936=CARTESIAN_POINT('Ctrl Pts',(39.4144401478995,43.7969047596342,40.1599502534424));
#208937=CARTESIAN_POINT('Ctrl Pts',(39.4393948122693,43.824634116048,40.10025));
#208938=CARTESIAN_POINT('Ctrl Pts',(39.4864862581822,43.876961627587,40.10025));
#208939=CARTESIAN_POINT('Ctrl Pts',(39.3492813761647,43.855543692452,40.1599500566037));
#208940=CARTESIAN_POINT('Ctrl Pts',(39.3919218645339,43.8673524484232,40.1002551305372));
#208941=CARTESIAN_POINT('Ctrl Pts',(39.4486296259974,43.9110175468021,40.10025));
#208942=CARTESIAN_POINT('Ctrl Pts',(39.3054399757372,43.928031216904,40.1203070619045));
#208943=CARTESIAN_POINT('Ctrl Pts',(39.3632835603686,43.9237065964665,40.0637098684499));
#208944=CARTESIAN_POINT('Ctrl Pts',(39.4300423632773,43.9607655567554,40.0772636213364));
#208945=CARTESIAN_POINT('Ctrl Pts',(39.2744854109878,44.0526112349802,40.0046102245803));
#208946=CARTESIAN_POINT('Ctrl Pts',(39.3564679665374,44.0109847679677,39.9670001894012));
#208947=CARTESIAN_POINT('Ctrl Pts',(39.4322155454632,44.0555161714739,40.0101788811208));
#208948=CARTESIAN_POINT('Ctrl Pts',(39.2856498807583,44.1047669487872,39.9303710930185));
#208949=CARTESIAN_POINT('Ctrl Pts',(39.3789590643339,44.0421591564552,39.9058663574116));
#208950=CARTESIAN_POINT('Ctrl Pts',(39.4516641985,44.1002097724411,39.9671344706361));
#208951=CARTESIAN_POINT('Ctrl Pts',(39.3160391863695,44.1385184650371,39.8576902534424));
#208952=CARTESIAN_POINT('Ctrl Pts',(39.4103156382737,44.0542875439835,39.8579948730703));
#208953=CARTESIAN_POINT('Ctrl Pts',(39.4820551873935,44.1339623850442,39.92499));
#208954=CARTESIAN_POINT('Origin',(39.3876757945579,44.2189419720518,39.92499));
#208955=CARTESIAN_POINT('Origin',(40.8647803215182,45.8594327453949,39.1925554488842));
#208956=CARTESIAN_POINT('Origin',(40.8100197873553,45.7986150108446,39.3343017080178));
#208957=CARTESIAN_POINT('Origin',(39.5068809815259,44.351332744489,39.639895506922));
#208958=CARTESIAN_POINT('Origin',(39.6260861683723,44.4837235168752,39.3548010137695));
#208959=CARTESIAN_POINT('Ctrl Pts',(40.5892333705628,45.5534068532507,39.3978017080178));
#208960=CARTESIAN_POINT('Ctrl Pts',(40.6836127633984,45.4684272662431,39.3978017080178));
#208961=CARTESIAN_POINT('Ctrl Pts',(40.6836127633984,45.4684272662431,39.5248017080178));
#208962=CARTESIAN_POINT('Ctrl Pts',(40.649636173698,45.6201409680068,39.3978017080178));
#208963=CARTESIAN_POINT('Ctrl Pts',(40.7437849681284,45.5352552698624,39.3980355775182));
#208964=CARTESIAN_POINT('Ctrl Pts',(40.7739548060691,45.5687622694484,39.5248015517192));
#208965=CARTESIAN_POINT('Ctrl Pts',(40.7067502157887,45.6832443225589,39.3484893995498));
#208966=CARTESIAN_POINT('Ctrl Pts',(40.8009661159848,45.598761368283,39.3489438303427));
#208967=CARTESIAN_POINT('Ctrl Pts',(40.8593796344556,45.6636361529315,39.4508333155593));
#208968=CARTESIAN_POINT('Ctrl Pts',(40.7368493365303,45.7165002428302,39.2708017080178));
#208969=CARTESIAN_POINT('Ctrl Pts',(40.8311340869943,45.6322662944328,39.2710850691866));
#208970=CARTESIAN_POINT('Ctrl Pts',(40.9043991801909,45.7136354238371,39.3343017080178));
#208971=CARTESIAN_POINT('Origin',(40.5892333705628,45.5534068532507,39.5248017080178));
#208972=CARTESIAN_POINT('Ctrl Pts',(39.5544469813076,44.4033023070485,39.2875012672119));
#208973=CARTESIAN_POINT('Ctrl Pts',(39.648864959584,44.3189410241791,39.2878045257518));
#208974=CARTESIAN_POINT('Ctrl Pts',(39.7205730817656,44.3988635551999,39.3549015218346));
#208975=CARTESIAN_POINT('Ctrl Pts',(39.6312929306926,44.4888328647709,39.1034938540228));
#208976=CARTESIAN_POINT('Ctrl Pts',(39.7256930794107,44.4042668857132,39.1038286278792));
#208977=CARTESIAN_POINT('Ctrl Pts',(39.7821007282715,44.4671969296239,39.2077506434031));
#208978=CARTESIAN_POINT('Ctrl Pts',(39.7693444365344,44.6424847942243,38.989));
#208979=CARTESIAN_POINT('Ctrl Pts',(39.8638218465944,44.5576736780982,38.9892298954635));
#208980=CARTESIAN_POINT('Ctrl Pts',(39.8926323785412,44.5899547640677,39.1161900347287));
#208981=CARTESIAN_POINT('Ctrl Pts',(39.9143573409162,44.803881088767,38.989));
#208982=CARTESIAN_POINT('Ctrl Pts',(40.0088781074275,44.7187742083301,38.989));
#208983=CARTESIAN_POINT('Ctrl Pts',(40.0087366280265,44.718901596955,39.1161900945644));
#208984=CARTESIAN_POINT('Origin',(39.9143573409162,44.803881088767,39.116));
#208985=CARTESIAN_POINT('Origin',(26.948440628206,30.4037717213983,39.5248017080178));
#208986=CARTESIAN_POINT('Origin',(40.4880553924349,45.4410373245167,39.5248017080178));
#208987=CARTESIAN_POINT('Origin',(26.8427652369017,30.2864073093063,39.116));
#208988=CARTESIAN_POINT('Origin',(40.1828829233537,45.1021848870408,39.1160402713856));
#208989=CARTESIAN_POINT('Ctrl Pts',(40.3404336838198,45.2779489569768,39.2708017080178));
#208990=CARTESIAN_POINT('Ctrl Pts',(40.4355776097274,45.1929563204585,39.27051194648));
#208991=CARTESIAN_POINT('Ctrl Pts',(40.3616483211489,45.1108495273508,39.3343017080178));
#208992=CARTESIAN_POINT('Ctrl Pts',(40.3706366483424,45.3113153943829,39.3487519301185));
#208993=CARTESIAN_POINT('Ctrl Pts',(40.4655326953331,45.2262248134121,39.3482879463962));
#208994=CARTESIAN_POINT('Ctrl Pts',(40.4068200107198,45.1610177711042,39.4512271261628));
#208995=CARTESIAN_POINT('Ctrl Pts',(40.4278556061236,45.3745283705079,39.3978017080178));
#208996=CARTESIAN_POINT('Ctrl Pts',(40.5223510102012,45.2893279449763,39.3975673827434));
#208997=CARTESIAN_POINT('Ctrl Pts',(40.4923970402304,45.2560606910606,39.5248015355199));
#208998=CARTESIAN_POINT('Ctrl Pts',(40.4880553924349,45.4410373245167,39.3978017080178));
#208999=CARTESIAN_POINT('Ctrl Pts',(40.5824347852705,45.3560577375091,39.3978017080178));
#209000=CARTESIAN_POINT('Ctrl Pts',(40.5824347852705,45.3560577375091,39.5248017080178));
#209001=CARTESIAN_POINT('Origin',(40.2672689283133,45.1958291143584,39.3343017080178));
#209002=CARTESIAN_POINT('Origin',(40.2128349746544,45.1353740846425,39.1934008533546));
#209003=CARTESIAN_POINT('Origin',(45.8594327460071,40.8647803224529,39.1925554495079));
#209004=CARTESIAN_POINT('Origin',(45.8923335519876,40.894334785052,39.1160373285244));
#209005=CARTESIAN_POINT('Origin',(45.7986150108456,40.8100197873542,39.3343017080178));
#209006=CARTESIAN_POINT('Ctrl Pts',(45.7165002428312,40.7368493365292,39.2708017080178));
#209007=CARTESIAN_POINT('Ctrl Pts',(45.6322662944338,40.8311340869932,39.2710850691866));
#209008=CARTESIAN_POINT('Ctrl Pts',(45.7136354238381,40.9043991801898,39.3343017080178));
#209009=CARTESIAN_POINT('Ctrl Pts',(45.6831319408695,40.7066485019686,39.3487519293518));
#209010=CARTESIAN_POINT('Ctrl Pts',(45.5986481858001,40.800864206016,39.3492068662937));
#209011=CARTESIAN_POINT('Ctrl Pts',(45.6634671987692,40.8592275074425,39.4512271248741));
#209012=CARTESIAN_POINT('Ctrl Pts',(45.6199161851854,40.6494327168512,39.3978017080178));
#209013=CARTESIAN_POINT('Ctrl Pts',(45.5350300257422,40.7435821574116,39.3980347781178));
#209014=CARTESIAN_POINT('Ctrl Pts',(45.5684243021845,40.773650498976,39.5248015355195));
#209015=CARTESIAN_POINT('Ctrl Pts',(45.5534068532516,40.5892333705617,39.3978017080178));
#209016=CARTESIAN_POINT('Ctrl Pts',(45.468427266244,40.6836127633974,39.3978017080178));
#209017=CARTESIAN_POINT('Ctrl Pts',(45.4684272662441,40.6836127633974,39.5248017080178));
#209018=CARTESIAN_POINT('Origin',(45.5534068532516,40.5892333705617,39.5248017080178));
#209019=CARTESIAN_POINT('Origin',(0.21244896751894,-0.235948482089075,39.116));
#209020=CARTESIAN_POINT('Origin',(46.190562802649,41.1629311642475,39.116));
#209021=CARTESIAN_POINT('Origin',(0.21244896751894,-0.235948482089075,39.5248017080178));
#209022=CARTESIAN_POINT('Origin',(45.4410373245177,40.4880553924338,39.5248017080178));
#209023=CARTESIAN_POINT('Ctrl Pts',(46.5911245387435,41.5228599914557,39.2875012672119));
#209024=CARTESIAN_POINT('Ctrl Pts',(46.5059978322081,41.6181024670992,39.287208709576));
#209025=CARTESIAN_POINT('Ctrl Pts',(46.4256208133857,41.5454735131714,39.3549016990122));
#209026=CARTESIAN_POINT('Ctrl Pts',(46.5055987918431,41.4460088704685,39.1034939173931));
#209027=CARTESIAN_POINT('Ctrl Pts',(46.4204321019733,41.5410583874199,39.1031692336321));
#209028=CARTESIAN_POINT('Ctrl Pts',(46.3572876358796,41.4839460439595,39.2077507202298));
#209029=CARTESIAN_POINT('Ctrl Pts',(46.3519544194676,41.307949174951,38.989));
#209030=CARTESIAN_POINT('Ctrl Pts',(46.2668368728777,41.402759982509,38.9887769311206));
#209031=CARTESIAN_POINT('Ctrl Pts',(46.2345298607752,41.3734144471008,39.1161898712915));
#209032=CARTESIAN_POINT('Ctrl Pts',(46.190562802649,41.1629311642475,38.989));
#209033=CARTESIAN_POINT('Ctrl Pts',(46.1054562600791,41.2574515555194,38.989));
#209034=CARTESIAN_POINT('Ctrl Pts',(46.1055833103327,41.2573104519178,39.1161895903854));
#209035=CARTESIAN_POINT('Origin',(46.5107200467162,41.4512020416168,39.3548010137695));
#209036=CARTESIAN_POINT('Ctrl Pts',(45.4410373245177,40.4880553924338,39.3978017080178));
#209037=CARTESIAN_POINT('Ctrl Pts',(45.3560577375101,40.5824347852694,39.3978017080178));
#209038=CARTESIAN_POINT('Ctrl Pts',(45.3560577375101,40.5824347852694,39.5248017080178));
#209039=CARTESIAN_POINT('Ctrl Pts',(45.374303589957,40.427652148686,39.3978017080178));
#209040=CARTESIAN_POINT('Ctrl Pts',(45.2891025640496,40.522148076296,39.3975666025003));
#209041=CARTESIAN_POINT('Ctrl Pts',(45.2557227253159,40.4920927345052,39.5248015517177));
#209042=CARTESIAN_POINT('Ctrl Pts',(45.3112030195537,40.3705349278756,39.3484894016716));
#209043=CARTESIAN_POINT('Ctrl Pts',(45.2261127332216,40.4654317778756,39.3480259000063));
#209044=CARTESIAN_POINT('Ctrl Pts',(45.1608488177568,40.4066678844405,39.4508333188951));
#209045=CARTESIAN_POINT('Ctrl Pts',(45.2779489569777,40.3404336838187,39.2708017080178));
#209046=CARTESIAN_POINT('Ctrl Pts',(45.1929563204594,40.4355776097263,39.27051194648));
#209047=CARTESIAN_POINT('Ctrl Pts',(45.1108495273517,40.3616483211478,39.3343017080178));
#209048=CARTESIAN_POINT('Origin',(45.1958291143593,40.2672689283122,39.3343017080178));
#209049=CARTESIAN_POINT('Origin',(46.6431106370703,41.5704070646306,39.6398955068182));
#209050=CARTESIAN_POINT('Origin',(46.7755012272978,41.6896120874665,39.92499));
#209051=CARTESIAN_POINT('Origin',(45.135374083614,40.2128349741385,39.1934008539952));
#209052=CARTESIAN_POINT('Origin',(45.1021848870414,40.1828829233542,39.1160402713843));
#209053=CARTESIAN_POINT('Ctrl Pts',(46.7942619810922,42.1132001505995,40.1599502534424));
#209054=CARTESIAN_POINT('Ctrl Pts',(46.7665330160784,42.088245051317,40.10025));
#209055=CARTESIAN_POINT('Ctrl Pts',(46.7142062431428,42.041152784689,40.10025));
#209056=CARTESIAN_POINT('Ctrl Pts',(46.8532067119185,42.0477032750699,40.1599500538466));
#209057=CARTESIAN_POINT('Ctrl Pts',(46.8094668591648,42.0405341034486,40.1002448353493));
#209058=CARTESIAN_POINT('Ctrl Pts',(46.7483190388756,42.0032346206966,40.10025));
#209059=CARTESIAN_POINT('Ctrl Pts',(46.889003015487,41.9705316734057,40.1202442001039));
#209060=CARTESIAN_POINT('Ctrl Pts',(46.8318174060864,41.9811230778537,40.0633873868017));
#209061=CARTESIAN_POINT('Ctrl Pts',(46.7612038509554,41.9515093836254,40.0772271723536));
#209062=CARTESIAN_POINT('Ctrl Pts',(46.906368706767,41.8426461117366,40.0045995998162));
#209063=CARTESIAN_POINT('Ctrl Pts',(46.829061965151,41.8933796070861,39.9663485808314));
#209064=CARTESIAN_POINT('Ctrl Pts',(46.7485125544802,41.8570065263029,40.0101727202467));
#209065=CARTESIAN_POINT('Ctrl Pts',(46.8896982576911,41.7917018131128,39.9304654349859));
#209066=CARTESIAN_POINT('Ctrl Pts',(46.8032976561906,41.8649047103976,39.9051900162946));
#209067=CARTESIAN_POINT('Ctrl Pts',(46.7243152668228,41.8144193983036,39.9671857458179));
#209068=CARTESIAN_POINT('Ctrl Pts',(46.855903642699,41.7612723673357,39.8576902534424));
#209069=CARTESIAN_POINT('Ctrl Pts',(46.7709043015507,41.8563683535925,39.8573998014387));
#209070=CARTESIAN_POINT('Ctrl Pts',(46.6905216402902,41.7839914803021,39.92499));
#209071=CARTESIAN_POINT('Origin',(46.7142062431428,42.041152784689,40.22725));
#209072=CARTESIAN_POINT('Origin',(0.21244896751894,-0.235948482089075,39.116));
#209073=CARTESIAN_POINT('Origin',(44.8038810887679,39.9143573409152,39.116));
#209074=CARTESIAN_POINT('Origin',(5.54214007001405E-15,5.58455191111112E-15,
40.22725));
#209075=CARTESIAN_POINT('Origin',(46.6938111422609,42.0638038389695,40.22725));
#209076=CARTESIAN_POINT('Ctrl Pts',(44.8038810887679,39.9143573409152,38.989));
#209077=CARTESIAN_POINT('Ctrl Pts',(44.7187741985015,40.0088781183433,38.989));
#209078=CARTESIAN_POINT('Ctrl Pts',(44.7189015969706,40.0087366280091,39.1161901092324));
#209079=CARTESIAN_POINT('Ctrl Pts',(44.642482288749,39.7693421853891,38.989));
#209080=CARTESIAN_POINT('Ctrl Pts',(44.5576711710494,39.8638196089392,38.9892298989784));
#209081=CARTESIAN_POINT('Ctrl Pts',(44.5899527660337,39.8926305794719,39.1161900493204));
#209082=CARTESIAN_POINT('Ctrl Pts',(44.4888315723744,39.6312917695255,39.1034966344368));
#209083=CARTESIAN_POINT('Ctrl Pts',(44.4042655856142,39.7256919284549,39.1038314102545));
#209084=CARTESIAN_POINT('Ctrl Pts',(44.4671959043828,39.782099805109,39.2077528789597));
#209085=CARTESIAN_POINT('Ctrl Pts',(44.4033023070494,39.5544469813066,39.2875012672119));
#209086=CARTESIAN_POINT('Ctrl Pts',(44.3189410144585,39.6488649704634,39.2878045257868));
#209087=CARTESIAN_POINT('Ctrl Pts',(44.3988635644387,39.720573090053,39.35490152959));
#209088=CARTESIAN_POINT('Origin',(44.4837235168761,39.6260861683712,39.3548010137695));
#209089=CARTESIAN_POINT('Ctrl Pts',(46.430275350543,42.2339804752696,39.8576902534424));
#209090=CARTESIAN_POINT('Ctrl Pts',(46.515965540528,42.1395065320994,39.8573998014387));
#209091=CARTESIAN_POINT('Ctrl Pts',(46.4355828792675,42.067129658809,39.92499));
#209092=CARTESIAN_POINT('Ctrl Pts',(46.4640859592749,42.2644230274448,39.930498490249));
#209093=CARTESIAN_POINT('Ctrl Pts',(46.5278479142031,42.1708479205164,39.9052171569796));
#209094=CARTESIAN_POINT('Ctrl Pts',(46.4693919041993,42.0975714415914,39.9672049726599));
#209095=CARTESIAN_POINT('Ctrl Pts',(46.5163638812303,42.2755508889258,40.0043437678663));
#209096=CARTESIAN_POINT('Ctrl Pts',(46.5588164356978,42.1933444849778,39.9661628577643));
#209097=CARTESIAN_POINT('Ctrl Pts',(46.5141432491637,42.1170605480846,40.0100243556234));
#209098=CARTESIAN_POINT('Ctrl Pts',(46.6408663419438,42.245403977454,40.1194874821986));
#209099=CARTESIAN_POINT('Ctrl Pts',(46.6457133039304,42.1872204559316,40.062755148314));
#209100=CARTESIAN_POINT('Ctrl Pts',(46.6088541045845,42.1199995355539,40.0767884282378));
#209101=CARTESIAN_POINT('Ctrl Pts',(46.7146600431958,42.2015749714286,40.1599502015389));
#209102=CARTESIAN_POINT('Ctrl Pts',(46.7029882531942,42.15879058965,40.1002449453872));
#209103=CARTESIAN_POINT('Ctrl Pts',(46.6595535157374,42.1018187547551,40.10025));
#209104=CARTESIAN_POINT('Ctrl Pts',(46.7738319284262,42.1358900227689,40.1599502534424));
#209105=CARTESIAN_POINT('Ctrl Pts',(46.7461150696877,42.1109214781056,40.10025));
#209106=CARTESIAN_POINT('Ctrl Pts',(46.6938111422609,42.0638038389695,40.10025));
#209107=CARTESIAN_POINT('Origin',(46.3506032922599,42.1615090516447,39.92499));
#209108=CARTESIAN_POINT('Origin',(44.3513327445049,39.5068809815356,39.6398955069335));
#209109=CARTESIAN_POINT('Origin',(44.2189419720528,39.3876757945569,39.92499));
#209110=CARTESIAN_POINT('Origin',(46.2182127020518,42.0423040287654,39.6398955068273));
#209111=CARTESIAN_POINT('Origin',(46.0858221116783,41.923099005795,39.3548010137695));
#209112=CARTESIAN_POINT('Ctrl Pts',(44.1385184650381,39.3160391863685,39.8576902534424));
#209113=CARTESIAN_POINT('Ctrl Pts',(44.0542875439845,39.4103156382726,39.8579948730703));
#209114=CARTESIAN_POINT('Ctrl Pts',(44.1339623850452,39.4820551873925,39.92499));
#209115=CARTESIAN_POINT('Ctrl Pts',(44.1047525536511,39.2856369388941,39.9304020711231));
#209116=CARTESIAN_POINT('Ctrl Pts',(44.0421527706783,39.3789425853227,39.9058915297377));
#209117=CARTESIAN_POINT('Ctrl Pts',(44.1001954303881,39.4516512848556,39.9671523786023));
#209118=CARTESIAN_POINT('Ctrl Pts',(44.0527517782422,39.2745942850996,40.0043257306693));
#209119=CARTESIAN_POINT('Ctrl Pts',(44.0110417363802,39.3566016867498,39.9667894847835));
#209120=CARTESIAN_POINT('Ctrl Pts',(44.0556530121006,39.4323285306298,40.0100138975202));
#209121=CARTESIAN_POINT('Ctrl Pts',(43.929007150946,39.3050549810245,40.1195533054857));
#209122=CARTESIAN_POINT('Ctrl Pts',(43.9243964923863,39.3631024520332,40.0630813209236));
#209123=CARTESIAN_POINT('Ctrl Pts',(43.9614781338115,39.4299498468373,40.0768265942418));
#209124=CARTESIAN_POINT('Ctrl Pts',(43.8557442421764,39.3490583909335,40.1599502027521));
#209125=CARTESIAN_POINT('Ctrl Pts',(43.867520632009,39.3917348424035,40.1002552791553));
#209126=CARTESIAN_POINT('Ctrl Pts',(43.9111340157067,39.4485000225461,40.10025));
#209127=CARTESIAN_POINT('Ctrl Pts',(43.7969047596351,39.4144401478985,40.1599502534424));
#209128=CARTESIAN_POINT('Ctrl Pts',(43.824634116049,39.4393948122683,40.10025));
#209129=CARTESIAN_POINT('Ctrl Pts',(43.8769616275879,39.4864862581812,40.10025));
#209130=CARTESIAN_POINT('Origin',(43.8769616275879,39.4864862581812,40.22725));
#209131=CARTESIAN_POINT('Ctrl Pts',(45.7656648676111,41.6348281284257,38.989));
#209132=CARTESIAN_POINT('Ctrl Pts',(45.8507714175132,41.5403077290104,38.989));
#209133=CARTESIAN_POINT('Ctrl Pts',(45.8506443599165,41.5404488407675,39.1161896013269));
#209134=CARTESIAN_POINT('Ctrl Pts',(45.9267609786665,41.7801793767983,38.989));
#209135=CARTESIAN_POINT('Ctrl Pts',(46.0121552117524,41.6856176794247,38.9887769275484));
#209136=CARTESIAN_POINT('Ctrl Pts',(45.9795929135641,41.6565546403119,39.1161898821851));
#209137=CARTESIAN_POINT('Ctrl Pts',(46.0801233673968,41.9185498083232,39.1034967087243));
#209138=CARTESIAN_POINT('Ctrl Pts',(46.1657498592349,41.8239142817232,39.103172023269));
#209139=CARTESIAN_POINT('Ctrl Pts',(46.1023497159534,41.7670853619627,39.2077529614997));
#209140=CARTESIAN_POINT('Ctrl Pts',(46.1654920697617,41.9955727382246,39.2875012672119));
#209141=CARTESIAN_POINT('Ctrl Pts',(46.251314640751,41.9009568069084,39.2872087095507));
#209142=CARTESIAN_POINT('Ctrl Pts',(46.1706818552411,41.8286118967072,39.3549017048229));
#209143=CARTESIAN_POINT('Origin',(45.7656648676111,41.6348281284257,39.116));
#209144=CARTESIAN_POINT('Origin',(5.70826774717982E-15,5.29195725359062E-15,
40.22725));
#209145=CARTESIAN_POINT('Origin',(43.8565665267061,39.5091373124617,40.22725));
#209146=CARTESIAN_POINT('Origin',(34.1507877370015,31.1767457860025,39.116));
#209147=CARTESIAN_POINT('Origin',(45.4673664422111,41.3663085755622,39.1160373285261));
#209148=CARTESIAN_POINT('Ctrl Pts',(43.7765468711727,39.4370498736003,40.1599502534424));
#209149=CARTESIAN_POINT('Ctrl Pts',(43.8042633382934,39.4620188529804,40.10025));
#209150=CARTESIAN_POINT('Ctrl Pts',(43.8565665267061,39.5091373124617,40.10025));
#209151=CARTESIAN_POINT('Ctrl Pts',(43.7178744835426,39.502178522486,40.1599500566038));
#209152=CARTESIAN_POINT('Ctrl Pts',(43.7615157339678,39.5094654441326,40.1002551305372));
#209153=CARTESIAN_POINT('Ctrl Pts',(43.8224770900139,39.5469637653742,40.10025));
#209154=CARTESIAN_POINT('Ctrl Pts',(43.68185026043,39.5788516269098,40.1203070619046));
#209155=CARTESIAN_POINT('Ctrl Pts',(43.7389249259235,39.5685043961837,40.0637098684499));
#209156=CARTESIAN_POINT('Ctrl Pts',(43.8091917332947,39.5983821485328,40.0772636213361));
#209157=CARTESIAN_POINT('Ctrl Pts',(43.6640874258696,39.7059848156952,40.0046102245802));
#209158=CARTESIAN_POINT('Ctrl Pts',(43.7412697217743,39.6560168722786,39.9670001894012));
#209159=CARTESIAN_POINT('Ctrl Pts',(43.8212571467122,39.6923865500758,40.010178881121));
#209160=CARTESIAN_POINT('Ctrl Pts',(43.6806424921205,39.7566878101775,39.9303710930186));
#209161=CARTESIAN_POINT('Ctrl Pts',(43.766896221903,39.6846695243133,39.9058663574107));
#209162=CARTESIAN_POINT('Ctrl Pts',(43.8452710114194,39.734802377006,39.9671344706363));
#209163=CARTESIAN_POINT('Ctrl Pts',(43.7143933160628,39.7870778846742,39.8576902534424));
#209164=CARTESIAN_POINT('Ctrl Pts',(43.7993487829618,39.6934538167795,39.8579948730703));
#209165=CARTESIAN_POINT('Ctrl Pts',(43.8790236240225,39.7651933658994,39.92499));
#209166=CARTESIAN_POINT('Origin',(43.7940440370149,39.859572758735,39.92499));
#209167=CARTESIAN_POINT('Origin',(45.4345348103669,41.3366772856866,39.1925554488846));
#209168=CARTESIAN_POINT('Origin',(45.3737170758078,41.2819167515323,39.3343017080178));
#209169=CARTESIAN_POINT('Origin',(43.9264348094888,39.9787779456578,39.6398955069202));
#209170=CARTESIAN_POINT('Origin',(44.0588255818383,40.0979831325494,39.3548010137695));
#209171=CARTESIAN_POINT('Ctrl Pts',(45.1285089182138,41.0611303347399,39.3978017080178));
#209172=CARTESIAN_POINT('Ctrl Pts',(45.2134885052213,40.9667509419042,39.3978017080178));
#209173=CARTESIAN_POINT('Ctrl Pts',(45.2134885052213,40.9667509419042,39.5248017080178));
#209174=CARTESIAN_POINT('Ctrl Pts',(45.1955564429368,41.1211850608436,39.3978017080178));
#209175=CARTESIAN_POINT('Ctrl Pts',(45.2803165088404,41.0269231466362,39.398035577521));
#209176=CARTESIAN_POINT('Ctrl Pts',(45.3138235084273,41.0570929845756,39.5248015517192));
#209177=CARTESIAN_POINT('Ctrl Pts',(45.2589537050069,41.1779726855665,39.3484893995498));
#209178=CARTESIAN_POINT('Ctrl Pts',(45.3438226072591,41.0841042944907,39.3489438303402));
#209179=CARTESIAN_POINT('Ctrl Pts',(45.4086973919088,41.1425178129605,39.450833315559));
#209180=CARTESIAN_POINT('Ctrl Pts',(45.2923641298562,41.2079002115902,39.2708017080178));
#209181=CARTESIAN_POINT('Ctrl Pts',(45.377327533411,41.1142722655001,39.2710850691866));
#209182=CARTESIAN_POINT('Ctrl Pts',(45.4586966628153,41.1875373586967,39.3343017080178));
#209183=CARTESIAN_POINT('Origin',(45.1285089182138,41.0611303347399,39.5248017080178));
#209184=CARTESIAN_POINT('Ctrl Pts',(43.9791725362587,40.0254908126583,39.2875012672119));
#209185=CARTESIAN_POINT('Ctrl Pts',(44.0642551277135,39.9317223035491,39.2878045257519));
#209186=CARTESIAN_POINT('Ctrl Pts',(44.1439246046469,40.0037114707674,39.3549015218347));
#209187=CARTESIAN_POINT('Ctrl Pts',(44.0645378932547,40.1025202360377,39.1034938540227));
#209188=CARTESIAN_POINT('Ctrl Pts',(44.1495813562438,40.0085500157857,39.1038286278816));
#209189=CARTESIAN_POINT('Ctrl Pts',(44.212257978885,40.0652391174778,39.2077506434029));
#209190=CARTESIAN_POINT('Ctrl Pts',(44.2178941385635,40.2409001323907,38.989));
#209191=CARTESIAN_POINT('Ctrl Pts',(44.3029888158492,40.1466780419453,38.9892298954605));
#209192=CARTESIAN_POINT('Ctrl Pts',(44.3350158129994,40.1757707681164,39.1161900347289));
#209193=CARTESIAN_POINT('Ctrl Pts',(44.37898315373,40.3862543050933,38.989));
#209194=CARTESIAN_POINT('Ctrl Pts',(44.464090034167,40.2917335385819,38.989));
#209195=CARTESIAN_POINT('Ctrl Pts',(44.463962645542,40.2918750179831,39.1161900945645));
#209196=CARTESIAN_POINT('Origin',(44.37898315373,40.3862543050933,39.116));
#209197=CARTESIAN_POINT('Origin',(33.3184119221875,30.4272712359683,39.5248017080178));
#209198=CARTESIAN_POINT('Origin',(45.0161393894798,40.959952356612,39.5248017080178));
#209199=CARTESIAN_POINT('Origin',(33.1880655373225,30.3099068238763,39.116));
#209200=CARTESIAN_POINT('Origin',(44.6772189625519,40.6548553974676,39.1160402713849));
#209201=CARTESIAN_POINT('Ctrl Pts',(44.8522789915946,40.8131880745601,39.2708017080178));
#209202=CARTESIAN_POINT('Ctrl Pts',(44.9380175594367,40.7187157882332,39.27051194648));
#209203=CARTESIAN_POINT('Ctrl Pts',(44.855910766329,40.6447864996547,39.3343017080178));
#209204=CARTESIAN_POINT('Ctrl Pts',(44.885804243544,40.8432146576635,39.3487519301186));
#209205=CARTESIAN_POINT('Ctrl Pts',(44.9712860523918,40.7486708738366,39.3482879463991));
#209206=CARTESIAN_POINT('Ctrl Pts',(44.9060790100825,40.6899581892257,39.4512271261641));
#209207=CARTESIAN_POINT('Ctrl Pts',(44.9493173051407,40.9001003367642,39.3978017080178));
#209208=CARTESIAN_POINT('Ctrl Pts',(45.0343891839563,40.8054891887056,39.3975673827397));
#209209=CARTESIAN_POINT('Ctrl Pts',(45.0011219300388,40.7755352187362,39.524801535518));
#209210=CARTESIAN_POINT('Ctrl Pts',(45.0161393894798,40.959952356612,39.3978017080178));
#209211=CARTESIAN_POINT('Ctrl Pts',(45.1011189764874,40.8655729637763,39.3978017080178));
#209212=CARTESIAN_POINT('Ctrl Pts',(45.1011189764874,40.8655729637763,39.5248017080178));
#209213=CARTESIAN_POINT('Origin',(44.7709311793215,40.7391658924904,39.3343017080178));
#209214=CARTESIAN_POINT('Origin',(44.7104761492018,40.6847319392788,39.1934008533551));
#209215=CARTESIAN_POINT('Origin',(49.8797426639511,35.8473027488275,39.1925554495088));
#209216=CARTESIAN_POINT('Origin',(49.9155525184341,35.8732562382978,39.116037328529));
#209217=CARTESIAN_POINT('Origin',(49.8135340601227,35.7991993820656,39.3343017080178));
#209218=CARTESIAN_POINT('Ctrl Pts',(49.7242207306179,35.7350130971383,39.2708017080178));
#209219=CARTESIAN_POINT('Ctrl Pts',(49.650303664679,35.8375861910551,39.2710850691866));
#209220=CARTESIAN_POINT('Ctrl Pts',(49.7388853330816,35.9019445403512,39.3343017080178));
#209221=CARTESIAN_POINT('Ctrl Pts',(49.6878783768803,35.7084656432346,39.3487519293517));
#209222=CARTESIAN_POINT('Ctrl Pts',(49.6137056554176,35.8109961808839,39.3492068662914));
#209223=CARTESIAN_POINT('Ctrl Pts',(49.6842702092628,35.8622643302246,39.4512271248739));
#209224=CARTESIAN_POINT('Ctrl Pts',(49.6190282456266,35.6581711379715,39.3978017080178));
#209225=CARTESIAN_POINT('Ctrl Pts',(49.5444483977887,35.7606778378455,39.3980347781197));
#209226=CARTESIAN_POINT('Ctrl Pts',(49.580802734425,35.7870908094896,39.5248015355195));
#209227=CARTESIAN_POINT('Ctrl Pts',(49.5465907136149,35.6052536882596,39.3978017080178));
#209228=CARTESIAN_POINT('Ctrl Pts',(49.4719419865738,35.7079988465452,39.3978017080178));
#209229=CARTESIAN_POINT('Ctrl Pts',(49.4719419865738,35.7079988465452,39.5248017080178));
#209230=CARTESIAN_POINT('Origin',(49.5465907136149,35.6052536882596,39.5248017080178));
#209231=CARTESIAN_POINT('Origin',(0.186621817602863,-0.256862895714048,
39.116));
#209232=CARTESIAN_POINT('Origin',(50.2402240048087,36.1092077731522,39.116));
#209233=CARTESIAN_POINT('Origin',(0.186621817602863,-0.256862895714048,
39.5248017080178));
#209234=CARTESIAN_POINT('Origin',(49.4242607783465,35.516375787839,39.5248017080178));
#209235=CARTESIAN_POINT('Ctrl Pts',(50.6762142289952,36.4252947698673,39.2875012672119));
#209236=CARTESIAN_POINT('Ctrl Pts',(50.6015094050819,36.528913661081,39.287208709576));
#209237=CARTESIAN_POINT('Ctrl Pts',(50.5139809070359,36.4650842624215,39.3549016990122));
#209238=CARTESIAN_POINT('Ctrl Pts',(50.5831238715085,36.3578045222543,39.1034939173931));
#209239=CARTESIAN_POINT('Ctrl Pts',(50.508359113622,36.461235691223,39.1031692336331));
#209240=CARTESIAN_POINT('Ctrl Pts',(50.4395906940219,36.4110366091596,39.2077507202294));
#209241=CARTESIAN_POINT('Ctrl Pts',(50.4158900112696,36.2365613423281,38.989));
#209242=CARTESIAN_POINT('Ctrl Pts',(50.3411491755186,36.3397499727017,38.9887769311176));
#209243=CARTESIAN_POINT('Ctrl Pts',(50.3059517008893,36.3139421975377,39.1161898712915));
#209244=CARTESIAN_POINT('Ctrl Pts',(50.2402240048087,36.1092077731522,38.989));
#209245=CARTESIAN_POINT('Ctrl Pts',(50.165463756031,36.2121064279398,38.989));
#209246=CARTESIAN_POINT('Ctrl Pts',(50.1655753609474,36.2119528169507,39.1161895903854));
#209247=CARTESIAN_POINT('Origin',(50.5887599058106,36.3624339277667,39.3548010137695));
#209248=CARTESIAN_POINT('Ctrl Pts',(49.4242607783465,35.516375787839,39.3978017080178));
#209249=CARTESIAN_POINT('Ctrl Pts',(49.3496120513054,35.6191209461246,39.3978017080178));
#209250=CARTESIAN_POINT('Ctrl Pts',(49.3496120513054,35.6191209461246,39.5248017080178));
#209251=CARTESIAN_POINT('Ctrl Pts',(49.3515787599206,35.4632790141025,39.3978017080178));
#209252=CARTESIAN_POINT('Ctrl Pts',(49.2767219882426,35.5661632154381,39.3975666025007));
#209253=CARTESIAN_POINT('Ctrl Pts',(49.2403833690702,35.5397616632027,39.5248015517177));
#209254=CARTESIAN_POINT('Ctrl Pts',(49.2828534857273,35.413070493059,39.3484894016716));
#209255=CARTESIAN_POINT('Ctrl Pts',(49.208148754793,35.5163418450557,39.3480259000045));
#209256=CARTESIAN_POINT('Ctrl Pts',(49.1370998624041,35.4647218031684,39.4508333188946));
#209257=CARTESIAN_POINT('Ctrl Pts',(49.2466351556017,35.3866101428254,39.2708017080178));
#209258=CARTESIAN_POINT('Ctrl Pts',(49.1720533660035,35.4901170100361,39.27051194648));
#209259=CARTESIAN_POINT('Ctrl Pts',(49.0826686475739,35.4251752107432,39.3343017080178));
#209260=CARTESIAN_POINT('Origin',(49.1573173746151,35.3224300524576,39.3343017080178));
#209261=CARTESIAN_POINT('Origin',(50.7328855645276,36.4671473482311,39.6398955068182));
#209262=CARTESIAN_POINT('Origin',(50.8770112231007,36.5718607685316,39.92499));
#209263=CARTESIAN_POINT('Origin',(49.0915036252755,35.274613564642,39.1934008539943));
#209264=CARTESIAN_POINT('Origin',(49.0553654007531,35.2482948100385,39.1160402713852));
#209265=CARTESIAN_POINT('Ctrl Pts',(50.9399462128206,36.9911673391701,40.1599502534424));
#209266=CARTESIAN_POINT('Ctrl Pts',(50.9097606317998,36.9692474126334,40.10025));
#209267=CARTESIAN_POINT('Ctrl Pts',(50.8527980281389,36.9278827595321,40.10025));
#209268=CARTESIAN_POINT('Ctrl Pts',(50.9917217504968,36.9198678602467,40.1599500538475));
#209269=CARTESIAN_POINT('Ctrl Pts',(50.9474721267427,36.9173100216912,40.100244835349));
#209270=CARTESIAN_POINT('Ctrl Pts',(50.8827604229976,36.8866065570948,40.10025));
#209271=CARTESIAN_POINT('Ctrl Pts',(51.0192553292382,36.8393772800889,40.1202442001042));
#209272=CARTESIAN_POINT('Ctrl Pts',(50.9634900918198,36.8558881875864,40.0633873868023));
#209273=CARTESIAN_POINT('Ctrl Pts',(50.8901678911828,36.8338178466774,40.0772271723542));
#209274=CARTESIAN_POINT('Ctrl Pts',(51.0231582082093,36.7103770798833,40.0045995998159));
#209275=CARTESIAN_POINT('Ctrl Pts',(50.951578055318,36.7689134067387,39.9663485808308));
#209276=CARTESIAN_POINT('Ctrl Pts',(50.8676678805082,36.7411592876123,40.0101727202462));
#209277=CARTESIAN_POINT('Ctrl Pts',(51.0012539523509,36.6614543958812,39.9304654349861));
#209278=CARTESIAN_POINT('Ctrl Pts',(50.922978448746,36.7432876021354,39.905190016294));
#209279=CARTESIAN_POINT('Ctrl Pts',(50.8391515810794,36.7013347616505,39.9671857458178));
#209280=CARTESIAN_POINT('Ctrl Pts',(50.9644637245897,36.6347241449648,39.8576902534424));
#209281=CARTESIAN_POINT('Ctrl Pts',(50.8898702560322,36.7381840359678,39.8573998014387));
#209282=CARTESIAN_POINT('Ctrl Pts',(50.8023624960595,36.6746059268172,39.92499));
#209283=CARTESIAN_POINT('Origin',(50.8527980281389,36.9278827595321,40.22725));
#209284=CARTESIAN_POINT('Origin',(0.186621817602863,-0.256862895714048,
39.116));
#209285=CARTESIAN_POINT('Origin',(48.7306271754181,35.0124214764579,39.116));
#209286=CARTESIAN_POINT('Origin',(5.53127843490691E-15,5.59796491342025E-15,
40.22725));
#209287=CARTESIAN_POINT('Origin',(50.8348823336491,36.9525415975206,40.22725));
#209288=CARTESIAN_POINT('Ctrl Pts',(48.7306271754181,35.0124214764579,38.989));
#209289=CARTESIAN_POINT('Ctrl Pts',(48.6558666212131,35.11532055163,38.989));
#209290=CARTESIAN_POINT('Ctrl Pts',(48.6559785320126,35.1151665196289,39.1161901092319));
#209291=CARTESIAN_POINT('Ctrl Pts',(48.5549543235576,34.8850714976633,38.989));
#209292=CARTESIAN_POINT('Ctrl Pts',(48.4804833899293,34.9878965398005,38.989229898976));
#209293=CARTESIAN_POINT('Ctrl Pts',(48.5155997094323,35.0131753353107,39.1161900493199));
#209294=CARTESIAN_POINT('Ctrl Pts',(48.3877151240586,34.7638382096872,39.1034966344368));
#209295=CARTESIAN_POINT('Ctrl Pts',(48.3134799021736,34.8665607873086,39.1038314102576));
#209296=CARTESIAN_POINT('Ctrl Pts',(48.3819617107294,34.9160816462013,39.20775287896));
#209297=CARTESIAN_POINT('Ctrl Pts',(48.2946219293751,34.6963546279279,39.2875012672119));
#209298=CARTESIAN_POINT('Ctrl Pts',(48.2205921440835,34.7990735417344,39.2878045257868));
#209299=CARTESIAN_POINT('Ctrl Pts',(48.3075724095164,34.8620346554122,39.3549015295898));
#209300=CARTESIAN_POINT('Origin',(48.3820909175334,34.7591950625528,39.3548010137695));
#209301=CARTESIAN_POINT('Ctrl Pts',(50.5905785208489,37.1493329797255,39.8576902534424));
#209302=CARTESIAN_POINT('Ctrl Pts',(50.6659240749088,37.0464195108247,39.8573998014387));
#209303=CARTESIAN_POINT('Ctrl Pts',(50.5784163149361,36.982841401674,39.92499));
#209304=CARTESIAN_POINT('Ctrl Pts',(50.6273860247246,37.1760745934428,39.9304984902491));
#209305=CARTESIAN_POINT('Ctrl Pts',(50.6810174228649,37.0763471615767,39.9052171569796));
#209306=CARTESIAN_POINT('Ctrl Pts',(50.6152221632648,37.0095824157642,39.9672049726605));
#209307=CARTESIAN_POINT('Ctrl Pts',(50.6805407410142,37.1816769644885,40.0043437678663));
#209308=CARTESIAN_POINT('Ctrl Pts',(50.7141678268707,37.0954833955422,39.9661628577642));
#209309=CARTESIAN_POINT('Ctrl Pts',(50.6617655220317,37.0242869695745,40.0100243556237));
#209310=CARTESIAN_POINT('Ctrl Pts',(50.8012099538928,37.1386811500604,40.1194874821986));
#209311=CARTESIAN_POINT('Ctrl Pts',(50.7999485296226,37.080309718469,40.062755148314));
#209312=CARTESIAN_POINT('Ctrl Pts',(50.7562647493206,37.0173098767917,40.0767884282375));
#209313=CARTESIAN_POINT('Ctrl Pts',(50.8700180268812,37.0873787017251,40.159950201538));
#209314=CARTESIAN_POINT('Ctrl Pts',(50.8539379904875,37.0460487315392,40.1002449453885));
#209315=CARTESIAN_POINT('Ctrl Pts',(50.804786014715,36.9939291606744,40.10025));
#209316=CARTESIAN_POINT('Ctrl Pts',(50.9219998155904,37.0158684358554,40.1599502534424));
#209317=CARTESIAN_POINT('Ctrl Pts',(50.8918248691005,36.9939338721427,40.10025));
#209318=CARTESIAN_POINT('Ctrl Pts',(50.8348823336491,36.9525415975206,40.10025));
#209319=CARTESIAN_POINT('Origin',(50.503767587895,37.0855865599597,39.92499));
#209320=CARTESIAN_POINT('Origin',(48.2379650606683,34.6544814981897,39.6398955069315));
#209321=CARTESIAN_POINT('Origin',(48.0938392037152,34.5497679336935,39.92499));
#209322=CARTESIAN_POINT('Origin',(50.3596419293387,36.9808731396133,39.6398955068266));
#209323=CARTESIAN_POINT('Origin',(50.2155162706049,36.8761597191948,39.3548010137695));
#209324=CARTESIAN_POINT('Ctrl Pts',(48.0063682005191,34.4869303039391,39.8576902534424));
#209325=CARTESIAN_POINT('Ctrl Pts',(47.9324532779042,34.5894948283128,39.8579948730703));
#209326=CARTESIAN_POINT('Ctrl Pts',(48.019190476674,34.6525130919791,39.92499));
#209327=CARTESIAN_POINT('Ctrl Pts',(47.9696093621204,34.4602241019841,39.9304020711231));
#209328=CARTESIAN_POINT('Ctrl Pts',(47.9171056031474,34.5595620694331,39.9058915297376));
#209329=CARTESIAN_POINT('Ctrl Pts',(47.9824304277187,34.6258053530815,39.9671523786031));
#209330=CARTESIAN_POINT('Ctrl Pts',(47.9167391807674,34.4546775021463,40.0043257306692));
#209331=CARTESIAN_POINT('Ctrl Pts',(47.88382973855,34.5405955452479,39.9667894847839));
#209332=CARTESIAN_POINT('Ctrl Pts',(47.9361122396534,34.6112444014583,40.01001389752));
#209333=CARTESIAN_POINT('Ctrl Pts',(47.7968564492225,34.4979061669203,40.1195533054858));
#209334=CARTESIAN_POINT('Ctrl Pts',(47.7983386612738,34.5561175928636,40.0630813209234));
#209335=CARTESIAN_POINT('Ctrl Pts',(47.8422046210396,34.618722703651,40.0768265942421));
#209336=CARTESIAN_POINT('Ctrl Pts',(47.7285944911492,34.5493265808145,40.1599502027515));
#209337=CARTESIAN_POINT('Ctrl Pts',(47.7447672725774,34.5905382782867,40.1002552791541));
#209338=CARTESIAN_POINT('Ctrl Pts',(47.794075314643,34.6424336528569,40.10025));
#209339=CARTESIAN_POINT('Ctrl Pts',(47.6769115920308,34.6205005703629,40.1599502534424));
#209340=CARTESIAN_POINT('Ctrl Pts',(47.7070975168468,34.6424200234569,40.10025));
#209341=CARTESIAN_POINT('Ctrl Pts',(47.7640607692767,34.683783783134,40.10025));
#209342=CARTESIAN_POINT('Origin',(47.7640607692768,34.683783783134,40.22725));
#209343=CARTESIAN_POINT('Ctrl Pts',(49.866980369603,36.6229335645803,38.989));
#209344=CARTESIAN_POINT('Ctrl Pts',(49.9417406248217,36.5200349009276,38.989));
#209345=CARTESIAN_POINT('Ctrl Pts',(49.9416290134548,36.5201885207951,39.116189601327));
#209346=CARTESIAN_POINT('Ctrl Pts',(50.0423873219322,36.7506494346797,38.989));
#209347=CARTESIAN_POINT('Ctrl Pts',(50.1174293675626,36.6476796282206,38.9887769275478));
#209348=CARTESIAN_POINT('Ctrl Pts',(50.0820075342354,36.6221794864672,39.1161898821852));
#209349=CARTESIAN_POINT('Ctrl Pts',(50.2093732240192,36.872231123686,39.1034967087243));
#209350=CARTESIAN_POINT('Ctrl Pts',(50.2846385388134,36.7691636147952,39.1031720232688));
#209351=CARTESIAN_POINT('Ctrl Pts',(50.215645468497,36.7192731293518,39.2077529614993));
#209352=CARTESIAN_POINT('Ctrl Pts',(50.3023253562,36.939908654648,39.2875012672119));
#209353=CARTESIAN_POINT('Ctrl Pts',(50.3777877242646,36.8368401378442,39.2872087095507));
#209354=CARTESIAN_POINT('Ctrl Pts',(50.2900345513018,36.773319961789,39.354901704823));
#209355=CARTESIAN_POINT('Origin',(49.866980369603,36.6229335645803,39.116));
#209356=CARTESIAN_POINT('Origin',(5.7121316272531E-15,5.28718575907493E-15,
40.22725));
#209357=CARTESIAN_POINT('Origin',(47.7461450747869,34.7084426211226,40.22725));
#209358=CARTESIAN_POINT('Origin',(40.5385041740537,29.8453988870283,39.116));
#209359=CARTESIAN_POINT('Origin',(49.5422481179707,36.3870656659227,39.1160373285231));
#209360=CARTESIAN_POINT('Ctrl Pts',(47.659028586094,34.645114416418,40.1599502534424));
#209361=CARTESIAN_POINT('Ctrl Pts',(47.6892031885518,34.6670494534012,40.10025));
#209362=CARTESIAN_POINT('Ctrl Pts',(47.7461450747869,34.7084426211226,40.10025));
#209363=CARTESIAN_POINT('Ctrl Pts',(47.6074854095246,34.7160192182659,40.1599500566043));
#209364=CARTESIAN_POINT('Ctrl Pts',(47.6516492793354,34.7187044685513,40.1002551305372));
#209365=CARTESIAN_POINT('Ctrl Pts',(47.7161963245886,34.7496251731987,40.10025));
#209366=CARTESIAN_POINT('Ctrl Pts',(47.5796730526558,34.7960378560832,40.1203070619043));
#209367=CARTESIAN_POINT('Ctrl Pts',(47.6353534770331,34.7797813814943,40.0637098684496));
#209368=CARTESIAN_POINT('Ctrl Pts',(47.7083584310198,34.8021505789967,40.0772636213362));
#209369=CARTESIAN_POINT('Ctrl Pts',(47.5752965616148,34.9243313177588,40.0046102245805));
#209370=CARTESIAN_POINT('Ctrl Pts',(47.6468329724886,34.8665693571818,39.9670001894015));
#209371=CARTESIAN_POINT('Ctrl Pts',(47.7301838844737,34.894378835469,40.010178881121));
#209372=CARTESIAN_POINT('Ctrl Pts',(47.5970608435776,34.9730260802971,39.9303710930184));
#209373=CARTESIAN_POINT('Ctrl Pts',(47.6753141056553,34.8923863483124,39.9058663574105));
#209374=CARTESIAN_POINT('Ctrl Pts',(47.7584998599247,34.9340521716862,39.9671344706362));
#209375=CARTESIAN_POINT('Ctrl Pts',(47.6338034047604,34.9997217530255,39.8576902534424));
#209376=CARTESIAN_POINT('Ctrl Pts',(47.7085070967808,34.8977303031696,39.8579948730703));
#209377=CARTESIAN_POINT('Ctrl Pts',(47.7952442955506,34.960748566836,39.92499));
#209378=CARTESIAN_POINT('Origin',(47.7205955685095,35.0634937251216,39.92499));
#209379=CARTESIAN_POINT('Origin',(49.5064990280466,36.3610285393793,39.1925554488851));
#209380=CARTESIAN_POINT('Origin',(49.440290424917,36.3129251734937,39.3343017080178));
#209381=CARTESIAN_POINT('Origin',(47.8647214254837,35.168207289561,39.6398955069212));
#209382=CARTESIAN_POINT('Origin',(48.0088472823277,35.2729208539809,39.3548010137695));
#209383=CARTESIAN_POINT('Ctrl Pts',(49.1733470784092,36.1189794796877,39.3978017080178));
#209384=CARTESIAN_POINT('Ctrl Pts',(49.2479958054503,36.0162343214021,39.3978017080178));
#209385=CARTESIAN_POINT('Ctrl Pts',(49.2479958054503,36.0162343214021,39.5248017080178));
#209386=CARTESIAN_POINT('Ctrl Pts',(49.246304738008,36.1716968449931,39.3978017080178));
#209387=CARTESIAN_POINT('Ctrl Pts',(49.3207474263632,36.0690914679777,39.3980355775182));
#209388=CARTESIAN_POINT('Ctrl Pts',(49.3572244778978,36.0955935972127,39.5248015517192));
#209389=CARTESIAN_POINT('Ctrl Pts',(49.3152906263885,36.2215465627858,39.3484893995498));
#209390=CARTESIAN_POINT('Ctrl Pts',(49.3898826892472,36.1193211766498,39.3489438303432));
#209391=CARTESIAN_POINT('Ctrl Pts',(49.4605079583586,36.1706334382079,39.4508333155597));
#209392=CARTESIAN_POINT('Ctrl Pts',(49.3516463037389,36.2478178023245,39.2708017080178));
#209393=CARTESIAN_POINT('Ctrl Pts',(49.4263574835555,36.1458216659119,39.2710850691866));
#209394=CARTESIAN_POINT('Ctrl Pts',(49.5149391519582,36.2101800152081,39.3343017080178));
#209395=CARTESIAN_POINT('Origin',(49.1733470784092,36.1189794796877,39.5248017080178));
#209396=CARTESIAN_POINT('Ctrl Pts',(47.9220530736691,35.2091516650522,39.2875012672119));
#209397=CARTESIAN_POINT('Ctrl Pts',(47.9968680956257,35.1070032771113,39.2878045257518));
#209398=CARTESIAN_POINT('Ctrl Pts',(48.0836260518497,35.1702703521463,39.3549015218348));
#209399=CARTESIAN_POINT('Ctrl Pts',(48.015002557561,35.2768360036059,39.1034938540228));
#209400=CARTESIAN_POINT('Ctrl Pts',(48.0897575808479,35.1744910995541,39.1038286278818));
#209401=CARTESIAN_POINT('Ctrl Pts',(48.1580164790724,35.2243181613709,39.2077506434029));
#209402=CARTESIAN_POINT('Ctrl Pts',(48.1819833392242,35.3984277477542,38.989));
#209403=CARTESIAN_POINT('Ctrl Pts',(48.2567629686452,35.2958269999271,38.9892298954605));
#209404=CARTESIAN_POINT('Ctrl Pts',(48.2916555365118,35.3214126203089,39.1161900347291));
#209405=CARTESIAN_POINT('Ctrl Pts',(48.3573835402124,35.526147267886,38.989));
#209406=CARTESIAN_POINT('Ctrl Pts',(48.4321440857833,35.4232482045976,38.989));
#209407=CARTESIAN_POINT('Ctrl Pts',(48.4320321836307,35.4234022246972,39.1161900945648));
#209408=CARTESIAN_POINT('Origin',(48.3573835402124,35.526147267886,39.116));
#209409=CARTESIAN_POINT('Origin',(39.5520252162596,29.1286799712085,39.5248017080178));
#209410=CARTESIAN_POINT('Origin',(49.0510171431408,36.0301015792671,39.5248017080178));
#209411=CARTESIAN_POINT('Origin',(39.3975469582356,29.0164449471018,39.116));
#209412=CARTESIAN_POINT('Origin',(48.6820620414863,35.7621028045846,39.116040271385));
#209413=CARTESIAN_POINT('Ctrl Pts',(48.8727133447948,35.9012693628899,39.2708017080178));
#209414=CARTESIAN_POINT('Ctrl Pts',(48.9481071848801,35.798352484893,39.27051194648));
#209415=CARTESIAN_POINT('Ctrl Pts',(48.8587224664505,35.7334106856,39.3343017080178));
#209416=CARTESIAN_POINT('Ctrl Pts',(48.9091935744939,35.927627114164,39.3487519301185));
#209417=CARTESIAN_POINT('Ctrl Pts',(48.9843245886202,35.8246659689635,39.3482879463985));
#209418=CARTESIAN_POINT('Ctrl Pts',(48.9133376106112,35.7730909105059,39.4512271261636));
#209419=CARTESIAN_POINT('Ctrl Pts',(48.978304877513,35.9775622448351,39.3978017080178));
#209420=CARTESIAN_POINT('Ctrl Pts',(49.0530211657558,35.8745769537834,39.3975673827383));
#209421=CARTESIAN_POINT('Ctrl Pts',(49.0168051108903,35.8482644497251,39.524801535518));
#209422=CARTESIAN_POINT('Ctrl Pts',(49.0510171431408,36.0301015792671,39.3978017080178));
#209423=CARTESIAN_POINT('Ctrl Pts',(49.1256658701819,35.9273564209814,39.3978017080178));
#209424=CARTESIAN_POINT('Ctrl Pts',(49.1256658701819,35.9273564209814,39.5248017080178));
#209425=CARTESIAN_POINT('Origin',(48.7840737394093,35.8361558438857,39.3343017080178));
#209426=CARTESIAN_POINT('Origin',(48.7182599907926,35.7883393569599,39.1934008533547));
#209427=CARTESIAN_POINT('Origin',(53.3535596832587,30.4370746247553,39.1925554495084));
#209428=CARTESIAN_POINT('Origin',(53.3918862459839,30.4591427892357,39.1160373285289));
#209429=CARTESIAN_POINT('Origin',(53.282685606085,30.396155456883,39.3343017080178));
#209430=CARTESIAN_POINT('Ctrl Pts',(53.1871522506179,30.3416565762229,39.2708017080178));
#209431=CARTESIAN_POINT('Ctrl Pts',(53.1243619179799,30.4513942013107,39.2710850691866));
#209432=CARTESIAN_POINT('Ctrl Pts',(53.219185606085,30.5061406831637,39.3343017080178));
#209433=CARTESIAN_POINT('Ctrl Pts',(53.1482340195352,30.3190533624392,39.3487519293517));
#209434=CARTESIAN_POINT('Ctrl Pts',(53.0851849835376,30.4287753876668,39.3492068662928));
#209435=CARTESIAN_POINT('Ctrl Pts',(53.1607219582396,30.4723866803423,39.4512271248731));
#209436=CARTESIAN_POINT('Ctrl Pts',(53.0745038491601,30.2762311741512,39.3978017080178));
#209437=CARTESIAN_POINT('Ctrl Pts',(53.0110474253454,30.3859720484841,39.3980347781174));
#209438=CARTESIAN_POINT('Ctrl Pts',(53.0499635164587,30.4084402641651,39.5248015355195));
#209439=CARTESIAN_POINT('Ctrl Pts',(52.9969317578291,30.2311753956706,39.3978017080178));
#209440=CARTESIAN_POINT('Ctrl Pts',(52.9334317578291,30.3411606219512,39.3978017080178));
#209441=CARTESIAN_POINT('Ctrl Pts',(52.9334317578291,30.3411606219512,39.5248017080178));
#209442=CARTESIAN_POINT('Origin',(52.9969317578291,30.2311753956706,39.5248017080178));
#209443=CARTESIAN_POINT('Origin',(0.158750000000002,-0.274963065701561,
39.116));
#209444=CARTESIAN_POINT('Origin',(53.739442799329,30.6598643453568,39.116));
#209445=CARTESIAN_POINT('Origin',(0.158750000000002,-0.274963065701561,
39.5248017080178));
#209446=CARTESIAN_POINT('Origin',(52.8659816883963,30.1555713378331,39.5248017080178));
#209447=CARTESIAN_POINT('Ctrl Pts',(54.2060847114746,30.9286463962971,39.2875012672119));
#209448=CARTESIAN_POINT('Ctrl Pts',(54.1426202518673,31.0395064328251,39.287208709576));
#209449=CARTESIAN_POINT('Ctrl Pts',(54.0488992551387,30.9851759176832,39.3549016990121));
#209450=CARTESIAN_POINT('Ctrl Pts',(54.1064496608385,30.8712564593342,39.1034939173931));
#209451=CARTESIAN_POINT('Ctrl Pts',(54.0429059732607,30.981936066786,39.1031692336358));
#209452=CARTESIAN_POINT('Ctrl Pts',(53.9692670413543,30.9392002377683,39.2077507202299));
#209453=CARTESIAN_POINT('Ctrl Pts',(53.927458561903,30.768158160653,38.989));
#209454=CARTESIAN_POINT('Ctrl Pts',(53.8639133132318,30.8785940576193,38.9887769311152));
#209455=CARTESIAN_POINT('Ctrl Pts',(53.8262110069739,30.8566067980793,39.1161898712914));
#209456=CARTESIAN_POINT('Ctrl Pts',(53.7394427993291,30.6598643453568,38.989));
#209457=CARTESIAN_POINT('Ctrl Pts',(53.6758479332738,30.7700138844651,38.989));
#209458=CARTESIAN_POINT('Ctrl Pts',(53.675942870086,30.7698494490828,39.1161895903852));
#209459=CARTESIAN_POINT('Origin',(54.1125387249983,30.8752713784755,39.3548010137695));
#209460=CARTESIAN_POINT('Ctrl Pts',(52.8659816883963,30.1555713378331,39.3978017080178));
#209461=CARTESIAN_POINT('Ctrl Pts',(52.8024816883963,30.2655565641137,39.3978017080178));
#209462=CARTESIAN_POINT('Ctrl Pts',(52.8024816883963,30.2655565641137,39.5248017080178));
#209463=CARTESIAN_POINT('Ctrl Pts',(52.788147705508,30.1103627734738,39.3978017080178));
#209464=CARTESIAN_POINT('Ctrl Pts',(52.7244553345199,30.2205080277001,39.3975666025026));
#209465=CARTESIAN_POINT('Ctrl Pts',(52.6855560684224,30.1980495259467,39.5248015517177));
#209466=CARTESIAN_POINT('Ctrl Pts',(52.7145506960115,30.0676130472584,39.3484894016716));
#209467=CARTESIAN_POINT('Ctrl Pts',(52.6510500011311,30.1781274387036,39.348025900004));
#209468=CARTESIAN_POINT('Ctrl Pts',(52.5749945583569,30.1342168083483,39.450833318895));
#209469=CARTESIAN_POINT('Ctrl Pts',(52.67576491394,30.045083495983,39.2708017080178));
#209470=CARTESIAN_POINT('Ctrl Pts',(52.612411104956,30.1558192615995,39.27051194648));
#209471=CARTESIAN_POINT('Ctrl Pts',(52.5167277788845,30.1005764675351,39.3343017080178));
#209472=CARTESIAN_POINT('Origin',(52.5802277788845,29.9905912412545,39.3343017080178));
#209473=CARTESIAN_POINT('Origin',(54.2668203812004,30.9643459342443,39.6398955068184));
#209474=CARTESIAN_POINT('Origin',(54.4211020372442,31.0534204898627,39.92499));
#209475=CARTESIAN_POINT('Origin',(52.5097763801592,29.949916107243,39.1934008539945));
#209476=CARTESIAN_POINT('Origin',(52.4710850656387,29.9275190026056,39.1160402713849));
#209477=CARTESIAN_POINT('Ctrl Pts',(54.5275217339724,31.4638515574734,40.1599502534424));
#209478=CARTESIAN_POINT('Ctrl Pts',(54.4952102564869,31.4452069629847,40.10025));
#209479=CARTESIAN_POINT('Ctrl Pts',(54.4342359163067,31.4100231232054,40.10025));
#209480=CARTESIAN_POINT('Ctrl Pts',(54.5715608148713,31.3875306471674,40.1599500538462));
#209481=CARTESIAN_POINT('Ctrl Pts',(54.5272862282505,31.389612165889,40.100244835349));
#209482=CARTESIAN_POINT('Ctrl Pts',(54.4597196360186,31.3658411130325,40.10025));
#209483=CARTESIAN_POINT('Ctrl Pts',(54.5905300051369,31.3046029601552,40.120244200104));
#209484=CARTESIAN_POINT('Ctrl Pts',(54.5367961153114,31.3268524737451,40.0633873868015));
#209485=CARTESIAN_POINT('Ctrl Pts',(54.4615686025423,31.3125672934286,40.0772271723538));
#209486=CARTESIAN_POINT('Ctrl Pts',(54.5809273110398,31.1759014746034,40.0045995998161));
#209487=CARTESIAN_POINT('Ctrl Pts',(54.5158579940075,31.2415992967178,39.9663485808318));
#209488=CARTESIAN_POINT('Ctrl Pts',(54.4295063924934,31.2227682191854,40.0101727202465));
#209489=CARTESIAN_POINT('Ctrl Pts',(54.5540292360084,31.1295364123882,39.930465434986));
#209490=CARTESIAN_POINT('Ctrl Pts',(54.4847364330958,31.2191033458804,39.9051900162941));
#209491=CARTESIAN_POINT('Ctrl Pts',(54.3969835118372,31.1861426211007,39.9671857458171));
#209492=CARTESIAN_POINT('Ctrl Pts',(54.5146464769142,31.1067982185528,39.8576902534424));
#209493=CARTESIAN_POINT('Ctrl Pts',(54.4512761425986,31.2174884860858,39.8573998014387));
#209494=CARTESIAN_POINT('Ctrl Pts',(54.3576020372442,31.1634057161433,39.92499));
#209495=CARTESIAN_POINT('Origin',(54.4342359163067,31.4100231232054,40.22725));
#209496=CARTESIAN_POINT('Origin',(0.158750000000002,-0.274963065701561,
39.116));
#209497=CARTESIAN_POINT('Origin',(52.123470313195,29.7268821954843,39.116));
#209498=CARTESIAN_POINT('Origin',(5.52187834149254E-15,5.61243978792563E-15,
40.22725));
#209499=CARTESIAN_POINT('Origin',(54.4189959163067,31.4364195775128,40.22725));
#209500=CARTESIAN_POINT('Ctrl Pts',(52.123470313195,29.7268821954843,38.989));
#209501=CARTESIAN_POINT('Ctrl Pts',(52.0598751873274,29.8370321846007,38.989));
#209502=CARTESIAN_POINT('Ctrl Pts',(52.0599703843398,29.8368672985386,39.1161901092325));
#209503=CARTESIAN_POINT('Ctrl Pts',(51.9354481180158,29.618592666444,38.989));
#209504=CARTESIAN_POINT('Ctrl Pts',(51.8721332875999,29.7286387544943,38.9892298989754));
#209505=CARTESIAN_POINT('Ctrl Pts',(51.9096995898764,29.7501084152007,39.1161900493205));
#209506=CARTESIAN_POINT('Ctrl Pts',(51.7564527430627,29.5155047636236,39.1034966344368));
#209507=CARTESIAN_POINT('Ctrl Pts',(51.693361622663,29.6254243098798,39.1038314102557));
#209508=CARTESIAN_POINT('Ctrl Pts',(51.7666446199927,29.667515590115,39.2077528789596));
#209509=CARTESIAN_POINT('Ctrl Pts',(51.6568155675431,29.4581217525667,39.2875012672119));
#209510=CARTESIAN_POINT('Ctrl Pts',(51.5939283753697,29.5680161811088,39.2878045257868));
#209511=CARTESIAN_POINT('Ctrl Pts',(51.6870133822667,29.6215404737376,39.3549015295901));
#209512=CARTESIAN_POINT('Origin',(51.7503740054947,29.5114749417999,39.3548010137695));
#209513=CARTESIAN_POINT('Ctrl Pts',(54.1966007261211,31.6576696180577,39.8576902534424));
#209514=CARTESIAN_POINT('Ctrl Pts',(54.2607761425987,31.5474441649277,39.8573998014387));
#209515=CARTESIAN_POINT('Ctrl Pts',(54.1671020372442,31.4933613949852,39.92499));
#209516=CARTESIAN_POINT('Ctrl Pts',(54.236001854427,31.6804173066,39.9304984902494));
#209517=CARTESIAN_POINT('Ctrl Pts',(54.2789150989591,31.5756301844099,39.9052171569793));
#209518=CARTESIAN_POINT('Ctrl Pts',(54.2065014563941,31.5161086602373,39.9672049726602));
#209519=CARTESIAN_POINT('Ctrl Pts',(54.2894509908546,31.6804328064617,40.0043437678658));
#209520=CARTESIAN_POINT('Ctrl Pts',(54.3138841827112,31.5911964272961,39.9661628577643));
#209521=CARTESIAN_POINT('Ctrl Pts',(54.2543268901843,31.5258675551963,40.0100243556234));
#209522=CARTESIAN_POINT('Ctrl Pts',(54.4049648787505,31.6250591602184,40.1194874821991));
#209523=CARTESIAN_POINT('Ctrl Pts',(54.3976088886511,31.5671393481771,40.0627551483141));
#209524=CARTESIAN_POINT('Ctrl Pts',(54.3475791360317,31.5090508246486,40.0767884282378));
#209525=CARTESIAN_POINT('Ctrl Pts',(54.4680334478299,31.5668453499333,40.1599502015398));
#209526=CARTESIAN_POINT('Ctrl Pts',(54.4477213412897,31.527422611143,40.1002449453872));
#209527=CARTESIAN_POINT('Ctrl Pts',(54.3933906465338,31.4807263372349,40.10025));
#209528=CARTESIAN_POINT('Ctrl Pts',(54.5122556166615,31.4902932482901,40.1599502534424));
#209529=CARTESIAN_POINT('Ctrl Pts',(54.4799531854483,31.4716329851982,40.10025));
#209530=CARTESIAN_POINT('Ctrl Pts',(54.4189959163067,31.4364195775128,40.10025));
#209531=CARTESIAN_POINT('Origin',(54.1036020372442,31.6033466212658,39.92499));
#209532=CARTESIAN_POINT('Origin',(51.5960921371897,29.422400263634,39.6398955069326));
#209533=CARTESIAN_POINT('Origin',(51.4418102687789,29.3333255853448,39.92499));
#209534=CARTESIAN_POINT('Origin',(53.9493203812093,31.5142720655996,39.6398955068286));
#209535=CARTESIAN_POINT('Origin',(53.7950387249983,31.4251975098786,39.3548010137695));
#209536=CARTESIAN_POINT('Ctrl Pts',(51.3482501200169,29.2799753962456,39.8576902534424));
#209537=CARTESIAN_POINT('Ctrl Pts',(51.2854610232005,29.3897042746967,39.8579948730703));
#209538=CARTESIAN_POINT('Ctrl Pts',(51.3783102687789,29.4433108116255,39.92499));
#209539=CARTESIAN_POINT('Ctrl Pts',(51.3089010921305,29.2572578385496,39.930402071123));
#209540=CARTESIAN_POINT('Ctrl Pts',(51.2670685993228,29.3615397594612,39.9058915297379));
#209541=CARTESIAN_POINT('Ctrl Pts',(51.3389598763137,29.420591851943,39.9671523786033));
#209542=CARTESIAN_POINT('Ctrl Pts',(51.255740761606,29.2572680623744,40.0043257306694));
#209543=CARTESIAN_POINT('Ctrl Pts',(51.2319924817695,29.3461554108682,39.9667894847842));
#209544=CARTESIAN_POINT('Ctrl Pts',(51.2913733902321,29.4109522357562,40.0100138975201));
#209545=CARTESIAN_POINT('Ctrl Pts',(51.141033386106,29.3127910737008,40.1195533054856));
#209546=CARTESIAN_POINT('Ctrl Pts',(51.1485922293425,29.3705286780139,40.0630813209231));
#209547=CARTESIAN_POINT('Ctrl Pts',(51.1987619028147,29.4282055900895,40.076826594242));
#209548=CARTESIAN_POINT('Ctrl Pts',(51.0785202710266,29.3710651187643,40.159950202751));
#209549=CARTESIAN_POINT('Ctrl Pts',(51.0989122516729,29.4103605382569,40.1002552791538));
#209550=CARTESIAN_POINT('Ctrl Pts',(51.1533747228781,29.4568175306711,40.10025));
#209551=CARTESIAN_POINT('Ctrl Pts',(51.0345602039891,29.4472515437729,40.1599502534424));
#209552=CARTESIAN_POINT('Ctrl Pts',(51.0668719738981,29.4658956314761,40.10025));
#209553=CARTESIAN_POINT('Ctrl Pts',(51.1278468659051,29.5010785149105,40.10025));
#209554=CARTESIAN_POINT('Origin',(51.1278468659051,29.5010785149105,40.22725));
#209555=CARTESIAN_POINT('Ctrl Pts',(53.421942799329,31.2097904767599,38.989));
#209556=CARTESIAN_POINT('Ctrl Pts',(53.4855376708633,31.0996409281618,38.989));
#209557=CARTESIAN_POINT('Ctrl Pts',(53.4854427285639,31.0998053730481,39.1161896013268));
#209558=CARTESIAN_POINT('Ctrl Pts',(53.6097387976563,31.3184716867868,38.989));
#209559=CARTESIAN_POINT('Ctrl Pts',(53.6736064794797,31.2082219299913,38.9887769275484));
#209560=CARTESIAN_POINT('Ctrl Pts',(53.6357132000302,31.1865640704867,39.116189882185));
#209561=CARTESIAN_POINT('Ctrl Pts',(53.788518680614,31.4219325588453,39.1034967087244));
#209562=CARTESIAN_POINT('Ctrl Pts',(53.8525981958187,31.3115622968575,39.1031720232692));
#209563=CARTESIAN_POINT('Ctrl Pts',(53.7787681009852,31.2691568563318,39.2077529614999));
#209564=CARTESIAN_POINT('Ctrl Pts',(53.8880358395974,31.4795232016783,39.2875012672119));
#209565=CARTESIAN_POINT('Ctrl Pts',(53.9523112232411,31.3691313396256,39.2872087095507));
#209566=CARTESIAN_POINT('Ctrl Pts',(53.8583991049523,31.3151318380577,39.3549017048228));
#209567=CARTESIAN_POINT('Origin',(53.421942799329,31.2097904767599,39.116));
#209568=CARTESIAN_POINT('Origin',(5.71547558359784E-15,5.28203651785913E-15,
40.22725));
#209569=CARTESIAN_POINT('Origin',(51.1126068659051,29.5274749692178,40.22725));
#209570=CARTESIAN_POINT('Origin',(46.508091798073,27.2180767400479,39.116));
#209571=CARTESIAN_POINT('Origin',(53.0743345559669,31.0091584503662,39.1160373285227));
#209572=CARTESIAN_POINT('Ctrl Pts',(51.0193480105331,29.4735998357331,40.1599502534424));
#209573=CARTESIAN_POINT('Ctrl Pts',(51.051650149069,29.492260605464,40.10025));
#209574=CARTESIAN_POINT('Ctrl Pts',(51.1126068659051,29.5274749692178,40.10025));
#209575=CARTESIAN_POINT('Ctrl Pts',(50.9754987628539,29.5495039426964,40.1599500566036));
#209576=CARTESIAN_POINT('Ctrl Pts',(51.0197013834521,29.547558101457,40.1002551305369));
#209577=CARTESIAN_POINT('Ctrl Pts',(51.0871269269775,29.5715624158005,40.10025));
#209578=CARTESIAN_POINT('Ctrl Pts',(50.9562029902292,29.6319914129666,40.1203070619046));
#209579=CARTESIAN_POINT('Ctrl Pts',(51.0098791271087,29.6100038038523,40.0637098684499));
#209580=CARTESIAN_POINT('Ctrl Pts',(51.0848223701587,29.6246193648989,40.0772636213361));
#209581=CARTESIAN_POINT('Ctrl Pts',(50.9652607924609,29.7600395375184,40.0046102245801));
#209582=CARTESIAN_POINT('Ctrl Pts',(51.0303675504168,29.6951164119088,39.9670001894011));
#209583=CARTESIAN_POINT('Ctrl Pts',(51.1161687394141,29.7140610042226,40.010178881121));
#209584=CARTESIAN_POINT('Ctrl Pts',(50.9919958361062,29.8061925581057,39.9303710930186));
#209585=CARTESIAN_POINT('Ctrl Pts',(51.061391271364,29.7178148857794,39.9058663574107));
#209586=CARTESIAN_POINT('Ctrl Pts',(51.1484765898563,29.7505571803532,39.9671344706363));
#209587=CARTESIAN_POINT('Ctrl Pts',(51.0313275753413,29.8289013456879,39.8576902534424));
#209588=CARTESIAN_POINT('Ctrl Pts',(51.0949610232005,29.7196599535386,39.8579948730703));
#209589=CARTESIAN_POINT('Ctrl Pts',(51.1878102687789,29.7732664904673,39.92499));
#209590=CARTESIAN_POINT('Origin',(51.1243102687789,29.883251716748,39.92499));
#209591=CARTESIAN_POINT('Origin',(53.036059682472,30.9870007553596,39.1925554488844));
#209592=CARTESIAN_POINT('Origin',(52.965185606085,30.9460815882862,39.3343017080178));
#209593=CARTESIAN_POINT('Origin',(51.2785921372027,29.9723263949817,39.6398955069224));
#209594=CARTESIAN_POINT('Origin',(51.4328740054947,30.061401073203,39.3548010137695));
#209595=CARTESIAN_POINT('Ctrl Pts',(52.6794317578291,30.7811015270737,39.3978017080178));
#209596=CARTESIAN_POINT('Ctrl Pts',(52.7429317578291,30.6711163007931,39.3978017080178));
#209597=CARTESIAN_POINT('Ctrl Pts',(52.7429317578291,30.671116300793,39.5248017080178));
#209598=CARTESIAN_POINT('Ctrl Pts',(52.7575002129179,30.8259039490945,39.3978017080178));
#209599=CARTESIAN_POINT('Ctrl Pts',(52.8208099140593,30.7160792752579,39.3980355775163));
#209600=CARTESIAN_POINT('Ctrl Pts',(52.8598573673292,30.7386233329131,39.5248015517192));
#209601=CARTESIAN_POINT('Ctrl Pts',(52.8313189037793,30.8682695960172,39.3484893995498));
#209602=CARTESIAN_POINT('Ctrl Pts',(52.8948168809868,30.7588072175363,39.3489438303427));
#209603=CARTESIAN_POINT('Ctrl Pts',(52.9704188493344,30.8024560343108,39.4508333155587));
#209604=CARTESIAN_POINT('Ctrl Pts',(52.870221513222,30.8905967158729,39.2708017080178));
#209605=CARTESIAN_POINT('Ctrl Pts',(52.9338619179799,30.7813498801525,39.2710850691866));
#209606=CARTESIAN_POINT('Ctrl Pts',(53.028685606085,30.8360963620055,39.3343017080178));
#209607=CARTESIAN_POINT('Origin',(52.6794317578291,30.7811015270737,39.5248017080178));
#209608=CARTESIAN_POINT('Ctrl Pts',(51.3398895692701,30.0070536838151,39.2875012672119));
#209609=CARTESIAN_POINT('Ctrl Pts',(51.4036173326916,29.8976445761568,39.2878045257519));
#209610=CARTESIAN_POINT('Ctrl Pts',(51.4965132298827,29.9514963916948,39.3549015218349));
#209611=CARTESIAN_POINT('Ctrl Pts',(51.439404806058,30.0646513737711,39.1034938540228));
#209612=CARTESIAN_POINT('Ctrl Pts',(51.5030523579595,29.9550530981016,39.1038286278801));
#209613=CARTESIAN_POINT('Ctrl Pts',(51.5761456730019,29.9974722043254,39.2077506434027));
#209614=CARTESIAN_POINT('Ctrl Pts',(51.6181806476922,30.1681227811157,38.989));
#209615=CARTESIAN_POINT('Ctrl Pts',(51.68182592798,30.0582674911773,38.9892298954611));
#209616=CARTESIAN_POINT('Ctrl Pts',(51.7192017762877,30.0800656843523,39.1161900347292));
#209617=CARTESIAN_POINT('Ctrl Pts',(51.805970313195,30.2768083268874,38.989));
#209618=CARTESIAN_POINT('Ctrl Pts',(51.8695654317178,30.1666583504926,38.989));
#209619=CARTESIAN_POINT('Ctrl Pts',(51.8694702420612,30.1668232238141,39.1161900945648));
#209620=CARTESIAN_POINT('Origin',(51.805970313195,30.2768083268874,39.116));
#209621=CARTESIAN_POINT('Origin',(45.3776875000007,26.5654375142628,39.5248017080178));
#209622=CARTESIAN_POINT('Origin',(52.5484816883963,30.7054974692362,39.5248017080178));
#209623=CARTESIAN_POINT('Origin',(45.2006711678738,26.4632370872583,39.116));
#209624=CARTESIAN_POINT('Origin',(52.1535342613181,30.4775331296733,39.1160402713849));
#209625=CARTESIAN_POINT('Ctrl Pts',(52.3576880233166,30.5960088312562,39.2708017080178));
#209626=CARTESIAN_POINT('Ctrl Pts',(52.421911104956,30.4857749404413,39.27051194648));
#209627=CARTESIAN_POINT('Ctrl Pts',(52.3262277788845,30.430532146377,39.3343017080178));
#209628=CARTESIAN_POINT('Ctrl Pts',(52.3967235457366,30.6184089696604,39.3487519301186));
#209629=CARTESIAN_POINT('Ctrl Pts',(52.4606806140229,30.5081585269356,39.3482879463987));
#209630=CARTESIAN_POINT('Ctrl Pts',(52.3846914485017,30.4642861617683,39.4512271261638));
#209631=CARTESIAN_POINT('Ctrl Pts',(52.4706758922783,30.6608464521626,39.3978017080178));
#209632=CARTESIAN_POINT('Ctrl Pts',(52.5342179826637,30.5506153465189,39.3975673827378));
#209633=CARTESIAN_POINT('Ctrl Pts',(52.4954499175228,30.5282325936726,39.524801535518));
#209634=CARTESIAN_POINT('Ctrl Pts',(52.5484816883963,30.7054974692362,39.3978017080178));
#209635=CARTESIAN_POINT('Ctrl Pts',(52.6119816883963,30.5955122429556,39.3978017080178));
#209636=CARTESIAN_POINT('Ctrl Pts',(52.6119816883963,30.5955122429556,39.5248017080178));
#209637=CARTESIAN_POINT('Origin',(52.2627277788845,30.5405173726576,39.3343017080178));
#209638=CARTESIAN_POINT('Origin',(52.1922763809709,30.4998422394554,39.1934008533551));
#209639=CARTESIAN_POINT('Origin',(56.2428239377263,24.693371541728,39.192555449508));
#209640=CARTESIAN_POINT('Origin',(56.2832472948506,24.7113125977902,39.1160373285274));
#209641=CARTESIAN_POINT('Origin',(56.1680608984281,24.6600848917104,39.3343017080178));
#209642=CARTESIAN_POINT('Ctrl Pts',(56.0673542004329,24.6158705164587,39.2708017080178));
#209643=CARTESIAN_POINT('Ctrl Pts',(56.0163785451201,24.7315703643328,39.2710850691866));
#209644=CARTESIAN_POINT('Ctrl Pts',(56.1164053447575,24.776105164831,39.3343017080178));
#209645=CARTESIAN_POINT('Ctrl Pts',(56.0262864882908,24.5974591883324,39.3487519293518));
#209646=CARTESIAN_POINT('Ctrl Pts',(55.9750519161942,24.7131705636675,39.3492068662925));
#209647=CARTESIAN_POINT('Ctrl Pts',(56.0547337128493,24.7486471852357,39.4512271248734));
#209648=CARTESIAN_POINT('Ctrl Pts',(55.9484840819673,24.5625784858799,39.3978017080178));
#209649=CARTESIAN_POINT('Ctrl Pts',(55.8968463240326,24.6783511906874,39.3980347781178));
#209650=CARTESIAN_POINT('Ctrl Pts',(55.9378977967849,24.6966284839295,39.5248015355195));
#209651=CARTESIAN_POINT('Ctrl Pts',(55.8666273273836,24.5258780191664,39.3978017080178));
#209652=CARTESIAN_POINT('Ctrl Pts',(55.814971773713,24.641898292287,39.3978017080178));
#209653=CARTESIAN_POINT('Ctrl Pts',(55.814971773713,24.641898292287,39.5248017080178));
#209654=CARTESIAN_POINT('Origin',(55.8666273273836,24.5258780191664,39.5248017080178));
#209655=CARTESIAN_POINT('Origin',(0.129138884176568,-0.290050682801527,
39.116));
#209656=CARTESIAN_POINT('Origin',(56.6498810128385,24.8746050278046,39.116));
#209657=CARTESIAN_POINT('Origin',(0.129138884176569,-0.290050682801527,
39.5248017080178));
#209658=CARTESIAN_POINT('Origin',(55.7284918401501,24.464376137791,39.5248017080178));
#209659=CARTESIAN_POINT('Ctrl Pts',(57.1420619865024,25.0931373005739,39.2875012672119));
#209660=CARTESIAN_POINT('Ctrl Pts',(57.0905332211014,25.2100238766572,39.287208709576));
#209661=CARTESIAN_POINT('Ctrl Pts',(56.9916465525426,25.1657875015258,39.3549016990122));
#209662=CARTESIAN_POINT('Ctrl Pts',(57.0369738651805,25.0464764504221,39.103493917393));
#209663=CARTESIAN_POINT('Ctrl Pts',(56.9853474458591,25.163191867418,39.1031692336325));
#209664=CARTESIAN_POINT('Ctrl Pts',(56.907644805189,25.1283875141298,39.2077507202298));
#209665=CARTESIAN_POINT('Ctrl Pts',(56.8481865914868,24.9626525995183,38.989));
#209666=CARTESIAN_POINT('Ctrl Pts',(56.7965331449327,25.0791258042751,38.9887769311176));
#209667=CARTESIAN_POINT('Ctrl Pts',(56.7567390814052,25.0611999573797,39.1161898712914));
#209668=CARTESIAN_POINT('Ctrl Pts',(56.6498810128385,24.8746050278046,38.989));
#209669=CARTESIAN_POINT('Ctrl Pts',(56.5981482881661,24.9907986298331,38.989));
#209670=CARTESIAN_POINT('Ctrl Pts',(56.5982255167267,24.9906251716458,39.1161895903853));
#209671=CARTESIAN_POINT('Origin',(57.0434492461382,25.0498328948958,39.3548010137695));
#209672=CARTESIAN_POINT('Ctrl Pts',(55.7284918401501,24.464376137791,39.3978017080178));
#209673=CARTESIAN_POINT('Ctrl Pts',(55.6768362864795,24.5803964109116,39.3978017080178));
#209674=CARTESIAN_POINT('Ctrl Pts',(55.6768362864795,24.5803964109116,39.5248017080178));
#209675=CARTESIAN_POINT('Ctrl Pts',(55.6463586582052,24.4275510972984,39.3978017080178));
#209676=CARTESIAN_POINT('Ctrl Pts',(55.5945285148525,24.5437506299592,39.3975666025021));
#209677=CARTESIAN_POINT('Ctrl Pts',(55.5534947903273,24.5254812387358,39.5248015517177));
#209678=CARTESIAN_POINT('Ctrl Pts',(55.5686962576402,24.3927285408614,39.3484894016716));
#209679=CARTESIAN_POINT('Ctrl Pts',(55.5170953257129,24.5092751529609,39.3480259000051));
#209680=CARTESIAN_POINT('Ctrl Pts',(55.4368666119038,24.4735550281864,39.4508333188952));
#209681=CARTESIAN_POINT('Ctrl Pts',(55.5277679687686,24.3743766270207,39.2708017080178));
#209682=CARTESIAN_POINT('Ctrl Pts',(55.4763362579877,24.4911280468219,39.27051194648));
#209683=CARTESIAN_POINT('Ctrl Pts',(55.3754026508178,24.4461895095982,39.3343017080178));
#209684=CARTESIAN_POINT('Origin',(55.4270582044884,24.3301692364776,39.3343017080178));
#209685=CARTESIAN_POINT('Origin',(57.2061965577142,25.1222926664913,39.6398955068201));
#209686=CARTESIAN_POINT('Origin',(57.3689438691199,25.1947524379609,39.92499));
#209687=CARTESIAN_POINT('Origin',(55.3527410366463,24.2970811015511,39.1934008539938));
#209688=CARTESIAN_POINT('Origin',(55.3119205422648,24.2788510342435,39.1160402713851));
#209689=CARTESIAN_POINT('Ctrl Pts',(57.5176823163891,25.5918112338787,40.1599502534424));
#209690=CARTESIAN_POINT('Ctrl Pts',(57.4835989537481,25.5766462455169,40.10025));
#209691=CARTESIAN_POINT('Ctrl Pts',(57.4192809246792,25.5480287005711,40.10025));
#209692=CARTESIAN_POINT('Ctrl Pts',(57.5535024391262,25.511305080055,40.1599500538472));
#209693=CARTESIAN_POINT('Ctrl Pts',(57.5096879712787,25.5180031505012,40.1002448353493));
#209694=CARTESIAN_POINT('Ctrl Pts',(57.4400067642829,25.5014249500138,40.10025));
#209695=CARTESIAN_POINT('Ctrl Pts',(57.5636994104965,25.4268488592814,40.1202442001043));
#209696=CARTESIAN_POINT('Ctrl Pts',(57.5125855880059,25.454593208637,40.0633873868017));
#209697=CARTESIAN_POINT('Ctrl Pts',(57.4362769714774,25.448249700338,40.0772271723539));
#209698=CARTESIAN_POINT('Ctrl Pts',(57.5406963524572,25.2998561687904,40.0045995998158));
#209699=CARTESIAN_POINT('Ctrl Pts',(57.4828507843374,25.371995687076,39.9663485808314));
#209700=CARTESIAN_POINT('Ctrl Pts',(57.3950038423349,25.3622939683639,40.0101727202464));
#209701=CARTESIAN_POINT('Ctrl Pts',(57.5090991591926,25.2565567136858,39.9304654349862));
#209702=CARTESIAN_POINT('Ctrl Pts',(57.4495482434219,25.3528760603468,39.9051900162946));
#209703=CARTESIAN_POINT('Ctrl Pts',(57.3588307079385,25.3292685758741,39.9671857458179));
#209704=CARTESIAN_POINT('Ctrl Pts',(57.4675553545144,25.2380597013423,39.8576902534424));
#209705=CARTESIAN_POINT('Ctrl Pts',(57.4161024530847,25.3547675996708,39.8573998014387));
#209706=CARTESIAN_POINT('Ctrl Pts',(57.3172883154493,25.3107727110816,39.92499));
#209707=CARTESIAN_POINT('Origin',(57.4192809246792,25.5480287005711,40.22725));
#209708=CARTESIAN_POINT('Origin',(0.129138884176568,-0.290050682801527,
39.116));
#209709=CARTESIAN_POINT('Origin',(54.9452378026832,24.115648972427,39.116));
#209710=CARTESIAN_POINT('Origin',(5.51404277916147E-15,5.62781794487312E-15,
40.22725));
#209711=CARTESIAN_POINT('Origin',(57.4068835917983,25.5758735661201,40.22725));
#209712=CARTESIAN_POINT('Ctrl Pts',(54.9452378026832,24.115648972427,38.989));
#209713=CARTESIAN_POINT('Ctrl Pts',(54.8935048666606,24.2318430491557,38.989));
#209714=CARTESIAN_POINT('Ctrl Pts',(54.8935823068869,24.2316691155597,39.1161901092321));
#209715=CARTESIAN_POINT('Ctrl Pts',(54.7469262747045,24.0276063358778,38.989));
#209716=CARTESIAN_POINT('Ctrl Pts',(54.6954612380262,24.14366778187,38.989229898976));
#209717=CARTESIAN_POINT('Ctrl Pts',(54.7350659388069,24.1610930816809,39.1161900493201));
#209718=CARTESIAN_POINT('Ctrl Pts',(54.5581358350802,23.9437932708521,39.1034966344368));
#209719=CARTESIAN_POINT('Ctrl Pts',(54.5068800556915,24.0597054841971,39.1038314102553));
#209720=CARTESIAN_POINT('Ctrl Pts',(54.5841613379366,24.0939060248992,39.2077528789598));
#209721=CARTESIAN_POINT('Ctrl Pts',(54.4530463244696,23.8971395307762,39.2875012672119));
#209722=CARTESIAN_POINT('Ctrl Pts',(54.4019907306522,24.0130054476969,39.2878045257868));
#209723=CARTESIAN_POINT('Ctrl Pts',(54.5001606201972,24.0565064959264,39.3549015295898));
#209724=CARTESIAN_POINT('Origin',(54.5516691663898,23.9404209259114,39.3548010137695));
#209725=CARTESIAN_POINT('Ctrl Pts',(57.2088336324702,25.8191582032614,39.8576902534424));
#209726=CARTESIAN_POINT('Ctrl Pts',(57.2611357920728,25.7028284190327,39.8573998014387));
#209727=CARTESIAN_POINT('Ctrl Pts',(57.1623216544374,25.6588335304434,39.92499));
#209728=CARTESIAN_POINT('Ctrl Pts',(57.2503966981987,25.8376627381923,39.9304984902489));
#209729=CARTESIAN_POINT('Ctrl Pts',(57.2821216226336,25.7289639953167,39.9052171569796));
#209730=CARTESIAN_POINT('Ctrl Pts',(57.2038829761268,25.6773378230588,39.9672049726602));
#209731=CARTESIAN_POINT('Ctrl Pts',(57.3035546548415,25.8320911970513,40.0043437678664));
#209732=CARTESIAN_POINT('Ctrl Pts',(57.3185262575354,25.7407897001102,39.9661628577643));
#209733=CARTESIAN_POINT('Ctrl Pts',(57.2524664994806,25.6820441386711,40.0100243556235));
#209734=CARTESIAN_POINT('Ctrl Pts',(57.4126476234253,25.7649464042474,40.1194874821986));
#209735=CARTESIAN_POINT('Ctrl Pts',(57.3992776612634,25.7081127933376,40.062755148314));
#209736=CARTESIAN_POINT('Ctrl Pts',(57.3434500727659,25.6555720179782,40.0767884282377));
#209737=CARTESIAN_POINT('Ctrl Pts',(57.4692856961537,25.7004590346998,40.1599502015384));
#209738=CARTESIAN_POINT('Ctrl Pts',(57.4449640631527,25.6633754510788,40.1002449453869));
#209739=CARTESIAN_POINT('Ctrl Pts',(57.3860499078766,25.6226140882765,40.10025));
#209740=CARTESIAN_POINT('Ctrl Pts',(57.5052637377735,25.6197038181291,40.1599502534424));
#209741=CARTESIAN_POINT('Ctrl Pts',(57.4711877340332,25.6045223014054,40.10025));
#209742=CARTESIAN_POINT('Ctrl Pts',(57.4068835917983,25.5758735661201,40.10025));
#209743=CARTESIAN_POINT('Origin',(57.1106661007668,25.774853803564,39.92499));
#209744=CARTESIAN_POINT('Origin',(54.3889216310757,23.8679610547579,39.639895506932));
#209745=CARTESIAN_POINT('Origin',(54.2261740956469,23.7955011834902,39.92499));
#209746=CARTESIAN_POINT('Origin',(56.9479187893705,25.7023940320462,39.6398955068271));
#209747=CARTESIAN_POINT('Origin',(56.7851714777851,25.6299342604988,39.3548010137695));
#209748=CARTESIAN_POINT('Ctrl Pts',(54.1275498658877,23.7522229508821,39.8576902534424));
#209749=CARTESIAN_POINT('Ctrl Pts',(54.0765745253539,23.8679139708562,39.8579948730703));
#209750=CARTESIAN_POINT('Ctrl Pts',(54.1745185419763,23.9115214566108,39.92499));
#209751=CARTESIAN_POINT('Ctrl Pts',(54.0860417646979,23.7337429357601,39.9304020711232));
#209752=CARTESIAN_POINT('Ctrl Pts',(54.0553388636001,23.8418262755854,39.905891529737));
#209753=CARTESIAN_POINT('Ctrl Pts',(54.1330089371354,23.8930401898198,39.9671523786031));
#209754=CARTESIAN_POINT('Ctrl Pts',(54.0331737207073,23.7393098712341,40.0043257306692));
#209755=CARTESIAN_POINT('Ctrl Pts',(54.0188467943745,23.8301926567289,39.9667894847835));
#209756=CARTESIAN_POINT('Ctrl Pts',(54.0846755205376,23.8884275227217,40.01001389752));
#209757=CARTESIAN_POINT('Ctrl Pts',(53.9248984592617,23.8065189073819,40.1195533054859));
#209758=CARTESIAN_POINT('Ctrl Pts',(53.9384511174158,23.8631501047899,40.0630813209236));
#209759=CARTESIAN_POINT('Ctrl Pts',(53.9943748351526,23.9152668978354,40.0768265942421));
#209760=CARTESIAN_POINT('Ctrl Pts',(53.8688190939463,23.8710081209819,40.1599502027519));
#209761=CARTESIAN_POINT('Ctrl Pts',(53.8932068549991,23.9079567336536,40.1002552791553));
#209762=CARTESIAN_POINT('Ctrl Pts',(53.952227053116,23.948466351383,40.10025));
#209763=CARTESIAN_POINT('Ctrl Pts',(53.8330634946841,23.9513722670358,40.1599502534424));
#209764=CARTESIAN_POINT('Ctrl Pts',(53.8671470951733,23.9665367208217,40.10025));
#209765=CARTESIAN_POINT('Ctrl Pts',(53.9314655730807,23.9951532569801,40.10025));
#209766=CARTESIAN_POINT('Origin',(53.9314655730807,23.9951532569801,40.22725));
#209767=CARTESIAN_POINT('Ctrl Pts',(56.3916032444854,25.4547063934076,38.989));
#209768=CARTESIAN_POINT('Ctrl Pts',(56.4433359736148,25.3385127813685,38.989));
#209769=CARTESIAN_POINT('Ctrl Pts',(56.4432587405905,25.3386862495813,39.116189601327));
#209770=CARTESIAN_POINT('Ctrl Pts',(56.589730756555,25.5431622092807,38.989));
#209771=CARTESIAN_POINT('Ctrl Pts',(56.6417243268786,25.426840421554,38.9887769275436));
#209772=CARTESIAN_POINT('Ctrl Pts',(56.6017747680085,25.4092621323405,39.1161898821828));
#209773=CARTESIAN_POINT('Ctrl Pts',(56.7783458705717,25.6273687254292,39.1034967087243));
#209774=CARTESIAN_POINT('Ctrl Pts',(56.8305375176146,25.5109049500354,39.1031720232718));
#209775=CARTESIAN_POINT('Ctrl Pts',(56.7526792962312,25.4764491573039,39.2077529615015));
#209776=CARTESIAN_POINT('Ctrl Pts',(56.8833377255397,25.6742415049973,39.2875012672119));
#209777=CARTESIAN_POINT('Ctrl Pts',(56.9357219102091,25.557735774037,39.2872087095508));
#209778=CARTESIAN_POINT('Ctrl Pts',(56.836679767414,25.5138485767958,39.354901704823));
#209779=CARTESIAN_POINT('Origin',(56.3916032444854,25.4547063934076,39.116));
#209780=CARTESIAN_POINT('Origin',(5.71826297912856E-15,5.27656594610754E-15,
40.22725));
#209781=CARTESIAN_POINT('Origin',(53.9190682401998,24.022998122529,40.22725));
#209782=CARTESIAN_POINT('Origin',(51.7995637473369,23.4101986852074,39.116));
#209783=CARTESIAN_POINT('Origin',(56.0249274780513,25.2915084057482,39.1160373285258));
#209784=CARTESIAN_POINT('Ctrl Pts',(53.8206887816839,23.9791663275007,40.1599502534424));
#209785=CARTESIAN_POINT('Ctrl Pts',(53.8547645473084,23.9943483786811,40.10025));
#209786=CARTESIAN_POINT('Ctrl Pts',(53.9190682401998,24.022998122529,40.10025));
#209787=CARTESIAN_POINT('Ctrl Pts',(53.7850138844278,24.0592381182994,40.159950056604));
#209788=CARTESIAN_POINT('Ctrl Pts',(53.8287709626494,24.0526825045778,40.1002551305369));
#209789=CARTESIAN_POINT('Ctrl Pts',(53.8983362760826,24.069507432326,40.10025));
#209790=CARTESIAN_POINT('Ctrl Pts',(53.7744461045709,24.1432906710366,40.1203070619048));
#209791=CARTESIAN_POINT('Ctrl Pts',(53.8255298669647,24.1158128282433,40.0637098684499));
#209792=CARTESIAN_POINT('Ctrl Pts',(53.9015903052237,24.122514621689,40.0772636213363));
#209793=CARTESIAN_POINT('Ctrl Pts',(53.796838960898,24.2696905364166,40.00461022458));
#209794=CARTESIAN_POINT('Ctrl Pts',(53.854802742671,24.1983175571248,39.9670001894012));
#209795=CARTESIAN_POINT('Ctrl Pts',(53.9421141528994,24.2081897025472,40.0101788811209));
#209796=CARTESIAN_POINT('Ctrl Pts',(53.8282518514941,24.3127961529,39.9303710930187));
#209797=CARTESIAN_POINT('Ctrl Pts',(53.8880291490201,24.2176488245059,39.90586635741));
#209798=CARTESIAN_POINT('Ctrl Pts',(53.9780599067612,24.2411088588473,39.9671344706352));
#209799=CARTESIAN_POINT('Ctrl Pts',(53.8697418420148,24.3312692531081,39.8576902534424));
#209800=CARTESIAN_POINT('Ctrl Pts',(53.921607864342,24.215974790218,39.8579948730703));
#209801=CARTESIAN_POINT('Ctrl Pts',(54.0195518809644,24.2595822759726,39.92499));
#209802=CARTESIAN_POINT('Origin',(53.9678963272938,24.3756025490932,39.92499));
#209803=CARTESIAN_POINT('Origin',(55.9845461685092,25.2734729066187,39.192555448885));
#209804=CARTESIAN_POINT('Origin',(55.909783130075,25.2401862573135,39.3343017080178));
#209805=CARTESIAN_POINT('Origin',(54.1306438627302,24.448062420301,39.6398955069211));
#209806=CARTESIAN_POINT('Origin',(54.2933913980367,24.5205222915145,39.3548010137695));
#209807=CARTESIAN_POINT('Ctrl Pts',(55.6083495590305,25.1059793847695,39.3978017080178));
#209808=CARTESIAN_POINT('Ctrl Pts',(55.6600051127011,24.9899591116489,39.3978017080178));
#209809=CARTESIAN_POINT('Ctrl Pts',(55.6600051127011,24.9899591116489,39.5248017080178));
#209810=CARTESIAN_POINT('Ctrl Pts',(55.6906734752783,25.1423759987946,39.3978017080178));
#209811=CARTESIAN_POINT('Ctrl Pts',(55.7421565548657,25.0265352902402,39.3980355775196));
#209812=CARTESIAN_POINT('Ctrl Pts',(55.7833465978042,25.0448742789053,39.5248015517192));
#209813=CARTESIAN_POINT('Ctrl Pts',(55.768516195596,25.1767934079536,39.3484893995498));
#209814=CARTESIAN_POINT('Ctrl Pts',(55.8202243900357,25.0612933298582,39.3489438303412));
#209815=CARTESIAN_POINT('Ctrl Pts',(55.899974746629,25.0968004762766,39.4508333155591));
#209816=CARTESIAN_POINT('Ctrl Pts',(55.809539512001,25.1949317875294,39.2708017080178));
#209817=CARTESIAN_POINT('Ctrl Pts',(55.8614118841082,25.0796311836947,39.2710850691866));
#209818=CARTESIAN_POINT('Ctrl Pts',(55.9614386837456,25.1241659841929,39.3343017080178));
#209819=CARTESIAN_POINT('Origin',(55.6083495590305,25.1059793847695,39.5248017080178));
#209820=CARTESIAN_POINT('Ctrl Pts',(54.1952354911875,24.4761921430385,39.2875012672119));
#209821=CARTESIAN_POINT('Ctrl Pts',(54.2471777813619,24.360721024742,39.2878045257519));
#209822=CARTESIAN_POINT('Ctrl Pts',(54.3451938326306,24.4045675690222,39.3549015218347));
#209823=CARTESIAN_POINT('Ctrl Pts',(54.3002261711149,24.5230721320487,39.1034938540228));
#209824=CARTESIAN_POINT('Ctrl Pts',(54.3520689157361,24.407421266411,39.1038286278805));
#209825=CARTESIAN_POINT('Ctrl Pts',(54.4291958219375,24.4419676644359,39.2077506434029));
#209826=CARTESIAN_POINT('Ctrl Pts',(54.4888383671844,24.6072895482032,38.989));
#209827=CARTESIAN_POINT('Ctrl Pts',(54.5406519873275,24.4913833136937,38.9892298954611));
#209828=CARTESIAN_POINT('Ctrl Pts',(54.5801016184621,24.5091552540987,39.1161900347288));
#209829=CARTESIAN_POINT('Ctrl Pts',(54.68696003433,24.6957503380301,38.989));
#209830=CARTESIAN_POINT('Ctrl Pts',(54.7386929643778,24.5795562747209,38.989));
#209831=CARTESIAN_POINT('Ctrl Pts',(54.7386155301352,24.5797301948774,39.1161900945645));
#209832=CARTESIAN_POINT('Origin',(54.68696003433,24.6957503380301,39.116));
#209833=CARTESIAN_POINT('Origin',(50.5417021396889,22.8501626153342,39.5248017080178));
#209834=CARTESIAN_POINT('Origin',(55.470214071797,25.0444775033941,39.5248017080178));
#209835=CARTESIAN_POINT('Origin',(50.3447265545032,22.7624634345041,39.116));
#209836=CARTESIAN_POINT('Origin',(55.0536014459541,24.8590452239595,39.1160402713848));
#209837=CARTESIAN_POINT('Ctrl Pts',(55.2690209153043,24.9555320242408,39.2708017080178));
#209838=CARTESIAN_POINT('Ctrl Pts',(55.3213695969759,24.8391888661838,39.27051194648));
#209839=CARTESIAN_POINT('Ctrl Pts',(55.2204359898059,24.79425032896,39.3343017080178));
#209840=CARTESIAN_POINT('Ctrl Pts',(55.3101840490931,24.9737291291706,39.3487519301186));
#209841=CARTESIAN_POINT('Ctrl Pts',(55.3622664445099,24.8573973158458,39.3482879463992));
#209842=CARTESIAN_POINT('Ctrl Pts',(55.2821076446824,24.8217083187815,39.4512271261636));
#209843=CARTESIAN_POINT('Ctrl Pts',(55.3881672017734,25.0082040095645,39.3978017080178));
#209844=CARTESIAN_POINT('Ctrl Pts',(55.4398389138645,24.8919348043911,39.3975673827383));
#209845=CARTESIAN_POINT('Ctrl Pts',(55.3989435894786,24.8737270328799,39.524801535518));
#209846=CARTESIAN_POINT('Ctrl Pts',(55.470214071797,25.0444775033941,39.3978017080178));
#209847=CARTESIAN_POINT('Ctrl Pts',(55.5218696254676,24.9284572302735,39.3978017080178));
#209848=CARTESIAN_POINT('Ctrl Pts',(55.5218696254676,24.9284572302735,39.5248017080178));
#209849=CARTESIAN_POINT('Origin',(55.1687804361353,24.9102706020807,39.3343017080178));
#209850=CARTESIAN_POINT('Origin',(55.0944632691829,24.8771824678734,39.1934008533556));
#209851=CARTESIAN_POINT('Origin',(58.5158800435652,18.6791227126689,39.1925554495078));
#209852=CARTESIAN_POINT('Origin',(58.5579573083286,18.6927400943489,39.1160373285261));
#209853=CARTESIAN_POINT('Origin',(58.4380471616457,18.6538332760097,39.3343017080178));
#209854=CARTESIAN_POINT('Ctrl Pts',(58.3332704847798,18.620387828114,39.2708017080178));
#209855=CARTESIAN_POINT('Ctrl Pts',(58.2946680067391,18.7407822670295,39.2710850691866));
#209856=CARTESIAN_POINT('Ctrl Pts',(58.3988020033601,18.7746174535792,39.3343017080178));
#209857=CARTESIAN_POINT('Ctrl Pts',(58.2905032380261,18.6063701040097,39.3487519293518));
#209858=CARTESIAN_POINT('Ctrl Pts',(58.2516444665234,18.7268030714124,39.3492068662928));
#209859=CARTESIAN_POINT('Ctrl Pts',(58.3345980746935,18.7537563325799,39.4512271248736));
#209860=CARTESIAN_POINT('Ctrl Pts',(58.2094810152003,18.5798130476652,39.3978017080178));
#209861=CARTESIAN_POINT('Ctrl Pts',(58.1702276772277,18.7003491529652,39.3980347781178));
#209862=CARTESIAN_POINT('Ctrl Pts',(58.2129647630919,18.7142352739225,39.5248015355195));
#209863=CARTESIAN_POINT('Ctrl Pts',(58.1242364370959,18.5518699907143,39.3978017080178));
#209864=CARTESIAN_POINT('Ctrl Pts',(58.0849912788103,18.6726541682838,39.3978017080178));
#209865=CARTESIAN_POINT('Ctrl Pts',(58.0849912788103,18.6726541682838,39.5248017080178));
#209866=CARTESIAN_POINT('Origin',(58.1242364370959,18.5518699907143,39.5248017080178));
#209867=CARTESIAN_POINT('Origin',(0.0981128957140474,-0.301960443923713,
39.116));
#209868=CARTESIAN_POINT('Origin',(58.9396512752216,18.8168143322219,39.116));
#209869=CARTESIAN_POINT('Origin',(0.0981128957140474,-0.301960443923713,
39.5248017080178));
#209870=CARTESIAN_POINT('Origin',(57.9804289733666,18.5051441132834,39.5248017080178));
#209871=CARTESIAN_POINT('Ctrl Pts',(59.451978872661,18.9827025415089,39.2875012672119));
#209872=CARTESIAN_POINT('Ctrl Pts',(59.4129503614028,19.1043350233602,39.287208709576));
#209873=CARTESIAN_POINT('Ctrl Pts',(59.309981444048,19.070677451222,39.3549016990123));
#209874=CARTESIAN_POINT('Ctrl Pts',(59.3425890481026,18.9472820042042,39.1034939173931));
#209875=CARTESIAN_POINT('Ctrl Pts',(59.3034455268856,19.0687544722107,39.1031692336326));
#209876=CARTESIAN_POINT('Ctrl Pts',(59.2225305038488,19.0422629184335,39.2077507202294));
#209877=CARTESIAN_POINT('Ctrl Pts',(59.1460739925267,18.8836509927317,38.989));
#209878=CARTESIAN_POINT('Ctrl Pts',(59.1068782740625,19.0048854004773,38.9887769311176));
#209879=CARTESIAN_POINT('Ctrl Pts',(59.0654284453484,18.9912173655536,39.1161898712917));
#209880=CARTESIAN_POINT('Ctrl Pts',(58.9396512752216,18.8168143322219,38.989));
#209881=CARTESIAN_POINT('Ctrl Pts',(58.9003474864893,18.9377789557519,38.989));
#209882=CARTESIAN_POINT('Ctrl Pts',(58.9004061606662,18.9375983752037,39.1161895903856));
#209883=CARTESIAN_POINT('Origin',(59.3493798002282,18.949943200105,39.3548010137695));
#209884=CARTESIAN_POINT('Ctrl Pts',(57.9804289733666,18.5051441132834,39.3978017080178));
#209885=CARTESIAN_POINT('Ctrl Pts',(57.941183815081,18.6259282908529,39.3978017080178));
#209886=CARTESIAN_POINT('Ctrl Pts',(57.941183815081,18.6259282908529,39.5248017080178));
#209887=CARTESIAN_POINT('Ctrl Pts',(57.8948964606935,18.4771060595082,39.3978017080178));
#209888=CARTESIAN_POINT('Ctrl Pts',(57.8554964068674,18.5980867642064,39.3975666025026));
#209889=CARTESIAN_POINT('Ctrl Pts',(57.8127777979911,18.5842066467856,39.5248015517177));
#209890=CARTESIAN_POINT('Ctrl Pts',(57.8140195545736,18.4505921960626,39.3484894016716));
#209891=CARTESIAN_POINT('Ctrl Pts',(57.7748837362164,18.5718941197449,39.3480259000037));
#209892=CARTESIAN_POINT('Ctrl Pts',(57.6913607539432,18.544755857716,39.4508333188947));
#209893=CARTESIAN_POINT('Ctrl Pts',(57.7713971777989,18.4366189870665,39.2708017080178));
#209894=CARTESIAN_POINT('Ctrl Pts',(57.7324510618073,18.5581069080653,39.27051194648));
#209895=CARTESIAN_POINT('Ctrl Pts',(57.6273730232608,18.5239649837,39.3343017080178));
#209896=CARTESIAN_POINT('Origin',(57.6666181815464,18.4031808061306,39.3343017080178));
#209897=CARTESIAN_POINT('Origin',(59.5188096735781,19.0049943031103,39.6398955068192));
#209898=CARTESIAN_POINT('Origin',(59.6882395467423,19.0600454060079,39.92499));
#209899=CARTESIAN_POINT('Origin',(57.5892494790285,18.3780421908169,39.1934008539945));
#209900=CARTESIAN_POINT('Origin',(57.5467470426663,18.3641788932747,39.1160402713848));
#209901=CARTESIAN_POINT('Ctrl Pts',(59.8776671349988,19.4393816709748,40.1599502534424));
#209902=CARTESIAN_POINT('Ctrl Pts',(59.8421853116555,19.4278624395259,40.10025));
#209903=CARTESIAN_POINT('Ctrl Pts',(59.7752282754839,19.4061247292246,40.10025));
#209904=CARTESIAN_POINT('Ctrl Pts',(59.9048758468125,19.3555723159016,40.1599500538468));
#209905=CARTESIAN_POINT('Ctrl Pts',(59.8620015382151,19.3668135526103,40.100244835349));
#209906=CARTESIAN_POINT('Ctrl Pts',(59.79096915834,19.357609838725,40.10025));
#209907=CARTESIAN_POINT('Ctrl Pts',(59.9061888791359,19.2705128813945,40.1202442001038));
#209908=CARTESIAN_POINT('Ctrl Pts',(59.8582551377157,19.303448093618,40.0633873868015));
#209909=CARTESIAN_POINT('Ctrl Pts',(59.7817014705984,19.3051157581411,40.0772271723538));
#209910=CARTESIAN_POINT('Ctrl Pts',(59.8700374834726,19.1466203444573,40.0045995998163));
#209911=CARTESIAN_POINT('Ctrl Pts',(59.8200494324146,19.2244111832563,39.9663485808318));
#209912=CARTESIAN_POINT('Ctrl Pts',(59.7316696194041,19.2239451174244,40.0101727202465));
#209913=CARTESIAN_POINT('Ctrl Pts',(59.8340873574359,19.1068608943535,39.9304654349858));
#209914=CARTESIAN_POINT('Ctrl Pts',(59.7849307811013,19.2088773592693,39.9051900162954));
#209915=CARTESIAN_POINT('Ctrl Pts',(59.692242551696,19.1948817636398,39.9671857458184));
#209916=CARTESIAN_POINT('Ctrl Pts',(59.7908376697914,19.0928077206404,39.8576902534424));
#209917=CARTESIAN_POINT('Ctrl Pts',(59.7518659300028,19.2142545736076,39.8573998014387));
#209918=CARTESIAN_POINT('Ctrl Pts',(59.6489943884567,19.1808295835774,39.92499));
#209919=CARTESIAN_POINT('Origin',(59.7752282754839,19.4061247292246,40.22725));
#209920=CARTESIAN_POINT('Origin',(0.0981128957140474,-0.301960443923713,
39.116));
#209921=CARTESIAN_POINT('Origin',(57.1650137687749,18.2401996527038,39.116));
#209922=CARTESIAN_POINT('Origin',(5.50785759597432E-15,5.64393089795711E-15,
40.22725));
#209923=CARTESIAN_POINT('Origin',(59.7658094374954,19.4351129318413,40.22725));
#209924=CARTESIAN_POINT('Ctrl Pts',(57.1650137687749,18.2401996527038,38.989));
#209925=CARTESIAN_POINT('Ctrl Pts',(57.12570981947,18.3611647704258,38.989));
#209926=CARTESIAN_POINT('Ctrl Pts',(57.1257686544592,18.3609836949479,39.1161901092325));
#209927=CARTESIAN_POINT('Ctrl Pts',(56.9585856505953,18.1733685221987,38.989));
#209928=CARTESIAN_POINT('Ctrl Pts',(56.9195342693658,18.2941737326422,38.989229898976));
#209929=CARTESIAN_POINT('Ctrl Pts',(56.9607434512663,18.307363756326,39.1161900493205));
#209930=CARTESIAN_POINT('Ctrl Pts',(56.7620685738646,18.109748568444,39.1034966344368));
#209931=CARTESIAN_POINT('Ctrl Pts',(56.7232097045345,18.2303834904104,39.1038314102557));
#209932=CARTESIAN_POINT('Ctrl Pts',(56.8036425617884,18.256318583299,39.2077528789596));
#209933=CARTESIAN_POINT('Ctrl Pts',(56.6526781108326,18.0743352474884,39.2875012672119));
#209934=CARTESIAN_POINT('Ctrl Pts',(56.6140134911409,18.1949032015564,39.2878045257868));
#209935=CARTESIAN_POINT('Ctrl Pts',(56.7161926934818,18.2279043987985,39.3549015295901));
#209936=CARTESIAN_POINT('Origin',(56.7552848242273,18.1070706485035,39.3548010137695));
#209937=CARTESIAN_POINT('Ctrl Pts',(59.5942745858238,19.6977666881838,39.8576902534424));
#209938=CARTESIAN_POINT('Ctrl Pts',(59.634130455146,19.5766071063161,39.8573998014387));
#209939=CARTESIAN_POINT('Ctrl Pts',(59.5312589135998,19.5431821162859,39.92499));
#209940=CARTESIAN_POINT('Ctrl Pts',(59.6375442153291,19.7118253299476,39.930498490249));
#209941=CARTESIAN_POINT('Ctrl Pts',(59.657733234755,19.6004058925617,39.9052171569797));
#209942=CARTESIAN_POINT('Ctrl Pts',(59.5745267832908,19.5572406993625,39.9672049726607));
#209943=CARTESIAN_POINT('Ctrl Pts',(59.68982858249,19.7007277907729,40.0043437678662));
#209944=CARTESIAN_POINT('Ctrl Pts',(59.6951745640082,19.6083614943627,39.9661628577643));
#209945=CARTESIAN_POINT('Ctrl Pts',(59.6233361049593,19.5568428722492,40.0100243556235));
#209946=CARTESIAN_POINT('Ctrl Pts',(59.7913053863693,19.6225475038102,40.1194874821987));
#209947=CARTESIAN_POINT('Ctrl Pts',(59.772067936249,19.5674227749664,40.062755148314));
#209948=CARTESIAN_POINT('Ctrl Pts',(59.7110541706151,19.5210053955052,40.0767884282377));
#209949=CARTESIAN_POINT('Ctrl Pts',(59.8408924241699,19.5524931121155,40.1599502015382));
#209950=CARTESIAN_POINT('Ctrl Pts',(59.8128277376098,19.5181549791671,40.100244945386));
#209951=CARTESIAN_POINT('Ctrl Pts',(59.749975597626,19.4837751174909,40.10025));
#209952=CARTESIAN_POINT('Ctrl Pts',(59.8682321556244,19.4684195516689,40.1599502534424));
#209953=CARTESIAN_POINT('Ctrl Pts',(59.8327559231849,19.4568831131876,40.10025));
#209954=CARTESIAN_POINT('Ctrl Pts',(59.7658094374954,19.4351129318413,40.10025));
#209955=CARTESIAN_POINT('Origin',(59.4920137553142,19.6639662938554,39.92499));
#209956=CARTESIAN_POINT('Origin',(56.5858547179605,18.0520194698706,39.6398955069319));
#209957=CARTESIAN_POINT('Origin',(56.4164246115666,17.9969682911404,39.92499));
#209958=CARTESIAN_POINT('Origin',(59.322583882151,19.6089151909096,39.6398955068279));
#209959=CARTESIAN_POINT('Origin',(59.1531540088002,19.5538640879525,39.3548010137695));
#209960=CARTESIAN_POINT('Ctrl Pts',(56.3138168485097,17.9642361803965,39.8576902534424));
#209961=CARTESIAN_POINT('Ctrl Pts',(56.2752137607568,18.0846218068688,39.8579948730703));
#209962=CARTESIAN_POINT('Ctrl Pts',(56.377179453281,18.1177524687099,39.92499));
#209963=CARTESIAN_POINT('Ctrl Pts',(56.2706044454597,17.9501961787615,39.9304020711229));
#209964=CARTESIAN_POINT('Ctrl Pts',(56.2513675234862,18.0608967538104,39.9058915297375));
#209965=CARTESIAN_POINT('Ctrl Pts',(56.3339654239817,18.103711379437,39.9671523786028));
#209966=CARTESIAN_POINT('Ctrl Pts',(56.2186079213555,17.961258833375,40.0043257306695));
#209967=CARTESIAN_POINT('Ctrl Pts',(56.2138593173292,18.0531413250547,39.9667894847838));
#209968=CARTESIAN_POINT('Ctrl Pts',(56.2854146278935,18.1041761987732,40.01001389752));
#209969=CARTESIAN_POINT('Ctrl Pts',(56.1179510603879,18.0394175380789,40.1195533054855));
#209970=CARTESIAN_POINT('Ctrl Pts',(56.1373490477008,18.094321865332,40.0630813209233));
#209971=CARTESIAN_POINT('Ctrl Pts',(56.1984140977479,18.1403075368572,40.076826594242));
#209972=CARTESIAN_POINT('Ctrl Pts',(56.0689198620977,18.109415362897,40.1599502027523));
#209973=CARTESIAN_POINT('Ctrl Pts',(56.0970362061477,18.1436123520178,40.1002552791541));
#209974=CARTESIAN_POINT('Ctrl Pts',(56.1599674935302,18.1777307632106,40.10025));
#209975=CARTESIAN_POINT('Ctrl Pts',(56.0417604764386,18.1930767435942,40.1599502534424));
#209976=CARTESIAN_POINT('Ctrl Pts',(56.0772424804487,18.2045954185338,40.10025));
#209977=CARTESIAN_POINT('Ctrl Pts',(56.144199857553,18.2263320786575,40.10025));
#209978=CARTESIAN_POINT('Origin',(56.144199857553,18.2263320786575,40.22725));
#209979=CARTESIAN_POINT('Ctrl Pts',(58.7434254837935,19.4207352200693,38.989));
#209980=CARTESIAN_POINT('Ctrl Pts',(58.7827292759118,19.2997705861181,38.989));
#209981=CARTESIAN_POINT('Ctrl Pts',(58.7826705983438,19.2999511771031,39.1161896013268));
#209982=CARTESIAN_POINT('Ctrl Pts',(58.949713783122,19.4879965013595,38.989));
#209983=CARTESIAN_POINT('Ctrl Pts',(58.9892635895134,19.3668771285518,38.9887769275436));
#209984=CARTESIAN_POINT('Ctrl Pts',(58.9476954469484,19.3535710010433,39.1161898821826));
#209985=CARTESIAN_POINT('Ctrl Pts',(59.1460976215391,19.552026077385,39.1034967087243));
#209986=CARTESIAN_POINT('Ctrl Pts',(59.185829577808,19.4307447900774,39.1031720232724));
#209987=CARTESIAN_POINT('Ctrl Pts',(59.1047962608428,19.4046161500175,39.207752961502));
#209988=CARTESIAN_POINT('Ctrl Pts',(59.2554138597574,19.5876674457071,39.2875012672119));
#209989=CARTESIAN_POINT('Ctrl Pts',(59.2953329133628,19.4663243070084,39.2872087095507));
#209990=CARTESIAN_POINT('Ctrl Pts',(59.1922458725045,19.4330302514106,39.3549017048229));
#209991=CARTESIAN_POINT('Origin',(58.7434254837935,19.4207352200693,39.116));
#209992=CARTESIAN_POINT('Origin',(5.72046327455653E-15,5.27083398054906E-15,
40.22725));
#209993=CARTESIAN_POINT('Origin',(56.1347810195644,18.2553202812742,40.22725));
#209994=CARTESIAN_POINT('Origin',(56.182627028633,18.588681363905,39.116));
#209995=CARTESIAN_POINT('Origin',(58.3616995707157,19.296759302446,39.1160373285272));
#209996=CARTESIAN_POINT('Ctrl Pts',(56.0323588238394,18.222012055021,40.1599502534424));
#209997=CARTESIAN_POINT('Ctrl Pts',(56.0678348753335,18.2335490499211,40.10025));
#209998=CARTESIAN_POINT('Ctrl Pts',(56.1347810195644,18.2553202812742,40.10025));
#209999=CARTESIAN_POINT('Ctrl Pts',(56.0052491386467,18.3053742463591,40.1599500566036));
#210000=CARTESIAN_POINT('Ctrl Pts',(56.048081262789,18.2942806848328,40.1002551305369));
#210001=CARTESIAN_POINT('Ctrl Pts',(56.1190241739986,18.3037418885561,40.10025));
#210002=CARTESIAN_POINT('Ctrl Pts',(56.0035251343647,18.3900709842064,40.1203070619046));
#210003=CARTESIAN_POINT('Ctrl Pts',(56.0514568378828,18.3574039607296,40.0637098684494));
#210004=CARTESIAN_POINT('Ctrl Pts',(56.1278011372726,18.3561185603235,40.0772636213363));
#210005=CARTESIAN_POINT('Ctrl Pts',(56.0390077039671,18.5134377270383,40.0046102245802));
#210006=CARTESIAN_POINT('Ctrl Pts',(56.0891934462337,18.4363968713613,39.9670001894019));
#210007=CARTESIAN_POINT('Ctrl Pts',(56.1770584756116,18.4370884086008,40.0101788811209));
#210008=CARTESIAN_POINT('Ctrl Pts',(56.0747542753111,18.5530236652636,39.9303710930186));
#210009=CARTESIAN_POINT('Ctrl Pts',(56.1242585025262,18.4521491348407,39.9058663574098));
#210010=CARTESIAN_POINT('Ctrl Pts',(56.2162483036945,18.4660698759066,39.9671344706357));
#210011=CARTESIAN_POINT('Ctrl Pts',(56.1179479440991,18.5670586829458,39.8576902534424));
#210012=CARTESIAN_POINT('Ctrl Pts',(56.1574782859,18.4469743395772,39.8579948730703));
#210013=CARTESIAN_POINT('Ctrl Pts',(56.2594439784241,18.4801050014183,39.92499));
#210014=CARTESIAN_POINT('Origin',(56.2201988201385,18.6008891789878,39.92499));
#210015=CARTESIAN_POINT('Origin',(58.3196542512034,19.283043599898,39.1925554488848));
#210016=CARTESIAN_POINT('Origin',(58.2418213702176,19.2577541638571,39.3343017080178));
#210017=CARTESIAN_POINT('Origin',(56.3896289265327,18.6559403576579,39.6398955069205));
#210018=CARTESIAN_POINT('Origin',(56.5590590327992,18.710991536351,39.3548010137695));
#210019=CARTESIAN_POINT('Ctrl Pts',(57.9280106456678,19.1557908785618,39.3978017080178));
#210020=CARTESIAN_POINT('Ctrl Pts',(57.9672558039534,19.0350067009923,39.3978017080178));
#210021=CARTESIAN_POINT('Ctrl Pts',(57.9672558039534,19.0350067009923,39.5248017080178));
#210022=CARTESIAN_POINT('Ctrl Pts',(58.0136880650213,19.1833829156704,39.3978017080178));
#210023=CARTESIAN_POINT('Ctrl Pts',(58.0527804636638,19.0627953474463,39.3980355775177));
#210024=CARTESIAN_POINT('Ctrl Pts',(58.0956618095403,19.076728341322,39.5248015517192));
#210025=CARTESIAN_POINT('Ctrl Pts',(58.0947019536607,19.2094750027313,39.3484893995498));
#210026=CARTESIAN_POINT('Ctrl Pts',(58.1340538395294,19.0892026680421,39.348943830342));
#210027=CARTESIAN_POINT('Ctrl Pts',(58.2170788227746,19.1161791203796,39.4508333155587));
#210028=CARTESIAN_POINT('Ctrl Pts',(58.1373965169896,19.2232259141432,39.2708017080178));
#210029=CARTESIAN_POINT('Ctrl Pts',(58.1769325318822,19.103134799738,39.2710850691866));
#210030=CARTESIAN_POINT('Ctrl Pts',(58.2810665285032,19.1369699862876,39.3343017080178));
#210031=CARTESIAN_POINT('Origin',(57.9280106456678,19.1557908785618,39.5248017080178));
#210032=CARTESIAN_POINT('Ctrl Pts',(56.4568070719814,18.6771643191703,39.2875012672119));
#210033=CARTESIAN_POINT('Ctrl Pts',(56.4963947983079,18.5568963159715,39.2878045257518));
#210034=CARTESIAN_POINT('Ctrl Pts',(56.5984571192852,18.5902571970793,39.3549015218345));
#210035=CARTESIAN_POINT('Ctrl Pts',(56.5661228951879,18.7128129802653,39.1034938540228));
#210036=CARTESIAN_POINT('Ctrl Pts',(56.6055928325719,18.5923766197456,39.1038286278815));
#210037=CARTESIAN_POINT('Ctrl Pts',(56.6859083114077,18.6186718120042,39.2077506434033));
#210038=CARTESIAN_POINT('Ctrl Pts',(56.7625049710037,18.7768537015935,38.989));
#210039=CARTESIAN_POINT('Ctrl Pts',(56.8019192501357,18.6561664154729,38.9892298954611));
#210040=CARTESIAN_POINT('Ctrl Pts',(56.8430104456831,18.6697173900106,39.1161900347285));
#210041=CARTESIAN_POINT('Ctrl Pts',(56.9687879773469,18.8441205405512,38.989));
#210042=CARTESIAN_POINT('Ctrl Pts',(57.0080919221123,18.7231554368006,38.989));
#210043=CARTESIAN_POINT('Ctrl Pts',(57.0080330916694,18.7233364982862,39.1161900945641));
#210044=CARTESIAN_POINT('Origin',(56.9687879773468,18.8441205405512,39.116));
#210045=CARTESIAN_POINT('Origin',(54.8193466381482,18.1457247135484,39.5248017080178));
#210046=CARTESIAN_POINT('Origin',(57.7842031819385,19.1090650011308,39.5248017080178));
#210047=CARTESIAN_POINT('Origin',(54.6058629360818,18.0763596539223,39.116));
#210048=CARTESIAN_POINT('Origin',(57.3504898524411,18.9681964166826,39.1160402713851));
#210049=CARTESIAN_POINT('Ctrl Pts',(57.5748148483578,19.0416371860871,39.2708017080178));
#210050=CARTESIAN_POINT('Ctrl Pts',(57.6147155869504,18.9204594407738,39.27051194648));
#210051=CARTESIAN_POINT('Ctrl Pts',(57.5096375484039,18.8863175164085,39.3343017080178));
#210052=CARTESIAN_POINT('Ctrl Pts',(57.617654601607,19.0554318862534,39.3487519301185));
#210053=CARTESIAN_POINT('Ctrl Pts',(57.6572916985381,18.9342932580151,39.3482879463994));
#210054=CARTESIAN_POINT('Ctrl Pts',(57.5738415009816,18.907178645177,39.4512271261639));
#210055=CARTESIAN_POINT('Ctrl Pts',(57.698814160686,19.0815664505361,39.3978017080178));
#210056=CARTESIAN_POINT('Ctrl Pts',(57.738049368389,18.9605330155748,39.3975673827378));
#210057=CARTESIAN_POINT('Ctrl Pts',(57.6954748424951,18.9466997135534,39.524801535518));
#210058=CARTESIAN_POINT('Ctrl Pts',(57.7842031819385,19.1090650011308,39.3978017080178));
#210059=CARTESIAN_POINT('Ctrl Pts',(57.8234483402241,18.9882808235613,39.3978017080178));
#210060=CARTESIAN_POINT('Ctrl Pts',(57.8234483402241,18.9882808235613,39.5248017080178));
#210061=CARTESIAN_POINT('Origin',(57.4703923901183,19.007101693978,39.3343017080178));
#210062=CARTESIAN_POINT('Origin',(57.3930236885618,18.9819630792876,39.1934008533553));
#210063=CARTESIAN_POINT('Origin',(60.1478239224126,12.4602215063114,39.192555449508));
#210064=CARTESIAN_POINT('Origin',(60.1910940874962,12.4693660187268,39.1160373285242));
#210065=CARTESIAN_POINT('Origin',(60.0677739512127,12.4432063593714,39.3343017080178));
#210066=CARTESIAN_POINT('Ctrl Pts',(59.9600752506739,12.4208962741579,39.2708017080178));
#210067=CARTESIAN_POINT('Ctrl Pts',(59.9342688867327,12.5446662374479,39.2710850691866));
#210068=CARTESIAN_POINT('Ctrl Pts',(60.0413691664789,12.5674311046646,39.3343017080178));
#210069=CARTESIAN_POINT('Ctrl Pts',(59.9160770362136,12.411425735194,39.3487519293518));
#210070=CARTESIAN_POINT('Ctrl Pts',(59.8900198101335,12.5352608058694,39.3492068662917));
#210071=CARTESIAN_POINT('Ctrl Pts',(59.9753363727294,12.5533954010678,39.4512271248731));
#210072=CARTESIAN_POINT('Ctrl Pts',(59.8327226933132,12.3934832896259,39.3978017080178));
#210073=CARTESIAN_POINT('Ctrl Pts',(59.8062838430906,12.517462176626,39.3980347781183));
#210074=CARTESIAN_POINT('Ctrl Pts',(59.8502383056106,12.5268049860494,39.5248015355195));
#210075=CARTESIAN_POINT('Ctrl Pts',(59.7450242491249,12.3746037924156,39.3978017080178));
#210076=CARTESIAN_POINT('Ctrl Pts',(59.7186194643911,12.4988285377088,39.3978017080178));
#210077=CARTESIAN_POINT('Ctrl Pts',(59.7186194643911,12.4988285377088,39.5248017080178));
#210078=CARTESIAN_POINT('Origin',(59.7450242491249,12.3746037924156,39.5248017080178));
#210079=CARTESIAN_POINT('Origin',(0.0660119618346401,-0.310561863232984,
39.116));
#210080=CARTESIAN_POINT('Origin',(60.5836663843183,12.5528626811439,39.116));
#210081=CARTESIAN_POINT('Origin',(0.0660119618346402,-0.310561863232984,
39.5248017080178));
#210082=CARTESIAN_POINT('Origin',(59.5971203935661,12.3431658574203,39.5248017080178));
#210083=CARTESIAN_POINT('Ctrl Pts',(61.1105274371643,12.6642893210134,39.2875012672119));
#210084=CARTESIAN_POINT('Ctrl Pts',(61.0844267845857,12.7893350777081,39.287208709576));
#210085=CARTESIAN_POINT('Ctrl Pts',(60.9785037674409,12.7666250679669,39.3549016990125));
#210086=CARTESIAN_POINT('Ctrl Pts',(60.9980344071778,12.6404971713765,39.103493917393));
#210087=CARTESIAN_POINT('Ctrl Pts',(60.9718026486744,12.7653958126118,39.1031692336348));
#210088=CARTESIAN_POINT('Ctrl Pts',(60.8885617651967,12.7475073053527,39.2077507202311));
#210089=CARTESIAN_POINT('Ctrl Pts',(60.7959446297927,12.5977561540106,38.989));
#210090=CARTESIAN_POINT('Ctrl Pts',(60.7696360759134,12.7224234952036,38.9887769311152));
#210091=CARTESIAN_POINT('Ctrl Pts',(60.7269846150093,12.7131630221032,39.1161898712895));
#210092=CARTESIAN_POINT('Ctrl Pts',(60.5836663843183,12.5528626811439,38.989));
#210093=CARTESIAN_POINT('Ctrl Pts',(60.5572221520605,12.6772730124465,38.989));
#210094=CARTESIAN_POINT('Ctrl Pts',(60.5572616290069,12.6770872880156,39.1161895903858));
#210095=CARTESIAN_POINT('Origin',(61.0050661295708,12.6424339620834,39.3548010137695));
#210096=CARTESIAN_POINT('Ctrl Pts',(59.5971203935661,12.3431658574203,39.3978017080178));
#210097=CARTESIAN_POINT('Ctrl Pts',(59.5707156088322,12.4673906027135,39.3978017080178));
#210098=CARTESIAN_POINT('Ctrl Pts',(59.5707156088322,12.4673906027135,39.5248017080178));
#210099=CARTESIAN_POINT('Ctrl Pts',(59.5091256622729,12.3242219811454,39.3978017080178));
#210100=CARTESIAN_POINT('Ctrl Pts',(59.4825873732131,12.4486583679636,39.3975666025021));
#210101=CARTESIAN_POINT('Ctrl Pts',(59.438651914001,12.4393195978187,39.5248015517177));
#210102=CARTESIAN_POINT('Ctrl Pts',(59.4259203549056,12.3063073021294,39.3484894016716));
#210103=CARTESIAN_POINT('Ctrl Pts',(59.399678430328,12.4310355281324,39.3480259000047));
#210104=CARTESIAN_POINT('Ctrl Pts',(59.313776274866,12.4127764613279,39.4508333188951));
#210105=CARTESIAN_POINT('Ctrl Pts',(59.3820708699072,12.2968658913796,39.2708017080178));
#210106=CARTESIAN_POINT('Ctrl Pts',(59.3560370505015,12.4217592664905,39.27051194648));
#210107=CARTESIAN_POINT('Ctrl Pts',(59.2479658375578,12.3987880210516,39.3343017080178));
#210108=CARTESIAN_POINT('Origin',(59.2743706222916,12.2745632757584,39.3343017080178));
#210109=CARTESIAN_POINT('Origin',(61.1793222555451,12.6794732450924,39.6398955068193));
#210110=CARTESIAN_POINT('Origin',(61.3535783813234,12.7165125280158,39.92499));
#210111=CARTESIAN_POINT('Origin',(59.1947980527947,12.2576496039896,39.193400853994));
#210112=CARTESIAN_POINT('Origin',(59.1510793400373,12.2483049653993,39.1160402713848));
#210113=CARTESIAN_POINT('Ctrl Pts',(61.5816197022699,13.0739701745317,40.1599502534424));
#210114=CARTESIAN_POINT('Ctrl Pts',(61.5451281645061,13.0662229071059,40.10025));
#210115=CARTESIAN_POINT('Ctrl Pts',(61.4762657165317,13.0516031943521,40.10025));
#210116=CARTESIAN_POINT('Ctrl Pts',(61.5999188988204,12.9877758510413,40.1599500538472));
#210117=CARTESIAN_POINT('Ctrl Pts',(61.5584544893695,13.0034370926703,40.100244835349));
#210118=CARTESIAN_POINT('Ctrl Pts',(61.4868491822358,13.0017087032037,40.10025));
#210119=CARTESIAN_POINT('Ctrl Pts',(61.5923336062397,12.9030451317653,40.1202442001039));
#210120=CARTESIAN_POINT('Ctrl Pts',(61.5481051179915,12.9408103617794,40.0633873868015));
#210121=CARTESIAN_POINT('Ctrl Pts',(61.4721451382827,12.9504709278431,40.0772271723536));
#210122=CARTESIAN_POINT('Ctrl Pts',(61.543429955208,12.7836101409423,40.0045995998162));
#210123=CARTESIAN_POINT('Ctrl Pts',(61.50184710076,12.8662000075457,39.9663485808317));
#210124=CARTESIAN_POINT('Ctrl Pts',(61.4139027244672,12.8749747009092,40.0101727202467));
#210125=CARTESIAN_POINT('Ctrl Pts',(61.5035207735038,12.7478263086943,39.9304654349859));
#210126=CARTESIAN_POINT('Ctrl Pts',(61.4652971063442,12.8544221781238,39.9051900162943));
#210127=CARTESIAN_POINT('Ctrl Pts',(61.3716536946539,12.8501918100163,39.9671857458174));
#210128=CARTESIAN_POINT('Ctrl Pts',(61.459039055521,12.7383709431243,39.8576902534424));
#210129=CARTESIAN_POINT('Ctrl Pts',(61.43297545991,12.8632261535947,39.8573998014387));
#210130=CARTESIAN_POINT('Ctrl Pts',(61.3271735965895,12.840737273309,39.92499));
#210131=CARTESIAN_POINT('Origin',(61.4762657165317,13.0516031943521,40.22725));
#210132=CARTESIAN_POINT('Origin',(0.0660119618346401,-0.310561863232984,
39.116));
#210133=CARTESIAN_POINT('Origin',(58.7584778814678,12.1649068885784,39.116));
#210134=CARTESIAN_POINT('Origin',(5.5033905580924E-15,5.66060211029175E-15,
40.22725));
#210135=CARTESIAN_POINT('Origin',(61.4699285681956,13.0814171332224,40.22725));
#210136=CARTESIAN_POINT('Ctrl Pts',(58.7584778814678,12.1649068885784,38.989));
#210137=CARTESIAN_POINT('Ctrl Pts',(58.7320335411742,12.2893177281492,38.989));
#210138=CARTESIAN_POINT('Ctrl Pts',(58.7320731263176,12.2891314946914,39.1161901092317));
#210139=CARTESIAN_POINT('Ctrl Pts',(58.5461948427484,12.1200194799672,38.989));
#210140=CARTESIAN_POINT('Ctrl Pts',(58.5199849720703,12.2442448876943,38.989229898976));
#210141=CARTESIAN_POINT('Ctrl Pts',(58.5623471386663,12.253055122593,39.1161900493197));
#210142=CARTESIAN_POINT('Ctrl Pts',(58.3441042111266,12.0772896710131,39.1034966344368));
#210143=CARTESIAN_POINT('Ctrl Pts',(58.3180679977636,12.2013256001478,39.103831410257));
#210144=CARTESIAN_POINT('Ctrl Pts',(58.4007711908128,12.2187110949216,39.2077528789602));
#210145=CARTESIAN_POINT('Ctrl Pts',(58.2316113004783,12.0535047649314,39.2875012672119));
#210146=CARTESIAN_POINT('Ctrl Pts',(58.205761272577,12.1774537884102,39.2878045257868));
#210147=CARTESIAN_POINT('Ctrl Pts',(58.3108302909892,12.1995935666429,39.3549015295897));
#210148=CARTESIAN_POINT('Origin',(58.3370777047236,12.0753355159225,39.3548010137695));
#210149=CARTESIAN_POINT('Ctrl Pts',(61.3267881959115,13.3605623192479,39.8576902534424));
#210150=CARTESIAN_POINT('Ctrl Pts',(61.3537611057085,13.2359003894743,39.8573998014387));
#210151=CARTESIAN_POINT('Ctrl Pts',(61.2479592423879,13.2134115091886,39.92499));
#210152=CARTESIAN_POINT('Ctrl Pts',(61.3712903180781,13.3700210384225,39.9304984902488));
#210153=CARTESIAN_POINT('Ctrl Pts',(61.3797222373778,13.257101641197,39.9052171569784));
#210154=CARTESIAN_POINT('Ctrl Pts',(61.2924596082479,13.2228703539488,39.9672049726591));
#210155=CARTESIAN_POINT('Ctrl Pts',(61.4221282572894,13.3535190881763,40.0043437678665));
#210156=CARTESIAN_POINT('Ctrl Pts',(61.4177900459395,13.2610999767695,39.9661628577646));
#210157=CARTESIAN_POINT('Ctrl Pts',(61.3409599630866,13.2173727427865,40.0100243556236));
#210158=CARTESIAN_POINT('Ctrl Pts',(61.5148770953648,13.2651598666395,40.1194874821984));
#210159=CARTESIAN_POINT('Ctrl Pts',(61.4899829268155,13.2123479779263,40.0627551483138));
#210160=CARTESIAN_POINT('Ctrl Pts',(61.4244514636298,13.1725625528863,40.0767884282376));
#210161=CARTESIAN_POINT('Ctrl Pts',(61.5568698122757,13.1903059833727,40.1599502015389));
#210162=CARTESIAN_POINT('Ctrl Pts',(61.5253695547392,13.1590895168683,40.1002449453881));
#210163=CARTESIAN_POINT('Ctrl Pts',(61.4592680512448,13.131467829277,40.10025));
#210164=CARTESIAN_POINT('Ctrl Pts',(61.5752716937453,13.103835206572,40.1599502534424));
#210165=CARTESIAN_POINT('Ctrl Pts',(61.5387839176329,13.0960702419672,40.10025));
#210166=CARTESIAN_POINT('Ctrl Pts',(61.4699285681956,13.0814171332224,40.10025));
#210167=CARTESIAN_POINT('Origin',(61.2215544576541,13.3376362544818,39.92499));
#210168=CARTESIAN_POINT('Origin',(58.1628213392008,12.0382961820508,39.6398955069312));
#210169=CARTESIAN_POINT('Origin',(57.9885649735461,12.0012568480852,39.92499));
#210170=CARTESIAN_POINT('Origin',(61.0472983318742,13.3005969715109,39.6398955068265));
#210171=CARTESIAN_POINT('Origin',(60.8730422059015,13.2635576885494,39.3548010137695));
#210172=CARTESIAN_POINT('Ctrl Pts',(57.8830978693157,11.9794294790605,39.8576902534424));
#210173=CARTESIAN_POINT('Ctrl Pts',(57.8572899778513,12.1031907419149,39.8579948730703));
#210174=CARTESIAN_POINT('Ctrl Pts',(57.9621601888122,12.1254815933784,39.92499));
#210175=CARTESIAN_POINT('Ctrl Pts',(57.8386546085357,11.9699833161083,39.930402071123));
#210176=CARTESIAN_POINT('Ctrl Pts',(57.8310944294252,12.0820882677175,39.9058915297371));
#210177=CARTESIAN_POINT('Ctrl Pts',(57.9177151970031,12.116034518736,39.967152378603));
#210178=CARTESIAN_POINT('Ctrl Pts',(57.7880992891176,11.9864204851022,40.0043257306694));
#210179=CARTESIAN_POINT('Ctrl Pts',(57.7929810340972,12.07829599916,39.9667894847842));
#210180=CARTESIAN_POINT('Ctrl Pts',(57.8694789541063,12.1215717318489,40.0100138975202));
#210181=CARTESIAN_POINT('Ctrl Pts',(57.6961636462599,12.0746725352383,40.1195533054856));
#210182=CARTESIAN_POINT('Ctrl Pts',(57.7211944343233,12.1272484490378,40.0630813209231));
#210183=CARTESIAN_POINT('Ctrl Pts',(57.7867317752137,12.1665991704017,40.0768265942418));
#210184=CARTESIAN_POINT('Ctrl Pts',(57.6547178110652,12.1494120604575,40.1599502027512));
#210185=CARTESIAN_POINT('Ctrl Pts',(57.6862546895629,12.1804827566577,40.1002552791553));
#210186=CARTESIAN_POINT('Ctrl Pts',(57.7524075778595,12.2078361528628,40.10025));
#210187=CARTESIAN_POINT('Ctrl Pts',(57.6364522029208,12.2354540642037,40.1599502534424));
#210188=CARTESIAN_POINT('Ctrl Pts',(57.6729438621908,12.243200759284,40.10025));
#210189=CARTESIAN_POINT('Ctrl Pts',(57.7418065394567,12.257819391976,40.10025));
#210190=CARTESIAN_POINT('Origin',(57.7418065394567,12.257819391976,40.22725));
#210191=CARTESIAN_POINT('Ctrl Pts',(60.4516424606491,13.1739864076099,38.989));
#210192=CARTESIAN_POINT('Ctrl Pts',(60.4780866951852,13.0495760655893,38.989));
#210193=CARTESIAN_POINT('Ctrl Pts',(60.4780472159571,13.0497618007542,39.116189601327));
#210194=CARTESIAN_POINT('Ctrl Pts',(60.6638314094603,13.2193162256446,38.989));
#210195=CARTESIAN_POINT('Ctrl Pts',(60.6905041359625,13.09472627695,38.9887769275436));
#210196=CARTESIAN_POINT('Ctrl Pts',(60.6477728389701,13.0858380958627,39.1161898821828));
#210197=CARTESIAN_POINT('Ctrl Pts',(60.8658323498481,13.2624673401125,39.1034967087243));
#210198=CARTESIAN_POINT('Ctrl Pts',(60.8926693037173,13.1376973240579,39.1031720232725));
#210199=CARTESIAN_POINT('Ctrl Pts',(60.8093487091504,13.1201821075159,39.2077529615018));
#210200=CARTESIAN_POINT('Ctrl Pts',(60.978275279735,13.2864868028988,39.2875012672119));
#210201=CARTESIAN_POINT('Ctrl Pts',(61.0052918407718,13.1616357172815,39.2872087095507));
#210202=CARTESIAN_POINT('Ctrl Pts',(60.8992893450416,13.1392995799678,39.354901704823));
#210203=CARTESIAN_POINT('Origin',(60.4516424606491,13.1739864076099,39.116));
#210204=CARTESIAN_POINT('Origin',(5.72205236298458E-15,5.26490342179783E-15,
40.22725));
#210205=CARTESIAN_POINT('Origin',(57.7354693911206,12.2876333308464,40.22725));
#210206=CARTESIAN_POINT('Origin',(59.4667368016504,12.9646382471638,39.116));
#210207=CARTESIAN_POINT('Origin',(60.0590486699124,13.090590866118,39.116037328527));
#210208=CARTESIAN_POINT('Ctrl Pts',(57.6301266171959,12.2652136052653,40.1599502534424));
#210209=CARTESIAN_POINT('Ctrl Pts',(57.6666142715157,12.2729791421547,40.10025));
#210210=CARTESIAN_POINT('Ctrl Pts',(57.7354693911206,12.2876333308464,40.10025));
#210211=CARTESIAN_POINT('Ctrl Pts',(57.6118791634503,12.3509528635298,40.1599500566038));
#210212=CARTESIAN_POINT('Ctrl Pts',(57.653317055794,12.3354428975785,40.1002551305378));
#210213=CARTESIAN_POINT('Ctrl Pts',(57.7248602994011,12.33743671835,40.10025));
#210214=CARTESIAN_POINT('Ctrl Pts',(57.6190178232952,12.4353658313036,40.1203070619047));
#210215=CARTESIAN_POINT('Ctrl Pts',(57.6632723181622,12.3978675338891,40.0637098684499));
#210216=CARTESIAN_POINT('Ctrl Pts',(57.7390640345626,12.388609022746,40.0772636213362));
#210217=CARTESIAN_POINT('Ctrl Pts',(57.6672013517154,12.5543478197367,40.0046102245801));
#210218=CARTESIAN_POINT('Ctrl Pts',(57.7090592089827,12.4724831634108,39.9670001894012));
#210219=CARTESIAN_POINT('Ctrl Pts',(57.7965151898612,12.4639865158414,40.0101788811209));
#210220=CARTESIAN_POINT('Ctrl Pts',(57.706889956891,12.5899803678805,39.9303710930187));
#210221=CARTESIAN_POINT('Ctrl Pts',(57.7455787351226,12.4844838378931,39.9058663574112));
#210222=CARTESIAN_POINT('Ctrl Pts',(57.8385197202051,12.4887127671316,39.9671344706359));
#210223=CARTESIAN_POINT('Ctrl Pts',(57.7513140650722,12.5994235324464,39.8576902534424));
#210224=CARTESIAN_POINT('Ctrl Pts',(57.7780756236497,12.4758649777945,39.8579948730703));
#210225=CARTESIAN_POINT('Ctrl Pts',(57.8829458346107,12.498155829258,39.92499));
#210226=CARTESIAN_POINT('Origin',(57.8565410498768,12.6223805745512,39.92499));
#210227=CARTESIAN_POINT('Origin',(60.0157999977491,13.0813452322602,39.1925554488844));
#210228=CARTESIAN_POINT('Origin',(59.9357500275435,13.0643300858374,39.3343017080178));
#210229=CARTESIAN_POINT('Origin',(58.0307974155297,12.6594199084523,39.6398955069217));
#210230=CARTESIAN_POINT('Origin',(58.2050537810543,12.6964592423885,39.3548010137695));
#210231=CARTESIAN_POINT('Ctrl Pts',(59.6130003254557,12.9957275188816,39.3978017080178));
#210232=CARTESIAN_POINT('Ctrl Pts',(59.6394051101895,12.8715027735884,39.3978017080178));
#210233=CARTESIAN_POINT('Ctrl Pts',(59.6394051101895,12.8715027735884,39.5248017080178));
#210234=CARTESIAN_POINT('Ctrl Pts',(59.7010925481784,13.0142126749437,39.3978017080178));
#210235=CARTESIAN_POINT('Ctrl Pts',(59.7273659613746,12.8901994296783,39.3980355775196));
#210236=CARTESIAN_POINT('Ctrl Pts',(59.7714687931893,12.8995737759683,39.5248015517192));
#210237=CARTESIAN_POINT('Ctrl Pts',(59.7843900000234,13.0316935695375,39.3484893995498));
#210238=CARTESIAN_POINT('Ctrl Pts',(59.8109544298265,12.9079667071261,39.348943830341));
#210239=CARTESIAN_POINT('Ctrl Pts',(59.896344400635,12.9261169057234,39.4508333155594));
#210240=CARTESIAN_POINT('Ctrl Pts',(59.8282880397057,13.0409063549231,39.2708017080178));
#210241=CARTESIAN_POINT('Ctrl Pts',(59.8550545325311,12.9173404733275,39.2710850691866));
#210242=CARTESIAN_POINT('Ctrl Pts',(59.9621548122773,12.9401053405442,39.3343017080178));
#210243=CARTESIAN_POINT('Origin',(59.6130003254557,12.9957275188816,39.5248017080178));
#210244=CARTESIAN_POINT('Ctrl Pts',(58.0998260601482,12.6735055745733,39.2875012672119));
#210245=CARTESIAN_POINT('Ctrl Pts',(58.1266254912132,12.5497583678823,39.2878045257519));
#210246=CARTESIAN_POINT('Ctrl Pts',(58.2316158657529,12.572268077024,39.3549015218347));
#210247=CARTESIAN_POINT('Ctrl Pts',(58.2122693395992,12.6975323335618,39.1034938540228));
#210248=CARTESIAN_POINT('Ctrl Pts',(58.2389340288488,12.5736300041238,39.1038286278811));
#210249=CARTESIAN_POINT('Ctrl Pts',(58.3215581271254,12.5913858949914,39.2077506434031));
#210250=CARTESIAN_POINT('Ctrl Pts',(58.4142696920429,12.7406947165192,38.989));
#210251=CARTESIAN_POINT('Ctrl Pts',(58.4408527990764,12.616548653953,38.9892298954611));
#210252=CARTESIAN_POINT('Ctrl Pts',(58.4831353553,12.6257301953092,39.1161900347289));
#210253=CARTESIAN_POINT('Ctrl Pts',(58.6264539577985,12.7860306150444,38.989));
#210254=CARTESIAN_POINT('Ctrl Pts',(58.6528982950381,12.6616197898418,38.989));
#210255=CARTESIAN_POINT('Ctrl Pts',(58.6528587129533,12.6618060089099,39.1161900945646));
#210256=CARTESIAN_POINT('Origin',(58.6264539577985,12.7860306150444,39.116));
#210257=CARTESIAN_POINT('Origin',(58.0246834617332,12.6581203474863,39.5248017080178));
#210258=CARTESIAN_POINT('Origin',(59.4650964698968,12.9642895838863,39.5248017080178));
#210259=CARTESIAN_POINT('Origin',(57.7988642628865,12.6101209950203,39.116));
#210260=CARTESIAN_POINT('Origin',(59.0190342907437,12.8695280801138,39.1160402713848));
#210261=CARTESIAN_POINT('Ctrl Pts',(59.2498070616281,12.9191181862038,39.2708017080178));
#210262=CARTESIAN_POINT('Ctrl Pts',(59.2768226963,12.7944335023701,39.27051194648));
#210263=CARTESIAN_POINT('Ctrl Pts',(59.1687514833562,12.7714622569312,39.3343017080178));
#210264=CARTESIAN_POINT('Ctrl Pts',(59.2938540730361,12.9283593439861,39.3487519301186));
#210265=CARTESIAN_POINT('Ctrl Pts',(59.3206115991492,12.8037411209992,39.3482879463993));
#210266=CARTESIAN_POINT('Ctrl Pts',(59.2347843016964,12.785497965755,39.4512271261639));
#210267=CARTESIAN_POINT('Ctrl Pts',(59.3773008374014,12.9458672564002,39.3978017080178));
#210268=CARTESIAN_POINT('Ctrl Pts',(59.4036696715717,12.8213956592928,39.3975673827383));
#210269=CARTESIAN_POINT('Ctrl Pts',(59.359882399582,12.812088387313,39.524801535518));
#210270=CARTESIAN_POINT('Ctrl Pts',(59.4650964698968,12.9642895838863,39.3978017080178));
#210271=CARTESIAN_POINT('Ctrl Pts',(59.4915012546307,12.8400648385931,39.3978017080178));
#210272=CARTESIAN_POINT('Ctrl Pts',(59.4915012546306,12.8400648385931,39.5248017080178));
#210273=CARTESIAN_POINT('Origin',(59.1423466986224,12.8956870022244,39.3343017080178));
#210274=CARTESIAN_POINT('Origin',(59.0627741301484,12.8787733309738,39.193400853354));
#210275=CARTESIAN_POINT('Origin',(61.1207756556245,6.10480350566312,39.1925554495082));
#210276=CARTESIAN_POINT('Origin',(61.1647646440471,6.10937495961979,39.1160373285255));
#210277=CARTESIAN_POINT('Origin',(61.0393856393805,6.09624906995156,39.3343017080178));
#210278=CARTESIAN_POINT('Ctrl Pts',(60.9299448846691,6.08531878138238,39.2708017080178));
#210279=CARTESIAN_POINT('Ctrl Pts',(60.9172173747511,6.21110821942853,39.2710850691866));
#210280=CARTESIAN_POINT('Ctrl Pts',(61.0261105245455,6.22255335066333,39.3343017080178));
#210281=CARTESIAN_POINT('Ctrl Pts',(60.8851977561471,6.08049918876568,39.3487519293518));
#210282=CARTESIAN_POINT('Ctrl Pts',(60.8722275639201,6.20637959976494,39.3492068662932));
#210283=CARTESIAN_POINT('Ctrl Pts',(60.9589723348255,6.21549684257569,39.4512271248742));
#210284=CARTESIAN_POINT('Ctrl Pts',(60.800424540796,6.07136793516269,39.3978017080178));
#210285=CARTESIAN_POINT('Ctrl Pts',(60.7870898478928,6.19743126523103,39.3980347781183));
#210286=CARTESIAN_POINT('Ctrl Pts',(60.8317801127809,6.20212840134595,39.5248015355195));
#210287=CARTESIAN_POINT('Ctrl Pts',(60.7112330730305,6.06175884541488,39.3978017080178));
#210288=CARTESIAN_POINT('Ctrl Pts',(60.6979579581955,6.18806312612664,39.3978017080178));
#210289=CARTESIAN_POINT('Ctrl Pts',(60.6979579581955,6.18806312612664,39.5248017080178));
#210290=CARTESIAN_POINT('Origin',(60.7112330730305,6.06175884541488,39.5248017080178));
#210291=CARTESIAN_POINT('Origin',(0.0331877870874813,-0.315760701779427,
39.116));
#210292=CARTESIAN_POINT('Origin',(61.5639141665613,6.15137923967592,39.116));
#210293=CARTESIAN_POINT('Origin',(0.0331877870874813,-0.315760701779427,
39.5248017080178));
#210294=CARTESIAN_POINT('Origin',(60.5608532912344,6.04595329344979,39.5248017080178));
#210295=CARTESIAN_POINT('Ctrl Pts',(62.099536274866,6.20712349654379,39.2875012672119));
#210296=CARTESIAN_POINT('Ctrl Pts',(62.0866494451786,6.33421250060427,39.287208709576));
#210297=CARTESIAN_POINT('Ctrl Pts',(61.9789328429853,6.32269886887908,39.3549016990127));
#210298=CARTESIAN_POINT('Ctrl Pts',(61.9851725366286,6.19522040634589,39.103493917393));
#210299=CARTESIAN_POINT('Ctrl Pts',(61.9721399414775,6.32217680516156,39.1031692336342));
#210300=CARTESIAN_POINT('Ctrl Pts',(61.8874852020945,6.31308733464671,39.207750720231));
#210301=CARTESIAN_POINT('Ctrl Pts',(61.7797221753254,6.17383766261649,38.989));
#210302=CARTESIAN_POINT('Ctrl Pts',(61.7665890280501,6.30057205577822,38.9887769311152));
#210303=CARTESIAN_POINT('Ctrl Pts',(61.7232032332894,6.29582060418239,39.1161898712899));
#210304=CARTESIAN_POINT('Ctrl Pts',(61.5639141665613,6.15137923967592,38.989));
#210305=CARTESIAN_POINT('Ctrl Pts',(61.5506192193202,6.27787221312686,38.989));
#210306=CARTESIAN_POINT('Ctrl Pts',(61.5506390665185,6.277683379649,39.1161895903862));
#210307=CARTESIAN_POINT('Origin',(61.992368188267,6.19641157197379,39.3548010137695));
#210308=CARTESIAN_POINT('Ctrl Pts',(60.5608532912344,6.04595329344978,39.3978017080178));
#210309=CARTESIAN_POINT('Ctrl Pts',(60.5475781763994,6.17225757416155,39.3978017080178));
#210310=CARTESIAN_POINT('Ctrl Pts',(60.5475781763994,6.17225757416155,39.5248017080178));
#210311=CARTESIAN_POINT('Ctrl Pts',(60.4713604300109,6.03631114774949,39.3978017080178));
#210312=CARTESIAN_POINT('Ctrl Pts',(60.457974664765,6.16283986559435,39.3975666025021));
#210313=CARTESIAN_POINT('Ctrl Pts',(60.413303721302,6.15814476024283,39.5248015517177));
#210314=CARTESIAN_POINT('Ctrl Pts',(60.3867383361559,6.02719193013296,39.3484894016716));
#210315=CARTESIAN_POINT('Ctrl Pts',(60.3736778173756,6.15397990991407,39.348025900005));
#210316=CARTESIAN_POINT('Ctrl Pts',(60.2863376507176,6.14480008848936,39.4508333188949));
#210317=CARTESIAN_POINT('Ctrl Pts',(60.3421421670676,6.02238575970194,39.2708017080178));
#210318=CARTESIAN_POINT('Ctrl Pts',(60.3293058762212,6.14931623097165,39.27051194648));
#210319=CARTESIAN_POINT('Ctrl Pts',(60.2194255397046,6.13776734223133,39.3343017080178));
#210320=CARTESIAN_POINT('Origin',(60.2327006545396,6.01146306151956,39.3343017080178));
#210321=CARTESIAN_POINT('Origin',(62.1695413802847,6.21503322485266,39.6398955068188));
#210322=CARTESIAN_POINT('Origin',(62.346714572097,6.2336548776654,39.92499));
#210323=CARTESIAN_POINT('Origin',(60.1517960317846,6.00295964302151,39.1934008539948));
#210324=CARTESIAN_POINT('Origin',(60.1073400339999,5.99823604520057,39.1160402713846));
#210325=CARTESIAN_POINT('Ctrl Pts',(62.6108711573006,6.56531752495217,40.1599502534424));
#210326=CARTESIAN_POINT('Ctrl Pts',(62.5737697140403,6.56142710223267,40.10025));
#210327=CARTESIAN_POINT('Ctrl Pts',(62.5037563256536,6.55408556365861,40.10025));
#210328=CARTESIAN_POINT('Ctrl Pts',(62.6200603487599,6.47768259608994,40.1599500538457));
#210329=CARTESIAN_POINT('Ctrl Pts',(62.5804601311999,6.49759225479877,40.100244835349));
#210330=CARTESIAN_POINT('Ctrl Pts',(62.5090664195357,6.50335812634666,40.10025));
#210331=CARTESIAN_POINT('Ctrl Pts',(62.6036598373291,6.39420891953678,40.1202442001038));
#210332=CARTESIAN_POINT('Ctrl Pts',(62.563621178826,6.43639040357846,40.0633873868017));
#210333=CARTESIAN_POINT('Ctrl Pts',(62.4890871199578,6.45393802799945,40.0772271723538));
#210334=CARTESIAN_POINT('Ctrl Pts',(62.5425397295636,6.28054002958054,40.0045995998163));
#210335=CARTESIAN_POINT('Ctrl Pts',(62.5098176621801,6.36702405212714,39.9663485808314));
#210336=CARTESIAN_POINT('Ctrl Pts',(62.4232722595963,6.38494336730895,40.0101727202465));
#210337=CARTESIAN_POINT('Ctrl Pts',(62.4991087455376,6.24912387034387,39.9304654349858));
#210338=CARTESIAN_POINT('Ctrl Pts',(62.4722367740482,6.35913125763675,39.9051900162951));
#210339=CARTESIAN_POINT('Ctrl Pts',(62.3786641568868,6.36471246584636,39.9671857458184));
#210340=CARTESIAN_POINT('Ctrl Pts',(62.4538823482276,6.24436990787975,39.8576902534424));
#210341=CARTESIAN_POINT('Ctrl Pts',(62.4410124550019,6.37126553603986,39.8573998014387));
#210342=CARTESIAN_POINT('Ctrl Pts',(62.333439457262,6.35995915837717,39.92499));
#210343=CARTESIAN_POINT('Origin',(62.5037563256536,6.55408556365861,40.22725));
#210344=CARTESIAN_POINT('Origin',(0.0331877870874813,-0.315760701779427,
39.116));
#210345=CARTESIAN_POINT('Origin',(59.7081718144893,5.95633285891129,39.116));
#210346=CARTESIAN_POINT('Origin',(5.50069060731754E-15,5.67764892858605E-15,
40.22725));
#210347=CARTESIAN_POINT('Origin',(62.5005702980932,6.58439859102944,40.22725));
#210348=CARTESIAN_POINT('Ctrl Pts',(59.7081718144893,5.95633285891129,38.989));
#210349=CARTESIAN_POINT('Ctrl Pts',(59.6948768129328,6.08282634913909,38.989));
#210350=CARTESIAN_POINT('Ctrl Pts',(59.6948967145276,6.08263699811301,39.1161901092323));
#210351=CARTESIAN_POINT('Ctrl Pts',(59.4923596726254,5.93388096803602,38.989));
#210352=CARTESIAN_POINT('Ctrl Pts',(59.4792784733323,6.06016553348709,38.9892298989766));
#210353=CARTESIAN_POINT('Ctrl Pts',(59.5223294958631,6.06449945282184,39.1161900493208));
#210354=CARTESIAN_POINT('Ctrl Pts',(59.286909633363,5.9125094606103,39.1034966344368));
#210355=CARTESIAN_POINT('Ctrl Pts',(59.2739813341599,6.03858743331972,39.1038314102557));
#210356=CARTESIAN_POINT('Ctrl Pts',(59.3580487495156,6.04723285085683,39.207752878959));
#210357=CARTESIAN_POINT('Ctrl Pts',(59.1725467709678,5.90061356181176,39.2875012672119));
#210358=CARTESIAN_POINT('Ctrl Pts',(59.1597945531718,6.02658564326341,39.2878045257868));
#210359=CARTESIAN_POINT('Ctrl Pts',(59.2666022295038,6.03762143444225,39.3549015295899));
#210360=CARTESIAN_POINT('Origin',(59.2797173540687,5.91130048050262,39.3548010137695));
#210361=CARTESIAN_POINT('Ctrl Pts',(62.3873926810692,6.8769768336648,39.8576902534424));
#210362=CARTESIAN_POINT('Ctrl Pts',(62.4011871104969,6.75017837817518,39.8573998014387));
#210363=CARTESIAN_POINT('Ctrl Pts',(62.293614112757,6.73887200051248,39.92499));
#210364=CARTESIAN_POINT('Ctrl Pts',(62.4326397213342,6.88173199854398,39.9304984902491));
#210365=CARTESIAN_POINT('Ctrl Pts',(62.4292221586334,6.76854981002337,39.9052171569783));
#210366=CARTESIAN_POINT('Ctrl Pts',(62.3388594194624,6.74362747387312,39.9672049726603));
#210367=CARTESIAN_POINT('Ctrl Pts',(62.4814742414947,6.86000643604644,40.0043437678662));
#210368=CARTESIAN_POINT('Ctrl Pts',(62.4674993676295,6.76854707276755,39.9661628577643));
#210369=CARTESIAN_POINT('Ctrl Pts',(62.3865194274378,6.73309031164093,40.0100243556236));
#210370=CARTESIAN_POINT('Ctrl Pts',(62.5644789380884,6.76243636205616,40.1194874821987));
#210371=CARTESIAN_POINT('Ctrl Pts',(62.5342007968288,6.71251593157812,40.062755148314));
#210372=CARTESIAN_POINT('Ctrl Pts',(62.4648696125156,6.67979835840173,40.0767884282376));
#210373=CARTESIAN_POINT('Ctrl Pts',(62.5984172531148,6.68360310202725,40.1599502015393));
#210374=CARTESIAN_POINT('Ctrl Pts',(62.5638265480141,6.65585031610542,40.1002449453885));
#210375=CARTESIAN_POINT('Ctrl Pts',(62.4951999029147,6.63528943158872,40.10025));
#210376=CARTESIAN_POINT('Ctrl Pts',(62.6076796697355,6.595682500798,40.1599502534424));
#210377=CARTESIAN_POINT('Ctrl Pts',(62.570580117661,6.59177408464689,40.10025));
#210378=CARTESIAN_POINT('Ctrl Pts',(62.5005702980932,6.58439859102943,40.10025));
#210379=CARTESIAN_POINT('Origin',(62.280338997922,6.86517628122425,39.92499));
#210380=CARTESIAN_POINT('Origin',(59.1025439185016,5.89267880207663,39.6398955069327));
#210381=CARTESIAN_POINT('Origin',(58.9253704827881,5.87405712357789,39.92499));
#210382=CARTESIAN_POINT('Origin',(62.1031658061007,6.84655462836685,39.6398955068273));
#210383=CARTESIAN_POINT('Origin',(61.925992614092,6.82793297553265,39.3548010137695));
#210384=CARTESIAN_POINT('Ctrl Pts',(58.8181995570486,5.863373641495,39.8576902534424));
#210385=CARTESIAN_POINT('Ctrl Pts',(58.8054696185321,5.98915458643714,39.8579948730703));
#210386=CARTESIAN_POINT('Ctrl Pts',(58.9120953679531,6.00036140428966,39.92499));
#210387=CARTESIAN_POINT('Ctrl Pts',(58.773012368204,5.85862481136378,39.9304020711231));
#210388=CARTESIAN_POINT('Ctrl Pts',(58.7772117628619,5.97090589422245,39.9058915297374));
#210389=CARTESIAN_POINT('Ctrl Pts',(58.8669063622644,5.99561184840434,39.967152378603));
#210390=CARTESIAN_POINT('Ctrl Pts',(58.7244521481309,5.88025640567497,40.0043257306692));
#210391=CARTESIAN_POINT('Ctrl Pts',(58.7389107566974,5.97111833475309,39.9667894847835));
#210392=CARTESIAN_POINT('Ctrl Pts',(58.8195131589314,6.00616078842818,40.0100138975201));
#210393=CARTESIAN_POINT('Ctrl Pts',(58.642244989525,5.97763489331366,40.1195533054858));
#210394=CARTESIAN_POINT('Ctrl Pts',(58.6726343357866,6.02730636094531,40.0630813209236));
#210395=CARTESIAN_POINT('Ctrl Pts',(58.7419259266988,6.0595909974108,40.0768265942419));
#210396=CARTESIAN_POINT('Ctrl Pts',(58.6088386066683,6.05629725705552,40.1599502027516));
#210397=CARTESIAN_POINT('Ctrl Pts',(58.6434504949707,6.08390124328528,40.1002552791541));
#210398=CARTESIAN_POINT('Ctrl Pts',(58.7121001992962,6.10418993496954,40.10025));
#210399=CARTESIAN_POINT('Ctrl Pts',(58.5996668978649,6.14377718965243,40.1599502534424));
#210400=CARTESIAN_POINT('Ctrl Pts',(58.6367684021393,6.14766703046091,40.10025));
#210401=CARTESIAN_POINT('Ctrl Pts',(58.7067819056644,6.15500747092236,40.10025));
#210402=CARTESIAN_POINT('Origin',(58.7067819056644,6.15500747092236,40.22725));
#210403=CARTESIAN_POINT('Ctrl Pts',(61.4975385923863,6.78290064323477,38.989));
#210404=CARTESIAN_POINT('Ctrl Pts',(61.5108335407727,6.65640765888665,38.989));
#210405=CARTESIAN_POINT('Ctrl Pts',(61.5108136924274,6.65659650327793,39.116189601327));
#210406=CARTESIAN_POINT('Ctrl Pts',(61.7133034041536,6.80580235504169,38.989));
#210407=CARTESIAN_POINT('Ctrl Pts',(61.7268068187943,6.67910686400998,38.9887769275436));
#210408=CARTESIAN_POINT('Ctrl Pts',(61.6833805404067,6.67473401011636,39.1161898821828));
#210409=CARTESIAN_POINT('Ctrl Pts',(61.9187082819379,6.82760223531297,39.1034967087243));
#210410=CARTESIAN_POINT('Ctrl Pts',(61.9323562021249,6.70071049691167,39.1031720232729));
#210411=CARTESIAN_POINT('Ctrl Pts',(61.8476612078252,6.69200060426922,39.2077529615018));
#210412=CARTESIAN_POINT('Ctrl Pts',(62.0330459552233,6.83973663030176,39.2875012672119));
#210413=CARTESIAN_POINT('Ctrl Pts',(62.0468640245951,6.71274549238693,39.2872087095507));
#210414=CARTESIAN_POINT('Ctrl Pts',(61.939107459519,6.70161199275173,39.354901704823));
#210415=CARTESIAN_POINT('Origin',(61.4975385923863,6.78290064323477,39.116));
#210416=CARTESIAN_POINT('Origin',(5.72301283402738E-15,5.25883924629658E-15,
40.22725));
#210417=CARTESIAN_POINT('Origin',(58.703595878104,6.18532049829319,40.22725));
#210418=CARTESIAN_POINT('Origin',(61.5094129706999,6.78414869068668,39.116));
#210419=CARTESIAN_POINT('Origin',(61.0983782637174,6.7409991768779,39.1160373285268));
#210420=CARTESIAN_POINT('Ctrl Pts',(58.5964866834552,6.17403490858941,40.1599502534424));
#210421=CARTESIAN_POINT('Ctrl Pts',(58.6335861742243,6.17794390662092,40.10025));
#210422=CARTESIAN_POINT('Ctrl Pts',(58.703595878104,6.18532049829319,40.10025));
#210423=CARTESIAN_POINT('Ctrl Pts',(58.5873013840786,6.26121185652462,40.1599500566038));
#210424=CARTESIAN_POINT('Ctrl Pts',(58.626891042407,6.24145541658181,40.1002551305375));
#210425=CARTESIAN_POINT('Ctrl Pts',(58.6982507756596,6.23596000968308,40.10025));
#210426=CARTESIAN_POINT('Ctrl Pts',(58.6032244953991,6.34441620808525,40.1203070619047));
#210427=CARTESIAN_POINT('Ctrl Pts',(58.6433169201086,6.3024974759265,40.0637098684499));
#210428=CARTESIAN_POINT('Ctrl Pts',(58.7177256636153,6.28536729223241,40.0772636213363));
#210429=CARTESIAN_POINT('Ctrl Pts',(58.6635810738165,6.45770985055596,40.0046102245801));
#210430=CARTESIAN_POINT('Ctrl Pts',(58.6966524426407,6.371918319887,39.9670001894012));
#210431=CARTESIAN_POINT('Ctrl Pts',(58.7827411889911,6.35432657855734,40.0101788811209));
#210432=CARTESIAN_POINT('Ctrl Pts',(58.7067768761601,6.48899861096476,39.9303710930187));
#210433=CARTESIAN_POINT('Ctrl Pts',(58.7342263230556,6.38003592347159,39.9058663574109));
#210434=CARTESIAN_POINT('Ctrl Pts',(58.8271002111738,6.37452670784879,39.9671344706364));
#210435=CARTESIAN_POINT('Ctrl Pts',(58.7519447039089,6.49374646112661,39.8576902534424));
#210436=CARTESIAN_POINT('Ctrl Pts',(58.7656442740271,6.36806742857246,39.8579948730703));
#210437=CARTESIAN_POINT('Ctrl Pts',(58.8722700234481,6.37927424642498,39.92499));
#210438=CARTESIAN_POINT('Origin',(58.8589949086131,6.50557852713675,39.92499));
#210439=CARTESIAN_POINT('Origin',(61.0544000804067,6.73632490881123,39.1925554488846));
#210440=CARTESIAN_POINT('Origin',(60.9730100652055,6.72777047351041,39.3343017080178));
#210441=CARTESIAN_POINT('Origin',(59.0361683443161,6.52420020557745,39.6398955069223));
#210442=CARTESIAN_POINT('Origin',(59.2133417798937,6.54282188406147,39.3548010137695));
#210443=CARTESIAN_POINT('Ctrl Pts',(60.6448574988555,6.69328024897373,39.3978017080178));
#210444=CARTESIAN_POINT('Ctrl Pts',(60.6581326136905,6.56697596826196,39.3978017080178));
#210445=CARTESIAN_POINT('Ctrl Pts',(60.6581326136905,6.56697596826196,39.5248017080178));
#210446=CARTESIAN_POINT('Ctrl Pts',(60.7343993681215,6.7024559967491,39.3978017080178));
#210447=CARTESIAN_POINT('Ctrl Pts',(60.747565938859,6.57637578951098,39.3980355775196));
#210448=CARTESIAN_POINT('Ctrl Pts',(60.7924070567583,6.58108878091632,39.5248015517192));
#210449=CARTESIAN_POINT('Ctrl Pts',(60.819067758858,6.71113417453909,39.3484893995498));
#210450=CARTESIAN_POINT('Ctrl Pts',(60.8325536871416,6.58530836180368,39.3489438303409));
#210451=CARTESIAN_POINT('Ctrl Pts',(60.9193730951232,6.59443344928337,39.4508333155592));
#210452=CARTESIAN_POINT('Ctrl Pts',(60.8636883187846,6.71570789669327,39.2708017080178));
#210453=CARTESIAN_POINT('Ctrl Pts',(60.8773920302462,6.59002106156384,39.2710850691866));
#210454=CARTESIAN_POINT('Ctrl Pts',(60.9862851800405,6.60146619279864,39.3343017080178));
#210455=CARTESIAN_POINT('Origin',(60.6448574988555,6.69328024897373,39.5248017080178));
#210456=CARTESIAN_POINT('Ctrl Pts',(59.1062911958297,6.53099325079975,39.2875012672119));
#210457=CARTESIAN_POINT('Ctrl Pts',(59.1200087114583,6.40512264090921,39.2878045257519));
#210458=CARTESIAN_POINT('Ctrl Pts',(59.2267768430461,6.41653455700044,39.3549015218347));
#210459=CARTESIAN_POINT('Ctrl Pts',(59.2206299794252,6.54313486548288,39.1034938540228));
#210460=CARTESIAN_POINT('Ctrl Pts',(59.2341972766244,6.41712406698054,39.1038286278808));
#210461=CARTESIAN_POINT('Ctrl Pts',(59.318224747433,6.42614611919662,39.2077506434031));
#210462=CARTESIAN_POINT('Ctrl Pts',(59.426035450364,6.56494601396981,38.989));
#210463=CARTESIAN_POINT('Ctrl Pts',(59.4394961352159,6.43870134519647,38.9892298954611));
#210464=CARTESIAN_POINT('Ctrl Pts',(59.48250679558,6.44341285848367,39.1161900347289));
#210465=CARTESIAN_POINT('Ctrl Pts',(59.6417962403144,6.58785426247015,38.989));
#210466=CARTESIAN_POINT('Ctrl Pts',(59.6550912403354,6.46136078685154,38.989));
#210467=CARTESIAN_POINT('Ctrl Pts',(59.6550713402783,6.46155012324659,39.1161900945646));
#210468=CARTESIAN_POINT('Origin',(59.6417962403144,6.58785426247015,39.116));
#210469=CARTESIAN_POINT('Origin',(60.0186752706393,6.62746584474012,39.5248017080178));
#210470=CARTESIAN_POINT('Origin',(60.4944777170595,6.67747469700864,39.5248017080178));
#210471=CARTESIAN_POINT('Origin',(59.7852323155142,6.60293000146354,39.116));
#210472=CARTESIAN_POINT('Origin',(60.04095383883,6.62985850077722,39.1160402713845));
#210473=CARTESIAN_POINT('Ctrl Pts',(60.275645989912,6.65505462397313,39.2708017080178));
#210474=CARTESIAN_POINT('Ctrl Pts',(60.2894805317163,6.52822907310695,39.27051194648));
#210475=CARTESIAN_POINT('Ctrl Pts',(60.1796001951996,6.51668018436665,39.3343017080178));
#210476=CARTESIAN_POINT('Ctrl Pts',(60.3204176712046,6.65964099131217,39.3487519301186));
#210477=CARTESIAN_POINT('Ctrl Pts',(60.3340024654441,6.53290851690509,39.3482879463988));
#210478=CARTESIAN_POINT('Ctrl Pts',(60.246738409926,6.52373669508256,39.4512271261639));
#210479=CARTESIAN_POINT('Ctrl Pts',(60.4052373806432,6.66833043150585,39.3978017080178));
#210480=CARTESIAN_POINT('Ctrl Pts',(60.4184509388162,6.54178440911706,39.3975673827397));
#210481=CARTESIAN_POINT('Ctrl Pts',(60.3739306632453,6.53710513959941,39.524801535518));
#210482=CARTESIAN_POINT('Ctrl Pts',(60.4944777170595,6.67747469700864,39.3978017080178));
#210483=CARTESIAN_POINT('Ctrl Pts',(60.5077528318945,6.55117041629687,39.3978017080178));
#210484=CARTESIAN_POINT('Ctrl Pts',(60.5077528318945,6.55117041629687,39.5248017080178));
#210485=CARTESIAN_POINT('Origin',(60.1663250803646,6.64298446507842,39.3343017080178));
#210486=CARTESIAN_POINT('Origin',(60.0854204586799,6.63448104699103,39.1934008533554));
#210487=CARTESIAN_POINT('Origin',(5.66467691768715E-15,1.86266069604307E-13,
2.53178198860262));
#210488=CARTESIAN_POINT('',(-0.0152399999993761,-59.0285534841294,2.65878198860221));
#210489=CARTESIAN_POINT('',(0.0152400000006239,-59.0285534841294,2.65878198860221));
#210490=CARTESIAN_POINT('Origin',(5.64679317051214E-15,1.85361349597066E-13,
2.65878198860263));
#210491=CARTESIAN_POINT('',(-0.015212193455297,-58.9208513795071,2.59908173515982));
#210492=CARTESIAN_POINT('Origin',(-0.015239999999376,-59.0285534841294,
2.5317819886022));
#210493=CARTESIAN_POINT('',(0.0152121934565426,-58.9208513795071,2.59908173515982));
#210494=CARTESIAN_POINT('Origin',(5.65519997554244E-15,1.85786641043733E-13,
2.59908173516023));
#210495=CARTESIAN_POINT('Origin',(0.0152400000006239,-59.0285534841294,
2.5317819886022));
#210496=CARTESIAN_POINT('Origin',(5.66467691768715E-15,1.86047439754084E-13,
2.53178198860262));
#210497=CARTESIAN_POINT('',(-0.0152661173102018,-62.9541448057646,2.59908173515979));
#210498=CARTESIAN_POINT('',(0.0152661173115319,-62.9541448057646,2.59908173515979));
#210499=CARTESIAN_POINT('Origin',(5.65519997554243E-15,1.8556801119351E-13,
2.59908173516023));
#210500=CARTESIAN_POINT('',(-0.0152399999993361,-62.8464427007194,2.65878198860218));
#210501=CARTESIAN_POINT('Origin',(-0.015239999999336,-62.8464427007194,
2.53178198860218));
#210502=CARTESIAN_POINT('',(0.0152400000006639,-62.8464427007194,2.65878198860218));
#210503=CARTESIAN_POINT('Origin',(5.64679317051213E-15,1.85142719746843E-13,
2.65878198860263));
#210504=CARTESIAN_POINT('Origin',(0.0152400000006639,-62.8464427007194,
2.53178198860217));
#210505=CARTESIAN_POINT('Origin',(3.5331177639001E-16,1.91577434745604E-13,
2.53178198860262));
#210506=CARTESIAN_POINT('',(-59.0285534841296,0.0152400000001907,2.65878198860261));
#210507=CARTESIAN_POINT('',(-59.0285534841296,-0.0152399999998093,2.65878198860261));
#210508=CARTESIAN_POINT('Origin',(3.17544282039971E-16,1.90690598485538E-13,
2.65878198860263));
#210509=CARTESIAN_POINT('',(-58.9208513795073,0.015212193456111,2.59908173516022));
#210510=CARTESIAN_POINT('Origin',(-59.0285534841296,0.0152400000001916,
2.53178198860261));
#210511=CARTESIAN_POINT('',(-58.9208513795073,-0.0152121934557287,2.59908173516022));
#210512=CARTESIAN_POINT('Origin',(3.34357892100574E-16,1.91107483127175E-13,
2.59908173516024));
#210513=CARTESIAN_POINT('Origin',(-59.0285534841296,-0.0152399999998084,
2.53178198860261));
#210514=CARTESIAN_POINT('Origin',(1.34681926167381E-16,1.91577434745604E-13,
2.53178198860262));
#210515=CARTESIAN_POINT('',(-62.9541448057648,0.0152661173110579,2.59908173516022));
#210516=CARTESIAN_POINT('',(-62.9541466567496,1.98817142546799E-13,2.59908173516022));
#210517=CARTESIAN_POINT('Origin',(1.15728041877948E-16,1.91107483127175E-13,
2.59908173516023));
#210518=CARTESIAN_POINT('',(-62.8464427007196,0.0152400000001907,2.65878198860261));
#210519=CARTESIAN_POINT('Origin',(-62.8464427007196,0.0152400000001916,
2.53178198860261));
#210520=CARTESIAN_POINT('',(-62.8464427007196,-0.0152399999998093,2.65878198860261));
#210521=CARTESIAN_POINT('Origin',(9.89144318173425E-17,1.90690598485538E-13,
2.65878198860263));
#210522=CARTESIAN_POINT('',(-62.9541448057648,-0.0152661173106757,2.59908173516022));
#210523=CARTESIAN_POINT('Origin',(-62.8464427007196,-0.0152399999998084,
2.5317819886026));
#210524=CARTESIAN_POINT('Origin',(1.15728041877948E-16,1.91107483127175E-13,
2.59908173516023));
#210525=CARTESIAN_POINT('Origin',(5.62443848654336E-15,1.89582053160455E-13,
2.81753198860262));
#210526=CARTESIAN_POINT('',(58.2189663438286,2.0114600153905E-13,2.18253198860263));
#210527=CARTESIAN_POINT('Origin',(5.71385722241845E-15,1.94016234460786E-13,
2.18253198860262));
#210528=CARTESIAN_POINT('',(57.6804558027693,1.98995629809826E-13,2.48103325581453));
#210529=CARTESIAN_POINT('Origin',(58.2189663438286,1.96711820238719E-13,
2.81753198860263));
#210530=CARTESIAN_POINT('',(-57.6804558027693,1.84867992695381E-13,2.48103325581451));
#210531=CARTESIAN_POINT('Origin',(5.67182319726696E-15,1.91931811252603E-13,
2.48103325581452));
#210532=CARTESIAN_POINT('Origin',(5.67182319726696E-15,1.91931811252603E-13,
2.48103325581452));
#210533=CARTESIAN_POINT('Origin',(5.62443848654336E-15,1.89582053160455E-13,
2.81753198860262));
#210534=CARTESIAN_POINT('',(58.8470884664677,1.99138501105563E-13,2.48103325581455));
#210535=CARTESIAN_POINT('Origin',(5.67182319726695E-15,1.91931811252603E-13,
2.48103325581454));
#210536=CARTESIAN_POINT('',(58.3085779254084,2.01156975792705E-13,2.18253198860263));
#210537=CARTESIAN_POINT('Origin',(58.3085779254084,1.96722794492374E-13,
2.81753198860263));
#210538=CARTESIAN_POINT('Origin',(5.71385722241845E-15,1.94016234460786E-13,
2.18253198860262));
#210539=CARTESIAN_POINT('Origin',(5.62443848654336E-15,1.89582053160455E-13,
2.81753198860262));
#210540=CARTESIAN_POINT('',(63.5664220745916,2.01800875993476E-13,2.18253198860263));
#210541=CARTESIAN_POINT('Origin',(5.71385722241845E-15,1.94016234460786E-13,
2.18253198860262));
#210542=CARTESIAN_POINT('',(63.0279115335323,1.99650504264252E-13,2.48103325581454));
#210543=CARTESIAN_POINT('Origin',(63.5664220745916,1.97366694693145E-13,
2.81753198860263));
#210544=CARTESIAN_POINT('',(-63.0279115335323,1.84213118240955E-13,2.48103325581452));
#210545=CARTESIAN_POINT('Origin',(5.67182319726696E-15,1.91931811252603E-13,
2.48103325581453));
#210546=CARTESIAN_POINT('Origin',(5.67182319726696E-15,1.91931811252603E-13,
2.48103325581453));
#210547=CARTESIAN_POINT('Origin',(5.62443848654336E-15,1.89582053160455E-13,
2.81753198860262));
#210548=CARTESIAN_POINT('',(64.1945441972308,1.99793375559989E-13,2.48103325581455));
#210549=CARTESIAN_POINT('Origin',(5.67182319726695E-15,1.91931811252603E-13,
2.48103325581454));
#210550=CARTESIAN_POINT('',(63.6560336561714,2.01811850247131E-13,2.18253198860263));
#210551=CARTESIAN_POINT('Origin',(63.6560336561714,1.973776689468E-13,2.81753198860263));
#210552=CARTESIAN_POINT('Origin',(5.71385722241845E-15,1.94016234460786E-13,
2.18253198860262));
#210553=CARTESIAN_POINT('Origin',(0.,-8.93279506303506E-14,42.7590319886026));
#210554=CARTESIAN_POINT('',(65.,1.88673894754252E-13,4.08753198860263));
#210555=CARTESIAN_POINT('Origin',(5.44560101479317E-15,1.80713690559794E-13,
4.08753198860262));
#210556=CARTESIAN_POINT('',(65.,1.90890985404417E-13,3.77003198860264));
#210557=CARTESIAN_POINT('',(65.,-8.13677464358929E-14,42.7590319886026));
#210558=CARTESIAN_POINT('Origin',(5.49031038273072E-15,1.82930781209959E-13,
3.77003198860263));
#210559=CARTESIAN_POINT('Origin',(5.71385722241845E-15,1.94016234460786E-13,
2.18253198860262));
#210560=CARTESIAN_POINT('',(64.008019903844,2.01854956130286E-13,2.18253198860263));
#210561=CARTESIAN_POINT('Origin',(5.49031038273072E-15,1.82930781209959E-13,
3.77003198860263));
#210562=CARTESIAN_POINT('',(62.9541448057648,-0.0152661173106757,2.59908173516024));
#210563=CARTESIAN_POINT('',(62.9541448057648,0.0152661173110579,2.59908173516024));
#210564=CARTESIAN_POINT('Origin',(-1.95097259456047E-16,1.91107483127175E-13,
2.59908173516023));
#210565=CARTESIAN_POINT('',(62.7644678366119,0.318045750793234,2.90134173516024));
#210566=CARTESIAN_POINT('Ctrl Pts',(62.9541448057648,0.0152661173110579,
2.59908173516025));
#210567=CARTESIAN_POINT('Ctrl Pts',(62.9541438736292,0.019087735244839,
2.59908174381684));
#210568=CARTESIAN_POINT('Ctrl Pts',(62.9540952129414,0.0228988721024147,
2.59915752000996));
#210569=CARTESIAN_POINT('Ctrl Pts',(62.9539999459718,0.0266975986405368,
2.59930729517471));
#210570=CARTESIAN_POINT('Ctrl Pts',(62.953449420412,0.0486495517943568,
2.60017281085929));
#210571=CARTESIAN_POINT('Ctrl Pts',(62.9513443281451,0.0701898812494245,
2.60350651800147));
#210572=CARTESIAN_POINT('Ctrl Pts',(62.94790035651,0.0909392844481384,2.60896880596674));
#210573=CARTESIAN_POINT('Ctrl Pts',(62.9465113235254,0.0993079960720901,
2.6111718723562));
#210574=CARTESIAN_POINT('Ctrl Pts',(62.9449047668207,0.107548428340682,
2.6137207657729));
#210575=CARTESIAN_POINT('Ctrl Pts',(62.9430957254317,0.115637319282417,
2.61659179896982));
#210576=CARTESIAN_POINT('Ctrl Pts',(62.9424282989905,0.118621628943673,
2.61765103591207));
#210577=CARTESIAN_POINT('Ctrl Pts',(62.9417332466658,0.121585194085759,
2.61875422455149));
#210578=CARTESIAN_POINT('Ctrl Pts',(62.941011293136,0.12452678807298,2.61990022440395));
#210579=CARTESIAN_POINT('Ctrl Pts',(62.9396576302675,0.13004227679902,2.62204897412732));
#210580=CARTESIAN_POINT('Ctrl Pts',(62.938209392844,0.135480523183793,2.62434823201769));
#210581=CARTESIAN_POINT('Ctrl Pts',(62.9366713579026,0.140833441493559,
2.62679048030304));
#210582=CARTESIAN_POINT('Ctrl Pts',(62.9312882356078,0.15956865557774,2.63533834930178));
#210583=CARTESIAN_POINT('Ctrl Pts',(62.9248050892389,0.177258600739159,
2.64563784783561));
#210584=CARTESIAN_POINT('Ctrl Pts',(62.9174267595942,0.193556601113839,
2.65736666737963));
#210585=CARTESIAN_POINT('Ctrl Pts',(62.9137375947719,0.201705601301178,
2.66323107715163));
#210586=CARTESIAN_POINT('Ctrl Pts',(62.9098246351408,0.209506615291594,
2.66945281780773));
#210587=CARTESIAN_POINT('Ctrl Pts',(62.9057134946881,0.216916308650584,
2.675991606312));
#210588=CARTESIAN_POINT('Ctrl Pts',(62.9036579244618,0.22062115533008,2.67926100056413));
#210589=CARTESIAN_POINT('Ctrl Pts',(62.9015528091474,0.224228171852737,
2.68260965685122));
#210590=CARTESIAN_POINT('Ctrl Pts',(62.8994013510256,0.227731941419725,
2.68603254012481));
#210591=CARTESIAN_POINT('Ctrl Pts',(62.8972498929038,0.231235710986713,
2.68945542339841));
#210592=CARTESIAN_POINT('Ctrl Pts',(62.8950520414621,0.23463611427692,2.69295261525384));
#210593=CARTESIAN_POINT('Ctrl Pts',(62.8928111037451,0.237927978231107,
2.69651891172098));
#210594=CARTESIAN_POINT('Ctrl Pts',(62.8927919932396,0.237956050936405,
2.69654932476087));
#210595=CARTESIAN_POINT('Ctrl Pts',(62.8927728797351,0.237984115711198,
2.69657974261145));
#210596=CARTESIAN_POINT('Ctrl Pts',(62.8927537632335,0.238012172553033,
2.69661016526973));
#210597=CARTESIAN_POINT('Ctrl Pts',(62.8829906867849,0.252341211296434,
2.71214746101059));
#210598=CARTESIAN_POINT('Ctrl Pts',(62.8725309380421,0.264702219189649,
2.72880565567421));
#210599=CARTESIAN_POINT('Ctrl Pts',(62.8615664772847,0.275152816745564,
2.7462804001209));
#210600=CARTESIAN_POINT('Ctrl Pts',(62.850231205745,0.285956846571411,2.7643461288212));
#210601=CARTESIAN_POINT('Ctrl Pts',(62.8383556508913,0.2947193320565,2.78328592654098));
#210602=CARTESIAN_POINT('Ctrl Pts',(62.8261370346469,0.301453885679487,
2.80278753267434));
#210603=CARTESIAN_POINT('Ctrl Pts',(62.814150842194,0.308060333921697,2.82191817722369));
#210604=CARTESIAN_POINT('Ctrl Pts',(62.8018335935207,0.312715155745102,
2.84159092314712));
#210605=CARTESIAN_POINT('Ctrl Pts',(62.7893708783688,0.315383336840664,
2.86151233816558));
#210606=CARTESIAN_POINT('Ctrl Pts',(62.7811147664987,0.317150913275342,
2.87470957721006));
#210607=CARTESIAN_POINT('Ctrl Pts',(62.7727948225172,0.318045664008643,
2.88801594388191));
#210608=CARTESIAN_POINT('Ctrl Pts',(62.7644678366119,0.318045750793233,
2.90134173516024));
#210609=CARTESIAN_POINT('',(62.4081695979768,0.318048871877314,3.47153072139072));
#210610=CARTESIAN_POINT('',(62.7644678366119,0.318045750793234,2.90134173516024));
#210611=CARTESIAN_POINT('',(62.0995362748659,6.20712349654482,3.47153072139077));
#210612=CARTESIAN_POINT('Origin',(5.53234440788222E-15,1.85015204418142E-13,
3.47153072139072));
#210613=CARTESIAN_POINT('',(62.4538823482275,6.24436990788079,2.90134173516028));
#210614=CARTESIAN_POINT('',(62.0995362748659,6.20712349654482,3.47153072139077));
#210615=CARTESIAN_POINT('',(62.6108711573006,6.56531752495322,2.59908173516028));
#210616=CARTESIAN_POINT('Ctrl Pts',(62.4538823482275,6.24436990788079,2.90134173516029));
#210617=CARTESIAN_POINT('Ctrl Pts',(62.4661208561101,6.24565635961461,2.88164837656795));
#210618=CARTESIAN_POINT('Ctrl Pts',(62.4781153572946,6.24887816048076,2.86203734439279));
#210619=CARTESIAN_POINT('Ctrl Pts',(62.4897034690548,6.25393874389341,2.84277945978351));
#210620=CARTESIAN_POINT('Ctrl Pts',(62.5015244311521,6.25910101415356,2.823134609203));
#210621=CARTESIAN_POINT('Ctrl Pts',(62.5129234356942,6.26617675898121,2.80385576863699));
#210622=CARTESIAN_POINT('Ctrl Pts',(62.5237314369727,6.27511683300188,2.78521678518818));
#210623=CARTESIAN_POINT('Ctrl Pts',(62.5341195571992,6.2837095932512,2.76730190934976));
#210624=CARTESIAN_POINT('Ctrl Pts',(62.5439624606622,6.29402509233161,2.74997687280356));
#210625=CARTESIAN_POINT('Ctrl Pts',(62.5531007542683,6.30606398946803,2.73349253346358));
#210626=CARTESIAN_POINT('Ctrl Pts',(62.5601204743134,6.31531185249283,2.72082983599693));
#210627=CARTESIAN_POINT('Ctrl Pts',(62.5667243349244,6.32557753707723,2.70866321039474));
#210628=CARTESIAN_POINT('Ctrl Pts',(62.5728320301413,6.3368780377171,2.6971164533585));
#210629=CARTESIAN_POINT('Ctrl Pts',(62.5728480373212,6.33690765431395,2.69708619136755));
#210630=CARTESIAN_POINT('Ctrl Pts',(62.5728640408535,6.33693727882116,2.69705593387223));
#210631=CARTESIAN_POINT('Ctrl Pts',(62.5728800407364,6.33696691123596,2.69702568087575));
#210632=CARTESIAN_POINT('Ctrl Pts',(62.5745955535553,6.34014410870347,2.6937819444327));
#210633=CARTESIAN_POINT('Ctrl Pts',(62.5762674929177,6.34341121944338,2.69059266624704));
#210634=CARTESIAN_POINT('Ctrl Pts',(62.5778935423008,6.34676388583406,2.68746219342681));
#210635=CARTESIAN_POINT('Ctrl Pts',(62.5869421374019,6.36542071200083,2.67004182395935));
#210636=CARTESIAN_POINT('Ctrl Pts',(62.5945741278863,6.38672471011596,2.65443567877611));
#210637=CARTESIAN_POINT('Ctrl Pts',(62.6004109483577,6.40987366744549,2.64136852352728));
#210638=CARTESIAN_POINT('Ctrl Pts',(62.6030305942149,6.42026324006697,2.63550380329468));
#210639=CARTESIAN_POINT('Ctrl Pts',(62.605288967123,6.43102458681701,2.6301499745099));
#210640=CARTESIAN_POINT('Ctrl Pts',(62.6071534261453,6.44208677567884,2.62536981119258));
#210641=CARTESIAN_POINT('Ctrl Pts',(62.607963694818,6.44689425333237,2.62329241687077));
#210642=CARTESIAN_POINT('Ctrl Pts',(62.6086994224563,6.45175840518007,2.62132362131432));
#210643=CARTESIAN_POINT('Ctrl Pts',(62.6093578414453,6.45667331290448,2.61946873372352));
#210644=CARTESIAN_POINT('Ctrl Pts',(62.6116623079068,6.47387548993995,2.61297662715572));
#210645=CARTESIAN_POINT('Ctrl Pts',(62.6130197402063,6.49169942613424,2.60787989113974));
#210646=CARTESIAN_POINT('Ctrl Pts',(62.6133114945132,6.50989137546638,2.60440616886185));
#210647=CARTESIAN_POINT('Ctrl Pts',(62.6134573716667,6.51898735013245,2.6026693077229));
#210648=CARTESIAN_POINT('Ctrl Pts',(62.6133368299269,6.52817532814412,2.60133820040189));
#210649=CARTESIAN_POINT('Ctrl Pts',(62.6129350466932,6.53742359207021,2.60044130723589));
#210650=CARTESIAN_POINT('Ctrl Pts',(62.6127341550764,6.54204772403325,2.59999286065289));
#210651=CARTESIAN_POINT('Ctrl Pts',(62.6124629532086,6.5466869274878,2.59965296768517));
#210652=CARTESIAN_POINT('Ctrl Pts',(62.6121195889602,6.55133723782971,2.59942518630959));
#210653=CARTESIAN_POINT('Ctrl Pts',(62.6117762247118,6.55598754817163,2.59919740493401));
#210654=CARTESIAN_POINT('Ctrl Pts',(62.6113606963859,6.56064896522291,2.59908173791625));
#210655=CARTESIAN_POINT('Ctrl Pts',(62.6108711573006,6.56531752495321,2.59908173516029));
#210656=CARTESIAN_POINT('',(62.6076796697354,6.59568250079905,2.59908173516029));
#210657=CARTESIAN_POINT('Origin',(5.50063869163689E-15,1.85396353497297E-13,
2.59908173516023));
#210658=CARTESIAN_POINT('',(62.3873926810691,6.87697683366584,2.90134173516029));
#210659=CARTESIAN_POINT('Ctrl Pts',(62.6076796697354,6.59568250079905,2.5990817351603));
#210660=CARTESIAN_POINT('Ctrl Pts',(62.6072792748563,6.59948308607522,2.59908174381695));
#210661=CARTESIAN_POINT('Ctrl Pts',(62.6068325084578,6.60326825869941,2.59915752001001));
#210662=CARTESIAN_POINT('Ctrl Pts',(62.6063406883232,6.60703621730616,2.59930729517476));
#210663=CARTESIAN_POINT('Ctrl Pts',(62.6034985746712,6.62881036977247,2.60017281085931));
#210664=CARTESIAN_POINT('Ctrl Pts',(62.5991534367839,6.65001265698881,2.60350651800137));
#210665=CARTESIAN_POINT('Ctrl Pts',(62.5935594283559,6.67028839972278,2.60896880596642));
#210666=CARTESIAN_POINT('Ctrl Pts',(62.5913032360736,6.67846607318599,2.61117187235597));
#210667=CARTESIAN_POINT('Ctrl Pts',(62.5888441205329,6.68649343260138,2.6137207657728));
#210668=CARTESIAN_POINT('Ctrl Pts',(62.5861994699221,6.69434891543626,2.61659179896988));
#210669=CARTESIAN_POINT('Ctrl Pts',(62.5852237544099,6.69724711167669,2.61765103591213));
#210670=CARTESIAN_POINT('Ctrl Pts',(62.5842227327444,6.70012178934745,2.61875422455152));
#210671=CARTESIAN_POINT('Ctrl Pts',(62.5831972538526,6.702971804282,2.61990022440399));
#210672=CARTESIAN_POINT('Ctrl Pts',(62.5812744809303,6.70831558228429,2.62204897412736));
#210673=CARTESIAN_POINT('Ctrl Pts',(62.5792657255654,6.71357265535402,2.62434823201774));
#210674=CARTESIAN_POINT('Ctrl Pts',(62.5771765838154,6.71873548138833,2.62679048030309));
#210675=CARTESIAN_POINT('Ctrl Pts',(62.5698645876906,6.7368053725084,2.63533834930182));
#210676=CARTESIAN_POINT('Ctrl Pts',(62.5615678538928,6.75372073697221,2.64563784783566));
#210677=CARTESIAN_POINT('Ctrl Pts',(62.5525263385764,6.76915820973631,2.65736666737968));
#210678=CARTESIAN_POINT('Ctrl Pts',(62.5480055809182,6.77687694611836,2.66323107715169));
#210679=CARTESIAN_POINT('Ctrl Pts',(62.5432986288851,6.78422620968084,2.66945281780777));
#210680=CARTESIAN_POINT('Ctrl Pts',(62.5384354858299,6.79116558077052,2.67599160631204));
#210681=CARTESIAN_POINT('Ctrl Pts',(62.5360039143022,6.79463526631536,2.67926100056418));
#210682=CARTESIAN_POINT('Ctrl Pts',(62.5335332951358,6.79800247875529,2.68260965685127));
#210683=CARTESIAN_POINT('Ctrl Pts',(62.5310273792782,6.80126216569473,2.68603254012487));
#210684=CARTESIAN_POINT('Ctrl Pts',(62.5285214634206,6.80452185263417,2.68945542339846));
#210685=CARTESIAN_POINT('Ctrl Pts',(62.5259802131086,6.80767389012568,2.69295261525388));
#210686=CARTESIAN_POINT('Ctrl Pts',(62.5234074580025,6.81071347912885,2.69651891172102));
#210687=CARTESIAN_POINT('Ctrl Pts',(62.5233855177896,6.81073940045716,2.6965493247609));
#210688=CARTESIAN_POINT('Ctrl Pts',(62.5233635754231,6.81076531358493,2.69657974261149));
#210689=CARTESIAN_POINT('Ctrl Pts',(62.5233416309052,6.81079121850992,2.69661016526977));
#210690=CARTESIAN_POINT('Ctrl Pts',(62.5121342452098,6.82402124190313,2.71214746101212));
#210691=CARTESIAN_POINT('Ctrl Pts',(62.5004397189044,6.83522119344041,2.72880565567745));
#210692=CARTESIAN_POINT('Ctrl Pts',(62.4884429377063,6.84446844329644,2.74628040012597));
#210693=CARTESIAN_POINT('Ctrl Pts',(62.4760404333341,6.85402842900223,2.76434612882814));
#210694=CARTESIAN_POINT('Ctrl Pts',(62.4633140048689,6.86150157917582,2.78328592654992));
#210695=CARTESIAN_POINT('Ctrl Pts',(62.4504583709406,6.86692204702988,2.80278753268532));
#210696=CARTESIAN_POINT('Ctrl Pts',(62.4378472782206,6.87223940617952,2.82191817723646));
#210697=CARTESIAN_POINT('Ctrl Pts',(62.4251109433513,6.87558122532578,2.84159092316169));
#210698=CARTESIAN_POINT('Ctrl Pts',(62.4124375993863,6.87693208138216,2.86151233818192));
#210699=CARTESIAN_POINT('Ctrl Pts',(62.404041953316,6.87782697616073,2.87470957722106));
#210700=CARTESIAN_POINT('Ctrl Pts',(62.3956740599424,6.87784715439664,2.88801594388745));
#210701=CARTESIAN_POINT('Ctrl Pts',(62.3873926810691,6.87697683366584,2.9013417351603));
#210702=CARTESIAN_POINT('',(62.0330459552232,6.83973663030279,3.47153072139077));
#210703=CARTESIAN_POINT('',(62.3873926810691,6.87697683366584,2.90134173516029));
#210704=CARTESIAN_POINT('',(61.1105274371641,12.6642893210144,3.47153072139081));
#210705=CARTESIAN_POINT('Origin',(5.53234440788222E-15,1.85015204418142E-13,
3.47153072139072));
#210706=CARTESIAN_POINT('',(61.4590390555209,12.7383709431253,2.90134173516033));
#210707=CARTESIAN_POINT('',(61.1105274371641,12.6642893210143,3.47153072139081));
#210708=CARTESIAN_POINT('',(61.5816197022698,13.0739701745327,2.59908173516033));
#210709=CARTESIAN_POINT('Ctrl Pts',(61.4590390555209,12.7383709431253,2.90134173516033));
#210710=CARTESIAN_POINT('Ctrl Pts',(61.4710760487544,12.7409296199637,2.88164837656726));
#210711=CARTESIAN_POINT('Ctrl Pts',(61.4826680729132,12.7453875382444,2.86203734439139));
#210712=CARTESIAN_POINT('Ctrl Pts',(61.4936637287778,12.7516316867664,2.84277945978143));
#210713=CARTESIAN_POINT('Ctrl Pts',(61.5048803302309,12.7580013045727,2.82313460920026));
#210714=CARTESIAN_POINT('Ctrl Pts',(61.5154772731004,12.7662298081578,2.80385576863363));
#210715=CARTESIAN_POINT('Ctrl Pts',(61.5252915748184,12.7762506512828,2.78521678518427));
#210716=CARTESIAN_POINT('Ctrl Pts',(61.5347245998114,12.7858821937365,2.76730190934541));
#210717=CARTESIAN_POINT('Ctrl Pts',(61.5434353195528,12.7971700470073,2.74997687279882));
#210718=CARTESIAN_POINT('Ctrl Pts',(61.5512651452133,12.8100982055938,2.73349253345852));
#210719=CARTESIAN_POINT('Ctrl Pts',(61.5572797455861,12.8200291684051,2.7208298359937));
#210720=CARTESIAN_POINT('Ctrl Pts',(61.5627743733228,12.8309289078952,2.70866321039323));
#210721=CARTESIAN_POINT('Ctrl Pts',(61.5676673859796,12.8428059312037,2.69711645335854));
#210722=CARTESIAN_POINT('Ctrl Pts',(61.5676802096931,12.8428370587636,2.6970861913676));
#210723=CARTESIAN_POINT('Ctrl Pts',(61.5676930289522,12.8428681938093,2.69705593387227));
#210724=CARTESIAN_POINT('Ctrl Pts',(61.5677058437553,12.8428993363378,2.69702568087579));
#210725=CARTESIAN_POINT('Ctrl Pts',(61.5690798512467,12.8462384487039,2.69378194443274));
#210726=CARTESIAN_POINT('Ctrl Pts',(61.5704011254854,12.8496624271215,2.69059266624708));
#210727=CARTESIAN_POINT('Ctrl Pts',(61.5716678181342,12.8531666956981,2.68746219342685));
#210728=CARTESIAN_POINT('Ctrl Pts',(61.5787166747153,12.8726671535583,2.67004182396061));
#210729=CARTESIAN_POINT('Ctrl Pts',(61.5840799821727,12.894652206378,2.65443567877833));
#210730=CARTESIAN_POINT('Ctrl Pts',(61.5874651029949,12.9182844651696,2.64136852353006));
#210731=CARTESIAN_POINT('Ctrl Pts',(61.5889843920982,12.9288909501824,2.63550380329639));
#210732=CARTESIAN_POINT('Ctrl Pts',(61.5901055263651,12.9398294094002,2.63014997451068));
#210733=CARTESIAN_POINT('Ctrl Pts',(61.5908034580838,12.9510258874722,2.62536981119262));
#210734=CARTESIAN_POINT('Ctrl Pts',(61.5911067697685,12.9558917253993,2.62329241687082));
#210735=CARTESIAN_POINT('Ctrl Pts',(61.5913300246961,12.9608061353937,2.62132362131436));
#210736=CARTESIAN_POINT('Ctrl Pts',(61.5914710890455,12.9657629422644,2.61946873372356));
#210737=CARTESIAN_POINT('Ctrl Pts',(61.5919648142682,12.9831117663121,2.61297662715576));
#210738=CARTESIAN_POINT('Ctrl Pts',(61.5914517017518,13.0009799514312,2.60787989113978));
#210739=CARTESIAN_POINT('Ctrl Pts',(61.5898402812905,13.0191027399908,2.60440616886188));
#210740=CARTESIAN_POINT('Ctrl Pts',(61.5890345710599,13.0281641342706,2.60266930772293));
#210741=CARTESIAN_POINT('Ctrl Pts',(61.5879542844384,13.0372891795345,2.60133820040193));
#210742=CARTESIAN_POINT('Ctrl Pts',(61.5865879953992,13.0464447827192,2.60044130723593));
#210743=CARTESIAN_POINT('Ctrl Pts',(61.5859048508796,13.0510225843115,2.59999286065293));
#210744=CARTESIAN_POINT('Ctrl Pts',(61.5851502058761,13.0556080254097,2.59965296768521));
#210745=CARTESIAN_POINT('Ctrl Pts',(61.5843226328192,13.0601969695277,2.59942518630963));
#210746=CARTESIAN_POINT('Ctrl Pts',(61.5834950597624,13.0647859136458,2.59919740493405));
#210747=CARTESIAN_POINT('Ctrl Pts',(61.5825945569831,13.0693783604294,2.59908173791627));
#210748=CARTESIAN_POINT('Ctrl Pts',(61.5816197022698,13.0739701745327,2.59908173516033));
#210749=CARTESIAN_POINT('',(61.5752716937451,13.103835206573,2.59908173516034));
#210750=CARTESIAN_POINT('Origin',(5.50318346416883E-15,1.85380286435869E-13,
2.59908173516022));
#210751=CARTESIAN_POINT('',(61.3267881959113,13.3605623192489,2.90134173516034));
#210752=CARTESIAN_POINT('Ctrl Pts',(61.5752716937451,13.103835206573,2.59908173516033));
#210753=CARTESIAN_POINT('Ctrl Pts',(61.5744762229326,13.1075731191839,2.59908174381695));
#210754=CARTESIAN_POINT('Ctrl Pts',(61.5736362456896,13.1112908564314,2.59915752001006));
#210755=CARTESIAN_POINT('Ctrl Pts',(61.5727532608744,13.1149867645638,2.5993072951748));
#210756=CARTESIAN_POINT('Ctrl Pts',(61.5676506979228,13.1363445541687,2.60017281085922));
#210757=CARTESIAN_POINT('Ctrl Pts',(61.5611131206563,13.1569765024481,2.60350651800036));
#210758=CARTESIAN_POINT('Ctrl Pts',(61.5534303645638,13.1765564394347,2.60896880596388));
#210759=CARTESIAN_POINT('Ctrl Pts',(61.5503317322976,13.1844534784381,2.61117187235401));
#210760=CARTESIAN_POINT('Ctrl Pts',(61.5470470005041,13.1921798155733,2.61372076577171));
#210761=CARTESIAN_POINT('Ctrl Pts',(61.5435957160157,13.19971582399,2.61659179896991));
#210762=CARTESIAN_POINT('Ctrl Pts',(61.542322401576,13.2024961535651,2.61765103591216));
#210763=CARTESIAN_POINT('Ctrl Pts',(61.5410263779726,13.2052504481944,2.61875422455157));
#210764=CARTESIAN_POINT('Ctrl Pts',(61.53970860908,13.2079776587163,2.61990022440403));
#210765=CARTESIAN_POINT('Ctrl Pts',(61.5372377924063,13.2130911784448,2.62204897412741));
#210766=CARTESIAN_POINT('Ctrl Pts',(61.5346905274442,13.2181094806068,2.62434823201777));
#210767=CARTESIAN_POINT('Ctrl Pts',(61.5320731679599,13.2230256493632,2.62679048030312));
#210768=CARTESIAN_POINT('Ctrl Pts',(61.5229124097647,13.2402322400107,2.63533834930186));
#210769=CARTESIAN_POINT('Ctrl Pts',(61.5128929892898,13.2561876955041,2.6456378478357));
#210770=CARTESIAN_POINT('Ctrl Pts',(61.5022873490355,13.2705955044755,2.65736666737972));
#210771=CARTESIAN_POINT('Ctrl Pts',(61.4969845289084,13.2777994089612,2.66323107715172));
#210772=CARTESIAN_POINT('Ctrl Pts',(61.4915351548247,13.2846164020262,2.66945281780781));
#210773=CARTESIAN_POINT('Ctrl Pts',(61.4859732907799,13.2910094216448,2.67599160631208));
#210774=CARTESIAN_POINT('Ctrl Pts',(61.4831923587575,13.2942059314541,2.67926100056422));
#210775=CARTESIAN_POINT('Ctrl Pts',(61.4803833043595,13.2972964479271,2.68260965685131));
#210776=CARTESIAN_POINT('Ctrl Pts',(61.4775503861047,13.3002763384268,2.68603254012491));
#210777=CARTESIAN_POINT('Ctrl Pts',(61.4747174678498,13.3032562289264,2.6894554233985));
#210778=CARTESIAN_POINT('Ctrl Pts',(61.4718606611378,13.3061253662368,2.69295261525394));
#210779=CARTESIAN_POINT('Ctrl Pts',(61.4689842762858,13.3088793779158,2.69651891172108));
#210780=CARTESIAN_POINT('Ctrl Pts',(61.4689597467471,13.3089028638676,2.69654932476096));
#210781=CARTESIAN_POINT('Ctrl Pts',(61.4689352159238,13.3089263414387,2.69657974261154));
#210782=CARTESIAN_POINT('Ctrl Pts',(61.4689106838182,13.3089498106271,2.69661016526982));
#210783=CARTESIAN_POINT('Ctrl Pts',(61.45638177934,13.320935867764,2.71214746101229));
#210784=CARTESIAN_POINT('Ctrl Pts',(61.4435806031503,13.3308520539316,2.72880565567773));
#210785=CARTESIAN_POINT('Ctrl Pts',(61.4306829407578,13.3387946412825,2.74628040012638));
#210786=CARTESIAN_POINT('Ctrl Pts',(61.4173490879876,13.3470058416637,2.76434612882863));
#210787=CARTESIAN_POINT('Ctrl Pts',(61.4039112193257,13.3531077791283,2.78328592655052));
#210788=CARTESIAN_POINT('Ctrl Pts',(61.3905594167301,13.3571547734334,2.80278753268603));
#210789=CARTESIAN_POINT('Ctrl Pts',(61.3774615935149,13.3611247853911,2.82191817723731));
#210790=CARTESIAN_POINT('Ctrl Pts',(61.3644457144006,13.3631169881908,2.8415909231627));
#210791=CARTESIAN_POINT('Ctrl Pts',(61.3517005934322,13.3631357189472,2.86151233818308));
#210792=CARTESIAN_POINT('Ctrl Pts',(61.3432573976137,13.3631481274166,2.87470957722185));
#210793=CARTESIAN_POINT('Ctrl Pts',(61.3349332352358,13.3622935120789,2.88801594388787));
#210794=CARTESIAN_POINT('Ctrl Pts',(61.3267881959113,13.3605623192489,2.90134173516034));
#210795=CARTESIAN_POINT('',(60.9782752797348,13.2864868028998,3.47153072139082));
#210796=CARTESIAN_POINT('',(61.3267881959113,13.3605623192489,2.90134173516034));
#210797=CARTESIAN_POINT('',(59.4519788726607,18.9827025415099,3.47153072139086));
#210798=CARTESIAN_POINT('Origin',(5.53234440788222E-15,1.85015204418142E-13,
3.47153072139072));
#210799=CARTESIAN_POINT('',(59.7908376697911,19.0928077206414,2.90134173516037));
#210800=CARTESIAN_POINT('',(59.4519788726608,18.9827025415099,3.47153072139085));
#210801=CARTESIAN_POINT('',(59.8776671349985,19.4393816709759,2.59908173516037));
#210802=CARTESIAN_POINT('Ctrl Pts',(59.7908376697911,19.0928077206414,2.90134173516037));
#210803=CARTESIAN_POINT('Ctrl Pts',(59.8025412685588,19.0966105891856,2.88164837656655));
#210804=CARTESIAN_POINT('Ctrl Pts',(59.8136038110496,19.1022557829952,2.86203734438993));
#210805=CARTESIAN_POINT('Ctrl Pts',(59.8238865403117,19.1096150844288,2.84277945977927));
#210806=CARTESIAN_POINT('Ctrl Pts',(59.834375889688,19.1171222629157,2.82313460919731));
#210807=CARTESIAN_POINT('Ctrl Pts',(59.8440546685612,19.1264133720513,2.80385576862993));
#210808=CARTESIAN_POINT('Ctrl Pts',(59.8527677431752,19.1374051938265,2.78521678517989));
#210809=CARTESIAN_POINT('Ctrl Pts',(59.861142322739,19.1479699932901,2.76730190934029));
#210810=CARTESIAN_POINT('Ctrl Pts',(59.8686254222904,19.160106528669,2.74997687279304));
#210811=CARTESIAN_POINT('Ctrl Pts',(59.8750609947968,19.1737823050951,2.73349253345219));
#210812=CARTESIAN_POINT('Ctrl Pts',(59.8800045782769,19.1842875619858,2.72082983598967));
#210813=CARTESIAN_POINT('Ctrl Pts',(59.8843297728482,19.1957019365543,2.70866321039134));
#210814=CARTESIAN_POINT('Ctrl Pts',(59.8879544940744,19.2080253553781,2.69711645335858));
#210815=CARTESIAN_POINT('Ctrl Pts',(59.8879639938223,19.2080576528611,2.69708619136764));
#210816=CARTESIAN_POINT('Ctrl Pts',(59.8879734883577,19.2080899573232,2.69705593387232));
#210817=CARTESIAN_POINT('Ctrl Pts',(59.8879829776793,19.2081222687613,2.69702568087584));
#210818=CARTESIAN_POINT('Ctrl Pts',(59.8890004259296,19.211586712012,2.69378194443279));
#210819=CARTESIAN_POINT('Ctrl Pts',(59.8899565588875,19.2151300442834,2.69059266624713));
#210820=CARTESIAN_POINT('Ctrl Pts',(59.8908500166522,19.2187475215461,2.6874621934269));
#210821=CARTESIAN_POINT('Ctrl Pts',(59.895821905966,19.2388779600025,2.67004182396195));
#210822=CARTESIAN_POINT('Ctrl Pts',(59.8988577688777,19.2613031946872,2.6544356787807));
#210823=CARTESIAN_POINT('Ctrl Pts',(59.8997541019592,19.285159834968,2.64136852353302));
#210824=CARTESIAN_POINT('Ctrl Pts',(59.9001563886589,19.2958670255031,2.63550380329822));
#210825=CARTESIAN_POINT('Ctrl Pts',(59.9001280009025,19.3068627531405,2.63014997451153));
#210826=CARTESIAN_POINT('Ctrl Pts',(59.8996517586312,19.318070849466,2.62536981119268));
#210827=CARTESIAN_POINT('Ctrl Pts',(59.8994447901818,19.3229417365281,2.62329241687088));
#210828=CARTESIAN_POINT('Ctrl Pts',(59.899153126371,19.3278525613648,2.62132362131442));
#210829=CARTESIAN_POINT('Ctrl Pts',(59.8987752905501,19.3327969595686,2.61946873372361));
#210830=CARTESIAN_POINT('Ctrl Pts',(59.8974528651773,19.3501023532816,2.61297662715581));
#210831=CARTESIAN_POINT('Ctrl Pts',(59.895074829613,19.3678190197503,2.60787989113983));
#210832=CARTESIAN_POINT('Ctrl Pts',(59.8915778894434,19.3856740904734,2.60440616886193));
#210833=CARTESIAN_POINT('Ctrl Pts',(59.8898294193586,19.394601625835,2.60266930772298));
#210834=CARTESIAN_POINT('Ctrl Pts',(59.8878012237015,19.4035637624458,2.60133820040198));
#210835=CARTESIAN_POINT('Ctrl Pts',(59.8854853982054,19.4125263941846,2.60044130723597));
#210836=CARTESIAN_POINT('Ctrl Pts',(59.8843274854574,19.417007710054,2.59999286065297));
#210837=CARTESIAN_POINT('Ctrl Pts',(59.8830976653668,19.4214891497435,2.59965296768525));
#210838=CARTESIAN_POINT('Ctrl Pts',(59.881794950565,19.4259664502057,2.59942518630967));
#210839=CARTESIAN_POINT('Ctrl Pts',(59.8804922357633,19.4304437506678,2.59919740493409));
#210840=CARTESIAN_POINT('Ctrl Pts',(59.8791166246276,19.4349169113757,2.59908173791627));
#210841=CARTESIAN_POINT('Ctrl Pts',(59.8776671349985,19.4393816709759,2.59908173516038));
#210842=CARTESIAN_POINT('',(59.8682321556242,19.4684195516699,2.59908173516038));
#210843=CARTESIAN_POINT('Origin',(5.50739376141089E-15,1.85364573392646E-13,
2.59908173516024));
#210844=CARTESIAN_POINT('',(59.5942745858235,19.6977666881848,2.90134173516037));
#210845=CARTESIAN_POINT('Ctrl Pts',(59.8682321556242,19.4684195516699,2.59908173516038));
#210846=CARTESIAN_POINT('Ctrl Pts',(59.8670503242229,19.4720538382629,2.59908174381699));
#210847=CARTESIAN_POINT('Ctrl Pts',(59.8658263391019,19.4756634078263,2.59915752001009));
#210848=CARTESIAN_POINT('Ctrl Pts',(59.8645618637724,19.4792467723414,2.59930729517484));
#210849=CARTESIAN_POINT('Ctrl Pts',(59.8572547562677,19.4999541986781,2.60017281085934));
#210850=CARTESIAN_POINT('Ctrl Pts',(59.8485963666847,19.5197897600826,2.60350651800101));
#210851=CARTESIAN_POINT('Ctrl Pts',(59.8389090368088,19.5384593694391,2.60896880596543));
#210852=CARTESIAN_POINT('Ctrl Pts',(59.8350019138237,19.5459892523658,2.61117187235522));
#210853=CARTESIAN_POINT('Ctrl Pts',(59.8309275539881,19.5533299158494,2.61372076577242));
#210854=CARTESIAN_POINT('Ctrl Pts',(59.8267074486193,19.560463883758,2.61659179896997));
#210855=CARTESIAN_POINT('Ctrl Pts',(59.8251504859514,19.5630958847952,2.61765103591222));
#210856=CARTESIAN_POINT('Ctrl Pts',(59.823573659916,19.5656996197547,2.61875422455163));
#210857=CARTESIAN_POINT('Ctrl Pts',(59.8219780387744,19.5682741459747,2.6199002244041));
#210858=CARTESIAN_POINT('Ctrl Pts',(59.8189862491339,19.5731013826371,2.62204897412747));
#210859=CARTESIAN_POINT('Ctrl Pts',(59.8159283829426,19.5778259323228,2.62434823201784));
#210860=CARTESIAN_POINT('Ctrl Pts',(59.8128114820621,19.5824415812277,2.62679048030319));
#210861=CARTESIAN_POINT('Ctrl Pts',(59.8019023289803,19.5985963523947,2.63533834930192));
#210862=CARTESIAN_POINT('Ctrl Pts',(59.7902699966956,19.6134170876084,2.64563784783576));
#210863=CARTESIAN_POINT('Ctrl Pts',(59.7782164291175,19.626637377817,2.65736666737978));
#210864=CARTESIAN_POINT('Ctrl Pts',(59.7721896453285,19.6332475229213,2.66323107715179));
#210865=CARTESIAN_POINT('Ctrl Pts',(59.766057553677,19.6394575570863,2.66945281780788));
#210866=CARTESIAN_POINT('Ctrl Pts',(59.7598579055891,19.645234181973,2.67599160631215));
#210867=CARTESIAN_POINT('Ctrl Pts',(59.7567580815451,19.6481224944163,2.67926100056428));
#210868=CARTESIAN_POINT('Ctrl Pts',(59.7536413685033,19.6509024545773,2.68260965685137));
#210869=CARTESIAN_POINT('Ctrl Pts',(59.7505124858965,19.6535699003333,2.68603254012496));
#210870=CARTESIAN_POINT('Ctrl Pts',(59.7473836032896,19.6562373460892,2.68945542339855));
#210871=CARTESIAN_POINT('Ctrl Pts',(59.7442425399497,19.6587921483498,2.69295261525399));
#210872=CARTESIAN_POINT('Ctrl Pts',(59.7410940396263,19.6612304091763,2.69651891172113));
#210873=CARTESIAN_POINT('Ctrl Pts',(59.7410671895125,19.6612512024346,2.696549324761));
#210874=CARTESIAN_POINT('Ctrl Pts',(59.7410403389972,19.6612719872239,2.69657974261158));
#210875=CARTESIAN_POINT('Ctrl Pts',(59.7410134880829,19.6612927635423,2.69661016526986));
#210876=CARTESIAN_POINT('Ctrl Pts',(59.7273003341214,19.6719035326723,2.71214746101201));
#210877=CARTESIAN_POINT('Ctrl Pts',(59.713532760413,19.6804273096593,2.7288056556771));
#210878=CARTESIAN_POINT('Ctrl Pts',(59.6998755263147,19.686978213856,2.74628040012537));
#210879=CARTESIAN_POINT('Ctrl Pts',(59.6857564136279,19.6937506652828,2.7643461288272));
#210880=CARTESIAN_POINT('Ctrl Pts',(59.6717543328707,19.6984145359348,2.78328592654863));
#210881=CARTESIAN_POINT('Ctrl Pts',(59.6580526467514,19.7010437169746,2.80278753268367));
#210882=CARTESIAN_POINT('Ctrl Pts',(59.6446115955335,19.7036228854586,2.82191817723442));
#210883=CARTESIAN_POINT('Ctrl Pts',(59.63145877687,19.7042436449213,2.84159092315926));
#210884=CARTESIAN_POINT('Ctrl Pts',(59.6187815171109,19.7029300451599,2.8615123381791));
#210885=CARTESIAN_POINT('Ctrl Pts',(59.6103832769634,19.7020598313705,2.87470957721919));
#210886=CARTESIAN_POINT('Ctrl Pts',(59.6021940468451,19.7003397858036,2.88801594388655));
#210887=CARTESIAN_POINT('Ctrl Pts',(59.5942745858236,19.6977666881848,2.90134173516037));
#210888=CARTESIAN_POINT('',(59.2554138597571,19.5876674457081,3.47153072139086));
#210889=CARTESIAN_POINT('',(59.5942745858236,19.6977666881848,2.90134173516038));
#210890=CARTESIAN_POINT('',(57.1420619865021,25.0931373005748,3.4715307213909));
#210891=CARTESIAN_POINT('Origin',(5.53234440788222E-15,1.85015204418142E-13,
3.47153072139072));
#210892=CARTESIAN_POINT('',(57.467555354514,25.2380597013433,2.90134173516042));
#210893=CARTESIAN_POINT('',(57.1420619865021,25.0931373005748,3.4715307213909));
#210894=CARTESIAN_POINT('',(57.5176823163888,25.5918112338797,2.59908173516042));
#210895=CARTESIAN_POINT('Ctrl Pts',(57.467555354514,25.2380597013433,2.90134173516042));
#210896=CARTESIAN_POINT('Ctrl Pts',(57.478797331737,25.2430650965687,2.88164837656886));
#210897=CARTESIAN_POINT('Ctrl Pts',(57.4892091890277,25.2498357159813,2.86203734439446));
#210898=CARTESIAN_POINT('Ctrl Pts',(57.4986663319526,25.2582295402783,2.84277945978591));
#210899=CARTESIAN_POINT('Ctrl Pts',(57.5083135057439,25.2667920292256,2.82313460920596));
#210900=CARTESIAN_POINT('Ctrl Pts',(57.5169680778932,25.2770439485736,2.80385576864049));
#210901=CARTESIAN_POINT('Ctrl Pts',(57.5244844631338,25.2888863202969,2.78521678519216));
#210902=CARTESIAN_POINT('Ctrl Pts',(57.5317088436217,25.3002686266143,2.7673019093538));
#210903=CARTESIAN_POINT('Ctrl Pts',(57.5378823365782,25.3131208736774,2.74997687280763));
#210904=CARTESIAN_POINT('Ctrl Pts',(57.5428531464515,25.3273944332716,2.73349253346765));
#210905=CARTESIAN_POINT('Ctrl Pts',(57.5466715501072,25.3383588864538,2.72082983599959));
#210906=CARTESIAN_POINT('Ctrl Pts',(57.5497799237789,25.3501628378305,2.70866321039607));
#210907=CARTESIAN_POINT('Ctrl Pts',(57.552096640372,25.3627976342212,2.69711645335863));
#210908=CARTESIAN_POINT('Ctrl Pts',(57.5521027120731,25.3628307477693,2.69708619136769));
#210909=CARTESIAN_POINT('Ctrl Pts',(57.5521087778605,25.3628638677134,2.69705593387237));
#210910=CARTESIAN_POINT('Ctrl Pts',(57.5521148377337,25.3628969940503,2.69702568087589));
#210911=CARTESIAN_POINT('Ctrl Pts',(57.552764579367,25.3664488110204,2.69378194443284));
#210912=CARTESIAN_POINT('Ctrl Pts',(57.5533450954513,25.3700726756556,2.69059266624717));
#210913=CARTESIAN_POINT('Ctrl Pts',(57.5538555294217,25.3737637277665,2.68746219342694));
#210914=CARTESIAN_POINT('Ctrl Pts',(57.5566959784088,25.3943035935237,2.67004182396249));
#210915=CARTESIAN_POINT('Ctrl Pts',(57.5573711352259,25.4169233145106,2.65443567878163));
#210916=CARTESIAN_POINT('Ctrl Pts',(57.5557688601538,25.4407429579385,2.64136852353417));
#210917=CARTESIAN_POINT('Ctrl Pts',(57.5550497369124,25.4514335437747,2.63550380329893));
#210918=CARTESIAN_POINT('Ctrl Pts',(57.5538721381545,25.4623660683379,2.63014997451186));
#210919=CARTESIAN_POINT('Ctrl Pts',(57.5522269397031,25.4734629846669,2.62536981119271));
#210920=CARTESIAN_POINT('Ctrl Pts',(57.5515119587092,25.4782855544061,2.62329241687091));
#210921=CARTESIAN_POINT('Ctrl Pts',(57.5507085716896,25.4831389900605,2.62132362131444));
#210922=CARTESIAN_POINT('Ctrl Pts',(57.549815975347,25.4880168077358,2.61946873372364));
#210923=CARTESIAN_POINT('Ctrl Pts',(57.5466918881476,25.5050891695995,2.61297662715584));
#210924=CARTESIAN_POINT('Ctrl Pts',(57.5424749837907,25.5224602099123,2.60787989113986));
#210925=CARTESIAN_POINT('Ctrl Pts',(57.537130837121,25.5398519389078,2.60440616886196));
#210926=CARTESIAN_POINT('Ctrl Pts',(57.5344587637862,25.5485478034055,2.60266930772301));
#210927=CARTESIAN_POINT('Ctrl Pts',(57.5315048804296,25.557248840319,2.60133820040202));
#210928=CARTESIAN_POINT('Ctrl Pts',(57.5282648911454,25.565920304143,2.60044130723602));
#210929=CARTESIAN_POINT('Ctrl Pts',(57.5266448965033,25.5702560360551,2.59999286065302));
#210930=CARTESIAN_POINT('Ctrl Pts',(57.5249533754919,25.5745843747449,2.5996529676853));
#210931=CARTESIAN_POINT('Ctrl Pts',(57.5231897917613,25.5789009773103,2.59942518630972));
#210932=CARTESIAN_POINT('Ctrl Pts',(57.5214262080306,25.5832175798758,2.59919740493414));
#210933=CARTESIAN_POINT('Ctrl Pts',(57.5195905600219,25.5875224456232,2.59908173791633));
#210934=CARTESIAN_POINT('Ctrl Pts',(57.5176823163888,25.5918112338797,2.59908173516042));
#210935=CARTESIAN_POINT('',(57.5052637377732,25.61970381813,2.59908173516043));
#210936=CARTESIAN_POINT('Origin',(5.5132234544654E-15,1.85349386523019E-13,
2.59908173516024));
#210937=CARTESIAN_POINT('',(57.2088336324698,25.8191582032623,2.90134173516042));
#210938=CARTESIAN_POINT('Ctrl Pts',(57.5052637377732,25.61970381813,2.59908173516043));
#210939=CARTESIAN_POINT('Ctrl Pts',(57.5037084941754,25.6231946607006,2.59908174381704));
#210940=CARTESIAN_POINT('Ctrl Pts',(57.5021139114133,25.6266565153805,2.59915752001015));
#210941=CARTESIAN_POINT('Ctrl Pts',(57.5004817994259,25.6300880761868,2.5993072951749));
#210942=CARTESIAN_POINT('Ctrl Pts',(57.491050205568,25.649918264356,2.60017281085936));
#210943=CARTESIAN_POINT('Ctrl Pts',(57.4803658667979,25.6687401163214,2.60350651800076));
#210944=CARTESIAN_POINT('Ctrl Pts',(57.4687800995534,25.6862948498987,2.60896880596472));
#210945=CARTESIAN_POINT('Ctrl Pts',(57.4641072931055,25.6933750777783,2.61117187235469));
#210946=CARTESIAN_POINT('Ctrl Pts',(57.4592879447655,25.7002496417677,2.61372076577214));
#210947=CARTESIAN_POINT('Ctrl Pts',(57.4543452548724,25.7069034079253,2.61659179897001));
#210948=CARTESIAN_POINT('Ctrl Pts',(57.4525217023852,25.7093582436704,2.61765103591227));
#210949=CARTESIAN_POINT('Ctrl Pts',(57.4506813499537,25.711782891895,2.61875422455167));
#210950=CARTESIAN_POINT('Ctrl Pts',(57.4488253585222,25.7141765267651,2.61990022440414));
#210951=CARTESIAN_POINT('Ctrl Pts',(57.4453453745883,25.7186645921465,2.62204897412751));
#210952=CARTESIAN_POINT('Ctrl Pts',(57.4418104097896,25.7230436262008,2.62434823201787));
#210953=CARTESIAN_POINT('Ctrl Pts',(57.4382281169313,25.7273081852389,2.62679048030323));
#210954=CARTESIAN_POINT('Ctrl Pts',(57.425690091927,25.742234141872,2.63533834930196));
#210955=CARTESIAN_POINT('Ctrl Pts',(57.4125722940993,25.7557577777295,2.64563784783579));
#210956=CARTESIAN_POINT('Ctrl Pts',(57.3992028606062,25.7676457049092,2.65736666737981));
#210957=CARTESIAN_POINT('Ctrl Pts',(57.3925181438596,25.7735896684991,2.66323107715181));
#210958=CARTESIAN_POINT('Ctrl Pts',(57.3857705191197,25.7791247053302,2.66945281780792));
#210959=CARTESIAN_POINT('Ctrl Pts',(57.3790010116303,25.7842216455739,2.67599160631219));
#210960=CARTESIAN_POINT('Ctrl Pts',(57.3756162578857,25.7867701156958,2.67926100056433));
#210961=CARTESIAN_POINT('Ctrl Pts',(57.3722260335605,25.7892090617194,2.68260965685141));
#210962=CARTESIAN_POINT('Ctrl Pts',(57.3688354672942,25.7915348376378,2.686032540125));
#210963=CARTESIAN_POINT('Ctrl Pts',(57.3654449010279,25.7938606135562,2.6894554233986));
#210964=CARTESIAN_POINT('Ctrl Pts',(57.3620539952074,25.7960730898187,2.69295261525401));
#210965=CARTESIAN_POINT('Ctrl Pts',(57.358667875041,25.7981688856969,2.69651891172116));
#210966=CARTESIAN_POINT('Ctrl Pts',(57.3586389985276,25.7981867584464,2.69654932476104));
#210967=CARTESIAN_POINT('Ctrl Pts',(57.3586101225001,25.7982046227313,2.69657974261162));
#210968=CARTESIAN_POINT('Ctrl Pts',(57.3585812469612,25.79822247855,2.6966101652699));
#210969=CARTESIAN_POINT('Ctrl Pts',(57.3438340876997,25.8073417058671,2.7121474610132));
#210970=CARTESIAN_POINT('Ctrl Pts',(57.3292509568899,25.8143796853896,2.72880565567959));
#210971=CARTESIAN_POINT('Ctrl Pts',(57.3149837825992,25.819467133355,2.74628040012926));
#210972=CARTESIAN_POINT('Ctrl Pts',(57.3002341019478,25.8247266354324,2.76434612883259));
#210973=CARTESIAN_POINT('Ctrl Pts',(57.2858212188209,25.8279013409287,2.78328592655563));
#210974=CARTESIAN_POINT('Ctrl Pts',(57.2719197677172,25.8290839028449,2.80278753269232));
#210975=CARTESIAN_POINT('Ctrl Pts',(57.2582827514651,25.8302439699451,2.82191817724463));
#210976=CARTESIAN_POINT('Ctrl Pts',(57.2451370982851,25.8294864848992,2.84159092317108));
#210977=CARTESIAN_POINT('Ctrl Pts',(57.2326665944452,25.8268549466926,2.8615123381925));
#210978=CARTESIAN_POINT('Ctrl Pts',(57.224405322849,25.8251116448887,2.87470957722821));
#210979=CARTESIAN_POINT('Ctrl Pts',(57.2164407479128,25.8225450142724,2.88801594389109));
#210980=CARTESIAN_POINT('Ctrl Pts',(57.2088336324698,25.8191582032623,2.90134173516042));
#210981=CARTESIAN_POINT('',(56.8833377255394,25.6742415049982,3.4715307213909));
#210982=CARTESIAN_POINT('',(57.2088336324698,25.8191582032623,2.90134173516042));
#210983=CARTESIAN_POINT('',(54.2060847114741,30.9286463962981,3.47153072139094));
#210984=CARTESIAN_POINT('Origin',(5.53234440788222E-15,1.85015204418142E-13,
3.47153072139072));
#210985=CARTESIAN_POINT('',(54.5146464769138,31.1067982185537,2.90134173516046));
#210986=CARTESIAN_POINT('',(54.2060847114741,30.9286463962981,3.47153072139094));
#210987=CARTESIAN_POINT('',(54.5275217339719,31.4638515574743,2.59908173516046));
#210988=CARTESIAN_POINT('Ctrl Pts',(54.5146464769138,31.1067982185537,2.90134173516046));
#210989=CARTESIAN_POINT('Ctrl Pts',(54.525303663139,31.1129513003043,2.88164837656733));
#210990=CARTESIAN_POINT('Ctrl Pts',(54.5349507607441,31.1207731649985,2.8620373443914));
#210991=CARTESIAN_POINT('Ctrl Pts',(54.5434787028964,31.1301095476656,2.84277945978138));
#210992=CARTESIAN_POINT('Ctrl Pts',(54.5521780046493,31.1396335346547,2.82313460920006));
#210993=CARTESIAN_POINT('Ctrl Pts',(54.5597135487721,31.150733942044,2.80385576863327));
#210994=CARTESIAN_POINT('Ctrl Pts',(54.5659508935503,31.1632971162157,2.78521678518377));
#210995=CARTESIAN_POINT('Ctrl Pts',(54.5719459231381,31.1753722224597,2.76730190934466));
#210996=CARTESIAN_POINT('Ctrl Pts',(54.5767421714191,31.1887993693014,2.74997687279784));
#210997=CARTESIAN_POINT('Ctrl Pts',(54.5801937574258,31.2035143279612,2.73349253345734));
#210998=CARTESIAN_POINT('Ctrl Pts',(54.5828451460238,31.2148178485853,2.720829835993));
#210999=CARTESIAN_POINT('Ctrl Pts',(54.5847026428007,31.2268820502013,2.70866321039296));
#211000=CARTESIAN_POINT('Ctrl Pts',(54.5856859723272,31.2396897946772,2.69711645335866));
#211001=CARTESIAN_POINT('Ctrl Pts',(54.5856885494585,31.2397233614914,2.69708619136772));
#211002=CARTESIAN_POINT('Ctrl Pts',(54.5856911200402,31.2397569340484,2.6970559338724));
#211003=CARTESIAN_POINT('Ctrl Pts',(54.5856936840716,31.239790512345,2.69702568087591));
#211004=CARTESIAN_POINT('Ctrl Pts',(54.5859686003825,31.2433907885846,2.69378194443287));
#211005=CARTESIAN_POINT('Ctrl Pts',(54.5861671393376,31.2470554817643,2.69059266624722));
#211006=CARTESIAN_POINT('Ctrl Pts',(54.5862889570923,31.2507796687841,2.68746219342699));
#211007=CARTESIAN_POINT('Ctrl Pts',(54.5869668451995,31.2715039227795,2.67004182395885));
#211008=CARTESIAN_POINT('Ctrl Pts',(54.5852738987617,31.2940703036778,2.65443567877506));
#211009=CARTESIAN_POINT('Ctrl Pts',(54.5811905703952,31.3175919772612,2.64136852352592));
#211010=CARTESIAN_POINT('Ctrl Pts',(54.5793579160776,31.3281488300975,2.63550380329393));
#211011=CARTESIAN_POINT('Ctrl Pts',(54.5770440083376,31.3388983725536,2.63014997450966));
#211012=CARTESIAN_POINT('Ctrl Pts',(54.5742478788459,31.3497625287428,2.62536981119277));
#211013=CARTESIAN_POINT('Ctrl Pts',(54.5730327187888,31.3544839440758,2.62329241687097));
#211014=CARTESIAN_POINT('Ctrl Pts',(54.5717264106369,31.3592268152914,2.6213236213145));
#211015=CARTESIAN_POINT('Ctrl Pts',(54.5703288332447,31.3639846100471,2.6194687337237));
#211016=CARTESIAN_POINT('Ctrl Pts',(54.5654373123719,31.3806368916921,2.6129766271559));
#211017=CARTESIAN_POINT('Ctrl Pts',(54.5594277405091,31.3974719850964,2.60787989113992));
#211018=CARTESIAN_POINT('Ctrl Pts',(54.5522949389286,31.4142098249418,2.60440616886202));
#211019=CARTESIAN_POINT('Ctrl Pts',(54.5487285381383,31.4225787448645,2.60266930772307));
#211020=CARTESIAN_POINT('Ctrl Pts',(54.5448813304464,31.4309233516995,2.60133820040207));
#211021=CARTESIAN_POINT('Ctrl Pts',(54.5407526753747,31.4392086412365,2.60044130723607));
#211022=CARTESIAN_POINT('Ctrl Pts',(54.5386883478389,31.443351286005,2.59999286065307));
#211023=CARTESIAN_POINT('Ctrl Pts',(54.5365536585648,31.4474791015107,2.59965296768534));
#211024=CARTESIAN_POINT('Ctrl Pts',(54.5343485280976,31.4515877125784,2.59942518630976));
#211025=CARTESIAN_POINT('Ctrl Pts',(54.5321433976305,31.4556963236462,2.59919740493418));
#211026=CARTESIAN_POINT('Ctrl Pts',(54.5298678244924,31.4597857294232,2.59908173791641));
#211027=CARTESIAN_POINT('Ctrl Pts',(54.5275217339719,31.4638515574743,2.59908173516046));
#211028=CARTESIAN_POINT('',(54.5122556166611,31.490293248291,2.59908173516046));
#211029=CARTESIAN_POINT('Origin',(5.52060867199534E-15,1.8533489221751E-13,
2.59908173516022));
#211030=CARTESIAN_POINT('',(54.1966007261207,31.6576696180587,2.90134173516046));
#211031=CARTESIAN_POINT('Ctrl Pts',(54.512255616661,31.490293248291,2.59908173516046));
#211032=CARTESIAN_POINT('Ctrl Pts',(54.510344000441,31.4936024004374,2.59908174381707));
#211033=CARTESIAN_POINT('Ctrl Pts',(54.5083962906204,31.4968786114295,2.59915752001018));
#211034=CARTESIAN_POINT('Ctrl Pts',(54.5064144237355,31.5001207716287,2.59930729517493));
#211035=CARTESIAN_POINT('Ctrl Pts',(54.4949616780397,31.5188564579406,2.60017281085941));
#211036=CARTESIAN_POINT('Ctrl Pts',(54.4823684499332,31.5364583843193,2.60350651800095));
#211037=CARTESIAN_POINT('Ctrl Pts',(54.4690111814096,31.5527059087838,2.60896880596516));
#211038=CARTESIAN_POINT('Ctrl Pts',(54.4636238877448,31.5592589091567,2.61117187235503));
#211039=CARTESIAN_POINT('Ctrl Pts',(54.4581123526902,31.5655920544889,2.61372076577234));
#211040=CARTESIAN_POINT('Ctrl Pts',(54.4525012314184,31.5716927188401,2.61659179897004));
#211041=CARTESIAN_POINT('Ctrl Pts',(54.4504310683346,31.5739434935989,2.61765103591229));
#211042=CARTESIAN_POINT('Ctrl Pts',(54.4483473527933,31.5761624901353,2.6187542245517));
#211043=CARTESIAN_POINT('Ctrl Pts',(54.4462513257025,31.5783490084909,2.61990022440417));
#211044=CARTESIAN_POINT('Ctrl Pts',(54.4423212749073,31.5824487304078,2.62204897412754));
#211045=CARTESIAN_POINT('Ctrl Pts',(54.4383479413154,31.5864342712172,2.62434823201791));
#211046=CARTESIAN_POINT('Ctrl Pts',(54.4343395048294,31.5903010169872,2.62679048030327));
#211047=CARTESIAN_POINT('Ctrl Pts',(54.4203099771284,31.6038346271821,2.635338349302));
#211048=CARTESIAN_POINT('Ctrl Pts',(54.4058504350957,31.6159129958989,2.64563784783584));
#211049=CARTESIAN_POINT('Ctrl Pts',(54.3913116139985,31.6263383134319,2.65736666737986));
#211050=CARTESIAN_POINT('Ctrl Pts',(54.38404220345,31.6315509721985,2.66323107715186));
#211051=CARTESIAN_POINT('Ctrl Pts',(54.3767529740104,31.6363503686739,2.66945281780794));
#211052=CARTESIAN_POINT('Ctrl Pts',(54.3694877752603,31.6407117811307,2.67599160631221));
#211053=CARTESIAN_POINT('Ctrl Pts',(54.3658551758853,31.6428924873591,2.67926100056434));
#211054=CARTESIAN_POINT('Ctrl Pts',(54.3622285842838,31.6449636976424,2.68260965685144));
#211055=CARTESIAN_POINT('Ctrl Pts',(54.3586134821116,31.6469223220355,2.68603254012503));
#211056=CARTESIAN_POINT('Ctrl Pts',(54.3549983799395,31.6488809464286,2.68945542339863));
#211057=CARTESIAN_POINT('Ctrl Pts',(54.3513947831121,31.6507268563402,2.69295261525406));
#211058=CARTESIAN_POINT('Ctrl Pts',(54.3478081421437,31.6524572252918,2.6965189117212));
#211059=CARTESIAN_POINT('Ctrl Pts',(54.3477775556079,31.652471981715,2.69654932476109));
#211060=CARTESIAN_POINT('Ctrl Pts',(54.34774697044,31.6524867297707,2.69657974261167));
#211061=CARTESIAN_POINT('Ctrl Pts',(54.3477163866431,31.6525014694577,2.69661016526995));
#211062=CARTESIAN_POINT('Ctrl Pts',(54.3320967950474,31.6600292427972,2.7121474610112));
#211063=CARTESIAN_POINT('Ctrl Pts',(54.316857882972,31.6655043152778,2.72880565567527));
#211064=CARTESIAN_POINT('Ctrl Pts',(54.3021370826389,31.6690725678673,2.74628040012244));
#211065=CARTESIAN_POINT('Ctrl Pts',(54.2869184346136,31.6727614963899,2.76434612882311));
#211066=CARTESIAN_POINT('Ctrl Pts',(54.2722526596834,31.6744122539933,2.78328592654331));
#211067=CARTESIAN_POINT('Ctrl Pts',(54.258303750805,31.6741352403916,2.80278753267708));
#211068=CARTESIAN_POINT('Ctrl Pts',(54.244620179525,31.6738634961715,2.82191817722668));
#211069=CARTESIAN_POINT('Ctrl Pts',(54.2316257183574,31.6717360657839,2.84159092315034));
#211070=CARTESIAN_POINT('Ctrl Pts',(54.2194985998879,31.6678154208183,2.86151233816903));
#211071=CARTESIAN_POINT('Ctrl Pts',(54.2114648090554,31.6652181309789,2.87470957721245));
#211072=CARTESIAN_POINT('Ctrl Pts',(54.2038121508433,31.6618330358534,2.88801594388323));
#211073=CARTESIAN_POINT('Ctrl Pts',(54.1966007261207,31.6576696180587,2.90134173516047));
#211074=CARTESIAN_POINT('',(53.888035839597,31.4795232016792,3.47153072139094));
#211075=CARTESIAN_POINT('',(54.1966007261207,31.6576696180587,2.90134173516047));
#211076=CARTESIAN_POINT('',(50.6762142289948,36.4252947698681,3.47153072139098));
#211077=CARTESIAN_POINT('Origin',(5.53234440788222E-15,1.85015204418142E-13,
3.47153072139072));
#211078=CARTESIAN_POINT('',(50.9644637245892,36.6347241449657,2.90134173516049));
#211079=CARTESIAN_POINT('',(50.6762142289948,36.4252947698681,3.47153072139097));
#211080=CARTESIAN_POINT('',(50.9399462128201,36.991167339171,2.5990817351605));
#211081=CARTESIAN_POINT('Ctrl Pts',(50.9644637245892,36.6347241449657,2.90134173516049));
#211082=CARTESIAN_POINT('Ctrl Pts',(50.9744193574537,36.6419574987897,2.88164837656693));
#211083=CARTESIAN_POINT('Ctrl Pts',(50.9831959997526,36.6507449107785,2.86203734439056));
#211084=CARTESIAN_POINT('Ctrl Pts',(50.9907013072129,36.6609215604528,2.84277945978012));
#211085=CARTESIAN_POINT('Ctrl Pts',(50.9983574255566,36.6713026986887,2.82313460919836));
#211086=CARTESIAN_POINT('Ctrl Pts',(51.0046913806542,36.6831299757322,2.80385576863117));
#211087=CARTESIAN_POINT('Ctrl Pts',(51.0095813473151,36.6962763075863,2.7852167851813));
#211088=CARTESIAN_POINT('Ctrl Pts',(51.0142813432041,36.7089119163653,2.76730190934179));
#211089=CARTESIAN_POINT('Ctrl Pts',(51.0176477981096,36.7227668523545,2.74997687279462));
#211090=CARTESIAN_POINT('Ctrl Pts',(51.0195423439511,36.7377619899128,2.73349253345383));
#211091=CARTESIAN_POINT('Ctrl Pts',(51.0209976683244,36.7492807342429,2.72082983599076));
#211092=CARTESIAN_POINT('Ctrl Pts',(51.0215839370839,36.7614730081827,2.70866321039192));
#211093=CARTESIAN_POINT('Ctrl Pts',(51.0212231059805,36.7743133764174,2.69711645335871));
#211094=CARTESIAN_POINT('Ctrl Pts',(51.0212221603065,36.7743470287326,2.69708619136776));
#211095=CARTESIAN_POINT('Ctrl Pts',(51.0212212075184,36.7743806860746,2.69705593387243));
#211096=CARTESIAN_POINT('Ctrl Pts',(51.021220247616,36.77441434844,2.69702568087595));
#211097=CARTESIAN_POINT('Ctrl Pts',(51.021117326564,36.7780236385692,2.69378194443291));
#211098=CARTESIAN_POINT('Ctrl Pts',(51.0209317131555,36.7816890091481,2.69059266624725));
#211099=CARTESIAN_POINT('Ctrl Pts',(51.0206635800337,36.7854055281044,2.68746219342702));
#211100=CARTESIAN_POINT('Ctrl Pts',(51.0191714801765,36.8060871110679,2.67004182396082));
#211101=CARTESIAN_POINT('Ctrl Pts',(51.0151289787604,36.8283529098782,2.65443567877857));
#211102=CARTESIAN_POINT('Ctrl Pts',(51.008609334902,36.8513189052307,2.64136852353032));
#211103=CARTESIAN_POINT('Ctrl Pts',(51.0056832284522,36.8616263619856,2.63550380329661));
#211104=CARTESIAN_POINT('Ctrl Pts',(51.0022583633864,36.8720751481058,2.63014997451086));
#211105=CARTESIAN_POINT('Ctrl Pts',(50.9983419378324,36.8825875141944,2.62536981119277));
#211106=CARTESIAN_POINT('Ctrl Pts',(50.9966399122601,36.8871560463068,2.62329241687097));
#211107=CARTESIAN_POINT('Ctrl Pts',(50.9948449951613,36.8917363891939,2.62132362131452));
#211108=CARTESIAN_POINT('Ctrl Pts',(50.9929577488699,36.896322033635,2.61946873372372));
#211109=CARTESIAN_POINT('Ctrl Pts',(50.98635238685,36.9123717891789,2.61297662715592));
#211110=CARTESIAN_POINT('Ctrl Pts',(50.9786159896081,36.9284864868683,2.60787989113995));
#211111=CARTESIAN_POINT('Ctrl Pts',(50.9697726815835,36.9443870542878,2.60440616886205));
#211112=CARTESIAN_POINT('Ctrl Pts',(50.9653510275712,36.9523373379975,2.6026693077231));
#211113=CARTESIAN_POINT('Ctrl Pts',(50.9606526463565,36.9602340894952,2.6013382004021));
#211114=CARTESIAN_POINT('Ctrl Pts',(50.9556805599063,36.9680424293792,2.6004413072361));
#211115=CARTESIAN_POINT('Ctrl Pts',(50.9531945166812,36.9719465993212,2.5999928606531));
#211116=CARTESIAN_POINT('Ctrl Pts',(50.9506400472468,36.9758286664323,2.59965296768539));
#211117=CARTESIAN_POINT('Ctrl Pts',(50.948017529914,36.9796842711997,2.59942518630981));
#211118=CARTESIAN_POINT('Ctrl Pts',(50.9453950125812,36.9835398759671,2.59919740493423));
#211119=CARTESIAN_POINT('Ctrl Pts',(50.9427044459694,36.9873690173882,2.59908173791644));
#211120=CARTESIAN_POINT('Ctrl Pts',(50.9399462128201,36.991167339171,2.59908173516051));
#211121=CARTESIAN_POINT('',(50.9219998155899,37.0158684358562,2.5990817351605));
#211122=CARTESIAN_POINT('Origin',(5.52946850001198E-15,1.85321249278761E-13,
2.59908173516024));
#211123=CARTESIAN_POINT('',(50.5905785208484,37.1493329797263,2.90134173516049));
#211124=CARTESIAN_POINT('Ctrl Pts',(50.9219998155899,37.0158684358562,2.5990817351605));
#211125=CARTESIAN_POINT('Ctrl Pts',(50.919752770815,37.0189596418151,2.5990817438171));
#211126=CARTESIAN_POINT('Ctrl Pts',(50.9174732734523,37.0220143142661,2.59915752001021));
#211127=CARTESIAN_POINT('Ctrl Pts',(50.9151633654183,37.0250315520726,2.59930729517496));
#211128=CARTESIAN_POINT('Ctrl Pts',(50.9018149465624,37.0424674644278,2.60017281085949));
#211129=CARTESIAN_POINT('Ctrl Pts',(50.8874508031614,37.0586566148313,2.60350651800136));
#211130=CARTESIAN_POINT('Ctrl Pts',(50.8724683783874,37.0734189189052,2.6089688059661));
#211131=CARTESIAN_POINT('Ctrl Pts',(50.866425621823,37.0793728957275,2.61117187235576));
#211132=CARTESIAN_POINT('Ctrl Pts',(50.8602822855856,37.0850952351367,2.61372076577277));
#211133=CARTESIAN_POINT('Ctrl Pts',(50.8540642095546,37.0905759575257,2.61659179897008));
#211134=CARTESIAN_POINT('Ctrl Pts',(50.851770117014,37.092598011339,2.61765103591234));
#211135=CARTESIAN_POINT('Ctrl Pts',(50.8494658679866,37.0945870443968,2.61875422455173));
#211136=CARTESIAN_POINT('Ctrl Pts',(50.8471527697479,37.0965424902854,2.6199002244042));
#211137=CARTESIAN_POINT('Ctrl Pts',(50.8428157105504,37.1002089513264,2.62204897412757));
#211138=CARTESIAN_POINT('Ctrl Pts',(50.8384475408395,37.1037573324719,2.62434823201794));
#211139=CARTESIAN_POINT('Ctrl Pts',(50.8340568779948,37.1071839000979,2.62679048030329));
#211140=CARTESIAN_POINT('Ctrl Pts',(50.8186895580383,37.1191768867891,2.63533834930203));
#211141=CARTESIAN_POINT('Ctrl Pts',(50.803046693569,37.1296776552302,2.64563784783587));
#211142=CARTESIAN_POINT('Ctrl Pts',(50.7874977752343,37.1385261411559,2.65736666737988));
#211143=CARTESIAN_POINT('Ctrl Pts',(50.7797233160669,37.1429503841188,2.66323107715189));
#211144=CARTESIAN_POINT('Ctrl Pts',(50.7719723442506,37.1469615570465,2.66945281780798));
#211145=CARTESIAN_POINT('Ctrl Pts',(50.7642910532777,37.1505396571688,2.67599160631225));
#211146=CARTESIAN_POINT('Ctrl Pts',(50.7604504077912,37.1523287072299,2.67926100056438));
#211147=CARTESIAN_POINT('Ctrl Pts',(50.75662718261,37.1540094891596,2.68260965685147));
#211148=CARTESIAN_POINT('Ctrl Pts',(50.7528271523479,37.1555795029288,2.68603254012506));
#211149=CARTESIAN_POINT('Ctrl Pts',(50.7490271220858,37.1571495166979,2.68945542339865));
#211150=CARTESIAN_POINT('Ctrl Pts',(50.7452503160124,37.1586086360832,2.69295261525409));
#211151=CARTESIAN_POINT('Ctrl Pts',(50.7415024502312,37.159954619824,2.69651891172123));
#211152=CARTESIAN_POINT('Ctrl Pts',(50.7414704887853,37.1599660982464,2.69654932476111));
#211153=CARTESIAN_POINT('Ctrl Pts',(50.7414385295747,37.1599775684901,2.6965797426117));
#211154=CARTESIAN_POINT('Ctrl Pts',(50.7414065726022,37.1599890305542,2.69661016526998));
#211155=CARTESIAN_POINT('Ctrl Pts',(50.725085680185,37.1658428740571,2.7121474610108));
#211156=CARTESIAN_POINT('Ctrl Pts',(50.7093579475521,37.1696950534567,2.72880565567438));
#211157=CARTESIAN_POINT('Ctrl Pts',(50.6943448053442,37.1717050161482,2.74628040012103));
#211158=CARTESIAN_POINT('Ctrl Pts',(50.6788239286359,37.1737829544433,2.76434612882126));
#211159=CARTESIAN_POINT('Ctrl Pts',(50.6640659432,37.1738916781079,2.78328592654098));
#211160=CARTESIAN_POINT('Ctrl Pts',(50.6502224037102,37.1721581240066,2.80278753267426));
#211161=CARTESIAN_POINT('Ctrl Pts',(50.6366421974712,37.1704575457521,2.82191817722355));
#211162=CARTESIAN_POINT('Ctrl Pts',(50.6239412983508,37.1669834785941,2.8415909231469));
#211163=CARTESIAN_POINT('Ctrl Pts',(50.6122904324984,37.1618166822747,2.8615123381653));
#211164=CARTESIAN_POINT('Ctrl Pts',(50.6045721423274,37.1583938608507,2.87470957720995));
#211165=CARTESIAN_POINT('Ctrl Pts',(50.5973152449684,37.1542273890273,2.88801594388198));
#211166=CARTESIAN_POINT('Ctrl Pts',(50.5905785208484,37.1493329797263,2.90134173516049));
#211167=CARTESIAN_POINT('',(50.3023253561995,36.9399086546489,3.47153072139098));
#211168=CARTESIAN_POINT('',(50.5905785208484,37.1493329797263,2.90134173516049));
#211169=CARTESIAN_POINT('',(46.5911245387429,41.5228599914565,3.47153072139101));
#211170=CARTESIAN_POINT('Origin',(5.53234440788222E-15,1.85015204418142E-13,
3.47153072139072));
#211171=CARTESIAN_POINT('',(46.8559036426985,41.7612723673365,2.90134173516054));
#211172=CARTESIAN_POINT('',(46.5911245387429,41.5228599914565,3.47153072139101));
#211173=CARTESIAN_POINT('',(46.7942619810916,42.1132001506003,2.59908173516053));
#211174=CARTESIAN_POINT('Ctrl Pts',(46.8559036426985,41.7612723673365,2.90134173516054));
#211175=CARTESIAN_POINT('Ctrl Pts',(46.8650486462049,41.7695067430958,2.88164837656678));
#211176=CARTESIAN_POINT('Ctrl Pts',(46.8728586744677,41.7791634256546,2.86203734439022));
#211177=CARTESIAN_POINT('Ctrl Pts',(46.8792591175168,41.7900688448325,2.84277945977961));
#211178=CARTESIAN_POINT('Ctrl Pts',(46.8857881704163,41.8011933963921,2.82313460919779));
#211179=CARTESIAN_POINT('Ctrl Pts',(46.8908511403512,41.8136179609673,2.80385576863053));
#211180=CARTESIAN_POINT('Ctrl Pts',(46.8943401533968,41.8272034165405,2.78521678518062));
#211181=CARTESIAN_POINT('Ctrl Pts',(46.8976936214484,41.8402610894801,2.76730190934118));
#211182=CARTESIAN_POINT('Ctrl Pts',(46.8995933993941,41.8543920170382,2.74997687279408));
#211183=CARTESIAN_POINT('Ctrl Pts',(46.8999101480297,41.8695030436293,2.73349253345337));
#211184=CARTESIAN_POINT('Ctrl Pts',(46.9001534633402,41.8811108098929,2.72082983599048));
#211185=CARTESIAN_POINT('Ctrl Pts',(46.8994620807994,41.8932975750526,2.70866321039181));
#211186=CARTESIAN_POINT('Ctrl Pts',(46.8977610424072,41.9060298852857,2.69711645335875));
#211187=CARTESIAN_POINT('Ctrl Pts',(46.8977565842889,41.9060632544002,2.6970861913678));
#211188=CARTESIAN_POINT('Ctrl Pts',(46.8977521185701,41.9060966277702,2.69705593387247));
#211189=CARTESIAN_POINT('Ctrl Pts',(46.8977476452509,41.9061300053926,2.69702568087599));
#211190=CARTESIAN_POINT('Ctrl Pts',(46.8972680144604,41.9097087652734,2.69378194443295));
#211191=CARTESIAN_POINT('Ctrl Pts',(46.8967002823076,41.9133346546844,2.69059266624729));
#211192=CARTESIAN_POINT('Ctrl Pts',(46.8960451360319,41.9170027866178,2.68746219342706));
#211193=CARTESIAN_POINT('Ctrl Pts',(46.8923993959693,41.9374151067975,2.6700418239636));
#211194=CARTESIAN_POINT('Ctrl Pts',(46.8860516300673,41.959136374768,2.65443567878352));
#211195=CARTESIAN_POINT('Ctrl Pts',(46.8771671013007,41.9812950716377,2.64136852353652));
#211196=CARTESIAN_POINT('Ctrl Pts',(46.8731796017524,41.9912402016588,2.6355038033004));
#211197=CARTESIAN_POINT('Ctrl Pts',(46.8686813028982,42.0012737523567,2.63014997451258));
#211198=CARTESIAN_POINT('Ctrl Pts',(46.8636874904589,42.0113191526628,2.62536981119282));
#211199=CARTESIAN_POINT('Ctrl Pts',(46.8615172471196,42.0156847477608,2.62329241687102));
#211200=CARTESIAN_POINT('Ctrl Pts',(46.8592533865613,42.0200523791243,2.62132362131456));
#211201=CARTESIAN_POINT('Ctrl Pts',(46.856897148436,42.0244156319707,2.61946873372376));
#211202=CARTESIAN_POINT('Ctrl Pts',(46.8486503149976,42.0396870169331,2.61297662715596));
#211203=CARTESIAN_POINT('Ctrl Pts',(46.8392718539638,42.0549047629076,2.60787989113997));
#211204=CARTESIAN_POINT('Ctrl Pts',(46.8288149286284,42.069793847957,2.60440616886208));
#211205=CARTESIAN_POINT('Ctrl Pts',(46.8235864659607,42.0772383904817,2.60266930772313));
#211206=CARTESIAN_POINT('Ctrl Pts',(46.8180883876711,42.0846007681801,2.60133820040213));
#211207=CARTESIAN_POINT('Ctrl Pts',(46.8123273450619,42.0918466086054,2.60044130723613));
#211208=CARTESIAN_POINT('Ctrl Pts',(46.8094468237573,42.0954695288181,2.59999286065313));
#211209=CARTESIAN_POINT('Ctrl Pts',(46.8065005614644,42.0990633147949,2.59965296768541));
#211210=CARTESIAN_POINT('Ctrl Pts',(46.8034893901146,42.1026236704492,2.59942518630983));
#211211=CARTESIAN_POINT('Ctrl Pts',(46.8004782187648,42.1061840261036,2.59919740493425));
#211212=CARTESIAN_POINT('Ctrl Pts',(46.79740213709,42.1097109502941,2.59908173791642));
#211213=CARTESIAN_POINT('Ctrl Pts',(46.7942619810916,42.1132001506003,2.59908173516054));
#211214=CARTESIAN_POINT('',(46.7738319284257,42.1358900227698,2.59908173516053));
#211215=CARTESIAN_POINT('Origin',(5.53970586838553E-15,1.85308607181667E-13,
2.59908173516024));
#211216=CARTESIAN_POINT('',(46.4302753505424,42.2339804752704,2.90134173516054));
#211217=CARTESIAN_POINT('Ctrl Pts',(46.7738319284257,42.1358900227698,2.59908173516054));
#211218=CARTESIAN_POINT('Ctrl Pts',(46.7712740741886,42.1387294146417,2.59908174381718));
#211219=CARTESIAN_POINT('Ctrl Pts',(46.7686877639338,42.1415290809211,2.59915752001025));
#211220=CARTESIAN_POINT('Ctrl Pts',(46.7660751225865,42.1442883388461,2.599307295175));
#211221=CARTESIAN_POINT('Ctrl Pts',(46.750977278643,42.1602334457376,2.60017281085945));
#211222=CARTESIAN_POINT('Ctrl Pts',(46.7349995965107,42.1748324484442,2.6035065180008));
#211223=CARTESIAN_POINT('Ctrl Pts',(46.7185561660696,42.1879477932332,2.60896880596467));
#211224=CARTESIAN_POINT('Ctrl Pts',(46.711924152309,42.1932375134913,2.61117187235468));
#211225=CARTESIAN_POINT('Ctrl Pts',(46.7052163225641,42.1982863518313,2.61372076577218));
#211226=CARTESIAN_POINT('Ctrl Pts',(46.6984594183138,42.2030870843187,2.61659179897014));
#211227=CARTESIAN_POINT('Ctrl Pts',(46.6959665308744,42.2048582631418,2.61765103591239));
#211228=CARTESIAN_POINT('Ctrl Pts',(46.6934669941953,42.2065955404586,2.61875422455181));
#211229=CARTESIAN_POINT('Ctrl Pts',(46.6909621675971,42.2082984896057,2.61990022440427));
#211230=CARTESIAN_POINT('Ctrl Pts',(46.6862656177253,42.2114915192565,2.62204897412764));
#211231=CARTESIAN_POINT('Ctrl Pts',(46.681550470477,42.2145638639316,2.624348232018));
#211232=CARTESIAN_POINT('Ctrl Pts',(46.6768256862945,42.2175127112218,2.62679048030335));
#211233=CARTESIAN_POINT('Ctrl Pts',(46.6602889416558,42.2278336767375,2.63533834930209));
#211234=CARTESIAN_POINT('Ctrl Pts',(46.6436341412466,42.2366417962862,2.64563784783592));
#211235=CARTESIAN_POINT('Ctrl Pts',(46.6272454828773,42.2438165047412,2.65736666737994));
#211236=CARTESIAN_POINT('Ctrl Pts',(46.6190511536927,42.2474038589687,2.66323107715194));
#211237=CARTESIAN_POINT('Ctrl Pts',(46.610923360769,42.2505828610986,2.66945281780803));
#211238=CARTESIAN_POINT('Ctrl Pts',(46.6029101354045,42.2533384464727,2.6759916063123));
#211239=CARTESIAN_POINT('Ctrl Pts',(46.5989035227223,42.2547162391598,2.67926100056443));
#211240=CARTESIAN_POINT('Ctrl Pts',(46.5949255520165,42.2559881777373,2.68260965685152));
#211241=CARTESIAN_POINT('Ctrl Pts',(46.5909822275911,42.2571523794831,2.68603254012511));
#211242=CARTESIAN_POINT('Ctrl Pts',(46.5870389031658,42.2583165812289,2.68945542339871));
#211243=CARTESIAN_POINT('Ctrl Pts',(46.5831302673242,42.2593729236706,2.69295261525413));
#211244=CARTESIAN_POINT('Ctrl Pts',(46.5792622391319,42.2603197753209,2.69651891172127));
#211245=CARTESIAN_POINT('Ctrl Pts',(46.5792292529523,42.2603278499825,2.69654932476115));
#211246=CARTESIAN_POINT('Ctrl Pts',(46.5791962698506,42.2603359167438,2.69657974261174));
#211247=CARTESIAN_POINT('Ctrl Pts',(46.5791632898298,42.2603439756044,2.69661016527002));
#211248=CARTESIAN_POINT('Ctrl Pts',(46.5623199117,42.2644597533374,2.71214746101394));
#211249=CARTESIAN_POINT('Ctrl Pts',(46.5462756748362,42.2666468343723,2.72880565568106));
#211250=CARTESIAN_POINT('Ctrl Pts',(46.5311346778782,42.2670764855935,2.74628040013152));
#211251=CARTESIAN_POINT('Ctrl Pts',(46.5154816224569,42.2675206673336,2.76434612883585));
#211252=CARTESIAN_POINT('Ctrl Pts',(46.5007931180894,42.2660861658586,2.78328592655997));
#211253=CARTESIAN_POINT('Ctrl Pts',(46.4872066207018,42.2629150644369,2.80278753269777));
#211254=CARTESIAN_POINT('Ctrl Pts',(46.4738785670832,42.2598042840369,2.82191817725141));
#211255=CARTESIAN_POINT('Ctrl Pts',(46.4616103837171,42.2550216427124,2.84159092317923));
#211256=CARTESIAN_POINT('Ctrl Pts',(46.4505634198054,42.2486653035374,2.861512338202));
#211257=CARTESIAN_POINT('Ctrl Pts',(46.4432451935067,42.2444544516793,2.87470957723464));
#211258=CARTESIAN_POINT('Ctrl Pts',(46.4364635650945,42.2395522518996,2.88801594389437));
#211259=CARTESIAN_POINT('Ctrl Pts',(46.4302753505424,42.2339804752704,2.90134173516054));
#211260=CARTESIAN_POINT('',(46.1654920697611,41.9955727382253,3.47153072139101));
#211261=CARTESIAN_POINT('',(46.4302753505424,42.2339804752704,2.90134173516054));
#211262=CARTESIAN_POINT('',(41.995572738225,46.1654920697615,3.47153072139104));
#211263=CARTESIAN_POINT('Origin',(5.53234440788222E-15,1.85015204418142E-13,
3.47153072139072));
#211264=CARTESIAN_POINT('',(42.23398047527,46.4302753505428,2.90134173516057));
#211265=CARTESIAN_POINT('',(41.995572738225,46.1654920697615,3.47153072139105));
#211266=CARTESIAN_POINT('',(42.1358900227694,46.773831928426,2.59908173516056));
#211267=CARTESIAN_POINT('Ctrl Pts',(42.23398047527,46.4302753505428,2.90134173516057));
#211268=CARTESIAN_POINT('Ctrl Pts',(42.2422146548459,46.4394205306929,2.8816483765676));
#211269=CARTESIAN_POINT('Ctrl Pts',(42.2489725007683,46.4498406831863,2.86203734439182));
#211270=CARTESIAN_POINT('Ctrl Pts',(42.2541979548125,46.4613553898124,2.84277945978195));
#211271=CARTESIAN_POINT('Ctrl Pts',(42.2595284085979,46.4731014717802,2.82313460920104));
#211272=CARTESIAN_POINT('Ctrl Pts',(42.2632649224119,46.4859871977567,2.80385576863465));
#211273=CARTESIAN_POINT('Ctrl Pts',(42.2653147554854,46.4998629319539,2.78521678518551));
#211274=CARTESIAN_POINT('Ctrl Pts',(42.2672849544021,46.5131996064559,2.76730190934719));
#211275=CARTESIAN_POINT('Ctrl Pts',(42.2676972410237,46.5274517041822,2.7499768728011));
#211276=CARTESIAN_POINT('Ctrl Pts',(42.2664327220898,46.5425130602354,2.73349253346124));
#211277=CARTESIAN_POINT('Ctrl Pts',(42.2654613625243,46.5540826713185,2.72082983599553));
#211278=CARTESIAN_POINT('Ctrl Pts',(42.263499903615,46.5661304069514,2.70866321039422));
#211279=CARTESIAN_POINT('Ctrl Pts',(42.2604772948659,46.5786151613303,2.69711645335877));
#211280=CARTESIAN_POINT('Ctrl Pts',(42.2604693731474,46.578647881645,2.69708619136783));
#211281=CARTESIAN_POINT('Ctrl Pts',(42.2604614434252,46.5786806053975,2.69705593387251));
#211282=CARTESIAN_POINT('Ctrl Pts',(42.2604535056997,46.5787133325846,2.69702568087603));
#211283=CARTESIAN_POINT('Ctrl Pts',(42.2596024201061,46.5822223525749,2.69378194443298));
#211284=CARTESIAN_POINT('Ctrl Pts',(42.2586587894014,46.5857690348148,2.69059266624733));
#211285=CARTESIAN_POINT('Ctrl Pts',(42.2576238078915,46.5893485909043,2.6874621934271));
#211286=CARTESIAN_POINT('Ctrl Pts',(42.2518643711132,46.609268006656,2.67004182396018));
#211287=CARTESIAN_POINT('Ctrl Pts',(42.2432808881735,46.6302067610372,2.65443567877737));
#211288=CARTESIAN_POINT('Ctrl Pts',(42.2321288152501,46.6513153841123,2.64136852352879));
#211289=CARTESIAN_POINT('Ctrl Pts',(42.2271236104851,46.6607892264664,2.63550380329572));
#211290=CARTESIAN_POINT('Ctrl Pts',(42.2216011621494,46.6702976120529,2.63014997451052));
#211291=CARTESIAN_POINT('Ctrl Pts',(42.2155846760829,46.6797659870608,2.62536981119287));
#211292=CARTESIAN_POINT('Ctrl Pts',(42.2129699926169,46.6838808147709,2.62329241687107));
#211293=CARTESIAN_POINT('Ctrl Pts',(42.210261991929,46.6879878819276,2.6213236213146));
#211294=CARTESIAN_POINT('Ctrl Pts',(42.2074625774078,46.6920809384681,2.6194687337238));
#211295=CARTESIAN_POINT('Ctrl Pts',(42.1976646265838,46.7064066363597,2.612976627156));
#211296=CARTESIAN_POINT('Ctrl Pts',(42.1867468541396,46.7205607018097,2.60787989114002));
#211297=CARTESIAN_POINT('Ctrl Pts',(42.1747908797557,46.7342751765575,2.60440616886212));
#211298=CARTESIAN_POINT('Ctrl Pts',(42.1688128925637,46.7411324139315,2.60266930772318));
#211299=CARTESIAN_POINT('Ctrl Pts',(42.1625753552954,46.74787975408,2.60133820040217));
#211300=CARTESIAN_POINT('Ctrl Pts',(42.1560884757157,46.7544837081026,2.60044130723617));
#211301=CARTESIAN_POINT('Ctrl Pts',(42.1528450359258,46.7577856851138,2.59999286065317));
#211302=CARTESIAN_POINT('Ctrl Pts',(42.1495392606405,46.7610518156852,2.59965296768545));
#211303=CARTESIAN_POINT('Ctrl Pts',(42.1461724262973,46.7642779142249,2.59942518630987));
#211304=CARTESIAN_POINT('Ctrl Pts',(42.142805591954,46.7675040127646,2.59919740493429));
#211305=CARTESIAN_POINT('Ctrl Pts',(42.1393776974108,46.770690078005,2.59908173791647));
#211306=CARTESIAN_POINT('Ctrl Pts',(42.1358900227694,46.773831928426,2.59908173516057));
#211307=CARTESIAN_POINT('',(42.1132001506,46.7942619810919,2.59908173516056));
#211308=CARTESIAN_POINT('Origin',(5.55120861436579E-15,1.85297104435686E-13,
2.59908173516022));
#211309=CARTESIAN_POINT('',(41.7612723673362,46.8559036426988,2.90134173516057));
#211310=CARTESIAN_POINT('Ctrl Pts',(42.1132001506,46.7942619810919,2.59908173516057));
#211311=CARTESIAN_POINT('Ctrl Pts',(42.1103595112871,46.7968184499055,2.59908174381712));
#211312=CARTESIAN_POINT('Ctrl Pts',(42.1074947242966,46.7993324362836,2.59915752001029));
#211313=CARTESIAN_POINT('Ctrl Pts',(42.1046079742813,46.8018034833199,2.59930729517504));
#211314=CARTESIAN_POINT('Ctrl Pts',(42.0879261203895,46.8160830868189,2.60017281085934));
#211315=CARTESIAN_POINT('Ctrl Pts',(42.0705099543567,46.8289319920994,2.60350651799969));
#211316=CARTESIAN_POINT('Ctrl Pts',(42.0527856759152,46.8402566831411,2.60896880596189));
#211317=CARTESIAN_POINT('Ctrl Pts',(42.0456370666871,46.8448241915535,2.61117187235254));
#211318=CARTESIAN_POINT('Ctrl Pts',(42.0384382358194,46.8491442126957,2.613720765771));
#211319=CARTESIAN_POINT('Ctrl Pts',(42.031216533405,46.8532123574522,2.61659179897017));
#211320=CARTESIAN_POINT('Ctrl Pts',(42.0285521636633,46.8547132558792,2.61765103591242));
#211321=CARTESIAN_POINT('Ctrl Pts',(42.0258847247795,46.8561797434811,2.61875422455182));
#211322=CARTESIAN_POINT('Ctrl Pts',(42.0232156132261,46.8576115380196,2.61990022440429));
#211323=CARTESIAN_POINT('Ctrl Pts',(42.0182110290634,46.8602961527791,2.62204897412766));
#211324=CARTESIAN_POINT('Ctrl Pts',(42.0132005644175,46.8628587997327,2.62434823201803));
#211325=CARTESIAN_POINT('Ctrl Pts',(42.0081934246215,46.865297618499,2.62679048030338));
#211326=CARTESIAN_POINT('Ctrl Pts',(41.9906684353354,46.8738334841811,2.63533834930212));
#211327=CARTESIAN_POINT('Ctrl Pts',(41.9731841724648,46.8808524512365,2.64563784783596));
#211328=CARTESIAN_POINT('Ctrl Pts',(41.9561353316316,46.8862747746136,2.65736666737997));
#211329=CARTESIAN_POINT('Ctrl Pts',(41.9476109112151,46.8889859363021,2.66323107715198));
#211330=CARTESIAN_POINT('Ctrl Pts',(41.939195346984,46.8912979378216,2.66945281780806));
#211331=CARTESIAN_POINT('Ctrl Pts',(41.930937981802,46.8932008176776,2.67599160631233));
#211332=CARTESIAN_POINT('Ctrl Pts',(41.926809299211,46.8941522576056,2.67926100056447));
#211333=CARTESIAN_POINT('Ctrl Pts',(41.92272016646,46.8950014172057,2.68260965685155));
#211334=CARTESIAN_POINT('Ctrl Pts',(41.9186767517591,46.8957470516901,2.68603254012514));
#211335=CARTESIAN_POINT('Ctrl Pts',(41.9146333370581,46.8964926861746,2.68945542339874));
#211336=CARTESIAN_POINT('Ctrl Pts',(41.9106356952805,46.8971346781639,2.69295261525418));
#211337=CARTESIAN_POINT('Ctrl Pts',(41.9066898836034,46.897672023819,2.69651891172132));
#211338=CARTESIAN_POINT('Ctrl Pts',(41.9066562340936,46.8976766062521,2.6965493247612));
#211339=CARTESIAN_POINT('Ctrl Pts',(41.9066225884706,46.8976811811499,2.69657974261178));
#211340=CARTESIAN_POINT('Ctrl Pts',(41.9065889467375,46.8976857485122,2.69661016527006));
#211341=CARTESIAN_POINT('Ctrl Pts',(41.8894076224749,46.9000183671519,2.71214746101303));
#211342=CARTESIAN_POINT('Ctrl Pts',(41.8732226654007,46.9005163877046,2.72880565567905));
#211343=CARTESIAN_POINT('Ctrl Pts',(41.858119701627,46.8993610201074,2.74628040012834));
#211344=CARTESIAN_POINT('Ctrl Pts',(41.8425059656474,46.8981665787453,2.76434612883104));
#211345=CARTESIAN_POINT('Ctrl Pts',(41.8280478726794,46.8952045688309,2.7832859265534));
#211346=CARTESIAN_POINT('Ctrl Pts',(41.8148672739051,46.8906306633424,2.8027875326894));
#211347=CARTESIAN_POINT('Ctrl Pts',(41.8019373978546,46.8861437631608,2.82191817724083));
#211348=CARTESIAN_POINT('Ctrl Pts',(41.7902363430293,46.8801049472928,2.84159092316637));
#211349=CARTESIAN_POINT('Ctrl Pts',(41.7799143139083,46.8726287066489,2.86151233818688));
#211350=CARTESIAN_POINT('Ctrl Pts',(41.7730763314897,46.8676759593275,2.87470957722448));
#211351=CARTESIAN_POINT('Ctrl Pts',(41.7668442729546,46.8620917411126,2.8880159438893));
#211352=CARTESIAN_POINT('Ctrl Pts',(41.7612723673362,46.8559036426988,2.90134173516057));
#211353=CARTESIAN_POINT('',(41.5228599914562,46.5911245387433,3.47153072139105));
#211354=CARTESIAN_POINT('',(41.7612723673362,46.8559036426988,2.90134173516057));
#211355=CARTESIAN_POINT('',(36.9399086546485,50.3023253561998,3.47153072139107));
#211356=CARTESIAN_POINT('Origin',(5.53234440788222E-15,1.85015204418142E-13,
3.47153072139072));
#211357=CARTESIAN_POINT('',(37.149332979726,50.5905785208487,2.90134173516058));
#211358=CARTESIAN_POINT('',(36.9399086546485,50.3023253561998,3.47153072139107));
#211359=CARTESIAN_POINT('',(37.0158684358559,50.9219998155902,2.59908173516059));
#211360=CARTESIAN_POINT('Ctrl Pts',(37.149332979726,50.5905785208487,2.90134173516059));
#211361=CARTESIAN_POINT('Ctrl Pts',(37.1565661199776,50.6005343088823,2.88164837656743));
#211362=CARTESIAN_POINT('Ctrl Pts',(37.1621977431859,50.6116037659393,2.86203734439147));
#211363=CARTESIAN_POINT('Ctrl Pts',(37.1661909570576,50.6236016024789,2.84277945978143));
#211364=CARTESIAN_POINT('Ctrl Pts',(37.1702644101621,50.6358405223237,2.82313460920001));
#211365=CARTESIAN_POINT('Ctrl Pts',(37.172633529828,50.6490462309924,2.80385576863314));
#211366=CARTESIAN_POINT('Ctrl Pts',(37.1732217245288,50.6630602183675,2.78521678518356));
#211367=CARTESIAN_POINT('Ctrl Pts',(37.1737870683988,50.676529775037,2.76730190934436));
#211368=CARTESIAN_POINT('Ctrl Pts',(37.172707346597,50.6907468939687,2.74997687279745));
#211369=CARTESIAN_POINT('Ctrl Pts',(37.1698754144267,50.7055935641174,2.73349253345689));
#211370=CARTESIAN_POINT('Ctrl Pts',(37.1677000224033,50.7169982609366,2.72082983599275));
#211371=CARTESIAN_POINT('Ctrl Pts',(37.1644899772797,50.7287749695264,2.7086632103929));
#211372=CARTESIAN_POINT('Ctrl Pts',(37.1601789145086,50.7408753824655,2.69711645335879));
#211373=CARTESIAN_POINT('Ctrl Pts',(37.1601676159819,50.7409070954899,2.69708619136785));
#211374=CARTESIAN_POINT('Ctrl Pts',(37.160156309136,50.7409388110965,2.69705593387252));
#211375=CARTESIAN_POINT('Ctrl Pts',(37.1601449939716,50.7409705292824,2.69702568087604));
#211376=CARTESIAN_POINT('Ctrl Pts',(37.1589317782469,50.7443713638248,2.693781944433));
#211377=CARTESIAN_POINT('Ctrl Pts',(37.1576225876056,50.7477999807009,2.69059266624734));
#211378=CARTESIAN_POINT('Ctrl Pts',(37.1562191103355,50.7512517425808,2.6874621934271));
#211379=CARTESIAN_POINT('Ctrl Pts',(37.1484090784356,50.770460012616,2.67004182395759));
#211380=CARTESIAN_POINT('Ctrl Pts',(37.1376839208933,50.7903868440317,2.65443567877273));
#211381=CARTESIAN_POINT('Ctrl Pts',(37.1243864882577,50.8102141228191,2.64136852352296));
#211382=CARTESIAN_POINT('Ctrl Pts',(37.1184184163473,50.8191128801081,2.63550380329217));
#211383=CARTESIAN_POINT('Ctrl Pts',(37.1119323236298,50.8279919247225,2.63014997450893));
#211384=CARTESIAN_POINT('Ctrl Pts',(37.1049590818166,50.8367795369357,2.62536981119286));
#211385=CARTESIAN_POINT('Ctrl Pts',(37.101928605243,50.8405985143444,2.62329241687106));
#211386=CARTESIAN_POINT('Ctrl Pts',(37.0988061338478,50.844400019407,2.6213236213146));
#211387=CARTESIAN_POINT('Ctrl Pts',(37.0955942139021,50.8481780352576,2.61946873372381));
#211388=CARTESIAN_POINT('Ctrl Pts',(37.084352494092,50.8614010907344,2.61297662715601));
#211389=CARTESIAN_POINT('Ctrl Pts',(37.0720150276372,50.874336400757,2.60787989114004));
#211390=CARTESIAN_POINT('Ctrl Pts',(37.058690996362,50.886726006548,2.60440616886214));
#211391=CARTESIAN_POINT('Ctrl Pts',(37.0520289807243,50.8929208094435,2.60266930772319));
#211392=CARTESIAN_POINT('Ctrl Pts',(37.045120324241,50.8989791867715,2.60133820040219));
#211393=CARTESIAN_POINT('Ctrl Pts',(37.0379786793009,50.904868900089,2.60044130723619));
#211394=CARTESIAN_POINT('Ctrl Pts',(37.0344078568308,50.9078137567478,2.59999286065319));
#211395=CARTESIAN_POINT('Ctrl Pts',(37.030778787319,50.9107164475037,2.59965296768547));
#211396=CARTESIAN_POINT('Ctrl Pts',(37.0270931777238,50.913572943118,2.59942518630989));
#211397=CARTESIAN_POINT('Ctrl Pts',(37.0234075681286,50.9164294387324,2.59919740493431));
#211398=CARTESIAN_POINT('Ctrl Pts',(37.0196654174469,50.9192397378252,2.59908173791651));
#211399=CARTESIAN_POINT('Ctrl Pts',(37.0158684358559,50.9219998155902,2.59908173516059));
#211400=CARTESIAN_POINT('',(36.9911673391707,50.9399462128204,2.5990817351606));
#211401=CARTESIAN_POINT('Origin',(5.56385071146069E-15,1.85286867067313E-13,
2.59908173516024));
#211402=CARTESIAN_POINT('',(36.6347241449654,50.9644637245895,2.90134173516059));
#211403=CARTESIAN_POINT('Ctrl Pts',(36.9911673391707,50.9399462128204,2.5990817351606));
#211404=CARTESIAN_POINT('Ctrl Pts',(36.9880750374206,50.9421917493682,2.59908174381721));
#211405=CARTESIAN_POINT('Ctrl Pts',(36.9849631609003,50.9443925120842,2.59915752001032));
#211406=CARTESIAN_POINT('Ctrl Pts',(36.9818339300542,50.9465482749234,2.59930729517507));
#211407=CARTESIAN_POINT('Ctrl Pts',(36.9637508360889,50.9590059247118,2.60017281085961));
#211408=CARTESIAN_POINT('Ctrl Pts',(36.9450870013071,50.9699639572759,2.6035065180015));
#211409=CARTESIAN_POINT('Ctrl Pts',(36.9262760657608,50.9793739188888,2.60896880596628));
#211410=CARTESIAN_POINT('Ctrl Pts',(36.9186891827317,50.9831691728722,2.61117187235594));
#211411=CARTESIAN_POINT('Ctrl Pts',(36.9110782226465,50.9867130457562,2.61372076577293));
#211412=CARTESIAN_POINT('Ctrl Pts',(36.9034708445587,50.9900040313324,2.61659179897021));
#211413=CARTESIAN_POINT('Ctrl Pts',(36.9006641839072,50.9912182052061,2.61765103591246));
#211414=CARTESIAN_POINT('Ctrl Pts',(36.8978580678372,50.9923978359481,2.61875422455187));
#211415=CARTESIAN_POINT('Ctrl Pts',(36.8950539146733,50.9935427888373,2.61990022440433));
#211416=CARTESIAN_POINT('Ctrl Pts',(36.8897961274911,50.9956895755044,2.6220489741277));
#211417=CARTESIAN_POINT('Ctrl Pts',(36.8845452411468,50.9977144478402,2.62434823201806));
#211418=CARTESIAN_POINT('Ctrl Pts',(36.8793106050087,50.9996165178739,2.62679048030342));
#211419=CARTESIAN_POINT('Ctrl Pts',(36.8609893785252,51.0062737629918,2.63533834930215));
#211420=CARTESIAN_POINT('Ctrl Pts',(36.8428672144359,51.0114266762821,2.64563784783598));
#211421=CARTESIAN_POINT('Ctrl Pts',(36.8253449818067,51.0150372064715,2.65736666737999));
#211422=CARTESIAN_POINT('Ctrl Pts',(36.8165838654922,51.0168424715662,2.663231077152));
#211423=CARTESIAN_POINT('Ctrl Pts',(36.8079727326367,51.0182621417029,2.6694528178081));
#211424=CARTESIAN_POINT('Ctrl Pts',(36.7995616970579,51.0192914676908,2.67599160631236));
#211425=CARTESIAN_POINT('Ctrl Pts',(36.7953561792686,51.0198061306848,2.6792610005645));
#211426=CARTESIAN_POINT('Ctrl Pts',(36.7912006858666,51.0202232077372,2.68260965685158));
#211427=CARTESIAN_POINT('Ctrl Pts',(36.7871014813876,51.0205421056329,2.68603254012517));
#211428=CARTESIAN_POINT('Ctrl Pts',(36.7830022769086,51.0208610035285,2.68945542339877));
#211429=CARTESIAN_POINT('Ctrl Pts',(36.7789594281949,51.0210816112669,2.6929526152542));
#211430=CARTESIAN_POINT('Ctrl Pts',(36.7749790641715,51.0212035636553,2.69651891172134));
#211431=CARTESIAN_POINT('Ctrl Pts',(36.7749451200025,51.0212046036538,2.69654932476122));
#211432=CARTESIAN_POINT('Ctrl Pts',(36.7749111804867,51.0212056365646,2.6965797426118));
#211433=CARTESIAN_POINT('Ctrl Pts',(36.7748772456272,51.0212066623878,2.69661016527007));
#211434=CARTESIAN_POINT('Ctrl Pts',(36.7575462174171,51.0217305652763,2.71214746101103));
#211435=CARTESIAN_POINT('Ctrl Pts',(36.7413978659101,51.0205340689296,2.72880565567476));
#211436=CARTESIAN_POINT('Ctrl Pts',(36.7264984065534,51.0178063409637,2.74628040012157));
#211437=CARTESIAN_POINT('Ctrl Pts',(36.7110950573747,51.0149863630491,2.76434612882204));
#211438=CARTESIAN_POINT('Ctrl Pts',(36.6970257816983,51.0105292970963,2.78328592654201));
#211439=CARTESIAN_POINT('Ctrl Pts',(36.6843954909359,51.0046027002071,2.80278753267555));
#211440=CARTESIAN_POINT('Ctrl Pts',(36.6720054548804,50.9987888396615,2.82191817722516));
#211441=CARTESIAN_POINT('Ctrl Pts',(36.6609997278005,50.9915600117806,2.84159092314885));
#211442=CARTESIAN_POINT('Ctrl Pts',(36.6515157237802,50.9830457809249,2.86151233816758));
#211443=CARTESIAN_POINT('Ctrl Pts',(36.6452329036075,50.9774054014754,2.87470957721151));
#211444=CARTESIAN_POINT('Ctrl Pts',(36.6396186946865,50.9712003466878,2.88801594388282));
#211445=CARTESIAN_POINT('Ctrl Pts',(36.6347241449653,50.9644637245895,2.90134173516059));
#211446=CARTESIAN_POINT('',(36.4252947698678,50.6762142289951,3.47153072139107));
#211447=CARTESIAN_POINT('',(36.6347241449653,50.9644637245895,2.90134173516059));
#211448=CARTESIAN_POINT('',(31.4795232016789,53.8880358395973,3.4715307213911));
#211449=CARTESIAN_POINT('Origin',(5.53234440788222E-15,1.85015204418142E-13,
3.47153072139072));
#211450=CARTESIAN_POINT('',(31.6576696180583,54.196600726121,2.90134173516061));
#211451=CARTESIAN_POINT('',(31.4795232016789,53.8880358395973,3.4715307213911));
#211452=CARTESIAN_POINT('',(31.4902932482907,54.5122556166613,2.59908173516061));
#211453=CARTESIAN_POINT('Ctrl Pts',(31.6576696180583,54.196600726121,2.90134173516061));
#211454=CARTESIAN_POINT('Ctrl Pts',(31.6638224711871,54.2072580443423,2.8816483765657));
#211455=CARTESIAN_POINT('Ctrl Pts',(31.668266170439,54.2188555266763,2.862037344388));
#211456=CARTESIAN_POINT('Ctrl Pts',(31.6709833936512,54.2312050423228,2.84277945977631));
#211457=CARTESIAN_POINT('Ctrl Pts',(31.6737552164697,54.2438027078783,2.82313460919356));
#211458=CARTESIAN_POINT('Ctrl Pts',(31.6747309854164,54.2571837147323,2.80385576862544));
#211459=CARTESIAN_POINT('Ctrl Pts',(31.67385109736,54.2711824151075,2.78521678517473));
#211460=CARTESIAN_POINT('Ctrl Pts',(31.6730053921571,54.2846372786627,2.76730190933514));
#211461=CARTESIAN_POINT('Ctrl Pts',(31.6704454915897,54.2986636530692,2.74997687278792));
#211462=CARTESIAN_POINT('Ctrl Pts',(31.6660771734241,54.3131329740882,2.73349253344715));
#211463=CARTESIAN_POINT('Ctrl Pts',(31.6627215829937,54.324247804397,2.72082983598652));
#211464=CARTESIAN_POINT('Ctrl Pts',(31.6582981215828,54.3356244578582,2.70866321038996));
#211465=CARTESIAN_POINT('Ctrl Pts',(31.6527458376967,54.3472079546996,2.69711645335882));
#211466=CARTESIAN_POINT('Ctrl Pts',(31.6527312861508,54.3472383129791,2.69708619136788));
#211467=CARTESIAN_POINT('Ctrl Pts',(31.6527167260613,54.3472686729571,2.69705593387255));
#211468=CARTESIAN_POINT('Ctrl Pts',(31.6527021574293,54.3472990346307,2.69702568087607));
#211469=CARTESIAN_POINT('Ctrl Pts',(31.6511401038187,54.3505544234703,2.69378194443303));
#211470=CARTESIAN_POINT('Ctrl Pts',(31.6494796970076,54.3538274103386,2.69059266624737));
#211471=CARTESIAN_POINT('Ctrl Pts',(31.6477231007679,54.3571135597835,2.68746219342714));
#211472=CARTESIAN_POINT('Ctrl Pts',(31.637948042092,54.3754002342713,2.67004182395931));
#211473=CARTESIAN_POINT('Ctrl Pts',(31.6251987170208,54.3940968201815,2.65443567877578));
#211474=CARTESIAN_POINT('Ctrl Pts',(31.6099016141321,54.4124255228606,2.64136852352678));
#211475=CARTESIAN_POINT('Ctrl Pts',(31.6030360625184,54.4206516984424,2.6355038032945));
#211476=CARTESIAN_POINT('Ctrl Pts',(31.5956573884051,54.4288041214188,2.63014997450999));
#211477=CARTESIAN_POINT('Ctrl Pts',(31.5878037911381,54.4368146919238,2.62536981119289));
#211478=CARTESIAN_POINT('Ctrl Pts',(31.5843907239925,54.4402959775155,2.62329241687109));
#211479=CARTESIAN_POINT('Ctrl Pts',(31.58088799234,54.4437502703991,2.62132362131464));
#211480=CARTESIAN_POINT('Ctrl Pts',(31.5772987574367,54.4471718528274,2.61946873372384));
#211481=CARTESIAN_POINT('Ctrl Pts',(31.5647364352753,54.4591473913265,2.61297662715605));
#211482=CARTESIAN_POINT('Ctrl Pts',(31.5511144466741,54.4707222239583,2.60787989114006));
#211483=CARTESIAN_POINT('Ctrl Pts',(31.5365683393825,54.4816512176787,2.60440616886217));
#211484=CARTESIAN_POINT('Ctrl Pts',(31.5292952857367,54.4871157145388,2.60266930772322));
#211485=CARTESIAN_POINT('Ctrl Pts',(31.5217912027244,54.4924187521965,2.60133820040221));
#211486=CARTESIAN_POINT('Ctrl Pts',(31.5140730377803,54.4975296958775,2.60044130723621));
#211487=CARTESIAN_POINT('Ctrl Pts',(31.5102139553083,54.5000851677179,2.59999286065321));
#211488=CARTESIAN_POINT('Ctrl Pts',(31.5063013524149,54.5025926161709,2.59965296768549));
#211489=CARTESIAN_POINT('Ctrl Pts',(31.5023373478778,54.5050482124963,2.59942518630991));
#211490=CARTESIAN_POINT('Ctrl Pts',(31.4983733433407,54.5075038088217,2.59919740493433));
#211491=CARTESIAN_POINT('Ctrl Pts',(31.4943579363065,54.5099075515419,2.59908173791649));
#211492=CARTESIAN_POINT('Ctrl Pts',(31.4902932482907,54.5122556166613,2.59908173516061));
#211493=CARTESIAN_POINT('',(31.4638515574739,54.5275217339722,2.59908173516062));
#211494=CARTESIAN_POINT('Origin',(5.57749365020894E-15,1.85278007239296E-13,
2.59908173516024));
#211495=CARTESIAN_POINT('',(31.1067982185534,54.5146464769141,2.90134173516061));
#211496=CARTESIAN_POINT('Ctrl Pts',(31.4638515574739,54.5275217339722,2.59908173516061));
#211497=CARTESIAN_POINT('Ctrl Pts',(31.4605414731919,54.529431735686,2.59908174381718));
#211498=CARTESIAN_POINT('Ctrl Pts',(31.457216601512,54.5312951627229,2.59915752001034));
#211499=CARTESIAN_POINT('Ctrl Pts',(31.4538791743432,54.5331120223762,2.59930729517509));
#211500=CARTESIAN_POINT('Ctrl Pts',(31.4345929624716,54.5436112298317,2.60017281085957));
#211501=CARTESIAN_POINT('Ctrl Pts',(31.4148859438265,54.5525583311779,2.60350651800109));
#211502=CARTESIAN_POINT('Ctrl Pts',(31.3951944477277,54.5599504658509,2.60896880596526));
#211503=CARTESIAN_POINT('Ctrl Pts',(31.3872524143699,54.5629318838125,2.61117187235515));
#211504=CARTESIAN_POINT('Ctrl Pts',(31.3793127123325,54.5656607810288,2.61372076577249));
#211505=CARTESIAN_POINT('Ctrl Pts',(31.3714030065918,54.568138550701,2.61659179897022));
#211506=CARTESIAN_POINT('Ctrl Pts',(31.3684848053918,54.5690526972783,2.61765103591248));
#211507=CARTESIAN_POINT('Ctrl Pts',(31.3655707565306,54.5699325468792,2.61875422455188));
#211508=CARTESIAN_POINT('Ctrl Pts',(31.3626622846451,54.5707781137756,2.61990022440434));
#211509=CARTESIAN_POINT('Ctrl Pts',(31.3572088998599,54.5723635517065,2.62204897412771));
#211510=CARTESIAN_POINT('Ctrl Pts',(31.3517751216268,54.5738284644993,2.62434823201808));
#211511=CARTESIAN_POINT('Ctrl Pts',(31.3463703409155,54.5751729463231,2.62679048030343));
#211512=CARTESIAN_POINT('Ctrl Pts',(31.3274536084259,54.5798786327062,2.63533834930216));
#211513=CARTESIAN_POINT('Ctrl Pts',(31.3088920933401,54.5831090358349,2.645637847836));
#211514=CARTESIAN_POINT('Ctrl Pts',(31.2910884461624,54.5848682151125,2.65736666738002));
#211515=CARTESIAN_POINT('Ctrl Pts',(31.2821866225735,54.5857478047513,2.66323107715202));
#211516=CARTESIAN_POINT('Ctrl Pts',(31.273474266467,54.586259589302,2.66945281780811));
#211517=CARTESIAN_POINT('Ctrl Pts',(31.2650017135576,54.586404083911,2.67599160631237));
#211518=CARTESIAN_POINT('Ctrl Pts',(31.2607654371028,54.5864763312154,2.67926100056451));
#211519=CARTESIAN_POINT('Ctrl Pts',(31.2565891115051,54.5864567561366,2.6826096568516));
#211520=CARTESIAN_POINT('Ctrl Pts',(31.2524790289902,54.5863454235315,2.6860325401252));
#211521=CARTESIAN_POINT('Ctrl Pts',(31.2483689464753,54.5862340909263,2.68945542339879));
#211522=CARTESIAN_POINT('Ctrl Pts',(31.244325185122,54.5860308973891,2.69295261525422));
#211523=CARTESIAN_POINT('Ctrl Pts',(31.2403538784534,54.585736120375,2.69651891172136));
#211524=CARTESIAN_POINT('Ctrl Pts',(31.2403200115247,54.5857336065444,2.69654932476124));
#211525=CARTESIAN_POINT('Ctrl Pts',(31.2402861499645,54.5857310861514,2.69657974261182));
#211526=CARTESIAN_POINT('Ctrl Pts',(31.240252293776,54.5857285591963,2.6966101652701));
#211527=CARTESIAN_POINT('Ctrl Pts',(31.2229614439884,54.5844380063444,2.71214746101062));
#211528=CARTESIAN_POINT('Ctrl Pts',(31.2070266227655,54.5815601021627,2.72880565567384));
#211529=CARTESIAN_POINT('Ctrl Pts',(31.1924939094189,54.577289899386,2.7462804001201));
#211530=CARTESIAN_POINT('Ctrl Pts',(31.1774697093569,54.572875281187,2.76434612881997));
#211531=CARTESIAN_POINT('Ctrl Pts',(31.1639433968999,54.5669719917423,2.78328592653931));
#211532=CARTESIAN_POINT('Ctrl Pts',(31.1520017942572,54.5597576364874,2.8027875326722));
#211533=CARTESIAN_POINT('Ctrl Pts',(31.1402873460242,54.5526805134498,2.82191817722124));
#211534=CARTESIAN_POINT('Ctrl Pts',(31.1300975277384,54.5443408741059,2.84159092314435));
#211535=CARTESIAN_POINT('Ctrl Pts',(31.1215554575517,54.5348819367323,2.86151233816251));
#211536=CARTESIAN_POINT('Ctrl Pts',(31.1158966355205,54.5286157223332,2.87470957720811));
#211537=CARTESIAN_POINT('Ctrl Pts',(31.1109617866641,54.5218578148532,2.88801594388113));
#211538=CARTESIAN_POINT('Ctrl Pts',(31.1067982185534,54.514646476914,2.90134173516061));
#211539=CARTESIAN_POINT('',(30.9286463962977,54.2060847114744,3.4715307213911));
#211540=CARTESIAN_POINT('',(31.1067982185534,54.514646476914,2.90134173516061));
#211541=CARTESIAN_POINT('',(25.6742415049979,56.8833377255397,3.47153072139112));
#211542=CARTESIAN_POINT('Origin',(5.53234440788222E-15,1.85015204418142E-13,
3.47153072139072));
#211543=CARTESIAN_POINT('',(25.8191582032619,57.2088336324701,2.90134173516063));
#211544=CARTESIAN_POINT('',(25.6742415049979,56.8833377255397,3.47153072139112));
#211545=CARTESIAN_POINT('',(25.6197038181297,57.5052637377734,2.59908173516064));
#211546=CARTESIAN_POINT('Ctrl Pts',(25.8191582032619,57.2088336324701,2.90134173516064));
#211547=CARTESIAN_POINT('Ctrl Pts',(25.8241633573214,57.220075717069,2.88164837656632));
#211548=CARTESIAN_POINT('Ctrl Pts',(25.8273704465176,57.2320741602348,2.86203734438921));
#211549=CARTESIAN_POINT('Ctrl Pts',(25.8287819086042,57.2446400511088,2.84277945977808));
#211550=CARTESIAN_POINT('Ctrl Pts',(25.8302217324661,57.2574584397136,2.82313460919575));
#211551=CARTESIAN_POINT('Ctrl Pts',(25.8297934599651,57.2708681396401,2.80385576862801));
#211552=CARTESIAN_POINT('Ctrl Pts',(25.8274551293899,57.2846981803233,2.78521678517766));
#211553=CARTESIAN_POINT('Ctrl Pts',(25.8252076408377,57.2979909364628,2.76730190933808));
#211554=CARTESIAN_POINT('Ctrl Pts',(25.8211956083118,57.3116728904502,2.74997687279086));
#211555=CARTESIAN_POINT('Ctrl Pts',(25.8153387643597,57.3256063334298,2.73349253345006));
#211556=CARTESIAN_POINT('Ctrl Pts',(25.8108397400729,57.3363095208249,2.72082983598839));
#211557=CARTESIAN_POINT('Ctrl Pts',(25.8052513267427,57.3471614741653,2.70866321039087));
#211558=CARTESIAN_POINT('Ctrl Pts',(25.798518653724,57.3581011436976,2.69711645335884));
#211559=CARTESIAN_POINT('Ctrl Pts',(25.7985010085887,57.3581298146205,2.6970861913679));
#211560=CARTESIAN_POINT('Ctrl Pts',(25.798483354779,57.3581584863396,2.69705593387257));
#211561=CARTESIAN_POINT('Ctrl Pts',(25.7984656922965,57.3581871588521,2.69702568087609));
#211562=CARTESIAN_POINT('Ctrl Pts',(25.7965719149862,57.3612614352675,2.69378194443305));
#211563=CARTESIAN_POINT('Ctrl Pts',(25.7945784837697,57.364342932599,2.6905926662474));
#211564=CARTESIAN_POINT('Ctrl Pts',(25.7924880141965,57.3674274658678,2.68746219342717));
#211565=CARTESIAN_POINT('Ctrl Pts',(25.7808550263308,57.3845921921799,2.67004182395704));
#211566=CARTESIAN_POINT('Ctrl Pts',(25.7662212180005,57.4018536888811,2.65443567877168));
#211567=CARTESIAN_POINT('Ctrl Pts',(25.7490920431143,57.4184830023538,2.64136852352162));
#211568=CARTESIAN_POINT('Ctrl Pts',(25.7414042322205,57.4259464685231,2.63550380329137));
#211569=CARTESIAN_POINT('Ctrl Pts',(25.7332138190127,57.4332829502053,2.63014997450861));
#211570=CARTESIAN_POINT('Ctrl Pts',(25.724565911951,57.4404287135114,2.62536981119292));
#211571=CARTESIAN_POINT('Ctrl Pts',(25.7208076485113,57.4435341655925,2.62329241687112));
#211572=CARTESIAN_POINT('Ctrl Pts',(25.7169630332625,57.4466034003414,2.62132362131468));
#211573=CARTESIAN_POINT('Ctrl Pts',(25.7130358078104,57.4496310617744,2.61946873372388));
#211574=CARTESIAN_POINT('Ctrl Pts',(25.699290518728,57.46022787679,2.61297662715608));
#211575=CARTESIAN_POINT('Ctrl Pts',(25.6845332533381,57.4703154157424,2.60787989114009));
#211576=CARTESIAN_POINT('Ctrl Pts',(25.6689244402255,57.47966405705,2.60440616886219));
#211577=CARTESIAN_POINT('Ctrl Pts',(25.6611200336693,57.4843383777037,2.60266930772324));
#211578=CARTESIAN_POINT('Ctrl Pts',(25.6531027404319,57.4888279745008,2.60133820040224));
#211579=CARTESIAN_POINT('Ctrl Pts',(25.6448926173141,57.4931041519766,2.60044130723624));
#211580=CARTESIAN_POINT('Ctrl Pts',(25.6407875557553,57.4952422407145,2.59999286065324));
#211581=CARTESIAN_POINT('Ctrl Pts',(25.6366342867764,57.4973269747347,2.59965296768552));
#211582=CARTESIAN_POINT('Ctrl Pts',(25.6324353177606,57.4993547677438,2.59942518630994));
#211583=CARTESIAN_POINT('Ctrl Pts',(25.6282363487449,57.5013825607529,2.59919740493437));
#211584=CARTESIAN_POINT('Ctrl Pts',(25.6239916789979,57.5033534111923,2.59908173791663));
#211585=CARTESIAN_POINT('Ctrl Pts',(25.6197038181297,57.5052637377734,2.59908173516064));
#211586=CARTESIAN_POINT('',(25.5918112338793,57.5176823163891,2.59908173516065));
#211587=CARTESIAN_POINT('Origin',(5.59198795571863E-15,1.85270622021766E-13,
2.59908173516023));
#211588=CARTESIAN_POINT('',(25.2380597013429,57.4675553545143,2.90134173516064));
#211589=CARTESIAN_POINT('Ctrl Pts',(25.5918112338793,57.5176823163891,2.59908173516064));
#211590=CARTESIAN_POINT('Ctrl Pts',(25.5883196330413,57.5192358568903,2.59908174381722));
#211591=CARTESIAN_POINT('Ctrl Pts',(25.5848181941918,57.5207415321518,2.59915752001036));
#211592=CARTESIAN_POINT('Ctrl Pts',(25.5813091362507,57.5221995827245,2.59930729517511));
#211593=CARTESIAN_POINT('Ctrl Pts',(25.5610311102461,57.5306253163333,2.60017281085954));
#211594=CARTESIAN_POINT('Ctrl Pts',(25.5404968219579,57.5374634601473,2.6035065180007));
#211595=CARTESIAN_POINT('Ctrl Pts',(25.5201405094588,57.5427567781063,2.60896880596427));
#211596=CARTESIAN_POINT('Ctrl Pts',(25.5119303403515,57.5448916950066,2.61117187235438));
#211597=CARTESIAN_POINT('Ctrl Pts',(25.503748885399,57.546775718186,2.61372076577206));
#211598=CARTESIAN_POINT('Ctrl Pts',(25.4956235123965,57.548413124991,2.61659179897022));
#211599=CARTESIAN_POINT('Ctrl Pts',(25.492625743071,57.5490172286908,2.61765103591247));
#211600=CARTESIAN_POINT('Ctrl Pts',(25.4896356883477,57.5495876573341,2.61875422455189));
#211601=CARTESIAN_POINT('Ctrl Pts',(25.4866547635673,57.55012457403,2.61990022440435));
#211602=CARTESIAN_POINT('Ctrl Pts',(25.481065529604,57.5511312928347,2.62204897412772));
#211603=CARTESIAN_POINT('Ctrl Pts',(25.4755083930936,57.5520201961936,2.62434823201809));
#211604=CARTESIAN_POINT('Ctrl Pts',(25.4699926837176,57.5527923593832,2.62679048030344));
#211605=CARTESIAN_POINT('Ctrl Pts',(25.4506877009016,57.5554949305468,2.63533834930218));
#211606=CARTESIAN_POINT('Ctrl Pts',(25.4318901986628,57.5567674305413,2.64563784783603));
#211607=CARTESIAN_POINT('Ctrl Pts',(25.4140001974206,57.5566559849707,2.65736666738005));
#211608=CARTESIAN_POINT('Ctrl Pts',(25.4050551967996,57.5566002621854,2.66323107715206));
#211609=CARTESIAN_POINT('Ctrl Pts',(25.3963370718388,57.5561985539316,2.66945281780813));
#211610=CARTESIAN_POINT('Ctrl Pts',(25.3878958286612,57.5554566340483,2.6759916063124));
#211611=CARTESIAN_POINT('Ctrl Pts',(25.3836752070724,57.5550856741067,2.67926100056454));
#211612=CARTESIAN_POINT('Ctrl Pts',(25.3795238059763,57.5546296613654,2.68260965685163));
#211613=CARTESIAN_POINT('Ctrl Pts',(25.3754478763495,57.5540893180427,2.68603254012523));
#211614=CARTESIAN_POINT('Ctrl Pts',(25.3713719467228,57.55354897472,2.68945542339882));
#211615=CARTESIAN_POINT('Ctrl Pts',(25.3673715770255,57.5529242061382,2.69295261525425));
#211616=CARTESIAN_POINT('Ctrl Pts',(25.3634528381786,57.5522159293601,2.69651891172139));
#211617=CARTESIAN_POINT('Ctrl Pts',(25.3634194195433,57.5522098892426,2.69654932476127));
#211618=CARTESIAN_POINT('Ctrl Pts',(25.3633860069332,57.5522038431597,2.69657974261185));
#211619=CARTESIAN_POINT('Ctrl Pts',(25.3633526003511,57.5521977911121,2.69661016527013));
#211620=CARTESIAN_POINT('Ctrl Pts',(25.3462913711518,57.5491069220865,2.71214746101287));
#211621=CARTESIAN_POINT('Ctrl Pts',(25.3307446654463,57.5445791409893,2.72880565567863));
#211622=CARTESIAN_POINT('Ctrl Pts',(25.3167379215565,57.5388132486358,2.74628040012763));
#211623=CARTESIAN_POINT('Ctrl Pts',(25.3022574788892,57.5328523576317,2.7643461288303));
#211624=CARTESIAN_POINT('Ctrl Pts',(25.2894223267598,57.5255675223679,2.78328592655263));
#211625=CARTESIAN_POINT('Ctrl Pts',(25.2783002469335,57.5171444507308,2.8027875326886));
#211626=CARTESIAN_POINT('Ctrl Pts',(25.2673897324687,57.5088816036403,2.82191817724038));
#211627=CARTESIAN_POINT('Ctrl Pts',(25.2581274647585,57.499522523665,2.84159092316628));
#211628=CARTESIAN_POINT('Ctrl Pts',(25.2506209171144,57.4892225138682,2.86151233818717));
#211629=CARTESIAN_POINT('Ctrl Pts',(25.245648092468,57.4823991184802,2.8747095772247));
#211630=CARTESIAN_POINT('Ctrl Pts',(25.2414466709169,57.4751623993613,2.88801594388944));
#211631=CARTESIAN_POINT('Ctrl Pts',(25.2380597013429,57.4675553545143,2.90134173516063));
#211632=CARTESIAN_POINT('',(25.0931373005745,57.1420619865024,3.47153072139112));
#211633=CARTESIAN_POINT('',(25.2380597013429,57.4675553545143,2.90134173516064));
#211634=CARTESIAN_POINT('',(19.5876674457077,59.2554138597574,3.47153072139113));
#211635=CARTESIAN_POINT('Origin',(5.53234440788222E-15,1.85015204418142E-13,
3.47153072139072));
#211636=CARTESIAN_POINT('',(19.6977666881844,59.5942745858238,2.90134173516065));
#211637=CARTESIAN_POINT('',(19.5876674457077,59.2554138597574,3.47153072139113));
#211638=CARTESIAN_POINT('',(19.4684195516695,59.8682321556244,2.59908173516065));
#211639=CARTESIAN_POINT('Ctrl Pts',(19.6977666881844,59.5942745858238,2.90134173516065));
#211640=CARTESIAN_POINT('Ctrl Pts',(19.7015693056591,59.6059782661683,2.88164837656773));
#211641=CARTESIAN_POINT('Ctrl Pts',(19.7035046472595,59.6182462127114,2.862037344392));
#211642=CARTESIAN_POINT('Ctrl Pts',(19.7035948839467,59.6308908042823,2.84277945978218));
#211643=CARTESIAN_POINT('Ctrl Pts',(19.7036869338407,59.6437894749879,2.82313460920108));
#211644=CARTESIAN_POINT('Ctrl Pts',(19.7018593121356,59.6570809485078,2.80385576863451));
#211645=CARTESIAN_POINT('Ctrl Pts',(19.6980881582811,59.6705908046785,2.7852167851852));
#211646=CARTESIAN_POINT('Ctrl Pts',(19.6944635103351,59.6835758151839,2.76730190934623));
#211647=CARTESIAN_POINT('Ctrl Pts',(19.6890433025191,59.6967634464006,2.74997687279954));
#211648=CARTESIAN_POINT('Ctrl Pts',(19.6817621015892,59.7100083536232,2.73349253345916));
#211649=CARTESIAN_POINT('Ctrl Pts',(19.6761689356969,59.7201826317454,2.72082983599423));
#211650=CARTESIAN_POINT('Ctrl Pts',(19.6694767982722,59.7303909886949,2.70866321039365));
#211651=CARTESIAN_POINT('Ctrl Pts',(19.661637500694,59.740566973611,2.69711645335886));
#211652=CARTESIAN_POINT('Ctrl Pts',(19.6616169552931,59.7405936430526,2.69708619136792));
#211653=CARTESIAN_POINT('Ctrl Pts',(19.6615964011821,59.7406203123795,2.69705593387259));
#211654=CARTESIAN_POINT('Ctrl Pts',(19.6615758383628,59.7406469815888,2.69702568087611));
#211655=CARTESIAN_POINT('Ctrl Pts',(19.6593710859735,59.7435064631644,2.69378194443307));
#211656=CARTESIAN_POINT('Ctrl Pts',(19.6570664708011,59.7463627094293,2.69059266624741));
#211657=CARTESIAN_POINT('Ctrl Pts',(19.6546650315164,59.7492118317302,2.68746219342718));
#211658=CARTESIAN_POINT('Ctrl Pts',(19.6413015679148,59.765066549527,2.67004182396116));
#211659=CARTESIAN_POINT('Ctrl Pts',(19.6249436073983,59.780703836443,2.65443567877906));
#211660=CARTESIAN_POINT('Ctrl Pts',(19.6061700313475,59.7954515664656,2.64136852353089));
#211661=CARTESIAN_POINT('Ctrl Pts',(19.5977441904329,59.8020705519314,2.63550380329702));
#211662=CARTESIAN_POINT('Ctrl Pts',(19.5888317740052,59.8085107122966,2.63014997451115));
#211663=CARTESIAN_POINT('Ctrl Pts',(19.5794843054211,59.8147133779312,2.62536981119295));
#211664=CARTESIAN_POINT('Ctrl Pts',(19.5754220220079,59.817408972519,2.62329241687115));
#211665=CARTESIAN_POINT('Ctrl Pts',(19.571277645572,59.820059521955,2.62132362131469));
#211666=CARTESIAN_POINT('Ctrl Pts',(19.5670554570749,59.8226600907005,2.61946873372389));
#211667=CARTESIAN_POINT('Ctrl Pts',(19.5522777973353,59.8317620813097,2.61297662715609));
#211668=CARTESIAN_POINT('Ctrl Pts',(19.5365469388443,59.840251805395,2.60787989114011));
#211669=CARTESIAN_POINT('Ctrl Pts',(19.5200464333337,59.8479176686192,2.60440616886221));
#211670=CARTESIAN_POINT('Ctrl Pts',(19.5117961805784,59.8517506002313,2.60266930772326));
#211671=CARTESIAN_POINT('Ctrl Pts',(19.5033535162583,59.8553775672057,2.60133820040226));
#211672=CARTESIAN_POINT('Ctrl Pts',(19.4947413867938,59.8587721277811,2.60044130723625));
#211673=CARTESIAN_POINT('Ctrl Pts',(19.4904353220616,59.8604694080689,2.59999286065325));
#211674=CARTESIAN_POINT('Ctrl Pts',(19.4860868910813,59.8621085868741,2.59965296768554));
#211675=CARTESIAN_POINT('Ctrl Pts',(19.4816989623701,59.8636863596424,2.59942518630996));
#211676=CARTESIAN_POINT('Ctrl Pts',(19.4773110336589,59.8652641324107,2.59919740493438));
#211677=CARTESIAN_POINT('Ctrl Pts',(19.4728836066891,59.8667804975195,2.5990817379166));
#211678=CARTESIAN_POINT('Ctrl Pts',(19.4684195516695,59.8682321556244,2.59908173516065));
#211679=CARTESIAN_POINT('',(19.4393816709755,59.8776671349988,2.59908173516066));
#211680=CARTESIAN_POINT('Origin',(5.60717482534548E-15,1.85264792328712E-13,
2.59908173516023));
#211681=CARTESIAN_POINT('',(19.092807720641,59.7908376697914,2.90134173516065));
#211682=CARTESIAN_POINT('Ctrl Pts',(19.4393816709755,59.8776671349988,2.59908173516065));
#211683=CARTESIAN_POINT('Ctrl Pts',(19.435746808291,59.8788471933726,2.59908174381724));
#211684=CARTESIAN_POINT('Ctrl Pts',(19.4321071647686,59.8799786203653,2.59915752001037));
#211685=CARTESIAN_POINT('Ctrl Pts',(19.4284649220283,59.8810618871503,2.59930729517512));
#211686=CARTESIAN_POINT('Ctrl Pts',(19.4074172521858,59.8873218328124,2.60017281085955));
#211687=CARTESIAN_POINT('Ctrl Pts',(19.3862806722129,59.8919760989601,2.60350651800072));
#211688=CARTESIAN_POINT('Ctrl Pts',(19.3654825713317,59.8951126055062,2.6089688059643));
#211689=CARTESIAN_POINT('Ctrl Pts',(19.3570942188071,59.8963776307484,2.61117187235441));
#211690=CARTESIAN_POINT('Ctrl Pts',(19.3487606486731,59.8973961381381,2.61372076577208));
#211691=CARTESIAN_POINT('Ctrl Pts',(19.3405086316971,59.8981752423039,2.61659179897023));
#211692=CARTESIAN_POINT('Ctrl Pts',(19.3374641384343,59.8984626844396,2.61765103591249));
#211693=CARTESIAN_POINT('Ctrl Pts',(19.3344308375141,59.8987174423899,2.61875422455189));
#211694=CARTESIAN_POINT('Ctrl Pts',(19.3314101194744,59.8989398263135,2.61990022440436));
#211695=CARTESIAN_POINT('Ctrl Pts',(19.32574627315,59.8993567961702,2.62204897412773));
#211696=CARTESIAN_POINT('Ctrl Pts',(19.3201266635128,59.8996599510839,2.6243482320181));
#211697=CARTESIAN_POINT('Ctrl Pts',(19.3145604567382,59.8998513356578,2.62679048030346));
#211698=CARTESIAN_POINT('Ctrl Pts',(19.2950787330274,59.9005211816666,2.63533834930219));
#211699=CARTESIAN_POINT('Ctrl Pts',(19.2762511930037,59.8998218367508,2.64563784783603));
#211700=CARTESIAN_POINT('Ctrl Pts',(19.2584708442945,59.8978409873529,2.65736666738005));
#211701=CARTESIAN_POINT('Ctrl Pts',(19.2495806699398,59.896850562654,2.66323107715206));
#211702=CARTESIAN_POINT('Ctrl Pts',(19.2409522937263,59.8955397627953,2.66945281780814));
#211703=CARTESIAN_POINT('Ctrl Pts',(19.2326348443073,59.8939195570494,2.67599160631241));
#211704=CARTESIAN_POINT('Ctrl Pts',(19.2284761195978,59.8931094541765,2.67926100056455));
#211705=CARTESIAN_POINT('Ctrl Pts',(19.2243951266223,59.8922219999437,2.68260965685163));
#211706=CARTESIAN_POINT('Ctrl Pts',(19.2203980066217,59.891258566018,2.68603254012523));
#211707=CARTESIAN_POINT('Ctrl Pts',(19.2164008866211,59.8902951320923,2.68945542339882));
#211708=CARTESIAN_POINT('Ctrl Pts',(19.2124877374673,59.8892556335612,2.69295261525426));
#211709=CARTESIAN_POINT('Ctrl Pts',(19.208664500965,59.8881416170478,2.6965189117214));
#211710=CARTESIAN_POINT('Ctrl Pts',(19.2086318967648,59.8881321168201,2.69654932476128));
#211711=CARTESIAN_POINT('Ctrl Pts',(19.2085992991801,59.8881226112894,2.69657974261186));
#211712=CARTESIAN_POINT('Ctrl Pts',(19.208566708214,59.888113100457,2.69661016527014));
#211713=CARTESIAN_POINT('Ctrl Pts',(19.1919220260051,59.8832557794662,2.71214746101075));
#211714=CARTESIAN_POINT('Ctrl Pts',(19.1769337687821,59.8771277287724,2.72880565567407));
#211715=CARTESIAN_POINT('Ctrl Pts',(19.1636064551693,59.8699293191676,2.74628040012045));
#211716=CARTESIAN_POINT('Ctrl Pts',(19.1498284206598,59.86248746413,2.76434612882027));
#211717=CARTESIAN_POINT('Ctrl Pts',(19.137825053473,59.8539008972299,2.78328592653955));
#211718=CARTESIAN_POINT('Ctrl Pts',(19.1276443522983,59.8443613941499,2.80278753267238));
#211719=CARTESIAN_POINT('Ctrl Pts',(19.1176573094823,59.8350033524917,2.82191817722113));
#211720=CARTESIAN_POINT('Ctrl Pts',(19.109424071691,59.8247273719278,2.84159092314393));
#211721=CARTESIAN_POINT('Ctrl Pts',(19.1030352898954,59.8136991387748,2.86151233816177));
#211722=CARTESIAN_POINT('Ctrl Pts',(19.0988029459333,59.806393320938,2.87470957720763));
#211723=CARTESIAN_POINT('Ctrl Pts',(19.0953809833349,59.7987570771806,2.8880159438809));
#211724=CARTESIAN_POINT('Ctrl Pts',(19.092807720641,59.7908376697914,2.90134173516065));
#211725=CARTESIAN_POINT('',(18.9827025415095,59.451978872661,3.47153072139113));
#211726=CARTESIAN_POINT('',(19.092807720641,59.7908376697914,2.90134173516065));
#211727=CARTESIAN_POINT('',(13.2864868028994,60.978275279735,3.47153072139114));
#211728=CARTESIAN_POINT('Origin',(5.53234440788222E-15,1.85015204418142E-13,
3.47153072139072));
#211729=CARTESIAN_POINT('',(13.3605623192485,61.3267881959115,2.90134173516065));
#211730=CARTESIAN_POINT('',(13.2864868028994,60.978275279735,3.47153072139114));
#211731=CARTESIAN_POINT('',(13.1038352065726,61.5752716937453,2.59908173516066));
#211732=CARTESIAN_POINT('Ctrl Pts',(13.3605623192485,61.3267881959115,2.90134173516065));
#211733=CARTESIAN_POINT('Ctrl Pts',(13.3631207378658,61.3388252440315,2.88164837656783));
#211734=CARTESIAN_POINT('Ctrl Pts',(13.3637631278629,61.3512282837631,2.8620373443922));
#211735=CARTESIAN_POINT('Ctrl Pts',(13.3625311504985,61.3638130392405,2.84277945978247));
#211736=CARTESIAN_POINT('Ctrl Pts',(13.3612744179065,61.3766506715123,2.82313460920144));
#211737=CARTESIAN_POINT('Ctrl Pts',(13.3580674708028,61.3896782944613,2.80385576863494));
#211738=CARTESIAN_POINT('Ctrl Pts',(13.3529048112192,61.402719949309,2.7852167851857));
#211739=CARTESIAN_POINT('Ctrl Pts',(13.3479427162803,61.4152549476886,2.76730190934671));
#211740=CARTESIAN_POINT('Ctrl Pts',(13.3411737181046,61.4278037696881,2.74997687279999));
#211741=CARTESIAN_POINT('Ctrl Pts',(13.3325479345572,61.4402150271791,2.73349253345958));
#211742=CARTESIAN_POINT('Ctrl Pts',(13.3259219069559,61.4497489245058,2.7208298359945));
#211743=CARTESIAN_POINT('Ctrl Pts',(13.3181993658957,61.4592018401669,2.70866321039379));
#211744=CARTESIAN_POINT('Ctrl Pts',(13.3093393327442,61.4685026502441,2.69711645335887));
#211745=CARTESIAN_POINT('Ctrl Pts',(13.3093161121774,61.4685270260086,2.69708619136793));
#211746=CARTESIAN_POINT('Ctrl Pts',(13.3092928829602,61.4685514007484,2.69705593387261));
#211747=CARTESIAN_POINT('Ctrl Pts',(13.3092696450948,61.4685757744611,2.69702568087613));
#211748=CARTESIAN_POINT('Ctrl Pts',(13.3067780733549,61.4711891321183,2.69378194443309));
#211749=CARTESIAN_POINT('Ctrl Pts',(13.3041875240728,61.4737888336849,2.69059266624742));
#211750=CARTESIAN_POINT('Ctrl Pts',(13.301501425748,61.4763713294376,2.68746219342719));
#211751=CARTESIAN_POINT('Ctrl Pts',(13.2865538993128,61.4907423311159,2.67004182396279));
#211752=CARTESIAN_POINT('Ctrl Pts',(13.2686510078465,61.5045840828619,2.65443567878197));
#211753=CARTESIAN_POINT('Ctrl Pts',(13.248438717856,61.5172886502207,2.64136852353454));
#211754=CARTESIAN_POINT('Ctrl Pts',(13.2393671621987,61.5229906359903,2.63550380329926));
#211755=CARTESIAN_POINT('Ctrl Pts',(13.2298303888527,61.5284639152911,2.63014997451216));
#211756=CARTESIAN_POINT('Ctrl Pts',(13.2198857715705,61.533655525549,2.62536981119297));
#211757=CARTESIAN_POINT('Ctrl Pts',(13.215563975411,61.535911729145,2.62329241687117));
#211758=CARTESIAN_POINT('Ctrl Pts',(13.2111652444435,61.5381145532938,2.62132362131472));
#211759=CARTESIAN_POINT('Ctrl Pts',(13.2066943520822,61.5402595369764,2.61946873372392));
#211760=CARTESIAN_POINT('Ctrl Pts',(13.1910462288177,61.5477669798655,2.61297662715612));
#211761=CARTESIAN_POINT('Ctrl Pts',(13.1745141278034,61.55456587389,2.60787989114012));
#211762=CARTESIAN_POINT('Ctrl Pts',(13.1573027128859,61.5604649702292,2.60440616886222));
#211763=CARTESIAN_POINT('Ctrl Pts',(13.1486970054272,61.5634145183988,2.60266930772327));
#211764=CARTESIAN_POINT('Ctrl Pts',(13.1399214696215,61.5661391177413,2.60133820040227));
#211765=CARTESIAN_POINT('Ctrl Pts',(13.1310016901029,61.5686148699004,2.60044130723627));
#211766=CARTESIAN_POINT('Ctrl Pts',(13.1265418003436,61.5698527459799,2.59999286065327));
#211767=CARTESIAN_POINT('Ctrl Pts',(13.1220458496817,61.5710284103841,2.59965296768555));
#211768=CARTESIAN_POINT('Ctrl Pts',(13.1175170363402,61.572138876503,2.59942518630997));
#211769=CARTESIAN_POINT('Ctrl Pts',(13.1129882229987,61.5732493426219,2.59919740493439));
#211770=CARTESIAN_POINT('Ctrl Pts',(13.1084265466226,61.5742946087866,2.59908173791658));
#211771=CARTESIAN_POINT('Ctrl Pts',(13.1038352065726,61.5752716937454,2.59908173516066));
#211772=CARTESIAN_POINT('',(13.0739701745323,61.58161970227,2.59908173516067));
#211773=CARTESIAN_POINT('Origin',(5.62288786856779E-15,1.8526058203147E-13,
2.59908173516022));
#211774=CARTESIAN_POINT('',(12.7383709431249,61.4590390555211,2.90134173516066));
#211775=CARTESIAN_POINT('Ctrl Pts',(13.0739701745323,61.58161970227,2.59908173516067));
#211776=CARTESIAN_POINT('Ctrl Pts',(13.0702318743176,61.58241334955,2.59908174381723));
#211777=CARTESIAN_POINT('Ctrl Pts',(13.0664939028184,61.583158132123,2.59915752001038));
#211778=CARTESIAN_POINT('Ctrl Pts',(13.0627583804525,61.5838547466228,2.59930729517513));
#211779=CARTESIAN_POINT('Ctrl Pts',(13.0411716694464,61.5878803190637,2.6001728108596));
#211780=CARTESIAN_POINT('Ctrl Pts',(13.0196643745811,61.5902997144312,2.60350651800106));
#211781=CARTESIAN_POINT('Ctrl Pts',(12.9986523536623,61.5912450453421,2.60896880596512));
#211782=CARTESIAN_POINT('Ctrl Pts',(12.990177722267,61.5916263190448,2.61117187235505));
#211783=CARTESIAN_POINT('Ctrl Pts',(12.981783341291,61.5917681516649,2.61372076577245));
#211784=CARTESIAN_POINT('Ctrl Pts',(12.9734950911672,61.5916804171631,2.61659179897026));
#211785=CARTESIAN_POINT('Ctrl Pts',(12.9704372300723,61.5916480484586,2.61765103591252));
#211786=CARTESIAN_POINT('Ctrl Pts',(12.9673939164349,61.5915843445343,2.61875422455192));
#211787=CARTESIAN_POINT('Ctrl Pts',(12.9643665007549,61.5914897592008,2.61990022440438));
#211788=CARTESIAN_POINT('Ctrl Pts',(12.9586900963549,61.5913124117006,2.62204897412776));
#211789=CARTESIAN_POINT('Ctrl Pts',(12.95306958321,61.5910264967404,2.62434823201813));
#211790=CARTESIAN_POINT('Ctrl Pts',(12.9475138635632,61.5906350058493,2.62679048030348));
#211791=CARTESIAN_POINT('Ctrl Pts',(12.9280688447993,61.5892647877302,2.63533834930222));
#211792=CARTESIAN_POINT('Ctrl Pts',(12.9094175454592,61.5866012600732,2.64563784783605));
#211793=CARTESIAN_POINT('Ctrl Pts',(12.8919416545041,61.5827727094487,2.65736666738007));
#211794=CARTESIAN_POINT('Ctrl Pts',(12.8832037090265,61.5808584341364,2.66323107715207));
#211795=CARTESIAN_POINT('Ctrl Pts',(12.8747596158555,61.5786529040704,2.66945281780816));
#211796=CARTESIAN_POINT('Ctrl Pts',(12.8666570879116,61.576172163775,2.67599160631243));
#211797=CARTESIAN_POINT('Ctrl Pts',(12.8626058239396,61.5749317936274,2.67926100056456));
#211798=CARTESIAN_POINT('Ctrl Pts',(12.8586399512977,61.5736226210374,2.68260965685165));
#211799=CARTESIAN_POINT('Ctrl Pts',(12.8547654342064,61.5722466520924,2.68603254012524));
#211800=CARTESIAN_POINT('Ctrl Pts',(12.8508909171151,61.5708706831473,2.68945542339884));
#211801=CARTESIAN_POINT('Ctrl Pts',(12.8471078617859,61.5694278436304,2.69295261525427));
#211802=CARTESIAN_POINT('Ctrl Pts',(12.8434220158074,61.5679202927798,2.69651891172141));
#211803=CARTESIAN_POINT('Ctrl Pts',(12.8433905832605,61.5679074365283,2.69654932476129));
#211804=CARTESIAN_POINT('Ctrl Pts',(12.8433591578474,61.5678945756945,2.69657974261187));
#211805=CARTESIAN_POINT('Ctrl Pts',(12.8433277395707,61.5678817102798,2.69661016527015));
#211806=CARTESIAN_POINT('Ctrl Pts',(12.8272819669693,61.561311155148,2.71214746101265));
#211807=CARTESIAN_POINT('Ctrl Pts',(12.8130163727079,61.5536499750614,2.72880565567815));
#211808=CARTESIAN_POINT('Ctrl Pts',(12.8005145062065,61.5450979154849,2.74628040012685));
#211809=CARTESIAN_POINT('Ctrl Pts',(12.7875898348814,61.5362566309324,2.76434612882922));
#211810=CARTESIAN_POINT('Ctrl Pts',(12.7765497640381,61.5264624086165,2.78328592655123));
#211811=CARTESIAN_POINT('Ctrl Pts',(12.7674219834068,61.515910990882,2.80278753268687));
#211812=CARTESIAN_POINT('Ctrl Pts',(12.7584678323699,61.5055602833153,2.82191817723828));
#211813=CARTESIAN_POINT('Ctrl Pts',(12.7513538295739,61.4944799879523,2.84159092316381));
#211814=CARTESIAN_POINT('Ctrl Pts',(12.7461528104582,61.4828443590693,2.86151233818433));
#211815=CARTESIAN_POINT('Ctrl Pts',(12.7427073176334,61.4751361628607,2.87470957722279));
#211816=CARTESIAN_POINT('Ctrl Pts',(12.7401023057312,61.4671840587583,2.8880159438885));
#211817=CARTESIAN_POINT('Ctrl Pts',(12.7383709431249,61.4590390555211,2.90134173516065));
#211818=CARTESIAN_POINT('',(12.664289321014,61.1105274371643,3.47153072139115));
#211819=CARTESIAN_POINT('',(12.7383709431249,61.4590390555211,2.90134173516066));
#211820=CARTESIAN_POINT('',(6.8397366303024,62.0330459552234,3.47153072139115));
#211821=CARTESIAN_POINT('Origin',(5.53234440788222E-15,1.85015204418142E-13,
3.47153072139072));
#211822=CARTESIAN_POINT('',(6.87697683366544,62.3873926810693,2.90134173516067));
#211823=CARTESIAN_POINT('',(6.8397366303024,62.0330459552234,3.47153072139115));
#211824=CARTESIAN_POINT('',(6.59568250079865,62.6076796697356,2.59908173516067));
#211825=CARTESIAN_POINT('Ctrl Pts',(6.87697683366544,62.3873926810693,2.90134173516067));
#211826=CARTESIAN_POINT('Ctrl Pts',(6.87826302285572,62.3996312165481,2.88164837656554));
#211827=CARTESIAN_POINT('Ctrl Pts',(6.87760542308992,62.412033459171,2.86203734438761));
#211828=CARTESIAN_POINT('Ctrl Pts',(6.8750647294751,62.424420497342,2.8427794597757));
#211829=CARTESIAN_POINT('Ctrl Pts',(6.87247298342164,62.4370564393959,2.82313460919239));
#211830=CARTESIAN_POINT('Ctrl Pts',(6.86792184690156,62.4496774784122,2.80385576862372));
#211831=CARTESIAN_POINT('Ctrl Pts',(6.86142424476594,62.4621080448389,2.78521678517253));
#211832=CARTESIAN_POINT('Ctrl Pts',(6.85517906858305,62.4740556950285,2.76730190933172));
#211833=CARTESIAN_POINT('Ctrl Pts',(6.84713544260611,62.4858282202922,2.74997687278339));
#211834=CARTESIAN_POINT('Ctrl Pts',(6.83725958232828,62.4972698477185,2.73349253344165));
#211835=CARTESIAN_POINT('Ctrl Pts',(6.82967328916546,62.506058908871,2.72082983598302));
#211836=CARTESIAN_POINT('Ctrl Pts',(6.82100495424929,62.5146528151173,2.70866321038834));
#211837=CARTESIAN_POINT('Ctrl Pts',(6.8112212579066,62.52297654873,2.69711645335888));
#211838=CARTESIAN_POINT('Ctrl Pts',(6.8111956165833,62.5229983637513,2.69708619136794));
#211839=CARTESIAN_POINT('Ctrl Pts',(6.8111699667641,62.5230201768494,2.69705593387261));
#211840=CARTESIAN_POINT('Ctrl Pts',(6.81114430845136,62.5230419880219,2.69702568087613));
#211841=CARTESIAN_POINT('Ctrl Pts',(6.80839321554227,62.5253805892673,2.69378194443309));
#211842=CARTESIAN_POINT('Ctrl Pts',(6.80554511475049,62.5276952632613,2.69059266624743));
#211843=CARTESIAN_POINT('Ctrl Pts',(6.80260378684096,62.529982838102,2.6874621934272));
#211844=CARTESIAN_POINT('Ctrl Pts',(6.78623596579732,62.5427126719625,2.67004182396155));
#211845=CARTESIAN_POINT('Ctrl Pts',(6.7669842912032,62.5546072354118,2.65443567877975));
#211846=CARTESIAN_POINT('Ctrl Pts',(6.74555473734773,62.56512944621,2.64136852353176));
#211847=CARTESIAN_POINT('Ctrl Pts',(6.73593685681286,62.5698519601318,2.63550380329757));
#211848=CARTESIAN_POINT('Ctrl Pts',(6.72588021343625,62.5742983919729,2.63014997451141));
#211849=CARTESIAN_POINT('Ctrl Pts',(6.71544740276757,62.5784220664836,2.62536981119299));
#211850=CARTESIAN_POINT('Ctrl Pts',(6.71091344436492,62.5802141596492,2.62329241687119));
#211851=CARTESIAN_POINT('Ctrl Pts',(6.70630855228275,62.5819451239084,2.62132362131473));
#211852=CARTESIAN_POINT('Ctrl Pts',(6.70163794008956,62.583611021638,2.61946873372393));
#211853=CARTESIAN_POINT('Ctrl Pts',(6.68529079741337,62.5894416636915,2.61297662715612));
#211854=CARTESIAN_POINT('Ctrl Pts',(6.66813858303384,62.5944752375496,2.60787989114014));
#211855=CARTESIAN_POINT('Ctrl Pts',(6.65040483057318,62.5985429352698,2.60440616886224));
#211856=CARTESIAN_POINT('Ctrl Pts',(6.64153795434285,62.6005767841299,2.60266930772329));
#211857=CARTESIAN_POINT('Ctrl Pts',(6.63252569365822,62.6023691645601,2.60133820040229));
#211858=CARTESIAN_POINT('Ctrl Pts',(6.6233959910565,62.603898983444,2.60044130723629));
#211859=CARTESIAN_POINT('Ctrl Pts',(6.61883113975564,62.604663892886,2.59999286065329));
#211860=CARTESIAN_POINT('Ctrl Pts',(6.61423692798837,62.6053631620639,2.59965296768557));
#211861=CARTESIAN_POINT('Ctrl Pts',(6.60961684864331,62.6059941550342,2.59942518630999));
#211862=CARTESIAN_POINT('Ctrl Pts',(6.60499676929825,62.6066251480045,2.59919740493441));
#211863=CARTESIAN_POINT('Ctrl Pts',(6.6003508221967,62.6071878630702,2.59908173791661));
#211864=CARTESIAN_POINT('Ctrl Pts',(6.59568250079866,62.6076796697356,2.59908173516068));
#211865=CARTESIAN_POINT('',(6.56531752495282,62.6108711573008,2.59908173516067));
#211866=CARTESIAN_POINT('Origin',(5.63895492999586E-15,1.85258037258938E-13,
2.59908173516024));
#211867=CARTESIAN_POINT('',(6.24436990788039,62.4538823482277,2.90134173516068));
#211868=CARTESIAN_POINT('Ctrl Pts',(6.56531752495282,62.6108711573008,2.59908173516068));
#211869=CARTESIAN_POINT('Ctrl Pts',(6.56151674480724,62.6112696981213,2.59908174381733));
#211870=CARTESIAN_POINT('Ctrl Pts',(6.55772139932922,62.6116196762809,2.59915752001041));
#211871=CARTESIAN_POINT('Ctrl Pts',(6.5539335245026,62.6119220062411,2.59930729517515));
#211872=CARTESIAN_POINT('Ctrl Pts',(6.53204428085627,62.6136691004466,2.60017281085965));
#211873=CARTESIAN_POINT('Ctrl Pts',(6.51040190952201,62.6138271176317,2.60350651800131));
#211874=CARTESIAN_POINT('Ctrl Pts',(6.48940618066432,62.6125709156641,2.6089688059657));
#211875=CARTESIAN_POINT('Ctrl Pts',(6.48093812023298,62.6120642605131,2.6111718723555));
#211876=CARTESIAN_POINT('Ctrl Pts',(6.47257489900914,62.6113278644157,2.61372076577271));
#211877=CARTESIAN_POINT('Ctrl Pts',(6.46434122354008,62.6103742524842,2.61659179897029));
#211878=CARTESIAN_POINT('Ctrl Pts',(6.46130349717915,62.6100224275776,2.61765103591254));
#211879=CARTESIAN_POINT('Ctrl Pts',(6.45828351400561,62.6096409597324,2.61875422455194));
#211880=CARTESIAN_POINT('Ctrl Pts',(6.45528256968501,62.6092304414386,2.61990022440441));
#211881=CARTESIAN_POINT('Ctrl Pts',(6.44965579908389,62.6084607196377,2.62204897412778));
#211882=CARTESIAN_POINT('Ctrl Pts',(6.4440959619495,62.6075888673477,2.62434823201815));
#211883=CARTESIAN_POINT('Ctrl Pts',(6.43861159905745,62.6066187902476,2.6267904803035));
#211884=CARTESIAN_POINT('Ctrl Pts',(6.41941632893527,62.6032235203972,2.63533834930224));
#211885=CARTESIAN_POINT('Ctrl Pts',(6.4011456178173,62.5986249921654,2.64563784783608));
#211886=CARTESIAN_POINT('Ctrl Pts',(6.38416565413472,62.5929906867161,2.65736666738009));
#211887=CARTESIAN_POINT('Ctrl Pts',(6.37567567229344,62.5901735339914,2.66323107715209));
#211888=CARTESIAN_POINT('Ctrl Pts',(6.36750837741684,62.587097437967,2.66945281780817));
#211889=CARTESIAN_POINT('Ctrl Pts',(6.35970954393956,62.5837833426319,2.67599160631244));
#211890=CARTESIAN_POINT('Ctrl Pts',(6.35581012720092,62.5821262949644,2.67926100056457));
#211891=CARTESIAN_POINT('Ctrl Pts',(6.35200282582338,62.5804097475861,2.68260965685166));
#211892=CARTESIAN_POINT('Ctrl Pts',(6.34829336166143,62.5786363190255,2.68603254012526));
#211893=CARTESIAN_POINT('Ctrl Pts',(6.34458389749948,62.5768628904649,2.68945542339885));
#211894=CARTESIAN_POINT('Ctrl Pts',(6.3409723839406,62.5750325180137,2.69295261525428));
#211895=CARTESIAN_POINT('Ctrl Pts',(6.33746431138575,62.5731479498684,2.69651891172142));
#211896=CARTESIAN_POINT('Ctrl Pts',(6.3374343948739,62.573131878449,2.6965493247613));
#211897=CARTESIAN_POINT('Ctrl Pts',(6.33740448593562,62.5731158032181,2.69657974261189));
#211898=CARTESIAN_POINT('Ctrl Pts',(6.33737458457357,62.5730997241773,2.69661016527017));
#211899=CARTESIAN_POINT('Ctrl Pts',(6.32210352242475,62.5648879232823,2.71214746101204));
#211900=CARTESIAN_POINT('Ctrl Pts',(6.30871688796312,62.5557775512965,2.7288056556768));
#211901=CARTESIAN_POINT('Ctrl Pts',(6.29717744164003,62.5459655399043,2.74628040012473));
#211902=CARTESIAN_POINT('Ctrl Pts',(6.28524773890477,62.5358216928023,2.76434612882623));
#211903=CARTESIAN_POINT('Ctrl Pts',(6.27529192173244,62.5249271226219,2.78328592654731));
#211904=CARTESIAN_POINT('Ctrl Pts',(6.26731706751958,62.513479393776,2.802787532682));
#211905=CARTESIAN_POINT('Ctrl Pts',(6.25949391181462,62.5022494248212,2.82191817723251));
#211906=CARTESIAN_POINT('Ctrl Pts',(6.25357708651698,62.4904862126961,2.84159092315711));
#211907=CARTESIAN_POINT('Ctrl Pts',(6.24962081353417,62.4783706704707,2.86151233817672));
#211908=CARTESIAN_POINT('Ctrl Pts',(6.24699992138298,62.4703445484958,2.87470957721769));
#211909=CARTESIAN_POINT('Ctrl Pts',(6.24524040122966,62.4621637089592,2.88801594388596));
#211910=CARTESIAN_POINT('Ctrl Pts',(6.24436990788039,62.4538823482277,2.90134173516068));
#211911=CARTESIAN_POINT('',(6.20712349654444,62.0995362748661,3.47153072139115));
#211912=CARTESIAN_POINT('',(6.24436990788039,62.4538823482277,2.90134173516068));
#211913=CARTESIAN_POINT('',(0.318048871876918,62.408169597977,3.47153072139115));
#211914=CARTESIAN_POINT('Origin',(5.53234440788222E-15,1.85015204418142E-13,
3.47153072139072));
#211915=CARTESIAN_POINT('',(0.318045750792831,62.7644678366121,2.90134173516067));
#211916=CARTESIAN_POINT('',(0.318048871876917,62.408169597977,3.47153072139115));
#211917=CARTESIAN_POINT('',(0.0152661173106527,62.954144805765,2.59908173516067));
#211918=CARTESIAN_POINT('Ctrl Pts',(0.318045750792831,62.7644678366121,
2.90134173516066));
#211919=CARTESIAN_POINT('Ctrl Pts',(0.318045618797917,62.7767737714906,
2.88164837656858));
#211920=CARTESIAN_POINT('Ctrl Pts',(0.316095234070562,62.7890393354359,
2.86203734439368));
#211921=CARTESIAN_POINT('Ctrl Pts',(0.312273660577917,62.8010929413147,
2.84277945978465));
#211922=CARTESIAN_POINT('Ctrl Pts',(0.308375296776869,62.8133887511219,
2.82313460920437));
#211923=CARTESIAN_POINT('Ctrl Pts',(0.302529834047427,62.8254649274575,
2.80385576863857));
#211924=CARTESIAN_POINT('Ctrl Pts',(0.294768478452471,62.8371482135729,
2.78521678518996));
#211925=CARTESIAN_POINT('Ctrl Pts',(0.287308644486513,62.848377614614,2.76730190935162));
#211926=CARTESIAN_POINT('Ctrl Pts',(0.27807851836262,62.8592448608886,2.74997687280549));
#211927=CARTESIAN_POINT('Ctrl Pts',(0.267060783352071,62.8695915013832,
2.73349253346556));
#211928=CARTESIAN_POINT('Ctrl Pts',(0.258597341637146,62.8775394315783,
2.72082983599834));
#211929=CARTESIAN_POINT('Ctrl Pts',(0.249078184947951,62.8851801717842,
2.70866321039561));
#211930=CARTESIAN_POINT('Ctrl Pts',(0.238478017627659,62.892435632374,2.69711645335889));
#211931=CARTESIAN_POINT('Ctrl Pts',(0.238450236479551,62.8924546476422,
2.69708619136795));
#211932=CARTESIAN_POINT('Ctrl Pts',(0.238422447083127,62.8924736601097,
2.69705593387262));
#211933=CARTESIAN_POINT('Ctrl Pts',(0.238394649440964,62.8924926697744,
2.69702568087614));
#211934=CARTESIAN_POINT('Ctrl Pts',(0.2354141769123,62.8945308924034,2.6937819444331));
#211935=CARTESIAN_POINT('Ctrl Pts',(0.232339728999105,62.896535178772,2.69059266624743));
#211936=CARTESIAN_POINT('Ctrl Pts',(0.229175397308913,62.8985027695521,
2.6874621934272));
#211937=CARTESIAN_POINT('Ctrl Pts',(0.211566610931505,62.9094519648693,
2.67004182396259));
#211938=CARTESIAN_POINT('Ctrl Pts',(0.191177078587904,62.9192690206943,
2.6544356787816));
#211939=CARTESIAN_POINT('Ctrl Pts',(0.168765047547321,62.9274935913875,
2.64136852353408));
#211940=CARTESIAN_POINT('Ctrl Pts',(0.158706217644123,62.9311848926123,
2.63550380329897));
#211941=CARTESIAN_POINT('Ctrl Pts',(0.148239886923453,62.9345557609572,
2.63014997451202));
#211942=CARTESIAN_POINT('Ctrl Pts',(0.137433186922148,62.9375663198811,
2.62536981119296));
#211943=CARTESIAN_POINT('Ctrl Pts',(0.1327367412734,62.9388746680685,2.62329241687116));
#211944=CARTESIAN_POINT('Ctrl Pts',(0.127976140237888,62.9401148076315,
2.62132362131471));
#211945=CARTESIAN_POINT('Ctrl Pts',(0.123156980417348,62.941283367484,2.61946873372391));
#211946=CARTESIAN_POINT('Ctrl Pts',(0.106289921045458,62.9453733269675,
2.61297662715611));
#211947=CARTESIAN_POINT('Ctrl Pts',(0.0887055165508409,62.9485864317706,
2.60787989114013));
#211948=CARTESIAN_POINT('Ctrl Pts',(0.0706437212499503,62.9507781643244,
2.60440616886223));
#211949=CARTESIAN_POINT('Ctrl Pts',(0.0616128235995051,62.9518740306013,
2.60266930772328));
#211950=CARTESIAN_POINT('Ctrl Pts',(0.0524625782499263,62.9527145544239,
2.60133820040229));
#211951=CARTESIAN_POINT('Ctrl Pts',(0.043222979497305,62.9532816790169,
2.60044130723629));
#211952=CARTESIAN_POINT('Ctrl Pts',(0.0386031801209943,62.9535652413134,
2.59999286065329));
#211953=CARTESIAN_POINT('Ctrl Pts',(0.0339610423938989,62.9537804539257,
2.59965296768556));
#211954=CARTESIAN_POINT('Ctrl Pts',(0.0293003156013865,62.9539250604563,
2.59942518630998));
#211955=CARTESIAN_POINT('Ctrl Pts',(0.0246395888088739,62.954069666987,
2.59919740493441));
#211956=CARTESIAN_POINT('Ctrl Pts',(0.0199602729505793,62.9541436657298,
2.59908173791657));
#211957=CARTESIAN_POINT('Ctrl Pts',(0.0152661173106527,62.954144805765,
2.59908173516068));
#211958=CARTESIAN_POINT('',(-0.015266117311081,62.954144805765,2.59908173516067));
#211959=CARTESIAN_POINT('Origin',(-3.96846087890508E-17,1.90952070476508E-13,
2.59908173516023));
#211960=CARTESIAN_POINT('',(-0.318045750793258,62.7644678366121,2.90134173516066));
#211961=CARTESIAN_POINT('Ctrl Pts',(-0.015266117311081,62.954144805765,
2.59908173516068));
#211962=CARTESIAN_POINT('Ctrl Pts',(-0.0190877352448647,62.9541438736294,
2.59908174381727));
#211963=CARTESIAN_POINT('Ctrl Pts',(-0.022898872102443,62.9540952129416,
2.59915752001039));
#211964=CARTESIAN_POINT('Ctrl Pts',(-0.0266975986405677,62.953999945972,
2.59930729517514));
#211965=CARTESIAN_POINT('Ctrl Pts',(-0.0486495517927879,62.9534494204122,
2.60017281085966));
#211966=CARTESIAN_POINT('Ctrl Pts',(-0.0701898812463166,62.9513443281456,
2.60350651800143));
#211967=CARTESIAN_POINT('Ctrl Pts',(-0.0909392844436332,62.947900356511,
2.608968805966));
#211968=CARTESIAN_POINT('Ctrl Pts',(-0.099307996069169,62.9465113235261,
2.61117187235574));
#211969=CARTESIAN_POINT('Ctrl Pts',(-0.107548428339302,62.9449047668212,
2.61372076577286));
#211970=CARTESIAN_POINT('Ctrl Pts',(-0.115637319282522,62.9430957254319,
2.6165917989703));
#211971=CARTESIAN_POINT('Ctrl Pts',(-0.118621628943776,62.9424282989907,
2.61765103591255));
#211972=CARTESIAN_POINT('Ctrl Pts',(-0.12158519408586,62.9417332466659,
2.61875422455195));
#211973=CARTESIAN_POINT('Ctrl Pts',(-0.124526788073079,62.9410112931361,
2.61990022440441));
#211974=CARTESIAN_POINT('Ctrl Pts',(-0.130042276799115,62.9396576302677,
2.62204897412778));
#211975=CARTESIAN_POINT('Ctrl Pts',(-0.135480523183885,62.9382093928442,
2.62434823201817));
#211976=CARTESIAN_POINT('Ctrl Pts',(-0.140833441493647,62.9366713579028,
2.62679048030352));
#211977=CARTESIAN_POINT('Ctrl Pts',(-0.159568655577816,62.931288235608,
2.63533834930225));
#211978=CARTESIAN_POINT('Ctrl Pts',(-0.177258600739223,62.924805089239,
2.64563784783608));
#211979=CARTESIAN_POINT('Ctrl Pts',(-0.193556601113891,62.9174267595944,
2.65736666738009));
#211980=CARTESIAN_POINT('Ctrl Pts',(-0.201705601301226,62.913737594772,
2.66323107715209));
#211981=CARTESIAN_POINT('Ctrl Pts',(-0.209506615291636,62.909824635141,
2.66945281780818));
#211982=CARTESIAN_POINT('Ctrl Pts',(-0.216916308650622,62.9057134946883,
2.67599160631244));
#211983=CARTESIAN_POINT('Ctrl Pts',(-0.220621155330115,62.903657924462,
2.67926100056457));
#211984=CARTESIAN_POINT('Ctrl Pts',(-0.22422817185277,62.9015528091476,
2.68260965685166));
#211985=CARTESIAN_POINT('Ctrl Pts',(-0.227731941419756,62.8994013510258,
2.68603254012525));
#211986=CARTESIAN_POINT('Ctrl Pts',(-0.231235710986742,62.897249892904,
2.68945542339885));
#211987=CARTESIAN_POINT('Ctrl Pts',(-0.234636114276948,62.8950520414623,
2.69295261525428));
#211988=CARTESIAN_POINT('Ctrl Pts',(-0.237927978231133,62.8928111037453,
2.69651891172142));
#211989=CARTESIAN_POINT('Ctrl Pts',(-0.237956050936432,62.8927919932398,
2.6965493247613));
#211990=CARTESIAN_POINT('Ctrl Pts',(-0.237984115711227,62.8927728797353,
2.69657974261189));
#211991=CARTESIAN_POINT('Ctrl Pts',(-0.238012172553063,62.8927537632337,
2.69661016527017));
#211992=CARTESIAN_POINT('Ctrl Pts',(-0.25234121129623,62.8829906867852,
2.71214746101078));
#211993=CARTESIAN_POINT('Ctrl Pts',(-0.264702219189273,62.8725309380426,
2.72880565567411));
#211994=CARTESIAN_POINT('Ctrl Pts',(-0.275152816745077,62.8615664772854,
2.74628040012049));
#211995=CARTESIAN_POINT('Ctrl Pts',(-0.285956846570814,62.8502312057459,
2.76434612882047));
#211996=CARTESIAN_POINT('Ctrl Pts',(-0.294719332055858,62.8383556508924,
2.78328592653991));
#211997=CARTESIAN_POINT('Ctrl Pts',(-0.301453885678867,62.8261370346483,
2.80278753267292));
#211998=CARTESIAN_POINT('Ctrl Pts',(-0.308060333921113,62.8141508421955,
2.82191817722197));
#211999=CARTESIAN_POINT('Ctrl Pts',(-0.31271515574461,62.8018335935224,
2.8415909231451));
#212000=CARTESIAN_POINT('Ctrl Pts',(-0.315383336840319,62.7893708783707,
2.86151233816327));
#212001=CARTESIAN_POINT('Ctrl Pts',(-0.317150913275242,62.7811147665001,
2.87470957720864));
#212002=CARTESIAN_POINT('Ctrl Pts',(-0.318045664008668,62.7727948225179,
2.88801594388141));
#212003=CARTESIAN_POINT('Ctrl Pts',(-0.318045750793257,62.7644678366121,
2.90134173516066));
#212004=CARTESIAN_POINT('',(-0.318048871877343,62.408169597977,3.47153072139115));
#212005=CARTESIAN_POINT('',(-0.318045750793259,62.7644678366121,2.90134173516066));
#212006=CARTESIAN_POINT('',(-6.20712349654485,62.099536274866,3.47153072139116));
#212007=CARTESIAN_POINT('Origin',(5.53234440788222E-15,1.85015204418142E-13,
3.47153072139072));
#212008=CARTESIAN_POINT('',(-6.2443699078808,62.4538823482277,2.90134173516068));
#212009=CARTESIAN_POINT('',(-6.20712349654485,62.099536274866,3.47153072139115));
#212010=CARTESIAN_POINT('',(-6.56531752495323,62.6108711573007,2.59908173516067));
#212011=CARTESIAN_POINT('Ctrl Pts',(-6.2443699078808,62.4538823482277,2.90134173516068));
#212012=CARTESIAN_POINT('Ctrl Pts',(-6.24565635961481,62.4661208561115,
2.88164837656632));
#212013=CARTESIAN_POINT('Ctrl Pts',(-6.24887816048149,62.4781153572972,
2.86203734438916));
#212014=CARTESIAN_POINT('Ctrl Pts',(-6.25393874389503,62.4897034690586,
2.84277945977798));
#212015=CARTESIAN_POINT('Ctrl Pts',(-6.25910101415609,62.501524431157,2.82313460919551));
#212016=CARTESIAN_POINT('Ctrl Pts',(-6.26617675898503,62.5129234357001,
2.80385576862764));
#212017=CARTESIAN_POINT('Ctrl Pts',(-6.27511683300737,62.5237314369795,
2.78521678517717));
#212018=CARTESIAN_POINT('Ctrl Pts',(-6.28370959325826,62.5341195572068,
2.76730190933723));
#212019=CARTESIAN_POINT('Ctrl Pts',(-6.29402509234058,62.5439624606704,
2.74997687278967));
#212020=CARTESIAN_POINT('Ctrl Pts',(-6.30606398947926,62.553100754277,2.73349253344858));
#212021=CARTESIAN_POINT('Ctrl Pts',(-6.31531185250115,62.5601204743189,
2.72082983598746));
#212022=CARTESIAN_POINT('Ctrl Pts',(-6.32557753708182,62.566724334927,2.70866321039045));
#212023=CARTESIAN_POINT('Ctrl Pts',(-6.33687803771711,62.5728320301414,
2.69711645335888));
#212024=CARTESIAN_POINT('Ctrl Pts',(-6.33690765431396,62.5728480373213,
2.69708619136794));
#212025=CARTESIAN_POINT('Ctrl Pts',(-6.33693727882117,62.5728640408536,
2.69705593387261));
#212026=CARTESIAN_POINT('Ctrl Pts',(-6.33696691123597,62.5728800407365,
2.69702568087613));
#212027=CARTESIAN_POINT('Ctrl Pts',(-6.34014410870348,62.5745955535555,
2.69378194443309));
#212028=CARTESIAN_POINT('Ctrl Pts',(-6.34341121944339,62.5762674929179,
2.69059266624743));
#212029=CARTESIAN_POINT('Ctrl Pts',(-6.34676388583407,62.577893542301,2.6874621934272));
#212030=CARTESIAN_POINT('Ctrl Pts',(-6.36542071199959,62.5869421374014,
2.67004182396091));
#212031=CARTESIAN_POINT('Ctrl Pts',(-6.38672471011312,62.5945741278854,
2.6544356787786));
#212032=CARTESIAN_POINT('Ctrl Pts',(-6.40987366744084,62.6004109483567,
2.64136852353031));
#212033=CARTESIAN_POINT('Ctrl Pts',(-6.42026324006377,62.6030305942144,
2.63550380329668));
#212034=CARTESIAN_POINT('Ctrl Pts',(-6.43102458681537,62.6052889671229,
2.630149974511));
#212035=CARTESIAN_POINT('Ctrl Pts',(-6.44208677567886,62.6071534261455,
2.62536981119296));
#212036=CARTESIAN_POINT('Ctrl Pts',(-6.44689425333239,62.6079636948181,
2.62329241687116));
#212037=CARTESIAN_POINT('Ctrl Pts',(-6.45175840518009,62.6086994224564,
2.6213236213147));
#212038=CARTESIAN_POINT('Ctrl Pts',(-6.45667331290451,62.6093578414454,
2.6194687337239));
#212039=CARTESIAN_POINT('Ctrl Pts',(-6.47387548993997,62.611662307907,2.6129766271561));
#212040=CARTESIAN_POINT('Ctrl Pts',(-6.49169942613426,62.6130197402064,
2.60787989114011));
#212041=CARTESIAN_POINT('Ctrl Pts',(-6.5098913754664,62.6133114945134,2.60440616886222));
#212042=CARTESIAN_POINT('Ctrl Pts',(-6.51898735013247,62.6134573716668,
2.60266930772327));
#212043=CARTESIAN_POINT('Ctrl Pts',(-6.52817532814414,62.6133368299271,
2.60133820040228));
#212044=CARTESIAN_POINT('Ctrl Pts',(-6.53742359207023,62.6129350466934,
2.60044130723627));
#212045=CARTESIAN_POINT('Ctrl Pts',(-6.54204772403327,62.6127341550766,
2.59999286065327));
#212046=CARTESIAN_POINT('Ctrl Pts',(-6.54668692748782,62.6124629532087,
2.59965296768555));
#212047=CARTESIAN_POINT('Ctrl Pts',(-6.55133723782973,62.6121195889603,
2.59942518630998));
#212048=CARTESIAN_POINT('Ctrl Pts',(-6.55598754817164,62.611776224712,2.5991974049344));
#212049=CARTESIAN_POINT('Ctrl Pts',(-6.56064896522293,62.6113606963861,
2.59908173791658));
#212050=CARTESIAN_POINT('Ctrl Pts',(-6.56531752495323,62.6108711573007,
2.59908173516068));
#212051=CARTESIAN_POINT('',(-6.59568250079906,62.6076796697356,2.59908173516067));
#212052=CARTESIAN_POINT('Origin',(-2.34395632424774E-17,1.90952921843269E-13,
2.59908173516024));
#212053=CARTESIAN_POINT('',(-6.87697683366585,62.3873926810693,2.90134173516067));
#212054=CARTESIAN_POINT('Ctrl Pts',(-6.59568250079906,62.6076796697356,
2.59908173516068));
#212055=CARTESIAN_POINT('Ctrl Pts',(-6.59948308607524,62.6072792748565,
2.59908174381726));
#212056=CARTESIAN_POINT('Ctrl Pts',(-6.60326825869943,62.606832508458,2.59915752001039));
#212057=CARTESIAN_POINT('Ctrl Pts',(-6.60703621730618,62.6063406883234,
2.59930729517514));
#212058=CARTESIAN_POINT('Ctrl Pts',(-6.62881036976983,62.6034985746717,
2.60017281085959));
#212059=CARTESIAN_POINT('Ctrl Pts',(-6.65001265698364,62.5991534367851,
2.60350651800094));
#212060=CARTESIAN_POINT('Ctrl Pts',(-6.67028839971536,62.5935594283582,
2.60896880596481));
#212061=CARTESIAN_POINT('Ctrl Pts',(-6.67846607318115,62.5913032360753,
2.61117187235482));
#212062=CARTESIAN_POINT('Ctrl Pts',(-6.68649343259904,62.5888441205338,
2.61372076577233));
#212063=CARTESIAN_POINT('Ctrl Pts',(-6.6943489154363,62.5861994699222,2.61659179897028));
#212064=CARTESIAN_POINT('Ctrl Pts',(-6.69724711167674,62.5852237544101,
2.61765103591253));
#212065=CARTESIAN_POINT('Ctrl Pts',(-6.70012178934749,62.5842227327446,
2.61875422455194));
#212066=CARTESIAN_POINT('Ctrl Pts',(-6.70297180428205,62.5831972538527,
2.61990022440441));
#212067=CARTESIAN_POINT('Ctrl Pts',(-6.70831558228433,62.5812744809304,
2.62204897412778));
#212068=CARTESIAN_POINT('Ctrl Pts',(-6.71357265535406,62.5792657255655,
2.62434823201814));
#212069=CARTESIAN_POINT('Ctrl Pts',(-6.71873548138837,62.5771765838156,
2.62679048030349));
#212070=CARTESIAN_POINT('Ctrl Pts',(-6.73680537250844,62.5698645876908,
2.63533834930223));
#212071=CARTESIAN_POINT('Ctrl Pts',(-6.75372073697224,62.561567853893,2.64563784783606));
#212072=CARTESIAN_POINT('Ctrl Pts',(-6.76915820973634,62.5525263385766,
2.65736666738008));
#212073=CARTESIAN_POINT('Ctrl Pts',(-6.77687694611839,62.5480055809184,
2.66323107715209));
#212074=CARTESIAN_POINT('Ctrl Pts',(-6.78422620968087,62.5432986288853,
2.66945281780817));
#212075=CARTESIAN_POINT('Ctrl Pts',(-6.79116558077055,62.53843548583,2.67599160631244));
#212076=CARTESIAN_POINT('Ctrl Pts',(-6.79463526631539,62.5360039143024,
2.67926100056457));
#212077=CARTESIAN_POINT('Ctrl Pts',(-6.79800247875532,62.533533295136,2.68260965685166));
#212078=CARTESIAN_POINT('Ctrl Pts',(-6.80126216569475,62.5310273792784,
2.68603254012526));
#212079=CARTESIAN_POINT('Ctrl Pts',(-6.80452185263419,62.5285214634208,
2.68945542339885));
#212080=CARTESIAN_POINT('Ctrl Pts',(-6.80767389012568,62.5259802131088,
2.69295261525429));
#212081=CARTESIAN_POINT('Ctrl Pts',(-6.81071347912886,62.5234074580026,
2.69651891172143));
#212082=CARTESIAN_POINT('Ctrl Pts',(-6.81073940045717,62.5233855177898,
2.69654932476131));
#212083=CARTESIAN_POINT('Ctrl Pts',(-6.81076531358493,62.5233635754233,
2.69657974261189));
#212084=CARTESIAN_POINT('Ctrl Pts',(-6.81079121850992,62.5233416309053,
2.69661016527016));
#212085=CARTESIAN_POINT('Ctrl Pts',(-6.82402124190201,62.5121342452109,
2.71214746101119));
#212086=CARTESIAN_POINT('Ctrl Pts',(-6.83522119343849,62.5004397189066,
2.72880565567501));
#212087=CARTESIAN_POINT('Ctrl Pts',(-6.84446844329406,62.4884429377095,
2.74628040012191));
#212088=CARTESIAN_POINT('Ctrl Pts',(-6.85402842899935,62.4760404333385,
2.76434612882238));
#212089=CARTESIAN_POINT('Ctrl Pts',(-6.86150157917281,62.4633140048744,
2.78328592654235));
#212090=CARTESIAN_POINT('Ctrl Pts',(-6.86692204702709,62.4504583709472,
2.8027875326759));
#212091=CARTESIAN_POINT('Ctrl Pts',(-6.87223940617701,62.4378472782282,
2.82191817722543));
#212092=CARTESIAN_POINT('Ctrl Pts',(-6.87558122532386,62.4251109433598,
2.84159092314904));
#212093=CARTESIAN_POINT('Ctrl Pts',(-6.87693208138113,62.4124375993958,
2.86151233816768));
#212094=CARTESIAN_POINT('Ctrl Pts',(-6.8778269761607,62.4040419533223,2.87470957721161));
#212095=CARTESIAN_POINT('Ctrl Pts',(-6.87784715439696,62.3956740599456,
2.8880159438829));
#212096=CARTESIAN_POINT('Ctrl Pts',(-6.87697683366585,62.3873926810693,
2.90134173516067));
#212097=CARTESIAN_POINT('',(-6.83973663030281,62.0330459552234,3.47153072139115));
#212098=CARTESIAN_POINT('',(-6.87697683366585,62.3873926810693,2.90134173516067));
#212099=CARTESIAN_POINT('',(-12.6642893210144,61.1105274371642,3.47153072139114));
#212100=CARTESIAN_POINT('Origin',(5.53234440788222E-15,1.85015204418142E-13,
3.47153072139072));
#212101=CARTESIAN_POINT('',(-12.7383709431253,61.459039055521,2.90134173516066));
#212102=CARTESIAN_POINT('',(-12.6642893210144,61.1105274371642,3.47153072139114));
#212103=CARTESIAN_POINT('',(-13.0739701745327,61.5816197022699,2.59908173516066));
#212104=CARTESIAN_POINT('Ctrl Pts',(-12.7383709431253,61.459039055521,2.90134173516066));
#212105=CARTESIAN_POINT('Ctrl Pts',(-12.7409296199638,61.4710760487557,
2.88164837656569));
#212106=CARTESIAN_POINT('Ctrl Pts',(-12.7453875382449,61.4826680729157,
2.86203734438793));
#212107=CARTESIAN_POINT('Ctrl Pts',(-12.7516316867679,61.4936637287812,
2.84277945977618));
#212108=CARTESIAN_POINT('Ctrl Pts',(-12.7580013045751,61.5048803302354,
2.82313460919295));
#212109=CARTESIAN_POINT('Ctrl Pts',(-12.7662298081617,61.5154772731058,
2.80385576862436));
#212110=CARTESIAN_POINT('Ctrl Pts',(-12.7762506512886,61.5252915748246,
2.78521678517323));
#212111=CARTESIAN_POINT('Ctrl Pts',(-12.7858821937442,61.5347245998185,
2.76730190933241));
#212112=CARTESIAN_POINT('Ctrl Pts',(-12.7971700470174,61.5434353195605,
2.74997687278406));
#212113=CARTESIAN_POINT('Ctrl Pts',(-12.8100982056066,61.5512651452213,
2.7334925334423));
#212114=CARTESIAN_POINT('Ctrl Pts',(-12.8200291684145,61.5572797455911,
2.72082983598343));
#212115=CARTESIAN_POINT('Ctrl Pts',(-12.8309289079003,61.5627743733251,
2.70866321038853));
#212116=CARTESIAN_POINT('Ctrl Pts',(-12.8428059312037,61.5676673859797,
2.69711645335887));
#212117=CARTESIAN_POINT('Ctrl Pts',(-12.8428370587636,61.5676802096933,
2.69708619136793));
#212118=CARTESIAN_POINT('Ctrl Pts',(-12.8428681938093,61.5676930289523,
2.6970559338726));
#212119=CARTESIAN_POINT('Ctrl Pts',(-12.8428993363378,61.5677058437554,
2.69702568087612));
#212120=CARTESIAN_POINT('Ctrl Pts',(-12.8462384487039,61.5690798512469,
2.69378194443308));
#212121=CARTESIAN_POINT('Ctrl Pts',(-12.8496624271215,61.5704011254856,
2.69059266624742));
#212122=CARTESIAN_POINT('Ctrl Pts',(-12.8531666956981,61.5716678181343,
2.68746219342719));
#212123=CARTESIAN_POINT('Ctrl Pts',(-12.8726671535595,61.5787166747159,
2.67004182395993));
#212124=CARTESIAN_POINT('Ctrl Pts',(-12.8946522063806,61.5840799821735,
2.65443567877684));
#212125=CARTESIAN_POINT('Ctrl Pts',(-12.9182844651737,61.5874651029957,
2.64136852352809));
#212126=CARTESIAN_POINT('Ctrl Pts',(-12.9288909501853,61.5889843920987,
2.63550380329533));
#212127=CARTESIAN_POINT('Ctrl Pts',(-12.9398294094017,61.5901055263653,
2.63014997451039));
#212128=CARTESIAN_POINT('Ctrl Pts',(-12.9510258874722,61.5908034580839,
2.62536981119295));
#212129=CARTESIAN_POINT('Ctrl Pts',(-12.9558917253993,61.5911067697687,
2.62329241687115));
#212130=CARTESIAN_POINT('Ctrl Pts',(-12.9608061353937,61.5913300246962,
2.6213236213147));
#212131=CARTESIAN_POINT('Ctrl Pts',(-12.9657629422644,61.5914710890456,
2.6194687337239));
#212132=CARTESIAN_POINT('Ctrl Pts',(-12.9831117663121,61.5919648142684,
2.6129766271561));
#212133=CARTESIAN_POINT('Ctrl Pts',(-13.0009799514312,61.5914517017519,
2.60787989114012));
#212134=CARTESIAN_POINT('Ctrl Pts',(-13.0191027399908,61.5898402812907,
2.60440616886223));
#212135=CARTESIAN_POINT('Ctrl Pts',(-13.0281641342706,61.58903457106,2.60266930772328));
#212136=CARTESIAN_POINT('Ctrl Pts',(-13.0372891795345,61.5879542844385,
2.60133820040226));
#212137=CARTESIAN_POINT('Ctrl Pts',(-13.0464447827192,61.5865879953993,
2.60044130723626));
#212138=CARTESIAN_POINT('Ctrl Pts',(-13.0510225843115,61.5859048508797,
2.59999286065326));
#212139=CARTESIAN_POINT('Ctrl Pts',(-13.0556080254097,61.5851502058762,
2.59965296768554));
#212140=CARTESIAN_POINT('Ctrl Pts',(-13.0601969695277,61.5843226328194,
2.59942518630996));
#212141=CARTESIAN_POINT('Ctrl Pts',(-13.0647859136458,61.5834950597625,
2.59919740493438));
#212142=CARTESIAN_POINT('Ctrl Pts',(-13.0693783604294,61.5825945569832,
2.59908173791658));
#212143=CARTESIAN_POINT('Ctrl Pts',(-13.0739701745327,61.5816197022699,
2.59908173516066));
#212144=CARTESIAN_POINT('',(-13.103835206573,61.5752716937453,2.59908173516066));
#212145=CARTESIAN_POINT('Origin',(-7.37250181440781E-18,1.90955466615801E-13,
2.59908173516024));
#212146=CARTESIAN_POINT('',(-13.3605623192489,61.3267881959114,2.90134173516066));
#212147=CARTESIAN_POINT('Ctrl Pts',(-13.103835206573,61.5752716937453,2.59908173516067));
#212148=CARTESIAN_POINT('Ctrl Pts',(-13.107573119184,61.5744762229328,2.59908174381721));
#212149=CARTESIAN_POINT('Ctrl Pts',(-13.1112908564314,61.5736362456897,
2.59915752001038));
#212150=CARTESIAN_POINT('Ctrl Pts',(-13.1149867645638,61.5727532608745,
2.59930729517513));
#212151=CARTESIAN_POINT('Ctrl Pts',(-13.1363445541693,61.5676506979228,
2.60017281085957));
#212152=CARTESIAN_POINT('Ctrl Pts',(-13.1569765024492,61.5611131206561,
2.60350651800086));
#212153=CARTESIAN_POINT('Ctrl Pts',(-13.1765564394362,61.5534303645633,
2.60896880596463));
#212154=CARTESIAN_POINT('Ctrl Pts',(-13.1844534784391,61.5503317322973,
2.61117187235468));
#212155=CARTESIAN_POINT('Ctrl Pts',(-13.1921798155738,61.547047000504,2.61372076577224));
#212156=CARTESIAN_POINT('Ctrl Pts',(-13.1997158239901,61.5435957160158,
2.61659179897027));
#212157=CARTESIAN_POINT('Ctrl Pts',(-13.2024961535652,61.5423224015761,
2.61765103591252));
#212158=CARTESIAN_POINT('Ctrl Pts',(-13.2052504481945,61.5410263779727,
2.61875422455193));
#212159=CARTESIAN_POINT('Ctrl Pts',(-13.2079776587163,61.5397086090801,
2.6199002244044));
#212160=CARTESIAN_POINT('Ctrl Pts',(-13.2130911784448,61.5372377924064,
2.62204897412777));
#212161=CARTESIAN_POINT('Ctrl Pts',(-13.2181094806068,61.5346905274443,
2.62434823201813));
#212162=CARTESIAN_POINT('Ctrl Pts',(-13.2230256493633,61.53207316796,2.62679048030349));
#212163=CARTESIAN_POINT('Ctrl Pts',(-13.2402322400107,61.5229124097648,
2.63533834930222));
#212164=CARTESIAN_POINT('Ctrl Pts',(-13.2561876955041,61.5128929892898,
2.64563784783606));
#212165=CARTESIAN_POINT('Ctrl Pts',(-13.2705955044755,61.5022873490356,
2.65736666738007));
#212166=CARTESIAN_POINT('Ctrl Pts',(-13.2777994089612,61.4969845289085,
2.66323107715208));
#212167=CARTESIAN_POINT('Ctrl Pts',(-13.2846164020262,61.4915351548249,
2.66945281780817));
#212168=CARTESIAN_POINT('Ctrl Pts',(-13.2910094216448,61.48597329078,2.67599160631244));
#212169=CARTESIAN_POINT('Ctrl Pts',(-13.2942059314541,61.4831923587576,
2.67926100056457));
#212170=CARTESIAN_POINT('Ctrl Pts',(-13.2972964479272,61.4803833043596,
2.68260965685166));
#212171=CARTESIAN_POINT('Ctrl Pts',(-13.3002763384268,61.4775503861048,
2.68603254012525));
#212172=CARTESIAN_POINT('Ctrl Pts',(-13.3032562289264,61.47471746785,2.68945542339885));
#212173=CARTESIAN_POINT('Ctrl Pts',(-13.3061253662369,61.4718606611379,
2.69295261525427));
#212174=CARTESIAN_POINT('Ctrl Pts',(-13.3088793779158,61.468984276286,2.69651891172141));
#212175=CARTESIAN_POINT('Ctrl Pts',(-13.3089028638677,61.4689597467473,
2.69654932476129));
#212176=CARTESIAN_POINT('Ctrl Pts',(-13.3089263414387,61.4689352159239,
2.69657974261188));
#212177=CARTESIAN_POINT('Ctrl Pts',(-13.3089498106271,61.4689106838184,
2.69661016527015));
#212178=CARTESIAN_POINT('Ctrl Pts',(-13.3209358677632,61.4563817793409,
2.71214746101158));
#212179=CARTESIAN_POINT('Ctrl Pts',(-13.3308520539303,61.4435806031522,
2.72880565567585));
#212180=CARTESIAN_POINT('Ctrl Pts',(-13.338794641281,61.4306829407606,2.74628040012323));
#212181=CARTESIAN_POINT('Ctrl Pts',(-13.3470058416618,61.4173490879912,
2.76434612882423));
#212182=CARTESIAN_POINT('Ctrl Pts',(-13.3531077791265,61.4039112193301,
2.78328592654476));
#212183=CARTESIAN_POINT('Ctrl Pts',(-13.3571547734318,61.3905594167353,
2.80278753267888));
#212184=CARTESIAN_POINT('Ctrl Pts',(-13.3611247853898,61.3774615935208,
2.82191817722895));
#212185=CARTESIAN_POINT('Ctrl Pts',(-13.36311698819,61.3644457144072,2.8415909231531));
#212186=CARTESIAN_POINT('Ctrl Pts',(-13.3631357189472,61.3517005934394,
2.86151233817227));
#212187=CARTESIAN_POINT('Ctrl Pts',(-13.3631481274171,61.3432573976185,
2.87470957721469));
#212188=CARTESIAN_POINT('Ctrl Pts',(-13.3622935120794,61.3349332352382,
2.88801594388444));
#212189=CARTESIAN_POINT('Ctrl Pts',(-13.3605623192489,61.3267881959114,
2.90134173516065));
#212190=CARTESIAN_POINT('',(-13.2864868028998,60.9782752797349,3.47153072139114));
#212191=CARTESIAN_POINT('',(-13.3605623192489,61.3267881959114,2.90134173516066));
#212192=CARTESIAN_POINT('',(-18.9827025415099,59.4519788726608,3.47153072139113));
#212193=CARTESIAN_POINT('Origin',(5.53234440788222E-15,1.85015204418142E-13,
3.47153072139072));
#212194=CARTESIAN_POINT('',(-19.0928077206414,59.7908376697913,2.90134173516065));
#212195=CARTESIAN_POINT('',(-18.9827025415099,59.4519788726608,3.47153072139113));
#212196=CARTESIAN_POINT('',(-19.4393816709759,59.8776671349986,2.59908173516064));
#212197=CARTESIAN_POINT('Ctrl Pts',(-19.0928077206414,59.7908376697913,
2.90134173516065));
#212198=CARTESIAN_POINT('Ctrl Pts',(-19.0966105891852,59.802541268558,2.88164837656838));
#212199=CARTESIAN_POINT('Ctrl Pts',(-19.1022557829942,59.813603811048,2.86203734439329));
#212200=CARTESIAN_POINT('Ctrl Pts',(-19.109615084427,59.8238865403095,2.84277945978409));
#212201=CARTESIAN_POINT('Ctrl Pts',(-19.117122262913,59.834375889685,2.82313460920358));
#212202=CARTESIAN_POINT('Ctrl Pts',(-19.1264133720475,59.8440546685577,
2.80385576863757));
#212203=CARTESIAN_POINT('Ctrl Pts',(-19.1374051938214,59.8527677431713,
2.78521678518877));
#212204=CARTESIAN_POINT('Ctrl Pts',(-19.1479699932837,59.8611423227348,
2.76730190935032));
#212205=CARTESIAN_POINT('Ctrl Pts',(-19.1601065286611,59.8686254222859,
2.74997687280409));
#212206=CARTESIAN_POINT('Ctrl Pts',(-19.1737823050855,59.8750609947923,
2.73349253346408));
#212207=CARTESIAN_POINT('Ctrl Pts',(-19.1842875619788,59.8800045782744,
2.72082983599738));
#212208=CARTESIAN_POINT('Ctrl Pts',(-19.1957019365505,59.8843297728472,
2.70866321039513));
#212209=CARTESIAN_POINT('Ctrl Pts',(-19.2080253553781,59.8879544940745,
2.69711645335885));
#212210=CARTESIAN_POINT('Ctrl Pts',(-19.2080576528611,59.8879639938225,
2.69708619136791));
#212211=CARTESIAN_POINT('Ctrl Pts',(-19.2080899573232,59.8879734883578,
2.69705593387258));
#212212=CARTESIAN_POINT('Ctrl Pts',(-19.2081222687613,59.8879829776794,
2.6970256808761));
#212213=CARTESIAN_POINT('Ctrl Pts',(-19.211586712012,59.8890004259297,2.69378194443306));
#212214=CARTESIAN_POINT('Ctrl Pts',(-19.2151300442834,59.8899565588876,
2.6905926662474));
#212215=CARTESIAN_POINT('Ctrl Pts',(-19.2187475215461,59.8908500166523,
2.68746219342717));
#212216=CARTESIAN_POINT('Ctrl Pts',(-19.2388779600059,59.8958219059669,
2.67004182395933));
#212217=CARTESIAN_POINT('Ctrl Pts',(-19.2613031946947,59.8988577688788,
2.6544356787758));
#212218=CARTESIAN_POINT('Ctrl Pts',(-19.2851598349798,59.8997541019597,
2.6413685235268));
#212219=CARTESIAN_POINT('Ctrl Pts',(-19.2958670255112,59.900156388659,2.63550380329453));
#212220=CARTESIAN_POINT('Ctrl Pts',(-19.3068627531447,59.9001280009024,
2.63014997451003));
#212221=CARTESIAN_POINT('Ctrl Pts',(-19.318070849466,59.8996517586313,2.62536981119294));
#212222=CARTESIAN_POINT('Ctrl Pts',(-19.3229417365281,59.8994447901819,
2.62329241687114));
#212223=CARTESIAN_POINT('Ctrl Pts',(-19.3278525613648,59.899153126371,2.62132362131468));
#212224=CARTESIAN_POINT('Ctrl Pts',(-19.3327969595686,59.8987752905502,
2.61946873372389));
#212225=CARTESIAN_POINT('Ctrl Pts',(-19.3501023532817,59.8974528651774,
2.61297662715609));
#212226=CARTESIAN_POINT('Ctrl Pts',(-19.3678190197503,59.8950748296131,
2.6078798911401));
#212227=CARTESIAN_POINT('Ctrl Pts',(-19.3856740904735,59.8915778894435,
2.6044061688622));
#212228=CARTESIAN_POINT('Ctrl Pts',(-19.394601625835,59.8898294193587,2.60266930772325));
#212229=CARTESIAN_POINT('Ctrl Pts',(-19.4035637624458,59.8878012237016,
2.60133820040226));
#212230=CARTESIAN_POINT('Ctrl Pts',(-19.4125263941846,59.8854853982055,
2.60044130723625));
#212231=CARTESIAN_POINT('Ctrl Pts',(-19.417007710054,59.8843274854575,2.59999286065325));
#212232=CARTESIAN_POINT('Ctrl Pts',(-19.4214891497435,59.8830976653669,
2.59965296768552));
#212233=CARTESIAN_POINT('Ctrl Pts',(-19.4259664502057,59.8817949505652,
2.59942518630994));
#212234=CARTESIAN_POINT('Ctrl Pts',(-19.4304437506678,59.8804922357634,
2.59919740493436));
#212235=CARTESIAN_POINT('Ctrl Pts',(-19.4349169113758,59.8791166246277,
2.59908173791657));
#212236=CARTESIAN_POINT('Ctrl Pts',(-19.4393816709759,59.8776671349986,
2.59908173516064));
#212237=CARTESIAN_POINT('',(-19.4684195516699,59.8682321556243,2.59908173516065));
#212238=CARTESIAN_POINT('Origin',(8.34054140790947E-18,1.90959676913043E-13,
2.59908173516022));
#212239=CARTESIAN_POINT('',(-19.6977666881848,59.5942745858237,2.90134173516065));
#212240=CARTESIAN_POINT('Ctrl Pts',(-19.4684195516699,59.8682321556243,
2.59908173516064));
#212241=CARTESIAN_POINT('Ctrl Pts',(-19.4720538382629,59.8670503242231,
2.59908174381719));
#212242=CARTESIAN_POINT('Ctrl Pts',(-19.4756634078263,59.8658263391019,
2.59915752001037));
#212243=CARTESIAN_POINT('Ctrl Pts',(-19.4792467723414,59.8645618637724,
2.59930729517512));
#212244=CARTESIAN_POINT('Ctrl Pts',(-19.4999541986765,59.8572547562683,
2.60017281085956));
#212245=CARTESIAN_POINT('Ctrl Pts',(-19.5197897600796,59.8485963666861,
2.60350651800078));
#212246=CARTESIAN_POINT('Ctrl Pts',(-19.538459369435,59.838909036811,2.60896880596448));
#212247=CARTESIAN_POINT('Ctrl Pts',(-19.5459892523631,59.8350019138254,
2.61117187235455));
#212248=CARTESIAN_POINT('Ctrl Pts',(-19.5533299158481,59.830927553989,2.61372076577216));
#212249=CARTESIAN_POINT('Ctrl Pts',(-19.560463883758,59.8267074486194,2.61659179897023));
#212250=CARTESIAN_POINT('Ctrl Pts',(-19.5630958847952,59.8251504859515,
2.61765103591249));
#212251=CARTESIAN_POINT('Ctrl Pts',(-19.5656996197547,59.8235736599161,
2.61875422455189));
#212252=CARTESIAN_POINT('Ctrl Pts',(-19.5682741459747,59.8219780387745,
2.61990022440436));
#212253=CARTESIAN_POINT('Ctrl Pts',(-19.5731013826371,59.818986249134,2.62204897412773));
#212254=CARTESIAN_POINT('Ctrl Pts',(-19.5778259323228,59.8159283829427,
2.62434823201809));
#212255=CARTESIAN_POINT('Ctrl Pts',(-19.5824415812277,59.8128114820622,
2.62679048030344));
#212256=CARTESIAN_POINT('Ctrl Pts',(-19.5985963523948,59.8019023289804,
2.63533834930218));
#212257=CARTESIAN_POINT('Ctrl Pts',(-19.6134170876084,59.7902699966957,
2.64563784783603));
#212258=CARTESIAN_POINT('Ctrl Pts',(-19.626637377817,59.7782164291177,2.65736666738005));
#212259=CARTESIAN_POINT('Ctrl Pts',(-19.6332475229213,59.7721896453286,
2.66323107715205));
#212260=CARTESIAN_POINT('Ctrl Pts',(-19.6394575570863,59.7660575536772,
2.66945281780814));
#212261=CARTESIAN_POINT('Ctrl Pts',(-19.645234181973,59.7598579055892,2.67599160631241));
#212262=CARTESIAN_POINT('Ctrl Pts',(-19.6481224944163,59.7567580815452,
2.67926100056455));
#212263=CARTESIAN_POINT('Ctrl Pts',(-19.6509024545773,59.7536413685034,
2.68260965685163));
#212264=CARTESIAN_POINT('Ctrl Pts',(-19.6535699003333,59.7505124858966,
2.68603254012522));
#212265=CARTESIAN_POINT('Ctrl Pts',(-19.6562373460892,59.7473836032897,
2.68945542339882));
#212266=CARTESIAN_POINT('Ctrl Pts',(-19.6587921483498,59.7442425399498,
2.69295261525425));
#212267=CARTESIAN_POINT('Ctrl Pts',(-19.6612304091763,59.7410940396264,
2.69651891172139));
#212268=CARTESIAN_POINT('Ctrl Pts',(-19.6612512024346,59.7410671895126,
2.69654932476127));
#212269=CARTESIAN_POINT('Ctrl Pts',(-19.6612719872239,59.7410403389973,
2.69657974261185));
#212270=CARTESIAN_POINT('Ctrl Pts',(-19.6612927635423,59.741013488083,2.69661016527013));
#212271=CARTESIAN_POINT('Ctrl Pts',(-19.6719035326719,59.727300334122,2.71214746101175));
#212272=CARTESIAN_POINT('Ctrl Pts',(-19.6804273096587,59.7135327604141,
2.72880565567622));
#212273=CARTESIAN_POINT('Ctrl Pts',(-19.6869782138553,59.6998755263162,
2.74628040012384));
#212274=CARTESIAN_POINT('Ctrl Pts',(-19.693750665282,59.68575641363,2.76434612882499));
#212275=CARTESIAN_POINT('Ctrl Pts',(-19.698414535934,59.6717543328732,2.78328592654569));
#212276=CARTESIAN_POINT('Ctrl Pts',(-19.7010437169739,59.6580526467544,
2.80278753267999));
#212277=CARTESIAN_POINT('Ctrl Pts',(-19.7036228854582,59.6446115955367,
2.82191817723016));
#212278=CARTESIAN_POINT('Ctrl Pts',(-19.7042436449211,59.6314587768735,
2.84159092315442));
#212279=CARTESIAN_POINT('Ctrl Pts',(-19.7029300451602,59.6187815171146,
2.86151233817369));
#212280=CARTESIAN_POINT('Ctrl Pts',(-19.7020598313709,59.6103832769659,
2.87470957721564));
#212281=CARTESIAN_POINT('Ctrl Pts',(-19.7003397858039,59.6021940468463,
2.88801594388491));
#212282=CARTESIAN_POINT('Ctrl Pts',(-19.6977666881848,59.5942745858237,
2.90134173516065));
#212283=CARTESIAN_POINT('',(-19.5876674457081,59.2554138597572,3.47153072139113));
#212284=CARTESIAN_POINT('',(-19.6977666881848,59.5942745858237,2.90134173516065));
#212285=CARTESIAN_POINT('',(-25.0931373005748,57.1420619865022,3.47153072139111));
#212286=CARTESIAN_POINT('Origin',(5.53234440788222E-15,1.85015204418142E-13,
3.47153072139072));
#212287=CARTESIAN_POINT('',(-25.2380597013433,57.4675553545141,2.90134173516062));
#212288=CARTESIAN_POINT('',(-25.0931373005748,57.1420619865022,3.47153072139111));
#212289=CARTESIAN_POINT('',(-25.5918112338797,57.5176823163889,2.59908173516063));
#212290=CARTESIAN_POINT('Ctrl Pts',(-25.2380597013433,57.4675553545141,
2.90134173516062));
#212291=CARTESIAN_POINT('Ctrl Pts',(-25.2430650965697,57.4787973317385,
2.88164837656627));
#212292=CARTESIAN_POINT('Ctrl Pts',(-25.2498357159836,57.4892091890306,
2.86203734438913));
#212293=CARTESIAN_POINT('Ctrl Pts',(-25.2582295402822,57.4986663319565,
2.84277945977796));
#212294=CARTESIAN_POINT('Ctrl Pts',(-25.2667920292312,57.5083135057489,
2.82313460919546));
#212295=CARTESIAN_POINT('Ctrl Pts',(-25.2770439485811,57.5169680778989,
2.80385576862757));
#212296=CARTESIAN_POINT('Ctrl Pts',(-25.2888863203068,57.5244844631399,
2.78521678517707));
#212297=CARTESIAN_POINT('Ctrl Pts',(-25.3002686266263,57.531708843628,2.76730190933709));
#212298=CARTESIAN_POINT('Ctrl Pts',(-25.3131208736917,57.5378823365845,
2.74997687278951));
#212299=CARTESIAN_POINT('Ctrl Pts',(-25.3273944332885,57.5428531464575,
2.73349253344838));
#212300=CARTESIAN_POINT('Ctrl Pts',(-25.3383588864659,57.5466715501105,
2.72082983598732));
#212301=CARTESIAN_POINT('Ctrl Pts',(-25.350162837837,57.5497799237802,2.70866321039035));
#212302=CARTESIAN_POINT('Ctrl Pts',(-25.3627976342212,57.5520966403721,
2.69711645335883));
#212303=CARTESIAN_POINT('Ctrl Pts',(-25.3628307477693,57.5521027120731,
2.69708619136789));
#212304=CARTESIAN_POINT('Ctrl Pts',(-25.3628638677133,57.5521087778607,
2.69705593387256));
#212305=CARTESIAN_POINT('Ctrl Pts',(-25.3628969940503,57.5521148377338,
2.69702568087608));
#212306=CARTESIAN_POINT('Ctrl Pts',(-25.3664488110204,57.5527645793671,
2.69378194443304));
#212307=CARTESIAN_POINT('Ctrl Pts',(-25.3700726756556,57.5533450954514,
2.69059266624738));
#212308=CARTESIAN_POINT('Ctrl Pts',(-25.3737637277665,57.5538555294218,
2.68746219342715));
#212309=CARTESIAN_POINT('Ctrl Pts',(-25.394303593528,57.5566959784095,2.67004182395906));
#212310=CARTESIAN_POINT('Ctrl Pts',(-25.41692331452,57.5573711352263,2.65443567877532));
#212311=CARTESIAN_POINT('Ctrl Pts',(-25.4407429579534,57.5557688601529,
2.6413685235262));
#212312=CARTESIAN_POINT('Ctrl Pts',(-25.4514335437849,57.5550497369114,
2.63550380329415));
#212313=CARTESIAN_POINT('Ctrl Pts',(-25.462366068343,57.5538721381539,2.63014997450983));
#212314=CARTESIAN_POINT('Ctrl Pts',(-25.4734629846669,57.5522269397032,
2.6253698111929));
#212315=CARTESIAN_POINT('Ctrl Pts',(-25.4782855544061,57.5515119587093,
2.6232924168711));
#212316=CARTESIAN_POINT('Ctrl Pts',(-25.4831389900605,57.5507085716897,
2.62132362131465));
#212317=CARTESIAN_POINT('Ctrl Pts',(-25.4880168077359,57.549815975347,2.61946873372385));
#212318=CARTESIAN_POINT('Ctrl Pts',(-25.5050891695995,57.5466918881477,
2.61297662715605));
#212319=CARTESIAN_POINT('Ctrl Pts',(-25.5224602099123,57.5424749837908,
2.60787989114007));
#212320=CARTESIAN_POINT('Ctrl Pts',(-25.5398519389078,57.5371308371211,
2.60440616886217));
#212321=CARTESIAN_POINT('Ctrl Pts',(-25.5485478034055,57.5344587637863,
2.60266930772322));
#212322=CARTESIAN_POINT('Ctrl Pts',(-25.557248840319,57.5315048804297,2.60133820040223));
#212323=CARTESIAN_POINT('Ctrl Pts',(-25.565920304143,57.5282648911455,2.60044130723623));
#212324=CARTESIAN_POINT('Ctrl Pts',(-25.5702560360551,57.5266448965034,
2.59999286065323));
#212325=CARTESIAN_POINT('Ctrl Pts',(-25.5745843747449,57.524953375492,2.5996529676855));
#212326=CARTESIAN_POINT('Ctrl Pts',(-25.5789009773103,57.5231897917614,
2.59942518630992));
#212327=CARTESIAN_POINT('Ctrl Pts',(-25.5832175798758,57.5214262080307,
2.59919740493434));
#212328=CARTESIAN_POINT('Ctrl Pts',(-25.5875224456232,57.5195905600219,
2.59908173791657));
#212329=CARTESIAN_POINT('Ctrl Pts',(-25.5918112338797,57.5176823163889,
2.59908173516063));
#212330=CARTESIAN_POINT('',(-25.61970381813,57.5052637377733,2.59908173516063));
#212331=CARTESIAN_POINT('Origin',(2.35274110347535E-17,1.90965506606098E-13,
2.59908173516024));
#212332=CARTESIAN_POINT('',(-25.8191582032623,57.2088336324699,2.90134173516062));
#212333=CARTESIAN_POINT('Ctrl Pts',(-25.61970381813,57.5052637377733,2.59908173516064));
#212334=CARTESIAN_POINT('Ctrl Pts',(-25.6231946607006,57.5037084941755,
2.59908174381719));
#212335=CARTESIAN_POINT('Ctrl Pts',(-25.6266565153805,57.5021139114134,
2.59915752001035));
#212336=CARTESIAN_POINT('Ctrl Pts',(-25.6300880761868,57.500481799426,2.59930729517509));
#212337=CARTESIAN_POINT('Ctrl Pts',(-25.649918264359,57.4910502055666,2.60017281085968));
#212338=CARTESIAN_POINT('Ctrl Pts',(-25.668740116327,57.4803658667948,2.60350651800195));
#212339=CARTESIAN_POINT('Ctrl Pts',(-25.6862948499065,57.4687800995483,
2.60896880596735));
#212340=CARTESIAN_POINT('Ctrl Pts',(-25.6933750777833,57.4641072931021,
2.61117187235676));
#212341=CARTESIAN_POINT('Ctrl Pts',(-25.7002496417701,57.4592879447638,
2.61372076577339));
#212342=CARTESIAN_POINT('Ctrl Pts',(-25.7069034079253,57.4543452548725,
2.61659179897021));
#212343=CARTESIAN_POINT('Ctrl Pts',(-25.7093582436704,57.4525217023853,
2.61765103591246));
#212344=CARTESIAN_POINT('Ctrl Pts',(-25.711782891895,57.4506813499538,2.61875422455187));
#212345=CARTESIAN_POINT('Ctrl Pts',(-25.7141765267651,57.4488253585223,
2.61990022440433));
#212346=CARTESIAN_POINT('Ctrl Pts',(-25.7186645921465,57.4453453745884,
2.6220489741277));
#212347=CARTESIAN_POINT('Ctrl Pts',(-25.7230436262008,57.4418104097897,
2.62434823201807));
#212348=CARTESIAN_POINT('Ctrl Pts',(-25.7273081852388,57.4382281169314,
2.62679048030342));
#212349=CARTESIAN_POINT('Ctrl Pts',(-25.742234141872,57.4256900919271,2.63533834930216));
#212350=CARTESIAN_POINT('Ctrl Pts',(-25.7557577777295,57.4125722940994,
2.645637847836));
#212351=CARTESIAN_POINT('Ctrl Pts',(-25.7676457049092,57.3992028606062,
2.65736666738001));
#212352=CARTESIAN_POINT('Ctrl Pts',(-25.7735896684991,57.3925181438597,
2.66323107715202));
#212353=CARTESIAN_POINT('Ctrl Pts',(-25.7791247053302,57.3857705191198,
2.66945281780811));
#212354=CARTESIAN_POINT('Ctrl Pts',(-25.7842216455739,57.3790010116304,
2.67599160631238));
#212355=CARTESIAN_POINT('Ctrl Pts',(-25.7867701156958,57.3756162578857,
2.67926100056452));
#212356=CARTESIAN_POINT('Ctrl Pts',(-25.7892090617194,57.3722260335606,
2.68260965685161));
#212357=CARTESIAN_POINT('Ctrl Pts',(-25.7915348376378,57.3688354672943,
2.6860325401252));
#212358=CARTESIAN_POINT('Ctrl Pts',(-25.7938606135562,57.365444901028,2.6894554233988));
#212359=CARTESIAN_POINT('Ctrl Pts',(-25.7960730898187,57.3620539952075,
2.69295261525422));
#212360=CARTESIAN_POINT('Ctrl Pts',(-25.7981688856969,57.358667875041,2.69651891172136));
#212361=CARTESIAN_POINT('Ctrl Pts',(-25.7981867584464,57.3586389985277,
2.69654932476124));
#212362=CARTESIAN_POINT('Ctrl Pts',(-25.7982046227313,57.3586101225002,
2.69657974261182));
#212363=CARTESIAN_POINT('Ctrl Pts',(-25.7982224785501,57.3585812469613,
2.6966101652701));
#212364=CARTESIAN_POINT('Ctrl Pts',(-25.8073417058664,57.3438340877009,
2.71214746101221));
#212365=CARTESIAN_POINT('Ctrl Pts',(-25.8143796853885,57.3292509568922,
2.72880565567726));
#212366=CARTESIAN_POINT('Ctrl Pts',(-25.8194671333539,57.3149837826026,
2.74628040012549));
#212367=CARTESIAN_POINT('Ctrl Pts',(-25.8247266354312,57.3002341019522,
2.76434612882735));
#212368=CARTESIAN_POINT('Ctrl Pts',(-25.8279013409277,57.2858212188262,
2.78328592654881));
#212369=CARTESIAN_POINT('Ctrl Pts',(-25.8290839028445,57.2719197677234,
2.80278753268388));
#212370=CARTESIAN_POINT('Ctrl Pts',(-25.8302439699452,57.2582827514722,
2.82191817723466));
#212371=CARTESIAN_POINT('Ctrl Pts',(-25.8294864849001,57.2451370982929,
2.84159092315952));
#212372=CARTESIAN_POINT('Ctrl Pts',(-25.8268549466945,57.2326665944535,
2.86151233817938));
#212373=CARTESIAN_POINT('Ctrl Pts',(-25.8251116448906,57.2244053228544,
2.87470957721946));
#212374=CARTESIAN_POINT('Ctrl Pts',(-25.8225450142736,57.2164407479154,
2.88801594388681));
#212375=CARTESIAN_POINT('Ctrl Pts',(-25.8191582032623,57.2088336324699,
2.90134173516062));
#212376=CARTESIAN_POINT('',(-25.6742415049982,56.8833377255395,3.47153072139111));
#212377=CARTESIAN_POINT('',(-25.8191582032623,57.2088336324699,2.90134173516062));
#212378=CARTESIAN_POINT('',(-30.9286463962981,54.2060847114742,3.47153072139109));
#212379=CARTESIAN_POINT('Origin',(5.53234440788222E-15,1.85015204418142E-13,
3.47153072139072));
#212380=CARTESIAN_POINT('',(-31.1067982185537,54.5146464769138,2.90134173516061));
#212381=CARTESIAN_POINT('',(-30.9286463962981,54.2060847114742,3.47153072139109));
#212382=CARTESIAN_POINT('',(-31.4638515574743,54.527521733972,2.59908173516061));
#212383=CARTESIAN_POINT('Ctrl Pts',(-31.1067982185537,54.5146464769138,
2.90134173516061));
#212384=CARTESIAN_POINT('Ctrl Pts',(-31.1129513003036,54.5253036631384,
2.88164837656892));
#212385=CARTESIAN_POINT('Ctrl Pts',(-31.120773164997,54.534950760743,2.8620373443944));
#212386=CARTESIAN_POINT('Ctrl Pts',(-31.1301095476631,54.5434787028948,
2.84277945978573));
#212387=CARTESIAN_POINT('Ctrl Pts',(-31.1396335346515,54.5521780046474,
2.82313460920559));
#212388=CARTESIAN_POINT('Ctrl Pts',(-31.1507339420397,54.5597135487699,
2.80385576863993));
#212389=CARTESIAN_POINT('Ctrl Pts',(-31.1632971162103,54.565950893548,2.78521678519144));
#212390=CARTESIAN_POINT('Ctrl Pts',(-31.1753722224535,54.5719459231359,
2.76730190935284));
#212391=CARTESIAN_POINT('Ctrl Pts',(-31.1887993692945,54.5767421714171,
2.74997687280646));
#212392=CARTESIAN_POINT('Ctrl Pts',(-31.2035143279533,54.580193757424,2.73349253346629));
#212393=CARTESIAN_POINT('Ctrl Pts',(-31.2148178485797,54.5828451460231,
2.72082983599878));
#212394=CARTESIAN_POINT('Ctrl Pts',(-31.2268820501983,54.5847026428005,
2.70866321039578));
#212395=CARTESIAN_POINT('Ctrl Pts',(-31.2396897946772,54.5856859723273,
2.69711645335882));
#212396=CARTESIAN_POINT('Ctrl Pts',(-31.2397233614914,54.5856885494586,
2.69708619136788));
#212397=CARTESIAN_POINT('Ctrl Pts',(-31.2397569340484,54.5856911200402,
2.69705593387255));
#212398=CARTESIAN_POINT('Ctrl Pts',(-31.239790512345,54.5856936840717,2.69702568087608));
#212399=CARTESIAN_POINT('Ctrl Pts',(-31.2433907885846,54.5859686003826,
2.69378194443303));
#212400=CARTESIAN_POINT('Ctrl Pts',(-31.2470554817643,54.5861671393377,
2.69059266624736));
#212401=CARTESIAN_POINT('Ctrl Pts',(-31.2507796687841,54.5862889570924,
2.68746219342713));
#212402=CARTESIAN_POINT('Ctrl Pts',(-31.2715039227763,54.5869668451994,
2.67004182396171));
#212403=CARTESIAN_POINT('Ctrl Pts',(-31.2940703036708,54.5852738987623,
2.65443567878008));
#212404=CARTESIAN_POINT('Ctrl Pts',(-31.3175919772501,54.5811905703971,
2.64136852353218));
#212405=CARTESIAN_POINT('Ctrl Pts',(-31.32814883009,54.5793579160793,2.63550380329779));
#212406=CARTESIAN_POINT('Ctrl Pts',(-31.3388983725498,54.5770440083387,
2.63014997451145));
#212407=CARTESIAN_POINT('Ctrl Pts',(-31.3497625287429,54.574247878846,2.62536981119289));
#212408=CARTESIAN_POINT('Ctrl Pts',(-31.3544839440759,54.5730327187889,
2.62329241687109));
#212409=CARTESIAN_POINT('Ctrl Pts',(-31.3592268152914,54.5717264106369,
2.62132362131464));
#212410=CARTESIAN_POINT('Ctrl Pts',(-31.3639846100471,54.5703288332447,
2.61946873372384));
#212411=CARTESIAN_POINT('Ctrl Pts',(-31.3806368916921,54.5654373123719,
2.61297662715604));
#212412=CARTESIAN_POINT('Ctrl Pts',(-31.3974719850964,54.5594277405091,
2.60787989114006));
#212413=CARTESIAN_POINT('Ctrl Pts',(-31.4142098249418,54.5522949389286,
2.60440616886217));
#212414=CARTESIAN_POINT('Ctrl Pts',(-31.4225787448645,54.5487285381383,
2.60266930772322));
#212415=CARTESIAN_POINT('Ctrl Pts',(-31.4309233516995,54.5448813304464,
2.60133820040221));
#212416=CARTESIAN_POINT('Ctrl Pts',(-31.4392086412365,54.5407526753748,
2.60044130723621));
#212417=CARTESIAN_POINT('Ctrl Pts',(-31.443351286005,54.5386883478389,2.59999286065321));
#212418=CARTESIAN_POINT('Ctrl Pts',(-31.4474791015107,54.5365536585648,
2.59965296768548));
#212419=CARTESIAN_POINT('Ctrl Pts',(-31.4515877125784,54.5343485280977,
2.5994251863099));
#212420=CARTESIAN_POINT('Ctrl Pts',(-31.4556963236462,54.5321433976305,
2.59919740493432));
#212421=CARTESIAN_POINT('Ctrl Pts',(-31.4597857294232,54.5298678244925,
2.59908173791653));
#212422=CARTESIAN_POINT('Ctrl Pts',(-31.4638515574743,54.527521733972,2.59908173516061));
#212423=CARTESIAN_POINT('',(-31.490293248291,54.5122556166611,2.59908173516061));
#212424=CARTESIAN_POINT('Origin',(3.80217165444497E-17,1.90972891823628E-13,
2.59908173516022));
#212425=CARTESIAN_POINT('',(-31.6576696180587,54.1966007261208,2.9013417351606));
#212426=CARTESIAN_POINT('Ctrl Pts',(-31.490293248291,54.5122556166611,2.59908173516061));
#212427=CARTESIAN_POINT('Ctrl Pts',(-31.4936024004374,54.5103440004411,
2.59908174381717));
#212428=CARTESIAN_POINT('Ctrl Pts',(-31.4968786114295,54.5083962906205,
2.59915752001032));
#212429=CARTESIAN_POINT('Ctrl Pts',(-31.5001207716287,54.5064144237356,
2.59930729517507));
#212430=CARTESIAN_POINT('Ctrl Pts',(-31.5188564579396,54.4949616780404,
2.6001728108595));
#212431=CARTESIAN_POINT('Ctrl Pts',(-31.5364583843175,54.4823684499346,
2.60350651800074));
#212432=CARTESIAN_POINT('Ctrl Pts',(-31.5527059087812,54.4690111814119,
2.60896880596443));
#212433=CARTESIAN_POINT('Ctrl Pts',(-31.559258909155,54.4636238877464,2.61117187235451));
#212434=CARTESIAN_POINT('Ctrl Pts',(-31.5655920544881,54.458112352691,2.61372076577212));
#212435=CARTESIAN_POINT('Ctrl Pts',(-31.57169271884,54.4525012314185,2.6165917989702));
#212436=CARTESIAN_POINT('Ctrl Pts',(-31.5739434935988,54.4504310683346,
2.61765103591245));
#212437=CARTESIAN_POINT('Ctrl Pts',(-31.5761624901353,54.4483473527934,
2.61875422455185));
#212438=CARTESIAN_POINT('Ctrl Pts',(-31.5783490084909,54.4462513257026,
2.61990022440431));
#212439=CARTESIAN_POINT('Ctrl Pts',(-31.5824487304078,54.4423212749074,
2.62204897412768));
#212440=CARTESIAN_POINT('Ctrl Pts',(-31.5864342712172,54.4383479413155,
2.62434823201804));
#212441=CARTESIAN_POINT('Ctrl Pts',(-31.5903010169872,54.4343395048295,
2.6267904803034));
#212442=CARTESIAN_POINT('Ctrl Pts',(-31.603834627182,54.4203099771284,2.63533834930213));
#212443=CARTESIAN_POINT('Ctrl Pts',(-31.6159129958989,54.4058504350958,
2.64563784783597));
#212444=CARTESIAN_POINT('Ctrl Pts',(-31.6263383134319,54.3913116139986,
2.65736666737999));
#212445=CARTESIAN_POINT('Ctrl Pts',(-31.6315509721984,54.3840422034501,
2.66323107715199));
#212446=CARTESIAN_POINT('Ctrl Pts',(-31.6363503686739,54.3767529740104,
2.66945281780809));
#212447=CARTESIAN_POINT('Ctrl Pts',(-31.6407117811307,54.3694877752603,
2.67599160631236));
#212448=CARTESIAN_POINT('Ctrl Pts',(-31.6428924873591,54.3658551758853,
2.67926100056449));
#212449=CARTESIAN_POINT('Ctrl Pts',(-31.6449636976424,54.3622285842839,
2.68260965685157));
#212450=CARTESIAN_POINT('Ctrl Pts',(-31.6469223220355,54.3586134821117,
2.68603254012517));
#212451=CARTESIAN_POINT('Ctrl Pts',(-31.6488809464286,54.3549983799396,
2.68945542339876));
#212452=CARTESIAN_POINT('Ctrl Pts',(-31.6507268563402,54.3513947831121,
2.6929526152542));
#212453=CARTESIAN_POINT('Ctrl Pts',(-31.6524572252918,54.3478081421438,
2.69651891172134));
#212454=CARTESIAN_POINT('Ctrl Pts',(-31.652471981715,54.347777555608,2.69654932476122));
#212455=CARTESIAN_POINT('Ctrl Pts',(-31.6524867297707,54.3477469704401,
2.6965797426118));
#212456=CARTESIAN_POINT('Ctrl Pts',(-31.6525014694577,54.3477163866432,
2.69661016527008));
#212457=CARTESIAN_POINT('Ctrl Pts',(-31.6600292427979,54.332096795046,2.71214746101276));
#212458=CARTESIAN_POINT('Ctrl Pts',(-31.6655043152788,54.3168578829693,
2.72880565567847));
#212459=CARTESIAN_POINT('Ctrl Pts',(-31.6690725678682,54.3021370826349,
2.7462804001274));
#212460=CARTESIAN_POINT('Ctrl Pts',(-31.6727614963908,54.2869184346083,
2.76434612882998));
#212461=CARTESIAN_POINT('Ctrl Pts',(-31.6744122539938,54.2722526596768,
2.78328592655222));
#212462=CARTESIAN_POINT('Ctrl Pts',(-31.6741352403914,54.2583037507974,
2.80278753268809));
#212463=CARTESIAN_POINT('Ctrl Pts',(-31.6738634961706,54.2446201795163,
2.82191817723965));
#212464=CARTESIAN_POINT('Ctrl Pts',(-31.6717360657818,54.2316257183479,
2.84159092316531));
#212465=CARTESIAN_POINT('Ctrl Pts',(-31.6678154208149,54.2194985998778,
2.86151233818597));
#212466=CARTESIAN_POINT('Ctrl Pts',(-31.6652181309759,54.211464809049,2.87470957722388));
#212467=CARTESIAN_POINT('Ctrl Pts',(-31.6618330358515,54.2038121508403,
2.88801594388901));
#212468=CARTESIAN_POINT('Ctrl Pts',(-31.6576696180587,54.1966007261208,
2.9013417351606));
#212469=CARTESIAN_POINT('',(-31.4795232016792,53.8880358395971,3.47153072139108));
#212470=CARTESIAN_POINT('',(-31.6576696180587,54.1966007261208,2.90134173516061));
#212471=CARTESIAN_POINT('',(-36.4252947698681,50.6762142289948,3.47153072139106));
#212472=CARTESIAN_POINT('Origin',(5.53234440788222E-15,1.85015204418142E-13,
3.47153072139072));
#212473=CARTESIAN_POINT('',(-36.6347241449657,50.9644637245893,2.90134173516059));
#212474=CARTESIAN_POINT('',(-36.4252947698681,50.6762142289948,3.47153072139106));
#212475=CARTESIAN_POINT('',(-36.991167339171,50.9399462128202,2.59908173516058));
#212476=CARTESIAN_POINT('Ctrl Pts',(-36.6347241449657,50.9644637245893,
2.90134173516059));
#212477=CARTESIAN_POINT('Ctrl Pts',(-36.6419574987897,50.9744193574538,
2.88164837656681));
#212478=CARTESIAN_POINT('Ctrl Pts',(-36.6507449107787,50.9831959997528,
2.86203734439024));
#212479=CARTESIAN_POINT('Ctrl Pts',(-36.6609215604531,50.9907013072131,
2.84277945977961));
#212480=CARTESIAN_POINT('Ctrl Pts',(-36.6713026986892,50.9983574255568,
2.82313460919768));
#212481=CARTESIAN_POINT('Ctrl Pts',(-36.6831299757328,51.0046913806545,
2.80385576863033));
#212482=CARTESIAN_POINT('Ctrl Pts',(-36.6962763075871,51.0095813473154,
2.78521678518032));
#212483=CARTESIAN_POINT('Ctrl Pts',(-36.7089119163662,51.0142813432044,
2.76730190934075));
#212484=CARTESIAN_POINT('Ctrl Pts',(-36.7227668523555,51.0176477981099,
2.74997687279352));
#212485=CARTESIAN_POINT('Ctrl Pts',(-36.7377619899139,51.0195423439513,
2.73349253345269));
#212486=CARTESIAN_POINT('Ctrl Pts',(-36.7492807342437,51.0209976683244,
2.72082983599006));
#212487=CARTESIAN_POINT('Ctrl Pts',(-36.7614730081831,51.0215839370839,
2.70866321039163));
#212488=CARTESIAN_POINT('Ctrl Pts',(-36.7743133764174,51.0212231059805,
2.69711645335879));
#212489=CARTESIAN_POINT('Ctrl Pts',(-36.7743470287326,51.0212221603065,
2.69708619136785));
#212490=CARTESIAN_POINT('Ctrl Pts',(-36.7743806860745,51.0212212075184,
2.69705593387252));
#212491=CARTESIAN_POINT('Ctrl Pts',(-36.77441434844,51.0212202476161,2.69702568087604));
#212492=CARTESIAN_POINT('Ctrl Pts',(-36.7780236385692,51.021117326564,2.693781944433));
#212493=CARTESIAN_POINT('Ctrl Pts',(-36.7816890091481,51.0209317131555,
2.69059266624734));
#212494=CARTESIAN_POINT('Ctrl Pts',(-36.7854055281044,51.0206635800337,
2.68746219342711));
#212495=CARTESIAN_POINT('Ctrl Pts',(-36.8060871110679,51.0191714801765,
2.67004182396082));
#212496=CARTESIAN_POINT('Ctrl Pts',(-36.8283529098785,51.0151289787604,
2.6544356787785));
#212497=CARTESIAN_POINT('Ctrl Pts',(-36.851318905231,51.008609334902,2.64136852353021));
#212498=CARTESIAN_POINT('Ctrl Pts',(-36.8616263619858,51.0056832284522,
2.63550380329658));
#212499=CARTESIAN_POINT('Ctrl Pts',(-36.8720751481058,51.0022583633864,
2.63014997451091));
#212500=CARTESIAN_POINT('Ctrl Pts',(-36.8825875141944,50.9983419378325,
2.62536981119287));
#212501=CARTESIAN_POINT('Ctrl Pts',(-36.8871560463068,50.9966399122601,
2.62329241687107));
#212502=CARTESIAN_POINT('Ctrl Pts',(-36.8917363891939,50.9948449951613,
2.62132362131461));
#212503=CARTESIAN_POINT('Ctrl Pts',(-36.896322033635,50.9929577488699,2.61946873372381));
#212504=CARTESIAN_POINT('Ctrl Pts',(-36.9123717891789,50.9863523868501,
2.61297662715601));
#212505=CARTESIAN_POINT('Ctrl Pts',(-36.9284864868683,50.9786159896082,
2.60787989114004));
#212506=CARTESIAN_POINT('Ctrl Pts',(-36.9443870542878,50.9697726815835,
2.60440616886214));
#212507=CARTESIAN_POINT('Ctrl Pts',(-36.9523373379975,50.9653510275712,
2.6026693077232));
#212508=CARTESIAN_POINT('Ctrl Pts',(-36.9602340894951,50.9606526463566,
2.60133820040219));
#212509=CARTESIAN_POINT('Ctrl Pts',(-36.9680424293792,50.9556805599063,
2.60044130723619));
#212510=CARTESIAN_POINT('Ctrl Pts',(-36.9719465993212,50.9531945166812,
2.59999286065319));
#212511=CARTESIAN_POINT('Ctrl Pts',(-36.9758286664323,50.9506400472469,
2.59965296768546));
#212512=CARTESIAN_POINT('Ctrl Pts',(-36.9796842711996,50.9480175299141,
2.59942518630988));
#212513=CARTESIAN_POINT('Ctrl Pts',(-36.983539875967,50.9453950125813,2.5991974049343));
#212514=CARTESIAN_POINT('Ctrl Pts',(-36.9873690173881,50.9427044459694,
2.59908173791649));
#212515=CARTESIAN_POINT('Ctrl Pts',(-36.991167339171,50.9399462128202,2.59908173516058));
#212516=CARTESIAN_POINT('',(-37.0158684358562,50.92199981559,2.59908173516059));
#212517=CARTESIAN_POINT('Origin',(5.16646552926933E-17,1.90981751651644E-13,
2.59908173516023));
#212518=CARTESIAN_POINT('',(-37.1493329797263,50.5905785208484,2.90134173516058));
#212519=CARTESIAN_POINT('Ctrl Pts',(-37.0158684358562,50.92199981559,2.59908173516059));
#212520=CARTESIAN_POINT('Ctrl Pts',(-37.0189596418151,50.9197527708151,
2.59908174381714));
#212521=CARTESIAN_POINT('Ctrl Pts',(-37.0220143142661,50.9174732734523,
2.5991575200103));
#212522=CARTESIAN_POINT('Ctrl Pts',(-37.0250315520727,50.9151633654183,
2.59930729517505));
#212523=CARTESIAN_POINT('Ctrl Pts',(-37.0424674644257,50.9018149465641,
2.60017281085948));
#212524=CARTESIAN_POINT('Ctrl Pts',(-37.0586566148275,50.8874508031649,
2.60350651800064));
#212525=CARTESIAN_POINT('Ctrl Pts',(-37.0734189188999,50.8724683783928,
2.60896880596422));
#212526=CARTESIAN_POINT('Ctrl Pts',(-37.0793728957242,50.8664256218267,
2.61117187235434));
#212527=CARTESIAN_POINT('Ctrl Pts',(-37.085095235135,50.8602822855875,2.61372076577201));
#212528=CARTESIAN_POINT('Ctrl Pts',(-37.0905759575257,50.8540642095547,
2.61659179897017));
#212529=CARTESIAN_POINT('Ctrl Pts',(-37.092598011339,50.851770117014,2.61765103591242));
#212530=CARTESIAN_POINT('Ctrl Pts',(-37.0945870443968,50.8494658679866,
2.61875422455183));
#212531=CARTESIAN_POINT('Ctrl Pts',(-37.0965424902854,50.8471527697479,
2.6199002244043));
#212532=CARTESIAN_POINT('Ctrl Pts',(-37.1002089513264,50.8428157105504,
2.62204897412767));
#212533=CARTESIAN_POINT('Ctrl Pts',(-37.1037573324719,50.8384475408395,
2.62434823201804));
#212534=CARTESIAN_POINT('Ctrl Pts',(-37.107183900098,50.8340568779948,2.62679048030339));
#212535=CARTESIAN_POINT('Ctrl Pts',(-37.1191768867891,50.8186895580383,
2.63533834930213));
#212536=CARTESIAN_POINT('Ctrl Pts',(-37.1296776552302,50.8030466935691,
2.64563784783596));
#212537=CARTESIAN_POINT('Ctrl Pts',(-37.1385261411559,50.7874977752343,
2.65736666737998));
#212538=CARTESIAN_POINT('Ctrl Pts',(-37.1429503841188,50.7797233160669,
2.66323107715198));
#212539=CARTESIAN_POINT('Ctrl Pts',(-37.1469615570465,50.7719723442507,
2.66945281780807));
#212540=CARTESIAN_POINT('Ctrl Pts',(-37.1505396571688,50.7642910532777,
2.67599160631234));
#212541=CARTESIAN_POINT('Ctrl Pts',(-37.1523287072299,50.7604504077913,
2.67926100056447));
#212542=CARTESIAN_POINT('Ctrl Pts',(-37.1540094891596,50.7566271826101,
2.68260965685158));
#212543=CARTESIAN_POINT('Ctrl Pts',(-37.1555795029288,50.7528271523479,
2.68603254012517));
#212544=CARTESIAN_POINT('Ctrl Pts',(-37.1571495166979,50.7490271220858,
2.68945542339877));
#212545=CARTESIAN_POINT('Ctrl Pts',(-37.1586086360832,50.7452503160125,
2.6929526152542));
#212546=CARTESIAN_POINT('Ctrl Pts',(-37.159954619824,50.7415024502313,2.69651891172134));
#212547=CARTESIAN_POINT('Ctrl Pts',(-37.1599660982463,50.7414704887854,
2.69654932476122));
#212548=CARTESIAN_POINT('Ctrl Pts',(-37.15997756849,50.7414385295747,2.6965797426118));
#212549=CARTESIAN_POINT('Ctrl Pts',(-37.1599890305542,50.7414065726022,
2.69661016527007));
#212550=CARTESIAN_POINT('Ctrl Pts',(-37.1658428740569,50.7250856801856,
2.71214746101035));
#212551=CARTESIAN_POINT('Ctrl Pts',(-37.1696950534564,50.7093579475533,
2.7288056556733));
#212552=CARTESIAN_POINT('Ctrl Pts',(-37.171705016148,50.6943448053458,2.74628040011927));
#212553=CARTESIAN_POINT('Ctrl Pts',(-37.1737829544432,50.6788239286381,
2.76434612881873));
#212554=CARTESIAN_POINT('Ctrl Pts',(-37.1738916781079,50.6640659432027,
2.78328592653761));
#212555=CARTESIAN_POINT('Ctrl Pts',(-37.172158124007,50.6502224037134,2.80278753267004));
#212556=CARTESIAN_POINT('Ctrl Pts',(-37.1704575457528,50.6366421974747,
2.82191817721855));
#212557=CARTESIAN_POINT('Ctrl Pts',(-37.1669834785952,50.6239412983545,
2.84159092314111));
#212558=CARTESIAN_POINT('Ctrl Pts',(-37.1618166822764,50.6122904325024,
2.86151233815872));
#212559=CARTESIAN_POINT('Ctrl Pts',(-37.1583938608521,50.6045721423299,
2.87470957720556));
#212560=CARTESIAN_POINT('Ctrl Pts',(-37.1542273890282,50.5973152449696,
2.88801594387984));
#212561=CARTESIAN_POINT('Ctrl Pts',(-37.1493329797263,50.5905785208484,
2.90134173516058));
#212562=CARTESIAN_POINT('',(-36.9399086546489,50.3023253561995,3.47153072139106));
#212563=CARTESIAN_POINT('',(-37.1493329797263,50.5905785208484,2.90134173516058));
#212564=CARTESIAN_POINT('',(-41.5228599914565,46.591124538743,3.47153072139103));
#212565=CARTESIAN_POINT('Origin',(5.53234440788222E-15,1.85015204418142E-13,
3.47153072139072));
#212566=CARTESIAN_POINT('',(-41.7612723673365,46.8559036426985,2.90134173516056));
#212567=CARTESIAN_POINT('',(-41.5228599914565,46.591124538743,3.47153072139103));
#212568=CARTESIAN_POINT('',(-42.1132001506003,46.7942619810917,2.59908173516055));
#212569=CARTESIAN_POINT('Ctrl Pts',(-41.7612723673365,46.8559036426985,
2.90134173516056));
#212570=CARTESIAN_POINT('Ctrl Pts',(-41.7695067430953,46.8650486462049,
2.88164837656725));
#212571=CARTESIAN_POINT('Ctrl Pts',(-41.7791634256538,46.8728586744676,
2.86203734439113));
#212572=CARTESIAN_POINT('Ctrl Pts',(-41.7900688448314,46.8792591175166,
2.84277945978094));
#212573=CARTESIAN_POINT('Ctrl Pts',(-41.8011933963908,46.8857881704162,
2.82313460919932));
#212574=CARTESIAN_POINT('Ctrl Pts',(-41.8136179609658,46.890851140351,2.80385576863226));
#212575=CARTESIAN_POINT('Ctrl Pts',(-41.8272034165388,46.8943401533967,
2.78521678518251));
#212576=CARTESIAN_POINT('Ctrl Pts',(-41.8402610894785,46.8976936214484,
2.76730190934294));
#212577=CARTESIAN_POINT('Ctrl Pts',(-41.8543920170367,46.8995933993941,
2.7499768727957));
#212578=CARTESIAN_POINT('Ctrl Pts',(-41.8695030436278,46.8999101480298,
2.73349253345484));
#212579=CARTESIAN_POINT('Ctrl Pts',(-41.8811108098919,46.9001534633403,
2.72082983599143));
#212580=CARTESIAN_POINT('Ctrl Pts',(-41.8932975750521,46.8994620807995,
2.70866321039226));
#212581=CARTESIAN_POINT('Ctrl Pts',(-41.9060298852857,46.8977610424072,
2.69711645335876));
#212582=CARTESIAN_POINT('Ctrl Pts',(-41.9060632544001,46.897756584289,2.69708619136782));
#212583=CARTESIAN_POINT('Ctrl Pts',(-41.9060966277702,46.8977521185701,
2.69705593387249));
#212584=CARTESIAN_POINT('Ctrl Pts',(-41.9061300053926,46.8977476452509,
2.69702568087601));
#212585=CARTESIAN_POINT('Ctrl Pts',(-41.9097087652734,46.8972680144605,
2.69378194443296));
#212586=CARTESIAN_POINT('Ctrl Pts',(-41.9133346546844,46.8967002823077,
2.6905926662473));
#212587=CARTESIAN_POINT('Ctrl Pts',(-41.9170027866178,46.896045136032,2.68746219342707));
#212588=CARTESIAN_POINT('Ctrl Pts',(-41.9374151068008,46.8923993959688,
2.67004182396078));
#212589=CARTESIAN_POINT('Ctrl Pts',(-41.9591363747749,46.8860516300653,
2.65443567877847));
#212590=CARTESIAN_POINT('Ctrl Pts',(-41.9812950716484,46.8771671012965,
2.64136852353018));
#212591=CARTESIAN_POINT('Ctrl Pts',(-41.991240201666,46.8731796017492,2.63550380329656));
#212592=CARTESIAN_POINT('Ctrl Pts',(-42.0012737523602,46.8686813028964,
2.63014997451089));
#212593=CARTESIAN_POINT('Ctrl Pts',(-42.0113191526627,46.863687490459,2.62536981119286));
#212594=CARTESIAN_POINT('Ctrl Pts',(-42.0156847477607,46.8615172471197,
2.62329241687106));
#212595=CARTESIAN_POINT('Ctrl Pts',(-42.0200523791242,46.8592533865613,
2.62132362131461));
#212596=CARTESIAN_POINT('Ctrl Pts',(-42.0244156319706,46.8568971484361,
2.61946873372381));
#212597=CARTESIAN_POINT('Ctrl Pts',(-42.039687016933,46.8486503149977,2.612976627156));
#212598=CARTESIAN_POINT('Ctrl Pts',(-42.0549047629075,46.8392718539638,
2.60787989114001));
#212599=CARTESIAN_POINT('Ctrl Pts',(-42.0697938479569,46.8288149286284,
2.60440616886211));
#212600=CARTESIAN_POINT('Ctrl Pts',(-42.0772383904816,46.8235864659607,
2.60266930772316));
#212601=CARTESIAN_POINT('Ctrl Pts',(-42.0846007681801,46.8180883876711,
2.60133820040216));
#212602=CARTESIAN_POINT('Ctrl Pts',(-42.0918466086054,46.8123273450619,
2.60044130723616));
#212603=CARTESIAN_POINT('Ctrl Pts',(-42.095469528818,46.8094468237573,2.59999286065315));
#212604=CARTESIAN_POINT('Ctrl Pts',(-42.0990633147948,46.8065005614644,
2.59965296768544));
#212605=CARTESIAN_POINT('Ctrl Pts',(-42.1026236704492,46.8034893901146,
2.59942518630986));
#212606=CARTESIAN_POINT('Ctrl Pts',(-42.1061840261035,46.8004782187649,
2.59919740493428));
#212607=CARTESIAN_POINT('Ctrl Pts',(-42.109710950294,46.79740213709,2.5990817379165));
#212608=CARTESIAN_POINT('Ctrl Pts',(-42.1132001506003,46.7942619810917,
2.59908173516055));
#212609=CARTESIAN_POINT('',(-42.1358900227697,46.7738319284257,2.59908173516056));
#212610=CARTESIAN_POINT('Origin',(6.43067523875937E-17,1.90991989020018E-13,
2.59908173516023));
#212611=CARTESIAN_POINT('',(-42.2339804752703,46.4302753505425,2.90134173516055));
#212612=CARTESIAN_POINT('Ctrl Pts',(-42.1358900227697,46.7738319284257,
2.59908173516056));
#212613=CARTESIAN_POINT('Ctrl Pts',(-42.1387294146417,46.7712740741887,
2.59908174381715));
#212614=CARTESIAN_POINT('Ctrl Pts',(-42.141529080921,46.7686877639339,2.59915752001027));
#212615=CARTESIAN_POINT('Ctrl Pts',(-42.1442883388461,46.7660751225865,
2.59930729517502));
#212616=CARTESIAN_POINT('Ctrl Pts',(-42.1602334457364,46.7509772786441,
2.60017281085941));
#212617=CARTESIAN_POINT('Ctrl Pts',(-42.1748324484422,46.7349995965129,
2.60350651800036));
#212618=CARTESIAN_POINT('Ctrl Pts',(-42.1879477932305,46.7185561660731,
2.60896880596357));
#212619=CARTESIAN_POINT('Ctrl Pts',(-42.1932375134895,46.7119241523113,
2.61117187235383));
#212620=CARTESIAN_POINT('Ctrl Pts',(-42.1982863518305,46.7052163225653,
2.61372076577171));
#212621=CARTESIAN_POINT('Ctrl Pts',(-42.2030870843187,46.6984594183138,
2.61659179897015));
#212622=CARTESIAN_POINT('Ctrl Pts',(-42.2048582631418,46.6959665308744,
2.6176510359124));
#212623=CARTESIAN_POINT('Ctrl Pts',(-42.2065955404586,46.6934669941954,
2.6187542245518));
#212624=CARTESIAN_POINT('Ctrl Pts',(-42.2082984896057,46.6909621675971,
2.61990022440427));
#212625=CARTESIAN_POINT('Ctrl Pts',(-42.2114915192564,46.6862656177254,
2.62204897412764));
#212626=CARTESIAN_POINT('Ctrl Pts',(-42.2145638639316,46.681550470477,2.624348232018));
#212627=CARTESIAN_POINT('Ctrl Pts',(-42.2175127112218,46.6768256862946,
2.62679048030335));
#212628=CARTESIAN_POINT('Ctrl Pts',(-42.2278336767374,46.6602889416559,
2.63533834930209));
#212629=CARTESIAN_POINT('Ctrl Pts',(-42.2366417962861,46.6436341412466,
2.64563784783593));
#212630=CARTESIAN_POINT('Ctrl Pts',(-42.2438165047411,46.6272454828774,
2.65736666737995));
#212631=CARTESIAN_POINT('Ctrl Pts',(-42.2474038589686,46.6190511536928,
2.66323107715195));
#212632=CARTESIAN_POINT('Ctrl Pts',(-42.2505828610985,46.610923360769,2.66945281780804));
#212633=CARTESIAN_POINT('Ctrl Pts',(-42.2533384464727,46.6029101354046,
2.67599160631231));
#212634=CARTESIAN_POINT('Ctrl Pts',(-42.2547162391598,46.5989035227223,
2.67926100056444));
#212635=CARTESIAN_POINT('Ctrl Pts',(-42.2559881777373,46.5949255520165,
2.68260965685153));
#212636=CARTESIAN_POINT('Ctrl Pts',(-42.257152379483,46.5909822275912,2.68603254012512));
#212637=CARTESIAN_POINT('Ctrl Pts',(-42.2583165812288,46.5870389031658,
2.68945542339871));
#212638=CARTESIAN_POINT('Ctrl Pts',(-42.2593729236706,46.5831302673243,
2.69295261525415));
#212639=CARTESIAN_POINT('Ctrl Pts',(-42.2603197753209,46.5792622391319,
2.69651891172129));
#212640=CARTESIAN_POINT('Ctrl Pts',(-42.2603278499825,46.5792292529524,
2.69654932476117));
#212641=CARTESIAN_POINT('Ctrl Pts',(-42.2603359167438,46.5791962698506,
2.69657974261176));
#212642=CARTESIAN_POINT('Ctrl Pts',(-42.2603439756043,46.5791632898298,
2.69661016527004));
#212643=CARTESIAN_POINT('Ctrl Pts',(-42.2644597533368,46.5623199117021,
2.71214746101208));
#212644=CARTESIAN_POINT('Ctrl Pts',(-42.2666468343717,46.5462756748402,
2.72880565567704));
#212645=CARTESIAN_POINT('Ctrl Pts',(-42.2670764855933,46.5311346778838,
2.74628040012518));
#212646=CARTESIAN_POINT('Ctrl Pts',(-42.2675206673338,46.5154816224641,
2.76434612882708));
#212647=CARTESIAN_POINT('Ctrl Pts',(-42.2660861658596,46.5007931180981,
2.78328592654859));
#212648=CARTESIAN_POINT('Ctrl Pts',(-42.2629150644391,46.4872066207116,
2.80278753268372));
#212649=CARTESIAN_POINT('Ctrl Pts',(-42.2598042840403,46.473878567094,2.82191817723495));
#212650=CARTESIAN_POINT('Ctrl Pts',(-42.2550216427174,46.4616103837285,
2.8415909231603));
#212651=CARTESIAN_POINT('Ctrl Pts',(-42.2486653035442,46.4505634198172,
2.86151233818066));
#212652=CARTESIAN_POINT('Ctrl Pts',(-42.2444544516846,46.443245193514,2.8747095772203));
#212653=CARTESIAN_POINT('Ctrl Pts',(-42.2395522519026,46.4364635650978,
2.8880159438872));
#212654=CARTESIAN_POINT('Ctrl Pts',(-42.2339804752703,46.4302753505425,
2.90134173516055));
#212655=CARTESIAN_POINT('',(-41.9955727382253,46.1654920697612,3.47153072139103));
#212656=CARTESIAN_POINT('',(-42.2339804752703,46.4302753505425,2.90134173516055));
#212657=CARTESIAN_POINT('',(-46.1654920697614,41.995572738225,3.47153072139101));
#212658=CARTESIAN_POINT('Origin',(5.53234440788222E-15,1.85015204418142E-13,
3.47153072139072));
#212659=CARTESIAN_POINT('',(-46.4302753505427,42.2339804752701,2.90134173516052));
#212660=CARTESIAN_POINT('',(-46.1654920697614,41.995572738225,3.471530721391));
#212661=CARTESIAN_POINT('',(-46.7738319284259,42.1358900227694,2.59908173516052));
#212662=CARTESIAN_POINT('Ctrl Pts',(-46.4302753505427,42.2339804752701,
2.90134173516052));
#212663=CARTESIAN_POINT('Ctrl Pts',(-46.4394205306926,42.2422146548461,
2.88164837656763));
#212664=CARTESIAN_POINT('Ctrl Pts',(-46.4498406831858,42.2489725007686,
2.86203734439193));
#212665=CARTESIAN_POINT('Ctrl Pts',(-46.4613553898119,42.2541979548129,
2.84277945978213));
#212666=CARTESIAN_POINT('Ctrl Pts',(-46.4731014717798,42.2595284085983,
2.82313460920106));
#212667=CARTESIAN_POINT('Ctrl Pts',(-46.4859871977564,42.2632649224123,
2.80385576863452));
#212668=CARTESIAN_POINT('Ctrl Pts',(-46.4998629319538,42.2653147554857,
2.78521678518525));
#212669=CARTESIAN_POINT('Ctrl Pts',(-46.5131996064562,42.2672849544025,
2.76730190934637));
#212670=CARTESIAN_POINT('Ctrl Pts',(-46.5274517041831,42.2676972410239,
2.74997687279975));
#212671=CARTESIAN_POINT('Ctrl Pts',(-46.5425130602368,42.2664327220898,
2.73349253345943));
#212672=CARTESIAN_POINT('Ctrl Pts',(-46.5540826713195,42.2654613625242,
2.72082983599435));
#212673=CARTESIAN_POINT('Ctrl Pts',(-46.566130406952,42.2634999036149,2.70866321039363));
#212674=CARTESIAN_POINT('Ctrl Pts',(-46.5786151613303,42.2604772948659,
2.69711645335872));
#212675=CARTESIAN_POINT('Ctrl Pts',(-46.578647881645,42.2604693731475,2.69708619136778));
#212676=CARTESIAN_POINT('Ctrl Pts',(-46.5786806053975,42.2604614434252,
2.69705593387246));
#212677=CARTESIAN_POINT('Ctrl Pts',(-46.5787133325845,42.2604535056997,
2.69702568087598));
#212678=CARTESIAN_POINT('Ctrl Pts',(-46.5822223525748,42.2596024201062,
2.69378194443293));
#212679=CARTESIAN_POINT('Ctrl Pts',(-46.5857690348148,42.2586587894014,
2.69059266624727));
#212680=CARTESIAN_POINT('Ctrl Pts',(-46.5893485909042,42.2576238078915,
2.68746219342704));
#212681=CARTESIAN_POINT('Ctrl Pts',(-46.6092680066546,42.2518643711136,
2.67004182396129));
#212682=CARTESIAN_POINT('Ctrl Pts',(-46.6302067610343,42.2432808881746,
2.65443567877939));
#212683=CARTESIAN_POINT('Ctrl Pts',(-46.6513153841081,42.2321288152523,
2.64136852353134));
#212684=CARTESIAN_POINT('Ctrl Pts',(-46.6607892264636,42.2271236104868,
2.63550380329725));
#212685=CARTESIAN_POINT('Ctrl Pts',(-46.6702976120515,42.2216011621503,
2.63014997451117));
#212686=CARTESIAN_POINT('Ctrl Pts',(-46.6797659870608,42.2155846760829,
2.62536981119281));
#212687=CARTESIAN_POINT('Ctrl Pts',(-46.6838808147709,42.2129699926169,
2.62329241687101));
#212688=CARTESIAN_POINT('Ctrl Pts',(-46.6879878819276,42.210261991929,2.62132362131455));
#212689=CARTESIAN_POINT('Ctrl Pts',(-46.692080938468,42.2074625774078,2.61946873372376));
#212690=CARTESIAN_POINT('Ctrl Pts',(-46.7064066363596,42.1976646265838,
2.61297662715596));
#212691=CARTESIAN_POINT('Ctrl Pts',(-46.7205607018097,42.1867468541397,
2.60787989113998));
#212692=CARTESIAN_POINT('Ctrl Pts',(-46.7342751765575,42.1747908797557,
2.60440616886208));
#212693=CARTESIAN_POINT('Ctrl Pts',(-46.7411324139314,42.1688128925637,
2.60266930772313));
#212694=CARTESIAN_POINT('Ctrl Pts',(-46.74787975408,42.1625753552954,2.60133820040213));
#212695=CARTESIAN_POINT('Ctrl Pts',(-46.7544837081025,42.1560884757157,
2.60044130723612));
#212696=CARTESIAN_POINT('Ctrl Pts',(-46.7577856851138,42.1528450359258,
2.59999286065312));
#212697=CARTESIAN_POINT('Ctrl Pts',(-46.7610518156851,42.1495392606406,
2.59965296768541));
#212698=CARTESIAN_POINT('Ctrl Pts',(-46.7642779142248,42.1461724262973,
2.59942518630983));
#212699=CARTESIAN_POINT('Ctrl Pts',(-46.7675040127646,42.142805591954,2.59919740493425));
#212700=CARTESIAN_POINT('Ctrl Pts',(-46.770690078005,42.1393776974108,2.59908173791641));
#212701=CARTESIAN_POINT('Ctrl Pts',(-46.773831928426,42.1358900227694,2.59908173516052));
#212702=CARTESIAN_POINT('',(-46.7942619810919,42.1132001506,2.59908173516053));
#212703=CARTESIAN_POINT('Origin',(7.58094983678529E-17,1.91003491765998E-13,
2.59908173516023));
#212704=CARTESIAN_POINT('',(-46.8559036426987,41.7612723673362,2.90134173516051));
#212705=CARTESIAN_POINT('Ctrl Pts',(-46.7942619810919,42.1132001506,2.59908173516052));
#212706=CARTESIAN_POINT('Ctrl Pts',(-46.7968184499054,42.1103595112871,
2.5990817438171));
#212707=CARTESIAN_POINT('Ctrl Pts',(-46.7993324362835,42.1074947242967,
2.59915752001025));
#212708=CARTESIAN_POINT('Ctrl Pts',(-46.8018034833198,42.1046079742813,
2.599307295175));
#212709=CARTESIAN_POINT('Ctrl Pts',(-46.8160830868207,42.0879261203874,
2.60017281085942));
#212710=CARTESIAN_POINT('Ctrl Pts',(-46.8289319921028,42.0705099543521,
2.60350651800053));
#212711=CARTESIAN_POINT('Ctrl Pts',(-46.8402566831455,42.0527856759081,
2.60896880596404));
#212712=CARTESIAN_POINT('Ctrl Pts',(-46.8448241915563,42.0456370666824,
2.61117187235418));
#212713=CARTESIAN_POINT('Ctrl Pts',(-46.849144212697,42.0384382358171,2.61372076577189));
#212714=CARTESIAN_POINT('Ctrl Pts',(-46.8532123574521,42.0312165334051,
2.6165917989701));
#212715=CARTESIAN_POINT('Ctrl Pts',(-46.8547132558791,42.0285521636634,
2.61765103591236));
#212716=CARTESIAN_POINT('Ctrl Pts',(-46.8561797434811,42.0258847247796,
2.61875422455176));
#212717=CARTESIAN_POINT('Ctrl Pts',(-46.8576115380195,42.0232156132262,
2.61990022440423));
#212718=CARTESIAN_POINT('Ctrl Pts',(-46.860296152779,42.0182110290635,2.6220489741276));
#212719=CARTESIAN_POINT('Ctrl Pts',(-46.8628587997326,42.0132005644176,
2.62434823201797));
#212720=CARTESIAN_POINT('Ctrl Pts',(-46.8652976184989,42.0081934246215,
2.62679048030332));
#212721=CARTESIAN_POINT('Ctrl Pts',(-46.873833484181,41.9906684353355,2.63533834930206));
#212722=CARTESIAN_POINT('Ctrl Pts',(-46.8808524512365,41.9731841724648,
2.64563784783589));
#212723=CARTESIAN_POINT('Ctrl Pts',(-46.8862747746135,41.9561353316317,
2.65736666737991));
#212724=CARTESIAN_POINT('Ctrl Pts',(-46.888985936302,41.9476109112151,2.66323107715191));
#212725=CARTESIAN_POINT('Ctrl Pts',(-46.8912979378216,41.9391953469841,
2.669452817808));
#212726=CARTESIAN_POINT('Ctrl Pts',(-46.8932008176775,41.930937981802,2.67599160631227));
#212727=CARTESIAN_POINT('Ctrl Pts',(-46.8941522576055,41.926809299211,2.6792610005644));
#212728=CARTESIAN_POINT('Ctrl Pts',(-46.8950014172056,41.92272016646,2.68260965685149));
#212729=CARTESIAN_POINT('Ctrl Pts',(-46.8957470516901,41.9186767517591,
2.68603254012509));
#212730=CARTESIAN_POINT('Ctrl Pts',(-46.8964926861745,41.9146333370581,
2.68945542339868));
#212731=CARTESIAN_POINT('Ctrl Pts',(-46.8971346781638,41.9106356952805,
2.69295261525412));
#212732=CARTESIAN_POINT('Ctrl Pts',(-46.8976720238189,41.9066898836034,
2.69651891172126));
#212733=CARTESIAN_POINT('Ctrl Pts',(-46.897676606252,41.9066562340936,2.69654932476114));
#212734=CARTESIAN_POINT('Ctrl Pts',(-46.8976811811498,41.9066225884706,
2.69657974261172));
#212735=CARTESIAN_POINT('Ctrl Pts',(-46.8976857485122,41.9065889467375,
2.69661016527));
#212736=CARTESIAN_POINT('Ctrl Pts',(-46.9000183671518,41.8894076224752,
2.71214746101269));
#212737=CARTESIAN_POINT('Ctrl Pts',(-46.9005163877045,41.8732226654013,
2.72880565567839));
#212738=CARTESIAN_POINT('Ctrl Pts',(-46.8993610201073,41.858119701628,2.74628040012732));
#212739=CARTESIAN_POINT('Ctrl Pts',(-46.8981665787452,41.8425059656485,
2.76434612882993));
#212740=CARTESIAN_POINT('Ctrl Pts',(-46.8952045688308,41.8280478726805,
2.7832859265522));
#212741=CARTESIAN_POINT('Ctrl Pts',(-46.8906306633423,41.8148672739063,
2.80278753268811));
#212742=CARTESIAN_POINT('Ctrl Pts',(-46.8861437631607,41.8019373978555,
2.82191817723983));
#212743=CARTESIAN_POINT('Ctrl Pts',(-46.8801049472927,41.79023634303,2.84159092316567));
#212744=CARTESIAN_POINT('Ctrl Pts',(-46.8726287066487,41.7799143139087,
2.8615123381865));
#212745=CARTESIAN_POINT('Ctrl Pts',(-46.8676759593274,41.77307633149,2.87470957722421));
#212746=CARTESIAN_POINT('Ctrl Pts',(-46.8620917411125,41.7668442729548,
2.88801594388914));
#212747=CARTESIAN_POINT('Ctrl Pts',(-46.8559036426987,41.7612723673362,
2.90134173516052));
#212748=CARTESIAN_POINT('',(-46.5911245387432,41.5228599914562,3.471530721391));
#212749=CARTESIAN_POINT('',(-46.8559036426987,41.7612723673362,2.90134173516051));
#212750=CARTESIAN_POINT('',(-50.3023253561997,36.9399086546485,3.47153072139096));
#212751=CARTESIAN_POINT('Origin',(5.53234440788222E-15,1.85015204418142E-13,
3.47153072139072));
#212752=CARTESIAN_POINT('',(-50.5905785208486,37.149332979726,2.90134173516049));
#212753=CARTESIAN_POINT('',(-50.3023253561997,36.9399086546485,3.47153072139097));
#212754=CARTESIAN_POINT('',(-50.9219998155902,37.0158684358559,2.59908173516048));
#212755=CARTESIAN_POINT('Ctrl Pts',(-50.5905785208486,37.149332979726,2.90134173516048));
#212756=CARTESIAN_POINT('Ctrl Pts',(-50.600534308882,37.1565661199777,2.88164837656735));
#212757=CARTESIAN_POINT('Ctrl Pts',(-50.611603765939,37.1621977431861,2.86203734439141));
#212758=CARTESIAN_POINT('Ctrl Pts',(-50.6236016024787,37.1661909570579,
2.84277945978138));
#212759=CARTESIAN_POINT('Ctrl Pts',(-50.6358405223235,37.1702644101623,
2.82313460919987));
#212760=CARTESIAN_POINT('Ctrl Pts',(-50.6490462309923,37.1726335298282,
2.80385576863291));
#212761=CARTESIAN_POINT('Ctrl Pts',(-50.6630602183674,37.173221724529,2.78521678518325));
#212762=CARTESIAN_POINT('Ctrl Pts',(-50.6765297750374,37.1737870683989,
2.76730190934354));
#212763=CARTESIAN_POINT('Ctrl Pts',(-50.6907468939695,37.172707346597,2.74997687279617));
#212764=CARTESIAN_POINT('Ctrl Pts',(-50.7055935641188,37.1698754144265,
2.73349253345519));
#212765=CARTESIAN_POINT('Ctrl Pts',(-50.7169982609376,37.1677000224031,
2.72082983599163));
#212766=CARTESIAN_POINT('Ctrl Pts',(-50.7287749695268,37.1644899772796,
2.70866321039233));
#212767=CARTESIAN_POINT('Ctrl Pts',(-50.7408753824654,37.1601789145087,
2.69711645335869));
#212768=CARTESIAN_POINT('Ctrl Pts',(-50.7409070954898,37.160167615982,2.69708619136775));
#212769=CARTESIAN_POINT('Ctrl Pts',(-50.7409388110965,37.160156309136,2.69705593387243));
#212770=CARTESIAN_POINT('Ctrl Pts',(-50.7409705292823,37.1601449939716,
2.69702568087595));
#212771=CARTESIAN_POINT('Ctrl Pts',(-50.7443713638247,37.1589317782469,
2.6937819444329));
#212772=CARTESIAN_POINT('Ctrl Pts',(-50.7477999807009,37.1576225876056,
2.69059266624724));
#212773=CARTESIAN_POINT('Ctrl Pts',(-50.7512517425808,37.1562191103355,
2.68746219342701));
#212774=CARTESIAN_POINT('Ctrl Pts',(-50.7704600126106,37.1484090784377,
2.6700418239623));
#212775=CARTESIAN_POINT('Ctrl Pts',(-50.7903868440206,37.1376839208992,
2.65443567878123));
#212776=CARTESIAN_POINT('Ctrl Pts',(-50.8102141228026,37.1243864882687,
2.64136852353366));
#212777=CARTESIAN_POINT('Ctrl Pts',(-50.8191128800971,37.1184184163553,
2.63550380329865));
#212778=CARTESIAN_POINT('Ctrl Pts',(-50.827991924717,37.1119323236341,2.63014997451179));
#212779=CARTESIAN_POINT('Ctrl Pts',(-50.8367795369356,37.1049590818167,
2.6253698111928));
#212780=CARTESIAN_POINT('Ctrl Pts',(-50.8405985143443,37.1019286052431,
2.62329241687099));
#212781=CARTESIAN_POINT('Ctrl Pts',(-50.8444000194069,37.0988061338479,
2.62132362131454));
#212782=CARTESIAN_POINT('Ctrl Pts',(-50.8481780352574,37.0955942139022,
2.61946873372374));
#212783=CARTESIAN_POINT('Ctrl Pts',(-50.8614010907342,37.084352494092,2.61297662715593));
#212784=CARTESIAN_POINT('Ctrl Pts',(-50.8743364007569,37.0720150276372,
2.60787989113995));
#212785=CARTESIAN_POINT('Ctrl Pts',(-50.8867260065479,37.058690996362,2.60440616886204));
#212786=CARTESIAN_POINT('Ctrl Pts',(-50.8929208094434,37.0520289807244,
2.60266930772309));
#212787=CARTESIAN_POINT('Ctrl Pts',(-50.8989791867714,37.045120324241,2.6013382004021));
#212788=CARTESIAN_POINT('Ctrl Pts',(-50.9048689000889,37.0379786793009,
2.6004413072361));
#212789=CARTESIAN_POINT('Ctrl Pts',(-50.9078137567477,37.0344078568308,
2.59999286065309));
#212790=CARTESIAN_POINT('Ctrl Pts',(-50.9107164475036,37.030778787319,2.59965296768537));
#212791=CARTESIAN_POINT('Ctrl Pts',(-50.913572943118,37.0270931777238,2.59942518630979));
#212792=CARTESIAN_POINT('Ctrl Pts',(-50.9164294387324,37.0234075681287,
2.59919740493421));
#212793=CARTESIAN_POINT('Ctrl Pts',(-50.9192397378252,37.0196654174469,
2.59908173791642));
#212794=CARTESIAN_POINT('Ctrl Pts',(-50.9219998155902,37.0158684358559,
2.59908173516049));
#212795=CARTESIAN_POINT('',(-50.9399462128204,36.9911673391707,2.59908173516048));
#212796=CARTESIAN_POINT('Origin',(8.60468667414046E-17,1.91016133863093E-13,
2.59908173516023));
#212797=CARTESIAN_POINT('',(-50.9644637245895,36.6347241449654,2.90134173516048));
#212798=CARTESIAN_POINT('Ctrl Pts',(-50.9399462128204,36.9911673391707,
2.59908173516049));
#212799=CARTESIAN_POINT('Ctrl Pts',(-50.9421917493682,36.9880750374207,
2.59908174381708));
#212800=CARTESIAN_POINT('Ctrl Pts',(-50.9443925120841,36.9849631609003,
2.5991575200102));
#212801=CARTESIAN_POINT('Ctrl Pts',(-50.9465482749233,36.9818339300543,
2.59930729517495));
#212802=CARTESIAN_POINT('Ctrl Pts',(-50.9590059247116,36.9637508360892,
2.60017281085948));
#212803=CARTESIAN_POINT('Ctrl Pts',(-50.9699639572756,36.9450870013076,
2.60350651800129));
#212804=CARTESIAN_POINT('Ctrl Pts',(-50.9793739188884,36.9262760657615,
2.60896880596596));
#212805=CARTESIAN_POINT('Ctrl Pts',(-50.983169172872,36.9186891827322,2.61117187235565));
#212806=CARTESIAN_POINT('Ctrl Pts',(-50.9867130457561,36.9110782226467,
2.61372076577271));
#212807=CARTESIAN_POINT('Ctrl Pts',(-50.9900040313323,36.9034708445588,
2.61659179897008));
#212808=CARTESIAN_POINT('Ctrl Pts',(-50.991218205206,36.9006641839072,2.61765103591233));
#212809=CARTESIAN_POINT('Ctrl Pts',(-50.9923978359481,36.8978580678373,
2.61875422455174));
#212810=CARTESIAN_POINT('Ctrl Pts',(-50.9935427888372,36.8950539146734,
2.61990022440421));
#212811=CARTESIAN_POINT('Ctrl Pts',(-50.9956895755044,36.8897961274911,
2.62204897412758));
#212812=CARTESIAN_POINT('Ctrl Pts',(-50.9977144478401,36.8845452411468,
2.62434823201794));
#212813=CARTESIAN_POINT('Ctrl Pts',(-50.9996165178738,36.8793106050087,
2.62679048030329));
#212814=CARTESIAN_POINT('Ctrl Pts',(-51.0062737629918,36.8609893785252,
2.63533834930203));
#212815=CARTESIAN_POINT('Ctrl Pts',(-51.011426676282,36.8428672144359,2.64563784783588));
#212816=CARTESIAN_POINT('Ctrl Pts',(-51.0150372064714,36.8253449818068,
2.65736666737989));
#212817=CARTESIAN_POINT('Ctrl Pts',(-51.0168424715662,36.8165838654922,
2.66323107715189));
#212818=CARTESIAN_POINT('Ctrl Pts',(-51.0182621417029,36.8079727326367,
2.66945281780798));
#212819=CARTESIAN_POINT('Ctrl Pts',(-51.0192914676908,36.799561697058,2.67599160631225));
#212820=CARTESIAN_POINT('Ctrl Pts',(-51.0198061306847,36.7953561792686,
2.67926100056438));
#212821=CARTESIAN_POINT('Ctrl Pts',(-51.0202232077371,36.7912006858666,
2.68260965685147));
#212822=CARTESIAN_POINT('Ctrl Pts',(-51.0205421056328,36.7871014813876,
2.68603254012506));
#212823=CARTESIAN_POINT('Ctrl Pts',(-51.0208610035285,36.7830022769086,
2.68945542339865));
#212824=CARTESIAN_POINT('Ctrl Pts',(-51.0210816112668,36.778959428195,2.69295261525409));
#212825=CARTESIAN_POINT('Ctrl Pts',(-51.0212035636552,36.7749790641715,
2.69651891172123));
#212826=CARTESIAN_POINT('Ctrl Pts',(-51.0212046036537,36.7749451200025,
2.69654932476111));
#212827=CARTESIAN_POINT('Ctrl Pts',(-51.0212056365645,36.7749111804867,
2.69657974261169));
#212828=CARTESIAN_POINT('Ctrl Pts',(-51.0212066623877,36.7748772456272,
2.69661016526997));
#212829=CARTESIAN_POINT('Ctrl Pts',(-51.0217305652763,36.7575462174155,
2.71214746101237));
#212830=CARTESIAN_POINT('Ctrl Pts',(-51.0205340689294,36.7413978659071,
2.72880565567775));
#212831=CARTESIAN_POINT('Ctrl Pts',(-51.0178063409629,36.7264984065491,
2.74628040012634));
#212832=CARTESIAN_POINT('Ctrl Pts',(-51.0149863630479,36.7110950573693,
2.7643461288285));
#212833=CARTESIAN_POINT('Ctrl Pts',(-51.0105292970942,36.6970257816921,
2.7832859265503));
#212834=CARTESIAN_POINT('Ctrl Pts',(-51.0046027002041,36.6843954909291,
2.80278753268571));
#212835=CARTESIAN_POINT('Ctrl Pts',(-50.9987888396576,36.6720054548733,
2.82191817723679));
#212836=CARTESIAN_POINT('Ctrl Pts',(-50.9915600117756,36.6609997277932,
2.84159092316196));
#212837=CARTESIAN_POINT('Ctrl Pts',(-50.9830457809187,36.6515157237731,
2.86151233818214));
#212838=CARTESIAN_POINT('Ctrl Pts',(-50.9774054014708,36.6452329036033,
2.87470957722126));
#212839=CARTESIAN_POINT('Ctrl Pts',(-50.9712003466853,36.6396186946847,
2.88801594388765));
#212840=CARTESIAN_POINT('Ctrl Pts',(-50.9644637245895,36.6347241449654,
2.90134173516048));
#212841=CARTESIAN_POINT('',(-50.676214228995,36.4252947698678,3.47153072139096));
#212842=CARTESIAN_POINT('',(-50.9644637245895,36.6347241449654,2.90134173516049));
#212843=CARTESIAN_POINT('',(-53.8880358395972,31.4795232016788,3.47153072139093));
#212844=CARTESIAN_POINT('Origin',(5.53234440788222E-15,1.85015204418142E-13,
3.47153072139072));
#212845=CARTESIAN_POINT('',(-54.1966007261209,31.6576696180583,2.90134173516045));
#212846=CARTESIAN_POINT('',(-53.8880358395972,31.4795232016789,3.47153072139093));
#212847=CARTESIAN_POINT('',(-54.5122556166612,31.4902932482906,2.59908173516044));
#212848=CARTESIAN_POINT('Ctrl Pts',(-54.1966007261209,31.6576696180583,
2.90134173516045));
#212849=CARTESIAN_POINT('Ctrl Pts',(-54.2072580443415,31.6638224711873,
2.8816483765665));
#212850=CARTESIAN_POINT('Ctrl Pts',(-54.2188555266747,31.6682661704392,
2.86203734438975));
#212851=CARTESIAN_POINT('Ctrl Pts',(-54.2312050423205,31.6709833936514,
2.84277945977895));
#212852=CARTESIAN_POINT('Ctrl Pts',(-54.2438027078756,31.6737552164701,
2.82313460919676));
#212853=CARTESIAN_POINT('Ctrl Pts',(-54.2571837147291,31.6747309854169,
2.80385576862914));
#212854=CARTESIAN_POINT('Ctrl Pts',(-54.2711824151039,31.6738510973608,
2.7852167851789));
#212855=CARTESIAN_POINT('Ctrl Pts',(-54.2846372786593,31.6730053921579,
2.76730190933893));
#212856=CARTESIAN_POINT('Ctrl Pts',(-54.298663653066,31.6704454915906,2.74997687279134));
#212857=CARTESIAN_POINT('Ctrl Pts',(-54.3131329740852,31.6660771734251,
2.7334925334502));
#212858=CARTESIAN_POINT('Ctrl Pts',(-54.3242478043949,31.6627215829945,
2.72082983598842));
#212859=CARTESIAN_POINT('Ctrl Pts',(-54.3356244578571,31.6582981215833,
2.70866321039078));
#212860=CARTESIAN_POINT('Ctrl Pts',(-54.3472079546995,31.6527458376967,
2.69711645335865));
#212861=CARTESIAN_POINT('Ctrl Pts',(-54.347238312979,31.6527312861508,2.69708619136771));
#212862=CARTESIAN_POINT('Ctrl Pts',(-54.347268672957,31.6527167260613,2.69705593387238));
#212863=CARTESIAN_POINT('Ctrl Pts',(-54.3472990346306,31.6527021574293,
2.6970256808759));
#212864=CARTESIAN_POINT('Ctrl Pts',(-54.3505544234702,31.6511401038187,
2.69378194443285));
#212865=CARTESIAN_POINT('Ctrl Pts',(-54.3538274103385,31.6494796970076,
2.6905926662472));
#212866=CARTESIAN_POINT('Ctrl Pts',(-54.3571135597834,31.6477231007679,
2.68746219342697));
#212867=CARTESIAN_POINT('Ctrl Pts',(-54.3754002342689,31.6379480420932,
2.67004182396126));
#212868=CARTESIAN_POINT('Ctrl Pts',(-54.3940968201768,31.6251987170239,
2.65443567877941));
#212869=CARTESIAN_POINT('Ctrl Pts',(-54.4124255228538,31.6099016141377,
2.64136852353138));
#212870=CARTESIAN_POINT('Ctrl Pts',(-54.4206516984379,31.6030360625224,
2.63550380329723));
#212871=CARTESIAN_POINT('Ctrl Pts',(-54.4288041214165,31.5956573884073,
2.63014997451111));
#212872=CARTESIAN_POINT('Ctrl Pts',(-54.4368146919238,31.5878037911381,
2.62536981119271));
#212873=CARTESIAN_POINT('Ctrl Pts',(-54.4402959775154,31.5843907239925,
2.62329241687091));
#212874=CARTESIAN_POINT('Ctrl Pts',(-54.443750270399,31.58088799234,2.62132362131446));
#212875=CARTESIAN_POINT('Ctrl Pts',(-54.4471718528273,31.5772987574367,
2.61946873372366));
#212876=CARTESIAN_POINT('Ctrl Pts',(-54.4591473913264,31.5647364352753,
2.61297662715587));
#212877=CARTESIAN_POINT('Ctrl Pts',(-54.4707222239582,31.5511144466741,
2.60787989113988));
#212878=CARTESIAN_POINT('Ctrl Pts',(-54.4816512176786,31.5365683393824,
2.60440616886199));
#212879=CARTESIAN_POINT('Ctrl Pts',(-54.4871157145388,31.5292952857366,
2.60266930772304));
#212880=CARTESIAN_POINT('Ctrl Pts',(-54.4924187521964,31.5217912027244,
2.60133820040204));
#212881=CARTESIAN_POINT('Ctrl Pts',(-54.4975296958774,31.5140730377803,
2.60044130723604));
#212882=CARTESIAN_POINT('Ctrl Pts',(-54.5000851677178,31.5102139553083,
2.59999286065304));
#212883=CARTESIAN_POINT('Ctrl Pts',(-54.5025926161709,31.5063013524149,
2.59965296768532));
#212884=CARTESIAN_POINT('Ctrl Pts',(-54.5050482124962,31.5023373478778,
2.59942518630974));
#212885=CARTESIAN_POINT('Ctrl Pts',(-54.5075038088216,31.4983733433407,
2.59919740493416));
#212886=CARTESIAN_POINT('Ctrl Pts',(-54.5099075515418,31.4943579363065,
2.59908173791634));
#212887=CARTESIAN_POINT('Ctrl Pts',(-54.5122556166612,31.4902932482907,
2.59908173516044));
#212888=CARTESIAN_POINT('',(-54.5275217339721,31.4638515574739,2.59908173516044));
#212889=CARTESIAN_POINT('Origin',(9.49066947580433E-17,1.91029776801841E-13,
2.59908173516024));
#212890=CARTESIAN_POINT('',(-54.514646476914,31.1067982185534,2.90134173516043));
#212891=CARTESIAN_POINT('Ctrl Pts',(-54.5275217339721,31.4638515574739,
2.59908173516045));
#212892=CARTESIAN_POINT('Ctrl Pts',(-54.5294317356859,31.4605414731919,
2.59908174381707));
#212893=CARTESIAN_POINT('Ctrl Pts',(-54.5312951627229,31.457216601512,2.59915752001016));
#212894=CARTESIAN_POINT('Ctrl Pts',(-54.5331120223761,31.4538791743432,
2.59930729517491));
#212895=CARTESIAN_POINT('Ctrl Pts',(-54.5436112298317,31.4345929624713,
2.60017281085941));
#212896=CARTESIAN_POINT('Ctrl Pts',(-54.5525583311781,31.4148859438258,
2.60350651800102));
#212897=CARTESIAN_POINT('Ctrl Pts',(-54.5599504658512,31.3951944477268,
2.60896880596534));
#212898=CARTESIAN_POINT('Ctrl Pts',(-54.5629318838126,31.3872524143692,
2.61117187235517));
#212899=CARTESIAN_POINT('Ctrl Pts',(-54.5656607810288,31.3793127123322,
2.61372076577242));
#212900=CARTESIAN_POINT('Ctrl Pts',(-54.5681385507009,31.3714030065918,
2.61659179897004));
#212901=CARTESIAN_POINT('Ctrl Pts',(-54.5690526972783,31.3684848053918,
2.61765103591229));
#212902=CARTESIAN_POINT('Ctrl Pts',(-54.5699325468791,31.3655707565306,
2.6187542245517));
#212903=CARTESIAN_POINT('Ctrl Pts',(-54.5707781137756,31.3626622846451,
2.61990022440417));
#212904=CARTESIAN_POINT('Ctrl Pts',(-54.5723635517064,31.3572088998599,
2.62204897412754));
#212905=CARTESIAN_POINT('Ctrl Pts',(-54.5738284644992,31.3517751216268,
2.62434823201791));
#212906=CARTESIAN_POINT('Ctrl Pts',(-54.575172946323,31.3463703409155,2.62679048030326));
#212907=CARTESIAN_POINT('Ctrl Pts',(-54.5798786327061,31.3274536084259,
2.635338349302));
#212908=CARTESIAN_POINT('Ctrl Pts',(-54.5831090358349,31.3088920933401,
2.64563784783583));
#212909=CARTESIAN_POINT('Ctrl Pts',(-54.5848682151124,31.2910884461624,
2.65736666737985));
#212910=CARTESIAN_POINT('Ctrl Pts',(-54.5857478047512,31.2821866225735,
2.66323107715185));
#212911=CARTESIAN_POINT('Ctrl Pts',(-54.5862595893019,31.273474266467,2.66945281780794));
#212912=CARTESIAN_POINT('Ctrl Pts',(-54.5864040839109,31.2650017135575,
2.67599160631221));
#212913=CARTESIAN_POINT('Ctrl Pts',(-54.5864763312153,31.2607654371028,
2.67926100056434));
#212914=CARTESIAN_POINT('Ctrl Pts',(-54.5864567561366,31.2565891115051,
2.68260965685142));
#212915=CARTESIAN_POINT('Ctrl Pts',(-54.5863454235314,31.2524790289902,
2.68603254012502));
#212916=CARTESIAN_POINT('Ctrl Pts',(-54.5862340909262,31.2483689464753,
2.68945542339861));
#212917=CARTESIAN_POINT('Ctrl Pts',(-54.586030897389,31.244325185122,2.69295261525404));
#212918=CARTESIAN_POINT('Ctrl Pts',(-54.5857361203749,31.2403538784534,
2.69651891172118));
#212919=CARTESIAN_POINT('Ctrl Pts',(-54.5857336065443,31.2403200115247,
2.69654932476107));
#212920=CARTESIAN_POINT('Ctrl Pts',(-54.5857310861513,31.2402861499645,
2.69657974261165));
#212921=CARTESIAN_POINT('Ctrl Pts',(-54.5857285591962,31.2402522937759,
2.69661016526993));
#212922=CARTESIAN_POINT('Ctrl Pts',(-54.5844380063442,31.2229614439869,
2.71214746101179));
#212923=CARTESIAN_POINT('Ctrl Pts',(-54.5815601021621,31.2070266227627,
2.72880565567653));
#212924=CARTESIAN_POINT('Ctrl Pts',(-54.5772898993849,31.1924939094151,
2.74628040012444));
#212925=CARTESIAN_POINT('Ctrl Pts',(-54.5728752811852,31.1774697093521,
2.76434612882594));
#212926=CARTESIAN_POINT('Ctrl Pts',(-54.5669719917397,31.1639433968943,
2.78328592654701));
#212927=CARTESIAN_POINT('Ctrl Pts',(-54.5597576364838,31.1520017942511,
2.80278753268169));
#212928=CARTESIAN_POINT('Ctrl Pts',(-54.5526805134453,31.1402873460179,
2.82191817723222));
#212929=CARTESIAN_POINT('Ctrl Pts',(-54.5443408741004,31.130097527732,2.84159092315684));
#212930=CARTESIAN_POINT('Ctrl Pts',(-54.5348819367256,31.1215554575456,
2.86151233817648));
#212931=CARTESIAN_POINT('Ctrl Pts',(-54.5286157223284,31.1158966355169,
2.87470957721744));
#212932=CARTESIAN_POINT('Ctrl Pts',(-54.5218578148506,31.1109617866625,
2.88801594388571));
#212933=CARTESIAN_POINT('Ctrl Pts',(-54.514646476914,31.1067982185534,2.90134173516043));
#212934=CARTESIAN_POINT('',(-54.2060847114743,30.9286463962977,3.47153072139093));
#212935=CARTESIAN_POINT('',(-54.514646476914,31.1067982185534,2.90134173516043));
#212936=CARTESIAN_POINT('',(-56.8833377255396,25.6742415049979,3.47153072139089));
#212937=CARTESIAN_POINT('Origin',(5.53234440788222E-15,1.85015204418142E-13,
3.47153072139072));
#212938=CARTESIAN_POINT('',(-57.20883363247,25.8191582032619,2.90134173516041));
#212939=CARTESIAN_POINT('',(-56.8833377255396,25.6742415049979,3.47153072139089));
#212940=CARTESIAN_POINT('',(-57.5052637377733,25.6197038181296,2.5990817351604));
#212941=CARTESIAN_POINT('Ctrl Pts',(-57.20883363247,25.8191582032619,2.90134173516041));
#212942=CARTESIAN_POINT('Ctrl Pts',(-57.2200757170682,25.8241633573212,
2.88164837656715));
#212943=CARTESIAN_POINT('Ctrl Pts',(-57.2320741602334,25.8273704465174,
2.86203734439109));
#212944=CARTESIAN_POINT('Ctrl Pts',(-57.2446400511066,25.8287819086041,
2.84277945978095));
#212945=CARTESIAN_POINT('Ctrl Pts',(-57.2574584397107,25.8302217324662,
2.82313460919956));
#212946=CARTESIAN_POINT('Ctrl Pts',(-57.2708681396365,25.8297934599655,
2.80385576863272));
#212947=CARTESIAN_POINT('Ctrl Pts',(-57.2846981803189,25.8274551293907,
2.78521678518317));
#212948=CARTESIAN_POINT('Ctrl Pts',(-57.2979909364578,25.825207640839,2.7673019093442));
#212949=CARTESIAN_POINT('Ctrl Pts',(-57.3116728904446,25.8211956083136,
2.74997687279751));
#212950=CARTESIAN_POINT('Ctrl Pts',(-57.3256063334235,25.8153387643623,
2.73349253345713));
#212951=CARTESIAN_POINT('Ctrl Pts',(-57.3363095208206,25.810839740075,2.72082983599284));
#212952=CARTESIAN_POINT('Ctrl Pts',(-57.3471614741631,25.805251326744,2.70866321039285));
#212953=CARTESIAN_POINT('Ctrl Pts',(-57.3581011436975,25.798518653724,2.69711645335861));
#212954=CARTESIAN_POINT('Ctrl Pts',(-57.3581298146204,25.7985010085887,
2.69708619136767));
#212955=CARTESIAN_POINT('Ctrl Pts',(-57.3581584863395,25.798483354779,2.69705593387234));
#212956=CARTESIAN_POINT('Ctrl Pts',(-57.358187158852,25.7984656922965,2.69702568087586));
#212957=CARTESIAN_POINT('Ctrl Pts',(-57.3612614352675,25.7965719149862,
2.69378194443282));
#212958=CARTESIAN_POINT('Ctrl Pts',(-57.3643429325989,25.7945784837697,
2.69059266624716));
#212959=CARTESIAN_POINT('Ctrl Pts',(-57.3674274658677,25.7924880141965,
2.68746219342693));
#212960=CARTESIAN_POINT('Ctrl Pts',(-57.3845921921772,25.7808550263326,
2.67004182395949));
#212961=CARTESIAN_POINT('Ctrl Pts',(-57.4018536888757,25.766221218005,2.65443567877626));
#212962=CARTESIAN_POINT('Ctrl Pts',(-57.418483002346,25.7490920431222,2.64136852352743));
#212963=CARTESIAN_POINT('Ctrl Pts',(-57.425946468518,25.7414042322261,2.63550380329482));
#212964=CARTESIAN_POINT('Ctrl Pts',(-57.4332829502027,25.7332138190157,
2.63014997451002));
#212965=CARTESIAN_POINT('Ctrl Pts',(-57.4404287135112,25.724565911951,2.6253698111927));
#212966=CARTESIAN_POINT('Ctrl Pts',(-57.4435341655924,25.7208076485113,
2.6232924168709));
#212967=CARTESIAN_POINT('Ctrl Pts',(-57.4466034003413,25.7169630332624,
2.62132362131444));
#212968=CARTESIAN_POINT('Ctrl Pts',(-57.4496310617743,25.7130358078103,
2.61946873372364));
#212969=CARTESIAN_POINT('Ctrl Pts',(-57.4602278767899,25.699290518728,2.61297662715584));
#212970=CARTESIAN_POINT('Ctrl Pts',(-57.4703154157423,25.6845332533381,
2.60787989113985));
#212971=CARTESIAN_POINT('Ctrl Pts',(-57.4796640570499,25.6689244402255,
2.60440616886196));
#212972=CARTESIAN_POINT('Ctrl Pts',(-57.4843383777036,25.6611200336692,
2.60266930772301));
#212973=CARTESIAN_POINT('Ctrl Pts',(-57.4888279745007,25.6531027404319,
2.601338200402));
#212974=CARTESIAN_POINT('Ctrl Pts',(-57.4931041519765,25.6448926173141,
2.600441307236));
#212975=CARTESIAN_POINT('Ctrl Pts',(-57.4952422407144,25.6407875557552,
2.599992860653));
#212976=CARTESIAN_POINT('Ctrl Pts',(-57.4973269747346,25.6366342867764,
2.59965296768529));
#212977=CARTESIAN_POINT('Ctrl Pts',(-57.4993547677437,25.6324353177606,
2.59942518630971));
#212978=CARTESIAN_POINT('Ctrl Pts',(-57.5013825607528,25.6282363487448,
2.59919740493413));
#212979=CARTESIAN_POINT('Ctrl Pts',(-57.5033534111923,25.6239916789979,
2.59908173791629));
#212980=CARTESIAN_POINT('Ctrl Pts',(-57.5052637377733,25.6197038181296,
2.5990817351604));
#212981=CARTESIAN_POINT('',(-57.517682316389,25.5918112338793,2.5990817351604));
#212982=CARTESIAN_POINT('Origin',(1.02291912287982E-16,1.91044271107351E-13,
2.59908173516023));
#212983=CARTESIAN_POINT('',(-57.4675553545142,25.2380597013429,2.90134173516039));
#212984=CARTESIAN_POINT('Ctrl Pts',(-57.517682316389,25.5918112338793,2.59908173516041));
#212985=CARTESIAN_POINT('Ctrl Pts',(-57.5192358568902,25.5883196330413,
2.59908174381697));
#212986=CARTESIAN_POINT('Ctrl Pts',(-57.5207415321516,25.5848181941918,
2.59915752001012));
#212987=CARTESIAN_POINT('Ctrl Pts',(-57.5221995827244,25.5813091362507,
2.59930729517487));
#212988=CARTESIAN_POINT('Ctrl Pts',(-57.5306253163332,25.5610311102459,
2.60017281085931));
#212989=CARTESIAN_POINT('Ctrl Pts',(-57.5374634601473,25.5404968219576,
2.60350651800052));
#212990=CARTESIAN_POINT('Ctrl Pts',(-57.5427567781063,25.5201405094583,
2.60896880596417));
#212991=CARTESIAN_POINT('Ctrl Pts',(-57.5448916950066,25.5119303403511,
2.61117187235426));
#212992=CARTESIAN_POINT('Ctrl Pts',(-57.5467757181859,25.5037488853987,
2.6137207657719));
#212993=CARTESIAN_POINT('Ctrl Pts',(-57.5484131249909,25.4956235123964,
2.61659179897001));
#212994=CARTESIAN_POINT('Ctrl Pts',(-57.5490172286907,25.492625743071,2.61765103591227));
#212995=CARTESIAN_POINT('Ctrl Pts',(-57.549587657334,25.4896356883477,2.61875422455167));
#212996=CARTESIAN_POINT('Ctrl Pts',(-57.5501245740299,25.4866547635672,
2.61990022440413));
#212997=CARTESIAN_POINT('Ctrl Pts',(-57.5511312928346,25.4810655296039,
2.6220489741275));
#212998=CARTESIAN_POINT('Ctrl Pts',(-57.5520201961935,25.4755083930936,
2.62434823201787));
#212999=CARTESIAN_POINT('Ctrl Pts',(-57.5527923593831,25.4699926837176,
2.62679048030322));
#213000=CARTESIAN_POINT('Ctrl Pts',(-57.5554949305467,25.4506877009016,
2.63533834930196));
#213001=CARTESIAN_POINT('Ctrl Pts',(-57.5567674305412,25.4318901986627,
2.64563784783579));
#213002=CARTESIAN_POINT('Ctrl Pts',(-57.5566559849706,25.4140001974206,
2.6573666673798));
#213003=CARTESIAN_POINT('Ctrl Pts',(-57.5566002621853,25.4050551967995,
2.66323107715181));
#213004=CARTESIAN_POINT('Ctrl Pts',(-57.5561985539314,25.3963370718388,
2.66945281780789));
#213005=CARTESIAN_POINT('Ctrl Pts',(-57.5554566340482,25.3878958286612,
2.67599160631216));
#213006=CARTESIAN_POINT('Ctrl Pts',(-57.5550856741066,25.3836752070724,
2.67926100056429));
#213007=CARTESIAN_POINT('Ctrl Pts',(-57.5546296613653,25.3795238059763,
2.68260965685139));
#213008=CARTESIAN_POINT('Ctrl Pts',(-57.5540893180426,25.3754478763495,
2.68603254012499));
#213009=CARTESIAN_POINT('Ctrl Pts',(-57.5535489747199,25.3713719467228,
2.68945542339858));
#213010=CARTESIAN_POINT('Ctrl Pts',(-57.5529242061381,25.3673715770255,
2.69295261525401));
#213011=CARTESIAN_POINT('Ctrl Pts',(-57.55221592936,25.3634528381786,2.69651891172115));
#213012=CARTESIAN_POINT('Ctrl Pts',(-57.5522098892425,25.3634194195433,
2.69654932476103));
#213013=CARTESIAN_POINT('Ctrl Pts',(-57.5522038431596,25.3633860069332,
2.69657974261161));
#213014=CARTESIAN_POINT('Ctrl Pts',(-57.552197791112,25.3633526003511,2.69661016526989));
#213015=CARTESIAN_POINT('Ctrl Pts',(-57.5491069220866,25.3462913711527,
2.71214746101178));
#213016=CARTESIAN_POINT('Ctrl Pts',(-57.5445791409896,25.330744665448,2.72880565567655));
#213017=CARTESIAN_POINT('Ctrl Pts',(-57.5388132486367,25.3167379215589,
2.74628040012449));
#213018=CARTESIAN_POINT('Ctrl Pts',(-57.532852357633,25.3022574788921,2.76434612882608));
#213019=CARTESIAN_POINT('Ctrl Pts',(-57.5255675223698,25.2894223267632,
2.78328592654724));
#213020=CARTESIAN_POINT('Ctrl Pts',(-57.5171444507335,25.2783002469371,
2.80278753268202));
#213021=CARTESIAN_POINT('Ctrl Pts',(-57.5088816036436,25.2673897324725,
2.82191817723273));
#213022=CARTESIAN_POINT('Ctrl Pts',(-57.4995225236691,25.2581274647623,
2.84159092315754));
#213023=CARTESIAN_POINT('Ctrl Pts',(-57.4892225138731,25.2506209171179,
2.86151233817736));
#213024=CARTESIAN_POINT('Ctrl Pts',(-57.4823991184836,25.24564809247,2.87470957721803));
#213025=CARTESIAN_POINT('Ctrl Pts',(-57.475162399363,25.2414466709177,2.88801594388598));
#213026=CARTESIAN_POINT('Ctrl Pts',(-57.4675553545142,25.2380597013429,
2.9013417351604));
#213027=CARTESIAN_POINT('',(-57.1420619865023,25.0931373005744,3.47153072139088));
#213028=CARTESIAN_POINT('',(-57.4675553545142,25.2380597013429,2.90134173516039));
#213029=CARTESIAN_POINT('',(-59.2554138597572,19.5876674457077,3.47153072139085));
#213030=CARTESIAN_POINT('Origin',(5.53234440788222E-15,1.85015204418142E-13,
3.47153072139072));
#213031=CARTESIAN_POINT('',(-59.5942745858237,19.6977666881844,2.90134173516036));
#213032=CARTESIAN_POINT('',(-59.2554138597572,19.5876674457077,3.47153072139084));
#213033=CARTESIAN_POINT('',(-59.8682321556243,19.4684195516695,2.59908173516036));
#213034=CARTESIAN_POINT('Ctrl Pts',(-59.5942745858237,19.6977666881844,
2.90134173516036));
#213035=CARTESIAN_POINT('Ctrl Pts',(-59.6059782661689,19.701569305659,2.8816483765663));
#213036=CARTESIAN_POINT('Ctrl Pts',(-59.6182462127128,19.7035046472594,
2.86203734438945));
#213037=CARTESIAN_POINT('Ctrl Pts',(-59.6308908042844,19.7035948839464,
2.84277945977856));
#213038=CARTESIAN_POINT('Ctrl Pts',(-59.6437894749908,19.7036869338401,
2.82313460919653));
#213039=CARTESIAN_POINT('Ctrl Pts',(-59.6570809485114,19.7018593121346,
2.80385576862909));
#213040=CARTESIAN_POINT('Ctrl Pts',(-59.6705908046827,19.6980881582796,
2.785216785179));
#213041=CARTESIAN_POINT('Ctrl Pts',(-59.6835758151885,19.6944635103332,
2.76730190933965));
#213042=CARTESIAN_POINT('Ctrl Pts',(-59.6967634464057,19.6890433025166,
2.74997687279263));
#213043=CARTESIAN_POINT('Ctrl Pts',(-59.7100083536286,19.6817621015861,
2.733492533452));
#213044=CARTESIAN_POINT('Ctrl Pts',(-59.7201826317489,19.6761689356945,
2.72082983598954));
#213045=CARTESIAN_POINT('Ctrl Pts',(-59.7303909886966,19.6694767982707,
2.70866321039127));
#213046=CARTESIAN_POINT('Ctrl Pts',(-59.7405669736108,19.661637500694,2.69711645335857));
#213047=CARTESIAN_POINT('Ctrl Pts',(-59.7405936430525,19.6616169552931,
2.69708619136763));
#213048=CARTESIAN_POINT('Ctrl Pts',(-59.7406203123794,19.6615964011821,
2.6970559338723));
#213049=CARTESIAN_POINT('Ctrl Pts',(-59.7406469815886,19.6615758383628,
2.69702568087582));
#213050=CARTESIAN_POINT('Ctrl Pts',(-59.7435064631642,19.6593710859734,
2.69378194443278));
#213051=CARTESIAN_POINT('Ctrl Pts',(-59.7463627094291,19.6570664708011,
2.69059266624713));
#213052=CARTESIAN_POINT('Ctrl Pts',(-59.74921183173,19.6546650315164,2.6874621934269));
#213053=CARTESIAN_POINT('Ctrl Pts',(-59.7650665495267,19.641301567915,2.67004182396107));
#213054=CARTESIAN_POINT('Ctrl Pts',(-59.7807038364425,19.6249436073987,
2.65443567877911));
#213055=CARTESIAN_POINT('Ctrl Pts',(-59.795451566465,19.6061700313481,2.64136852353103));
#213056=CARTESIAN_POINT('Ctrl Pts',(-59.8020705519309,19.5977441904333,
2.63550380329699));
#213057=CARTESIAN_POINT('Ctrl Pts',(-59.8085107122963,19.5888317740054,
2.63014997451096));
#213058=CARTESIAN_POINT('Ctrl Pts',(-59.8147133779311,19.579484305421,2.62536981119264));
#213059=CARTESIAN_POINT('Ctrl Pts',(-59.8174089725189,19.5754220220078,
2.62329241687084));
#213060=CARTESIAN_POINT('Ctrl Pts',(-59.8200595219549,19.5712776455719,
2.62132362131439));
#213061=CARTESIAN_POINT('Ctrl Pts',(-59.8226600907004,19.5670554570749,
2.61946873372359));
#213062=CARTESIAN_POINT('Ctrl Pts',(-59.8317620813096,19.5522777973352,
2.6129766271558));
#213063=CARTESIAN_POINT('Ctrl Pts',(-59.8402518053949,19.5365469388443,
2.60787989113981));
#213064=CARTESIAN_POINT('Ctrl Pts',(-59.8479176686191,19.5200464333337,
2.60440616886191));
#213065=CARTESIAN_POINT('Ctrl Pts',(-59.8517506002312,19.5117961805783,
2.60266930772296));
#213066=CARTESIAN_POINT('Ctrl Pts',(-59.8553775672056,19.5033535162583,
2.60133820040197));
#213067=CARTESIAN_POINT('Ctrl Pts',(-59.858772127781,19.4947413867938,2.60044130723597));
#213068=CARTESIAN_POINT('Ctrl Pts',(-59.8604694080688,19.4904353220616,
2.59999286065296));
#213069=CARTESIAN_POINT('Ctrl Pts',(-59.862108586874,19.4860868910813,2.59965296768524));
#213070=CARTESIAN_POINT('Ctrl Pts',(-59.8636863596423,19.4816989623701,
2.59942518630966));
#213071=CARTESIAN_POINT('Ctrl Pts',(-59.8652641324106,19.4773110336588,
2.59919740493408));
#213072=CARTESIAN_POINT('Ctrl Pts',(-59.8667804975194,19.4728836066891,
2.59908173791629));
#213073=CARTESIAN_POINT('Ctrl Pts',(-59.8682321556243,19.4684195516695,
2.59908173516036));
#213074=CARTESIAN_POINT('',(-59.8776671349986,19.4393816709755,2.59908173516036));
#213075=CARTESIAN_POINT('Origin',(1.08121605342496E-16,1.91059457976978E-13,
2.59908173516023));
#213076=CARTESIAN_POINT('',(-59.7908376697913,19.092807720641,2.90134173516036));
#213077=CARTESIAN_POINT('Ctrl Pts',(-59.8776671349986,19.4393816709755,
2.59908173516036));
#213078=CARTESIAN_POINT('Ctrl Pts',(-59.8788471933725,19.435746808291,2.59908174381695));
#213079=CARTESIAN_POINT('Ctrl Pts',(-59.8799786203652,19.4321071647686,
2.59915752001008));
#213080=CARTESIAN_POINT('Ctrl Pts',(-59.8810618871502,19.4284649220283,
2.59930729517482));
#213081=CARTESIAN_POINT('Ctrl Pts',(-59.8873218328134,19.4074172521822,
2.6001728108594));
#213082=CARTESIAN_POINT('Ctrl Pts',(-59.8919760989615,19.3862806722057,
2.60350651800157));
#213083=CARTESIAN_POINT('Ctrl Pts',(-59.8951126055077,19.3654825713211,
2.60896880596681));
#213084=CARTESIAN_POINT('Ctrl Pts',(-59.8963776307491,19.3570942188,2.61117187235629));
#213085=CARTESIAN_POINT('Ctrl Pts',(-59.8973961381383,19.3487606486696,
2.61372076577302));
#213086=CARTESIAN_POINT('Ctrl Pts',(-59.8981752423037,19.340508631697,2.61659179896998));
#213087=CARTESIAN_POINT('Ctrl Pts',(-59.8984626844395,19.3374641384342,
2.61765103591223));
#213088=CARTESIAN_POINT('Ctrl Pts',(-59.8987174423897,19.334430837514,2.61875422455163));
#213089=CARTESIAN_POINT('Ctrl Pts',(-59.8989398263133,19.3314101194743,
2.61990022440409));
#213090=CARTESIAN_POINT('Ctrl Pts',(-59.8993567961701,19.3257462731499,
2.62204897412746));
#213091=CARTESIAN_POINT('Ctrl Pts',(-59.8996599510838,19.3201266635127,
2.62434823201782));
#213092=CARTESIAN_POINT('Ctrl Pts',(-59.8998513356577,19.3145604567382,
2.62679048030317));
#213093=CARTESIAN_POINT('Ctrl Pts',(-59.9005211816665,19.2950787330273,
2.63533834930191));
#213094=CARTESIAN_POINT('Ctrl Pts',(-59.8998218367506,19.2762511930036,
2.64563784783575));
#213095=CARTESIAN_POINT('Ctrl Pts',(-59.8978409873528,19.2584708442944,
2.65736666737977));
#213096=CARTESIAN_POINT('Ctrl Pts',(-59.8968505626539,19.2495806699398,
2.66323107715177));
#213097=CARTESIAN_POINT('Ctrl Pts',(-59.8955397627952,19.2409522937262,
2.66945281780786));
#213098=CARTESIAN_POINT('Ctrl Pts',(-59.8939195570493,19.2326348443073,
2.67599160631213));
#213099=CARTESIAN_POINT('Ctrl Pts',(-59.8931094541763,19.2284761195978,
2.67926100056426));
#213100=CARTESIAN_POINT('Ctrl Pts',(-59.8922219999436,19.2243951266223,
2.68260965685134));
#213101=CARTESIAN_POINT('Ctrl Pts',(-59.8912585660179,19.2203980066217,
2.68603254012494));
#213102=CARTESIAN_POINT('Ctrl Pts',(-59.8902951320921,19.2164008866211,
2.68945542339853));
#213103=CARTESIAN_POINT('Ctrl Pts',(-59.889255633561,19.2124877374673,2.69295261525395));
#213104=CARTESIAN_POINT('Ctrl Pts',(-59.8881416170477,19.208664500965,2.69651891172109));
#213105=CARTESIAN_POINT('Ctrl Pts',(-59.8881321168199,19.2086318967647,
2.69654932476097));
#213106=CARTESIAN_POINT('Ctrl Pts',(-59.8881226112893,19.2085992991801,
2.69657974261156));
#213107=CARTESIAN_POINT('Ctrl Pts',(-59.8881131004568,19.208566708214,2.69661016526983));
#213108=CARTESIAN_POINT('Ctrl Pts',(-59.8832557794656,19.1919220260032,
2.71214746101221));
#213109=CARTESIAN_POINT('Ctrl Pts',(-59.8771277287708,19.1769337687786,
2.72880565567756));
#213110=CARTESIAN_POINT('Ctrl Pts',(-59.8699293191651,19.1636064551647,
2.7462804001261));
#213111=CARTESIAN_POINT('Ctrl Pts',(-59.8624874641263,19.1498284206539,
2.7643461288283));
#213112=CARTESIAN_POINT('Ctrl Pts',(-59.8539008972247,19.1378250534663,
2.78328592655013));
#213113=CARTESIAN_POINT('Ctrl Pts',(-59.8443613941432,19.1276443522912,
2.80278753268557));
#213114=CARTESIAN_POINT('Ctrl Pts',(-59.8350033524835,19.117657309475,2.82191817723668));
#213115=CARTESIAN_POINT('Ctrl Pts',(-59.824727371918,19.1094240716838,2.84159092316188));
#213116=CARTESIAN_POINT('Ctrl Pts',(-59.8136991387633,19.1030352898888,
2.86151233818209));
#213117=CARTESIAN_POINT('Ctrl Pts',(-59.8063933209299,19.0988029459297,
2.87470957722119));
#213118=CARTESIAN_POINT('Ctrl Pts',(-59.7987570771764,19.0953809833336,
2.88801594388754));
#213119=CARTESIAN_POINT('Ctrl Pts',(-59.7908376697913,19.092807720641,2.90134173516036));
#213120=CARTESIAN_POINT('',(-59.4519788726609,18.9827025415095,3.47153072139084));
#213121=CARTESIAN_POINT('',(-59.7908376697913,19.092807720641,2.90134173516036));
#213122=CARTESIAN_POINT('',(-60.9782752797349,13.2864868028993,3.4715307213908));
#213123=CARTESIAN_POINT('Origin',(5.53234440788222E-15,1.85015204418142E-13,
3.47153072139072));
#213124=CARTESIAN_POINT('',(-61.3267881959114,13.3605623192485,2.90134173516031));
#213125=CARTESIAN_POINT('',(-60.9782752797349,13.2864868028994,3.4715307213908));
#213126=CARTESIAN_POINT('',(-61.5752716937452,13.1038352065726,2.59908173516031));
#213127=CARTESIAN_POINT('Ctrl Pts',(-61.3267881959114,13.3605623192485,
2.90134173516031));
#213128=CARTESIAN_POINT('Ctrl Pts',(-61.3388252440314,13.3631207378657,
2.88164837656731));
#213129=CARTESIAN_POINT('Ctrl Pts',(-61.3512282837632,13.3637631278628,
2.8620373443915));
#213130=CARTESIAN_POINT('Ctrl Pts',(-61.3638130392407,13.3625311504984,
2.8427794597816));
#213131=CARTESIAN_POINT('Ctrl Pts',(-61.3766506715126,13.3612744179064,
2.82313460920043));
#213132=CARTESIAN_POINT('Ctrl Pts',(-61.3896782944617,13.3580674708025,
2.80385576863379));
#213133=CARTESIAN_POINT('Ctrl Pts',(-61.4027199493095,13.3529048112189,
2.78521678518442));
#213134=CARTESIAN_POINT('Ctrl Pts',(-61.4152549476891,13.3479427162799,
2.7673019093454));
#213135=CARTESIAN_POINT('Ctrl Pts',(-61.4278037696887,13.3411737181041,
2.74997687279866));
#213136=CARTESIAN_POINT('Ctrl Pts',(-61.4402150271797,13.3325479345567,
2.73349253345823));
#213137=CARTESIAN_POINT('Ctrl Pts',(-61.4497489245061,13.3259219069554,
2.72082983599351));
#213138=CARTESIAN_POINT('Ctrl Pts',(-61.459201840167,13.3181993658954,2.70866321039313));
#213139=CARTESIAN_POINT('Ctrl Pts',(-61.4685026502439,13.3093393327442,
2.69711645335852));
#213140=CARTESIAN_POINT('Ctrl Pts',(-61.4685270260084,13.3093161121774,
2.69708619136758));
#213141=CARTESIAN_POINT('Ctrl Pts',(-61.4685514007483,13.3092928829602,
2.69705593387226));
#213142=CARTESIAN_POINT('Ctrl Pts',(-61.4685757744609,13.3092696450948,
2.69702568087578));
#213143=CARTESIAN_POINT('Ctrl Pts',(-61.4711891321181,13.3067780733548,
2.69378194443274));
#213144=CARTESIAN_POINT('Ctrl Pts',(-61.4737888336847,13.3041875240727,
2.69059266624707));
#213145=CARTESIAN_POINT('Ctrl Pts',(-61.4763713294375,13.301501425748,2.68746219342684));
#213146=CARTESIAN_POINT('Ctrl Pts',(-61.4907423311174,13.2865538993111,
2.67004182396047));
#213147=CARTESIAN_POINT('Ctrl Pts',(-61.5045840828649,13.2686510078425,
2.65443567877809));
#213148=CARTESIAN_POINT('Ctrl Pts',(-61.5172886502248,13.2484387178491,
2.64136852352976));
#213149=CARTESIAN_POINT('Ctrl Pts',(-61.5229906359929,13.2393671621939,
2.6355038032962));
#213150=CARTESIAN_POINT('Ctrl Pts',(-61.5284639152923,13.2298303888501,
2.63014997451059));
#213151=CARTESIAN_POINT('Ctrl Pts',(-61.5336555255488,13.2198857715704,
2.6253698111926));
#213152=CARTESIAN_POINT('Ctrl Pts',(-61.5359117291449,13.2155639754109,
2.6232924168708));
#213153=CARTESIAN_POINT('Ctrl Pts',(-61.5381145532937,13.2111652444434,
2.62132362131434));
#213154=CARTESIAN_POINT('Ctrl Pts',(-61.5402595369763,13.2066943520821,
2.61946873372354));
#213155=CARTESIAN_POINT('Ctrl Pts',(-61.5477669798653,13.1910462288177,
2.61297662715574));
#213156=CARTESIAN_POINT('Ctrl Pts',(-61.5545658738899,13.1745141278033,
2.60787989113976));
#213157=CARTESIAN_POINT('Ctrl Pts',(-61.560464970229,13.1573027128859,2.60440616886186));
#213158=CARTESIAN_POINT('Ctrl Pts',(-61.5634145183986,13.1486970054272,
2.60266930772291));
#213159=CARTESIAN_POINT('Ctrl Pts',(-61.5661391177411,13.1399214696215,
2.60133820040192));
#213160=CARTESIAN_POINT('Ctrl Pts',(-61.5686148699002,13.1310016901029,
2.60044130723592));
#213161=CARTESIAN_POINT('Ctrl Pts',(-61.5698527459798,13.1265418003436,
2.59999286065292));
#213162=CARTESIAN_POINT('Ctrl Pts',(-61.571028410384,13.1220458496817,2.59965296768519));
#213163=CARTESIAN_POINT('Ctrl Pts',(-61.5721388765028,13.1175170363402,
2.59942518630961));
#213164=CARTESIAN_POINT('Ctrl Pts',(-61.5732493426217,13.1129882229987,
2.59919740493403));
#213165=CARTESIAN_POINT('Ctrl Pts',(-61.5742946087864,13.1084265466226,
2.59908173791626));
#213166=CARTESIAN_POINT('Ctrl Pts',(-61.5752716937452,13.1038352065726,
2.59908173516031));
#213167=CARTESIAN_POINT('',(-61.5816197022698,13.0739701745323,2.59908173516031));
#213168=CARTESIAN_POINT('Origin',(1.12331902584552E-16,1.910751710202E-13,
2.59908173516024));
#213169=CARTESIAN_POINT('',(-61.4590390555209,12.7383709431249,2.90134173516031));
#213170=CARTESIAN_POINT('Ctrl Pts',(-61.5816197022698,13.0739701745323,
2.59908173516032));
#213171=CARTESIAN_POINT('Ctrl Pts',(-61.5824133495499,13.0702318743175,
2.59908174381692));
#213172=CARTESIAN_POINT('Ctrl Pts',(-61.5831581321229,13.0664939028184,
2.59915752001004));
#213173=CARTESIAN_POINT('Ctrl Pts',(-61.5838547466226,13.0627583804525,
2.59930729517479));
#213174=CARTESIAN_POINT('Ctrl Pts',(-61.5878803190636,13.0411716694462,
2.60017281085927));
#213175=CARTESIAN_POINT('Ctrl Pts',(-61.5902997144311,13.0196643745807,
2.60350651800077));
#213176=CARTESIAN_POINT('Ctrl Pts',(-61.591245045342,12.9986523536618,2.60896880596491));
#213177=CARTESIAN_POINT('Ctrl Pts',(-61.5916263190447,12.9901777222667,
2.61117187235481));
#213178=CARTESIAN_POINT('Ctrl Pts',(-61.5917681516647,12.9817833412908,
2.61372076577216));
#213179=CARTESIAN_POINT('Ctrl Pts',(-61.591680417163,12.9734950911671,2.61659179896992));
#213180=CARTESIAN_POINT('Ctrl Pts',(-61.5916480484584,12.9704372300723,
2.61765103591218));
#213181=CARTESIAN_POINT('Ctrl Pts',(-61.5915843445341,12.9673939164349,
2.61875422455157));
#213182=CARTESIAN_POINT('Ctrl Pts',(-61.5914897592007,12.9643665007549,
2.61990022440404));
#213183=CARTESIAN_POINT('Ctrl Pts',(-61.5913124117005,12.9586900963548,
2.62204897412741));
#213184=CARTESIAN_POINT('Ctrl Pts',(-61.5910264967403,12.9530695832099,
2.62434823201778));
#213185=CARTESIAN_POINT('Ctrl Pts',(-61.5906350058491,12.9475138635631,
2.62679048030314));
#213186=CARTESIAN_POINT('Ctrl Pts',(-61.5892647877301,12.9280688447993,
2.63533834930187));
#213187=CARTESIAN_POINT('Ctrl Pts',(-61.5866012600731,12.9094175454591,
2.6456378478357));
#213188=CARTESIAN_POINT('Ctrl Pts',(-61.5827727094485,12.891941654504,2.65736666737971));
#213189=CARTESIAN_POINT('Ctrl Pts',(-61.5808584341363,12.8832037090265,
2.66323107715172));
#213190=CARTESIAN_POINT('Ctrl Pts',(-61.5786529040703,12.8747596158555,
2.66945281780782));
#213191=CARTESIAN_POINT('Ctrl Pts',(-61.5761721637749,12.8666570879115,
2.67599160631208));
#213192=CARTESIAN_POINT('Ctrl Pts',(-61.5749317936272,12.8626058239395,
2.67926100056422));
#213193=CARTESIAN_POINT('Ctrl Pts',(-61.5736226210373,12.8586399512977,
2.6826096568513));
#213194=CARTESIAN_POINT('Ctrl Pts',(-61.5722466520922,12.8547654342064,
2.68603254012489));
#213195=CARTESIAN_POINT('Ctrl Pts',(-61.5708706831472,12.8508909171151,
2.68945542339849));
#213196=CARTESIAN_POINT('Ctrl Pts',(-61.5694278436302,12.8471078617859,
2.69295261525392));
#213197=CARTESIAN_POINT('Ctrl Pts',(-61.5679202927796,12.8434220158074,
2.69651891172106));
#213198=CARTESIAN_POINT('Ctrl Pts',(-61.5679074365282,12.8433905832605,
2.69654932476094));
#213199=CARTESIAN_POINT('Ctrl Pts',(-61.5678945756944,12.8433591578474,
2.69657974261152));
#213200=CARTESIAN_POINT('Ctrl Pts',(-61.5678817102797,12.8433277395707,
2.6966101652698));
#213201=CARTESIAN_POINT('Ctrl Pts',(-61.5613111551478,12.8272819669692,
2.71214746101236));
#213202=CARTESIAN_POINT('Ctrl Pts',(-61.5536499750612,12.8130163727078,
2.72880565567793));
#213203=CARTESIAN_POINT('Ctrl Pts',(-61.5450979154847,12.8005145062063,
2.74628040012671));
#213204=CARTESIAN_POINT('Ctrl Pts',(-61.5362566309321,12.7875898348812,
2.76434612882914));
#213205=CARTESIAN_POINT('Ctrl Pts',(-61.5264624086162,12.7765497640378,
2.78328592655121));
#213206=CARTESIAN_POINT('Ctrl Pts',(-61.5159109908817,12.7674219834065,
2.8027875326869));
#213207=CARTESIAN_POINT('Ctrl Pts',(-61.5055602833149,12.7584678323696,
2.82191817723834));
#213208=CARTESIAN_POINT('Ctrl Pts',(-61.4944799879519,12.7513538295737,
2.8415909231639));
#213209=CARTESIAN_POINT('Ctrl Pts',(-61.4828443590689,12.746152810458,2.86151233818444));
#213210=CARTESIAN_POINT('Ctrl Pts',(-61.4751361628604,12.7427073176333,
2.87470957722276));
#213211=CARTESIAN_POINT('Ctrl Pts',(-61.4671840587581,12.7401023057312,
2.8880159438883));
#213212=CARTESIAN_POINT('Ctrl Pts',(-61.4590390555209,12.7383709431249,
2.9013417351603));
#213213=CARTESIAN_POINT('',(-61.1105274371642,12.6642893210139,3.47153072139079));
#213214=CARTESIAN_POINT('',(-61.4590390555209,12.7383709431249,2.90134173516031));
#213215=CARTESIAN_POINT('',(-62.0330459552233,6.83973663030237,3.47153072139075));
#213216=CARTESIAN_POINT('Origin',(5.53234440788222E-15,1.85015204418142E-13,
3.47153072139072));
#213217=CARTESIAN_POINT('',(-62.3873926810692,6.87697683366542,2.90134173516027));
#213218=CARTESIAN_POINT('',(-62.0330459552233,6.83973663030238,3.47153072139076));
#213219=CARTESIAN_POINT('',(-62.6076796697355,6.59568250079864,2.59908173516026));
#213220=CARTESIAN_POINT('Ctrl Pts',(-62.3873926810692,6.87697683366542,
2.90134173516026));
#213221=CARTESIAN_POINT('Ctrl Pts',(-62.3996312165471,6.87826302285565,
2.88164837656657));
#213222=CARTESIAN_POINT('Ctrl Pts',(-62.412033459169,6.87760542309004,2.86203734439007));
#213223=CARTESIAN_POINT('Ctrl Pts',(-62.4244204973391,6.87506472947568,
2.84277945977952));
#213224=CARTESIAN_POINT('Ctrl Pts',(-62.4370564393921,6.87247298342269,
2.82313460919761));
#213225=CARTESIAN_POINT('Ctrl Pts',(-62.4496774784074,6.86792184690335,
2.80385576863027));
#213226=CARTESIAN_POINT('Ctrl Pts',(-62.4621080448333,6.86142424476877,
2.78521678518027));
#213227=CARTESIAN_POINT('Ctrl Pts',(-62.4740556950222,6.85517906858685,
2.76730190934053));
#213228=CARTESIAN_POINT('Ctrl Pts',(-62.4858282202851,6.84713544261114,
2.74997687279314));
#213229=CARTESIAN_POINT('Ctrl Pts',(-62.4972698477107,6.8372595823348,2.73349253345217));
#213230=CARTESIAN_POINT('Ctrl Pts',(-62.5060589088659,6.82967328917041,
2.72082983598962));
#213231=CARTESIAN_POINT('Ctrl Pts',(-62.5146528151147,6.82100495425208,
2.70866321039126));
#213232=CARTESIAN_POINT('Ctrl Pts',(-62.5229765487298,6.81122125790657,
2.69711645335848));
#213233=CARTESIAN_POINT('Ctrl Pts',(-62.5229983637511,6.81119561658327,
2.69708619136754));
#213234=CARTESIAN_POINT('Ctrl Pts',(-62.5230201768492,6.81116996676408,
2.69705593387221));
#213235=CARTESIAN_POINT('Ctrl Pts',(-62.5230419880218,6.81114430845134,
2.69702568087573));
#213236=CARTESIAN_POINT('Ctrl Pts',(-62.5253805892672,6.80839321554225,
2.69378194443269));
#213237=CARTESIAN_POINT('Ctrl Pts',(-62.5276952632611,6.80554511475047,
2.69059266624703));
#213238=CARTESIAN_POINT('Ctrl Pts',(-62.5299828381019,6.80260378684094,
2.6874621934268));
#213239=CARTESIAN_POINT('Ctrl Pts',(-62.5427126719616,6.7862359657982,2.6700418239621));
#213240=CARTESIAN_POINT('Ctrl Pts',(-62.5546072354103,6.76698429120527,
2.65443567878105));
#213241=CARTESIAN_POINT('Ctrl Pts',(-62.5651294462082,6.74555473735121,
2.64136852353349));
#213242=CARTESIAN_POINT('Ctrl Pts',(-62.5698519601306,6.73593685681528,
2.63550380329846));
#213243=CARTESIAN_POINT('Ctrl Pts',(-62.5742983919722,6.72588021343749,
2.63014997451158));
#213244=CARTESIAN_POINT('Ctrl Pts',(-62.5784220664834,6.71544740276753,
2.62536981119257));
#213245=CARTESIAN_POINT('Ctrl Pts',(-62.580214159649,6.71091344436488,2.62329241687077));
#213246=CARTESIAN_POINT('Ctrl Pts',(-62.5819451239082,6.70630855228272,
2.62132362131432));
#213247=CARTESIAN_POINT('Ctrl Pts',(-62.5836110216378,6.70163794008952,
2.61946873372352));
#213248=CARTESIAN_POINT('Ctrl Pts',(-62.5894416636914,6.68529079741334,
2.61297662715572));
#213249=CARTESIAN_POINT('Ctrl Pts',(-62.5944752375494,6.66813858303381,
2.60787989113972));
#213250=CARTESIAN_POINT('Ctrl Pts',(-62.5985429352697,6.65040483057315,
2.60440616886183));
#213251=CARTESIAN_POINT('Ctrl Pts',(-62.6005767841298,6.64153795434282,
2.60266930772288));
#213252=CARTESIAN_POINT('Ctrl Pts',(-62.6023691645599,6.63252569365819,
2.60133820040187));
#213253=CARTESIAN_POINT('Ctrl Pts',(-62.6038989834438,6.62339599105648,
2.60044130723587));
#213254=CARTESIAN_POINT('Ctrl Pts',(-62.6046638928858,6.61883113975562,
2.59999286065287));
#213255=CARTESIAN_POINT('Ctrl Pts',(-62.6053631620638,6.61423692798835,
2.59965296768515));
#213256=CARTESIAN_POINT('Ctrl Pts',(-62.6059941550341,6.60961684864329,
2.59942518630957));
#213257=CARTESIAN_POINT('Ctrl Pts',(-62.6066251480043,6.60499676929823,
2.59919740493399));
#213258=CARTESIAN_POINT('Ctrl Pts',(-62.6071878630701,6.60035082219668,
2.59908173791619));
#213259=CARTESIAN_POINT('Ctrl Pts',(-62.6076796697355,6.59568250079864,
2.59908173516027));
#213260=CARTESIAN_POINT('',(-62.6108711573006,6.5653175249528,2.59908173516027));
#213261=CARTESIAN_POINT('Origin',(1.148766751165E-16,1.91091238081628E-13,
2.59908173516023));
#213262=CARTESIAN_POINT('',(-62.4538823482276,6.24436990788037,2.90134173516026));
#213263=CARTESIAN_POINT('Ctrl Pts',(-62.6108711573006,6.5653175249528,2.59908173516027));
#213264=CARTESIAN_POINT('Ctrl Pts',(-62.6112696981211,6.56151674480722,
2.59908174381689));
#213265=CARTESIAN_POINT('Ctrl Pts',(-62.6116196762807,6.5577213993292,2.59915752000999));
#213266=CARTESIAN_POINT('Ctrl Pts',(-62.6119220062409,6.55393352450258,
2.59930729517474));
#213267=CARTESIAN_POINT('Ctrl Pts',(-62.6136691004464,6.53204428085739,
2.60017281085919));
#213268=CARTESIAN_POINT('Ctrl Pts',(-62.6138271176316,6.51040190952424,
2.60350651800055));
#213269=CARTESIAN_POINT('Ctrl Pts',(-62.6125709156642,6.48940618066758,
2.60896880596443));
#213270=CARTESIAN_POINT('Ctrl Pts',(-62.6120642605131,6.48093812023513,
2.61117187235443));
#213271=CARTESIAN_POINT('Ctrl Pts',(-62.6113278644157,6.4725748990102,2.61372076577192));
#213272=CARTESIAN_POINT('Ctrl Pts',(-62.610374252484,6.46434122354008,2.61659179896986));
#213273=CARTESIAN_POINT('Ctrl Pts',(-62.6100224275775,6.46130349717916,
2.61765103591212));
#213274=CARTESIAN_POINT('Ctrl Pts',(-62.6096409597322,6.45828351400561,
2.61875422455152));
#213275=CARTESIAN_POINT('Ctrl Pts',(-62.6092304414384,6.45528256968502,
2.61990022440398));
#213276=CARTESIAN_POINT('Ctrl Pts',(-62.6084607196375,6.4496557990839,2.62204897412735));
#213277=CARTESIAN_POINT('Ctrl Pts',(-62.6075888673476,6.4440959619495,2.62434823201773));
#213278=CARTESIAN_POINT('Ctrl Pts',(-62.6066187902475,6.43861159905745,
2.62679048030308));
#213279=CARTESIAN_POINT('Ctrl Pts',(-62.6032235203971,6.41941632893527,
2.63533834930182));
#213280=CARTESIAN_POINT('Ctrl Pts',(-62.5986249921653,6.40114561781729,
2.64563784783565));
#213281=CARTESIAN_POINT('Ctrl Pts',(-62.5929906867159,6.38416565413471,
2.65736666737967));
#213282=CARTESIAN_POINT('Ctrl Pts',(-62.5901735339912,6.37567567229342,
2.66323107715167));
#213283=CARTESIAN_POINT('Ctrl Pts',(-62.5870974379668,6.36750837741682,
2.66945281780776));
#213284=CARTESIAN_POINT('Ctrl Pts',(-62.5837833426318,6.35970954393955,
2.67599160631203));
#213285=CARTESIAN_POINT('Ctrl Pts',(-62.5821262949642,6.35581012720091,
2.67926100056416));
#213286=CARTESIAN_POINT('Ctrl Pts',(-62.580409747586,6.35200282582336,2.68260965685125));
#213287=CARTESIAN_POINT('Ctrl Pts',(-62.5786363190253,6.34829336166141,
2.68603254012485));
#213288=CARTESIAN_POINT('Ctrl Pts',(-62.5768628904647,6.34458389749946,
2.68945542339844));
#213289=CARTESIAN_POINT('Ctrl Pts',(-62.5750325180135,6.34097238394057,
2.69295261525388));
#213290=CARTESIAN_POINT('Ctrl Pts',(-62.5731479498682,6.33746431138572,
2.69651891172102));
#213291=CARTESIAN_POINT('Ctrl Pts',(-62.5731318784488,6.33743439487387,
2.6965493247609));
#213292=CARTESIAN_POINT('Ctrl Pts',(-62.5731158032179,6.3374044859356,2.69657974261148));
#213293=CARTESIAN_POINT('Ctrl Pts',(-62.5730997241771,6.33737458457355,
2.69661016526975));
#213294=CARTESIAN_POINT('Ctrl Pts',(-62.5648879232822,6.32210352242481,
2.71214746101154));
#213295=CARTESIAN_POINT('Ctrl Pts',(-62.5557775512964,6.30871688796325,
2.72880565567622));
#213296=CARTESIAN_POINT('Ctrl Pts',(-62.5459655399043,6.2971774416402,2.74628040012404));
#213297=CARTESIAN_POINT('Ctrl Pts',(-62.5358216928023,6.28524773890498,
2.76434612882545));
#213298=CARTESIAN_POINT('Ctrl Pts',(-62.524927122622,6.27529192173268,2.78328592654642));
#213299=CARTESIAN_POINT('Ctrl Pts',(-62.5134793937762,6.26731706751981,
2.802787532681));
#213300=CARTESIAN_POINT('Ctrl Pts',(-62.5022494248214,6.25949391181485,
2.82191817723141));
#213301=CARTESIAN_POINT('Ctrl Pts',(-62.4904862126964,6.25357708651719,
2.84159092315592));
#213302=CARTESIAN_POINT('Ctrl Pts',(-62.4783706704711,6.24962081353434,
2.86151233817543));
#213303=CARTESIAN_POINT('Ctrl Pts',(-62.470344548496,6.24699992138305,2.87470957721668));
#213304=CARTESIAN_POINT('Ctrl Pts',(-62.4621637089593,6.24524040122967,
2.88801594388524));
#213305=CARTESIAN_POINT('Ctrl Pts',(-62.4538823482276,6.24436990788038,
2.90134173516025));
#213306=CARTESIAN_POINT('',(-62.0995362748659,6.20712349654441,3.47153072139075));
#213307=CARTESIAN_POINT('',(-62.4538823482276,6.24436990788037,2.90134173516027));
#213308=CARTESIAN_POINT('',(-62.4081695979768,0.318048871877305,3.47153072139071));
#213309=CARTESIAN_POINT('Origin',(5.53234440788222E-15,1.85015204418142E-13,
3.47153072139072));
#213310=CARTESIAN_POINT('',(-62.7644678366119,0.318045750793233,2.90134173516022));
#213311=CARTESIAN_POINT('',(-62.4081695979768,0.318048871877314,3.47153072139071));
#213312=CARTESIAN_POINT('Ctrl Pts',(-62.7644678366119,0.318045750793234,
2.90134173516022));
#213313=CARTESIAN_POINT('Ctrl Pts',(-62.7767737714904,0.318045618798321,
2.88164837656814));
#213314=CARTESIAN_POINT('Ctrl Pts',(-62.7890393354357,0.316095234070967,
2.86203734439325));
#213315=CARTESIAN_POINT('Ctrl Pts',(-62.8010929413145,0.312273660578323,
2.84277945978422));
#213316=CARTESIAN_POINT('Ctrl Pts',(-62.8133887511217,0.308375296777275,
2.82313460920393));
#213317=CARTESIAN_POINT('Ctrl Pts',(-62.8254649274573,0.302529834047833,
2.80385576863813));
#213318=CARTESIAN_POINT('Ctrl Pts',(-62.8371482135727,0.294768478452875,
2.78521678518951));
#213319=CARTESIAN_POINT('Ctrl Pts',(-62.8483776146138,0.287308644486914,
2.76730190935116));
#213320=CARTESIAN_POINT('Ctrl Pts',(-62.8592448608884,0.278078518363015,
2.74997687280502));
#213321=CARTESIAN_POINT('Ctrl Pts',(-62.869591501383,0.267060783352459,
2.73349253346508));
#213322=CARTESIAN_POINT('Ctrl Pts',(-62.8775394315781,0.258597341637538,
2.72082983599787));
#213323=CARTESIAN_POINT('Ctrl Pts',(-62.885180171784,0.249078184948348,
2.70866321039515));
#213324=CARTESIAN_POINT('Ctrl Pts',(-62.8924356323738,0.238478017628062,
2.69711645335844));
#213325=CARTESIAN_POINT('Ctrl Pts',(-62.892454647642,0.238450236479951,
2.6970861913675));
#213326=CARTESIAN_POINT('Ctrl Pts',(-62.8924736601095,0.238422447083525,
2.69705593387217));
#213327=CARTESIAN_POINT('Ctrl Pts',(-62.8924926697742,0.23839464944136,
2.69702568087569));
#213328=CARTESIAN_POINT('Ctrl Pts',(-62.8945308924032,0.235414176912695,
2.69378194443264));
#213329=CARTESIAN_POINT('Ctrl Pts',(-62.8965351787718,0.232339728999503,
2.69059266624698));
#213330=CARTESIAN_POINT('Ctrl Pts',(-62.8985027695519,0.22917539730931,
2.68746219342675));
#213331=CARTESIAN_POINT('Ctrl Pts',(-62.9094519648697,0.211566610930952,
2.6700418239612));
#213332=CARTESIAN_POINT('Ctrl Pts',(-62.9192690206952,0.191177078586108,
2.65443567877947));
#213333=CARTESIAN_POINT('Ctrl Pts',(-62.9274935913887,0.168765047544095,
2.64136852353151));
#213334=CARTESIAN_POINT('Ctrl Pts',(-62.9311848926129,0.158706217641999,
2.63550380329723));
#213335=CARTESIAN_POINT('Ctrl Pts',(-62.9345557609574,0.148239886922536,
2.63014997451099));
#213336=CARTESIAN_POINT('Ctrl Pts',(-62.9375663198809,0.137433186922523,
2.6253698111925));
#213337=CARTESIAN_POINT('Ctrl Pts',(-62.9388746680683,0.132736741273776,
2.6232924168707));
#213338=CARTESIAN_POINT('Ctrl Pts',(-62.9401148076313,0.127976140238265,
2.62132362131425));
#213339=CARTESIAN_POINT('Ctrl Pts',(-62.9412833674838,0.123156980417726,
2.61946873372345));
#213340=CARTESIAN_POINT('Ctrl Pts',(-62.9453733269673,0.10628992104584,
2.61297662715565));
#213341=CARTESIAN_POINT('Ctrl Pts',(-62.9485864317704,0.0887055165512269,
2.60787989113966));
#213342=CARTESIAN_POINT('Ctrl Pts',(-62.9507781643242,0.070643721250341,
2.60440616886177));
#213343=CARTESIAN_POINT('Ctrl Pts',(-62.9518740306011,0.061612823599898,
2.60266930772282));
#213344=CARTESIAN_POINT('Ctrl Pts',(-62.9527145544237,0.0524625782503221,
2.60133820040182));
#213345=CARTESIAN_POINT('Ctrl Pts',(-62.9532816790167,0.0432229794977032,
2.60044130723581));
#213346=CARTESIAN_POINT('Ctrl Pts',(-62.9535652413132,0.0386031801213938,
2.59999286065281));
#213347=CARTESIAN_POINT('Ctrl Pts',(-62.9537804539255,0.0339610423942995,
2.5996529676851));
#213348=CARTESIAN_POINT('Ctrl Pts',(-62.9539250604562,0.0293003156017882,
2.59942518630953));
#213349=CARTESIAN_POINT('Ctrl Pts',(-62.9540696669868,0.0246395888092768,
2.59919740493395));
#213350=CARTESIAN_POINT('Ctrl Pts',(-62.9541436657296,0.0199602729509832,
2.59908173791615));
#213351=CARTESIAN_POINT('Ctrl Pts',(-62.9541448057648,0.0152661173110579,
2.59908173516022));
#213352=CARTESIAN_POINT('',(-62.2224557307631,1.90550834334536E-13,3.77003198860262));
#213353=CARTESIAN_POINT('',(-62.7644678366119,-0.318045750792855,2.90134173516021));
#213354=CARTESIAN_POINT('Ctrl Pts',(-62.9541448057648,-0.0152661173106757,
2.59908173516023));
#213355=CARTESIAN_POINT('Ctrl Pts',(-62.9541438736292,-0.0190877352444563,
2.59908174381683));
#213356=CARTESIAN_POINT('Ctrl Pts',(-62.9540952129414,-0.0228988721020315,
2.59915752000994));
#213357=CARTESIAN_POINT('Ctrl Pts',(-62.9539999459718,-0.0266975986401531,
2.59930729517469));
#213358=CARTESIAN_POINT('Ctrl Pts',(-62.9534494204121,-0.0486495517880578,
2.60017281085904));
#213359=CARTESIAN_POINT('Ctrl Pts',(-62.9513443281462,-0.0701898812374375,
2.60350651799966));
#213360=CARTESIAN_POINT('Ctrl Pts',(-62.9479003565128,-0.0909392844309831,
2.60896880596233));
#213361=CARTESIAN_POINT('Ctrl Pts',(-62.9465113235275,-0.0993079960606954,
2.6111718723528));
#213362=CARTESIAN_POINT('Ctrl Pts',(-62.9449047668219,-0.107548428334892,
2.61372076577099));
#213363=CARTESIAN_POINT('Ctrl Pts',(-62.9430957254317,-0.11563731928203,
2.61659179896983));
#213364=CARTESIAN_POINT('Ctrl Pts',(-62.9424282989905,-0.118621628943286,
2.61765103591208));
#213365=CARTESIAN_POINT('Ctrl Pts',(-62.9417332466658,-0.121585194085372,
2.61875422455148));
#213366=CARTESIAN_POINT('Ctrl Pts',(-62.941011293136,-0.124526788072593,
2.61990022440394));
#213367=CARTESIAN_POINT('Ctrl Pts',(-62.9396576302675,-0.130042276798633,
2.62204897412731));
#213368=CARTESIAN_POINT('Ctrl Pts',(-62.938209392844,-0.135480523183407,
2.62434823201768));
#213369=CARTESIAN_POINT('Ctrl Pts',(-62.9366713579026,-0.140833441493173,
2.62679048030304));
#213370=CARTESIAN_POINT('Ctrl Pts',(-62.9312882356078,-0.159568655577355,
2.63533834930178));
#213371=CARTESIAN_POINT('Ctrl Pts',(-62.9248050892389,-0.177258600738774,
2.64563784783561));
#213372=CARTESIAN_POINT('Ctrl Pts',(-62.9174267595942,-0.193556601113454,
2.65736666737962));
#213373=CARTESIAN_POINT('Ctrl Pts',(-62.9137375947719,-0.201705601300794,
2.66323107715163));
#213374=CARTESIAN_POINT('Ctrl Pts',(-62.9098246351408,-0.20950661529121,
2.66945281780772));
#213375=CARTESIAN_POINT('Ctrl Pts',(-62.9057134946881,-0.216916308650201,
2.67599160631199));
#213376=CARTESIAN_POINT('Ctrl Pts',(-62.9036579244618,-0.220621155329696,
2.67926100056413));
#213377=CARTESIAN_POINT('Ctrl Pts',(-62.9015528091474,-0.224228171852353,
2.68260965685121));
#213378=CARTESIAN_POINT('Ctrl Pts',(-62.8994013510256,-0.227731941419342,
2.68603254012481));
#213379=CARTESIAN_POINT('Ctrl Pts',(-62.8972498929038,-0.23123571098633,
2.6894554233984));
#213380=CARTESIAN_POINT('Ctrl Pts',(-62.8950520414621,-0.234636114276541,
2.69295261525383));
#213381=CARTESIAN_POINT('Ctrl Pts',(-62.8928111037451,-0.237927978230728,
2.69651891172097));
#213382=CARTESIAN_POINT('Ctrl Pts',(-62.8927919932396,-0.237956050936022,
2.69654932476085));
#213383=CARTESIAN_POINT('Ctrl Pts',(-62.8927728797351,-0.237984115710813,
2.69657974261143));
#213384=CARTESIAN_POINT('Ctrl Pts',(-62.8927537632335,-0.238012172552645,
2.69661016526971));
#213385=CARTESIAN_POINT('Ctrl Pts',(-62.8829906867838,-0.252341211297632,
2.71214746101229));
#213386=CARTESIAN_POINT('Ctrl Pts',(-62.8725309380398,-0.264702219192015,
2.72880565567787));
#213387=CARTESIAN_POINT('Ctrl Pts',(-62.861566477281,-0.275152816748675,
2.74628040012666));
#213388=CARTESIAN_POINT('Ctrl Pts',(-62.8502312057401,-0.285956846575219,
2.76434612882901));
#213389=CARTESIAN_POINT('Ctrl Pts',(-62.8383556508849,-0.294719332060581,
2.783285926551));
#213390=CARTESIAN_POINT('Ctrl Pts',(-62.8261370346392,-0.301453885683407,
2.80278753268661));
#213391=CARTESIAN_POINT('Ctrl Pts',(-62.8141508421851,-0.308060333925367,
2.82191817723792));
#213392=CARTESIAN_POINT('Ctrl Pts',(-62.8018335935106,-0.31271515574816,
2.84159092316334));
#213393=CARTESIAN_POINT('Ctrl Pts',(-62.7893708783575,-0.315383336842736,
2.86151233818375));
#213394=CARTESIAN_POINT('Ctrl Pts',(-62.7811147664911,-0.31715091327579,
2.87470957722226));
#213395=CARTESIAN_POINT('Ctrl Pts',(-62.7727948225133,-0.318045664008263,
2.88801594388801));
#213396=CARTESIAN_POINT('Ctrl Pts',(-62.7644678366119,-0.318045750792856,
2.90134173516021));
#213397=CARTESIAN_POINT('',(-62.4081695979768,-0.318048871876942,3.4715307213907));
#213398=CARTESIAN_POINT('',(-62.7644678366119,-0.318045750792856,2.90134173516021));
#213399=CARTESIAN_POINT('',(-62.0995362748658,-6.20712349654488,3.47153072139067));
#213400=CARTESIAN_POINT('Origin',(5.53234440788222E-15,1.85015204418142E-13,
3.47153072139072));
#213401=CARTESIAN_POINT('',(-62.4538823482275,-6.24436990788084,2.90134173516018));
#213402=CARTESIAN_POINT('',(-62.0995362748658,-6.20712349654488,3.47153072139066));
#213403=CARTESIAN_POINT('',(-62.6108711573005,-6.56531752495326,2.59908173516017));
#213404=CARTESIAN_POINT('Ctrl Pts',(-62.4538823482275,-6.24436990788084,
2.90134173516018));
#213405=CARTESIAN_POINT('Ctrl Pts',(-62.4661208561115,-6.24565635961485,
2.8816483765655));
#213406=CARTESIAN_POINT('Ctrl Pts',(-62.4781153572974,-6.24887816048161,
2.86203734438804));
#213407=CARTESIAN_POINT('Ctrl Pts',(-62.4897034690589,-6.25393874389528,
2.84277945977656));
#213408=CARTESIAN_POINT('Ctrl Pts',(-62.5015244311575,-6.25910101415649,
2.82313460919377));
#213409=CARTESIAN_POINT('Ctrl Pts',(-62.5129234357008,-6.26617675898563,
2.80385576862559));
#213410=CARTESIAN_POINT('Ctrl Pts',(-62.5237314369803,-6.27511683300826,
2.78521678517484));
#213411=CARTESIAN_POINT('Ctrl Pts',(-62.5341195572078,-6.28370959325942,
2.76730190933462));
#213412=CARTESIAN_POINT('Ctrl Pts',(-62.5439624606715,-6.29402509234208,
2.74997687278681));
#213413=CARTESIAN_POINT('Ctrl Pts',(-62.5531007542782,-6.30606398948117,
2.73349253344551));
#213414=CARTESIAN_POINT('Ctrl Pts',(-62.5601204743196,-6.31531185250257,
2.72082983598532));
#213415=CARTESIAN_POINT('Ctrl Pts',(-62.5667243349272,-6.32557753708262,
2.70866321038916));
#213416=CARTESIAN_POINT('Ctrl Pts',(-62.5728320301412,-6.33687803771715,
2.69711645335838));
#213417=CARTESIAN_POINT('Ctrl Pts',(-62.5728480373211,-6.33690765431399,
2.69708619136744));
#213418=CARTESIAN_POINT('Ctrl Pts',(-62.5728640408534,-6.3369372788212,
2.69705593387211));
#213419=CARTESIAN_POINT('Ctrl Pts',(-62.5728800407363,-6.33696691123601,
2.69702568087563));
#213420=CARTESIAN_POINT('Ctrl Pts',(-62.5745955535552,-6.34014410870351,
2.69378194443259));
#213421=CARTESIAN_POINT('Ctrl Pts',(-62.5762674929177,-6.34341121944343,
2.69059266624693));
#213422=CARTESIAN_POINT('Ctrl Pts',(-62.5778935423007,-6.34676388583411,
2.6874621934267));
#213423=CARTESIAN_POINT('Ctrl Pts',(-62.5869421374015,-6.36542071200024,
2.67004182395984));
#213424=CARTESIAN_POINT('Ctrl Pts',(-62.5945741278857,-6.38672471011456,
2.65443567877707));
#213425=CARTESIAN_POINT('Ctrl Pts',(-62.6004109483571,-6.40987366744317,
2.64136852352852));
#213426=CARTESIAN_POINT('Ctrl Pts',(-62.6030305942145,-6.42026324006541,
2.63550380329538));
#213427=CARTESIAN_POINT('Ctrl Pts',(-62.6052889671228,-6.43102458681625,
2.63014997451014));
#213428=CARTESIAN_POINT('Ctrl Pts',(-62.6071534261453,-6.44208677567895,
2.62536981119245));
#213429=CARTESIAN_POINT('Ctrl Pts',(-62.6079636948179,-6.44689425333248,
2.62329241687065));
#213430=CARTESIAN_POINT('Ctrl Pts',(-62.6086994224562,-6.45175840518017,
2.62132362131419));
#213431=CARTESIAN_POINT('Ctrl Pts',(-62.6093578414452,-6.45667331290459,
2.61946873372339));
#213432=CARTESIAN_POINT('Ctrl Pts',(-62.6116623079068,-6.47387548994004,
2.6129766271556));
#213433=CARTESIAN_POINT('Ctrl Pts',(-62.6130197402062,-6.49169942613433,
2.60787989113962));
#213434=CARTESIAN_POINT('Ctrl Pts',(-62.6133114945132,-6.50989137546646,
2.60440616886172));
#213435=CARTESIAN_POINT('Ctrl Pts',(-62.6134573716666,-6.51898735013253,
2.60266930772277));
#213436=CARTESIAN_POINT('Ctrl Pts',(-62.6133368299269,-6.52817532814419,
2.60133820040178));
#213437=CARTESIAN_POINT('Ctrl Pts',(-62.6129350466932,-6.53742359207027,
2.60044130723578));
#213438=CARTESIAN_POINT('Ctrl Pts',(-62.6127341550763,-6.54204772403331,
2.59999286065278));
#213439=CARTESIAN_POINT('Ctrl Pts',(-62.6124629532085,-6.54668692748786,
2.59965296768506));
#213440=CARTESIAN_POINT('Ctrl Pts',(-62.6121195889601,-6.55133723782977,
2.59942518630948));
#213441=CARTESIAN_POINT('Ctrl Pts',(-62.6117762247117,-6.55598754817168,
2.5991974049339));
#213442=CARTESIAN_POINT('Ctrl Pts',(-62.6113606963859,-6.56064896522296,
2.59908173791611));
#213443=CARTESIAN_POINT('Ctrl Pts',(-62.6108711573005,-6.56531752495326,
2.59908173516018));
#213444=CARTESIAN_POINT('',(-62.6076796697354,-6.5956825007991,2.59908173516018));
#213445=CARTESIAN_POINT('Origin',(1.14876675116497E-16,1.91123728172721E-13,
2.59908173516023));
#213446=CARTESIAN_POINT('',(-62.3873926810691,-6.87697683366589,2.90134173516017));
#213447=CARTESIAN_POINT('Ctrl Pts',(-62.6076796697354,-6.5956825007991,
2.59908173516018));
#213448=CARTESIAN_POINT('Ctrl Pts',(-62.6072792748562,-6.59948308607527,
2.59908174381681));
#213449=CARTESIAN_POINT('Ctrl Pts',(-62.6068325084578,-6.60326825869946,
2.59915752000989));
#213450=CARTESIAN_POINT('Ctrl Pts',(-62.6063406883232,-6.60703621730621,
2.59930729517464));
#213451=CARTESIAN_POINT('Ctrl Pts',(-62.6034985746717,-6.62881036976824,
2.60017281085903));
#213452=CARTESIAN_POINT('Ctrl Pts',(-62.5991534367856,-6.65001265698052,
2.60350651799994));
#213453=CARTESIAN_POINT('Ctrl Pts',(-62.5935594283592,-6.67028839971087,
2.60896880596309));
#213454=CARTESIAN_POINT('Ctrl Pts',(-62.591303236076,-6.67846607317822,
2.61117187235337));
#213455=CARTESIAN_POINT('Ctrl Pts',(-62.5888441205341,-6.68649343259762,
2.61372076577129));
#213456=CARTESIAN_POINT('Ctrl Pts',(-62.586199469922,-6.69434891543633,
2.61659179896978));
#213457=CARTESIAN_POINT('Ctrl Pts',(-62.5852237544099,-6.69724711167676,
2.61765103591203));
#213458=CARTESIAN_POINT('Ctrl Pts',(-62.5842227327444,-6.70012178934752,
2.61875422455144));
#213459=CARTESIAN_POINT('Ctrl Pts',(-62.5831972538525,-6.70297180428207,
2.6199002244039));
#213460=CARTESIAN_POINT('Ctrl Pts',(-62.5812744809302,-6.70831558228435,
2.62204897412727));
#213461=CARTESIAN_POINT('Ctrl Pts',(-62.5792657255653,-6.71357265535409,
2.62434823201763));
#213462=CARTESIAN_POINT('Ctrl Pts',(-62.5771765838154,-6.71873548138839,
2.62679048030299));
#213463=CARTESIAN_POINT('Ctrl Pts',(-62.5698645876906,-6.73680537250846,
2.63533834930172));
#213464=CARTESIAN_POINT('Ctrl Pts',(-62.5615678538927,-6.75372073697227,
2.64563784783556));
#213465=CARTESIAN_POINT('Ctrl Pts',(-62.5525263385764,-6.76915820973636,
2.65736666737958));
#213466=CARTESIAN_POINT('Ctrl Pts',(-62.5480055809182,-6.77687694611841,
2.66323107715158));
#213467=CARTESIAN_POINT('Ctrl Pts',(-62.5432986288851,-6.7842262096809,
2.66945281780768));
#213468=CARTESIAN_POINT('Ctrl Pts',(-62.5384354858298,-6.79116558077058,
2.67599160631195));
#213469=CARTESIAN_POINT('Ctrl Pts',(-62.5360039143022,-6.79463526631542,
2.67926100056409));
#213470=CARTESIAN_POINT('Ctrl Pts',(-62.5335332951357,-6.79800247875535,
2.68260965685116));
#213471=CARTESIAN_POINT('Ctrl Pts',(-62.5310273792781,-6.80126216569478,
2.68603254012475));
#213472=CARTESIAN_POINT('Ctrl Pts',(-62.5285214634206,-6.80452185263422,
2.68945542339835));
#213473=CARTESIAN_POINT('Ctrl Pts',(-62.5259802131086,-6.80767389012573,
2.69295261525378));
#213474=CARTESIAN_POINT('Ctrl Pts',(-62.5234074580024,-6.8107134791289,
2.69651891172092));
#213475=CARTESIAN_POINT('Ctrl Pts',(-62.5233855177896,-6.81073940045721,
2.6965493247608));
#213476=CARTESIAN_POINT('Ctrl Pts',(-62.5233635754231,-6.81076531358497,
2.69657974261138));
#213477=CARTESIAN_POINT('Ctrl Pts',(-62.5233416309051,-6.81079121850996,
2.69661016526966));
#213478=CARTESIAN_POINT('Ctrl Pts',(-62.5121342452089,-6.82402124190414,
2.71214746101314));
#213479=CARTESIAN_POINT('Ctrl Pts',(-62.5004397189026,-6.8352211934421,
2.72880565567975));
#213480=CARTESIAN_POINT('Ctrl Pts',(-62.4884429377036,-6.84446844329853,
2.74628040012967));
#213481=CARTESIAN_POINT('Ctrl Pts',(-62.4760404333306,-6.85402842900468,
2.76434612883316));
#213482=CARTESIAN_POINT('Ctrl Pts',(-62.4633140048645,-6.86150157917835,
2.78328592655637));
#213483=CARTESIAN_POINT('Ctrl Pts',(-62.4504583709352,-6.86692204703221,
2.80278753269324));
#213484=CARTESIAN_POINT('Ctrl Pts',(-62.4378472782144,-6.8722394061816,
2.82191817724563));
#213485=CARTESIAN_POINT('Ctrl Pts',(-62.4251109433444,-6.87558122532737,
2.84159092317214));
#213486=CARTESIAN_POINT('Ctrl Pts',(-62.4124375993787,-6.87693208138303,
2.86151233819362));
#213487=CARTESIAN_POINT('Ctrl Pts',(-62.4040419533109,-6.87782697616081,
2.87470957722888));
#213488=CARTESIAN_POINT('Ctrl Pts',(-62.3956740599399,-6.87784715439644,
2.8880159438913));
#213489=CARTESIAN_POINT('Ctrl Pts',(-62.3873926810691,-6.87697683366589,
2.90134173516017));
#213490=CARTESIAN_POINT('',(-62.0330459552232,-6.83973663030285,3.47153072139066));
#213491=CARTESIAN_POINT('',(-62.3873926810691,-6.87697683366589,2.90134173516017));
#213492=CARTESIAN_POINT('',(-61.110527437164,-12.6642893210144,3.47153072139062));
#213493=CARTESIAN_POINT('Origin',(5.53234440788222E-15,1.85015204418142E-13,
3.47153072139072));
#213494=CARTESIAN_POINT('',(-61.4590390555207,-12.7383709431253,2.90134173516013));
#213495=CARTESIAN_POINT('',(-61.110527437164,-12.6642893210144,3.47153072139062));
#213496=CARTESIAN_POINT('',(-61.5816197022697,-13.0739701745327,2.59908173516013));
#213497=CARTESIAN_POINT('Ctrl Pts',(-61.4590390555208,-12.7383709431253,
2.90134173516013));
#213498=CARTESIAN_POINT('Ctrl Pts',(-61.4710760487536,-12.7409296199635,
2.88164837656823));
#213499=CARTESIAN_POINT('Ctrl Pts',(-61.4826680729118,-12.7453875382437,
2.8620373443935));
#213500=CARTESIAN_POINT('Ctrl Pts',(-61.4936637287758,-12.7516316867652,
2.84277945978463));
#213501=CARTESIAN_POINT('Ctrl Pts',(-61.5048803302284,-12.7580013045708,
2.8231346092045));
#213502=CARTESIAN_POINT('Ctrl Pts',(-61.5154772730974,-12.7662298081553,
2.80385576863884));
#213503=CARTESIAN_POINT('Ctrl Pts',(-61.525291574815,-12.7762506512793,
2.78521678519036));
#213504=CARTESIAN_POINT('Ctrl Pts',(-61.5347245998078,-12.7858821937322,
2.76730190935215));
#213505=CARTESIAN_POINT('Ctrl Pts',(-61.543435319549,-12.7971700470021,
2.74997687280613));
#213506=CARTESIAN_POINT('Ctrl Pts',(-61.5512651452094,-12.8100982055875,
2.73349253346629));
#213507=CARTESIAN_POINT('Ctrl Pts',(-61.5572797455837,-12.8200291684005,
2.72082983599861));
#213508=CARTESIAN_POINT('Ctrl Pts',(-61.5627743733217,-12.8309289078927,
2.70866321039545));
#213509=CARTESIAN_POINT('Ctrl Pts',(-61.5676673859795,-12.8428059312037,
2.69711645335834));
#213510=CARTESIAN_POINT('Ctrl Pts',(-61.567680209693,-12.8428370587637,
2.6970861913674));
#213511=CARTESIAN_POINT('Ctrl Pts',(-61.5676930289521,-12.8428681938094,
2.69705593387208));
#213512=CARTESIAN_POINT('Ctrl Pts',(-61.5677058437552,-12.8428993363379,
2.6970256808756));
#213513=CARTESIAN_POINT('Ctrl Pts',(-61.5690798512466,-12.8462384487039,
2.69378194443255));
#213514=CARTESIAN_POINT('Ctrl Pts',(-61.5704011254853,-12.8496624271216,
2.69059266624688));
#213515=CARTESIAN_POINT('Ctrl Pts',(-61.5716678181341,-12.8531666956982,
2.68746219342665));
#213516=CARTESIAN_POINT('Ctrl Pts',(-61.5787166747154,-12.8726671535587,
2.67004182396012));
#213517=CARTESIAN_POINT('Ctrl Pts',(-61.5840799821728,-12.8946522063788,
2.65443567877762));
#213518=CARTESIAN_POINT('Ctrl Pts',(-61.587465102995,-12.9182844651708,
2.64136852352922));
#213519=CARTESIAN_POINT('Ctrl Pts',(-61.5889843920982,-12.9288909501833,
2.6355038032958));
#213520=CARTESIAN_POINT('Ctrl Pts',(-61.590105526365,-12.9398294094007,
2.63014997451031));
#213521=CARTESIAN_POINT('Ctrl Pts',(-61.5908034580837,-12.9510258874722,
2.62536981119243));
#213522=CARTESIAN_POINT('Ctrl Pts',(-61.5911067697684,-12.9558917253993,
2.62329241687063));
#213523=CARTESIAN_POINT('Ctrl Pts',(-61.591330024696,-12.9608061353937,
2.62132362131416));
#213524=CARTESIAN_POINT('Ctrl Pts',(-61.5914710890454,-12.9657629422644,
2.61946873372336));
#213525=CARTESIAN_POINT('Ctrl Pts',(-61.5919648142681,-12.9831117663121,
2.61297662715556));
#213526=CARTESIAN_POINT('Ctrl Pts',(-61.5914517017517,-13.0009799514312,
2.60787989113959));
#213527=CARTESIAN_POINT('Ctrl Pts',(-61.5898402812904,-13.0191027399908,
2.60440616886169));
#213528=CARTESIAN_POINT('Ctrl Pts',(-61.5890345710598,-13.0281641342706,
2.60266930772274));
#213529=CARTESIAN_POINT('Ctrl Pts',(-61.5879542844383,-13.0372891795346,
2.60133820040173));
#213530=CARTESIAN_POINT('Ctrl Pts',(-61.5865879953991,-13.0464447827192,
2.60044130723573));
#213531=CARTESIAN_POINT('Ctrl Pts',(-61.5859048508795,-13.0510225843115,
2.59999286065273));
#213532=CARTESIAN_POINT('Ctrl Pts',(-61.585150205876,-13.0556080254097,
2.599652967685));
#213533=CARTESIAN_POINT('Ctrl Pts',(-61.5843226328191,-13.0601969695278,
2.59942518630943));
#213534=CARTESIAN_POINT('Ctrl Pts',(-61.5834950597623,-13.0647859136458,
2.59919740493385));
#213535=CARTESIAN_POINT('Ctrl Pts',(-61.582594556983,-13.0693783604294,
2.59908173791607));
#213536=CARTESIAN_POINT('Ctrl Pts',(-61.5816197022697,-13.0739701745327,
2.59908173516013));
#213537=CARTESIAN_POINT('',(-61.575271693745,-13.103835206573,2.59908173516013));
#213538=CARTESIAN_POINT('Origin',(1.12331902584553E-16,1.91139795234149E-13,
2.59908173516023));
#213539=CARTESIAN_POINT('',(-61.3267881959112,-13.3605623192489,2.90134173516012));
#213540=CARTESIAN_POINT('Ctrl Pts',(-61.575271693745,-13.103835206573,2.59908173516014));
#213541=CARTESIAN_POINT('Ctrl Pts',(-61.5744762229325,-13.107573119184,
2.5990817438167));
#213542=CARTESIAN_POINT('Ctrl Pts',(-61.5736362456895,-13.1112908564314,
2.59915752000985));
#213543=CARTESIAN_POINT('Ctrl Pts',(-61.5727532608743,-13.1149867645638,
2.59930729517459));
#213544=CARTESIAN_POINT('Ctrl Pts',(-61.5676506979224,-13.1363445541701,
2.60017281085907));
#213545=CARTESIAN_POINT('Ctrl Pts',(-61.5611131206554,-13.1569765024506,
2.60350651800056));
#213546=CARTESIAN_POINT('Ctrl Pts',(-61.5534303645623,-13.1765564394382,
2.60896880596467));
#213547=CARTESIAN_POINT('Ctrl Pts',(-61.5503317322965,-13.1844534784405,
2.61117187235458));
#213548=CARTESIAN_POINT('Ctrl Pts',(-61.5470470005034,-13.1921798155745,
2.61372076577195));
#213549=CARTESIAN_POINT('Ctrl Pts',(-61.5435957160156,-13.19971582399,2.61659179896972));
#213550=CARTESIAN_POINT('Ctrl Pts',(-61.5423224015758,-13.2024961535652,
2.61765103591197));
#213551=CARTESIAN_POINT('Ctrl Pts',(-61.5410263779725,-13.2052504481945,
2.61875422455137));
#213552=CARTESIAN_POINT('Ctrl Pts',(-61.5397086090799,-13.2079776587163,
2.61990022440384));
#213553=CARTESIAN_POINT('Ctrl Pts',(-61.5372377924062,-13.2130911784448,
2.62204897412721));
#213554=CARTESIAN_POINT('Ctrl Pts',(-61.5346905274441,-13.2181094806068,
2.62434823201759));
#213555=CARTESIAN_POINT('Ctrl Pts',(-61.5320731679598,-13.2230256493633,
2.62679048030294));
#213556=CARTESIAN_POINT('Ctrl Pts',(-61.5229124097646,-13.2402322400107,
2.63533834930168));
#213557=CARTESIAN_POINT('Ctrl Pts',(-61.5128929892896,-13.2561876955041,
2.64563784783551));
#213558=CARTESIAN_POINT('Ctrl Pts',(-61.5022873490354,-13.2705955044755,
2.65736666737953));
#213559=CARTESIAN_POINT('Ctrl Pts',(-61.4969845289083,-13.2777994089612,
2.66323107715154));
#213560=CARTESIAN_POINT('Ctrl Pts',(-61.4915351548246,-13.2846164020263,
2.66945281780763));
#213561=CARTESIAN_POINT('Ctrl Pts',(-61.4859732907798,-13.2910094216448,
2.6759916063119));
#213562=CARTESIAN_POINT('Ctrl Pts',(-61.4831923587574,-13.2942059314541,
2.67926100056404));
#213563=CARTESIAN_POINT('Ctrl Pts',(-61.4803833043594,-13.2972964479272,
2.68260965685112));
#213564=CARTESIAN_POINT('Ctrl Pts',(-61.4775503861045,-13.3002763384268,
2.68603254012471));
#213565=CARTESIAN_POINT('Ctrl Pts',(-61.4747174678497,-13.3032562289265,
2.68945542339831));
#213566=CARTESIAN_POINT('Ctrl Pts',(-61.4718606611377,-13.3061253662369,
2.69295261525373));
#213567=CARTESIAN_POINT('Ctrl Pts',(-61.4689842762857,-13.3088793779159,
2.69651891172087));
#213568=CARTESIAN_POINT('Ctrl Pts',(-61.468959746747,-13.3089028638677,
2.69654932476075));
#213569=CARTESIAN_POINT('Ctrl Pts',(-61.4689352159237,-13.3089263414388,
2.69657974261133));
#213570=CARTESIAN_POINT('Ctrl Pts',(-61.4689106838181,-13.3089498106271,
2.69661016526961));
#213571=CARTESIAN_POINT('Ctrl Pts',(-61.4563817793397,-13.3209358677642,
2.71214746101225));
#213572=CARTESIAN_POINT('Ctrl Pts',(-61.4435806031499,-13.3308520539319,
2.7288056556779));
#213573=CARTESIAN_POINT('Ctrl Pts',(-61.4306829407573,-13.3387946412829,
2.74628040012677));
#213574=CARTESIAN_POINT('Ctrl Pts',(-61.4173490879869,-13.3470058416641,
2.76434612882926));
#213575=CARTESIAN_POINT('Ctrl Pts',(-61.4039112193248,-13.3531077791288,
2.7832859265514));
#213576=CARTESIAN_POINT('Ctrl Pts',(-61.390559416729,-13.3571547734338,
2.80278753268716));
#213577=CARTESIAN_POINT('Ctrl Pts',(-61.3774615935137,-13.3611247853914,
2.82191817723859));
#213578=CARTESIAN_POINT('Ctrl Pts',(-61.3644457143994,-13.3631169881911,
2.84159092316412));
#213579=CARTESIAN_POINT('Ctrl Pts',(-61.3517005934309,-13.3631357189473,
2.86151233818464));
#213580=CARTESIAN_POINT('Ctrl Pts',(-61.3432573976128,-13.3631481274167,
2.87470957722283));
#213581=CARTESIAN_POINT('Ctrl Pts',(-61.3349332352353,-13.3622935120789,
2.88801594388825));
#213582=CARTESIAN_POINT('Ctrl Pts',(-61.3267881959112,-13.3605623192489,
2.90134173516012));
#213583=CARTESIAN_POINT('',(-60.9782752797347,-13.2864868028998,3.47153072139061));
#213584=CARTESIAN_POINT('',(-61.3267881959112,-13.3605623192489,2.90134173516012));
#213585=CARTESIAN_POINT('',(-59.4519788726606,-18.98270254151,3.47153072139058));
#213586=CARTESIAN_POINT('Origin',(5.53234440788222E-15,1.85015204418142E-13,
3.47153072139072));
#213587=CARTESIAN_POINT('',(-59.790837669791,-19.0928077206414,2.90134173516009));
#213588=CARTESIAN_POINT('',(-59.4519788726606,-18.98270254151,3.47153072139058));
#213589=CARTESIAN_POINT('',(-59.8776671349984,-19.4393816709759,2.59908173516009));
#213590=CARTESIAN_POINT('Ctrl Pts',(-59.790837669791,-19.0928077206414,
2.90134173516009));
#213591=CARTESIAN_POINT('Ctrl Pts',(-59.8025412685584,-19.0966105891854,
2.88164837656674));
#213592=CARTESIAN_POINT('Ctrl Pts',(-59.813603811049,-19.1022557829948,
2.86203734439059));
#213593=CARTESIAN_POINT('Ctrl Pts',(-59.8238865403109,-19.1096150844282,
2.84277945978036));
#213594=CARTESIAN_POINT('Ctrl Pts',(-59.834375889687,-19.1171222629148,
2.82313460919879));
#213595=CARTESIAN_POINT('Ctrl Pts',(-59.84405466856,-19.1264133720502,2.80385576863178));
#213596=CARTESIAN_POINT('Ctrl Pts',(-59.8527677431739,-19.137405193825,
2.78521678518207));
#213597=CARTESIAN_POINT('Ctrl Pts',(-59.8611423227377,-19.1479699932883,
2.76730190934267));
#213598=CARTESIAN_POINT('Ctrl Pts',(-59.868625422289,-19.1601065286669,
2.74997687279559));
#213599=CARTESIAN_POINT('Ctrl Pts',(-59.8750609947955,-19.1737823050926,
2.73349253345488));
#213600=CARTESIAN_POINT('Ctrl Pts',(-59.8800045782761,-19.184287561984,
2.72082983599128));
#213601=CARTESIAN_POINT('Ctrl Pts',(-59.8843297728478,-19.1957019365533,
2.70866321039196));
#213602=CARTESIAN_POINT('Ctrl Pts',(-59.8879544940743,-19.2080253553781,
2.6971164533583));
#213603=CARTESIAN_POINT('Ctrl Pts',(-59.8879639938222,-19.2080576528611,
2.69708619136736));
#213604=CARTESIAN_POINT('Ctrl Pts',(-59.8879734883575,-19.2080899573232,
2.69705593387203));
#213605=CARTESIAN_POINT('Ctrl Pts',(-59.8879829776791,-19.2081222687614,
2.69702568087555));
#213606=CARTESIAN_POINT('Ctrl Pts',(-59.8890004259295,-19.2115867120121,
2.6937819444325));
#213607=CARTESIAN_POINT('Ctrl Pts',(-59.8899565588874,-19.2151300442834,
2.69059266624684));
#213608=CARTESIAN_POINT('Ctrl Pts',(-59.8908500166521,-19.2187475215461,
2.68746219342661));
#213609=CARTESIAN_POINT('Ctrl Pts',(-59.8958219059659,-19.2388779600028,
2.67004182396144));
#213610=CARTESIAN_POINT('Ctrl Pts',(-59.8988577688777,-19.2613031946878,
2.65443567878001));
#213611=CARTESIAN_POINT('Ctrl Pts',(-59.8997541019591,-19.2851598349689,
2.64136852353223));
#213612=CARTESIAN_POINT('Ctrl Pts',(-59.9001563886588,-19.2958670255037,
2.63550380329761));
#213613=CARTESIAN_POINT('Ctrl Pts',(-59.9001280009023,-19.3068627531409,
2.63014997451108));
#213614=CARTESIAN_POINT('Ctrl Pts',(-59.8996517586311,-19.3180708494661,
2.62536981119236));
#213615=CARTESIAN_POINT('Ctrl Pts',(-59.8994447901816,-19.3229417365282,
2.62329241687056));
#213616=CARTESIAN_POINT('Ctrl Pts',(-59.8991531263708,-19.3278525613649,
2.62132362131411));
#213617=CARTESIAN_POINT('Ctrl Pts',(-59.89877529055,-19.3327969595686,2.61946873372331));
#213618=CARTESIAN_POINT('Ctrl Pts',(-59.8974528651771,-19.3501023532817,
2.61297662715552));
#213619=CARTESIAN_POINT('Ctrl Pts',(-59.8950748296128,-19.3678190197503,
2.60787989113953));
#213620=CARTESIAN_POINT('Ctrl Pts',(-59.8915778894432,-19.3856740904735,
2.60440616886164));
#213621=CARTESIAN_POINT('Ctrl Pts',(-59.8898294193584,-19.3946016258351,
2.60266930772269));
#213622=CARTESIAN_POINT('Ctrl Pts',(-59.8878012237013,-19.4035637624459,
2.6013382004017));
#213623=CARTESIAN_POINT('Ctrl Pts',(-59.8854853982053,-19.4125263941846,
2.6004413072357));
#213624=CARTESIAN_POINT('Ctrl Pts',(-59.8843274854572,-19.417007710054,
2.5999928606527));
#213625=CARTESIAN_POINT('Ctrl Pts',(-59.8830976653666,-19.4214891497435,
2.59965296768497));
#213626=CARTESIAN_POINT('Ctrl Pts',(-59.8817949505649,-19.4259664502057,
2.59942518630939));
#213627=CARTESIAN_POINT('Ctrl Pts',(-59.8804922357631,-19.4304437506678,
2.59919740493381));
#213628=CARTESIAN_POINT('Ctrl Pts',(-59.8791166246274,-19.4349169113758,
2.59908173791598));
#213629=CARTESIAN_POINT('Ctrl Pts',(-59.8776671349984,-19.4393816709759,
2.59908173516009));
#213630=CARTESIAN_POINT('',(-59.868232155624,-19.4684195516699,2.59908173516009));
#213631=CARTESIAN_POINT('Origin',(1.08121605342496E-16,1.91155508277372E-13,
2.59908173516023));
#213632=CARTESIAN_POINT('',(-59.5942745858234,-19.6977666881848,2.90134173516009));
#213633=CARTESIAN_POINT('Ctrl Pts',(-59.868232155624,-19.4684195516699,
2.59908173516009));
#213634=CARTESIAN_POINT('Ctrl Pts',(-59.8670503242228,-19.4720538382629,
2.59908174381669));
#213635=CARTESIAN_POINT('Ctrl Pts',(-59.8658263391017,-19.4756634078263,
2.59915752000981));
#213636=CARTESIAN_POINT('Ctrl Pts',(-59.8645618637722,-19.4792467723414,
2.59930729517456));
#213637=CARTESIAN_POINT('Ctrl Pts',(-59.8572547562677,-19.4999541986775,
2.60017281085904));
#213638=CARTESIAN_POINT('Ctrl Pts',(-59.848596366685,-19.5197897600815,
2.60350651800056));
#213639=CARTESIAN_POINT('Ctrl Pts',(-59.8389090368093,-19.5384593694377,
2.60896880596472));
#213640=CARTESIAN_POINT('Ctrl Pts',(-59.8350019138241,-19.5459892523649,
2.61117187235461));
#213641=CARTESIAN_POINT('Ctrl Pts',(-59.8309275539882,-19.553329915849,
2.61372076577195));
#213642=CARTESIAN_POINT('Ctrl Pts',(-59.8267074486191,-19.560463883758,
2.61659179896968));
#213643=CARTESIAN_POINT('Ctrl Pts',(-59.8251504859513,-19.5630958847952,
2.61765103591193));
#213644=CARTESIAN_POINT('Ctrl Pts',(-59.8235736599158,-19.5656996197547,
2.61875422455134));
#213645=CARTESIAN_POINT('Ctrl Pts',(-59.8219780387742,-19.5682741459747,
2.6199002244038));
#213646=CARTESIAN_POINT('Ctrl Pts',(-59.8189862491337,-19.5731013826371,
2.62204897412717));
#213647=CARTESIAN_POINT('Ctrl Pts',(-59.8159283829424,-19.5778259323228,
2.62434823201754));
#213648=CARTESIAN_POINT('Ctrl Pts',(-59.8128114820619,-19.5824415812277,
2.62679048030289));
#213649=CARTESIAN_POINT('Ctrl Pts',(-59.8019023289802,-19.5985963523948,
2.63533834930163));
#213650=CARTESIAN_POINT('Ctrl Pts',(-59.7902699966955,-19.6134170876084,
2.64563784783547));
#213651=CARTESIAN_POINT('Ctrl Pts',(-59.7782164291174,-19.626637377817,
2.65736666737949));
#213652=CARTESIAN_POINT('Ctrl Pts',(-59.7721896453284,-19.6332475229213,
2.6632310771515));
#213653=CARTESIAN_POINT('Ctrl Pts',(-59.7660575536769,-19.6394575570863,
2.66945281780758));
#213654=CARTESIAN_POINT('Ctrl Pts',(-59.7598579055889,-19.645234181973,
2.67599160631185));
#213655=CARTESIAN_POINT('Ctrl Pts',(-59.7567580815449,-19.6481224944163,
2.67926100056399));
#213656=CARTESIAN_POINT('Ctrl Pts',(-59.7536413685032,-19.6509024545773,
2.68260965685108));
#213657=CARTESIAN_POINT('Ctrl Pts',(-59.7505124858963,-19.6535699003333,
2.68603254012467));
#213658=CARTESIAN_POINT('Ctrl Pts',(-59.7473836032895,-19.6562373460893,
2.68945542339827));
#213659=CARTESIAN_POINT('Ctrl Pts',(-59.7442425399495,-19.6587921483498,
2.6929526152537));
#213660=CARTESIAN_POINT('Ctrl Pts',(-59.7410940396261,-19.6612304091763,
2.69651891172084));
#213661=CARTESIAN_POINT('Ctrl Pts',(-59.7410671895124,-19.6612512024347,
2.69654932476071));
#213662=CARTESIAN_POINT('Ctrl Pts',(-59.741040338997,-19.6612719872239,
2.6965797426113));
#213663=CARTESIAN_POINT('Ctrl Pts',(-59.7410134880827,-19.6612927635423,
2.69661016526957));
#213664=CARTESIAN_POINT('Ctrl Pts',(-59.7273003341204,-19.6719035326729,
2.71214746101264));
#213665=CARTESIAN_POINT('Ctrl Pts',(-59.7135327604112,-19.6804273096603,
2.72880565567879));
#213666=CARTESIAN_POINT('Ctrl Pts',(-59.6998755263121,-19.6869782138572,
2.7462804001282));
#213667=CARTESIAN_POINT('Ctrl Pts',(-59.6857564136245,-19.6937506652841,
2.76434612883127));
#213668=CARTESIAN_POINT('Ctrl Pts',(-59.6717543328665,-19.698414535936,
2.78328592655404));
#213669=CARTESIAN_POINT('Ctrl Pts',(-59.6580526467464,-19.7010437169754,
2.80278753269046));
#213670=CARTESIAN_POINT('Ctrl Pts',(-59.6446115955276,-19.7036228854591,
2.82191817724254));
#213671=CARTESIAN_POINT('Ctrl Pts',(-59.6314587768635,-19.7042436449212,
2.84159092316874));
#213672=CARTESIAN_POINT('Ctrl Pts',(-59.6187815171037,-19.7029300451591,
2.86151233818992));
#213673=CARTESIAN_POINT('Ctrl Pts',(-59.6103832769587,-19.7020598313695,
2.87470957722636));
#213674=CARTESIAN_POINT('Ctrl Pts',(-59.6021940468427,-19.7003397858028,
2.88801594389));
#213675=CARTESIAN_POINT('Ctrl Pts',(-59.5942745858234,-19.6977666881848,
2.90134173516009));
#213676=CARTESIAN_POINT('',(-59.255413859757,-19.5876674457081,3.47153072139057));
#213677=CARTESIAN_POINT('',(-59.5942745858234,-19.6977666881848,2.90134173516009));
#213678=CARTESIAN_POINT('',(-57.1420619865019,-25.0931373005748,3.47153072139054));
#213679=CARTESIAN_POINT('Origin',(5.53234440788222E-15,1.85015204418142E-13,
3.47153072139072));
#213680=CARTESIAN_POINT('',(-57.4675553545138,-25.2380597013433,2.90134173516005));
#213681=CARTESIAN_POINT('',(-57.1420619865019,-25.0931373005748,3.47153072139053));
#213682=CARTESIAN_POINT('',(-57.5176823163886,-25.5918112338797,2.59908173516005));
#213683=CARTESIAN_POINT('Ctrl Pts',(-57.4675553545138,-25.2380597013433,
2.90134173516005));
#213684=CARTESIAN_POINT('Ctrl Pts',(-57.4787973317383,-25.2430650965696,
2.88164837656564));
#213685=CARTESIAN_POINT('Ctrl Pts',(-57.4892091890304,-25.2498357159834,
2.86203734438844));
#213686=CARTESIAN_POINT('Ctrl Pts',(-57.4986663319564,-25.2582295402821,
2.84277945977721));
#213687=CARTESIAN_POINT('Ctrl Pts',(-57.5083135057489,-25.2667920292311,
2.82313460919456));
#213688=CARTESIAN_POINT('Ctrl Pts',(-57.5169680778989,-25.2770439485812,
2.80385576862652));
#213689=CARTESIAN_POINT('Ctrl Pts',(-57.5244844631399,-25.2888863203071,
2.78521678517588));
#213690=CARTESIAN_POINT('Ctrl Pts',(-57.5317088436281,-25.3002686266268,
2.76730190933564));
#213691=CARTESIAN_POINT('Ctrl Pts',(-57.5378823365847,-25.3131208736925,
2.74997687278781));
#213692=CARTESIAN_POINT('Ctrl Pts',(-57.5428531464576,-25.3273944332896,
2.73349253344648));
#213693=CARTESIAN_POINT('Ctrl Pts',(-57.5466715501105,-25.3383588864668,
2.72082983598588));
#213694=CARTESIAN_POINT('Ctrl Pts',(-57.54977992378,-25.3501628378374,2.70866321038936));
#213695=CARTESIAN_POINT('Ctrl Pts',(-57.5520966403719,-25.3627976342212,
2.69711645335824));
#213696=CARTESIAN_POINT('Ctrl Pts',(-57.5521027120729,-25.3628307477693,
2.6970861913673));
#213697=CARTESIAN_POINT('Ctrl Pts',(-57.5521087778604,-25.3628638677133,
2.69705593387198));
#213698=CARTESIAN_POINT('Ctrl Pts',(-57.5521148377335,-25.3628969940503,
2.6970256808755));
#213699=CARTESIAN_POINT('Ctrl Pts',(-57.5527645793668,-25.3664488110204,
2.69378194443245));
#213700=CARTESIAN_POINT('Ctrl Pts',(-57.5533450954511,-25.3700726756556,
2.6905926662468));
#213701=CARTESIAN_POINT('Ctrl Pts',(-57.5538555294215,-25.3737637277665,
2.68746219342657));
#213702=CARTESIAN_POINT('Ctrl Pts',(-57.5566959784091,-25.3943035935275,
2.67004182395887));
#213703=CARTESIAN_POINT('Ctrl Pts',(-57.5573711352259,-25.416923314519,
2.65443567877544));
#213704=CARTESIAN_POINT('Ctrl Pts',(-57.5557688601527,-25.4407429579518,
2.6413685235265));
#213705=CARTESIAN_POINT('Ctrl Pts',(-57.5550497369112,-25.4514335437838,
2.63550380329411));
#213706=CARTESIAN_POINT('Ctrl Pts',(-57.5538721381537,-25.4623660683425,
2.63014997450951));
#213707=CARTESIAN_POINT('Ctrl Pts',(-57.5522269397029,-25.4734629846669,
2.62536981119234));
#213708=CARTESIAN_POINT('Ctrl Pts',(-57.551511958709,-25.478285554406,2.62329241687053));
#213709=CARTESIAN_POINT('Ctrl Pts',(-57.5507085716895,-25.4831389900605,
2.62132362131408));
#213710=CARTESIAN_POINT('Ctrl Pts',(-57.5498159753468,-25.4880168077358,
2.61946873372328));
#213711=CARTESIAN_POINT('Ctrl Pts',(-57.5466918881474,-25.5050891695994,
2.61297662715548));
#213712=CARTESIAN_POINT('Ctrl Pts',(-57.5424749837906,-25.5224602099123,
2.6078798911395));
#213713=CARTESIAN_POINT('Ctrl Pts',(-57.5371308371209,-25.5398519389078,
2.6044061688616));
#213714=CARTESIAN_POINT('Ctrl Pts',(-57.534458763786,-25.5485478034055,
2.60266930772265));
#213715=CARTESIAN_POINT('Ctrl Pts',(-57.5315048804294,-25.557248840319,
2.60133820040166));
#213716=CARTESIAN_POINT('Ctrl Pts',(-57.5282648911452,-25.565920304143,
2.60044130723566));
#213717=CARTESIAN_POINT('Ctrl Pts',(-57.5266448965032,-25.5702560360551,
2.59999286065266));
#213718=CARTESIAN_POINT('Ctrl Pts',(-57.5249533754917,-25.5745843747449,
2.59965296768492));
#213719=CARTESIAN_POINT('Ctrl Pts',(-57.5231897917611,-25.5789009773103,
2.59942518630934));
#213720=CARTESIAN_POINT('Ctrl Pts',(-57.5214262080304,-25.5832175798758,
2.59919740493376));
#213721=CARTESIAN_POINT('Ctrl Pts',(-57.5195905600217,-25.5875224456232,
2.59908173791597));
#213722=CARTESIAN_POINT('Ctrl Pts',(-57.5176823163886,-25.5918112338797,
2.59908173516005));
#213723=CARTESIAN_POINT('',(-57.505263737773,-25.61970381813,2.59908173516005));
#213724=CARTESIAN_POINT('Origin',(1.02291912287982E-16,1.91170695146999E-13,
2.59908173516023));
#213725=CARTESIAN_POINT('',(-57.2088336324697,-25.8191582032623,2.90134173516005));
#213726=CARTESIAN_POINT('Ctrl Pts',(-57.505263737773,-25.61970381813,2.59908173516005));
#213727=CARTESIAN_POINT('Ctrl Pts',(-57.5037084941752,-25.6231946607006,
2.59908174381664));
#213728=CARTESIAN_POINT('Ctrl Pts',(-57.5021139114131,-25.6266565153805,
2.59915752000977));
#213729=CARTESIAN_POINT('Ctrl Pts',(-57.5004817994257,-25.6300880761868,
2.59930729517452));
#213730=CARTESIAN_POINT('Ctrl Pts',(-57.4910502055666,-25.6499182643584,
2.60017281085909));
#213731=CARTESIAN_POINT('Ctrl Pts',(-57.4803658667951,-25.668740116326,
2.60350651800119));
#213732=CARTESIAN_POINT('Ctrl Pts',(-57.468780099549,-25.6862948499051,
2.60896880596634));
#213733=CARTESIAN_POINT('Ctrl Pts',(-57.4641072931024,-25.6933750777824,
2.61117187235585));
#213734=CARTESIAN_POINT('Ctrl Pts',(-57.4592879447638,-25.7002496417697,
2.61372076577263));
#213735=CARTESIAN_POINT('Ctrl Pts',(-57.4543452548722,-25.7069034079254,
2.61659179896964));
#213736=CARTESIAN_POINT('Ctrl Pts',(-57.452521702385,-25.7093582436704,
2.6176510359119));
#213737=CARTESIAN_POINT('Ctrl Pts',(-57.4506813499535,-25.7117828918951,
2.61875422455131));
#213738=CARTESIAN_POINT('Ctrl Pts',(-57.448825358522,-25.7141765267651,
2.61990022440377));
#213739=CARTESIAN_POINT('Ctrl Pts',(-57.4453453745881,-25.7186645921465,
2.62204897412714));
#213740=CARTESIAN_POINT('Ctrl Pts',(-57.4418104097894,-25.7230436262008,
2.62434823201751));
#213741=CARTESIAN_POINT('Ctrl Pts',(-57.4382281169311,-25.7273081852389,
2.62679048030286));
#213742=CARTESIAN_POINT('Ctrl Pts',(-57.4256900919268,-25.742234141872,
2.6353383493016));
#213743=CARTESIAN_POINT('Ctrl Pts',(-57.4125722940991,-25.7557577777295,
2.64563784783544));
#213744=CARTESIAN_POINT('Ctrl Pts',(-57.399202860606,-25.7676457049092,
2.65736666737945));
#213745=CARTESIAN_POINT('Ctrl Pts',(-57.3925181438594,-25.7735896684991,
2.66323107715146));
#213746=CARTESIAN_POINT('Ctrl Pts',(-57.3857705191195,-25.7791247053303,
2.66945281780755));
#213747=CARTESIAN_POINT('Ctrl Pts',(-57.3790010116301,-25.7842216455739,
2.67599160631182));
#213748=CARTESIAN_POINT('Ctrl Pts',(-57.3756162578855,-25.7867701156958,
2.67926100056395));
#213749=CARTESIAN_POINT('Ctrl Pts',(-57.3722260335603,-25.7892090617194,
2.68260965685103));
#213750=CARTESIAN_POINT('Ctrl Pts',(-57.368835467294,-25.7915348376378,
2.68603254012463));
#213751=CARTESIAN_POINT('Ctrl Pts',(-57.3654449010277,-25.7938606135562,
2.68945542339822));
#213752=CARTESIAN_POINT('Ctrl Pts',(-57.3620539952072,-25.7960730898187,
2.69295261525365));
#213753=CARTESIAN_POINT('Ctrl Pts',(-57.3586678750408,-25.7981688856969,
2.69651891172079));
#213754=CARTESIAN_POINT('Ctrl Pts',(-57.3586389985274,-25.7981867584464,
2.69654932476067));
#213755=CARTESIAN_POINT('Ctrl Pts',(-57.3586101224999,-25.7982046227313,
2.69657974261125));
#213756=CARTESIAN_POINT('Ctrl Pts',(-57.3585812469611,-25.79822247855,2.69661016526953));
#213757=CARTESIAN_POINT('Ctrl Pts',(-57.343834087701,-25.8073417058661,
2.71214746101119));
#213758=CARTESIAN_POINT('Ctrl Pts',(-57.3292509568927,-25.8143796853881,
2.72880565567573));
#213759=CARTESIAN_POINT('Ctrl Pts',(-57.3149837826035,-25.8194671333533,
2.74628040012341));
#213760=CARTESIAN_POINT('Ctrl Pts',(-57.3002341019535,-25.8247266354307,
2.76434612882476));
#213761=CARTESIAN_POINT('Ctrl Pts',(-57.285821218828,-25.8279013409272,
2.78328592654568));
#213762=CARTESIAN_POINT('Ctrl Pts',(-57.2719197677254,-25.8290839028441,
2.80278753268019));
#213763=CARTESIAN_POINT('Ctrl Pts',(-57.2582827514744,-25.830243969945,
2.82191817723063));
#213764=CARTESIAN_POINT('Ctrl Pts',(-57.2451370982952,-25.8294864849001,
2.84159092315515));
#213765=CARTESIAN_POINT('Ctrl Pts',(-57.2326665944559,-25.8268549466949,
2.8615123381747));
#213766=CARTESIAN_POINT('Ctrl Pts',(-57.2244053228559,-25.825111644891,
2.87470957721612));
#213767=CARTESIAN_POINT('Ctrl Pts',(-57.2164407479159,-25.8225450142739,
2.88801594388485));
#213768=CARTESIAN_POINT('Ctrl Pts',(-57.2088336324697,-25.8191582032623,
2.90134173516005));
#213769=CARTESIAN_POINT('',(-56.8833377255392,-25.6742415049982,3.47153072139053));
#213770=CARTESIAN_POINT('',(-57.2088336324697,-25.8191582032623,2.90134173516005));
#213771=CARTESIAN_POINT('',(-54.2060847114739,-30.9286463962981,3.47153072139049));
#213772=CARTESIAN_POINT('Origin',(5.53234440788222E-15,1.85015204418142E-13,
3.47153072139072));
#213773=CARTESIAN_POINT('',(-54.5146464769135,-31.1067982185537,2.90134173516001));
#213774=CARTESIAN_POINT('',(-54.2060847114739,-30.9286463962981,3.47153072139049));
#213775=CARTESIAN_POINT('',(-54.5275217339717,-31.4638515574743,2.59908173516001));
#213776=CARTESIAN_POINT('Ctrl Pts',(-54.5146464769135,-31.1067982185537,
2.90134173516001));
#213777=CARTESIAN_POINT('Ctrl Pts',(-54.525303663139,-31.1129513003045,
2.88164837656633));
#213778=CARTESIAN_POINT('Ctrl Pts',(-54.5349507607444,-31.120773164999,
2.86203734438985));
#213779=CARTESIAN_POINT('Ctrl Pts',(-54.5434787028968,-31.1301095476664,
2.84277945977932));
#213780=CARTESIAN_POINT('Ctrl Pts',(-54.5521780046499,-31.1396335346559,
2.82313460919749));
#213781=CARTESIAN_POINT('Ctrl Pts',(-54.5597135487728,-31.1507339420456,
2.80385576863023));
#213782=CARTESIAN_POINT('Ctrl Pts',(-54.565950893551,-31.1632971162178,
2.78521678518031));
#213783=CARTESIAN_POINT('Ctrl Pts',(-54.5719459231389,-31.1753722224622,
2.76730190934082));
#213784=CARTESIAN_POINT('Ctrl Pts',(-54.5767421714198,-31.1887993693045,
2.74997687279367));
#213785=CARTESIAN_POINT('Ctrl Pts',(-54.5801937574263,-31.2035143279648,
2.73349253345291));
#213786=CARTESIAN_POINT('Ctrl Pts',(-54.582845146024,-31.2148178485878,
2.72082983598999));
#213787=CARTESIAN_POINT('Ctrl Pts',(-54.5847026428005,-31.2268820502026,
2.70866321039129));
#213788=CARTESIAN_POINT('Ctrl Pts',(-54.585685972327,-31.2396897946772,
2.69711645335821));
#213789=CARTESIAN_POINT('Ctrl Pts',(-54.5856885494583,-31.2397233614914,
2.69708619136727));
#213790=CARTESIAN_POINT('Ctrl Pts',(-54.5856911200399,-31.2397569340484,
2.69705593387194));
#213791=CARTESIAN_POINT('Ctrl Pts',(-54.5856936840713,-31.239790512345,
2.69702568087546));
#213792=CARTESIAN_POINT('Ctrl Pts',(-54.5859686003823,-31.2433907885846,
2.69378194443242));
#213793=CARTESIAN_POINT('Ctrl Pts',(-54.5861671393374,-31.2470554817643,
2.69059266624676));
#213794=CARTESIAN_POINT('Ctrl Pts',(-54.5862889570921,-31.2507796687841,
2.68746219342653));
#213795=CARTESIAN_POINT('Ctrl Pts',(-54.5869668451991,-31.2715039227755,
2.67004182396178));
#213796=CARTESIAN_POINT('Ctrl Pts',(-54.5852738987621,-31.294070303669,
2.6544356787807));
#213797=CARTESIAN_POINT('Ctrl Pts',(-54.5811905703973,-31.3175919772474,
2.64136852353312));
#213798=CARTESIAN_POINT('Ctrl Pts',(-54.5793579160794,-31.3281488300881,
2.63550380329813));
#213799=CARTESIAN_POINT('Ctrl Pts',(-54.5770440083386,-31.3388983725489,
2.63014997451128));
#213800=CARTESIAN_POINT('Ctrl Pts',(-54.5742478788456,-31.3497625287429,
2.6253698111923));
#213801=CARTESIAN_POINT('Ctrl Pts',(-54.5730327187885,-31.3544839440759,
2.6232924168705));
#213802=CARTESIAN_POINT('Ctrl Pts',(-54.5717264106366,-31.3592268152914,
2.62132362131404));
#213803=CARTESIAN_POINT('Ctrl Pts',(-54.5703288332444,-31.3639846100471,
2.61946873372324));
#213804=CARTESIAN_POINT('Ctrl Pts',(-54.5654373123717,-31.3806368916921,
2.61297662715544));
#213805=CARTESIAN_POINT('Ctrl Pts',(-54.5594277405088,-31.3974719850964,
2.60787989113946));
#213806=CARTESIAN_POINT('Ctrl Pts',(-54.5522949389283,-31.4142098249418,
2.60440616886156));
#213807=CARTESIAN_POINT('Ctrl Pts',(-54.548728538138,-31.4225787448646,
2.60266930772261));
#213808=CARTESIAN_POINT('Ctrl Pts',(-54.5448813304461,-31.4309233516995,
2.60133820040161));
#213809=CARTESIAN_POINT('Ctrl Pts',(-54.5407526753744,-31.4392086412365,
2.60044130723561));
#213810=CARTESIAN_POINT('Ctrl Pts',(-54.5386883478386,-31.443351286005,
2.59999286065261));
#213811=CARTESIAN_POINT('Ctrl Pts',(-54.5365536585645,-31.4474791015107,
2.59965296768489));
#213812=CARTESIAN_POINT('Ctrl Pts',(-54.5343485280974,-31.4515877125784,
2.59942518630931));
#213813=CARTESIAN_POINT('Ctrl Pts',(-54.5321433976302,-31.4556963236462,
2.59919740493373));
#213814=CARTESIAN_POINT('Ctrl Pts',(-54.5298678244922,-31.4597857294232,
2.59908173791588));
#213815=CARTESIAN_POINT('Ctrl Pts',(-54.5275217339717,-31.4638515574743,
2.59908173516001));
#213816=CARTESIAN_POINT('',(-54.5122556166608,-31.490293248291,2.59908173516001));
#213817=CARTESIAN_POINT('Origin',(9.49066947580418E-17,1.91185189452508E-13,
2.59908173516023));
#213818=CARTESIAN_POINT('',(-54.1966007261205,-31.6576696180587,2.90134173516001));
#213819=CARTESIAN_POINT('Ctrl Pts',(-54.5122556166608,-31.490293248291,
2.59908173516001));
#213820=CARTESIAN_POINT('Ctrl Pts',(-54.5103440004408,-31.4936024004374,
2.5990817438166));
#213821=CARTESIAN_POINT('Ctrl Pts',(-54.5083962906202,-31.4968786114295,
2.59915752000972));
#213822=CARTESIAN_POINT('Ctrl Pts',(-54.5064144237353,-31.5001207716287,
2.59930729517447));
#213823=CARTESIAN_POINT('Ctrl Pts',(-54.4949616780389,-31.5188564579415,
2.60017281085899));
#213824=CARTESIAN_POINT('Ctrl Pts',(-54.4823684499318,-31.5364583843209,
2.6035065180008));
#213825=CARTESIAN_POINT('Ctrl Pts',(-54.4690111814076,-31.552705908786,
2.60896880596544));
#213826=CARTESIAN_POINT('Ctrl Pts',(-54.4636238877434,-31.5592589091581,
2.61117187235515));
#213827=CARTESIAN_POINT('Ctrl Pts',(-54.4581123526894,-31.5655920544896,
2.61372076577221));
#213828=CARTESIAN_POINT('Ctrl Pts',(-54.4525012314182,-31.5716927188401,
2.61659179896959));
#213829=CARTESIAN_POINT('Ctrl Pts',(-54.4504310683343,-31.5739434935989,
2.61765103591185));
#213830=CARTESIAN_POINT('Ctrl Pts',(-54.4483473527931,-31.5761624901353,
2.61875422455126));
#213831=CARTESIAN_POINT('Ctrl Pts',(-54.4462513257023,-31.578349008491,
2.61990022440373));
#213832=CARTESIAN_POINT('Ctrl Pts',(-54.4423212749071,-31.5824487304078,
2.6220489741271));
#213833=CARTESIAN_POINT('Ctrl Pts',(-54.4383479413152,-31.5864342712173,
2.62434823201746));
#213834=CARTESIAN_POINT('Ctrl Pts',(-54.4343395048292,-31.5903010169872,
2.62679048030282));
#213835=CARTESIAN_POINT('Ctrl Pts',(-54.4203099771281,-31.6038346271821,
2.63533834930155));
#213836=CARTESIAN_POINT('Ctrl Pts',(-54.4058504350955,-31.6159129958989,
2.64563784783538));
#213837=CARTESIAN_POINT('Ctrl Pts',(-54.3913116139983,-31.6263383134319,
2.6573666673794));
#213838=CARTESIAN_POINT('Ctrl Pts',(-54.3840422034498,-31.6315509721985,
2.6632310771514));
#213839=CARTESIAN_POINT('Ctrl Pts',(-54.3767529740101,-31.6363503686739,
2.66945281780751));
#213840=CARTESIAN_POINT('Ctrl Pts',(-54.36948777526,-31.6407117811307,2.67599160631178));
#213841=CARTESIAN_POINT('Ctrl Pts',(-54.365855175885,-31.6428924873591,
2.67926100056391));
#213842=CARTESIAN_POINT('Ctrl Pts',(-54.3622285842836,-31.6449636976424,
2.682609656851));
#213843=CARTESIAN_POINT('Ctrl Pts',(-54.3586134821114,-31.6469223220355,
2.68603254012459));
#213844=CARTESIAN_POINT('Ctrl Pts',(-54.3549983799392,-31.6488809464287,
2.68945542339819));
#213845=CARTESIAN_POINT('Ctrl Pts',(-54.3513947831118,-31.6507268563402,
2.69295261525361));
#213846=CARTESIAN_POINT('Ctrl Pts',(-54.3478081421435,-31.6524572252918,
2.69651891172075));
#213847=CARTESIAN_POINT('Ctrl Pts',(-54.3477775556076,-31.652471981715,
2.69654932476063));
#213848=CARTESIAN_POINT('Ctrl Pts',(-54.3477469704398,-31.6524867297707,
2.69657974261121));
#213849=CARTESIAN_POINT('Ctrl Pts',(-54.3477163866429,-31.6525014694577,
2.69661016526948));
#213850=CARTESIAN_POINT('Ctrl Pts',(-54.3320967950441,-31.6600292427987,
2.71214746101382));
#213851=CARTESIAN_POINT('Ctrl Pts',(-54.3168578829657,-31.66550431528,2.72880565568142));
#213852=CARTESIAN_POINT('Ctrl Pts',(-54.3021370826299,-31.6690725678695,
2.7462804001324));
#213853=CARTESIAN_POINT('Ctrl Pts',(-54.2869184346017,-31.672761496392,
2.76434612883701));
#213854=CARTESIAN_POINT('Ctrl Pts',(-54.272252659669,-31.6744122539947,
2.78328592656142));
#213855=CARTESIAN_POINT('Ctrl Pts',(-54.2583037507884,-31.6741352403914,
2.80278753269951));
#213856=CARTESIAN_POINT('Ctrl Pts',(-54.2446201795064,-31.6738634961698,
2.82191817725287));
#213857=CARTESIAN_POINT('Ctrl Pts',(-54.2316257183374,-31.67173606578,2.84159092318038));
#213858=CARTESIAN_POINT('Ctrl Pts',(-54.2194985998668,-31.6678154208116,
2.86151233820282));
#213859=CARTESIAN_POINT('Ctrl Pts',(-54.2114648090419,-31.6652181309731,
2.87470957723501));
#213860=CARTESIAN_POINT('Ctrl Pts',(-54.2038121508368,-31.6618330358498,
2.88801594389429));
#213861=CARTESIAN_POINT('Ctrl Pts',(-54.1966007261205,-31.6576696180587,
2.90134173516001));
#213862=CARTESIAN_POINT('',(-53.8880358395968,-31.4795232016792,3.47153072139049));
#213863=CARTESIAN_POINT('',(-54.1966007261205,-31.6576696180587,2.90134173516001));
#213864=CARTESIAN_POINT('',(-50.6762142289945,-36.4252947698681,3.47153072139046));
#213865=CARTESIAN_POINT('Origin',(5.53234440788222E-15,1.85015204418142E-13,
3.47153072139072));
#213866=CARTESIAN_POINT('',(-50.964463724589,-36.6347241449657,2.90134173515997));
#213867=CARTESIAN_POINT('',(-50.6762142289945,-36.4252947698681,3.47153072139045));
#213868=CARTESIAN_POINT('',(-50.9399462128199,-36.991167339171,2.59908173515996));
#213869=CARTESIAN_POINT('Ctrl Pts',(-50.964463724589,-36.6347241449657,
2.90134173515997));
#213870=CARTESIAN_POINT('Ctrl Pts',(-50.9744193574531,-36.6419574987894,
2.88164837656707));
#213871=CARTESIAN_POINT('Ctrl Pts',(-50.9831959997518,-36.6507449107779,
2.86203734439136));
#213872=CARTESIAN_POINT('Ctrl Pts',(-50.9907013072118,-36.6609215604517,
2.84277945978155));
#213873=CARTESIAN_POINT('Ctrl Pts',(-50.9983574255554,-36.6713026986872,
2.82313460920043));
#213874=CARTESIAN_POINT('Ctrl Pts',(-51.0046913806529,-36.6831299757302,
2.80385576863384));
#213875=CARTESIAN_POINT('Ctrl Pts',(-51.0095813473138,-36.6962763075836,
2.78521678518451));
#213876=CARTESIAN_POINT('Ctrl Pts',(-51.0142813432029,-36.708911916362,
2.76730190934553));
#213877=CARTESIAN_POINT('Ctrl Pts',(-51.0176477981085,-36.7227668523506,
2.74997687279883));
#213878=CARTESIAN_POINT('Ctrl Pts',(-51.0195423439502,-36.7377619899081,
2.73349253345843));
#213879=CARTESIAN_POINT('Ctrl Pts',(-51.0209976683239,-36.7492807342396,
2.72082983599352));
#213880=CARTESIAN_POINT('Ctrl Pts',(-51.0215839370837,-36.7614730081809,
2.70866321039295));
#213881=CARTESIAN_POINT('Ctrl Pts',(-51.0212231059802,-36.7743133764174,
2.69711645335817));
#213882=CARTESIAN_POINT('Ctrl Pts',(-51.0212221603062,-36.7743470287326,
2.69708619136723));
#213883=CARTESIAN_POINT('Ctrl Pts',(-51.0212212075181,-36.7743806860745,
2.6970559338719));
#213884=CARTESIAN_POINT('Ctrl Pts',(-51.0212202476158,-36.77441434844,2.69702568087542));
#213885=CARTESIAN_POINT('Ctrl Pts',(-51.0211173265637,-36.7780236385692,
2.69378194443237));
#213886=CARTESIAN_POINT('Ctrl Pts',(-51.0209317131552,-36.7816890091481,
2.69059266624672));
#213887=CARTESIAN_POINT('Ctrl Pts',(-51.0206635800334,-36.7854055281044,
2.68746219342649));
#213888=CARTESIAN_POINT('Ctrl Pts',(-51.0191714801761,-36.8060871110696,
2.67004182395884));
#213889=CARTESIAN_POINT('Ctrl Pts',(-51.0151289787594,-36.8283529098819,
2.65443567877545));
#213890=CARTESIAN_POINT('Ctrl Pts',(-51.0086093349001,-36.8513189052364,
2.64136852352653));
#213891=CARTESIAN_POINT('Ctrl Pts',(-51.0056832284506,-36.8616263619894,
2.6355038032941));
#213892=CARTESIAN_POINT('Ctrl Pts',(-51.0022583633854,-36.8720751481077,
2.63014997450945));
#213893=CARTESIAN_POINT('Ctrl Pts',(-50.9983419378322,-36.8825875141944,
2.62536981119224));
#213894=CARTESIAN_POINT('Ctrl Pts',(-50.9966399122598,-36.8871560463068,
2.62329241687044));
#213895=CARTESIAN_POINT('Ctrl Pts',(-50.994844995161,-36.8917363891939,
2.62132362131399));
#213896=CARTESIAN_POINT('Ctrl Pts',(-50.9929577488696,-36.896322033635,
2.61946873372319));
#213897=CARTESIAN_POINT('Ctrl Pts',(-50.9863523868497,-36.9123717891789,
2.61297662715539));
#213898=CARTESIAN_POINT('Ctrl Pts',(-50.9786159896078,-36.9284864868683,
2.6078798911394));
#213899=CARTESIAN_POINT('Ctrl Pts',(-50.9697726815832,-36.9443870542878,
2.60440616886151));
#213900=CARTESIAN_POINT('Ctrl Pts',(-50.9653510275709,-36.9523373379975,
2.60266930772256));
#213901=CARTESIAN_POINT('Ctrl Pts',(-50.9606526463563,-36.9602340894951,
2.60133820040158));
#213902=CARTESIAN_POINT('Ctrl Pts',(-50.955680559906,-36.9680424293792,
2.60044130723558));
#213903=CARTESIAN_POINT('Ctrl Pts',(-50.9531945166809,-36.9719465993212,
2.59999286065257));
#213904=CARTESIAN_POINT('Ctrl Pts',(-50.9506400472466,-36.9758286664323,
2.59965296768485));
#213905=CARTESIAN_POINT('Ctrl Pts',(-50.9480175299138,-36.9796842711996,
2.59942518630927));
#213906=CARTESIAN_POINT('Ctrl Pts',(-50.9453950125809,-36.983539875967,
2.59919740493369));
#213907=CARTESIAN_POINT('Ctrl Pts',(-50.9427044459691,-36.9873690173881,
2.59908173791591));
#213908=CARTESIAN_POINT('Ctrl Pts',(-50.9399462128199,-36.991167339171,
2.59908173515997));
#213909=CARTESIAN_POINT('',(-50.9219998155897,-37.0158684358562,2.59908173515996));
#213910=CARTESIAN_POINT('Origin',(8.60468667414046E-17,1.91198832391256E-13,
2.59908173516023));
#213911=CARTESIAN_POINT('',(-50.5905785208481,-37.1493329797263,2.90134173515997));
#213912=CARTESIAN_POINT('Ctrl Pts',(-50.9219998155897,-37.0158684358562,
2.59908173515997));
#213913=CARTESIAN_POINT('Ctrl Pts',(-50.9197527708147,-37.0189596418151,
2.59908174381654));
#213914=CARTESIAN_POINT('Ctrl Pts',(-50.917473273452,-37.0220143142661,
2.59915752000969));
#213915=CARTESIAN_POINT('Ctrl Pts',(-50.915163365418,-37.0250315520726,
2.59930729517444));
#213916=CARTESIAN_POINT('Ctrl Pts',(-50.9018149465594,-37.0424674644314,
2.60017281085915));
#213917=CARTESIAN_POINT('Ctrl Pts',(-50.8874508031551,-37.0586566148381,
2.60350651800223));
#213918=CARTESIAN_POINT('Ctrl Pts',(-50.8724683783777,-37.0734189189144,
2.608968805969));
#213919=CARTESIAN_POINT('Ctrl Pts',(-50.8664256218163,-37.0793728957335,
2.61117187235788));
#213920=CARTESIAN_POINT('Ctrl Pts',(-50.8602822855821,-37.0850952351395,
2.61372076577374));
#213921=CARTESIAN_POINT('Ctrl Pts',(-50.8540642095543,-37.0905759575257,
2.61659179896957));
#213922=CARTESIAN_POINT('Ctrl Pts',(-50.8517701170137,-37.092598011339,
2.61765103591182));
#213923=CARTESIAN_POINT('Ctrl Pts',(-50.8494658679863,-37.0945870443968,
2.61875422455122));
#213924=CARTESIAN_POINT('Ctrl Pts',(-50.8471527697476,-37.0965424902854,
2.61990022440369));
#213925=CARTESIAN_POINT('Ctrl Pts',(-50.84281571055,-37.1002089513264,2.62204897412706));
#213926=CARTESIAN_POINT('Ctrl Pts',(-50.8384475408392,-37.1037573324719,
2.62434823201744));
#213927=CARTESIAN_POINT('Ctrl Pts',(-50.8340568779945,-37.107183900098,
2.62679048030279));
#213928=CARTESIAN_POINT('Ctrl Pts',(-50.818689558038,-37.1191768867891,
2.63533834930153));
#213929=CARTESIAN_POINT('Ctrl Pts',(-50.8030466935687,-37.1296776552301,
2.64563784783535));
#213930=CARTESIAN_POINT('Ctrl Pts',(-50.787497775234,-37.1385261411559,
2.65736666737937));
#213931=CARTESIAN_POINT('Ctrl Pts',(-50.7797233160666,-37.1429503841188,
2.66323107715137));
#213932=CARTESIAN_POINT('Ctrl Pts',(-50.7719723442504,-37.1469615570464,
2.66945281780747));
#213933=CARTESIAN_POINT('Ctrl Pts',(-50.7642910532774,-37.1505396571688,
2.67599160631173));
#213934=CARTESIAN_POINT('Ctrl Pts',(-50.760450407791,-37.1523287072299,
2.67926100056387));
#213935=CARTESIAN_POINT('Ctrl Pts',(-50.7566271826098,-37.1540094891596,
2.68260965685095));
#213936=CARTESIAN_POINT('Ctrl Pts',(-50.7528271523476,-37.1555795029287,
2.68603254012454));
#213937=CARTESIAN_POINT('Ctrl Pts',(-50.7490271220855,-37.1571495166979,
2.68945542339814));
#213938=CARTESIAN_POINT('Ctrl Pts',(-50.7452503160122,-37.1586086360832,
2.69295261525356));
#213939=CARTESIAN_POINT('Ctrl Pts',(-50.7415024502309,-37.159954619824,
2.69651891172071));
#213940=CARTESIAN_POINT('Ctrl Pts',(-50.7414704887851,-37.1599660982464,
2.69654932476058));
#213941=CARTESIAN_POINT('Ctrl Pts',(-50.7414385295744,-37.15997756849,2.69657974261116));
#213942=CARTESIAN_POINT('Ctrl Pts',(-50.7414065726019,-37.1599890305542,
2.69661016526944));
#213943=CARTESIAN_POINT('Ctrl Pts',(-50.7250856801847,-37.1658428740571,
2.7121474610103));
#213944=CARTESIAN_POINT('Ctrl Pts',(-50.7093579475518,-37.1696950534567,
2.72880565567393));
#213945=CARTESIAN_POINT('Ctrl Pts',(-50.6943448053438,-37.1717050161482,
2.74628040012063));
#213946=CARTESIAN_POINT('Ctrl Pts',(-50.6788239286353,-37.1737829544433,
2.76434612882107));
#213947=CARTESIAN_POINT('Ctrl Pts',(-50.6640659431993,-37.1738916781079,
2.78328592654099));
#213948=CARTESIAN_POINT('Ctrl Pts',(-50.6502224037094,-37.1721581240065,
2.80278753267449));
#213949=CARTESIAN_POINT('Ctrl Pts',(-50.6366421974703,-37.1704575457519,
2.82191817722402));
#213950=CARTESIAN_POINT('Ctrl Pts',(-50.6239412983497,-37.1669834785938,
2.84159092314762));
#213951=CARTESIAN_POINT('Ctrl Pts',(-50.6122904324973,-37.1618166822743,
2.86151233816625));
#213952=CARTESIAN_POINT('Ctrl Pts',(-50.6045721423266,-37.1583938608503,
2.87470957721041));
#213953=CARTESIAN_POINT('Ctrl Pts',(-50.5973152449679,-37.1542273890271,
2.88801594388195));
#213954=CARTESIAN_POINT('Ctrl Pts',(-50.5905785208481,-37.1493329797263,
2.90134173515997));
#213955=CARTESIAN_POINT('',(-50.3023253561992,-36.9399086546488,3.47153072139045));
#213956=CARTESIAN_POINT('',(-50.5905785208481,-37.1493329797263,2.90134173515997));
#213957=CARTESIAN_POINT('',(-46.5911245387426,-41.5228599914565,3.47153072139042));
#213958=CARTESIAN_POINT('Origin',(5.53234440788222E-15,1.85015204418142E-13,
3.47153072139072));
#213959=CARTESIAN_POINT('',(-46.8559036426981,-41.7612723673365,2.90134173515993));
#213960=CARTESIAN_POINT('',(-46.5911245387426,-41.5228599914565,3.47153072139042));
#213961=CARTESIAN_POINT('',(-46.7942619810913,-42.1132001506003,2.59908173515993));
#213962=CARTESIAN_POINT('Ctrl Pts',(-46.8559036426982,-41.7612723673365,
2.90134173515993));
#213963=CARTESIAN_POINT('Ctrl Pts',(-46.865048646205,-41.7695067430963,
2.88164837656519));
#213964=CARTESIAN_POINT('Ctrl Pts',(-46.872858674468,-41.7791634256558,
2.86203734438765));
#213965=CARTESIAN_POINT('Ctrl Pts',(-46.8792591175172,-41.7900688448343,
2.84277945977611));
#213966=CARTESIAN_POINT('Ctrl Pts',(-46.8857881704169,-41.8011933963946,
2.82313460919348));
#213967=CARTESIAN_POINT('Ctrl Pts',(-46.8908511403517,-41.8136179609704,
2.80385576862546));
#213968=CARTESIAN_POINT('Ctrl Pts',(-46.8943401533973,-41.8272034165444,
2.78521678517485));
#213969=CARTESIAN_POINT('Ctrl Pts',(-46.8976936214487,-41.8402610894845,
2.76730190933515));
#213970=CARTESIAN_POINT('Ctrl Pts',(-46.8995933993942,-41.854392017043,
2.74997687278782));
#213971=CARTESIAN_POINT('Ctrl Pts',(-46.8999101480295,-41.8695030436346,
2.73349253344695));
#213972=CARTESIAN_POINT('Ctrl Pts',(-46.9001534633396,-41.8811108098966,
2.72082983598615));
#213973=CARTESIAN_POINT('Ctrl Pts',(-46.8994620807989,-41.8932975750545,
2.70866321038944));
#213974=CARTESIAN_POINT('Ctrl Pts',(-46.8977610424069,-41.9060298852857,
2.69711645335814));
#213975=CARTESIAN_POINT('Ctrl Pts',(-46.8977565842887,-41.9060632544001,
2.6970861913672));
#213976=CARTESIAN_POINT('Ctrl Pts',(-46.8977521185698,-41.9060966277702,
2.69705593387187));
#213977=CARTESIAN_POINT('Ctrl Pts',(-46.8977476452506,-41.9061300053925,
2.69702568087538));
#213978=CARTESIAN_POINT('Ctrl Pts',(-46.8972680144601,-41.9097087652733,
2.69378194443234));
#213979=CARTESIAN_POINT('Ctrl Pts',(-46.8967002823073,-41.9133346546844,
2.69059266624669));
#213980=CARTESIAN_POINT('Ctrl Pts',(-46.8960451360316,-41.9170027866178,
2.68746219342646));
#213981=CARTESIAN_POINT('Ctrl Pts',(-46.8923993959683,-41.9374151068017,
2.67004182395936));
#213982=CARTESIAN_POINT('Ctrl Pts',(-46.8860516300644,-41.959136374777,
2.65443567877639));
#213983=CARTESIAN_POINT('Ctrl Pts',(-46.8771671012949,-41.9812950716515,
2.64136852352772));
#213984=CARTESIAN_POINT('Ctrl Pts',(-46.8731796017479,-41.9912402016681,
2.6355038032948));
#213985=CARTESIAN_POINT('Ctrl Pts',(-46.8686813028956,-42.0012737523613,
2.63014997450974));
#213986=CARTESIAN_POINT('Ctrl Pts',(-46.8636874904586,-42.0113191526628,
2.6253698111922));
#213987=CARTESIAN_POINT('Ctrl Pts',(-46.8615172471193,-42.0156847477607,
2.6232924168704));
#213988=CARTESIAN_POINT('Ctrl Pts',(-46.859253386561,-42.0200523791242,
2.62132362131394));
#213989=CARTESIAN_POINT('Ctrl Pts',(-46.8568971484357,-42.0244156319706,
2.61946873372314));
#213990=CARTESIAN_POINT('Ctrl Pts',(-46.8486503149973,-42.0396870169331,
2.61297662715535));
#213991=CARTESIAN_POINT('Ctrl Pts',(-46.8392718539635,-42.0549047629075,
2.60787989113938));
#213992=CARTESIAN_POINT('Ctrl Pts',(-46.8288149286281,-42.0697938479569,
2.60440616886149));
#213993=CARTESIAN_POINT('Ctrl Pts',(-46.8235864659604,-42.0772383904816,
2.60266930772254));
#213994=CARTESIAN_POINT('Ctrl Pts',(-46.8180883876707,-42.0846007681801,
2.60133820040154));
#213995=CARTESIAN_POINT('Ctrl Pts',(-46.8123273450616,-42.0918466086054,
2.60044130723554));
#213996=CARTESIAN_POINT('Ctrl Pts',(-46.809446823757,-42.095469528818,2.59999286065254));
#213997=CARTESIAN_POINT('Ctrl Pts',(-46.8065005614641,-42.0990633147948,
2.59965296768481));
#213998=CARTESIAN_POINT('Ctrl Pts',(-46.8034893901143,-42.1026236704492,
2.59942518630923));
#213999=CARTESIAN_POINT('Ctrl Pts',(-46.8004782187645,-42.1061840261035,
2.59919740493365));
#214000=CARTESIAN_POINT('Ctrl Pts',(-46.7974021370897,-42.109710950294,
2.59908173791585));
#214001=CARTESIAN_POINT('Ctrl Pts',(-46.7942619810913,-42.1132001506003,
2.59908173515993));
#214002=CARTESIAN_POINT('',(-46.7738319284254,-42.1358900227697,2.59908173515994));
#214003=CARTESIAN_POINT('Origin',(7.58094983678529E-17,1.91211474488351E-13,
2.59908173516023));
#214004=CARTESIAN_POINT('',(-46.4302753505421,-42.2339804752703,2.90134173515993));
#214005=CARTESIAN_POINT('Ctrl Pts',(-46.7738319284254,-42.1358900227697,
2.59908173515993));
#214006=CARTESIAN_POINT('Ctrl Pts',(-46.7712740741883,-42.1387294146417,
2.5990817438165));
#214007=CARTESIAN_POINT('Ctrl Pts',(-46.7686877639335,-42.141529080921,
2.59915752000965));
#214008=CARTESIAN_POINT('Ctrl Pts',(-46.7660751225862,-42.1442883388461,
2.5993072951744));
#214009=CARTESIAN_POINT('Ctrl Pts',(-46.7509772786436,-42.1602334457366,
2.6001728108588));
#214010=CARTESIAN_POINT('Ctrl Pts',(-46.7349995965123,-42.1748324484425,
2.60350651799981));
#214011=CARTESIAN_POINT('Ctrl Pts',(-46.7185561660722,-42.1879477932309,
2.60896880596313));
#214012=CARTESIAN_POINT('Ctrl Pts',(-46.7119241523106,-42.1932375134898,
2.61117187235334));
#214013=CARTESIAN_POINT('Ctrl Pts',(-46.7052163225648,-42.1982863518306,
2.61372076577116));
#214014=CARTESIAN_POINT('Ctrl Pts',(-46.6984594183135,-42.2030870843186,
2.61659179896952));
#214015=CARTESIAN_POINT('Ctrl Pts',(-46.6959665308741,-42.2048582631417,
2.61765103591177));
#214016=CARTESIAN_POINT('Ctrl Pts',(-46.6934669941951,-42.2065955404585,
2.61875422455118));
#214017=CARTESIAN_POINT('Ctrl Pts',(-46.6909621675968,-42.2082984896056,
2.61990022440364));
#214018=CARTESIAN_POINT('Ctrl Pts',(-46.6862656177251,-42.2114915192564,
2.62204897412702));
#214019=CARTESIAN_POINT('Ctrl Pts',(-46.6815504704767,-42.2145638639315,
2.62434823201738));
#214020=CARTESIAN_POINT('Ctrl Pts',(-46.6768256862942,-42.2175127112217,
2.62679048030273));
#214021=CARTESIAN_POINT('Ctrl Pts',(-46.6602889416556,-42.2278336767374,
2.63533834930146));
#214022=CARTESIAN_POINT('Ctrl Pts',(-46.6436341412463,-42.2366417962861,
2.64563784783531));
#214023=CARTESIAN_POINT('Ctrl Pts',(-46.6272454828771,-42.2438165047411,
2.65736666737932));
#214024=CARTESIAN_POINT('Ctrl Pts',(-46.6190511536924,-42.2474038589686,
2.66323107715133));
#214025=CARTESIAN_POINT('Ctrl Pts',(-46.6109233607687,-42.2505828610985,
2.66945281780743));
#214026=CARTESIAN_POINT('Ctrl Pts',(-46.6029101354043,-42.2533384464727,
2.6759916063117));
#214027=CARTESIAN_POINT('Ctrl Pts',(-46.598903522722,-42.2547162391598,
2.67926100056383));
#214028=CARTESIAN_POINT('Ctrl Pts',(-46.5949255520162,-42.2559881777373,
2.68260965685092));
#214029=CARTESIAN_POINT('Ctrl Pts',(-46.5909822275908,-42.257152379483,
2.68603254012451));
#214030=CARTESIAN_POINT('Ctrl Pts',(-46.5870389031655,-42.2583165812288,
2.68945542339811));
#214031=CARTESIAN_POINT('Ctrl Pts',(-46.5831302673239,-42.2593729236706,
2.69295261525354));
#214032=CARTESIAN_POINT('Ctrl Pts',(-46.5792622391316,-42.2603197753209,
2.69651891172068));
#214033=CARTESIAN_POINT('Ctrl Pts',(-46.579229252952,-42.2603278499825,
2.69654932476056));
#214034=CARTESIAN_POINT('Ctrl Pts',(-46.5791962698503,-42.2603359167438,
2.69657974261114));
#214035=CARTESIAN_POINT('Ctrl Pts',(-46.5791632898295,-42.2603439756043,
2.69661016526942));
#214036=CARTESIAN_POINT('Ctrl Pts',(-46.5623199117004,-42.2644597533371,
2.71214746101271));
#214037=CARTESIAN_POINT('Ctrl Pts',(-46.5462756748372,-42.2666468343722,
2.7288056556791));
#214038=CARTESIAN_POINT('Ctrl Pts',(-46.5311346778796,-42.2670764855936,
2.74628040012878));
#214039=CARTESIAN_POINT('Ctrl Pts',(-46.515481622459,-42.2675206673339,
2.7643461288319));
#214040=CARTESIAN_POINT('Ctrl Pts',(-46.5007931180922,-42.2660861658594,
2.7832859265547));
#214041=CARTESIAN_POINT('Ctrl Pts',(-46.4872066207052,-42.2629150644383,
2.80278753269116));
#214042=CARTESIAN_POINT('Ctrl Pts',(-46.4738785670876,-42.259804284039,
2.82191817724294));
#214043=CARTESIAN_POINT('Ctrl Pts',(-46.4616103837222,-42.2550216427155,
2.84159092316883));
#214044=CARTESIAN_POINT('Ctrl Pts',(-46.4505634198111,-42.2486653035416,
2.86151233818969));
#214045=CARTESIAN_POINT('Ctrl Pts',(-46.44324519351,-42.2444544516826,2.87470957722616));
#214046=CARTESIAN_POINT('Ctrl Pts',(-46.4364635650958,-42.2395522519014,
2.88801594388982));
#214047=CARTESIAN_POINT('Ctrl Pts',(-46.4302753505421,-42.2339804752703,
2.90134173515993));
#214048=CARTESIAN_POINT('',(-46.1654920697608,-41.9955727382253,3.47153072139041));
#214049=CARTESIAN_POINT('',(-46.4302753505421,-42.2339804752703,2.90134173515993));
#214050=CARTESIAN_POINT('',(-41.9955727382247,-46.1654920697614,3.47153072139039));
#214051=CARTESIAN_POINT('Origin',(5.53234440788222E-15,1.85015204418142E-13,
3.47153072139072));
#214052=CARTESIAN_POINT('',(-42.2339804752697,-46.4302753505427,2.90134173515991));
#214053=CARTESIAN_POINT('',(-41.9955727382247,-46.1654920697614,3.47153072139039));
#214054=CARTESIAN_POINT('',(-42.1358900227691,-46.7738319284259,2.5990817351599));
#214055=CARTESIAN_POINT('Ctrl Pts',(-42.2339804752697,-46.4302753505427,
2.90134173515991));
#214056=CARTESIAN_POINT('Ctrl Pts',(-42.2422146548454,-46.4394205306916,
2.88164837656848));
#214057=CARTESIAN_POINT('Ctrl Pts',(-42.2489725007676,-46.4498406831839,
2.86203734439424));
#214058=CARTESIAN_POINT('Ctrl Pts',(-42.2541979548117,-46.4613553898089,
2.84277945978583));
#214059=CARTESIAN_POINT('Ctrl Pts',(-42.2595284085971,-46.4731014717758,
2.82313460920593));
#214060=CARTESIAN_POINT('Ctrl Pts',(-42.2632649224112,-46.4859871977515,
2.80385576864049));
#214061=CARTESIAN_POINT('Ctrl Pts',(-42.2653147554849,-46.4998629319478,
2.7852167851922));
#214062=CARTESIAN_POINT('Ctrl Pts',(-42.2672849544019,-46.5131996064496,
2.76730190935379));
#214063=CARTESIAN_POINT('Ctrl Pts',(-42.2676972410237,-46.5274517041758,
2.74997687280757));
#214064=CARTESIAN_POINT('Ctrl Pts',(-42.2664327220902,-46.5425130602287,
2.73349253346754));
#214065=CARTESIAN_POINT('Ctrl Pts',(-42.2654613625248,-46.5540826713139,
2.72082983599933));
#214066=CARTESIAN_POINT('Ctrl Pts',(-42.2634999036152,-46.566130406949,
2.70866321039567));
#214067=CARTESIAN_POINT('Ctrl Pts',(-42.2604772948656,-46.5786151613302,
2.69711645335811));
#214068=CARTESIAN_POINT('Ctrl Pts',(-42.2604693731471,-46.5786478816449,
2.69708619136717));
#214069=CARTESIAN_POINT('Ctrl Pts',(-42.2604614434249,-46.5786806053974,
2.69705593387185));
#214070=CARTESIAN_POINT('Ctrl Pts',(-42.2604535056994,-46.5787133325845,
2.69702568087537));
#214071=CARTESIAN_POINT('Ctrl Pts',(-42.2596024201058,-46.5822223525748,
2.69378194443233));
#214072=CARTESIAN_POINT('Ctrl Pts',(-42.2586587894011,-46.5857690348147,
2.69059266624667));
#214073=CARTESIAN_POINT('Ctrl Pts',(-42.2576238078912,-46.5893485909042,
2.68746219342644));
#214074=CARTESIAN_POINT('Ctrl Pts',(-42.2518643711134,-46.609268006654,
2.67004182396122));
#214075=CARTESIAN_POINT('Ctrl Pts',(-42.2432808881748,-46.630206761033,
2.65443567877976));
#214076=CARTESIAN_POINT('Ctrl Pts',(-42.232128815253,-46.6513153841061,
2.64136852353196));
#214077=CARTESIAN_POINT('Ctrl Pts',(-42.2271236104872,-46.6607892264622,
2.63550380329738));
#214078=CARTESIAN_POINT('Ctrl Pts',(-42.2216011621503,-46.6702976120509,
2.63014997451088));
#214079=CARTESIAN_POINT('Ctrl Pts',(-42.2155846760825,-46.6797659870608,
2.62536981119219));
#214080=CARTESIAN_POINT('Ctrl Pts',(-42.2129699926165,-46.6838808147709,
2.62329241687039));
#214081=CARTESIAN_POINT('Ctrl Pts',(-42.2102619919286,-46.6879878819275,
2.62132362131393));
#214082=CARTESIAN_POINT('Ctrl Pts',(-42.2074625774075,-46.692080938468,
2.61946873372313));
#214083=CARTESIAN_POINT('Ctrl Pts',(-42.1976646265834,-46.7064066363596,
2.61297662715533));
#214084=CARTESIAN_POINT('Ctrl Pts',(-42.1867468541393,-46.7205607018097,
2.60787989113935));
#214085=CARTESIAN_POINT('Ctrl Pts',(-42.1747908797553,-46.7342751765575,
2.60440616886145));
#214086=CARTESIAN_POINT('Ctrl Pts',(-42.1688128925633,-46.7411324139314,
2.6026693077225));
#214087=CARTESIAN_POINT('Ctrl Pts',(-42.1625753552951,-46.74787975408,2.60133820040151));
#214088=CARTESIAN_POINT('Ctrl Pts',(-42.1560884757153,-46.7544837081025,
2.6004413072355));
#214089=CARTESIAN_POINT('Ctrl Pts',(-42.1528450359255,-46.7577856851137,
2.5999928606525));
#214090=CARTESIAN_POINT('Ctrl Pts',(-42.1495392606402,-46.7610518156851,
2.59965296768478));
#214091=CARTESIAN_POINT('Ctrl Pts',(-42.1461724262969,-46.7642779142248,
2.5994251863092));
#214092=CARTESIAN_POINT('Ctrl Pts',(-42.1428055919536,-46.7675040127645,
2.59919740493363));
#214093=CARTESIAN_POINT('Ctrl Pts',(-42.1393776974104,-46.770690078005,
2.59908173791579));
#214094=CARTESIAN_POINT('Ctrl Pts',(-42.1358900227691,-46.7738319284259,
2.5990817351599));
#214095=CARTESIAN_POINT('',(-42.1132001505997,-46.7942619810918,2.5990817351599));
#214096=CARTESIAN_POINT('Origin',(6.43067523875891E-17,1.91222977234332E-13,
2.59908173516023));
#214097=CARTESIAN_POINT('',(-41.7612723673359,-46.8559036426987,2.9013417351599));
#214098=CARTESIAN_POINT('Ctrl Pts',(-42.1132001505997,-46.7942619810919,
2.5990817351599));
#214099=CARTESIAN_POINT('Ctrl Pts',(-42.1103595112868,-46.7968184499054,
2.59908174381644));
#214100=CARTESIAN_POINT('Ctrl Pts',(-42.1074947242963,-46.7993324362835,
2.59915752000963));
#214101=CARTESIAN_POINT('Ctrl Pts',(-42.104607974281,-46.8018034833198,
2.59930729517438));
#214102=CARTESIAN_POINT('Ctrl Pts',(-42.0879261203875,-46.8160830868203,
2.60017281085878));
#214103=CARTESIAN_POINT('Ctrl Pts',(-42.0705099543527,-46.828931992102,
2.60350651799972));
#214104=CARTESIAN_POINT('Ctrl Pts',(-42.0527856759093,-46.8402566831445,
2.60896880596294));
#214105=CARTESIAN_POINT('Ctrl Pts',(-42.0456370666831,-46.8448241915556,
2.61117187235319));
#214106=CARTESIAN_POINT('Ctrl Pts',(-42.0384382358172,-46.8491442126966,
2.61372076577107));
#214107=CARTESIAN_POINT('Ctrl Pts',(-42.0312165334047,-46.8532123574521,
2.61659179896951));
#214108=CARTESIAN_POINT('Ctrl Pts',(-42.028552163663,-46.8547132558791,
2.61765103591176));
#214109=CARTESIAN_POINT('Ctrl Pts',(-42.0258847247792,-46.8561797434811,
2.61875422455116));
#214110=CARTESIAN_POINT('Ctrl Pts',(-42.0232156132257,-46.8576115380195,
2.61990022440363));
#214111=CARTESIAN_POINT('Ctrl Pts',(-42.0182110290631,-46.860296152779,
2.622048974127));
#214112=CARTESIAN_POINT('Ctrl Pts',(-42.0132005644171,-46.8628587997326,
2.62434823201736));
#214113=CARTESIAN_POINT('Ctrl Pts',(-42.0081934246211,-46.8652976184989,
2.62679048030272));
#214114=CARTESIAN_POINT('Ctrl Pts',(-41.9906684353351,-46.873833484181,
2.63533834930145));
#214115=CARTESIAN_POINT('Ctrl Pts',(-41.9731841724644,-46.8808524512364,
2.6456378478353));
#214116=CARTESIAN_POINT('Ctrl Pts',(-41.9561353316313,-46.8862747746135,
2.65736666737931));
#214117=CARTESIAN_POINT('Ctrl Pts',(-41.9476109112147,-46.888985936302,
2.66323107715131));
#214118=CARTESIAN_POINT('Ctrl Pts',(-41.9391953469837,-46.8912979378215,
2.6694528178074));
#214119=CARTESIAN_POINT('Ctrl Pts',(-41.9309379818016,-46.8932008176775,
2.67599160631167));
#214120=CARTESIAN_POINT('Ctrl Pts',(-41.9268092992106,-46.8941522576055,
2.6792610005638));
#214121=CARTESIAN_POINT('Ctrl Pts',(-41.9227201664597,-46.8950014172056,
2.68260965685089));
#214122=CARTESIAN_POINT('Ctrl Pts',(-41.9186767517587,-46.89574705169,2.68603254012449));
#214123=CARTESIAN_POINT('Ctrl Pts',(-41.9146333370577,-46.8964926861745,
2.68945542339808));
#214124=CARTESIAN_POINT('Ctrl Pts',(-41.9106356952802,-46.8971346781638,
2.69295261525351));
#214125=CARTESIAN_POINT('Ctrl Pts',(-41.9066898836031,-46.8976720238189,
2.69651891172065));
#214126=CARTESIAN_POINT('Ctrl Pts',(-41.9066562340933,-46.897676606252,
2.69654932476053));
#214127=CARTESIAN_POINT('Ctrl Pts',(-41.9066225884702,-46.8976811811498,
2.69657974261112));
#214128=CARTESIAN_POINT('Ctrl Pts',(-41.9065889467371,-46.8976857485121,
2.6966101652694));
#214129=CARTESIAN_POINT('Ctrl Pts',(-41.8894076224763,-46.9000183671516,
2.71214746101077));
#214130=CARTESIAN_POINT('Ctrl Pts',(-41.8732226654037,-46.9005163877043,
2.72880565567496));
#214131=CARTESIAN_POINT('Ctrl Pts',(-41.8581197016315,-46.8993610201075,
2.74628040012227));
#214132=CARTESIAN_POINT('Ctrl Pts',(-41.8425059656531,-46.8981665787458,
2.76434612882316));
#214133=CARTESIAN_POINT('Ctrl Pts',(-41.8280478726861,-46.8952045688321,
2.7832859265436));
#214134=CARTESIAN_POINT('Ctrl Pts',(-41.8148672739126,-46.8906306633446,
2.80278753267762));
#214135=CARTESIAN_POINT('Ctrl Pts',(-41.8019373978624,-46.8861437631639,
2.82191817722768));
#214136=CARTESIAN_POINT('Ctrl Pts',(-41.7902363430373,-46.8801049472969,
2.84159092315182));
#214137=CARTESIAN_POINT('Ctrl Pts',(-41.7799143139161,-46.8726287066543,
2.86151233817099));
#214138=CARTESIAN_POINT('Ctrl Pts',(-41.7730763314944,-46.8676759593315,
2.87470957721359));
#214139=CARTESIAN_POINT('Ctrl Pts',(-41.7668442729565,-46.8620917411148,
2.88801594388352));
#214140=CARTESIAN_POINT('Ctrl Pts',(-41.7612723673359,-46.8559036426987,
2.90134173515991));
#214141=CARTESIAN_POINT('',(-41.5228599914559,-46.5911245387432,3.47153072139039));
#214142=CARTESIAN_POINT('',(-41.7612723673359,-46.8559036426987,2.9013417351599));
#214143=CARTESIAN_POINT('',(-36.9399086546482,-50.3023253561997,3.47153072139036));
#214144=CARTESIAN_POINT('Origin',(5.53234440788222E-15,1.85015204418142E-13,
3.47153072139072));
#214145=CARTESIAN_POINT('',(-37.1493329797256,-50.5905785208485,2.90134173515987));
#214146=CARTESIAN_POINT('',(-36.9399086546482,-50.3023253561997,3.47153072139036));
#214147=CARTESIAN_POINT('',(-37.0158684358555,-50.9219998155901,2.59908173515987));
#214148=CARTESIAN_POINT('Ctrl Pts',(-37.1493329797256,-50.5905785208486,
2.90134173515987));
#214149=CARTESIAN_POINT('Ctrl Pts',(-37.156566119977,-50.6005343088816,
2.88164837656766));
#214150=CARTESIAN_POINT('Ctrl Pts',(-37.1621977431852,-50.611603765938,
2.86203734439262));
#214151=CARTESIAN_POINT('Ctrl Pts',(-37.1661909570569,-50.623601602477,
2.84277945978346));
#214152=CARTESIAN_POINT('Ctrl Pts',(-37.1702644101613,-50.6358405223211,
2.82313460920288));
#214153=CARTESIAN_POINT('Ctrl Pts',(-37.1726335298273,-50.6490462309891,
2.8038557686368));
#214154=CARTESIAN_POINT('Ctrl Pts',(-37.1732217245285,-50.6630602183634,
2.78521678518795));
#214155=CARTESIAN_POINT('Ctrl Pts',(-37.1737870683987,-50.6765297750326,
2.76730190934898));
#214156=CARTESIAN_POINT('Ctrl Pts',(-37.1727073465972,-50.6907468939638,
2.74997687280227));
#214157=CARTESIAN_POINT('Ctrl Pts',(-37.1698754144273,-50.7055935641122,
2.73349253346184));
#214158=CARTESIAN_POINT('Ctrl Pts',(-37.167700022404,-50.716998260933,2.72082983599567));
#214159=CARTESIAN_POINT('Ctrl Pts',(-37.16448997728,-50.7287749695245,2.70866321039392));
#214160=CARTESIAN_POINT('Ctrl Pts',(-37.1601789145083,-50.7408753824654,
2.69711645335808));
#214161=CARTESIAN_POINT('Ctrl Pts',(-37.1601676159816,-50.7409070954897,
2.69708619136714));
#214162=CARTESIAN_POINT('Ctrl Pts',(-37.1601563091356,-50.7409388110964,
2.69705593387181));
#214163=CARTESIAN_POINT('Ctrl Pts',(-37.1601449939712,-50.7409705292823,
2.69702568087533));
#214164=CARTESIAN_POINT('Ctrl Pts',(-37.1589317782465,-50.7443713638247,
2.69378194443228));
#214165=CARTESIAN_POINT('Ctrl Pts',(-37.1576225876053,-50.7477999807008,
2.69059266624662));
#214166=CARTESIAN_POINT('Ctrl Pts',(-37.1562191103351,-50.7512517425807,
2.68746219342639));
#214167=CARTESIAN_POINT('Ctrl Pts',(-37.1484090784387,-50.7704600126073,
2.67004182396466));
#214168=CARTESIAN_POINT('Ctrl Pts',(-37.1376839209025,-50.7903868440138,
2.65443567878596));
#214169=CARTESIAN_POINT('Ctrl Pts',(-37.1243864882752,-50.8102141227924,
2.64136852353976));
#214170=CARTESIAN_POINT('Ctrl Pts',(-37.1184184163599,-50.8191128800903,
2.63550380330212));
#214171=CARTESIAN_POINT('Ctrl Pts',(-37.1119323236364,-50.8279919247136,
2.63014997451299));
#214172=CARTESIAN_POINT('Ctrl Pts',(-37.1049590818163,-50.8367795369355,
2.62536981119217));
#214173=CARTESIAN_POINT('Ctrl Pts',(-37.1019286052427,-50.8405985143442,
2.62329241687037));
#214174=CARTESIAN_POINT('Ctrl Pts',(-37.0988061338475,-50.8444000194069,
2.62132362131391));
#214175=CARTESIAN_POINT('Ctrl Pts',(-37.0955942139018,-50.8481780352574,
2.61946873372311));
#214176=CARTESIAN_POINT('Ctrl Pts',(-37.0843524940917,-50.8614010907342,
2.61297662715531));
#214177=CARTESIAN_POINT('Ctrl Pts',(-37.0720150276369,-50.8743364007569,
2.60787989113933));
#214178=CARTESIAN_POINT('Ctrl Pts',(-37.0586909963616,-50.8867260065479,
2.60440616886143));
#214179=CARTESIAN_POINT('Ctrl Pts',(-37.052028980724,-50.8929208094433,
2.60266930772248));
#214180=CARTESIAN_POINT('Ctrl Pts',(-37.0451203242406,-50.8989791867714,
2.60133820040147));
#214181=CARTESIAN_POINT('Ctrl Pts',(-37.0379786793005,-50.9048689000889,
2.60044130723546));
#214182=CARTESIAN_POINT('Ctrl Pts',(-37.0344078568305,-50.9078137567477,
2.59999286065246));
#214183=CARTESIAN_POINT('Ctrl Pts',(-37.0307787873186,-50.9107164475035,
2.59965296768475));
#214184=CARTESIAN_POINT('Ctrl Pts',(-37.0270931777235,-50.9135729431179,
2.59942518630917));
#214185=CARTESIAN_POINT('Ctrl Pts',(-37.0234075681283,-50.9164294387323,
2.59919740493359));
#214186=CARTESIAN_POINT('Ctrl Pts',(-37.0196654174466,-50.9192397378252,
2.59908173791576));
#214187=CARTESIAN_POINT('Ctrl Pts',(-37.0158684358555,-50.9219998155901,
2.59908173515987));
#214188=CARTESIAN_POINT('',(-36.9911673391703,-50.9399462128203,2.59908173515987));
#214189=CARTESIAN_POINT('Origin',(5.16646552926871E-17,1.91233214602705E-13,
2.59908173516024));
#214190=CARTESIAN_POINT('',(-36.634724144965,-50.9644637245894,2.90134173515987));
#214191=CARTESIAN_POINT('Ctrl Pts',(-36.9911673391703,-50.9399462128203,
2.59908173515988));
#214192=CARTESIAN_POINT('Ctrl Pts',(-36.9880750374203,-50.9421917493681,
2.59908174381648));
#214193=CARTESIAN_POINT('Ctrl Pts',(-36.9849631609,-50.9443925120841,2.5991575200096));
#214194=CARTESIAN_POINT('Ctrl Pts',(-36.9818339300539,-50.9465482749232,
2.59930729517435));
#214195=CARTESIAN_POINT('Ctrl Pts',(-36.9637508360892,-50.9590059247113,
2.60017281085885));
#214196=CARTESIAN_POINT('Ctrl Pts',(-36.945087001308,-50.9699639572751,
2.60350651800055));
#214197=CARTESIAN_POINT('Ctrl Pts',(-36.9262760657623,-50.9793739188877,
2.60896880596501));
#214198=CARTESIAN_POINT('Ctrl Pts',(-36.9186891827326,-50.9831691728715,
2.61117187235478));
#214199=CARTESIAN_POINT('Ctrl Pts',(-36.9110782226468,-50.9867130457558,
2.61372076577195));
#214200=CARTESIAN_POINT('Ctrl Pts',(-36.9034708445584,-50.9900040313322,
2.61659179896946));
#214201=CARTESIAN_POINT('Ctrl Pts',(-36.9006641839069,-50.9912182052059,
2.61765103591171));
#214202=CARTESIAN_POINT('Ctrl Pts',(-36.8978580678369,-50.992397835948,
2.61875422455112));
#214203=CARTESIAN_POINT('Ctrl Pts',(-36.8950539146731,-50.9935427888371,
2.61990022440358));
#214204=CARTESIAN_POINT('Ctrl Pts',(-36.8897961274908,-50.9956895755043,
2.62204897412696));
#214205=CARTESIAN_POINT('Ctrl Pts',(-36.8845452411465,-50.99771444784,2.62434823201732));
#214206=CARTESIAN_POINT('Ctrl Pts',(-36.8793106050084,-50.9996165178737,
2.62679048030267));
#214207=CARTESIAN_POINT('Ctrl Pts',(-36.8609893785248,-51.0062737629917,
2.63533834930141));
#214208=CARTESIAN_POINT('Ctrl Pts',(-36.8428672144356,-51.0114266762819,
2.64563784783525));
#214209=CARTESIAN_POINT('Ctrl Pts',(-36.8253449818064,-51.0150372064714,
2.65736666737927));
#214210=CARTESIAN_POINT('Ctrl Pts',(-36.8165838654919,-51.0168424715661,
2.66323107715127));
#214211=CARTESIAN_POINT('Ctrl Pts',(-36.8079727326363,-51.0182621417028,
2.66945281780736));
#214212=CARTESIAN_POINT('Ctrl Pts',(-36.7995616970576,-51.0192914676907,
2.67599160631163));
#214213=CARTESIAN_POINT('Ctrl Pts',(-36.7953561792682,-51.0198061306847,
2.67926100056377));
#214214=CARTESIAN_POINT('Ctrl Pts',(-36.7912006858663,-51.020223207737,
2.68260965685085));
#214215=CARTESIAN_POINT('Ctrl Pts',(-36.7871014813873,-51.0205421056327,
2.68603254012445));
#214216=CARTESIAN_POINT('Ctrl Pts',(-36.7830022769083,-51.0208610035284,
2.68945542339804));
#214217=CARTESIAN_POINT('Ctrl Pts',(-36.7789594281946,-51.0210816112668,
2.69295261525347));
#214218=CARTESIAN_POINT('Ctrl Pts',(-36.7749790641711,-51.0212035636552,
2.69651891172061));
#214219=CARTESIAN_POINT('Ctrl Pts',(-36.7749451200022,-51.0212046036537,
2.69654932476049));
#214220=CARTESIAN_POINT('Ctrl Pts',(-36.7749111804864,-51.0212056365644,
2.69657974261108));
#214221=CARTESIAN_POINT('Ctrl Pts',(-36.7748772456268,-51.0212066623876,
2.69661016526935));
#214222=CARTESIAN_POINT('Ctrl Pts',(-36.7575462174152,-51.0217305652762,
2.71214746101165));
#214223=CARTESIAN_POINT('Ctrl Pts',(-36.7413978659069,-51.0205340689294,
2.7288056556769));
#214224=CARTESIAN_POINT('Ctrl Pts',(-36.726498406549,-51.0178063409629,
2.74628040012535));
#214225=CARTESIAN_POINT('Ctrl Pts',(-36.7110950573694,-51.014986363048,
2.76434612882721));
#214226=CARTESIAN_POINT('Ctrl Pts',(-36.6970257816923,-51.0105292970946,
2.78328592654866));
#214227=CARTESIAN_POINT('Ctrl Pts',(-36.6843954909294,-51.0046027002046,
2.80278753268373));
#214228=CARTESIAN_POINT('Ctrl Pts',(-36.6720054548738,-50.9987888396584,
2.82191817723423));
#214229=CARTESIAN_POINT('Ctrl Pts',(-36.6609997277939,-50.9915600117767,
2.84159092315881));
#214230=CARTESIAN_POINT('Ctrl Pts',(-36.651515723774,-50.9830457809201,
2.86151233817839));
#214231=CARTESIAN_POINT('Ctrl Pts',(-36.6452329036036,-50.9774054014718,
2.87470957721854));
#214232=CARTESIAN_POINT('Ctrl Pts',(-36.6396186946846,-50.9712003466859,
2.88801594388598));
#214233=CARTESIAN_POINT('Ctrl Pts',(-36.634724144965,-50.9644637245894,
2.90134173515987));
#214234=CARTESIAN_POINT('',(-36.4252947698674,-50.6762142289949,3.47153072139035));
#214235=CARTESIAN_POINT('',(-36.634724144965,-50.9644637245894,2.90134173515987));
#214236=CARTESIAN_POINT('',(-31.4795232016785,-53.8880358395971,3.47153072139033));
#214237=CARTESIAN_POINT('Origin',(5.53234440788222E-15,1.85015204418142E-13,
3.47153072139072));
#214238=CARTESIAN_POINT('',(-31.6576696180579,-54.1966007261208,2.90134173515985));
#214239=CARTESIAN_POINT('',(-31.4795232016785,-53.8880358395971,3.47153072139033));
#214240=CARTESIAN_POINT('',(-31.4902932482903,-54.5122556166612,2.59908173515985));
#214241=CARTESIAN_POINT('Ctrl Pts',(-31.6576696180579,-54.1966007261208,
2.90134173515985));
#214242=CARTESIAN_POINT('Ctrl Pts',(-31.663822471187,-54.207258044342,2.8816483765649));
#214243=CARTESIAN_POINT('Ctrl Pts',(-31.668266170439,-54.2188555266759,
2.86203734438717));
#214244=CARTESIAN_POINT('Ctrl Pts',(-31.6709833936512,-54.2312050423224,
2.84277945977544));
#214245=CARTESIAN_POINT('Ctrl Pts',(-31.6737552164698,-54.2438027078782,
2.82313460919239));
#214246=CARTESIAN_POINT('Ctrl Pts',(-31.6747309854165,-54.2571837147324,
2.80385576862396));
#214247=CARTESIAN_POINT('Ctrl Pts',(-31.67385109736,-54.2711824151079,2.78521678517299));
#214248=CARTESIAN_POINT('Ctrl Pts',(-31.6730053921568,-54.2846372786638,
2.76730190933255));
#214249=CARTESIAN_POINT('Ctrl Pts',(-31.6704454915891,-54.2986636530711,
2.74997687278455));
#214250=CARTESIAN_POINT('Ctrl Pts',(-31.6660771734229,-54.3131329740909,
2.73349253344308));
#214251=CARTESIAN_POINT('Ctrl Pts',(-31.6627215829926,-54.3242478043988,
2.72082983598364));
#214252=CARTESIAN_POINT('Ctrl Pts',(-31.658298121582,-54.335624457859,2.7086632103882));
#214253=CARTESIAN_POINT('Ctrl Pts',(-31.6527458376963,-54.3472079546995,
2.69711645335805));
#214254=CARTESIAN_POINT('Ctrl Pts',(-31.6527312861504,-54.3472383129789,
2.69708619136711));
#214255=CARTESIAN_POINT('Ctrl Pts',(-31.6527167260609,-54.3472686729569,
2.69705593387179));
#214256=CARTESIAN_POINT('Ctrl Pts',(-31.6527021574289,-54.3472990346305,
2.69702568087531));
#214257=CARTESIAN_POINT('Ctrl Pts',(-31.6511401038183,-54.3505544234701,
2.69378194443226));
#214258=CARTESIAN_POINT('Ctrl Pts',(-31.6494796970072,-54.3538274103384,
2.6905926662466));
#214259=CARTESIAN_POINT('Ctrl Pts',(-31.6477231007675,-54.3571135597833,
2.68746219342637));
#214260=CARTESIAN_POINT('Ctrl Pts',(-31.6379480420931,-54.3754002342685,
2.67004182396106));
#214261=CARTESIAN_POINT('Ctrl Pts',(-31.6251987170241,-54.3940968201759,
2.65443567877953));
#214262=CARTESIAN_POINT('Ctrl Pts',(-31.6099016141384,-54.4124255228524,
2.64136852353169));
#214263=CARTESIAN_POINT('Ctrl Pts',(-31.6030360625228,-54.4206516984369,
2.6355038032972));
#214264=CARTESIAN_POINT('Ctrl Pts',(-31.5956573884073,-54.428804121416,
2.63014997451078));
#214265=CARTESIAN_POINT('Ctrl Pts',(-31.5878037911378,-54.4368146919236,
2.62536981119215));
#214266=CARTESIAN_POINT('Ctrl Pts',(-31.5843907239922,-54.4402959775153,
2.62329241687035));
#214267=CARTESIAN_POINT('Ctrl Pts',(-31.5808879923396,-54.4437502703989,
2.62132362131389));
#214268=CARTESIAN_POINT('Ctrl Pts',(-31.5772987574364,-54.4471718528272,
2.61946873372309));
#214269=CARTESIAN_POINT('Ctrl Pts',(-31.5647364352749,-54.4591473913263,
2.61297662715529));
#214270=CARTESIAN_POINT('Ctrl Pts',(-31.5511144466737,-54.4707222239581,
2.6078798911393));
#214271=CARTESIAN_POINT('Ctrl Pts',(-31.5365683393821,-54.4816512176785,
2.6044061688614));
#214272=CARTESIAN_POINT('Ctrl Pts',(-31.5292952857363,-54.4871157145387,
2.60266930772245));
#214273=CARTESIAN_POINT('Ctrl Pts',(-31.521791202724,-54.4924187521964,
2.60133820040144));
#214274=CARTESIAN_POINT('Ctrl Pts',(-31.51407303778,-54.4975296958773,2.60044130723544));
#214275=CARTESIAN_POINT('Ctrl Pts',(-31.5102139553079,-54.5000851677178,
2.59999286065244));
#214276=CARTESIAN_POINT('Ctrl Pts',(-31.5063013524145,-54.5025926161708,
2.59965296768472));
#214277=CARTESIAN_POINT('Ctrl Pts',(-31.5023373478775,-54.5050482124961,
2.59942518630914));
#214278=CARTESIAN_POINT('Ctrl Pts',(-31.4983733433404,-54.5075038088215,
2.59919740493356));
#214279=CARTESIAN_POINT('Ctrl Pts',(-31.4943579363061,-54.5099075515418,
2.59908173791574));
#214280=CARTESIAN_POINT('Ctrl Pts',(-31.4902932482903,-54.5122556166612,
2.59908173515985));
#214281=CARTESIAN_POINT('',(-31.4638515574735,-54.527521733972,2.59908173515985));
#214282=CARTESIAN_POINT('Origin',(3.80217165444466E-17,1.91242074430722E-13,
2.59908173516022));
#214283=CARTESIAN_POINT('',(-31.106798218553,-54.5146464769139,2.90134173515985));
#214284=CARTESIAN_POINT('Ctrl Pts',(-31.4638515574735,-54.527521733972,
2.59908173515985));
#214285=CARTESIAN_POINT('Ctrl Pts',(-31.4605414731915,-54.5294317356858,
2.59908174381641));
#214286=CARTESIAN_POINT('Ctrl Pts',(-31.4572166015116,-54.5312951627228,
2.59915752000956));
#214287=CARTESIAN_POINT('Ctrl Pts',(-31.4538791743428,-54.533112022376,
2.59930729517431));
#214288=CARTESIAN_POINT('Ctrl Pts',(-31.4345929624711,-54.5436112298315,
2.60017281085879));
#214289=CARTESIAN_POINT('Ctrl Pts',(-31.4148859438259,-54.5525583311778,
2.60350651800034));
#214290=CARTESIAN_POINT('Ctrl Pts',(-31.3951944477271,-54.5599504658508,
2.60896880596455));
#214291=CARTESIAN_POINT('Ctrl Pts',(-31.3872524143693,-54.5629318838124,
2.61117187235442));
#214292=CARTESIAN_POINT('Ctrl Pts',(-31.3793127123321,-54.5656607810286,
2.61372076577173));
#214293=CARTESIAN_POINT('Ctrl Pts',(-31.3714030065914,-54.5681385507008,
2.61659179896942));
#214294=CARTESIAN_POINT('Ctrl Pts',(-31.3684848053914,-54.5690526972782,
2.61765103591167));
#214295=CARTESIAN_POINT('Ctrl Pts',(-31.3655707565302,-54.569932546879,
2.61875422455108));
#214296=CARTESIAN_POINT('Ctrl Pts',(-31.3626622846448,-54.5707781137755,
2.61990022440354));
#214297=CARTESIAN_POINT('Ctrl Pts',(-31.3572088998595,-54.5723635517063,
2.62204897412691));
#214298=CARTESIAN_POINT('Ctrl Pts',(-31.3517751216265,-54.5738284644992,
2.62434823201728));
#214299=CARTESIAN_POINT('Ctrl Pts',(-31.3463703409152,-54.5751729463229,
2.62679048030263));
#214300=CARTESIAN_POINT('Ctrl Pts',(-31.3274536084255,-54.579878632706,
2.63533834930137));
#214301=CARTESIAN_POINT('Ctrl Pts',(-31.3088920933397,-54.5831090358348,
2.64563784783522));
#214302=CARTESIAN_POINT('Ctrl Pts',(-31.291088446162,-54.5848682151123,
2.65736666737923));
#214303=CARTESIAN_POINT('Ctrl Pts',(-31.2821866225732,-54.5857478047511,
2.66323107715124));
#214304=CARTESIAN_POINT('Ctrl Pts',(-31.2734742664667,-54.5862595893019,
2.66945281780732));
#214305=CARTESIAN_POINT('Ctrl Pts',(-31.2650017135572,-54.5864040839108,
2.67599160631159));
#214306=CARTESIAN_POINT('Ctrl Pts',(-31.2607654371024,-54.5864763312153,
2.67926100056373));
#214307=CARTESIAN_POINT('Ctrl Pts',(-31.2565891115048,-54.5864567561365,
2.68260965685083));
#214308=CARTESIAN_POINT('Ctrl Pts',(-31.2524790289898,-54.5863454235313,
2.68603254012442));
#214309=CARTESIAN_POINT('Ctrl Pts',(-31.2483689464749,-54.5862340909261,
2.68945542339802));
#214310=CARTESIAN_POINT('Ctrl Pts',(-31.2443251851216,-54.5860308973889,
2.69295261525344));
#214311=CARTESIAN_POINT('Ctrl Pts',(-31.240353878453,-54.5857361203748,
2.69651891172058));
#214312=CARTESIAN_POINT('Ctrl Pts',(-31.2403200115243,-54.5857336065442,
2.69654932476046));
#214313=CARTESIAN_POINT('Ctrl Pts',(-31.2402861499641,-54.5857310861512,
2.69657974261105));
#214314=CARTESIAN_POINT('Ctrl Pts',(-31.2402522937756,-54.5857285591961,
2.69661016526932));
#214315=CARTESIAN_POINT('Ctrl Pts',(-31.2229614439844,-54.584438006344,
2.71214746101312));
#214316=CARTESIAN_POINT('Ctrl Pts',(-31.2070266227583,-54.5815601021613,
2.72880565568009));
#214317=CARTESIAN_POINT('Ctrl Pts',(-31.1924939094092,-54.5772898993832,
2.74628040013039));
#214318=CARTESIAN_POINT('Ctrl Pts',(-31.1774697093447,-54.5728752811827,
2.76434612883432));
#214319=CARTESIAN_POINT('Ctrl Pts',(-31.1639433968857,-54.566971991736,
2.783285926558));
#214320=CARTESIAN_POINT('Ctrl Pts',(-31.1520017942418,-54.5597576364785,
2.80278753269533));
#214321=CARTESIAN_POINT('Ctrl Pts',(-31.1402873460082,-54.5526805134387,
2.82191817724808));
#214322=CARTESIAN_POINT('Ctrl Pts',(-31.1300975277222,-54.5443408740922,
2.84159092317495));
#214323=CARTESIAN_POINT('Ctrl Pts',(-31.1215554575361,-54.5348819367156,
2.86151233819678));
#214324=CARTESIAN_POINT('Ctrl Pts',(-31.1158966355112,-54.5286157223212,
2.8747095772309));
#214325=CARTESIAN_POINT('Ctrl Pts',(-31.1109617866599,-54.5218578148468,
2.88801594389215));
#214326=CARTESIAN_POINT('Ctrl Pts',(-31.106798218553,-54.5146464769139,
2.90134173515985));
#214327=CARTESIAN_POINT('',(-30.9286463962973,-54.2060847114743,3.47153072139033));
#214328=CARTESIAN_POINT('',(-31.106798218553,-54.5146464769139,2.90134173515985));
#214329=CARTESIAN_POINT('',(-25.6742415049975,-56.8833377255395,3.47153072139031));
#214330=CARTESIAN_POINT('Origin',(5.53234440788222E-15,1.85015204418142E-13,
3.47153072139072));
#214331=CARTESIAN_POINT('',(-25.8191582032616,-57.2088336324699,2.90134173515983));
#214332=CARTESIAN_POINT('',(-25.6742415049975,-56.8833377255395,3.47153072139031));
#214333=CARTESIAN_POINT('',(-25.6197038181293,-57.5052637377732,2.59908173515982));
#214334=CARTESIAN_POINT('Ctrl Pts',(-25.8191582032616,-57.2088336324699,
2.90134173515983));
#214335=CARTESIAN_POINT('Ctrl Pts',(-25.8241633573204,-57.2200757170667,
2.88164837656895));
#214336=CARTESIAN_POINT('Ctrl Pts',(-25.8273704465166,-57.2320741602303,
2.86203734439522));
#214337=CARTESIAN_POINT('Ctrl Pts',(-25.8287819086035,-57.2446400511018,
2.84277945978731));
#214338=CARTESIAN_POINT('Ctrl Pts',(-25.8302217324659,-57.2574584397044,
2.8231346092081));
#214339=CARTESIAN_POINT('Ctrl Pts',(-25.8297934599659,-57.2708681396284,
2.80385576864333));
#214340=CARTESIAN_POINT('Ctrl Pts',(-25.8274551293922,-57.284698180309,
2.78521678519563));
#214341=CARTESIAN_POINT('Ctrl Pts',(-25.8252076408415,-57.2979909364466,
2.76730190935802));
#214342=CARTESIAN_POINT('Ctrl Pts',(-25.8211956083174,-57.3116728904319,
2.74997687281252));
#214343=CARTESIAN_POINT('Ctrl Pts',(-25.8153387643678,-57.3256063334094,
2.7334925334731));
#214344=CARTESIAN_POINT('Ctrl Pts',(-25.8108397400796,-57.336309520811,
2.72082983600286));
#214345=CARTESIAN_POINT('Ctrl Pts',(-25.8052513267465,-57.3471614741582,
2.70866321039731));
#214346=CARTESIAN_POINT('Ctrl Pts',(-25.7985186537236,-57.3581011436974,
2.69711645335804));
#214347=CARTESIAN_POINT('Ctrl Pts',(-25.7985010085883,-57.3581298146203,
2.6970861913671));
#214348=CARTESIAN_POINT('Ctrl Pts',(-25.7984833547786,-57.3581584863394,
2.69705593387177));
#214349=CARTESIAN_POINT('Ctrl Pts',(-25.7984656922961,-57.3581871588519,
2.69702568087529));
#214350=CARTESIAN_POINT('Ctrl Pts',(-25.7965719149858,-57.3612614352674,
2.69378194443225));
#214351=CARTESIAN_POINT('Ctrl Pts',(-25.7945784837693,-57.3643429325988,
2.69059266624658));
#214352=CARTESIAN_POINT('Ctrl Pts',(-25.7924880141961,-57.3674274658676,
2.68746219342635));
#214353=CARTESIAN_POINT('Ctrl Pts',(-25.7808550263337,-57.3845921921749,
2.67004182396113));
#214354=CARTESIAN_POINT('Ctrl Pts',(-25.7662212180083,-57.4018536888712,
2.65443567877967));
#214355=CARTESIAN_POINT('Ctrl Pts',(-25.7490920431284,-57.4184830023395,
2.64136852353187));
#214356=CARTESIAN_POINT('Ctrl Pts',(-25.7414042322304,-57.4259464685137,
2.63550380329729));
#214357=CARTESIAN_POINT('Ctrl Pts',(-25.7332138190178,-57.4332829502006,
2.6301499745108));
#214358=CARTESIAN_POINT('Ctrl Pts',(-25.7245659119506,-57.4404287135112,
2.62536981119211));
#214359=CARTESIAN_POINT('Ctrl Pts',(-25.7208076485109,-57.4435341655923,
2.62329241687031));
#214360=CARTESIAN_POINT('Ctrl Pts',(-25.7169630332621,-57.4466034003412,
2.62132362131385));
#214361=CARTESIAN_POINT('Ctrl Pts',(-25.71303580781,-57.4496310617742,2.61946873372305));
#214362=CARTESIAN_POINT('Ctrl Pts',(-25.6992905187276,-57.4602278767898,
2.61297662715525));
#214363=CARTESIAN_POINT('Ctrl Pts',(-25.6845332533377,-57.4703154157422,
2.60787989113927));
#214364=CARTESIAN_POINT('Ctrl Pts',(-25.6689244402251,-57.4796640570498,
2.60440616886137));
#214365=CARTESIAN_POINT('Ctrl Pts',(-25.6611200336689,-57.4843383777035,
2.60266930772242));
#214366=CARTESIAN_POINT('Ctrl Pts',(-25.6531027404315,-57.4888279745006,
2.60133820040143));
#214367=CARTESIAN_POINT('Ctrl Pts',(-25.6448926173138,-57.4931041519764,
2.60044130723543));
#214368=CARTESIAN_POINT('Ctrl Pts',(-25.6407875557549,-57.4952422407143,
2.59999286065242));
#214369=CARTESIAN_POINT('Ctrl Pts',(-25.636634286776,-57.4973269747345,
2.5996529676847));
#214370=CARTESIAN_POINT('Ctrl Pts',(-25.6324353177602,-57.4993547677436,
2.59942518630912));
#214371=CARTESIAN_POINT('Ctrl Pts',(-25.6282363487445,-57.5013825607527,
2.59919740493354));
#214372=CARTESIAN_POINT('Ctrl Pts',(-25.6239916789975,-57.5033534111922,
2.59908173791572));
#214373=CARTESIAN_POINT('Ctrl Pts',(-25.6197038181293,-57.5052637377732,
2.59908173515983));
#214374=CARTESIAN_POINT('',(-25.5918112338789,-57.5176823163889,2.59908173515983));
#214375=CARTESIAN_POINT('Origin',(2.35274110347535E-17,1.91249459648252E-13,
2.59908173516024));
#214376=CARTESIAN_POINT('',(-25.2380597013425,-57.4675553545141,2.90134173515982));
#214377=CARTESIAN_POINT('Ctrl Pts',(-25.5918112338789,-57.5176823163889,
2.59908173515983));
#214378=CARTESIAN_POINT('Ctrl Pts',(-25.5883196330409,-57.5192358568901,
2.59908174381641));
#214379=CARTESIAN_POINT('Ctrl Pts',(-25.5848181941914,-57.5207415321516,
2.59915752000954));
#214380=CARTESIAN_POINT('Ctrl Pts',(-25.5813091362503,-57.5221995827243,
2.59930729517429));
#214381=CARTESIAN_POINT('Ctrl Pts',(-25.5610311102427,-57.5306253163343,
2.60017281085885));
#214382=CARTESIAN_POINT('Ctrl Pts',(-25.5404968219514,-57.5374634601491,
2.60350651800088));
#214383=CARTESIAN_POINT('Ctrl Pts',(-25.5201405094493,-57.5427567781085,
2.60896880596589));
#214384=CARTESIAN_POINT('Ctrl Pts',(-25.5119303403451,-57.5448916950078,
2.61117187235545));
#214385=CARTESIAN_POINT('Ctrl Pts',(-25.5037488853955,-57.5467757181864,
2.61372076577231));
#214386=CARTESIAN_POINT('Ctrl Pts',(-25.495623512396,-57.5484131249907,
2.61659179896943));
#214387=CARTESIAN_POINT('Ctrl Pts',(-25.4926257430706,-57.5490172286906,
2.61765103591169));
#214388=CARTESIAN_POINT('Ctrl Pts',(-25.4896356883473,-57.5495876573339,
2.61875422455109));
#214389=CARTESIAN_POINT('Ctrl Pts',(-25.4866547635669,-57.5501245740298,
2.61990022440355));
#214390=CARTESIAN_POINT('Ctrl Pts',(-25.4810655296035,-57.5511312928345,
2.62204897412692));
#214391=CARTESIAN_POINT('Ctrl Pts',(-25.4755083930932,-57.5520201961934,
2.62434823201729));
#214392=CARTESIAN_POINT('Ctrl Pts',(-25.4699926837172,-57.552792359383,
2.62679048030264));
#214393=CARTESIAN_POINT('Ctrl Pts',(-25.4506877009012,-57.5554949305466,
2.63533834930138));
#214394=CARTESIAN_POINT('Ctrl Pts',(-25.4318901986623,-57.5567674305411,
2.64563784783521));
#214395=CARTESIAN_POINT('Ctrl Pts',(-25.4140001974202,-57.5566559849705,
2.65736666737922));
#214396=CARTESIAN_POINT('Ctrl Pts',(-25.4050551967991,-57.5566002621852,
2.66323107715123));
#214397=CARTESIAN_POINT('Ctrl Pts',(-25.3963370718384,-57.5561985539314,
2.66945281780733));
#214398=CARTESIAN_POINT('Ctrl Pts',(-25.3878958286608,-57.5554566340481,
2.67599160631159));
#214399=CARTESIAN_POINT('Ctrl Pts',(-25.383675207072,-57.5550856741065,
2.67926100056373));
#214400=CARTESIAN_POINT('Ctrl Pts',(-25.3795238059759,-57.5546296613652,
2.6826096568508));
#214401=CARTESIAN_POINT('Ctrl Pts',(-25.3754478763491,-57.5540893180425,
2.6860325401244));
#214402=CARTESIAN_POINT('Ctrl Pts',(-25.3713719467224,-57.5535489747198,
2.68945542339799));
#214403=CARTESIAN_POINT('Ctrl Pts',(-25.3673715770251,-57.552924206138,
2.69295261525342));
#214404=CARTESIAN_POINT('Ctrl Pts',(-25.3634528381782,-57.5522159293599,
2.69651891172056));
#214405=CARTESIAN_POINT('Ctrl Pts',(-25.363419419543,-57.5522098892424,
2.69654932476044));
#214406=CARTESIAN_POINT('Ctrl Pts',(-25.3633860069328,-57.5522038431595,
2.69657974261102));
#214407=CARTESIAN_POINT('Ctrl Pts',(-25.3633526003507,-57.552197791112,
2.6966101652693));
#214408=CARTESIAN_POINT('Ctrl Pts',(-25.3462913711525,-57.5491069220865,
2.71214746101104));
#214409=CARTESIAN_POINT('Ctrl Pts',(-25.3307446654479,-57.5445791409897,
2.72880565567566));
#214410=CARTESIAN_POINT('Ctrl Pts',(-25.3167379215588,-57.5388132486368,
2.74628040012343));
#214411=CARTESIAN_POINT('Ctrl Pts',(-25.3022574788921,-57.5328523576332,
2.76434612882484));
#214412=CARTESIAN_POINT('Ctrl Pts',(-25.2894223267632,-57.5255675223701,
2.78328592654582));
#214413=CARTESIAN_POINT('Ctrl Pts',(-25.2783002469372,-57.5171444507339,
2.80278753268039));
#214414=CARTESIAN_POINT('Ctrl Pts',(-25.2673897324726,-57.5088816036442,
2.82191817723078));
#214415=CARTESIAN_POINT('Ctrl Pts',(-25.2581274647625,-57.4995225236699,
2.84159092315524));
#214416=CARTESIAN_POINT('Ctrl Pts',(-25.2506209171182,-57.4892225138741,
2.86151233817473));
#214417=CARTESIAN_POINT('Ctrl Pts',(-25.2456480924699,-57.4823991184843,
2.87470957721607));
#214418=CARTESIAN_POINT('Ctrl Pts',(-25.2414466709174,-57.4751623993634,
2.88801594388471));
#214419=CARTESIAN_POINT('Ctrl Pts',(-25.2380597013425,-57.4675553545141,
2.90134173515982));
#214420=CARTESIAN_POINT('',(-25.0931373005741,-57.1420619865022,3.47153072139031));
#214421=CARTESIAN_POINT('',(-25.2380597013425,-57.4675553545141,2.90134173515982));
#214422=CARTESIAN_POINT('',(-19.5876674457072,-59.2554138597571,3.4715307213903));
#214423=CARTESIAN_POINT('Origin',(5.53234440788222E-15,1.85015204418142E-13,
3.47153072139072));
#214424=CARTESIAN_POINT('',(-19.697766688184,-59.5942745858236,2.90134173515981));
#214425=CARTESIAN_POINT('',(-19.5876674457073,-59.2554138597571,3.4715307213903));
#214426=CARTESIAN_POINT('',(-19.4684195516691,-59.8682321556242,2.5990817351598));
#214427=CARTESIAN_POINT('Ctrl Pts',(-19.697766688184,-59.5942745858236,
2.90134173515981));
#214428=CARTESIAN_POINT('Ctrl Pts',(-19.7015693056586,-59.6059782661681,
2.8816483765668));
#214429=CARTESIAN_POINT('Ctrl Pts',(-19.703504647259,-59.6182462127113,
2.86203734439098));
#214430=CARTESIAN_POINT('Ctrl Pts',(-19.7035948839462,-59.6308908042823,
2.84277945978107));
#214431=CARTESIAN_POINT('Ctrl Pts',(-19.7036869338402,-59.6437894749879,
2.82313460919993));
#214432=CARTESIAN_POINT('Ctrl Pts',(-19.701859312135,-59.6570809485079,
2.80385576863333));
#214433=CARTESIAN_POINT('Ctrl Pts',(-19.6980881582805,-59.6705908046785,
2.78521678518401));
#214434=CARTESIAN_POINT('Ctrl Pts',(-19.6944635103345,-59.6835758151839,
2.76730190934502));
#214435=CARTESIAN_POINT('Ctrl Pts',(-19.6890433025185,-59.6967634464007,
2.74997687279832));
#214436=CARTESIAN_POINT('Ctrl Pts',(-19.6817621015886,-59.7100083536232,
2.73349253345792));
#214437=CARTESIAN_POINT('Ctrl Pts',(-19.6761689356963,-59.7201826317453,
2.72082983599314));
#214438=CARTESIAN_POINT('Ctrl Pts',(-19.6694767982717,-59.7303909886947,
2.70866321039269));
#214439=CARTESIAN_POINT('Ctrl Pts',(-19.6616375006935,-59.7405669736107,
2.69711645335803));
#214440=CARTESIAN_POINT('Ctrl Pts',(-19.6616169552926,-59.7405936430524,
2.69708619136709));
#214441=CARTESIAN_POINT('Ctrl Pts',(-19.6615964011816,-59.7406203123792,
2.69705593387176));
#214442=CARTESIAN_POINT('Ctrl Pts',(-19.6615758383624,-59.7406469815885,
2.69702568087528));
#214443=CARTESIAN_POINT('Ctrl Pts',(-19.659371085973,-59.7435064631641,
2.69378194443223));
#214444=CARTESIAN_POINT('Ctrl Pts',(-19.6570664708007,-59.746362709429,
2.69059266624656));
#214445=CARTESIAN_POINT('Ctrl Pts',(-19.654665031516,-59.7492118317299,
2.68746219342633));
#214446=CARTESIAN_POINT('Ctrl Pts',(-19.6413015679163,-59.7650665495245,
2.67004182396276));
#214447=CARTESIAN_POINT('Ctrl Pts',(-19.6249436074025,-59.7807038364384,
2.6544356787826));
#214448=CARTESIAN_POINT('Ctrl Pts',(-19.606170031355,-59.7954515664591,
2.64136852353555));
#214449=CARTESIAN_POINT('Ctrl Pts',(-19.5977441904381,-59.8020705519271,
2.63550380329953));
#214450=CARTESIAN_POINT('Ctrl Pts',(-19.5888317740078,-59.8085107122944,
2.6301499745118));
#214451=CARTESIAN_POINT('Ctrl Pts',(-19.5794843054207,-59.814713377931,
2.6253698111921));
#214452=CARTESIAN_POINT('Ctrl Pts',(-19.5754220220075,-59.8174089725188,
2.6232924168703));
#214453=CARTESIAN_POINT('Ctrl Pts',(-19.5712776455715,-59.8200595219548,
2.62132362131385));
#214454=CARTESIAN_POINT('Ctrl Pts',(-19.5670554570745,-59.8226600907003,
2.61946873372305));
#214455=CARTESIAN_POINT('Ctrl Pts',(-19.5522777973348,-59.8317620813095,
2.61297662715524));
#214456=CARTESIAN_POINT('Ctrl Pts',(-19.5365469388439,-59.8402518053948,
2.60787989113925));
#214457=CARTESIAN_POINT('Ctrl Pts',(-19.5200464333333,-59.847917668619,
2.60440616886135));
#214458=CARTESIAN_POINT('Ctrl Pts',(-19.5117961805779,-59.8517506002311,
2.60266930772241));
#214459=CARTESIAN_POINT('Ctrl Pts',(-19.5033535162579,-59.8553775672055,
2.60133820040141));
#214460=CARTESIAN_POINT('Ctrl Pts',(-19.4947413867934,-59.8587721277809,
2.60044130723541));
#214461=CARTESIAN_POINT('Ctrl Pts',(-19.4904353220612,-59.8604694080687,
2.59999286065241));
#214462=CARTESIAN_POINT('Ctrl Pts',(-19.4860868910809,-59.8621085868739,
2.59965296768468));
#214463=CARTESIAN_POINT('Ctrl Pts',(-19.4816989623697,-59.8636863596422,
2.5994251863091));
#214464=CARTESIAN_POINT('Ctrl Pts',(-19.4773110336585,-59.8652641324105,
2.59919740493352));
#214465=CARTESIAN_POINT('Ctrl Pts',(-19.4728836066887,-59.8667804975192,
2.59908173791576));
#214466=CARTESIAN_POINT('Ctrl Pts',(-19.4684195516691,-59.8682321556242,
2.59908173515981));
#214467=CARTESIAN_POINT('',(-19.4393816709751,-59.8776671349985,2.59908173515981));
#214468=CARTESIAN_POINT('Origin',(8.34054140790793E-18,1.91255289341306E-13,
2.59908173516022));
#214469=CARTESIAN_POINT('',(-19.0928077206406,-59.7908376697911,2.90134173515981));
#214470=CARTESIAN_POINT('Ctrl Pts',(-19.4393816709751,-59.8776671349985,
2.59908173515981));
#214471=CARTESIAN_POINT('Ctrl Pts',(-19.4357468082906,-59.8788471933724,
2.59908174381641));
#214472=CARTESIAN_POINT('Ctrl Pts',(-19.4321071647682,-59.879978620365,
2.59915752000953));
#214473=CARTESIAN_POINT('Ctrl Pts',(-19.4284649220279,-59.8810618871501,
2.59930729517428));
#214474=CARTESIAN_POINT('Ctrl Pts',(-19.4074172521841,-59.8873218328126,
2.60017281085876));
#214475=CARTESIAN_POINT('Ctrl Pts',(-19.3862806722099,-59.8919760989604,
2.6035065180003));
#214476=CARTESIAN_POINT('Ctrl Pts',(-19.3654825713274,-59.8951126055065,
2.60896880596449));
#214477=CARTESIAN_POINT('Ctrl Pts',(-19.3570942188041,-59.8963776307484,
2.61117187235437));
#214478=CARTESIAN_POINT('Ctrl Pts',(-19.3487606486714,-59.897396138138,
2.61372076577169));
#214479=CARTESIAN_POINT('Ctrl Pts',(-19.3405086316967,-59.8981752423036,
2.6165917989694));
#214480=CARTESIAN_POINT('Ctrl Pts',(-19.3374641384339,-59.8984626844394,
2.61765103591166));
#214481=CARTESIAN_POINT('Ctrl Pts',(-19.3344308375137,-59.8987174423896,
2.61875422455106));
#214482=CARTESIAN_POINT('Ctrl Pts',(-19.331410119474,-59.8989398263132,
2.61990022440352));
#214483=CARTESIAN_POINT('Ctrl Pts',(-19.3257462731495,-59.89935679617,2.62204897412689));
#214484=CARTESIAN_POINT('Ctrl Pts',(-19.3201266635123,-59.8996599510836,
2.62434823201726));
#214485=CARTESIAN_POINT('Ctrl Pts',(-19.3145604567378,-59.8998513356576,
2.62679048030262));
#214486=CARTESIAN_POINT('Ctrl Pts',(-19.295078733027,-59.9005211816664,
2.63533834930135));
#214487=CARTESIAN_POINT('Ctrl Pts',(-19.2762511930033,-59.8998218367505,
2.64563784783519));
#214488=CARTESIAN_POINT('Ctrl Pts',(-19.258470844294,-59.8978409873527,
2.6573666673792));
#214489=CARTESIAN_POINT('Ctrl Pts',(-19.2495806699394,-59.8968505626538,
2.66323107715121));
#214490=CARTESIAN_POINT('Ctrl Pts',(-19.2409522937258,-59.8955397627951,
2.66945281780731));
#214491=CARTESIAN_POINT('Ctrl Pts',(-19.2326348443069,-59.8939195570492,
2.67599160631158));
#214492=CARTESIAN_POINT('Ctrl Pts',(-19.2284761195974,-59.8931094541762,
2.67926100056371));
#214493=CARTESIAN_POINT('Ctrl Pts',(-19.2243951266219,-59.8922219999435,
2.6826096568508));
#214494=CARTESIAN_POINT('Ctrl Pts',(-19.2203980066213,-59.8912585660177,
2.68603254012439));
#214495=CARTESIAN_POINT('Ctrl Pts',(-19.2164008866207,-59.890295132092,
2.68945542339799));
#214496=CARTESIAN_POINT('Ctrl Pts',(-19.2124877374669,-59.8892556335609,
2.69295261525341));
#214497=CARTESIAN_POINT('Ctrl Pts',(-19.2086645009646,-59.8881416170476,
2.69651891172055));
#214498=CARTESIAN_POINT('Ctrl Pts',(-19.2086318967643,-59.8881321168198,
2.69654932476043));
#214499=CARTESIAN_POINT('Ctrl Pts',(-19.2085992991797,-59.8881226112892,
2.69657974261101));
#214500=CARTESIAN_POINT('Ctrl Pts',(-19.2085667082136,-59.8881131004567,
2.69661016526929));
#214501=CARTESIAN_POINT('Ctrl Pts',(-19.191922026002,-59.8832557794652,
2.7121474610124));
#214502=CARTESIAN_POINT('Ctrl Pts',(-19.1769337687768,-59.8771277287701,
2.7288056556786));
#214503=CARTESIAN_POINT('Ctrl Pts',(-19.1636064551624,-59.8699293191639,
2.74628040012806));
#214504=CARTESIAN_POINT('Ctrl Pts',(-19.1498284206512,-59.8624874641247,
2.76434612883123));
#214505=CARTESIAN_POINT('Ctrl Pts',(-19.1378250534633,-59.8539008972225,
2.7832859265541));
#214506=CARTESIAN_POINT('Ctrl Pts',(-19.1276443522881,-59.8443613941403,
2.80278753269061));
#214507=CARTESIAN_POINT('Ctrl Pts',(-19.1176573094717,-59.8350033524799,
2.82191817724284));
#214508=CARTESIAN_POINT('Ctrl Pts',(-19.1094240716806,-59.8247273719136,
2.8415909231692));
#214509=CARTESIAN_POINT('Ctrl Pts',(-19.1030352898857,-59.8136991387581,
2.86151233819053));
#214510=CARTESIAN_POINT('Ctrl Pts',(-19.0988029459279,-59.8063933209263,
2.87470957722669));
#214511=CARTESIAN_POINT('Ctrl Pts',(-19.0953809833327,-59.7987570771744,
2.88801594389002));
#214512=CARTESIAN_POINT('Ctrl Pts',(-19.0928077206406,-59.7908376697912,
2.90134173515981));
#214513=CARTESIAN_POINT('',(-18.9827025415091,-59.4519788726608,3.4715307213903));
#214514=CARTESIAN_POINT('',(-19.0928077206406,-59.7908376697911,2.90134173515981));
#214515=CARTESIAN_POINT('',(-13.2864868028989,-60.9782752797347,3.47153072139029));
#214516=CARTESIAN_POINT('Origin',(5.53234440788222E-15,1.85015204418142E-13,
3.47153072139072));
#214517=CARTESIAN_POINT('',(-13.360562319248,-61.3267881959112,2.90134173515981));
#214518=CARTESIAN_POINT('',(-13.2864868028989,-60.9782752797348,3.47153072139029));
#214519=CARTESIAN_POINT('',(-13.1038352065721,-61.5752716937451,2.5990817351598));
#214520=CARTESIAN_POINT('Ctrl Pts',(-13.360562319248,-61.3267881959112,
2.9013417351598));
#214521=CARTESIAN_POINT('Ctrl Pts',(-13.3631207378652,-61.3388252440305,
2.88164837656816));
#214522=CARTESIAN_POINT('Ctrl Pts',(-13.3637631278624,-61.3512282837613,
2.86203734439369));
#214523=CARTESIAN_POINT('Ctrl Pts',(-13.3625311504984,-61.363813039238,
2.84277945978507));
#214524=CARTESIAN_POINT('Ctrl Pts',(-13.3612744179067,-61.376650671509,
2.82313460920513));
#214525=CARTESIAN_POINT('Ctrl Pts',(-13.3580674708034,-61.3896782944572,
2.80385576863965));
#214526=CARTESIAN_POINT('Ctrl Pts',(-13.3529048112206,-61.4027199493042,
2.78521678519133));
#214527=CARTESIAN_POINT('Ctrl Pts',(-13.3479427162824,-61.415254947683,
2.76730190935321));
#214528=CARTESIAN_POINT('Ctrl Pts',(-13.3411737181076,-61.4278037696819,
2.74997687280727));
#214529=CARTESIAN_POINT('Ctrl Pts',(-13.3325479345614,-61.4402150271722,
2.73349253346748));
#214530=CARTESIAN_POINT('Ctrl Pts',(-13.325921906959,-61.4497489245011,
2.72082983599925));
#214531=CARTESIAN_POINT('Ctrl Pts',(-13.3181993658972,-61.4592018401645,
2.70866321039559));
#214532=CARTESIAN_POINT('Ctrl Pts',(-13.3093393327438,-61.4685026502438,
2.69711645335801));
#214533=CARTESIAN_POINT('Ctrl Pts',(-13.309316112177,-61.4685270260083,
2.69708619136707));
#214534=CARTESIAN_POINT('Ctrl Pts',(-13.3092928829598,-61.4685514007481,
2.69705593387175));
#214535=CARTESIAN_POINT('Ctrl Pts',(-13.3092696450943,-61.4685757744608,
2.69702568087527));
#214536=CARTESIAN_POINT('Ctrl Pts',(-13.3067780733544,-61.471189132118,
2.69378194443222));
#214537=CARTESIAN_POINT('Ctrl Pts',(-13.3041875240723,-61.4737888336846,
2.69059266624656));
#214538=CARTESIAN_POINT('Ctrl Pts',(-13.3015014257475,-61.4763713294374,
2.68746219342633));
#214539=CARTESIAN_POINT('Ctrl Pts',(-13.2865538993097,-61.4907423311182,
2.67004182395882));
#214540=CARTESIAN_POINT('Ctrl Pts',(-13.2686510078397,-61.5045840828665,
2.65443567877554));
#214541=CARTESIAN_POINT('Ctrl Pts',(-13.2484387178447,-61.5172886502272,
2.64136852352668));
#214542=CARTESIAN_POINT('Ctrl Pts',(-13.2393671621907,-61.5229906359943,
2.63550380329413));
#214543=CARTESIAN_POINT('Ctrl Pts',(-13.2298303888482,-61.5284639152929,
2.63014997450939));
#214544=CARTESIAN_POINT('Ctrl Pts',(-13.21988577157,-61.5336555255487,2.6253698111921));
#214545=CARTESIAN_POINT('Ctrl Pts',(-13.2155639754105,-61.5359117291448,
2.6232924168703));
#214546=CARTESIAN_POINT('Ctrl Pts',(-13.211165244443,-61.5381145532936,
2.62132362131384));
#214547=CARTESIAN_POINT('Ctrl Pts',(-13.2066943520817,-61.5402595369762,
2.61946873372304));
#214548=CARTESIAN_POINT('Ctrl Pts',(-13.1910462288172,-61.5477669798652,
2.61297662715524));
#214549=CARTESIAN_POINT('Ctrl Pts',(-13.1745141278029,-61.5545658738897,
2.60787989113926));
#214550=CARTESIAN_POINT('Ctrl Pts',(-13.1573027128855,-61.5604649702289,
2.60440616886136));
#214551=CARTESIAN_POINT('Ctrl Pts',(-13.1486970054267,-61.5634145183985,
2.60266930772241));
#214552=CARTESIAN_POINT('Ctrl Pts',(-13.1399214696211,-61.566139117741,
2.60133820040141));
#214553=CARTESIAN_POINT('Ctrl Pts',(-13.1310016901025,-61.5686148699001,
2.6004413072354));
#214554=CARTESIAN_POINT('Ctrl Pts',(-13.1265418003432,-61.5698527459796,
2.5999928606524));
#214555=CARTESIAN_POINT('Ctrl Pts',(-13.1220458496813,-61.5710284103838,
2.59965296768468));
#214556=CARTESIAN_POINT('Ctrl Pts',(-13.1175170363398,-61.5721388765027,
2.5994251863091));
#214557=CARTESIAN_POINT('Ctrl Pts',(-13.1129882229983,-61.5732493426216,
2.59919740493352));
#214558=CARTESIAN_POINT('Ctrl Pts',(-13.1084265466222,-61.5742946087863,
2.59908173791573));
#214559=CARTESIAN_POINT('Ctrl Pts',(-13.1038352065721,-61.5752716937451,
2.5990817351598));
#214560=CARTESIAN_POINT('',(-13.0739701745318,-61.5816197022697,2.5990817351598));
#214561=CARTESIAN_POINT('Origin',(-7.37250181440935E-18,1.91259499638548E-13,
2.59908173516023));
#214562=CARTESIAN_POINT('',(-12.7383709431244,-61.4590390555208,2.9013417351598));
#214563=CARTESIAN_POINT('Ctrl Pts',(-13.0739701745318,-61.5816197022697,
2.59908173515981));
#214564=CARTESIAN_POINT('Ctrl Pts',(-13.0702318743171,-61.5824133495498,
2.59908174381637));
#214565=CARTESIAN_POINT('Ctrl Pts',(-13.0664939028179,-61.5831581321227,
2.59915752000952));
#214566=CARTESIAN_POINT('Ctrl Pts',(-13.0627583804521,-61.5838547466225,
2.59930729517427));
#214567=CARTESIAN_POINT('Ctrl Pts',(-13.0411716694484,-61.587880319063,
2.60017281085864));
#214568=CARTESIAN_POINT('Ctrl Pts',(-13.0196643745854,-61.5902997144304,
2.60350651799945));
#214569=CARTESIAN_POINT('Ctrl Pts',(-12.9986523536689,-61.5912450453415,
2.60896880596243));
#214570=CARTESIAN_POINT('Ctrl Pts',(-12.9901777222712,-61.5916263190445,
2.61117187235278));
#214571=CARTESIAN_POINT('Ctrl Pts',(-12.9817833412928,-61.5917681516646,
2.6137207657708));
#214572=CARTESIAN_POINT('Ctrl Pts',(-12.9734950911667,-61.5916804171628,
2.6165917989694));
#214573=CARTESIAN_POINT('Ctrl Pts',(-12.9704372300718,-61.5916480484583,
2.61765103591165));
#214574=CARTESIAN_POINT('Ctrl Pts',(-12.9673939164345,-61.591584344534,
2.61875422455105));
#214575=CARTESIAN_POINT('Ctrl Pts',(-12.9643665007544,-61.5914897592006,
2.61990022440352));
#214576=CARTESIAN_POINT('Ctrl Pts',(-12.9586900963544,-61.5913124117003,
2.62204897412689));
#214577=CARTESIAN_POINT('Ctrl Pts',(-12.9530695832095,-61.5910264967401,
2.62434823201725));
#214578=CARTESIAN_POINT('Ctrl Pts',(-12.9475138635627,-61.590635005849,
2.6267904803026));
#214579=CARTESIAN_POINT('Ctrl Pts',(-12.9280688447988,-61.58926478773,2.63533834930134));
#214580=CARTESIAN_POINT('Ctrl Pts',(-12.9094175454587,-61.586601260073,
2.64563784783519));
#214581=CARTESIAN_POINT('Ctrl Pts',(-12.8919416545036,-61.5827727094484,
2.6573666673792));
#214582=CARTESIAN_POINT('Ctrl Pts',(-12.8832037090261,-61.5808584341362,
2.66323107715121));
#214583=CARTESIAN_POINT('Ctrl Pts',(-12.8747596158551,-61.5786529040702,
2.66945281780729));
#214584=CARTESIAN_POINT('Ctrl Pts',(-12.8666570879111,-61.5761721637748,
2.67599160631156));
#214585=CARTESIAN_POINT('Ctrl Pts',(-12.8626058239391,-61.5749317936271,
2.6792610005637));
#214586=CARTESIAN_POINT('Ctrl Pts',(-12.8586399512973,-61.5736226210371,
2.68260965685079));
#214587=CARTESIAN_POINT('Ctrl Pts',(-12.854765434206,-61.5722466520921,
2.68603254012439));
#214588=CARTESIAN_POINT('Ctrl Pts',(-12.8508909171147,-61.5708706831471,
2.68945542339798));
#214589=CARTESIAN_POINT('Ctrl Pts',(-12.8471078617854,-61.5694278436301,
2.69295261525342));
#214590=CARTESIAN_POINT('Ctrl Pts',(-12.8434220158069,-61.5679202927795,
2.69651891172056));
#214591=CARTESIAN_POINT('Ctrl Pts',(-12.8433905832601,-61.567907436528,
2.69654932476044));
#214592=CARTESIAN_POINT('Ctrl Pts',(-12.8433591578469,-61.5678945756942,
2.69657974261102));
#214593=CARTESIAN_POINT('Ctrl Pts',(-12.8433277395702,-61.5678817102795,
2.6966101652693));
#214594=CARTESIAN_POINT('Ctrl Pts',(-12.8272819669698,-61.5613111551481,
2.71214746101087));
#214595=CARTESIAN_POINT('Ctrl Pts',(-12.8130163727092,-61.553649975062,
2.72880565567529));
#214596=CARTESIAN_POINT('Ctrl Pts',(-12.8005145062083,-61.5450979154862,
2.74628040012284));
#214597=CARTESIAN_POINT('Ctrl Pts',(-12.7875898348838,-61.5362566309343,
2.76434612882401));
#214598=CARTESIAN_POINT('Ctrl Pts',(-12.7765497640409,-61.5264624086191,
2.78328592654474));
#214599=CARTESIAN_POINT('Ctrl Pts',(-12.7674219834097,-61.5159109908855,
2.80278753267906));
#214600=CARTESIAN_POINT('Ctrl Pts',(-12.7584678323728,-61.5055602833195,
2.82191817722935));
#214601=CARTESIAN_POINT('Ctrl Pts',(-12.7513538295766,-61.4944799879572,
2.84159092315374));
#214602=CARTESIAN_POINT('Ctrl Pts',(-12.7461528104605,-61.4828443590751,
2.86151233817315));
#214603=CARTESIAN_POINT('Ctrl Pts',(-12.7427073176343,-61.4751361628646,
2.874709577215));
#214604=CARTESIAN_POINT('Ctrl Pts',(-12.7401023057313,-61.4671840587602,
2.88801594388417));
#214605=CARTESIAN_POINT('Ctrl Pts',(-12.7383709431244,-61.4590390555208,
2.9013417351598));
#214606=CARTESIAN_POINT('',(-12.6642893210135,-61.1105274371641,3.47153072139029));
#214607=CARTESIAN_POINT('',(-12.7383709431244,-61.4590390555208,2.90134173515981));
#214608=CARTESIAN_POINT('',(-6.83973663030197,-62.0330459552231,3.47153072139028));
#214609=CARTESIAN_POINT('Origin',(5.53234440788222E-15,1.85015204418142E-13,
3.47153072139072));
#214610=CARTESIAN_POINT('',(-6.87697683366501,-62.387392681069,2.9013417351598));
#214611=CARTESIAN_POINT('',(-6.83973663030197,-62.0330459552231,3.47153072139028));
#214612=CARTESIAN_POINT('',(-6.59568250079822,-62.6076796697353,2.59908173515979));
#214613=CARTESIAN_POINT('Ctrl Pts',(-6.87697683366501,-62.387392681069,
2.9013417351598));
#214614=CARTESIAN_POINT('Ctrl Pts',(-6.87826302285514,-62.3996312165462,
2.88164837656717));
#214615=CARTESIAN_POINT('Ctrl Pts',(-6.87760542308965,-62.4120334591675,
2.86203734439173));
#214616=CARTESIAN_POINT('Ctrl Pts',(-6.87506472947562,-62.4244204973369,
2.84277945978219));
#214617=CARTESIAN_POINT('Ctrl Pts',(-6.87247298342297,-62.4370564393892,
2.82313460920135));
#214618=CARTESIAN_POINT('Ctrl Pts',(-6.8679218469042,-62.4496774784038,
2.80385576863502));
#214619=CARTESIAN_POINT('Ctrl Pts',(-6.86142424477042,-62.462108044829,
2.78521678518593));
#214620=CARTESIAN_POINT('Ctrl Pts',(-6.85517906858932,-62.4740556950172,
2.76730190934719));
#214621=CARTESIAN_POINT('Ctrl Pts',(-6.84713544261466,-62.4858282202794,
2.7499768728007));
#214622=CARTESIAN_POINT('Ctrl Pts',(-6.83725958233962,-62.4972698477045,
2.73349253346047));
#214623=CARTESIAN_POINT('Ctrl Pts',(-6.829673289174,-62.5060589088617,2.72082983599476));
#214624=CARTESIAN_POINT('Ctrl Pts',(-6.82100495425393,-62.5146528151126,
2.70866321039345));
#214625=CARTESIAN_POINT('Ctrl Pts',(-6.81122125790617,-62.5229765487296,
2.69711645335801));
#214626=CARTESIAN_POINT('Ctrl Pts',(-6.81119561658287,-62.522998363751,
2.69708619136706));
#214627=CARTESIAN_POINT('Ctrl Pts',(-6.81116996676367,-62.5230201768491,
2.69705593387174));
#214628=CARTESIAN_POINT('Ctrl Pts',(-6.81114430845093,-62.5230419880216,
2.69702568087526));
#214629=CARTESIAN_POINT('Ctrl Pts',(-6.80839321554184,-62.525380589267,
2.69378194443221));
#214630=CARTESIAN_POINT('Ctrl Pts',(-6.80554511475005,-62.5276952632609,
2.69059266624656));
#214631=CARTESIAN_POINT('Ctrl Pts',(-6.80260378684053,-62.5299828381017,
2.68746219342633));
#214632=CARTESIAN_POINT('Ctrl Pts',(-6.78623596579703,-62.542712671962,
2.67004182396084));
#214633=CARTESIAN_POINT('Ctrl Pts',(-6.76698429120308,-62.5546072354113,
2.65443567877915));
#214634=CARTESIAN_POINT('Ctrl Pts',(-6.74555473734785,-62.5651294462094,
2.64136852353122));
#214635=CARTESIAN_POINT('Ctrl Pts',(-6.73593685681281,-62.5698519601313,
2.6355038032969));
#214636=CARTESIAN_POINT('Ctrl Pts',(-6.72588021343601,-62.5742983919725,
2.63014997451062));
#214637=CARTESIAN_POINT('Ctrl Pts',(-6.71544740276711,-62.5784220664832,
2.6253698111921));
#214638=CARTESIAN_POINT('Ctrl Pts',(-6.71091344436447,-62.5802141596488,
2.6232924168703));
#214639=CARTESIAN_POINT('Ctrl Pts',(-6.7063085522823,-62.5819451239081,
2.62132362131385));
#214640=CARTESIAN_POINT('Ctrl Pts',(-6.70163794008911,-62.5836110216377,
2.61946873372305));
#214641=CARTESIAN_POINT('Ctrl Pts',(-6.68529079741292,-62.5894416636912,
2.61297662715525));
#214642=CARTESIAN_POINT('Ctrl Pts',(-6.66813858303339,-62.5944752375492,
2.60787989113926));
#214643=CARTESIAN_POINT('Ctrl Pts',(-6.65040483057274,-62.5985429352695,
2.60440616886136));
#214644=CARTESIAN_POINT('Ctrl Pts',(-6.64153795434241,-62.6005767841296,
2.60266930772241));
#214645=CARTESIAN_POINT('Ctrl Pts',(-6.63252569365778,-62.6023691645597,
2.6013382004014));
#214646=CARTESIAN_POINT('Ctrl Pts',(-6.62339599105606,-62.6038989834437,
2.6004413072354));
#214647=CARTESIAN_POINT('Ctrl Pts',(-6.6188311397552,-62.6046638928856,
2.59999286065239));
#214648=CARTESIAN_POINT('Ctrl Pts',(-6.61423692798793,-62.6053631620636,
2.59965296768467));
#214649=CARTESIAN_POINT('Ctrl Pts',(-6.60961684864287,-62.6059941550339,
2.59942518630909));
#214650=CARTESIAN_POINT('Ctrl Pts',(-6.60499676929781,-62.6066251480041,
2.59919740493351));
#214651=CARTESIAN_POINT('Ctrl Pts',(-6.60035082219627,-62.6071878630699,
2.59908173791564));
#214652=CARTESIAN_POINT('Ctrl Pts',(-6.59568250079822,-62.6076796697353,
2.5990817351598));
#214653=CARTESIAN_POINT('',(-6.56531752495238,-62.6108711573004,2.59908173515979));
#214654=CARTESIAN_POINT('Origin',(-2.34395632424767E-17,1.9126204441108E-13,
2.59908173516022));
#214655=CARTESIAN_POINT('',(-6.24436990787996,-62.4538823482274,2.9013417351598));
#214656=CARTESIAN_POINT('Ctrl Pts',(-6.56531752495238,-62.6108711573004,
2.5990817351598));
#214657=CARTESIAN_POINT('Ctrl Pts',(-6.5615167448068,-62.6112696981209,
2.59908174381637));
#214658=CARTESIAN_POINT('Ctrl Pts',(-6.55772139932878,-62.6116196762805,
2.59915752000953));
#214659=CARTESIAN_POINT('Ctrl Pts',(-6.55393352450217,-62.6119220062407,
2.59930729517428));
#214660=CARTESIAN_POINT('Ctrl Pts',(-6.53204428085601,-62.6136691004463,
2.60017281085877));
#214661=CARTESIAN_POINT('Ctrl Pts',(-6.51040190952193,-62.6138271176314,
2.60350651800037));
#214662=CARTESIAN_POINT('Ctrl Pts',(-6.4894061806644,-62.6125709156638,
2.60896880596468));
#214663=CARTESIAN_POINT('Ctrl Pts',(-6.48093812023291,-62.6120642605128,
2.61117187235451));
#214664=CARTESIAN_POINT('Ctrl Pts',(-6.47257489900891,-62.6113278644154,
2.61372076577177));
#214665=CARTESIAN_POINT('Ctrl Pts',(-6.46434122353971,-62.6103742524839,
2.61659179896939));
#214666=CARTESIAN_POINT('Ctrl Pts',(-6.46130349717878,-62.6100224275773,
2.61765103591164));
#214667=CARTESIAN_POINT('Ctrl Pts',(-6.45828351400523,-62.609640959732,
2.61875422455104));
#214668=CARTESIAN_POINT('Ctrl Pts',(-6.45528256968463,-62.6092304414382,
2.61990022440351));
#214669=CARTESIAN_POINT('Ctrl Pts',(-6.44965579908351,-62.6084607196374,
2.62204897412688));
#214670=CARTESIAN_POINT('Ctrl Pts',(-6.44409596194912,-62.6075888673474,
2.62434823201725));
#214671=CARTESIAN_POINT('Ctrl Pts',(-6.43861159905706,-62.6066187902473,
2.6267904803026));
#214672=CARTESIAN_POINT('Ctrl Pts',(-6.41941632893488,-62.6032235203969,
2.63533834930134));
#214673=CARTESIAN_POINT('Ctrl Pts',(-6.40114561781689,-62.5986249921651,
2.64563784783518));
#214674=CARTESIAN_POINT('Ctrl Pts',(-6.38416565413431,-62.5929906867157,
2.6573666673792));
#214675=CARTESIAN_POINT('Ctrl Pts',(-6.37567567229302,-62.590173533991,
2.66323107715121));
#214676=CARTESIAN_POINT('Ctrl Pts',(-6.36750837741642,-62.5870974379666,
2.66945281780729));
#214677=CARTESIAN_POINT('Ctrl Pts',(-6.35970954393914,-62.5837833426316,
2.67599160631156));
#214678=CARTESIAN_POINT('Ctrl Pts',(-6.3558101272005,-62.5821262949641,
2.6792610005637));
#214679=CARTESIAN_POINT('Ctrl Pts',(-6.35200282582295,-62.5804097475858,
2.68260965685079));
#214680=CARTESIAN_POINT('Ctrl Pts',(-6.348293361661,-62.5786363190252,2.68603254012438));
#214681=CARTESIAN_POINT('Ctrl Pts',(-6.34458389749905,-62.5768628904645,
2.68945542339798));
#214682=CARTESIAN_POINT('Ctrl Pts',(-6.34097238394016,-62.5750325180134,
2.69295261525342));
#214683=CARTESIAN_POINT('Ctrl Pts',(-6.33746431138531,-62.573147949868,
2.69651891172056));
#214684=CARTESIAN_POINT('Ctrl Pts',(-6.33743439487346,-62.5731318784487,
2.69654932476044));
#214685=CARTESIAN_POINT('Ctrl Pts',(-6.33740448593519,-62.5731158032177,
2.69657974261102));
#214686=CARTESIAN_POINT('Ctrl Pts',(-6.33737458457315,-62.5730997241769,
2.69661016526929));
#214687=CARTESIAN_POINT('Ctrl Pts',(-6.32210352242668,-62.5648879232833,
2.71214746100876));
#214688=CARTESIAN_POINT('Ctrl Pts',(-6.30871688796685,-62.555777551299,
2.72880565567079));
#214689=CARTESIAN_POINT('Ctrl Pts',(-6.29717744164499,-62.5459655399085,
2.74628040011576));
#214690=CARTESIAN_POINT('Ctrl Pts',(-6.28524773891098,-62.5358216928083,
2.76434612881422));
#214691=CARTESIAN_POINT('Ctrl Pts',(-6.2752919217393,-62.5249271226299,
2.78328592653204));
#214692=CARTESIAN_POINT('Ctrl Pts',(-6.26731706752645,-62.5134793937861,
2.80278753266338));
#214693=CARTESIAN_POINT('Ctrl Pts',(-6.25949391182138,-62.5022494248331,
2.8219181772109));
#214694=CARTESIAN_POINT('Ctrl Pts',(-6.25357708652309,-62.4904862127101,
2.84159092313247));
#214695=CARTESIAN_POINT('Ctrl Pts',(-6.24962081353905,-62.4783706704866,
2.86151233814911));
#214696=CARTESIAN_POINT('Ctrl Pts',(-6.24699992138491,-62.4703445485065,
2.87470957719884));
#214697=CARTESIAN_POINT('Ctrl Pts',(-6.24524040122981,-62.4621637089645,
2.88801594387607));
#214698=CARTESIAN_POINT('Ctrl Pts',(-6.24436990787996,-62.4538823482274,
2.90134173515979));
#214699=CARTESIAN_POINT('',(-6.207123496544,-62.0995362748658,3.47153072139028));
#214700=CARTESIAN_POINT('',(-6.24436990787996,-62.4538823482274,2.9013417351598));
#214701=CARTESIAN_POINT('',(-0.318048871876464,-62.4081695979766,3.47153072139028));
#214702=CARTESIAN_POINT('Origin',(5.53234440788222E-15,1.85015204418142E-13,
3.47153072139072));
#214703=CARTESIAN_POINT('',(-0.318045750792381,-62.7644678366118,2.9013417351598));
#214704=CARTESIAN_POINT('',(-0.31804887187647,-62.4081695979766,3.47153072139028));
#214705=CARTESIAN_POINT('Ctrl Pts',(-0.318045750792382,-62.7644678366118,
2.9013417351598));
#214706=CARTESIAN_POINT('Ctrl Pts',(-0.318045618797467,-62.7767737714908,
2.88164837656695));
#214707=CARTESIAN_POINT('Ctrl Pts',(-0.31609523406997,-62.7890393354365,
2.86203734439129));
#214708=CARTESIAN_POINT('Ctrl Pts',(-0.312273660577038,-62.8010929413157,
2.84277945978154));
#214709=CARTESIAN_POINT('Ctrl Pts',(-0.308375296775692,-62.8133887511234,
2.8231346092005));
#214710=CARTESIAN_POINT('Ctrl Pts',(-0.302529834045799,-62.8254649274595,
2.80385576863398));
#214711=CARTESIAN_POINT('Ctrl Pts',(-0.294768478450234,-62.8371482135753,
2.78521678518473));
#214712=CARTESIAN_POINT('Ctrl Pts',(-0.287308644483666,-62.8483776146167,
2.76730190934571));
#214713=CARTESIAN_POINT('Ctrl Pts',(-0.278078518359005,-62.8592448608917,
2.74997687279897));
#214714=CARTESIAN_POINT('Ctrl Pts',(-0.26706078334753,-62.8695915013867,
2.73349253345854));
#214715=CARTESIAN_POINT('Ctrl Pts',(-0.258597341633625,-62.8775394315804,
2.72082983599353));
#214716=CARTESIAN_POINT('Ctrl Pts',(-0.249078184945788,-62.885180171785,
2.70866321039287));
#214717=CARTESIAN_POINT('Ctrl Pts',(-0.238478017627207,-62.8924356323736,
2.69711645335801));
#214718=CARTESIAN_POINT('Ctrl Pts',(-0.238450236479097,-62.8924546476418,
2.69708619136707));
#214719=CARTESIAN_POINT('Ctrl Pts',(-0.238422447082671,-62.8924736601093,
2.69705593387174));
#214720=CARTESIAN_POINT('Ctrl Pts',(-0.238394649440506,-62.892492669774,
2.69702568087526));
#214721=CARTESIAN_POINT('Ctrl Pts',(-0.235414176911842,-62.894530892403,
2.69378194443221));
#214722=CARTESIAN_POINT('Ctrl Pts',(-0.232339728998653,-62.8965351787716,
2.69059266624654));
#214723=CARTESIAN_POINT('Ctrl Pts',(-0.229175397308462,-62.8985027695517,
2.68746219342631));
#214724=CARTESIAN_POINT('Ctrl Pts',(-0.211566610931929,-62.9094519648683,
2.67004182396257));
#214725=CARTESIAN_POINT('Ctrl Pts',(-0.191177078589483,-62.919269020693,
2.65443567878226));
#214726=CARTESIAN_POINT('Ctrl Pts',(-0.168765047550213,-62.9274935913859,
2.64136852353514));
#214727=CARTESIAN_POINT('Ctrl Pts',(-0.158706217646005,-62.9311848926112,
2.63550380329928));
#214728=CARTESIAN_POINT('Ctrl Pts',(-0.148239886924228,-62.9345557609565,
2.63014997451169));
#214729=CARTESIAN_POINT('Ctrl Pts',(-0.137433186921743,-62.9375663198807,
2.6253698111921));
#214730=CARTESIAN_POINT('Ctrl Pts',(-0.132736741272993,-62.9388746680681,
2.6232924168703));
#214731=CARTESIAN_POINT('Ctrl Pts',(-0.12797614023748,-62.9401148076311,
2.62132362131384));
#214732=CARTESIAN_POINT('Ctrl Pts',(-0.123156980416938,-62.9412833674836,
2.61946873372304));
#214733=CARTESIAN_POINT('Ctrl Pts',(-0.106289921045043,-62.9453733269671,
2.61297662715524));
#214734=CARTESIAN_POINT('Ctrl Pts',(-0.0887055165504184,-62.9485864317702,
2.60787989113925));
#214735=CARTESIAN_POINT('Ctrl Pts',(-0.0706437212495209,-62.950778164324,
2.60440616886136));
#214736=CARTESIAN_POINT('Ctrl Pts',(-0.0616128235990723,-62.9518740306009,
2.60266930772241));
#214737=CARTESIAN_POINT('Ctrl Pts',(-0.0524625782494904,-62.9527145544236,
2.60133820040141));
#214738=CARTESIAN_POINT('Ctrl Pts',(-0.0432229794968653,-62.9532816790165,
2.60044130723541));
#214739=CARTESIAN_POINT('Ctrl Pts',(-0.0386031801205529,-62.953565241313,
2.59999286065241));
#214740=CARTESIAN_POINT('Ctrl Pts',(-0.0339610423934555,-62.9537804539253,
2.59965296768468));
#214741=CARTESIAN_POINT('Ctrl Pts',(-0.0293003156009411,-62.953925060456,
2.5994251863091));
#214742=CARTESIAN_POINT('Ctrl Pts',(-0.0246395888084267,-62.9540696669866,
2.59919740493352));
#214743=CARTESIAN_POINT('Ctrl Pts',(-0.0199602729501303,-62.9541436657294,
2.5990817379157));
#214744=CARTESIAN_POINT('Ctrl Pts',(-0.0152661173102018,-62.9541448057646,
2.5990817351598));
#214745=CARTESIAN_POINT('',(0.318045750793708,-62.7644678366118,2.90134173515979));
#214746=CARTESIAN_POINT('Ctrl Pts',(0.0152661173115319,-62.9541448057646,
2.5990817351598));
#214747=CARTESIAN_POINT('Ctrl Pts',(0.0190877352453155,-62.954143873629,
2.59908174381636));
#214748=CARTESIAN_POINT('Ctrl Pts',(0.0228988721028936,-62.9540952129412,
2.59915752000952));
#214749=CARTESIAN_POINT('Ctrl Pts',(0.0266975986410181,-62.9539999459716,
2.59930729517427));
#214750=CARTESIAN_POINT('Ctrl Pts',(0.0486495517930506,-62.9534494204118,
2.60017281085878));
#214751=CARTESIAN_POINT('Ctrl Pts',(0.0701898812463959,-62.9513443281452,
2.60350651800049));
#214752=CARTESIAN_POINT('Ctrl Pts',(0.0909392844435494,-62.9479003565107,
2.60896880596498));
#214753=CARTESIAN_POINT('Ctrl Pts',(0.0993079960692669,-62.9465113235258,
2.61117187235474));
#214754=CARTESIAN_POINT('Ctrl Pts',(0.107548428339577,-62.9449047668209,
2.61372076577191));
#214755=CARTESIAN_POINT('Ctrl Pts',(0.115637319282967,-62.9430957254315,
2.61659179896941));
#214756=CARTESIAN_POINT('Ctrl Pts',(0.118621628944221,-62.9424282989903,
2.61765103591166));
#214757=CARTESIAN_POINT('Ctrl Pts',(0.121585194086305,-62.9417332466656,
2.61875422455107));
#214758=CARTESIAN_POINT('Ctrl Pts',(0.124526788073524,-62.9410112931357,
2.61990022440354));
#214759=CARTESIAN_POINT('Ctrl Pts',(0.13004227679956,-62.9396576302673,
2.62204897412691));
#214760=CARTESIAN_POINT('Ctrl Pts',(0.13548052318433,-62.9382093928438,
2.62434823201728));
#214761=CARTESIAN_POINT('Ctrl Pts',(0.140833441494092,-62.9366713579024,
2.62679048030263));
#214762=CARTESIAN_POINT('Ctrl Pts',(0.15956865557826,-62.9312882356076,
2.63533834930136));
#214763=CARTESIAN_POINT('Ctrl Pts',(0.177258600739667,-62.9248050892387,
2.64563784783519));
#214764=CARTESIAN_POINT('Ctrl Pts',(0.193556601114335,-62.917426759594,
2.6573666673792));
#214765=CARTESIAN_POINT('Ctrl Pts',(0.20170560130167,-62.9137375947717,
2.66323107715121));
#214766=CARTESIAN_POINT('Ctrl Pts',(0.20950661529208,-62.9098246351406,
2.66945281780729));
#214767=CARTESIAN_POINT('Ctrl Pts',(0.216916308651066,-62.9057134946879,
2.67599160631155));
#214768=CARTESIAN_POINT('Ctrl Pts',(0.220621155330559,-62.9036579244616,
2.67926100056369));
#214769=CARTESIAN_POINT('Ctrl Pts',(0.224228171853214,-62.9015528091472,
2.68260965685078));
#214770=CARTESIAN_POINT('Ctrl Pts',(0.2277319414202,-62.8994013510254,2.68603254012437));
#214771=CARTESIAN_POINT('Ctrl Pts',(0.231235710987187,-62.8972498929036,
2.68945542339796));
#214772=CARTESIAN_POINT('Ctrl Pts',(0.234636114277403,-62.8950520414619,
2.69295261525339));
#214773=CARTESIAN_POINT('Ctrl Pts',(0.237927978231588,-62.8928111037449,
2.69651891172053));
#214774=CARTESIAN_POINT('Ctrl Pts',(0.237956050936886,-62.8927919932394,
2.69654932476041));
#214775=CARTESIAN_POINT('Ctrl Pts',(0.23798411571168,-62.8927728797349,
2.696579742611));
#214776=CARTESIAN_POINT('Ctrl Pts',(0.238012172553516,-62.8927537632333,
2.69661016526928));
#214777=CARTESIAN_POINT('Ctrl Pts',(0.252341211298998,-62.8829906867833,
2.7121474610124));
#214778=CARTESIAN_POINT('Ctrl Pts',(0.26470221919375,-62.8725309380389,
2.72880565567861));
#214779=CARTESIAN_POINT('Ctrl Pts',(0.275152816750645,-62.8615664772797,
2.74628040012808));
#214780=CARTESIAN_POINT('Ctrl Pts',(0.285956846577482,-62.8502312057383,
2.76434612883121));
#214781=CARTESIAN_POINT('Ctrl Pts',(0.294719332062974,-62.8383556508826,
2.78328592655403));
#214782=CARTESIAN_POINT('Ctrl Pts',(0.301453885685765,-62.8261370346363,
2.8027875326905));
#214783=CARTESIAN_POINT('Ctrl Pts',(0.308060333927675,-62.8141508421817,
2.8219181772426));
#214784=CARTESIAN_POINT('Ctrl Pts',(0.312715155750267,-62.8018335935067,
2.84159092316882));
#214785=CARTESIAN_POINT('Ctrl Pts',(0.315383336844492,-62.7893708783531,
2.86151233819002));
#214786=CARTESIAN_POINT('Ctrl Pts',(0.317150913276949,-62.7811147664881,
2.87470957722633));
#214787=CARTESIAN_POINT('Ctrl Pts',(0.318045664009116,-62.7727948225118,
2.88801594388984));
#214788=CARTESIAN_POINT('Ctrl Pts',(0.318045750793708,-62.7644678366117,
2.90134173515979));
#214789=CARTESIAN_POINT('',(0.318048871877787,-62.4081695979766,3.47153072139028));
#214790=CARTESIAN_POINT('',(0.318045750793708,-62.7644678366118,2.90134173515979));
#214791=CARTESIAN_POINT('',(6.20712349654527,-62.0995362748656,3.47153072139028));
#214792=CARTESIAN_POINT('Origin',(5.53234440788222E-15,1.85015204418142E-13,
3.47153072139072));
#214793=CARTESIAN_POINT('',(6.24436990788122,-62.4538823482273,2.9013417351598));
#214794=CARTESIAN_POINT('',(6.20712349654526,-62.0995362748656,3.47153072139028));
#214795=CARTESIAN_POINT('',(6.56531752495365,-62.6108711573003,2.5990817351598));
#214796=CARTESIAN_POINT('Ctrl Pts',(6.24436990788123,-62.4538823482273,
2.9013417351598));
#214797=CARTESIAN_POINT('Ctrl Pts',(6.24565635961516,-62.4661208561104,
2.88164837656655));
#214798=CARTESIAN_POINT('Ctrl Pts',(6.24887816048156,-62.4781153572954,
2.86203734439049));
#214799=CARTESIAN_POINT('Ctrl Pts',(6.25393874389462,-62.4897034690562,
2.84277945978035));
#214800=CARTESIAN_POINT('Ctrl Pts',(6.25910101415518,-62.501524431154,2.82313460919898));
#214801=CARTESIAN_POINT('Ctrl Pts',(6.26617675898339,-62.5129234356965,
2.80385576863215));
#214802=CARTESIAN_POINT('Ctrl Pts',(6.27511683300479,-62.5237314369754,
2.78521678518261));
#214803=CARTESIAN_POINT('Ctrl Pts',(6.2837095932548,-62.5341195572022,2.76730190934353));
#214804=CARTESIAN_POINT('Ctrl Pts',(6.29402509233604,-62.5439624606655,
2.74997687279674));
#214805=CARTESIAN_POINT('Ctrl Pts',(6.30606398947345,-62.5531007542718,
2.73349253345627));
#214806=CARTESIAN_POINT('Ctrl Pts',(6.31531185249695,-62.5601204743155,
2.72082983599208));
#214807=CARTESIAN_POINT('Ctrl Pts',(6.3255775370797,-62.5667243349252,2.70866321039218));
#214808=CARTESIAN_POINT('Ctrl Pts',(6.33687803771754,-62.572832030141,2.69711645335801));
#214809=CARTESIAN_POINT('Ctrl Pts',(6.33690765431438,-62.5728480373209,
2.69708619136707));
#214810=CARTESIAN_POINT('Ctrl Pts',(6.3369372788216,-62.5728640408532,2.69705593387174));
#214811=CARTESIAN_POINT('Ctrl Pts',(6.3369669112364,-62.5728800407361,2.69702568087526));
#214812=CARTESIAN_POINT('Ctrl Pts',(6.34014410870391,-62.574595553555,2.69378194443222));
#214813=CARTESIAN_POINT('Ctrl Pts',(6.34341121944381,-62.5762674929175,
2.69059266624656));
#214814=CARTESIAN_POINT('Ctrl Pts',(6.34676388583449,-62.5778935423005,
2.68746219342633));
#214815=CARTESIAN_POINT('Ctrl Pts',(6.36542071199915,-62.5869421374006,
2.67004182396085));
#214816=CARTESIAN_POINT('Ctrl Pts',(6.38672471011157,-62.5945741278843,
2.65443567877916));
#214817=CARTESIAN_POINT('Ctrl Pts',(6.40987366743805,-62.6004109483555,
2.64136852353124));
#214818=CARTESIAN_POINT('Ctrl Pts',(6.42026324006196,-62.6030305942135,
2.63550380329691));
#214819=CARTESIAN_POINT('Ctrl Pts',(6.43102458681462,-62.6052889671223,
2.63014997451063));
#214820=CARTESIAN_POINT('Ctrl Pts',(6.44208677567923,-62.607153426145,2.6253698111921));
#214821=CARTESIAN_POINT('Ctrl Pts',(6.44689425333277,-62.6079636948177,
2.6232924168703));
#214822=CARTESIAN_POINT('Ctrl Pts',(6.45175840518046,-62.608699422456,2.62132362131385));
#214823=CARTESIAN_POINT('Ctrl Pts',(6.45667331290488,-62.609357841445,2.61946873372305));
#214824=CARTESIAN_POINT('Ctrl Pts',(6.47387548994035,-62.6116623079065,
2.61297662715525));
#214825=CARTESIAN_POINT('Ctrl Pts',(6.49169942613465,-62.613019740206,2.60787989113926));
#214826=CARTESIAN_POINT('Ctrl Pts',(6.5098913754668,-62.6133114945129,2.60440616886136));
#214827=CARTESIAN_POINT('Ctrl Pts',(6.51898735013288,-62.6134573716664,
2.60266930772241));
#214828=CARTESIAN_POINT('Ctrl Pts',(6.52817532814455,-62.6133368299267,
2.60133820040141));
#214829=CARTESIAN_POINT('Ctrl Pts',(6.53742359207063,-62.612935046693,2.60044130723541));
#214830=CARTESIAN_POINT('Ctrl Pts',(6.54204772403368,-62.6127341550761,
2.5999928606524));
#214831=CARTESIAN_POINT('Ctrl Pts',(6.54668692748823,-62.6124629532083,
2.59965296768468));
#214832=CARTESIAN_POINT('Ctrl Pts',(6.55133723783014,-62.6121195889599,
2.5994251863091));
#214833=CARTESIAN_POINT('Ctrl Pts',(6.55598754817206,-62.6117762247115,
2.59919740493352));
#214834=CARTESIAN_POINT('Ctrl Pts',(6.56064896522335,-62.6113606963857,
2.59908173791572));
#214835=CARTESIAN_POINT('Ctrl Pts',(6.56531752495365,-62.6108711573003,
2.5990817351598));
#214836=CARTESIAN_POINT('',(6.59568250079948,-62.6076796697351,2.5990817351598));
#214837=CARTESIAN_POINT('Origin',(5.63895492999586E-15,1.85567159826749E-13,
2.59908173516024));
#214838=CARTESIAN_POINT('',(6.87697683366627,-62.3873926810689,2.9013417351598));
#214839=CARTESIAN_POINT('Ctrl Pts',(6.59568250079948,-62.6076796697352,
2.59908173515981));
#214840=CARTESIAN_POINT('Ctrl Pts',(6.59948308607566,-62.607279274856,2.59908174381644));
#214841=CARTESIAN_POINT('Ctrl Pts',(6.60326825869985,-62.6068325084576,
2.59915752000952));
#214842=CARTESIAN_POINT('Ctrl Pts',(6.60703621730659,-62.606340688323,2.59930729517427));
#214843=CARTESIAN_POINT('Ctrl Pts',(6.62881036977196,-62.6034985746711,
2.60017281085879));
#214844=CARTESIAN_POINT('Ctrl Pts',(6.6500126569874,-62.599153436784,2.6035065180006));
#214845=CARTESIAN_POINT('Ctrl Pts',(6.67028839972057,-62.5935594283564,
2.60896880596523));
#214846=CARTESIAN_POINT('Ctrl Pts',(6.67846607318471,-62.5913032360739,
2.61117187235494));
#214847=CARTESIAN_POINT('Ctrl Pts',(6.68649343260099,-62.5888441205329,
2.61372076577201));
#214848=CARTESIAN_POINT('Ctrl Pts',(6.69434891543672,-62.5861994699218,
2.61659179896941));
#214849=CARTESIAN_POINT('Ctrl Pts',(6.69724711167715,-62.5852237544096,
2.61765103591166));
#214850=CARTESIAN_POINT('Ctrl Pts',(6.70012178934791,-62.5842227327442,
2.61875422455107));
#214851=CARTESIAN_POINT('Ctrl Pts',(6.70297180428246,-62.5831972538523,
2.61990022440353));
#214852=CARTESIAN_POINT('Ctrl Pts',(6.70831558228475,-62.58127448093,2.6220489741269));
#214853=CARTESIAN_POINT('Ctrl Pts',(6.71357265535448,-62.5792657255651,
2.62434823201727));
#214854=CARTESIAN_POINT('Ctrl Pts',(6.71873548138878,-62.5771765838151,
2.62679048030263));
#214855=CARTESIAN_POINT('Ctrl Pts',(6.73680537250885,-62.5698645876903,
2.63533834930136));
#214856=CARTESIAN_POINT('Ctrl Pts',(6.75372073697266,-62.5615678538925,
2.6456378478352));
#214857=CARTESIAN_POINT('Ctrl Pts',(6.76915820973675,-62.5525263385762,
2.65736666737921));
#214858=CARTESIAN_POINT('Ctrl Pts',(6.7768769461188,-62.548005580918,2.66323107715122));
#214859=CARTESIAN_POINT('Ctrl Pts',(6.78422620968128,-62.5432986288849,
2.6694528178073));
#214860=CARTESIAN_POINT('Ctrl Pts',(6.79116558077096,-62.5384354858296,
2.67599160631157));
#214861=CARTESIAN_POINT('Ctrl Pts',(6.7946352663158,-62.536003914302,2.6792610005637));
#214862=CARTESIAN_POINT('Ctrl Pts',(6.79800247875573,-62.5335332951355,
2.68260965685079));
#214863=CARTESIAN_POINT('Ctrl Pts',(6.80126216569517,-62.5310273792779,
2.68603254012438));
#214864=CARTESIAN_POINT('Ctrl Pts',(6.8045218526346,-62.5285214634203,2.68945542339798));
#214865=CARTESIAN_POINT('Ctrl Pts',(6.80767389012611,-62.5259802131084,
2.6929526152534));
#214866=CARTESIAN_POINT('Ctrl Pts',(6.81071347912929,-62.5234074580022,
2.69651891172054));
#214867=CARTESIAN_POINT('Ctrl Pts',(6.8107394004576,-62.5233855177894,2.69654932476042));
#214868=CARTESIAN_POINT('Ctrl Pts',(6.81076531358537,-62.5233635754229,
2.69657974261101));
#214869=CARTESIAN_POINT('Ctrl Pts',(6.81079121851035,-62.5233416309049,
2.69661016526929));
#214870=CARTESIAN_POINT('Ctrl Pts',(6.82402124190353,-62.5121342452096,
2.7121474610116));
#214871=CARTESIAN_POINT('Ctrl Pts',(6.83522119344078,-62.5004397189042,
2.72880565567688));
#214872=CARTESIAN_POINT('Ctrl Pts',(6.84446844329679,-62.4884429377061,
2.74628040012536));
#214873=CARTESIAN_POINT('Ctrl Pts',(6.85402842900256,-62.4760404333339,
2.7643461288275));
#214874=CARTESIAN_POINT('Ctrl Pts',(6.86150157917614,-62.4633140048688,
2.78328592654925));
#214875=CARTESIAN_POINT('Ctrl Pts',(6.86692204703019,-62.4504583709405,
2.80278753268463));
#214876=CARTESIAN_POINT('Ctrl Pts',(6.87223940617985,-62.4378472782204,
2.82191817723579));
#214877=CARTESIAN_POINT('Ctrl Pts',(6.87558122532613,-62.4251109433511,
2.84159092316106));
#214878=CARTESIAN_POINT('Ctrl Pts',(6.87693208138253,-62.4124375993861,
2.86151233818132));
#214879=CARTESIAN_POINT('Ctrl Pts',(6.87782697616112,-62.4040419533157,
2.87470957722049));
#214880=CARTESIAN_POINT('Ctrl Pts',(6.87784715439705,-62.3956740599421,
2.88801594388692));
#214881=CARTESIAN_POINT('Ctrl Pts',(6.87697683366627,-62.3873926810689,
2.90134173515981));
#214882=CARTESIAN_POINT('',(6.83973663030322,-62.033045955223,3.47153072139028));
#214883=CARTESIAN_POINT('',(6.87697683366627,-62.3873926810689,2.9013417351598));
#214884=CARTESIAN_POINT('',(12.6642893210148,-61.1105274371638,3.47153072139029));
#214885=CARTESIAN_POINT('Origin',(5.53234440788222E-15,1.85015204418142E-13,
3.47153072139072));
#214886=CARTESIAN_POINT('',(12.7383709431257,-61.4590390555205,2.90134173515981));
#214887=CARTESIAN_POINT('',(12.6642893210148,-61.1105274371638,3.47153072139029));
#214888=CARTESIAN_POINT('',(13.0739701745332,-61.5816197022694,2.59908173515981));
#214889=CARTESIAN_POINT('Ctrl Pts',(12.7383709431257,-61.4590390555205,
2.90134173515981));
#214890=CARTESIAN_POINT('Ctrl Pts',(12.740929619964,-61.471076048754,2.88164837656683));
#214891=CARTESIAN_POINT('Ctrl Pts',(12.7453875382446,-61.4826680729129,
2.86203734439105));
#214892=CARTESIAN_POINT('Ctrl Pts',(12.7516316867666,-61.4936637287773,
2.84277945978117));
#214893=CARTESIAN_POINT('Ctrl Pts',(12.7580013045728,-61.5048803302305,
2.82313460919998));
#214894=CARTESIAN_POINT('Ctrl Pts',(12.766229808158,-61.5154772731,2.80385576863331));
#214895=CARTESIAN_POINT('Ctrl Pts',(12.776250651283,-61.525291574818,2.78521678518393));
#214896=CARTESIAN_POINT('Ctrl Pts',(12.7858821937368,-61.5347245998112,
2.76730190934486));
#214897=CARTESIAN_POINT('Ctrl Pts',(12.7971700470077,-61.5434353195526,
2.74997687279808));
#214898=CARTESIAN_POINT('Ctrl Pts',(12.8100982055944,-61.5512651452132,
2.73349253345762));
#214899=CARTESIAN_POINT('Ctrl Pts',(12.8200291684057,-61.5572797455859,
2.72082983599294));
#214900=CARTESIAN_POINT('Ctrl Pts',(12.8309289078957,-61.5627743733226,
2.70866321039259));
#214901=CARTESIAN_POINT('Ctrl Pts',(12.8428059312041,-61.5676673859793,
2.69711645335802));
#214902=CARTESIAN_POINT('Ctrl Pts',(12.8428370587641,-61.5676802096928,
2.69708619136708));
#214903=CARTESIAN_POINT('Ctrl Pts',(12.8428681938098,-61.5676930289519,
2.69705593387175));
#214904=CARTESIAN_POINT('Ctrl Pts',(12.8428993363383,-61.567705843755,2.69702568087527));
#214905=CARTESIAN_POINT('Ctrl Pts',(12.8462384487043,-61.5690798512464,
2.69378194443223));
#214906=CARTESIAN_POINT('Ctrl Pts',(12.849662427122,-61.5704011254851,2.69059266624657));
#214907=CARTESIAN_POINT('Ctrl Pts',(12.8531666956986,-61.5716678181338,
2.68746219342633));
#214908=CARTESIAN_POINT('Ctrl Pts',(12.8726671535588,-61.578716674715,2.67004182396007));
#214909=CARTESIAN_POINT('Ctrl Pts',(12.8946522063786,-61.5840799821724,
2.65443567877777));
#214910=CARTESIAN_POINT('Ctrl Pts',(12.9182844651701,-61.5874651029946,
2.64136852352948));
#214911=CARTESIAN_POINT('Ctrl Pts',(12.928890950183,-61.5889843920979,2.63550380329583));
#214912=CARTESIAN_POINT('Ctrl Pts',(12.9398294094008,-61.5901055263647,
2.63014997451013));
#214913=CARTESIAN_POINT('Ctrl Pts',(12.9510258874727,-61.5908034580834,
2.62536981119208));
#214914=CARTESIAN_POINT('Ctrl Pts',(12.9558917253998,-61.5911067697682,
2.62329241687029));
#214915=CARTESIAN_POINT('Ctrl Pts',(12.9608061353942,-61.5913300246958,
2.62132362131383));
#214916=CARTESIAN_POINT('Ctrl Pts',(12.9657629422649,-61.5914710890451,
2.61946873372304));
#214917=CARTESIAN_POINT('Ctrl Pts',(12.9831117663126,-61.5919648142679,
2.61297662715524));
#214918=CARTESIAN_POINT('Ctrl Pts',(13.0009799514317,-61.5914517017514,
2.60787989113925));
#214919=CARTESIAN_POINT('Ctrl Pts',(13.0191027399913,-61.5898402812902,
2.60440616886136));
#214920=CARTESIAN_POINT('Ctrl Pts',(13.0281641342711,-61.5890345710596,
2.60266930772241));
#214921=CARTESIAN_POINT('Ctrl Pts',(13.037289179535,-61.587954284438,2.60133820040142));
#214922=CARTESIAN_POINT('Ctrl Pts',(13.0464447827197,-61.5865879953988,
2.60044130723542));
#214923=CARTESIAN_POINT('Ctrl Pts',(13.051022584312,-61.5859048508792,2.59999286065241));
#214924=CARTESIAN_POINT('Ctrl Pts',(13.0556080254101,-61.5851502058757,
2.59965296768469));
#214925=CARTESIAN_POINT('Ctrl Pts',(13.0601969695282,-61.5843226328189,
2.59942518630911));
#214926=CARTESIAN_POINT('Ctrl Pts',(13.0647859136462,-61.583495059762,2.59919740493353));
#214927=CARTESIAN_POINT('Ctrl Pts',(13.0693783604298,-61.5825945569828,
2.59908173791571));
#214928=CARTESIAN_POINT('Ctrl Pts',(13.0739701745332,-61.5816197022694,
2.59908173515981));
#214929=CARTESIAN_POINT('',(13.1038352065734,-61.5752716937448,2.59908173515981));
#214930=CARTESIAN_POINT('Origin',(5.62288786856779E-15,1.85564615054217E-13,
2.59908173516023));
#214931=CARTESIAN_POINT('',(13.3605623192493,-61.326788195911,2.90134173515982));
#214932=CARTESIAN_POINT('Ctrl Pts',(13.1038352065734,-61.5752716937448,
2.5990817351598));
#214933=CARTESIAN_POINT('Ctrl Pts',(13.1075731191844,-61.5744762229323,
2.59908174381639));
#214934=CARTESIAN_POINT('Ctrl Pts',(13.1112908564318,-61.5736362456893,
2.59915752000952));
#214935=CARTESIAN_POINT('Ctrl Pts',(13.1149867645642,-61.572753260874,2.59930729517427));
#214936=CARTESIAN_POINT('Ctrl Pts',(13.1363445541695,-61.5676506979224,
2.6001728108587));
#214937=CARTESIAN_POINT('Ctrl Pts',(13.1569765024491,-61.5611131206558,
2.60350651799992));
#214938=CARTESIAN_POINT('Ctrl Pts',(13.1765564394358,-61.5534303645632,
2.60896880596356));
#214939=CARTESIAN_POINT('Ctrl Pts',(13.184453478439,-61.5503317322971,2.61117187235366));
#214940=CARTESIAN_POINT('Ctrl Pts',(13.192179815574,-61.5470470005036,2.61372076577129));
#214941=CARTESIAN_POINT('Ctrl Pts',(13.1997158239905,-61.5435957160154,
2.61659179896941));
#214942=CARTESIAN_POINT('Ctrl Pts',(13.2024961535656,-61.5423224015756,
2.61765103591166));
#214943=CARTESIAN_POINT('Ctrl Pts',(13.2052504481949,-61.5410263779723,
2.61875422455106));
#214944=CARTESIAN_POINT('Ctrl Pts',(13.2079776587167,-61.5397086090796,
2.61990022440353));
#214945=CARTESIAN_POINT('Ctrl Pts',(13.2130911784452,-61.537237792406,2.6220489741269));
#214946=CARTESIAN_POINT('Ctrl Pts',(13.2181094806073,-61.5346905274439,
2.62434823201727));
#214947=CARTESIAN_POINT('Ctrl Pts',(13.2230256493637,-61.5320731679596,
2.62679048030262));
#214948=CARTESIAN_POINT('Ctrl Pts',(13.2402322400112,-61.5229124097644,
2.63533834930136));
#214949=CARTESIAN_POINT('Ctrl Pts',(13.2561876955045,-61.5128929892894,
2.6456378478352));
#214950=CARTESIAN_POINT('Ctrl Pts',(13.2705955044759,-61.5022873490352,
2.65736666737921));
#214951=CARTESIAN_POINT('Ctrl Pts',(13.2777994089617,-61.4969845289081,
2.66323107715122));
#214952=CARTESIAN_POINT('Ctrl Pts',(13.2846164020267,-61.4915351548244,
2.6694528178073));
#214953=CARTESIAN_POINT('Ctrl Pts',(13.2910094216452,-61.4859732907796,
2.67599160631157));
#214954=CARTESIAN_POINT('Ctrl Pts',(13.2942059314545,-61.4831923587572,
2.67926100056371));
#214955=CARTESIAN_POINT('Ctrl Pts',(13.2972964479276,-61.4803833043592,
2.6826096568508));
#214956=CARTESIAN_POINT('Ctrl Pts',(13.3002763384272,-61.4775503861043,
2.6860325401244));
#214957=CARTESIAN_POINT('Ctrl Pts',(13.3032562289269,-61.4747174678495,
2.68945542339799));
#214958=CARTESIAN_POINT('Ctrl Pts',(13.3061253662373,-61.4718606611374,
2.69295261525341));
#214959=CARTESIAN_POINT('Ctrl Pts',(13.3088793779163,-61.4689842762855,
2.69651891172055));
#214960=CARTESIAN_POINT('Ctrl Pts',(13.3089028638681,-61.4689597467468,
2.69654932476043));
#214961=CARTESIAN_POINT('Ctrl Pts',(13.3089263414392,-61.4689352159235,
2.69657974261101));
#214962=CARTESIAN_POINT('Ctrl Pts',(13.3089498106276,-61.4689106838179,
2.69661016526929));
#214963=CARTESIAN_POINT('Ctrl Pts',(13.3209358677647,-61.4563817793394,
2.71214746101209));
#214964=CARTESIAN_POINT('Ctrl Pts',(13.3308520539325,-61.4435806031494,
2.72880565567793));
#214965=CARTESIAN_POINT('Ctrl Pts',(13.3387946412835,-61.4306829407567,
2.746280400127));
#214966=CARTESIAN_POINT('Ctrl Pts',(13.3470058416648,-61.4173490879861,
2.76434612882973));
#214967=CARTESIAN_POINT('Ctrl Pts',(13.3531077791294,-61.4039112193238,
2.78328592655213));
#214968=CARTESIAN_POINT('Ctrl Pts',(13.3571547734345,-61.3905594167279,
2.80278753268816));
#214969=CARTESIAN_POINT('Ctrl Pts',(13.361124785392,-61.3774615935124,2.82191817723989));
#214970=CARTESIAN_POINT('Ctrl Pts',(13.3631169881916,-61.3644457143979,
2.84159092316572));
#214971=CARTESIAN_POINT('Ctrl Pts',(13.3631357189477,-61.3517005934293,
2.86151233818654));
#214972=CARTESIAN_POINT('Ctrl Pts',(13.3631481274169,-61.3432573976117,
2.87470957722401));
#214973=CARTESIAN_POINT('Ctrl Pts',(13.3622935120792,-61.3349332352346,
2.88801594388869));
#214974=CARTESIAN_POINT('Ctrl Pts',(13.3605623192493,-61.326788195911,2.90134173515982));
#214975=CARTESIAN_POINT('',(13.2864868029002,-60.9782752797345,3.47153072139029));
#214976=CARTESIAN_POINT('',(13.3605623192493,-61.326788195911,2.90134173515982));
#214977=CARTESIAN_POINT('',(18.9827025415103,-59.4519788726604,3.4715307213903));
#214978=CARTESIAN_POINT('Origin',(5.53234440788222E-15,1.85015204418142E-13,
3.47153072139072));
#214979=CARTESIAN_POINT('',(19.0928077206418,-59.7908376697908,2.90134173515982));
#214980=CARTESIAN_POINT('',(18.9827025415103,-59.4519788726604,3.4715307213903));
#214981=CARTESIAN_POINT('',(19.4393816709763,-59.8776671349981,2.59908173515982));
#214982=CARTESIAN_POINT('Ctrl Pts',(19.0928077206418,-59.7908376697907,
2.90134173515982));
#214983=CARTESIAN_POINT('Ctrl Pts',(19.0966105891854,-59.8025412685574,
2.88164837656781));
#214984=CARTESIAN_POINT('Ctrl Pts',(19.1022557829942,-59.8136038110473,
2.86203734439298));
#214985=CARTESIAN_POINT('Ctrl Pts',(19.1096150844268,-59.8238865403086,
2.84277945978402));
#214986=CARTESIAN_POINT('Ctrl Pts',(19.1171222629127,-59.8343758896842,
2.82313460920365));
#214987=CARTESIAN_POINT('Ctrl Pts',(19.1264133720472,-59.8440546685567,
2.80385576863777));
#214988=CARTESIAN_POINT('Ctrl Pts',(19.1374051938209,-59.8527677431703,
2.78521678518909));
#214989=CARTESIAN_POINT('Ctrl Pts',(19.1479699932833,-59.8611423227339,
2.76730190935045));
#214990=CARTESIAN_POINT('Ctrl Pts',(19.1601065286608,-59.8686254222852,
2.74997687280405));
#214991=CARTESIAN_POINT('Ctrl Pts',(19.1737823050853,-59.8750609947916,
2.73349253346387));
#214992=CARTESIAN_POINT('Ctrl Pts',(19.1842875619788,-59.8800045782738,
2.72082983599695));
#214993=CARTESIAN_POINT('Ctrl Pts',(19.1957019365507,-59.8843297728467,
2.7086632103945));
#214994=CARTESIAN_POINT('Ctrl Pts',(19.2080253553785,-59.887954494074,2.69711645335803));
#214995=CARTESIAN_POINT('Ctrl Pts',(19.2080576528615,-59.8879639938219,
2.69708619136709));
#214996=CARTESIAN_POINT('Ctrl Pts',(19.2080899573236,-59.8879734883573,
2.69705593387176));
#214997=CARTESIAN_POINT('Ctrl Pts',(19.2081222687617,-59.8879829776789,
2.69702568087529));
#214998=CARTESIAN_POINT('Ctrl Pts',(19.2115867120124,-59.8890004259292,
2.69378194443224));
#214999=CARTESIAN_POINT('Ctrl Pts',(19.2151300442838,-59.8899565588871,
2.69059266624658));
#215000=CARTESIAN_POINT('Ctrl Pts',(19.2187475215465,-59.8908500166518,
2.68746219342635));
#215001=CARTESIAN_POINT('Ctrl Pts',(19.238877960004,-59.8958219059659,2.67004182396045));
#215002=CARTESIAN_POINT('Ctrl Pts',(19.2613031946901,-59.8988577688777,
2.65443567877845));
#215003=CARTESIAN_POINT('Ctrl Pts',(19.2851598349722,-59.8997541019589,
2.64136852353034));
#215004=CARTESIAN_POINT('Ctrl Pts',(19.2958670255061,-59.9001563886585,
2.63550380329636));
#215005=CARTESIAN_POINT('Ctrl Pts',(19.3068627531423,-59.900128000902,2.63014997451039));
#215006=CARTESIAN_POINT('Ctrl Pts',(19.3180708494664,-59.8996517586308,
2.62536981119211));
#215007=CARTESIAN_POINT('Ctrl Pts',(19.3229417365285,-59.8994447901814,
2.62329241687031));
#215008=CARTESIAN_POINT('Ctrl Pts',(19.3278525613652,-59.8991531263706,
2.62132362131386));
#215009=CARTESIAN_POINT('Ctrl Pts',(19.332796959569,-59.8987752905497,2.61946873372306));
#215010=CARTESIAN_POINT('Ctrl Pts',(19.350102353282,-59.8974528651769,2.61297662715526));
#215011=CARTESIAN_POINT('Ctrl Pts',(19.3678190197507,-59.8950748296126,
2.60787989113928));
#215012=CARTESIAN_POINT('Ctrl Pts',(19.3856740904738,-59.891577889443,2.60440616886138));
#215013=CARTESIAN_POINT('Ctrl Pts',(19.3946016258354,-59.8898294193582,
2.60266930772243));
#215014=CARTESIAN_POINT('Ctrl Pts',(19.4035637624462,-59.8878012237011,
2.60133820040143));
#215015=CARTESIAN_POINT('Ctrl Pts',(19.412526394185,-59.885485398205,2.60044130723542));
#215016=CARTESIAN_POINT('Ctrl Pts',(19.4170077100544,-59.884327485457,2.59999286065242));
#215017=CARTESIAN_POINT('Ctrl Pts',(19.4214891497439,-59.8830976653664,
2.59965296768469));
#215018=CARTESIAN_POINT('Ctrl Pts',(19.4259664502061,-59.8817949505647,
2.59942518630911));
#215019=CARTESIAN_POINT('Ctrl Pts',(19.4304437506682,-59.8804922357629,
2.59919740493353));
#215020=CARTESIAN_POINT('Ctrl Pts',(19.4349169113761,-59.8791166246272,
2.59908173791573));
#215021=CARTESIAN_POINT('Ctrl Pts',(19.4393816709763,-59.8776671349981,
2.59908173515982));
#215022=CARTESIAN_POINT('',(19.4684195516703,-59.8682321556238,2.59908173515982));
#215023=CARTESIAN_POINT('Origin',(5.60717482534548E-15,1.85560404756975E-13,
2.59908173516023));
#215024=CARTESIAN_POINT('',(19.6977666881852,-59.5942745858232,2.90134173515982));
#215025=CARTESIAN_POINT('Ctrl Pts',(19.4684195516703,-59.8682321556238,
2.59908173515982));
#215026=CARTESIAN_POINT('Ctrl Pts',(19.4720538382633,-59.8670503242226,
2.59908174381642));
#215027=CARTESIAN_POINT('Ctrl Pts',(19.4756634078267,-59.8658263391015,
2.59915752000954));
#215028=CARTESIAN_POINT('Ctrl Pts',(19.4792467723418,-59.864561863772,2.59930729517429));
#215029=CARTESIAN_POINT('Ctrl Pts',(19.4999541986788,-59.8572547562672,
2.6001728108588));
#215030=CARTESIAN_POINT('Ctrl Pts',(19.5197897600835,-59.848596366684,2.60350651800055));
#215031=CARTESIAN_POINT('Ctrl Pts',(19.5384593694403,-59.8389090368079,
2.60896880596511));
#215032=CARTESIAN_POINT('Ctrl Pts',(19.5459892523667,-59.8350019138231,
2.61117187235484));
#215033=CARTESIAN_POINT('Ctrl Pts',(19.5533299158501,-59.8309275539876,
2.61372076577195));
#215034=CARTESIAN_POINT('Ctrl Pts',(19.5604638837584,-59.8267074486189,
2.61659179896939));
#215035=CARTESIAN_POINT('Ctrl Pts',(19.5630958847955,-59.825150485951,2.61765103591165));
#215036=CARTESIAN_POINT('Ctrl Pts',(19.5656996197551,-59.8235736599156,
2.61875422455105));
#215037=CARTESIAN_POINT('Ctrl Pts',(19.568274145975,-59.821978038774,2.61990022440351));
#215038=CARTESIAN_POINT('Ctrl Pts',(19.5731013826375,-59.8189862491335,
2.62204897412688));
#215039=CARTESIAN_POINT('Ctrl Pts',(19.5778259323232,-59.8159283829422,
2.62434823201726));
#215040=CARTESIAN_POINT('Ctrl Pts',(19.5824415812281,-59.8128114820617,
2.62679048030261));
#215041=CARTESIAN_POINT('Ctrl Pts',(19.5985963523951,-59.80190232898,2.63533834930135));
#215042=CARTESIAN_POINT('Ctrl Pts',(19.6134170876088,-59.7902699966952,
2.64563784783519));
#215043=CARTESIAN_POINT('Ctrl Pts',(19.6266373778174,-59.7782164291172,
2.65736666737921));
#215044=CARTESIAN_POINT('Ctrl Pts',(19.6332475229217,-59.7721896453281,
2.66323107715121));
#215045=CARTESIAN_POINT('Ctrl Pts',(19.6394575570867,-59.7660575536767,
2.6694528178073));
#215046=CARTESIAN_POINT('Ctrl Pts',(19.6452341819734,-59.7598579055887,
2.67599160631157));
#215047=CARTESIAN_POINT('Ctrl Pts',(19.6481224944167,-59.7567580815447,
2.67926100056371));
#215048=CARTESIAN_POINT('Ctrl Pts',(19.6509024545777,-59.7536413685029,
2.6826096568508));
#215049=CARTESIAN_POINT('Ctrl Pts',(19.6535699003337,-59.7505124858961,
2.68603254012439));
#215050=CARTESIAN_POINT('Ctrl Pts',(19.6562373460896,-59.7473836032892,
2.68945542339799));
#215051=CARTESIAN_POINT('Ctrl Pts',(19.6587921483502,-59.7442425399493,
2.69295261525343));
#215052=CARTESIAN_POINT('Ctrl Pts',(19.6612304091767,-59.7410940396259,
2.69651891172057));
#215053=CARTESIAN_POINT('Ctrl Pts',(19.661251202435,-59.7410671895121,2.69654932476045));
#215054=CARTESIAN_POINT('Ctrl Pts',(19.6612719872243,-59.7410403389968,
2.69657974261104));
#215055=CARTESIAN_POINT('Ctrl Pts',(19.6612927635427,-59.7410134880825,
2.69661016526931));
#215056=CARTESIAN_POINT('Ctrl Pts',(19.6719035326714,-59.7273003341226,
2.71214746100963));
#215057=CARTESIAN_POINT('Ctrl Pts',(19.6804273096576,-59.7135327604159,
2.72880565567262));
#215058=CARTESIAN_POINT('Ctrl Pts',(19.6869782138541,-59.6998755263192,
2.74628040011863));
#215059=CARTESIAN_POINT('Ctrl Pts',(19.6937506652805,-59.685756413634,2.76434612881815));
#215060=CARTESIAN_POINT('Ctrl Pts',(19.6984145359326,-59.6717543328784,
2.7832859265371));
#215061=CARTESIAN_POINT('Ctrl Pts',(19.7010437169731,-59.6580526467606,
2.80278753266961));
#215062=CARTESIAN_POINT('Ctrl Pts',(19.7036228854578,-59.6446115955438,
2.82191817721815));
#215063=CARTESIAN_POINT('Ctrl Pts',(19.7042436449215,-59.6314587768815,
2.84159092314074));
#215064=CARTESIAN_POINT('Ctrl Pts',(19.7029300451616,-59.6187815171233,
2.86151233815839));
#215065=CARTESIAN_POINT('Ctrl Pts',(19.7020598313726,-59.6103832769714,
2.87470957720509));
#215066=CARTESIAN_POINT('Ctrl Pts',(19.7003397858053,-59.6021940468487,
2.88801594387922));
#215067=CARTESIAN_POINT('Ctrl Pts',(19.6977666881852,-59.5942745858232,
2.90134173515983));
#215068=CARTESIAN_POINT('',(19.5876674457085,-59.2554138597567,3.4715307213903));
#215069=CARTESIAN_POINT('',(19.6977666881852,-59.5942745858232,2.90134173515982));
#215070=CARTESIAN_POINT('',(25.0931373005752,-57.1420619865017,3.47153072139032));
#215071=CARTESIAN_POINT('Origin',(5.53234440788222E-15,1.85015204418142E-13,
3.47153072139072));
#215072=CARTESIAN_POINT('',(25.2380597013437,-57.4675553545136,2.90134173515983));
#215073=CARTESIAN_POINT('',(25.0931373005752,-57.1420619865017,3.47153072139032));
#215074=CARTESIAN_POINT('',(25.5918112338801,-57.5176823163884,2.59908173515984));
#215075=CARTESIAN_POINT('Ctrl Pts',(25.2380597013437,-57.4675553545136,
2.90134173515984));
#215076=CARTESIAN_POINT('Ctrl Pts',(25.2430650965697,-57.4787973317373,
2.88164837656666));
#215077=CARTESIAN_POINT('Ctrl Pts',(25.249835715983,-57.4892091890288,2.86203734439068));
#215078=CARTESIAN_POINT('Ctrl Pts',(25.258229540281,-57.4986663319543,2.84277945978062));
#215079=CARTESIAN_POINT('Ctrl Pts',(25.2667920292293,-57.5083135057463,
2.82313460919922));
#215080=CARTESIAN_POINT('Ctrl Pts',(25.2770439485784,-57.5169680778959,
2.80385576863236));
#215081=CARTESIAN_POINT('Ctrl Pts',(25.288886320303,-57.5244844631367,2.78521678518279));
#215082=CARTESIAN_POINT('Ctrl Pts',(25.3002686266216,-57.5317088436247,
2.76730190934361));
#215083=CARTESIAN_POINT('Ctrl Pts',(25.3131208736859,-57.5378823365812,
2.74997687279672));
#215084=CARTESIAN_POINT('Ctrl Pts',(25.3273944332815,-57.5428531464543,
2.73349253345617));
#215085=CARTESIAN_POINT('Ctrl Pts',(25.338358886461,-57.5466715501085,2.72082983599201));
#215086=CARTESIAN_POINT('Ctrl Pts',(25.3501628378345,-57.5497799237791,
2.70866321039216));
#215087=CARTESIAN_POINT('Ctrl Pts',(25.3627976342216,-57.5520966403716,
2.69711645335804));
#215088=CARTESIAN_POINT('Ctrl Pts',(25.3628307477697,-57.5521027120726,
2.6970861913671));
#215089=CARTESIAN_POINT('Ctrl Pts',(25.3628638677137,-57.5521087778601,
2.69705593387177));
#215090=CARTESIAN_POINT('Ctrl Pts',(25.3628969940507,-57.5521148377332,
2.69702568087529));
#215091=CARTESIAN_POINT('Ctrl Pts',(25.3664488110208,-57.5527645793665,
2.69378194443225));
#215092=CARTESIAN_POINT('Ctrl Pts',(25.370072675656,-57.5533450954509,2.69059266624659));
#215093=CARTESIAN_POINT('Ctrl Pts',(25.3737637277669,-57.5538555294213,
2.68746219342636));
#215094=CARTESIAN_POINT('Ctrl Pts',(25.3943035935288,-57.556695978409,2.67004182395796));
#215095=CARTESIAN_POINT('Ctrl Pts',(25.4169233145212,-57.5573711352257,
2.65443567877397));
#215096=CARTESIAN_POINT('Ctrl Pts',(25.4407429579551,-57.5557688601523,
2.6413685235247));
#215097=CARTESIAN_POINT('Ctrl Pts',(25.4514335437862,-57.5550497369108,
2.63550380329293));
#215098=CARTESIAN_POINT('Ctrl Pts',(25.4623660683439,-57.5538721381532,
2.63014997450885));
#215099=CARTESIAN_POINT('Ctrl Pts',(25.4734629846673,-57.5522269397027,
2.62536981119211));
#215100=CARTESIAN_POINT('Ctrl Pts',(25.4782855544065,-57.5515119587087,
2.62329241687031));
#215101=CARTESIAN_POINT('Ctrl Pts',(25.483138990061,-57.5507085716892,2.62132362131385));
#215102=CARTESIAN_POINT('Ctrl Pts',(25.4880168077363,-57.5498159753465,
2.61946873372305));
#215103=CARTESIAN_POINT('Ctrl Pts',(25.5050891695999,-57.5466918881471,
2.61297662715526));
#215104=CARTESIAN_POINT('Ctrl Pts',(25.5224602099127,-57.5424749837903,
2.60787989113927));
#215105=CARTESIAN_POINT('Ctrl Pts',(25.5398519389082,-57.5371308371206,
2.60440616886138));
#215106=CARTESIAN_POINT('Ctrl Pts',(25.5485478034059,-57.5344587637858,
2.60266930772243));
#215107=CARTESIAN_POINT('Ctrl Pts',(25.5572488403194,-57.5315048804291,
2.60133820040144));
#215108=CARTESIAN_POINT('Ctrl Pts',(25.5659203041435,-57.528264891145,2.60044130723544));
#215109=CARTESIAN_POINT('Ctrl Pts',(25.5702560360555,-57.5266448965029,
2.59999286065244));
#215110=CARTESIAN_POINT('Ctrl Pts',(25.5745843747453,-57.5249533754915,
2.59965296768472));
#215111=CARTESIAN_POINT('Ctrl Pts',(25.5789009773107,-57.5231897917608,
2.59942518630914));
#215112=CARTESIAN_POINT('Ctrl Pts',(25.5832175798762,-57.5214262080301,
2.59919740493356));
#215113=CARTESIAN_POINT('Ctrl Pts',(25.5875224456236,-57.5195905600214,
2.5990817379158));
#215114=CARTESIAN_POINT('Ctrl Pts',(25.5918112338801,-57.5176823163884,
2.59908173515984));
#215115=CARTESIAN_POINT('',(25.6197038181304,-57.5052637377727,2.59908173515984));
#215116=CARTESIAN_POINT('Origin',(5.59198795571863E-15,1.8555457506392E-13,
2.59908173516024));
#215117=CARTESIAN_POINT('',(25.8191582032627,-57.2088336324694,2.90134173515984));
#215118=CARTESIAN_POINT('Ctrl Pts',(25.6197038181304,-57.5052637377727,
2.59908173515983));
#215119=CARTESIAN_POINT('Ctrl Pts',(25.623194660701,-57.5037084941749,2.59908174381647));
#215120=CARTESIAN_POINT('Ctrl Pts',(25.6266565153809,-57.5021139114129,
2.59915752000955));
#215121=CARTESIAN_POINT('Ctrl Pts',(25.6300880761872,-57.5004817994255,
2.5993072951743));
#215122=CARTESIAN_POINT('Ctrl Pts',(25.6499182643553,-57.4910502055681,
2.60017281085871));
#215123=CARTESIAN_POINT('Ctrl Pts',(25.6687401163196,-57.4803658667987,
2.60350651799978));
#215124=CARTESIAN_POINT('Ctrl Pts',(25.686294849896,-57.468780099555,2.60896880596317));
#215125=CARTESIAN_POINT('Ctrl Pts',(25.6933750777767,-57.4641072931065,
2.61117187235336));
#215126=CARTESIAN_POINT('Ctrl Pts',(25.7002496417671,-57.4592879447658,
2.61372076577113));
#215127=CARTESIAN_POINT('Ctrl Pts',(25.7069034079257,-57.4543452548719,
2.61659179896943));
#215128=CARTESIAN_POINT('Ctrl Pts',(25.7093582436708,-57.4525217023847,
2.61765103591169));
#215129=CARTESIAN_POINT('Ctrl Pts',(25.7117828918954,-57.4506813499532,
2.61875422455108));
#215130=CARTESIAN_POINT('Ctrl Pts',(25.7141765267655,-57.4488253585218,
2.61990022440354));
#215131=CARTESIAN_POINT('Ctrl Pts',(25.7186645921469,-57.4453453745878,
2.62204897412692));
#215132=CARTESIAN_POINT('Ctrl Pts',(25.7230436262012,-57.4418104097892,
2.6243482320173));
#215133=CARTESIAN_POINT('Ctrl Pts',(25.7273081852392,-57.4382281169308,
2.62679048030265));
#215134=CARTESIAN_POINT('Ctrl Pts',(25.7422341418724,-57.4256900919266,
2.63533834930139));
#215135=CARTESIAN_POINT('Ctrl Pts',(25.7557577777299,-57.4125722940988,
2.64563784783522));
#215136=CARTESIAN_POINT('Ctrl Pts',(25.7676457049096,-57.3992028606057,
2.65736666737924));
#215137=CARTESIAN_POINT('Ctrl Pts',(25.7735896684995,-57.3925181438591,
2.66323107715125));
#215138=CARTESIAN_POINT('Ctrl Pts',(25.7791247053306,-57.3857705191192,
2.66945281780733));
#215139=CARTESIAN_POINT('Ctrl Pts',(25.7842216455743,-57.3790010116299,
2.6759916063116));
#215140=CARTESIAN_POINT('Ctrl Pts',(25.7867701156962,-57.3756162578852,
2.67926100056373));
#215141=CARTESIAN_POINT('Ctrl Pts',(25.7892090617198,-57.37222603356,2.68260965685083));
#215142=CARTESIAN_POINT('Ctrl Pts',(25.7915348376382,-57.3688354672937,
2.68603254012442));
#215143=CARTESIAN_POINT('Ctrl Pts',(25.7938606135566,-57.3654449010275,
2.68945542339802));
#215144=CARTESIAN_POINT('Ctrl Pts',(25.7960730898191,-57.3620539952069,
2.69295261525343));
#215145=CARTESIAN_POINT('Ctrl Pts',(25.7981688856973,-57.3586678750405,
2.69651891172058));
#215146=CARTESIAN_POINT('Ctrl Pts',(25.7981867584468,-57.3586389985271,
2.69654932476046));
#215147=CARTESIAN_POINT('Ctrl Pts',(25.7982046227317,-57.3586101224996,
2.69657974261104));
#215148=CARTESIAN_POINT('Ctrl Pts',(25.7982224785504,-57.3585812469608,
2.69661016526931));
#215149=CARTESIAN_POINT('Ctrl Pts',(25.8073417058679,-57.3438340876984,
2.7121474610134));
#215150=CARTESIAN_POINT('Ctrl Pts',(25.8143796853907,-57.3292509568879,
2.7288056556807));
#215151=CARTESIAN_POINT('Ctrl Pts',(25.8194671333562,-57.3149837825966,
2.74628040013136));
#215152=CARTESIAN_POINT('Ctrl Pts',(25.8247266354337,-57.3002341019445,
2.76434612883568));
#215153=CARTESIAN_POINT('Ctrl Pts',(25.8279013409298,-57.2858212188169,
2.7832859265598));
#215154=CARTESIAN_POINT('Ctrl Pts',(25.8290839028457,-57.2719197677126,
2.80278753269758));
#215155=CARTESIAN_POINT('Ctrl Pts',(25.8302439699455,-57.25828275146,2.82191817725084));
#215156=CARTESIAN_POINT('Ctrl Pts',(25.8294864848991,-57.2451370982795,
2.84159092317825));
#215157=CARTESIAN_POINT('Ctrl Pts',(25.8268549466919,-57.2326665944393,
2.86151233820061));
#215158=CARTESIAN_POINT('Ctrl Pts',(25.825111644888,-57.2244053228451,2.87470957723346));
#215159=CARTESIAN_POINT('Ctrl Pts',(25.8225450142721,-57.2164407479107,
2.88801594389343));
#215160=CARTESIAN_POINT('Ctrl Pts',(25.8191582032627,-57.2088336324694,
2.90134173515983));
#215161=CARTESIAN_POINT('',(25.6742415049986,-56.883337725539,3.47153072139032));
#215162=CARTESIAN_POINT('',(25.8191582032627,-57.2088336324694,2.90134173515984));
#215163=CARTESIAN_POINT('',(30.9286463962985,-54.2060847114736,3.47153072139034));
#215164=CARTESIAN_POINT('Origin',(5.53234440788222E-15,1.85015204418142E-13,
3.47153072139072));
#215165=CARTESIAN_POINT('',(31.1067982185541,-54.5146464769132,2.90134173515985));
#215166=CARTESIAN_POINT('',(30.9286463962985,-54.2060847114736,3.47153072139034));
#215167=CARTESIAN_POINT('',(31.4638515574747,-54.5275217339714,2.59908173515985));
#215168=CARTESIAN_POINT('Ctrl Pts',(31.1067982185541,-54.5146464769132,
2.90134173515985));
#215169=CARTESIAN_POINT('Ctrl Pts',(31.1129513003042,-54.5253036631379,
2.8816483765679));
#215170=CARTESIAN_POINT('Ctrl Pts',(31.1207731649977,-54.5349507607426,
2.86203734439313));
#215171=CARTESIAN_POINT('Ctrl Pts',(31.1301095476641,-54.5434787028944,
2.84277945978422));
#215172=CARTESIAN_POINT('Ctrl Pts',(31.1396335346525,-54.5521780046471,
2.82313460920393));
#215173=CARTESIAN_POINT('Ctrl Pts',(31.1507339420409,-54.5597135487696,
2.80385576863812));
#215174=CARTESIAN_POINT('Ctrl Pts',(31.1632971162117,-54.5659508935477,
2.78521678518951));
#215175=CARTESIAN_POINT('Ctrl Pts',(31.1753722224549,-54.5719459231356,
2.7673019093509));
#215176=CARTESIAN_POINT('Ctrl Pts',(31.1887993692959,-54.5767421714167,
2.74997687280452));
#215177=CARTESIAN_POINT('Ctrl Pts',(31.2035143279548,-54.5801937574236,
2.73349253346437));
#215178=CARTESIAN_POINT('Ctrl Pts',(31.2148178485808,-54.5828451460226,
2.72082983599728));
#215179=CARTESIAN_POINT('Ctrl Pts',(31.2268820501991,-54.5847026428,2.70866321039468));
#215180=CARTESIAN_POINT('Ctrl Pts',(31.2396897946776,-54.5856859723267,
2.69711645335807));
#215181=CARTESIAN_POINT('Ctrl Pts',(31.2397233614918,-54.585688549458,2.69708619136713));
#215182=CARTESIAN_POINT('Ctrl Pts',(31.2397569340488,-54.5856911200396,
2.6970559338718));
#215183=CARTESIAN_POINT('Ctrl Pts',(31.2397905123454,-54.585693684071,2.69702568087532));
#215184=CARTESIAN_POINT('Ctrl Pts',(31.243390788585,-54.585968600382,2.69378194443227));
#215185=CARTESIAN_POINT('Ctrl Pts',(31.2470554817647,-54.5861671393371,
2.69059266624661));
#215186=CARTESIAN_POINT('Ctrl Pts',(31.2507796687845,-54.5862889570918,
2.68746219342638));
#215187=CARTESIAN_POINT('Ctrl Pts',(31.2715039227768,-54.5869668451988,
2.67004182396089));
#215188=CARTESIAN_POINT('Ctrl Pts',(31.2940703036714,-54.5852738987617,
2.6544356787792));
#215189=CARTESIAN_POINT('Ctrl Pts',(31.3175919772508,-54.5811905703965,
2.64136852353127));
#215190=CARTESIAN_POINT('Ctrl Pts',(31.3281488300906,-54.5793579160787,
2.63550380329693));
#215191=CARTESIAN_POINT('Ctrl Pts',(31.3388983725504,-54.577044008338,2.63014997451064));
#215192=CARTESIAN_POINT('Ctrl Pts',(31.3497625287433,-54.5742478788453,
2.62536981119211));
#215193=CARTESIAN_POINT('Ctrl Pts',(31.3544839440763,-54.5730327187882,
2.62329241687031));
#215194=CARTESIAN_POINT('Ctrl Pts',(31.3592268152919,-54.5717264106363,
2.62132362131385));
#215195=CARTESIAN_POINT('Ctrl Pts',(31.3639846100476,-54.5703288332441,
2.61946873372305));
#215196=CARTESIAN_POINT('Ctrl Pts',(31.3806368916926,-54.5654373123713,
2.61297662715526));
#215197=CARTESIAN_POINT('Ctrl Pts',(31.3974719850968,-54.5594277405085,
2.60787989113929));
#215198=CARTESIAN_POINT('Ctrl Pts',(31.4142098249423,-54.552294938928,2.6044061688614));
#215199=CARTESIAN_POINT('Ctrl Pts',(31.422578744865,-54.5487285381377,2.60266930772245));
#215200=CARTESIAN_POINT('Ctrl Pts',(31.4309233516999,-54.5448813304458,
2.60133820040145));
#215201=CARTESIAN_POINT('Ctrl Pts',(31.4392086412369,-54.5407526753742,
2.60044130723545));
#215202=CARTESIAN_POINT('Ctrl Pts',(31.4433512860054,-54.5386883478383,
2.59999286065245));
#215203=CARTESIAN_POINT('Ctrl Pts',(31.4474791015111,-54.5365536585642,
2.59965296768473));
#215204=CARTESIAN_POINT('Ctrl Pts',(31.4515877125788,-54.5343485280971,
2.59942518630915));
#215205=CARTESIAN_POINT('Ctrl Pts',(31.4556963236466,-54.5321433976299,
2.59919740493357));
#215206=CARTESIAN_POINT('Ctrl Pts',(31.4597857294236,-54.5298678244919,
2.59908173791582));
#215207=CARTESIAN_POINT('Ctrl Pts',(31.4638515574747,-54.5275217339714,
2.59908173515985));
#215208=CARTESIAN_POINT('',(31.4902932482914,-54.5122556166605,2.59908173515986));
#215209=CARTESIAN_POINT('Origin',(5.57749365020894E-15,1.8554718984639E-13,
2.59908173516024));
#215210=CARTESIAN_POINT('',(31.6576696180591,-54.1966007261202,2.90134173515985));
#215211=CARTESIAN_POINT('Ctrl Pts',(31.4902932482914,-54.5122556166605,
2.59908173515986));
#215212=CARTESIAN_POINT('Ctrl Pts',(31.4936024004378,-54.5103440004405,
2.59908174381646));
#215213=CARTESIAN_POINT('Ctrl Pts',(31.4968786114299,-54.5083962906199,
2.59915752000958));
#215214=CARTESIAN_POINT('Ctrl Pts',(31.5001207716291,-54.506414423735,2.59930729517433));
#215215=CARTESIAN_POINT('Ctrl Pts',(31.518856457946,-54.4949616780362,2.60017281085903));
#215216=CARTESIAN_POINT('Ctrl Pts',(31.536458384329,-54.482368449926,2.6035065180021));
#215217=CARTESIAN_POINT('Ctrl Pts',(31.552705908797,-54.4690111813986,2.60896880596886));
#215218=CARTESIAN_POINT('Ctrl Pts',(31.5592589091653,-54.4636238877371,
2.61117187235774));
#215219=CARTESIAN_POINT('Ctrl Pts',(31.5655920544933,-54.458112352686,2.61372076577361));
#215220=CARTESIAN_POINT('Ctrl Pts',(31.5716927188404,-54.4525012314179,
2.61659179896944));
#215221=CARTESIAN_POINT('Ctrl Pts',(31.5739434935992,-54.450431068334,2.61765103591169));
#215222=CARTESIAN_POINT('Ctrl Pts',(31.5761624901357,-54.4483473527928,
2.61875422455109));
#215223=CARTESIAN_POINT('Ctrl Pts',(31.5783490084913,-54.446251325702,2.61990022440356));
#215224=CARTESIAN_POINT('Ctrl Pts',(31.5824487304082,-54.4423212749068,
2.62204897412693));
#215225=CARTESIAN_POINT('Ctrl Pts',(31.5864342712176,-54.4383479413149,
2.62434823201731));
#215226=CARTESIAN_POINT('Ctrl Pts',(31.5903010169876,-54.4343395048289,
2.62679048030266));
#215227=CARTESIAN_POINT('Ctrl Pts',(31.6038346271824,-54.4203099771278,
2.6353383493014));
#215228=CARTESIAN_POINT('Ctrl Pts',(31.6159129958993,-54.4058504350952,
2.64563784783522));
#215229=CARTESIAN_POINT('Ctrl Pts',(31.6263383134323,-54.391311613998,2.65736666737924));
#215230=CARTESIAN_POINT('Ctrl Pts',(31.6315509721988,-54.3840422034495,
2.66323107715124));
#215231=CARTESIAN_POINT('Ctrl Pts',(31.6363503686743,-54.3767529740098,
2.66945281780734));
#215232=CARTESIAN_POINT('Ctrl Pts',(31.6407117811311,-54.3694877752597,
2.67599160631161));
#215233=CARTESIAN_POINT('Ctrl Pts',(31.6428924873595,-54.3658551758847,
2.67926100056374));
#215234=CARTESIAN_POINT('Ctrl Pts',(31.6449636976428,-54.3622285842833,
2.68260965685083));
#215235=CARTESIAN_POINT('Ctrl Pts',(31.6469223220359,-54.3586134821111,
2.68603254012442));
#215236=CARTESIAN_POINT('Ctrl Pts',(31.648880946429,-54.3549983799389,2.68945542339802));
#215237=CARTESIAN_POINT('Ctrl Pts',(31.6507268563406,-54.3513947831115,
2.69295261525345));
#215238=CARTESIAN_POINT('Ctrl Pts',(31.6524572252922,-54.3478081421432,
2.69651891172059));
#215239=CARTESIAN_POINT('Ctrl Pts',(31.6524719817154,-54.3477775556074,
2.69654932476047));
#215240=CARTESIAN_POINT('Ctrl Pts',(31.6524867297711,-54.3477469704395,
2.69657974261105));
#215241=CARTESIAN_POINT('Ctrl Pts',(31.6525014694581,-54.3477163866426,
2.69661016526933));
#215242=CARTESIAN_POINT('Ctrl Pts',(31.6600292427972,-54.3320967950475,
2.71214746100997));
#215243=CARTESIAN_POINT('Ctrl Pts',(31.6655043152777,-54.3168578829727,
2.72880565567334));
#215244=CARTESIAN_POINT('Ctrl Pts',(31.6690725678672,-54.3021370826402,
2.74628040011975));
#215245=CARTESIAN_POINT('Ctrl Pts',(31.6727614963898,-54.2869184346153,
2.76434612881985));
#215246=CARTESIAN_POINT('Ctrl Pts',(31.6744122539934,-54.2722526596854,
2.78328592653942));
#215247=CARTESIAN_POINT('Ctrl Pts',(31.674135240392,-54.2583037508073,2.80278753267255));
#215248=CARTESIAN_POINT('Ctrl Pts',(31.6738634961721,-54.2446201795274,
2.82191817722171));
#215249=CARTESIAN_POINT('Ctrl Pts',(31.6717360657848,-54.23162571836,2.84159092314493));
#215250=CARTESIAN_POINT('Ctrl Pts',(31.6678154208197,-54.2194985998906,
2.86151233816319));
#215251=CARTESIAN_POINT('Ctrl Pts',(31.6652181309801,-54.2114648090569,
2.87470957720832));
#215252=CARTESIAN_POINT('Ctrl Pts',(31.6618330358543,-54.2038121508437,
2.88801594388085));
#215253=CARTESIAN_POINT('Ctrl Pts',(31.6576696180591,-54.1966007261202,
2.90134173515986));
#215254=CARTESIAN_POINT('',(31.4795232016796,-53.8880358395965,3.47153072139034));
#215255=CARTESIAN_POINT('',(31.6576696180591,-54.1966007261202,2.90134173515985));
#215256=CARTESIAN_POINT('',(36.4252947698685,-50.6762142289942,3.47153072139037));
#215257=CARTESIAN_POINT('Origin',(5.53234440788222E-15,1.85015204418142E-13,
3.47153072139072));
#215258=CARTESIAN_POINT('',(36.634724144966,-50.9644637245887,2.90134173515987));
#215259=CARTESIAN_POINT('',(36.4252947698685,-50.6762142289942,3.47153072139037));
#215260=CARTESIAN_POINT('',(36.9911673391713,-50.9399462128196,2.59908173515987));
#215261=CARTESIAN_POINT('Ctrl Pts',(36.634724144966,-50.9644637245887,2.90134173515987));
#215262=CARTESIAN_POINT('Ctrl Pts',(36.6419574987901,-50.9744193574537,
2.88164837656548));
#215263=CARTESIAN_POINT('Ctrl Pts',(36.6507449107794,-50.9831959997529,
2.8620373443883));
#215264=CARTESIAN_POINT('Ctrl Pts',(36.6609215604541,-50.9907013072134,
2.8427794597771));
#215265=CARTESIAN_POINT('Ctrl Pts',(36.6713026986907,-50.9983574255574,
2.82313460919437));
#215266=CARTESIAN_POINT('Ctrl Pts',(36.683129975735,-51.0046913806552,2.80385576862625));
#215267=CARTESIAN_POINT('Ctrl Pts',(36.6962763075901,-51.0095813473161,
2.78521678517554));
#215268=CARTESIAN_POINT('Ctrl Pts',(36.7089119163701,-51.0142813432051,
2.76730190933505));
#215269=CARTESIAN_POINT('Ctrl Pts',(36.7227668523605,-51.0176477981104,
2.74997687278699));
#215270=CARTESIAN_POINT('Ctrl Pts',(36.7377619899201,-51.0195423439515,
2.73349253344545));
#215271=CARTESIAN_POINT('Ctrl Pts',(36.7492807342482,-51.0209976683241,
2.72082983598517));
#215272=CARTESIAN_POINT('Ctrl Pts',(36.7614730081857,-51.0215839370833,
2.70866321038893));
#215273=CARTESIAN_POINT('Ctrl Pts',(36.7743133764177,-51.0212231059799,
2.69711645335807));
#215274=CARTESIAN_POINT('Ctrl Pts',(36.7743470287329,-51.0212221603059,
2.69708619136713));
#215275=CARTESIAN_POINT('Ctrl Pts',(36.7743806860749,-51.0212212075178,
2.69705593387181));
#215276=CARTESIAN_POINT('Ctrl Pts',(36.7744143484403,-51.0212202476155,
2.69702568087533));
#215277=CARTESIAN_POINT('Ctrl Pts',(36.7780236385695,-51.0211173265635,
2.69378194443228));
#215278=CARTESIAN_POINT('Ctrl Pts',(36.7816890091485,-51.0209317131549,
2.69059266624663));
#215279=CARTESIAN_POINT('Ctrl Pts',(36.7854055281047,-51.0206635800331,
2.68746219342639));
#215280=CARTESIAN_POINT('Ctrl Pts',(36.806087111073,-51.0191714801756,2.67004182395614));
#215281=CARTESIAN_POINT('Ctrl Pts',(36.8283529098889,-51.015128978758,2.65443567877069));
#215282=CARTESIAN_POINT('Ctrl Pts',(36.851318905247,-51.0086093348969,2.64136852352057));
#215283=CARTESIAN_POINT('Ctrl Pts',(36.8616263619967,-51.0056832284481,
2.63550380329042));
#215284=CARTESIAN_POINT('Ctrl Pts',(36.8720751481116,-51.0022583633838,
2.63014997450773));
#215285=CARTESIAN_POINT('Ctrl Pts',(36.8825875141948,-50.9983419378318,
2.62536981119211));
#215286=CARTESIAN_POINT('Ctrl Pts',(36.8871560463072,-50.9966399122595,
2.62329241687032));
#215287=CARTESIAN_POINT('Ctrl Pts',(36.8917363891943,-50.9948449951607,
2.62132362131386));
#215288=CARTESIAN_POINT('Ctrl Pts',(36.8963220336354,-50.9929577488693,
2.61946873372307));
#215289=CARTESIAN_POINT('Ctrl Pts',(36.9123717891793,-50.9863523868494,
2.61297662715528));
#215290=CARTESIAN_POINT('Ctrl Pts',(36.9284864868687,-50.9786159896075,
2.60787989113931));
#215291=CARTESIAN_POINT('Ctrl Pts',(36.9443870542882,-50.9697726815829,
2.60440616886143));
#215292=CARTESIAN_POINT('Ctrl Pts',(36.9523373379979,-50.9653510275706,
2.60266930772248));
#215293=CARTESIAN_POINT('Ctrl Pts',(36.9602340894955,-50.960652646356,2.60133820040148));
#215294=CARTESIAN_POINT('Ctrl Pts',(36.9680424293796,-50.9556805599057,
2.60044130723547));
#215295=CARTESIAN_POINT('Ctrl Pts',(36.9719465993216,-50.9531945166806,
2.59999286065247));
#215296=CARTESIAN_POINT('Ctrl Pts',(36.9758286664326,-50.9506400472463,
2.59965296768476));
#215297=CARTESIAN_POINT('Ctrl Pts',(36.9796842712,-50.9480175299135,2.59942518630919));
#215298=CARTESIAN_POINT('Ctrl Pts',(36.9835398759674,-50.9453950125807,
2.59919740493361));
#215299=CARTESIAN_POINT('Ctrl Pts',(36.9873690173885,-50.9427044459688,
2.59908173791584));
#215300=CARTESIAN_POINT('Ctrl Pts',(36.9911673391713,-50.9399462128196,
2.59908173515988));
#215301=CARTESIAN_POINT('',(37.0158684358566,-50.9219998155894,2.59908173515989));
#215302=CARTESIAN_POINT('Origin',(5.56385071146069E-15,1.85538330018374E-13,
2.59908173516024));
#215303=CARTESIAN_POINT('',(37.1493329797267,-50.5905785208478,2.90134173515988));
#215304=CARTESIAN_POINT('Ctrl Pts',(37.0158684358566,-50.9219998155894,
2.59908173515989));
#215305=CARTESIAN_POINT('Ctrl Pts',(37.0189596418154,-50.9197527708144,
2.59908174381647));
#215306=CARTESIAN_POINT('Ctrl Pts',(37.0220143142664,-50.9174732734517,
2.5991575200096));
#215307=CARTESIAN_POINT('Ctrl Pts',(37.025031552073,-50.9151633654177,2.59930729517435));
#215308=CARTESIAN_POINT('Ctrl Pts',(37.0424674644288,-50.9018149465613,
2.60017281085891));
#215309=CARTESIAN_POINT('Ctrl Pts',(37.058656614833,-50.8874508031597,2.60350651800102));
#215310=CARTESIAN_POINT('Ctrl Pts',(37.0734189189074,-50.8724683783849,
2.60896880596616));
#215311=CARTESIAN_POINT('Ctrl Pts',(37.0793728957291,-50.8664256218212,
2.61117187235567));
#215312=CARTESIAN_POINT('Ctrl Pts',(37.0850952351376,-50.8602822855845,
2.61372076577245));
#215313=CARTESIAN_POINT('Ctrl Pts',(37.090575957526,-50.8540642095541,2.61659179896946));
#215314=CARTESIAN_POINT('Ctrl Pts',(37.0925980113393,-50.8517701170135,
2.61765103591172));
#215315=CARTESIAN_POINT('Ctrl Pts',(37.0945870443972,-50.849465867986,2.61875422455113));
#215316=CARTESIAN_POINT('Ctrl Pts',(37.0965424902857,-50.8471527697473,
2.61990022440359));
#215317=CARTESIAN_POINT('Ctrl Pts',(37.1002089513267,-50.8428157105498,
2.62204897412696));
#215318=CARTESIAN_POINT('Ctrl Pts',(37.1037573324722,-50.8384475408389,
2.62434823201734));
#215319=CARTESIAN_POINT('Ctrl Pts',(37.1071839000983,-50.8340568779942,
2.62679048030269));
#215320=CARTESIAN_POINT('Ctrl Pts',(37.1191768867895,-50.8186895580377,
2.63533834930143));
#215321=CARTESIAN_POINT('Ctrl Pts',(37.1296776552305,-50.8030466935685,
2.64563784783527));
#215322=CARTESIAN_POINT('Ctrl Pts',(37.1385261411562,-50.7874977752337,
2.65736666737928));
#215323=CARTESIAN_POINT('Ctrl Pts',(37.1429503841191,-50.7797233160663,
2.66323107715129));
#215324=CARTESIAN_POINT('Ctrl Pts',(37.1469615570468,-50.7719723442501,
2.66945281780737));
#215325=CARTESIAN_POINT('Ctrl Pts',(37.1505396571691,-50.7642910532771,
2.67599160631164));
#215326=CARTESIAN_POINT('Ctrl Pts',(37.1523287072303,-50.7604504077907,
2.67926100056378));
#215327=CARTESIAN_POINT('Ctrl Pts',(37.15400948916,-50.7566271826095,2.68260965685087));
#215328=CARTESIAN_POINT('Ctrl Pts',(37.1555795029291,-50.7528271523473,
2.68603254012446));
#215329=CARTESIAN_POINT('Ctrl Pts',(37.1571495166982,-50.7490271220852,
2.68945542339806));
#215330=CARTESIAN_POINT('Ctrl Pts',(37.1586086360836,-50.7452503160119,
2.69295261525348));
#215331=CARTESIAN_POINT('Ctrl Pts',(37.1599546198243,-50.7415024502306,
2.69651891172063));
#215332=CARTESIAN_POINT('Ctrl Pts',(37.1599660982467,-50.7414704887848,
2.69654932476051));
#215333=CARTESIAN_POINT('Ctrl Pts',(37.1599775684904,-50.7414385295741,
2.69657974261109));
#215334=CARTESIAN_POINT('Ctrl Pts',(37.1599890305545,-50.7414065726016,
2.69661016526937));
#215335=CARTESIAN_POINT('Ctrl Pts',(37.1658428740579,-50.7250856801833,
2.71214746101124));
#215336=CARTESIAN_POINT('Ctrl Pts',(37.1696950534575,-50.7093579475494,
2.72880565567602));
#215337=CARTESIAN_POINT('Ctrl Pts',(37.171705016149,-50.6943448053406,2.74628040012395));
#215338=CARTESIAN_POINT('Ctrl Pts',(37.173782954444,-50.6788239286313,2.76434612882549));
#215339=CARTESIAN_POINT('Ctrl Pts',(37.1738916781082,-50.6640659431946,
2.78328592654661));
#215340=CARTESIAN_POINT('Ctrl Pts',(37.1721581240063,-50.6502224037042,
2.80278753268133));
#215341=CARTESIAN_POINT('Ctrl Pts',(37.1704575457512,-50.6366421974646,
2.82191817723184));
#215342=CARTESIAN_POINT('Ctrl Pts',(37.1669834785924,-50.6239412983438,
2.84159092315645));
#215343=CARTESIAN_POINT('Ctrl Pts',(37.1618166822721,-50.6122904324912,
2.86151233817606));
#215344=CARTESIAN_POINT('Ctrl Pts',(37.1583938608486,-50.6045721423226,
2.87470957721698));
#215345=CARTESIAN_POINT('Ctrl Pts',(37.1542273890263,-50.5973152449659,
2.88801594388519));
#215346=CARTESIAN_POINT('Ctrl Pts',(37.1493329797266,-50.5905785208478,
2.90134173515986));
#215347=CARTESIAN_POINT('',(36.9399086546492,-50.3023253561989,3.47153072139037));
#215348=CARTESIAN_POINT('',(37.1493329797266,-50.5905785208478,2.90134173515989));
#215349=CARTESIAN_POINT('',(41.5228599914568,-46.5911245387423,3.4715307213904));
#215350=CARTESIAN_POINT('Origin',(5.53234440788222E-15,1.85015204418142E-13,
3.47153072139072));
#215351=CARTESIAN_POINT('',(41.7612723673368,-46.8559036426978,2.90134173515992));
#215352=CARTESIAN_POINT('',(41.5228599914568,-46.5911245387423,3.4715307213904));
#215353=CARTESIAN_POINT('',(42.1132001506006,-46.794261981091,2.59908173515991));
#215354=CARTESIAN_POINT('Ctrl Pts',(41.7612723673369,-46.8559036426978,
2.90134173515992));
#215355=CARTESIAN_POINT('Ctrl Pts',(41.7695067430959,-46.8650486462041,
2.88164837656661));
#215356=CARTESIAN_POINT('Ctrl Pts',(41.7791634256545,-46.8728586744666,
2.86203734439051));
#215357=CARTESIAN_POINT('Ctrl Pts',(41.7900688448321,-46.8792591175156,
2.84277945978033));
#215358=CARTESIAN_POINT('Ctrl Pts',(41.8011933963914,-46.8857881704151,
2.82313460919898));
#215359=CARTESIAN_POINT('Ctrl Pts',(41.8136179609662,-46.8908511403499,
2.80385576863217));
#215360=CARTESIAN_POINT('Ctrl Pts',(41.8272034165389,-46.8943401533956,
2.78521678518265));
#215361=CARTESIAN_POINT('Ctrl Pts',(41.8402610894779,-46.8976936214472,
2.76730190934385));
#215362=CARTESIAN_POINT('Ctrl Pts',(41.8543920170353,-46.899593399393,2.74997687279733));
#215363=CARTESIAN_POINT('Ctrl Pts',(41.8695030436256,-46.899910148029,2.73349253345709));
#215364=CARTESIAN_POINT('Ctrl Pts',(41.8811108098904,-46.9001534633397,
2.72082983599264));
#215365=CARTESIAN_POINT('Ctrl Pts',(41.8932975750515,-46.899462080799,2.7086632103925));
#215366=CARTESIAN_POINT('Ctrl Pts',(41.906029885286,-46.8977610424066,2.69711645335812));
#215367=CARTESIAN_POINT('Ctrl Pts',(41.9060632544005,-46.8977565842883,
2.69708619136718));
#215368=CARTESIAN_POINT('Ctrl Pts',(41.9060966277705,-46.8977521185695,
2.69705593387185));
#215369=CARTESIAN_POINT('Ctrl Pts',(41.9061300053929,-46.8977476452502,
2.69702568087537));
#215370=CARTESIAN_POINT('Ctrl Pts',(41.9097087652737,-46.8972680144598,
2.69378194443233));
#215371=CARTESIAN_POINT('Ctrl Pts',(41.9133346546847,-46.896700282307,2.69059266624667));
#215372=CARTESIAN_POINT('Ctrl Pts',(41.9170027866181,-46.8960451360313,
2.68746219342645));
#215373=CARTESIAN_POINT('Ctrl Pts',(41.9374151068032,-46.8923993959678,
2.67004182395839));
#215374=CARTESIAN_POINT('Ctrl Pts',(41.9591363747797,-46.8860516300634,
2.65443567877468));
#215375=CARTESIAN_POINT('Ctrl Pts',(41.9812950716555,-46.8771671012931,
2.64136852352558));
#215376=CARTESIAN_POINT('Ctrl Pts',(41.9912402016709,-46.8731796017465,
2.63550380329351));
#215377=CARTESIAN_POINT('Ctrl Pts',(42.0012737523628,-46.8686813028947,
2.63014997450917));
#215378=CARTESIAN_POINT('Ctrl Pts',(42.011319152663,-46.8636874904583,2.62536981119221));
#215379=CARTESIAN_POINT('Ctrl Pts',(42.015684747761,-46.861517247119,2.62329241687041));
#215380=CARTESIAN_POINT('Ctrl Pts',(42.0200523791245,-46.8592533865607,
2.62132362131396));
#215381=CARTESIAN_POINT('Ctrl Pts',(42.0244156319709,-46.8568971484354,
2.61946873372316));
#215382=CARTESIAN_POINT('Ctrl Pts',(42.0396870169334,-46.848650314997,2.61297662715536));
#215383=CARTESIAN_POINT('Ctrl Pts',(42.0549047629078,-46.8392718539632,
2.60787989113937));
#215384=CARTESIAN_POINT('Ctrl Pts',(42.0697938479572,-46.8288149286278,
2.60440616886147));
#215385=CARTESIAN_POINT('Ctrl Pts',(42.0772383904819,-46.8235864659601,
2.60266930772252));
#215386=CARTESIAN_POINT('Ctrl Pts',(42.0846007681804,-46.8180883876704,
2.60133820040152));
#215387=CARTESIAN_POINT('Ctrl Pts',(42.0918466086057,-46.8123273450613,
2.60044130723551));
#215388=CARTESIAN_POINT('Ctrl Pts',(42.0954695288184,-46.8094468237567,
2.59999286065251));
#215389=CARTESIAN_POINT('Ctrl Pts',(42.0990633147952,-46.8065005614637,
2.59965296768479));
#215390=CARTESIAN_POINT('Ctrl Pts',(42.1026236704495,-46.803489390114,2.59942518630921));
#215391=CARTESIAN_POINT('Ctrl Pts',(42.1061840261039,-46.8004782187642,
2.59919740493363));
#215392=CARTESIAN_POINT('Ctrl Pts',(42.1097109502944,-46.7974021370894,
2.59908173791584));
#215393=CARTESIAN_POINT('Ctrl Pts',(42.1132001506006,-46.794261981091,2.59908173515992));
#215394=CARTESIAN_POINT('',(42.1358900227701,-46.773831928425,2.59908173515991));
#215395=CARTESIAN_POINT('Origin',(5.55120861436579E-15,1.8552809265E-13,
2.59908173516023));
#215396=CARTESIAN_POINT('',(42.2339804752707,-46.4302753505418,2.90134173515992));
#215397=CARTESIAN_POINT('Ctrl Pts',(42.1358900227701,-46.773831928425,2.59908173515991));
#215398=CARTESIAN_POINT('Ctrl Pts',(42.138729414642,-46.771274074188,2.59908174381655));
#215399=CARTESIAN_POINT('Ctrl Pts',(42.1415290809214,-46.7686877639332,
2.59915752000963));
#215400=CARTESIAN_POINT('Ctrl Pts',(42.1442883388465,-46.7660751225859,
2.59930729517438));
#215401=CARTESIAN_POINT('Ctrl Pts',(42.1602334457314,-46.7509772786485,
2.60017281085848));
#215402=CARTESIAN_POINT('Ctrl Pts',(42.1748324484328,-46.734999596523,2.60350651799748));
#215403=CARTESIAN_POINT('Ctrl Pts',(42.1879477932176,-46.7185561660889,
2.60896880595744));
#215404=CARTESIAN_POINT('Ctrl Pts',(42.1932375134815,-46.7119241523218,
2.61117187234895));
#215405=CARTESIAN_POINT('Ctrl Pts',(42.1982863518268,-46.7052163225703,
2.61372076576869));
#215406=CARTESIAN_POINT('Ctrl Pts',(42.203087084319,-46.6984594183132,2.6165917989695));
#215407=CARTESIAN_POINT('Ctrl Pts',(42.2048582631421,-46.6959665308738,
2.61765103591176));
#215408=CARTESIAN_POINT('Ctrl Pts',(42.2065955404589,-46.6934669941947,
2.61875422455116));
#215409=CARTESIAN_POINT('Ctrl Pts',(42.208298489606,-46.6909621675965,2.61990022440363));
#215410=CARTESIAN_POINT('Ctrl Pts',(42.2114915192568,-46.6862656177247,
2.622048974127));
#215411=CARTESIAN_POINT('Ctrl Pts',(42.2145638639319,-46.6815504704764,
2.62434823201736));
#215412=CARTESIAN_POINT('Ctrl Pts',(42.2175127112221,-46.6768256862939,
2.62679048030272));
#215413=CARTESIAN_POINT('Ctrl Pts',(42.2278336767378,-46.6602889416552,
2.63533834930145));
#215414=CARTESIAN_POINT('Ctrl Pts',(42.2366417962865,-46.643634141246,2.6456378478353));
#215415=CARTESIAN_POINT('Ctrl Pts',(42.2438165047415,-46.6272454828767,
2.65736666737931));
#215416=CARTESIAN_POINT('Ctrl Pts',(42.247403858969,-46.6190511536921,2.66323107715132));
#215417=CARTESIAN_POINT('Ctrl Pts',(42.2505828610989,-46.6109233607684,
2.66945281780741));
#215418=CARTESIAN_POINT('Ctrl Pts',(42.253338446473,-46.6029101354039,2.67599160631168));
#215419=CARTESIAN_POINT('Ctrl Pts',(42.2547162391601,-46.5989035227217,
2.67926100056381));
#215420=CARTESIAN_POINT('Ctrl Pts',(42.2559881777376,-46.5949255520158,
2.6826096568509));
#215421=CARTESIAN_POINT('Ctrl Pts',(42.2571523794834,-46.5909822275905,
2.6860325401245));
#215422=CARTESIAN_POINT('Ctrl Pts',(42.2583165812292,-46.5870389031651,
2.68945542339809));
#215423=CARTESIAN_POINT('Ctrl Pts',(42.2593729236709,-46.5831302673236,
2.69295261525354));
#215424=CARTESIAN_POINT('Ctrl Pts',(42.2603197753212,-46.5792622391313,
2.69651891172068));
#215425=CARTESIAN_POINT('Ctrl Pts',(42.2603278499828,-46.5792292529517,
2.69654932476056));
#215426=CARTESIAN_POINT('Ctrl Pts',(42.2603359167441,-46.57919626985,2.69657974261114));
#215427=CARTESIAN_POINT('Ctrl Pts',(42.2603439756046,-46.5791632898291,
2.69661016526942));
#215428=CARTESIAN_POINT('Ctrl Pts',(42.264459753338,-46.562319911698,2.71214746101455));
#215429=CARTESIAN_POINT('Ctrl Pts',(42.266646834373,-46.5462756748331,2.72880565568302));
#215430=CARTESIAN_POINT('Ctrl Pts',(42.2670764855939,-46.531134677874,2.74628040013495));
#215431=CARTESIAN_POINT('Ctrl Pts',(42.2675206673338,-46.5154816224519,
2.76434612884054));
#215432=CARTESIAN_POINT('Ctrl Pts',(42.2660861658583,-46.5007931180837,
2.78328592656602));
#215433=CARTESIAN_POINT('Ctrl Pts',(42.2629150644359,-46.4872066206955,
2.80278753270522));
#215434=CARTESIAN_POINT('Ctrl Pts',(42.2598042840353,-46.4738785670766,
2.82191817725999));
#215435=CARTESIAN_POINT('Ctrl Pts',(42.25502164271,-46.4616103837102,2.84159092318895));
#215436=CARTESIAN_POINT('Ctrl Pts',(42.2486653035341,-46.4505634197984,
2.86151233821282));
#215437=CARTESIAN_POINT('Ctrl Pts',(42.2444544516768,-46.4432451935021,
2.87470957724171));
#215438=CARTESIAN_POINT('Ctrl Pts',(42.2395522518982,-46.436463565092,2.88801594389761));
#215439=CARTESIAN_POINT('Ctrl Pts',(42.2339804752707,-46.4302753505418,
2.90134173515992));
#215440=CARTESIAN_POINT('',(41.9955727382257,-46.1654920697605,3.4715307213904));
#215441=CARTESIAN_POINT('',(42.2339804752707,-46.4302753505418,2.90134173515992));
#215442=CARTESIAN_POINT('',(46.1654920697617,-41.9955727382244,3.47153072139043));
#215443=CARTESIAN_POINT('Origin',(5.53234440788222E-15,1.85015204418142E-13,
3.47153072139072));
#215444=CARTESIAN_POINT('',(46.430275350543,-42.2339804752694,2.90134173515995));
#215445=CARTESIAN_POINT('',(46.1654920697617,-41.9955727382244,3.47153072139043));
#215446=CARTESIAN_POINT('',(46.7738319284262,-42.1358900227688,2.59908173515994));
#215447=CARTESIAN_POINT('Ctrl Pts',(46.430275350543,-42.2339804752694,2.90134173515995));
#215448=CARTESIAN_POINT('Ctrl Pts',(46.4394205306929,-42.2422146548451,
2.88164837656735));
#215449=CARTESIAN_POINT('Ctrl Pts',(46.449840683186,-42.2489725007674,2.86203734439194));
#215450=CARTESIAN_POINT('Ctrl Pts',(46.4613553898119,-42.2541979548116,
2.84277945978242));
#215451=CARTESIAN_POINT('Ctrl Pts',(46.4731014717795,-42.259528408597,2.82313460920183));
#215452=CARTESIAN_POINT('Ctrl Pts',(46.4859871977557,-42.2632649224111,
2.80385576863575));
#215453=CARTESIAN_POINT('Ctrl Pts',(46.4998629319526,-42.2653147554846,
2.78521678518688));
#215454=CARTESIAN_POINT('Ctrl Pts',(46.5131996064543,-42.2672849544014,
2.76730190934884));
#215455=CARTESIAN_POINT('Ctrl Pts',(46.5274517041803,-42.2676972410231,
2.749976872803));
#215456=CARTESIAN_POINT('Ctrl Pts',(46.5425130602331,-42.2664327220894,
2.73349253346334));
#215457=CARTESIAN_POINT('Ctrl Pts',(46.554082671317,-42.265461362524,2.72082983599665));
#215458=CARTESIAN_POINT('Ctrl Pts',(46.5661304069508,-42.2634999036146,
2.70866321039442));
#215459=CARTESIAN_POINT('Ctrl Pts',(46.5786151613305,-42.2604772948653,
2.69711645335815));
#215460=CARTESIAN_POINT('Ctrl Pts',(46.5786478816452,-42.2604693731468,
2.69708619136721));
#215461=CARTESIAN_POINT('Ctrl Pts',(46.5786806053978,-42.2604614434245,
2.69705593387188));
#215462=CARTESIAN_POINT('Ctrl Pts',(46.5787133325848,-42.260453505699,2.6970256808754));
#215463=CARTESIAN_POINT('Ctrl Pts',(46.5822223525751,-42.2596024201055,
2.69378194443235));
#215464=CARTESIAN_POINT('Ctrl Pts',(46.5857690348151,-42.2586587894008,
2.69059266624671));
#215465=CARTESIAN_POINT('Ctrl Pts',(46.5893485909045,-42.2576238078908,
2.68746219342648));
#215466=CARTESIAN_POINT('Ctrl Pts',(46.6092680066585,-42.2518643711119,
2.67004182395757));
#215467=CARTESIAN_POINT('Ctrl Pts',(46.6302067610422,-42.2432808881709,
2.65443567877319));
#215468=CARTESIAN_POINT('Ctrl Pts',(46.6513153841198,-42.2321288152456,
2.64136852352369));
#215469=CARTESIAN_POINT('Ctrl Pts',(46.6607892264715,-42.2271236104816,
2.63550380329236));
#215470=CARTESIAN_POINT('Ctrl Pts',(46.6702976120556,-42.2216011621472,
2.63014997450866));
#215471=CARTESIAN_POINT('Ctrl Pts',(46.6797659870611,-42.2155846760822,
2.62536981119222));
#215472=CARTESIAN_POINT('Ctrl Pts',(46.6838808147712,-42.2129699926162,
2.62329241687042));
#215473=CARTESIAN_POINT('Ctrl Pts',(46.6879878819279,-42.2102619919283,
2.62132362131396));
#215474=CARTESIAN_POINT('Ctrl Pts',(46.6920809384683,-42.2074625774071,
2.61946873372316));
#215475=CARTESIAN_POINT('Ctrl Pts',(46.7064066363599,-42.1976646265831,
2.61297662715537));
#215476=CARTESIAN_POINT('Ctrl Pts',(46.72056070181,-42.186746854139,2.60787989113939));
#215477=CARTESIAN_POINT('Ctrl Pts',(46.7342751765578,-42.174790879755,2.60440616886149));
#215478=CARTESIAN_POINT('Ctrl Pts',(46.7411324139317,-42.168812892563,2.60266930772254));
#215479=CARTESIAN_POINT('Ctrl Pts',(46.7478797540803,-42.1625753552947,
2.60133820040155));
#215480=CARTESIAN_POINT('Ctrl Pts',(46.7544837081028,-42.156088475715,2.60044130723554));
#215481=CARTESIAN_POINT('Ctrl Pts',(46.7577856851141,-42.1528450359252,
2.59999286065254));
#215482=CARTESIAN_POINT('Ctrl Pts',(46.7610518156854,-42.1495392606399,
2.59965296768483));
#215483=CARTESIAN_POINT('Ctrl Pts',(46.7642779142252,-42.1461724262966,
2.59942518630925));
#215484=CARTESIAN_POINT('Ctrl Pts',(46.7675040127649,-42.1428055919533,
2.59919740493367));
#215485=CARTESIAN_POINT('Ctrl Pts',(46.7706900780053,-42.1393776974101,
2.59908173791585));
#215486=CARTESIAN_POINT('Ctrl Pts',(46.7738319284262,-42.1358900227688,
2.59908173515995));
#215487=CARTESIAN_POINT('',(46.7942619810922,-42.1132001505994,2.59908173515994));
#215488=CARTESIAN_POINT('Origin',(5.53970586838553E-15,1.8551658990402E-13,
2.59908173516022));
#215489=CARTESIAN_POINT('',(46.855903642699,-41.7612723673355,2.90134173515995));
#215490=CARTESIAN_POINT('Ctrl Pts',(46.7942619810922,-42.1132001505994,
2.59908173515994));
#215491=CARTESIAN_POINT('Ctrl Pts',(46.7968184499057,-42.1103595112864,
2.59908174381654));
#215492=CARTESIAN_POINT('Ctrl Pts',(46.7993324362838,-42.107494724296,2.59915752000967));
#215493=CARTESIAN_POINT('Ctrl Pts',(46.8018034833201,-42.1046079742807,
2.59930729517442));
#215494=CARTESIAN_POINT('Ctrl Pts',(46.8160830868215,-42.0879261203861,
2.60017281085887));
#215495=CARTESIAN_POINT('Ctrl Pts',(46.828931992104,-42.0705099543501,2.6035065180002));
#215496=CARTESIAN_POINT('Ctrl Pts',(46.840256683147,-42.0527856759055,2.60896880596406));
#215497=CARTESIAN_POINT('Ctrl Pts',(46.8448241915573,-42.0456370666804,
2.61117187235407));
#215498=CARTESIAN_POINT('Ctrl Pts',(46.8491442126976,-42.0384382358158,
2.61372076577158));
#215499=CARTESIAN_POINT('Ctrl Pts',(46.8532123574524,-42.0312165334044,
2.61659179896954));
#215500=CARTESIAN_POINT('Ctrl Pts',(46.8547132558794,-42.0285521636627,
2.61765103591179));
#215501=CARTESIAN_POINT('Ctrl Pts',(46.8561797434814,-42.0258847247789,
2.6187542245512));
#215502=CARTESIAN_POINT('Ctrl Pts',(46.8576115380198,-42.0232156132254,
2.61990022440366));
#215503=CARTESIAN_POINT('Ctrl Pts',(46.8602961527793,-42.0182110290628,
2.62204897412703));
#215504=CARTESIAN_POINT('Ctrl Pts',(46.8628587997329,-42.0132005644169,
2.6243482320174));
#215505=CARTESIAN_POINT('Ctrl Pts',(46.8652976184992,-42.0081934246209,
2.62679048030275));
#215506=CARTESIAN_POINT('Ctrl Pts',(46.8738334841813,-41.9906684353348,
2.63533834930149));
#215507=CARTESIAN_POINT('Ctrl Pts',(46.8808524512368,-41.9731841724641,
2.64563784783532));
#215508=CARTESIAN_POINT('Ctrl Pts',(46.8862747746138,-41.956135331631,2.65736666737934));
#215509=CARTESIAN_POINT('Ctrl Pts',(46.8889859363023,-41.9476109112144,
2.66323107715134));
#215510=CARTESIAN_POINT('Ctrl Pts',(46.8912979378218,-41.9391953469834,
2.66945281780743));
#215511=CARTESIAN_POINT('Ctrl Pts',(46.8932008176778,-41.9309379818013,
2.6759916063117));
#215512=CARTESIAN_POINT('Ctrl Pts',(46.8941522576058,-41.9268092992103,
2.67926100056383));
#215513=CARTESIAN_POINT('Ctrl Pts',(46.8950014172059,-41.9227201664594,
2.68260965685093));
#215514=CARTESIAN_POINT('Ctrl Pts',(46.8957470516903,-41.9186767517584,
2.68603254012452));
#215515=CARTESIAN_POINT('Ctrl Pts',(46.8964926861748,-41.9146333370574,
2.68945542339811));
#215516=CARTESIAN_POINT('Ctrl Pts',(46.8971346781641,-41.9106356952798,
2.69295261525355));
#215517=CARTESIAN_POINT('Ctrl Pts',(46.8976720238192,-41.9066898836027,
2.69651891172069));
#215518=CARTESIAN_POINT('Ctrl Pts',(46.8976766062523,-41.9066562340929,
2.69654932476057));
#215519=CARTESIAN_POINT('Ctrl Pts',(46.8976811811501,-41.9066225884699,
2.69657974261115));
#215520=CARTESIAN_POINT('Ctrl Pts',(46.8976857485125,-41.9065889467368,
2.69661016526943));
#215521=CARTESIAN_POINT('Ctrl Pts',(46.9000183671521,-41.8894076224748,
2.71214746101187));
#215522=CARTESIAN_POINT('Ctrl Pts',(46.9005163877047,-41.8732226654011,
2.7288056556773));
#215523=CARTESIAN_POINT('Ctrl Pts',(46.8993610201076,-41.858119701628,2.74628040012593));
#215524=CARTESIAN_POINT('Ctrl Pts',(46.8981665787456,-41.8425059656487,
2.76434612882826));
#215525=CARTESIAN_POINT('Ctrl Pts',(46.8952045688313,-41.8280478726808,
2.78328592655023));
#215526=CARTESIAN_POINT('Ctrl Pts',(46.890630663343,-41.8148672739068,2.80278753268583));
#215527=CARTESIAN_POINT('Ctrl Pts',(46.8861437631615,-41.8019373978561,
2.8219181772373));
#215528=CARTESIAN_POINT('Ctrl Pts',(46.8801049472937,-41.7902363430306,
2.84159092316289));
#215529=CARTESIAN_POINT('Ctrl Pts',(46.8726287066499,-41.7799143139093,
2.86151233818347));
#215530=CARTESIAN_POINT('Ctrl Pts',(46.8676759593283,-41.7730763314901,
2.87470957722199));
#215531=CARTESIAN_POINT('Ctrl Pts',(46.8620917411132,-41.7668442729545,
2.88801594388774));
#215532=CARTESIAN_POINT('Ctrl Pts',(46.855903642699,-41.7612723673355,2.90134173515995));
#215533=CARTESIAN_POINT('',(46.5911245387435,-41.5228599914555,3.47153072139043));
#215534=CARTESIAN_POINT('',(46.855903642699,-41.7612723673355,2.90134173515995));
#215535=CARTESIAN_POINT('',(50.3023253562,-36.9399086546478,3.47153072139046));
#215536=CARTESIAN_POINT('Origin',(5.53234440788222E-15,1.85015204418142E-13,
3.47153072139072));
#215537=CARTESIAN_POINT('',(50.5905785208489,-37.1493329797253,2.90134173515998));
#215538=CARTESIAN_POINT('',(50.3023253562,-36.9399086546478,3.47153072139047));
#215539=CARTESIAN_POINT('',(50.9219998155904,-37.0158684358552,2.59908173515998));
#215540=CARTESIAN_POINT('Ctrl Pts',(50.5905785208489,-37.1493329797253,
2.90134173515998));
#215541=CARTESIAN_POINT('Ctrl Pts',(50.6005343088832,-37.1565661199774,
2.88164837656534));
#215542=CARTESIAN_POINT('Ctrl Pts',(50.6116037659411,-37.162197743186,2.86203734438791));
#215543=CARTESIAN_POINT('Ctrl Pts',(50.6236016024818,-37.1661909570578,
2.84277945977646));
#215544=CARTESIAN_POINT('Ctrl Pts',(50.6358405223277,-37.1702644101623,
2.82313460919363));
#215545=CARTESIAN_POINT('Ctrl Pts',(50.6490462309976,-37.172633529828,2.80385576862541));
#215546=CARTESIAN_POINT('Ctrl Pts',(50.6630602183739,-37.1732217245284,
2.78521678517463));
#215547=CARTESIAN_POINT('Ctrl Pts',(50.6765297750448,-37.1737870683979,
2.76730190933408));
#215548=CARTESIAN_POINT('Ctrl Pts',(50.690746893978,-37.1727073465953,2.74997687278597));
#215549=CARTESIAN_POINT('Ctrl Pts',(50.7055935641283,-37.1698754144239,
2.7334925334444));
#215550=CARTESIAN_POINT('Ctrl Pts',(50.7169982609442,-37.1677000224006,
2.72082983598454));
#215551=CARTESIAN_POINT('Ctrl Pts',(50.7287749695304,-37.1644899772777,
2.7086632103887));
#215552=CARTESIAN_POINT('Ctrl Pts',(50.7408753824657,-37.1601789145079,
2.69711645335819));
#215553=CARTESIAN_POINT('Ctrl Pts',(50.7409070954901,-37.1601676159812,
2.69708619136725));
#215554=CARTESIAN_POINT('Ctrl Pts',(50.7409388110967,-37.1601563091353,
2.69705593387192));
#215555=CARTESIAN_POINT('Ctrl Pts',(50.7409705292826,-37.1601449939709,
2.69702568087544));
#215556=CARTESIAN_POINT('Ctrl Pts',(50.744371363825,-37.1589317782461,2.6937819444324));
#215557=CARTESIAN_POINT('Ctrl Pts',(50.7477999807011,-37.1576225876049,
2.69059266624673));
#215558=CARTESIAN_POINT('Ctrl Pts',(50.751251742581,-37.1562191103348,2.6874621934265));
#215559=CARTESIAN_POINT('Ctrl Pts',(50.7704600126089,-37.1484090784378,
2.67004182396362));
#215560=CARTESIAN_POINT('Ctrl Pts',(50.7903868440168,-37.1376839209007,
2.65443567878399));
#215561=CARTESIAN_POINT('Ctrl Pts',(50.8102141227966,-37.1243864882722,
2.64136852353726));
#215562=CARTESIAN_POINT('Ctrl Pts',(50.8191128800932,-37.1184184163576,
2.63550380330065));
#215563=CARTESIAN_POINT('Ctrl Pts',(50.8279919247152,-37.111932323635,2.6301499745124));
#215564=CARTESIAN_POINT('Ctrl Pts',(50.8367795369359,-37.104959081816,2.6253698111923));
#215565=CARTESIAN_POINT('Ctrl Pts',(50.8405985143445,-37.1019286052424,
2.62329241687049));
#215566=CARTESIAN_POINT('Ctrl Pts',(50.8444000194072,-37.0988061338472,
2.62132362131403));
#215567=CARTESIAN_POINT('Ctrl Pts',(50.8481780352577,-37.0955942139014,
2.61946873372323));
#215568=CARTESIAN_POINT('Ctrl Pts',(50.8614010907345,-37.0843524940913,
2.61297662715543));
#215569=CARTESIAN_POINT('Ctrl Pts',(50.8743364007572,-37.0720150276365,
2.60787989113944));
#215570=CARTESIAN_POINT('Ctrl Pts',(50.8867260065482,-37.0586909963613,
2.60440616886155));
#215571=CARTESIAN_POINT('Ctrl Pts',(50.8929208094436,-37.0520289807237,
2.6026693077226));
#215572=CARTESIAN_POINT('Ctrl Pts',(50.8989791867717,-37.0451203242403,
2.6013382004016));
#215573=CARTESIAN_POINT('Ctrl Pts',(50.9048689000892,-37.0379786793002,
2.6004413072356));
#215574=CARTESIAN_POINT('Ctrl Pts',(50.907813756748,-37.0344078568301,2.59999286065259));
#215575=CARTESIAN_POINT('Ctrl Pts',(50.9107164475038,-37.0307787873183,
2.59965296768487));
#215576=CARTESIAN_POINT('Ctrl Pts',(50.9135729431182,-37.0270931777231,
2.59942518630929));
#215577=CARTESIAN_POINT('Ctrl Pts',(50.9164294387326,-37.0234075681279,
2.59919740493371));
#215578=CARTESIAN_POINT('Ctrl Pts',(50.9192397378254,-37.0196654174462,
2.59908173791591));
#215579=CARTESIAN_POINT('Ctrl Pts',(50.9219998155904,-37.0158684358552,
2.59908173515998));
#215580=CARTESIAN_POINT('',(50.9399462128206,-36.9911673391699,2.59908173515998));
#215581=CARTESIAN_POINT('Origin',(5.52946850001198E-15,1.85503947806925E-13,
2.59908173516023));
#215582=CARTESIAN_POINT('',(50.9644637245897,-36.6347241449646,2.90134173515999));
#215583=CARTESIAN_POINT('Ctrl Pts',(50.9399462128206,-36.9911673391699,
2.59908173515998));
#215584=CARTESIAN_POINT('Ctrl Pts',(50.9421917493684,-36.9880750374199,
2.59908174381653));
#215585=CARTESIAN_POINT('Ctrl Pts',(50.9443925120844,-36.9849631608996,
2.5991575200097));
#215586=CARTESIAN_POINT('Ctrl Pts',(50.9465482749236,-36.9818339300535,
2.59930729517445));
#215587=CARTESIAN_POINT('Ctrl Pts',(50.9590059247082,-36.9637508360938,
2.60017281085871));
#215588=CARTESIAN_POINT('Ctrl Pts',(50.9699639572693,-36.945087001318,2.60350651799879));
#215589=CARTESIAN_POINT('Ctrl Pts',(50.9793739188802,-36.9262760657776,
2.60896880596056));
#215590=CARTESIAN_POINT('Ctrl Pts',(50.983169172867,-36.9186891827427,2.61117187235137));
#215591=CARTESIAN_POINT('Ctrl Pts',(50.9867130457539,-36.9110782226516,
2.61372076577008));
#215592=CARTESIAN_POINT('Ctrl Pts',(50.9900040313326,-36.9034708445581,
2.61659179896957));
#215593=CARTESIAN_POINT('Ctrl Pts',(50.9912182052063,-36.9006641839065,
2.61765103591182));
#215594=CARTESIAN_POINT('Ctrl Pts',(50.9923978359483,-36.8978580678366,
2.61875422455123));
#215595=CARTESIAN_POINT('Ctrl Pts',(50.9935427888375,-36.8950539146727,
2.6199002244037));
#215596=CARTESIAN_POINT('Ctrl Pts',(50.9956895755046,-36.8897961274904,
2.62204897412707));
#215597=CARTESIAN_POINT('Ctrl Pts',(50.9977144478404,-36.8845452411461,
2.62434823201743));
#215598=CARTESIAN_POINT('Ctrl Pts',(50.9996165178741,-36.879310605008,2.62679048030278));
#215599=CARTESIAN_POINT('Ctrl Pts',(51.006273762992,-36.8609893785245,2.63533834930152));
#215600=CARTESIAN_POINT('Ctrl Pts',(51.0114266762823,-36.8428672144352,
2.64563784783535));
#215601=CARTESIAN_POINT('Ctrl Pts',(51.0150372064717,-36.8253449818061,
2.65736666737937));
#215602=CARTESIAN_POINT('Ctrl Pts',(51.0168424715664,-36.8165838654915,
2.66323107715138));
#215603=CARTESIAN_POINT('Ctrl Pts',(51.0182621417031,-36.807972732636,2.66945281780747));
#215604=CARTESIAN_POINT('Ctrl Pts',(51.019291467691,-36.7995616970572,2.67599160631174));
#215605=CARTESIAN_POINT('Ctrl Pts',(51.019806130685,-36.7953561792679,2.67926100056388));
#215606=CARTESIAN_POINT('Ctrl Pts',(51.0202232077374,-36.7912006858659,
2.68260965685096));
#215607=CARTESIAN_POINT('Ctrl Pts',(51.0205421056331,-36.7871014813869,
2.68603254012456));
#215608=CARTESIAN_POINT('Ctrl Pts',(51.0208610035287,-36.7830022769079,
2.68945542339815));
#215609=CARTESIAN_POINT('Ctrl Pts',(51.0210816112671,-36.7789594281942,
2.6929526152536));
#215610=CARTESIAN_POINT('Ctrl Pts',(51.0212035636555,-36.7749790641708,
2.69651891172074));
#215611=CARTESIAN_POINT('Ctrl Pts',(51.021204603654,-36.7749451200018,2.69654932476061));
#215612=CARTESIAN_POINT('Ctrl Pts',(51.0212056365647,-36.774911180486,2.6965797426112));
#215613=CARTESIAN_POINT('Ctrl Pts',(51.0212066623879,-36.7748772456265,
2.69661016526947));
#215614=CARTESIAN_POINT('Ctrl Pts',(51.0217305652766,-36.7575462174142,
2.71214746101235));
#215615=CARTESIAN_POINT('Ctrl Pts',(51.0205340689296,-36.7413978659053,
2.72880565567827));
#215616=CARTESIAN_POINT('Ctrl Pts',(51.017806340963,-36.7264984065469,2.74628040012743));
#215617=CARTESIAN_POINT('Ctrl Pts',(51.0149863630479,-36.711095057367,2.76434612882988));
#215618=CARTESIAN_POINT('Ctrl Pts',(51.0105292970941,-36.6970257816896,
2.78328592655197));
#215619=CARTESIAN_POINT('Ctrl Pts',(51.0046027002038,-36.6843954909265,
2.80278753268768));
#215620=CARTESIAN_POINT('Ctrl Pts',(50.9987888396572,-36.6720054548709,
2.8219181772387));
#215621=CARTESIAN_POINT('Ctrl Pts',(50.9915600117752,-36.660999727791,2.84159092316381));
#215622=CARTESIAN_POINT('Ctrl Pts',(50.9830457809182,-36.6515157237711,
2.8615123381839));
#215623=CARTESIAN_POINT('Ctrl Pts',(50.9774054014705,-36.6452329036017,
2.87470957722229));
#215624=CARTESIAN_POINT('Ctrl Pts',(50.9712003466852,-36.6396186946836,
2.88801594388792));
#215625=CARTESIAN_POINT('Ctrl Pts',(50.9644637245897,-36.6347241449646,
2.90134173515999));
#215626=CARTESIAN_POINT('',(50.6762142289952,-36.4252947698671,3.47153072139047));
#215627=CARTESIAN_POINT('',(50.9644637245897,-36.6347241449646,2.90134173515999));
#215628=CARTESIAN_POINT('',(53.8880358395974,-31.4795232016781,3.4715307213905));
#215629=CARTESIAN_POINT('Origin',(5.53234440788222E-15,1.85015204418142E-13,
3.47153072139072));
#215630=CARTESIAN_POINT('',(54.1966007261211,-31.6576696180576,2.90134173516002));
#215631=CARTESIAN_POINT('',(53.8880358395974,-31.4795232016781,3.4715307213905));
#215632=CARTESIAN_POINT('',(54.5122556166615,-31.4902932482899,2.59908173516002));
#215633=CARTESIAN_POINT('Ctrl Pts',(54.1966007261211,-31.6576696180576,
2.90134173516003));
#215634=CARTESIAN_POINT('Ctrl Pts',(54.2072580443422,-31.6638224711865,
2.88164837656537));
#215635=CARTESIAN_POINT('Ctrl Pts',(54.2188555266759,-31.6682661704385,
2.86203734438793));
#215636=CARTESIAN_POINT('Ctrl Pts',(54.2312050423222,-31.6709833936507,
2.84277945977648));
#215637=CARTESIAN_POINT('Ctrl Pts',(54.2438027078777,-31.6737552164693,
2.82313460919376));
#215638=CARTESIAN_POINT('Ctrl Pts',(54.2571837147316,-31.674730985416,2.80385576862566));
#215639=CARTESIAN_POINT('Ctrl Pts',(54.2711824151068,-31.6738510973596,
2.78521678517498));
#215640=CARTESIAN_POINT('Ctrl Pts',(54.2846372786624,-31.6730053921566,
2.76730190933489));
#215641=CARTESIAN_POINT('Ctrl Pts',(54.2986636530693,-31.6704454915891,
2.74997687278722));
#215642=CARTESIAN_POINT('Ctrl Pts',(54.3131329740888,-31.6660771734233,
2.73349253344603));
#215643=CARTESIAN_POINT('Ctrl Pts',(54.3242478043974,-31.6627215829929,
2.72082983598559));
#215644=CARTESIAN_POINT('Ctrl Pts',(54.3356244578585,-31.658298121582,2.70866321038921));
#215645=CARTESIAN_POINT('Ctrl Pts',(54.3472079546998,-31.6527458376959,
2.69711645335823));
#215646=CARTESIAN_POINT('Ctrl Pts',(54.3472383129792,-31.65273128615,2.69708619136728));
#215647=CARTESIAN_POINT('Ctrl Pts',(54.3472686729573,-31.6527167260605,
2.69705593387196));
#215648=CARTESIAN_POINT('Ctrl Pts',(54.3472990346309,-31.6527021574285,
2.69702568087547));
#215649=CARTESIAN_POINT('Ctrl Pts',(54.3505544234705,-31.6511401038179,
2.69378194443243));
#215650=CARTESIAN_POINT('Ctrl Pts',(54.3538274103387,-31.6494796970068,
2.69059266624677));
#215651=CARTESIAN_POINT('Ctrl Pts',(54.3571135597836,-31.6477231007671,
2.68746219342654));
#215652=CARTESIAN_POINT('Ctrl Pts',(54.3754002342682,-31.637948042093,2.67004182396181));
#215653=CARTESIAN_POINT('Ctrl Pts',(54.394096820175,-31.6251987170246,2.65443567878073));
#215654=CARTESIAN_POINT('Ctrl Pts',(54.4124255228509,-31.6099016141395,
2.64136852353315));
#215655=CARTESIAN_POINT('Ctrl Pts',(54.4206516984361,-31.6030360625235,
2.63550380329814));
#215656=CARTESIAN_POINT('Ctrl Pts',(54.4288041214158,-31.5956573884075,
2.63014997451128));
#215657=CARTESIAN_POINT('Ctrl Pts',(54.436814691924,-31.5878037911374,2.62536981119229));
#215658=CARTESIAN_POINT('Ctrl Pts',(54.4402959775156,-31.5843907239917,
2.62329241687049));
#215659=CARTESIAN_POINT('Ctrl Pts',(54.4437502703992,-31.5808879923392,
2.62132362131404));
#215660=CARTESIAN_POINT('Ctrl Pts',(54.4471718528276,-31.577298757436,2.61946873372324));
#215661=CARTESIAN_POINT('Ctrl Pts',(54.4591473913267,-31.5647364352745,
2.61297662715544));
#215662=CARTESIAN_POINT('Ctrl Pts',(54.4707222239585,-31.5511144466733,
2.60787989113945));
#215663=CARTESIAN_POINT('Ctrl Pts',(54.4816512176788,-31.5365683393817,
2.60440616886156));
#215664=CARTESIAN_POINT('Ctrl Pts',(54.487115714539,-31.5292952857359,2.60266930772261));
#215665=CARTESIAN_POINT('Ctrl Pts',(54.4924187521967,-31.5217912027236,
2.60133820040162));
#215666=CARTESIAN_POINT('Ctrl Pts',(54.4975296958776,-31.5140730377796,
2.60044130723562));
#215667=CARTESIAN_POINT('Ctrl Pts',(54.5000851677181,-31.5102139553076,
2.59999286065261));
#215668=CARTESIAN_POINT('Ctrl Pts',(54.5025926161711,-31.5063013524142,
2.5996529676849));
#215669=CARTESIAN_POINT('Ctrl Pts',(54.5050482124964,-31.5023373478771,
2.59942518630932));
#215670=CARTESIAN_POINT('Ctrl Pts',(54.5075038088218,-31.49837334334,2.59919740493374));
#215671=CARTESIAN_POINT('Ctrl Pts',(54.5099075515421,-31.4943579363058,
2.59908173791587));
#215672=CARTESIAN_POINT('Ctrl Pts',(54.5122556166615,-31.4902932482899,
2.59908173516002));
#215673=CARTESIAN_POINT('',(54.5275217339723,-31.4638515574732,2.59908173516003));
#215674=CARTESIAN_POINT('Origin',(5.52060867199534E-15,1.85490304868177E-13,
2.59908173516022));
#215675=CARTESIAN_POINT('',(54.5146464769142,-31.1067982185526,2.90134173516002));
#215676=CARTESIAN_POINT('Ctrl Pts',(54.5275217339724,-31.4638515574732,
2.59908173516003));
#215677=CARTESIAN_POINT('Ctrl Pts',(54.5294317356861,-31.4605414731911,
2.59908174381663));
#215678=CARTESIAN_POINT('Ctrl Pts',(54.5312951627231,-31.4572166015113,
2.59915752000975));
#215679=CARTESIAN_POINT('Ctrl Pts',(54.5331120223763,-31.4538791743424,
2.5993072951745));
#215680=CARTESIAN_POINT('Ctrl Pts',(54.5436112298312,-31.434592962472,2.60017281085893));
#215681=CARTESIAN_POINT('Ctrl Pts',(54.552558331177,-31.414885943828,2.60350651800011));
#215682=CARTESIAN_POINT('Ctrl Pts',(54.5599504658498,-31.3951944477304,
2.60896880596372));
#215683=CARTESIAN_POINT('Ctrl Pts',(54.5629318838118,-31.3872524143714,
2.61117187235382));
#215684=CARTESIAN_POINT('Ctrl Pts',(54.5656607810285,-31.3793127123329,
2.61372076577147));
#215685=CARTESIAN_POINT('Ctrl Pts',(54.5681385507011,-31.3714030065911,
2.6165917989696));
#215686=CARTESIAN_POINT('Ctrl Pts',(54.5690526972785,-31.3684848053911,
2.61765103591185));
#215687=CARTESIAN_POINT('Ctrl Pts',(54.5699325468793,-31.3655707565299,
2.61875422455126));
#215688=CARTESIAN_POINT('Ctrl Pts',(54.5707781137758,-31.3626622846444,
2.61990022440373));
#215689=CARTESIAN_POINT('Ctrl Pts',(54.5723635517066,-31.3572088998592,
2.6220489741271));
#215690=CARTESIAN_POINT('Ctrl Pts',(54.5738284644995,-31.3517751216261,
2.62434823201746));
#215691=CARTESIAN_POINT('Ctrl Pts',(54.5751729463232,-31.3463703409148,
2.62679048030281));
#215692=CARTESIAN_POINT('Ctrl Pts',(54.5798786327063,-31.3274536084252,
2.63533834930155));
#215693=CARTESIAN_POINT('Ctrl Pts',(54.5831090358351,-31.3088920933393,
2.64563784783539));
#215694=CARTESIAN_POINT('Ctrl Pts',(54.5848682151126,-31.2910884461616,
2.65736666737941));
#215695=CARTESIAN_POINT('Ctrl Pts',(54.5857478047514,-31.2821866225728,
2.66323107715142));
#215696=CARTESIAN_POINT('Ctrl Pts',(54.5862595893022,-31.2734742664663,
2.66945281780751));
#215697=CARTESIAN_POINT('Ctrl Pts',(54.5864040839111,-31.2650017135568,
2.67599160631178));
#215698=CARTESIAN_POINT('Ctrl Pts',(54.5864763312156,-31.260765437102,2.67926100056391));
#215699=CARTESIAN_POINT('Ctrl Pts',(54.5864567561368,-31.2565891115044,
2.68260965685101));
#215700=CARTESIAN_POINT('Ctrl Pts',(54.5863454235316,-31.2524790289895,
2.6860325401246));
#215701=CARTESIAN_POINT('Ctrl Pts',(54.5862340909264,-31.2483689464745,
2.6894554233982));
#215702=CARTESIAN_POINT('Ctrl Pts',(54.5860308973892,-31.2443251851212,
2.69295261525362));
#215703=CARTESIAN_POINT('Ctrl Pts',(54.5857361203751,-31.2403538784526,
2.69651891172076));
#215704=CARTESIAN_POINT('Ctrl Pts',(54.5857336065445,-31.2403200115239,
2.69654932476065));
#215705=CARTESIAN_POINT('Ctrl Pts',(54.5857310861515,-31.2402861499638,
2.69657974261123));
#215706=CARTESIAN_POINT('Ctrl Pts',(54.5857285591964,-31.2402522937752,
2.69661016526951));
#215707=CARTESIAN_POINT('Ctrl Pts',(54.5844380063444,-31.2229614439857,
2.71214746101182));
#215708=CARTESIAN_POINT('Ctrl Pts',(54.5815601021622,-31.207026622761,2.7288056556771));
#215709=CARTESIAN_POINT('Ctrl Pts',(54.5772898993847,-31.192493909413,2.74628040012557));
#215710=CARTESIAN_POINT('Ctrl Pts',(54.5728752811848,-31.1774697093497,
2.76434612882767));
#215711=CARTESIAN_POINT('Ctrl Pts',(54.566971991739,-31.1639433968916,2.78328592654939));
#215712=CARTESIAN_POINT('Ctrl Pts',(54.5597576364827,-31.1520017942483,
2.80278753268472));
#215713=CARTESIAN_POINT('Ctrl Pts',(54.5526805134439,-31.1402873460149,
2.82191817723584));
#215714=CARTESIAN_POINT('Ctrl Pts',(54.5443408740986,-31.130097527729,2.84159092316106));
#215715=CARTESIAN_POINT('Ctrl Pts',(54.5348819367233,-31.1215554575426,
2.86151233818129));
#215716=CARTESIAN_POINT('Ctrl Pts',(54.5286157223268,-31.1158966355148,
2.87470957722054));
#215717=CARTESIAN_POINT('Ctrl Pts',(54.5218578148499,-31.1109617866612,
2.88801594388705));
#215718=CARTESIAN_POINT('Ctrl Pts',(54.5146464769142,-31.1067982185526,
2.90134173516002));
#215719=CARTESIAN_POINT('',(54.2060847114746,-30.928646396297,3.47153072139051));
#215720=CARTESIAN_POINT('',(54.5146464769142,-31.1067982185526,2.90134173516002));
#215721=CARTESIAN_POINT('',(56.8833377255397,-25.6742415049971,3.47153072139054));
#215722=CARTESIAN_POINT('Origin',(5.53234440788222E-15,1.85015204418142E-13,
3.47153072139072));
#215723=CARTESIAN_POINT('',(57.2088336324702,-25.8191582032612,2.90134173516006));
#215724=CARTESIAN_POINT('',(56.8833377255398,-25.6742415049971,3.47153072139054));
#215725=CARTESIAN_POINT('',(57.5052637377735,-25.6197038181289,2.59908173516006));
#215726=CARTESIAN_POINT('Ctrl Pts',(57.2088336324702,-25.8191582032612,
2.90134173516006));
#215727=CARTESIAN_POINT('Ctrl Pts',(57.220075717068,-25.8241633573203,2.88164837656754));
#215728=CARTESIAN_POINT('Ctrl Pts',(57.2320741602326,-25.8273704465165,
2.86203734439222));
#215729=CARTESIAN_POINT('Ctrl Pts',(57.2446400511053,-25.8287819086033,
2.84277945978278));
#215730=CARTESIAN_POINT('Ctrl Pts',(57.257458439709,-25.8302217324655,2.82313460920208));
#215731=CARTESIAN_POINT('Ctrl Pts',(57.2708681396342,-25.829793459965,2.80385576863588));
#215732=CARTESIAN_POINT('Ctrl Pts',(57.284698180316,-25.8274551293905,2.78521678518692));
#215733=CARTESIAN_POINT('Ctrl Pts',(57.2979909364545,-25.8252076408391,
2.76730190934833));
#215734=CARTESIAN_POINT('Ctrl Pts',(57.3116728904409,-25.8211956083142,
2.74997687280199));
#215735=CARTESIAN_POINT('Ctrl Pts',(57.3256063334194,-25.8153387643633,
2.73349253346188));
#215736=CARTESIAN_POINT('Ctrl Pts',(57.3363095208179,-25.8108397400758,
2.72082983599576));
#215737=CARTESIAN_POINT('Ctrl Pts',(57.3471614741618,-25.8052513267441,
2.70866321039406));
#215738=CARTESIAN_POINT('Ctrl Pts',(57.3581011436977,-25.7985186537232,
2.69711645335827));
#215739=CARTESIAN_POINT('Ctrl Pts',(57.3581298146206,-25.7985010085879,
2.69708619136733));
#215740=CARTESIAN_POINT('Ctrl Pts',(57.3581584863397,-25.7984833547782,
2.697055933872));
#215741=CARTESIAN_POINT('Ctrl Pts',(57.3581871588522,-25.7984656922957,
2.69702568087553));
#215742=CARTESIAN_POINT('Ctrl Pts',(57.3612614352676,-25.7965719149855,
2.69378194443248));
#215743=CARTESIAN_POINT('Ctrl Pts',(57.364342932599,-25.7945784837689,2.69059266624683));
#215744=CARTESIAN_POINT('Ctrl Pts',(57.3674274658679,-25.7924880141957,
2.68746219342659));
#215745=CARTESIAN_POINT('Ctrl Pts',(57.3845921921775,-25.7808550263318,
2.67004182395904));
#215746=CARTESIAN_POINT('Ctrl Pts',(57.4018536888761,-25.766221218004,2.65443567877572));
#215747=CARTESIAN_POINT('Ctrl Pts',(57.4184830023465,-25.7490920431211,
2.64136852352685));
#215748=CARTESIAN_POINT('Ctrl Pts',(57.4259464685184,-25.7414042322251,
2.63550380329434));
#215749=CARTESIAN_POINT('Ctrl Pts',(57.433282950203,-25.7332138190148,2.63014997450962));
#215750=CARTESIAN_POINT('Ctrl Pts',(57.4404287135114,-25.7245659119503,
2.62536981119236));
#215751=CARTESIAN_POINT('Ctrl Pts',(57.4435341655926,-25.7208076485105,
2.62329241687056));
#215752=CARTESIAN_POINT('Ctrl Pts',(57.4466034003415,-25.7169630332617,
2.6213236213141));
#215753=CARTESIAN_POINT('Ctrl Pts',(57.4496310617745,-25.7130358078096,
2.6194687337233));
#215754=CARTESIAN_POINT('Ctrl Pts',(57.4602278767901,-25.6992905187273,
2.6129766271555));
#215755=CARTESIAN_POINT('Ctrl Pts',(57.4703154157425,-25.6845332533373,
2.60787989113952));
#215756=CARTESIAN_POINT('Ctrl Pts',(57.47966405705,-25.6689244402248,2.60440616886163));
#215757=CARTESIAN_POINT('Ctrl Pts',(57.4843383777038,-25.6611200336685,
2.60266930772268));
#215758=CARTESIAN_POINT('Ctrl Pts',(57.4888279745008,-25.6531027404311,
2.60133820040167));
#215759=CARTESIAN_POINT('Ctrl Pts',(57.4931041519767,-25.6448926173134,
2.60044130723566));
#215760=CARTESIAN_POINT('Ctrl Pts',(57.4952422407146,-25.6407875557545,
2.59999286065266));
#215761=CARTESIAN_POINT('Ctrl Pts',(57.4973269747348,-25.6366342867756,
2.59965296768494));
#215762=CARTESIAN_POINT('Ctrl Pts',(57.4993547677439,-25.6324353177599,
2.59942518630936));
#215763=CARTESIAN_POINT('Ctrl Pts',(57.501382560753,-25.6282363487441,2.59919740493378));
#215764=CARTESIAN_POINT('Ctrl Pts',(57.5033534111924,-25.6239916789971,
2.599081737916));
#215765=CARTESIAN_POINT('Ctrl Pts',(57.5052637377735,-25.6197038181289,
2.59908173516006));
#215766=CARTESIAN_POINT('',(57.5176823163891,-25.5918112338785,2.59908173516007));
#215767=CARTESIAN_POINT('Origin',(5.5132234544654E-15,1.85475810562667E-13,
2.59908173516024));
#215768=CARTESIAN_POINT('',(57.4675553545143,-25.2380597013421,2.90134173516006));
#215769=CARTESIAN_POINT('Ctrl Pts',(57.5176823163891,-25.5918112338785,
2.59908173516007));
#215770=CARTESIAN_POINT('Ctrl Pts',(57.5192358568904,-25.5883196330406,
2.59908174381659));
#215771=CARTESIAN_POINT('Ctrl Pts',(57.5207415321518,-25.5848181941911,
2.59915752000978));
#215772=CARTESIAN_POINT('Ctrl Pts',(57.5221995827245,-25.5813091362499,
2.59930729517453));
#215773=CARTESIAN_POINT('Ctrl Pts',(57.5306253163349,-25.5610311102414,
2.60017281085912));
#215774=CARTESIAN_POINT('Ctrl Pts',(57.53746346015,-25.5404968219493,2.60350651800139));
#215775=CARTESIAN_POINT('Ctrl Pts',(57.5427567781094,-25.5201405094463,
2.60896880596683));
#215776=CARTESIAN_POINT('Ctrl Pts',(57.5448916950085,-25.5119303403429,
2.61117187235623));
#215777=CARTESIAN_POINT('Ctrl Pts',(57.5467757181868,-25.5037488853943,
2.61372076577285));
#215778=CARTESIAN_POINT('Ctrl Pts',(57.548413124991,-25.4956235123957,2.61659179896965));
#215779=CARTESIAN_POINT('Ctrl Pts',(57.5490172286909,-25.4926257430702,
2.61765103591191));
#215780=CARTESIAN_POINT('Ctrl Pts',(57.5495876573342,-25.4896356883469,
2.61875422455132));
#215781=CARTESIAN_POINT('Ctrl Pts',(57.5501245740301,-25.4866547635665,
2.61990022440379));
#215782=CARTESIAN_POINT('Ctrl Pts',(57.5511312928348,-25.4810655296032,
2.62204897412716));
#215783=CARTESIAN_POINT('Ctrl Pts',(57.5520201961937,-25.4755083930928,
2.62434823201752));
#215784=CARTESIAN_POINT('Ctrl Pts',(57.5527923593833,-25.4699926837168,
2.62679048030287));
#215785=CARTESIAN_POINT('Ctrl Pts',(57.5554949305468,-25.4506877009008,
2.63533834930161));
#215786=CARTESIAN_POINT('Ctrl Pts',(57.5567674305414,-25.4318901986619,
2.64563784783545));
#215787=CARTESIAN_POINT('Ctrl Pts',(57.5566559849708,-25.4140001974198,
2.65736666737946));
#215788=CARTESIAN_POINT('Ctrl Pts',(57.5566002621854,-25.4050551967988,
2.66323107715147));
#215789=CARTESIAN_POINT('Ctrl Pts',(57.5561985539316,-25.396337071838,2.66945281780755));
#215790=CARTESIAN_POINT('Ctrl Pts',(57.5554566340484,-25.3878958286604,
2.67599160631182));
#215791=CARTESIAN_POINT('Ctrl Pts',(57.5550856741068,-25.3836752070716,
2.67926100056396));
#215792=CARTESIAN_POINT('Ctrl Pts',(57.5546296613655,-25.3795238059755,
2.68260965685105));
#215793=CARTESIAN_POINT('Ctrl Pts',(57.5540893180428,-25.3754478763487,
2.68603254012464));
#215794=CARTESIAN_POINT('Ctrl Pts',(57.5535489747201,-25.371371946722,2.68945542339823));
#215795=CARTESIAN_POINT('Ctrl Pts',(57.5529242061383,-25.3673715770247,
2.69295261525366));
#215796=CARTESIAN_POINT('Ctrl Pts',(57.5522159293602,-25.3634528381778,
2.6965189117208));
#215797=CARTESIAN_POINT('Ctrl Pts',(57.5522098892427,-25.3634194195426,
2.69654932476068));
#215798=CARTESIAN_POINT('Ctrl Pts',(57.5522038431597,-25.3633860069324,
2.69657974261126));
#215799=CARTESIAN_POINT('Ctrl Pts',(57.5521977911122,-25.3633526003503,
2.69661016526954));
#215800=CARTESIAN_POINT('Ctrl Pts',(57.5491069220867,-25.3462913711517,
2.71214746101163));
#215801=CARTESIAN_POINT('Ctrl Pts',(57.5445791409897,-25.3307446654468,
2.72880565567666));
#215802=CARTESIAN_POINT('Ctrl Pts',(57.5388132486366,-25.3167379215575,
2.74628040012487));
#215803=CARTESIAN_POINT('Ctrl Pts',(57.5328523576328,-25.3022574788905,
2.76434612882686));
#215804=CARTESIAN_POINT('Ctrl Pts',(57.5255675223694,-25.2894223267614,
2.78328592654847));
#215805=CARTESIAN_POINT('Ctrl Pts',(57.5171444507328,-25.2783002469352,
2.80278753268369));
#215806=CARTESIAN_POINT('Ctrl Pts',(57.5088816036426,-25.2673897324705,
2.82191817723485));
#215807=CARTESIAN_POINT('Ctrl Pts',(57.4995225236678,-25.2581274647602,
2.84159092316011));
#215808=CARTESIAN_POINT('Ctrl Pts',(57.4892225138715,-25.2506209171159,
2.86151233818038));
#215809=CARTESIAN_POINT('Ctrl Pts',(57.4823991184825,-25.2456480924685,
2.87470957721994));
#215810=CARTESIAN_POINT('Ctrl Pts',(57.4751623993626,-25.2414466709166,
2.88801594388677));
#215811=CARTESIAN_POINT('Ctrl Pts',(57.4675553545144,-25.2380597013421,
2.90134173516006));
#215812=CARTESIAN_POINT('',(57.1420619865024,-25.0931373005737,3.47153072139055));
#215813=CARTESIAN_POINT('',(57.4675553545144,-25.2380597013421,2.90134173516006));
#215814=CARTESIAN_POINT('',(59.2554138597574,-19.5876674457069,3.47153072139059));
#215815=CARTESIAN_POINT('Origin',(5.53234440788222E-15,1.85015204418142E-13,
3.47153072139072));
#215816=CARTESIAN_POINT('',(59.5942745858238,-19.6977666881836,2.90134173516011));
#215817=CARTESIAN_POINT('',(59.2554138597574,-19.5876674457069,3.47153072139059));
#215818=CARTESIAN_POINT('',(59.8682321556244,-19.4684195516687,2.5990817351601));
#215819=CARTESIAN_POINT('Ctrl Pts',(59.5942745858238,-19.6977666881836,
2.90134173516011));
#215820=CARTESIAN_POINT('Ctrl Pts',(59.6059782661688,-19.7015693056584,
2.88164837656642));
#215821=CARTESIAN_POINT('Ctrl Pts',(59.6182462127124,-19.7035046472589,
2.86203734438993));
#215822=CARTESIAN_POINT('Ctrl Pts',(59.6308908042838,-19.703594883946,2.84277945977939));
#215823=CARTESIAN_POINT('Ctrl Pts',(59.6437894749899,-19.7036869338398,
2.82313460919753));
#215824=CARTESIAN_POINT('Ctrl Pts',(59.6570809485104,-19.7018593121344,
2.80385576863025));
#215825=CARTESIAN_POINT('Ctrl Pts',(59.6705908046816,-19.6980881582794,
2.78521678518031));
#215826=CARTESIAN_POINT('Ctrl Pts',(59.6835758151876,-19.694463510333,2.76730190934067));
#215827=CARTESIAN_POINT('Ctrl Pts',(59.696763446405,-19.6890433025163,2.74997687279338));
#215828=CARTESIAN_POINT('Ctrl Pts',(59.7100083536281,-19.6817621015857,
2.73349253345249));
#215829=CARTESIAN_POINT('Ctrl Pts',(59.7201826317487,-19.676168935694,2.72082983598977));
#215830=CARTESIAN_POINT('Ctrl Pts',(59.7303909886965,-19.6694767982701,
2.70866321039124));
#215831=CARTESIAN_POINT('Ctrl Pts',(59.740566973611,-19.6616375006931,2.69711645335832));
#215832=CARTESIAN_POINT('Ctrl Pts',(59.7405936430526,-19.6616169552923,
2.69708619136737));
#215833=CARTESIAN_POINT('Ctrl Pts',(59.7406203123795,-19.6615964011813,
2.69705593387205));
#215834=CARTESIAN_POINT('Ctrl Pts',(59.7406469815888,-19.661575838362,2.69702568087556));
#215835=CARTESIAN_POINT('Ctrl Pts',(59.7435064631644,-19.6593710859726,
2.69378194443252));
#215836=CARTESIAN_POINT('Ctrl Pts',(59.7463627094293,-19.6570664708003,
2.69059266624686));
#215837=CARTESIAN_POINT('Ctrl Pts',(59.7492118317302,-19.6546650315156,
2.68746219342663));
#215838=CARTESIAN_POINT('Ctrl Pts',(59.765066549526,-19.6413015679148,2.67004182396168));
#215839=CARTESIAN_POINT('Ctrl Pts',(59.7807038364411,-19.6249436073995,
2.65443567878043));
#215840=CARTESIAN_POINT('Ctrl Pts',(59.7954515664629,-19.6061700313502,
2.64136852353275));
#215841=CARTESIAN_POINT('Ctrl Pts',(59.8020705519296,-19.5977441904346,
2.63550380329795));
#215842=CARTESIAN_POINT('Ctrl Pts',(59.8085107122957,-19.5888317740057,
2.63014997451126));
#215843=CARTESIAN_POINT('Ctrl Pts',(59.8147133779312,-19.5794843054203,
2.62536981119241));
#215844=CARTESIAN_POINT('Ctrl Pts',(59.817408972519,-19.5754220220071,2.62329241687061));
#215845=CARTESIAN_POINT('Ctrl Pts',(59.820059521955,-19.5712776455712,2.62132362131414));
#215846=CARTESIAN_POINT('Ctrl Pts',(59.8226600907005,-19.5670554570741,
2.61946873372334));
#215847=CARTESIAN_POINT('Ctrl Pts',(59.8317620813098,-19.5522777973345,
2.61297662715554));
#215848=CARTESIAN_POINT('Ctrl Pts',(59.8402518053951,-19.5365469388435,
2.60787989113955));
#215849=CARTESIAN_POINT('Ctrl Pts',(59.8479176686193,-19.5200464333329,
2.60440616886165));
#215850=CARTESIAN_POINT('Ctrl Pts',(59.8517506002314,-19.5117961805776,
2.60266930772271));
#215851=CARTESIAN_POINT('Ctrl Pts',(59.8553775672057,-19.5033535162575,
2.60133820040171));
#215852=CARTESIAN_POINT('Ctrl Pts',(59.8587721277812,-19.494741386793,2.60044130723571));
#215853=CARTESIAN_POINT('Ctrl Pts',(59.8604694080689,-19.4904353220608,
2.5999928606527));
#215854=CARTESIAN_POINT('Ctrl Pts',(59.8621085868741,-19.4860868910805,
2.59965296768499));
#215855=CARTESIAN_POINT('Ctrl Pts',(59.8636863596424,-19.4816989623693,
2.59942518630941));
#215856=CARTESIAN_POINT('Ctrl Pts',(59.8652641324107,-19.4773110336581,
2.59919740493383));
#215857=CARTESIAN_POINT('Ctrl Pts',(59.8667804975195,-19.4728836066883,
2.59908173791605));
#215858=CARTESIAN_POINT('Ctrl Pts',(59.8682321556244,-19.4684195516687,
2.5990817351601));
#215859=CARTESIAN_POINT('',(59.8776671349988,-19.4393816709747,2.59908173516011));
#215860=CARTESIAN_POINT('Origin',(5.50739376141089E-15,1.8546062369304E-13,
2.59908173516023));
#215861=CARTESIAN_POINT('',(59.7908376697914,-19.0928077206402,2.90134173516011));
#215862=CARTESIAN_POINT('Ctrl Pts',(59.8776671349988,-19.4393816709747,
2.59908173516011));
#215863=CARTESIAN_POINT('Ctrl Pts',(59.8788471933727,-19.4357468082902,
2.59908174381669));
#215864=CARTESIAN_POINT('Ctrl Pts',(59.8799786203653,-19.4321071647678,
2.59915752000983));
#215865=CARTESIAN_POINT('Ctrl Pts',(59.8810618871504,-19.4284649220275,
2.59930729517458));
#215866=CARTESIAN_POINT('Ctrl Pts',(59.8873218328134,-19.4074172521818,
2.60017281085914));
#215867=CARTESIAN_POINT('Ctrl Pts',(59.8919760989615,-19.3862806722057,
2.60350651800119));
#215868=CARTESIAN_POINT('Ctrl Pts',(59.8951126055077,-19.3654825713214,
2.60896880596625));
#215869=CARTESIAN_POINT('Ctrl Pts',(59.8963776307492,-19.3570942188,2.61117187235579));
#215870=CARTESIAN_POINT('Ctrl Pts',(59.8973961381385,-19.3487606486692,
2.61372076577263));
#215871=CARTESIAN_POINT('Ctrl Pts',(59.8981752423039,-19.3405086316963,
2.61659179896971));
#215872=CARTESIAN_POINT('Ctrl Pts',(59.8984626844396,-19.3374641384334,
2.61765103591196));
#215873=CARTESIAN_POINT('Ctrl Pts',(59.8987174423899,-19.3344308375133,
2.61875422455137));
#215874=CARTESIAN_POINT('Ctrl Pts',(59.8989398263135,-19.3314101194736,
2.61990022440383));
#215875=CARTESIAN_POINT('Ctrl Pts',(59.8993567961702,-19.3257462731491,
2.6220489741272));
#215876=CARTESIAN_POINT('Ctrl Pts',(59.8996599510839,-19.3201266635119,
2.62434823201758));
#215877=CARTESIAN_POINT('Ctrl Pts',(59.8998513356578,-19.3145604567374,
2.62679048030293));
#215878=CARTESIAN_POINT('Ctrl Pts',(59.9005211816666,-19.2950787330265,
2.63533834930166));
#215879=CARTESIAN_POINT('Ctrl Pts',(59.8998218367508,-19.2762511930029,
2.64563784783549));
#215880=CARTESIAN_POINT('Ctrl Pts',(59.897840987353,-19.2584708442936,2.6573666673795));
#215881=CARTESIAN_POINT('Ctrl Pts',(59.8968505626541,-19.249580669939,2.66323107715151));
#215882=CARTESIAN_POINT('Ctrl Pts',(59.8955397627954,-19.2409522937254,
2.6694528178076));
#215883=CARTESIAN_POINT('Ctrl Pts',(59.8939195570494,-19.2326348443065,
2.67599160631187));
#215884=CARTESIAN_POINT('Ctrl Pts',(59.8931094541765,-19.228476119597,2.679261000564));
#215885=CARTESIAN_POINT('Ctrl Pts',(59.8922219999437,-19.2243951266215,
2.6826096568511));
#215886=CARTESIAN_POINT('Ctrl Pts',(59.891258566018,-19.2203980066209,2.68603254012469));
#215887=CARTESIAN_POINT('Ctrl Pts',(59.8902951320923,-19.2164008866203,
2.68945542339829));
#215888=CARTESIAN_POINT('Ctrl Pts',(59.8892556335612,-19.2124877374665,
2.69295261525372));
#215889=CARTESIAN_POINT('Ctrl Pts',(59.8881416170478,-19.2086645009642,
2.69651891172086));
#215890=CARTESIAN_POINT('Ctrl Pts',(59.8881321168201,-19.2086318967639,
2.69654932476074));
#215891=CARTESIAN_POINT('Ctrl Pts',(59.8881226112894,-19.2085992991793,
2.69657974261132));
#215892=CARTESIAN_POINT('Ctrl Pts',(59.888113100457,-19.2085667082132,2.69661016526959));
#215893=CARTESIAN_POINT('Ctrl Pts',(59.8832557794663,-19.1919220260043,
2.71214746101014));
#215894=CARTESIAN_POINT('Ctrl Pts',(59.8771277287724,-19.1769337687814,
2.72880565567341));
#215895=CARTESIAN_POINT('Ctrl Pts',(59.8699293191677,-19.1636064551686,
2.74628040011972));
#215896=CARTESIAN_POINT('Ctrl Pts',(59.8624874641301,-19.1498284206591,
2.76434612881963));
#215897=CARTESIAN_POINT('Ctrl Pts',(59.8539008972298,-19.1378250534723,
2.78328592653901));
#215898=CARTESIAN_POINT('Ctrl Pts',(59.8443613941499,-19.1276443522976,
2.80278753267194));
#215899=CARTESIAN_POINT('Ctrl Pts',(59.8350033524915,-19.1176573094815,
2.82191817722094));
#215900=CARTESIAN_POINT('Ctrl Pts',(59.8247273719274,-19.1094240716901,
2.84159092314401));
#215901=CARTESIAN_POINT('Ctrl Pts',(59.8136991387743,-19.1030352898944,
2.86151233816212));
#215902=CARTESIAN_POINT('Ctrl Pts',(59.8063933209376,-19.0988029459324,
2.87470957720769));
#215903=CARTESIAN_POINT('Ctrl Pts',(59.7987570771804,-19.0953809833341,
2.88801594388066));
#215904=CARTESIAN_POINT('Ctrl Pts',(59.7908376697914,-19.0928077206402,
2.90134173516011));
#215905=CARTESIAN_POINT('',(59.451978872661,-18.9827025415087,3.47153072139059));
#215906=CARTESIAN_POINT('',(59.7908376697914,-19.0928077206402,2.90134173516011));
#215907=CARTESIAN_POINT('',(60.978275279735,-13.2864868028986,3.47153072139063));
#215908=CARTESIAN_POINT('Origin',(5.53234440788222E-15,1.85015204418142E-13,
3.47153072139072));
#215909=CARTESIAN_POINT('',(61.3267881959115,-13.3605623192477,2.90134173516014));
#215910=CARTESIAN_POINT('',(60.978275279735,-13.2864868028986,3.47153072139063));
#215911=CARTESIAN_POINT('',(61.5752716937453,-13.1038352065718,2.59908173516015));
#215912=CARTESIAN_POINT('Ctrl Pts',(61.3267881959115,-13.3605623192477,
2.90134173516014));
#215913=CARTESIAN_POINT('Ctrl Pts',(61.3388252440308,-13.3631207378649,
2.88164837656838));
#215914=CARTESIAN_POINT('Ctrl Pts',(61.3512282837617,-13.363763127862,2.86203734439379));
#215915=CARTESIAN_POINT('Ctrl Pts',(61.3638130392384,-13.3625311504979,
2.84277945978506));
#215916=CARTESIAN_POINT('Ctrl Pts',(61.3766506715095,-13.3612744179062,
2.82313460920505));
#215917=CARTESIAN_POINT('Ctrl Pts',(61.3896782944578,-13.3580674708029,
2.80385576863951));
#215918=CARTESIAN_POINT('Ctrl Pts',(61.4027199493048,-13.35290481122,2.78521678519113));
#215919=CARTESIAN_POINT('Ctrl Pts',(61.4152549476837,-13.3479427162818,
2.767301909353));
#215920=CARTESIAN_POINT('Ctrl Pts',(61.4278037696825,-13.341173718107,2.74997687280706));
#215921=CARTESIAN_POINT('Ctrl Pts',(61.4402150271729,-13.3325479345607,
2.73349253346727));
#215922=CARTESIAN_POINT('Ctrl Pts',(61.4497489245016,-13.3259219069584,
2.72082983599924));
#215923=CARTESIAN_POINT('Ctrl Pts',(61.4592018401648,-13.3181993658968,
2.70866321039576));
#215924=CARTESIAN_POINT('Ctrl Pts',(61.468502650244,-13.3093393327434,2.69711645335836));
#215925=CARTESIAN_POINT('Ctrl Pts',(61.4685270260085,-13.3093161121766,
2.69708619136742));
#215926=CARTESIAN_POINT('Ctrl Pts',(61.4685514007484,-13.3092928829594,
2.69705593387209));
#215927=CARTESIAN_POINT('Ctrl Pts',(61.468575774461,-13.309269645094,2.69702568087561));
#215928=CARTESIAN_POINT('Ctrl Pts',(61.4711891321182,-13.3067780733541,
2.69378194443257));
#215929=CARTESIAN_POINT('Ctrl Pts',(61.4737888336848,-13.304187524072,2.6905926662469));
#215930=CARTESIAN_POINT('Ctrl Pts',(61.4763713294376,-13.3015014257472,
2.68746219342667));
#215931=CARTESIAN_POINT('Ctrl Pts',(61.4907423311174,-13.2865538993104,
2.67004182396043));
#215932=CARTESIAN_POINT('Ctrl Pts',(61.5045840828647,-13.2686510078419,
2.65443567877815));
#215933=CARTESIAN_POINT('Ctrl Pts',(61.5172886502247,-13.2484387178487,
2.64136852352988));
#215934=CARTESIAN_POINT('Ctrl Pts',(61.5229906359928,-13.2393671621934,
2.63550380329622));
#215935=CARTESIAN_POINT('Ctrl Pts',(61.5284639152923,-13.2298303888495,
2.63014997451051));
#215936=CARTESIAN_POINT('Ctrl Pts',(61.5336555255489,-13.2198857715696,
2.62536981119244));
#215937=CARTESIAN_POINT('Ctrl Pts',(61.535911729145,-13.2155639754102,2.62329241687064));
#215938=CARTESIAN_POINT('Ctrl Pts',(61.5381145532938,-13.2111652444426,
2.62132362131419));
#215939=CARTESIAN_POINT('Ctrl Pts',(61.5402595369764,-13.2066943520814,
2.61946873372339));
#215940=CARTESIAN_POINT('Ctrl Pts',(61.5477669798654,-13.1910462288169,
2.61297662715559));
#215941=CARTESIAN_POINT('Ctrl Pts',(61.55456587389,-13.1745141278025,2.6078798911396));
#215942=CARTESIAN_POINT('Ctrl Pts',(61.5604649702292,-13.1573027128851,
2.6044061688617));
#215943=CARTESIAN_POINT('Ctrl Pts',(61.5634145183988,-13.1486970054264,
2.60266930772275));
#215944=CARTESIAN_POINT('Ctrl Pts',(61.5661391177412,-13.1399214696207,
2.60133820040177));
#215945=CARTESIAN_POINT('Ctrl Pts',(61.5686148699003,-13.1310016901021,
2.60044130723576));
#215946=CARTESIAN_POINT('Ctrl Pts',(61.5698527459799,-13.1265418003428,
2.59999286065276));
#215947=CARTESIAN_POINT('Ctrl Pts',(61.5710284103841,-13.1220458496809,
2.59965296768503));
#215948=CARTESIAN_POINT('Ctrl Pts',(61.572138876503,-13.1175170363394,2.59942518630945));
#215949=CARTESIAN_POINT('Ctrl Pts',(61.5732493426218,-13.1129882229979,
2.59919740493387));
#215950=CARTESIAN_POINT('Ctrl Pts',(61.5742946087865,-13.1084265466218,
2.59908173791606));
#215951=CARTESIAN_POINT('Ctrl Pts',(61.5752716937453,-13.1038352065718,
2.59908173516015));
#215952=CARTESIAN_POINT('',(61.5816197022699,-13.0739701745315,2.59908173516015));
#215953=CARTESIAN_POINT('Origin',(5.50318346416883E-15,1.85444910649818E-13,
2.59908173516024));
#215954=CARTESIAN_POINT('',(61.459039055521,-12.7383709431241,2.90134173516015));
#215955=CARTESIAN_POINT('Ctrl Pts',(61.58161970227,-13.0739701745315,2.59908173516016));
#215956=CARTESIAN_POINT('Ctrl Pts',(61.58241334955,-13.0702318743168,2.59908174381671));
#215957=CARTESIAN_POINT('Ctrl Pts',(61.583158132123,-13.0664939028176,2.59915752000987));
#215958=CARTESIAN_POINT('Ctrl Pts',(61.5838547466227,-13.0627583804517,
2.59930729517462));
#215959=CARTESIAN_POINT('Ctrl Pts',(61.5878803190637,-13.0411716694454,
2.60017281085909));
#215960=CARTESIAN_POINT('Ctrl Pts',(61.5902997144312,-13.0196643745799,
2.6035065180006));
#215961=CARTESIAN_POINT('Ctrl Pts',(61.5912450453421,-12.998652353661,2.60896880596475));
#215962=CARTESIAN_POINT('Ctrl Pts',(61.5916263190448,-12.9901777222658,
2.61117187235465));
#215963=CARTESIAN_POINT('Ctrl Pts',(61.5917681516648,-12.98178334129,2.613720765772));
#215964=CARTESIAN_POINT('Ctrl Pts',(61.5916804171631,-12.9734950911664,
2.61659179896975));
#215965=CARTESIAN_POINT('Ctrl Pts',(61.5916480484585,-12.9704372300715,
2.617651035912));
#215966=CARTESIAN_POINT('Ctrl Pts',(61.5915843445342,-12.9673939164341,
2.61875422455141));
#215967=CARTESIAN_POINT('Ctrl Pts',(61.5914897592008,-12.9643665007541,
2.61990022440388));
#215968=CARTESIAN_POINT('Ctrl Pts',(61.5913124117006,-12.9586900963541,
2.62204897412725));
#215969=CARTESIAN_POINT('Ctrl Pts',(61.5910264967404,-12.9530695832092,
2.62434823201762));
#215970=CARTESIAN_POINT('Ctrl Pts',(61.5906350058492,-12.9475138635623,
2.62679048030297));
#215971=CARTESIAN_POINT('Ctrl Pts',(61.5892647877302,-12.9280688447985,
2.63533834930171));
#215972=CARTESIAN_POINT('Ctrl Pts',(61.5866012600732,-12.9094175454583,
2.64563784783553));
#215973=CARTESIAN_POINT('Ctrl Pts',(61.5827727094487,-12.8919416545033,
2.65736666737954));
#215974=CARTESIAN_POINT('Ctrl Pts',(61.5808584341364,-12.8832037090257,
2.66323107715155));
#215975=CARTESIAN_POINT('Ctrl Pts',(61.5786529040704,-12.8747596158547,
2.66945281780765));
#215976=CARTESIAN_POINT('Ctrl Pts',(61.576172163775,-12.8666570879107,2.67599160631192));
#215977=CARTESIAN_POINT('Ctrl Pts',(61.5749317936273,-12.8626058239388,
2.67926100056405));
#215978=CARTESIAN_POINT('Ctrl Pts',(61.5736226210374,-12.8586399512969,
2.68260965685114));
#215979=CARTESIAN_POINT('Ctrl Pts',(61.5722466520923,-12.8547654342056,
2.68603254012473));
#215980=CARTESIAN_POINT('Ctrl Pts',(61.5708706831473,-12.8508909171143,
2.68945542339832));
#215981=CARTESIAN_POINT('Ctrl Pts',(61.5694278436303,-12.8471078617851,
2.69295261525376));
#215982=CARTESIAN_POINT('Ctrl Pts',(61.5679202927797,-12.8434220158066,
2.6965189117209));
#215983=CARTESIAN_POINT('Ctrl Pts',(61.5679074365282,-12.8433905832597,
2.69654932476078));
#215984=CARTESIAN_POINT('Ctrl Pts',(61.5678945756945,-12.8433591578466,
2.69657974261137));
#215985=CARTESIAN_POINT('Ctrl Pts',(61.5678817102797,-12.8433277395699,
2.69661016526964));
#215986=CARTESIAN_POINT('Ctrl Pts',(61.5613111551486,-12.8272819669702,
2.71214746101055));
#215987=CARTESIAN_POINT('Ctrl Pts',(61.5536499750629,-12.8130163727101,
2.72880565567422));
#215988=CARTESIAN_POINT('Ctrl Pts',(61.5450979154875,-12.8005145062095,
2.74628040012097));
#215989=CARTESIAN_POINT('Ctrl Pts',(61.5362566309361,-12.7875898348854,
2.76434612882128));
#215990=CARTESIAN_POINT('Ctrl Pts',(61.5264624086214,-12.7765497640427,
2.78328592654109));
#215991=CARTESIAN_POINT('Ctrl Pts',(61.5159109908884,-12.7674219834115,
2.80278753267447));
#215992=CARTESIAN_POINT('Ctrl Pts',(61.505560283323,-12.7584678323747,2.82191817722384));
#215993=CARTESIAN_POINT('Ctrl Pts',(61.4944799879613,-12.7513538295784,
2.84159092314728));
#215994=CARTESIAN_POINT('Ctrl Pts',(61.4828443590798,-12.7461528104621,
2.86151233816575));
#215995=CARTESIAN_POINT('Ctrl Pts',(61.475136162868,-12.7427073176349,2.87470957721014));
#215996=CARTESIAN_POINT('Ctrl Pts',(61.467184058762,-12.7401023057312,2.88801594388191));
#215997=CARTESIAN_POINT('Ctrl Pts',(61.459039055521,-12.7383709431241,2.90134173516015));
#215998=CARTESIAN_POINT('',(61.1105274371643,-12.6642893210132,3.47153072139064));
#215999=CARTESIAN_POINT('',(61.459039055521,-12.7383709431241,2.90134173516015));
#216000=CARTESIAN_POINT('',(62.0330459552233,-6.83973663030158,3.47153072139068));
#216001=CARTESIAN_POINT('Origin',(5.53234440788222E-15,1.85015204418142E-13,
3.47153072139072));
#216002=CARTESIAN_POINT('',(62.3873926810692,-6.87697683366461,2.90134173516019));
#216003=CARTESIAN_POINT('',(62.0330459552233,-6.83973663030158,3.47153072139067));
#216004=CARTESIAN_POINT('',(62.6076796697355,-6.59568250079781,2.59908173516019));
#216005=CARTESIAN_POINT('Ctrl Pts',(62.3873926810692,-6.87697683366461,
2.90134173516019));
#216006=CARTESIAN_POINT('Ctrl Pts',(62.3996312165471,-6.87826302285487,
2.88164837656645));
#216007=CARTESIAN_POINT('Ctrl Pts',(62.4120334591692,-6.87760542308927,
2.86203734438992));
#216008=CARTESIAN_POINT('Ctrl Pts',(62.4244204973392,-6.87506472947491,
2.84277945977932));
#216009=CARTESIAN_POINT('Ctrl Pts',(62.4370564393923,-6.8724729834219,2.82313460919733));
#216010=CARTESIAN_POINT('Ctrl Pts',(62.4496774784077,-6.86792184690252,
2.80385576862992));
#216011=CARTESIAN_POINT('Ctrl Pts',(62.4621080448336,-6.86142424476788,
2.78521678517985));
#216012=CARTESIAN_POINT('Ctrl Pts',(62.4740556950225,-6.85517906858589,
2.76730190934001));
#216013=CARTESIAN_POINT('Ctrl Pts',(62.4858282202855,-6.84713544261008,
2.74997687279252));
#216014=CARTESIAN_POINT('Ctrl Pts',(62.4972698477112,-6.83725958233362,
2.73349253345147));
#216015=CARTESIAN_POINT('Ctrl Pts',(62.5060589088662,-6.82967328916932,
2.72082983598914));
#216016=CARTESIAN_POINT('Ctrl Pts',(62.5146528151149,-6.82100495425111,
2.70866321039099));
#216017=CARTESIAN_POINT('Ctrl Pts',(62.5229765487298,-6.81122125790576,
2.6971164533584));
#216018=CARTESIAN_POINT('Ctrl Pts',(62.5229983637512,-6.81119561658246,
2.69708619136746));
#216019=CARTESIAN_POINT('Ctrl Pts',(62.5230201768493,-6.81116996676326,
2.69705593387214));
#216020=CARTESIAN_POINT('Ctrl Pts',(62.5230419880218,-6.81114430845053,
2.69702568087566));
#216021=CARTESIAN_POINT('Ctrl Pts',(62.5253805892672,-6.80839321554143,
2.69378194443261));
#216022=CARTESIAN_POINT('Ctrl Pts',(62.5276952632612,-6.80554511474964,
2.69059266624695));
#216023=CARTESIAN_POINT('Ctrl Pts',(62.5299828381019,-6.80260378684012,
2.68746219342672));
#216024=CARTESIAN_POINT('Ctrl Pts',(62.5427126719616,-6.78623596579746,
2.67004182396211));
#216025=CARTESIAN_POINT('Ctrl Pts',(62.5546072354103,-6.76698429120464,
2.65443567878113));
#216026=CARTESIAN_POINT('Ctrl Pts',(62.5651294462081,-6.74555473735071,
2.64136852353361));
#216027=CARTESIAN_POINT('Ctrl Pts',(62.5698519601306,-6.73593685681467,
2.6355038032985));
#216028=CARTESIAN_POINT('Ctrl Pts',(62.5742983919722,-6.72588021343676,
2.63014997451154));
#216029=CARTESIAN_POINT('Ctrl Pts',(62.5784220664835,-6.71544740276666,
2.62536981119248));
#216030=CARTESIAN_POINT('Ctrl Pts',(62.5802141596491,-6.71091344436403,
2.62329241687068));
#216031=CARTESIAN_POINT('Ctrl Pts',(62.5819451239083,-6.70630855228186,
2.62132362131423));
#216032=CARTESIAN_POINT('Ctrl Pts',(62.5836110216379,-6.70163794008866,
2.61946873372343));
#216033=CARTESIAN_POINT('Ctrl Pts',(62.5894416636914,-6.68529079741248,
2.61297662715563));
#216034=CARTESIAN_POINT('Ctrl Pts',(62.5944752375495,-6.66813858303296,
2.60787989113965));
#216035=CARTESIAN_POINT('Ctrl Pts',(62.5985429352697,-6.65040483057231,
2.60440616886175));
#216036=CARTESIAN_POINT('Ctrl Pts',(62.6005767841298,-6.64153795434199,
2.6026693077228));
#216037=CARTESIAN_POINT('Ctrl Pts',(62.6023691645599,-6.63252569365736,
2.6013382004018));
#216038=CARTESIAN_POINT('Ctrl Pts',(62.6038989834439,-6.62339599105565,
2.6004413072358));
#216039=CARTESIAN_POINT('Ctrl Pts',(62.6046638928858,-6.61883113975479,
2.59999286065279));
#216040=CARTESIAN_POINT('Ctrl Pts',(62.6053631620638,-6.61423692798752,
2.59965296768508));
#216041=CARTESIAN_POINT('Ctrl Pts',(62.6059941550341,-6.60961684864246,
2.5994251863095));
#216042=CARTESIAN_POINT('Ctrl Pts',(62.6066251480044,-6.60499676929741,
2.59919740493392));
#216043=CARTESIAN_POINT('Ctrl Pts',(62.6071878630701,-6.60035082219586,
2.59908173791609));
#216044=CARTESIAN_POINT('Ctrl Pts',(62.6076796697355,-6.59568250079782,
2.5990817351602));
#216045=CARTESIAN_POINT('',(62.6108711573006,-6.56531752495198,2.5990817351602));
#216046=CARTESIAN_POINT('Origin',(5.50063869163689E-15,1.8542884358839E-13,
2.59908173516023));
#216047=CARTESIAN_POINT('',(62.4538823482276,-6.24436990787956,2.9013417351602));
#216048=CARTESIAN_POINT('Ctrl Pts',(62.6108711573006,-6.56531752495198,
2.59908173516019));
#216049=CARTESIAN_POINT('Ctrl Pts',(62.6112696981211,-6.56151674480639,
2.59908174381683));
#216050=CARTESIAN_POINT('Ctrl Pts',(62.6116196762807,-6.55772139932838,
2.59915752000993));
#216051=CARTESIAN_POINT('Ctrl Pts',(62.6119220062409,-6.55393352450177,
2.59930729517467));
#216052=CARTESIAN_POINT('Ctrl Pts',(62.6136691004465,-6.53204428085526,
2.60017281085918));
#216053=CARTESIAN_POINT('Ctrl Pts',(62.6138271176316,-6.51040190952082,
2.60350651800088));
#216054=CARTESIAN_POINT('Ctrl Pts',(62.612570915664,-6.48940618066297,2.60896880596535));
#216055=CARTESIAN_POINT('Ctrl Pts',(62.6120642605129,-6.48093812023183,
2.61117187235511));
#216056=CARTESIAN_POINT('Ctrl Pts',(62.6113278644156,-6.47257489900818,
2.61372076577227));
#216057=CARTESIAN_POINT('Ctrl Pts',(62.6103742524841,-6.46434122353931,
2.61659179896978));
#216058=CARTESIAN_POINT('Ctrl Pts',(62.6100224275775,-6.46130349717838,
2.61765103591203));
#216059=CARTESIAN_POINT('Ctrl Pts',(62.6096409597323,-6.45828351400483,
2.61875422455144));
#216060=CARTESIAN_POINT('Ctrl Pts',(62.6092304414385,-6.45528256968424,
2.61990022440391));
#216061=CARTESIAN_POINT('Ctrl Pts',(62.6084607196376,-6.44965579908311,
2.62204897412728));
#216062=CARTESIAN_POINT('Ctrl Pts',(62.6075888673476,-6.44409596194872,
2.62434823201764));
#216063=CARTESIAN_POINT('Ctrl Pts',(62.6066187902475,-6.43861159905666,
2.626790480303));
#216064=CARTESIAN_POINT('Ctrl Pts',(62.6032235203971,-6.41941632893448,
2.63533834930173));
#216065=CARTESIAN_POINT('Ctrl Pts',(62.5986249921653,-6.40114561781649,
2.64563784783558));
#216066=CARTESIAN_POINT('Ctrl Pts',(62.5929906867159,-6.38416565413391,
2.6573666673796));
#216067=CARTESIAN_POINT('Ctrl Pts',(62.5901735339913,-6.37567567229262,
2.66323107715161));
#216068=CARTESIAN_POINT('Ctrl Pts',(62.5870974379669,-6.36750837741602,
2.66945281780769));
#216069=CARTESIAN_POINT('Ctrl Pts',(62.5837833426318,-6.35970954393874,
2.67599160631196));
#216070=CARTESIAN_POINT('Ctrl Pts',(62.5821262949643,-6.3558101272001,2.67926100056409));
#216071=CARTESIAN_POINT('Ctrl Pts',(62.580409747586,-6.35200282582255,2.68260965685118));
#216072=CARTESIAN_POINT('Ctrl Pts',(62.5786363190254,-6.3482933616606,2.68603254012478));
#216073=CARTESIAN_POINT('Ctrl Pts',(62.5768628904648,-6.34458389749865,
2.68945542339837));
#216074=CARTESIAN_POINT('Ctrl Pts',(62.5750325180136,-6.34097238393975,
2.6929526152538));
#216075=CARTESIAN_POINT('Ctrl Pts',(62.5731479498683,-6.3374643113849,2.69651891172094));
#216076=CARTESIAN_POINT('Ctrl Pts',(62.5731318784489,-6.33743439487305,
2.69654932476082));
#216077=CARTESIAN_POINT('Ctrl Pts',(62.573115803218,-6.33740448593478,2.69657974261141));
#216078=CARTESIAN_POINT('Ctrl Pts',(62.5730997241771,-6.33737458457273,
2.69661016526968));
#216079=CARTESIAN_POINT('Ctrl Pts',(62.564887923282,-6.32210352242355,2.71214746101192));
#216080=CARTESIAN_POINT('Ctrl Pts',(62.555777551296,-6.30871688796164,2.7288056556771));
#216081=CARTESIAN_POINT('Ctrl Pts',(62.5459655399035,-6.29717744163835,
2.74628040012548));
#216082=CARTESIAN_POINT('Ctrl Pts',(62.5358216928012,-6.2852477389029,2.76434612882741));
#216083=CARTESIAN_POINT('Ctrl Pts',(62.5249271226206,-6.27529192173046,
2.78328592654895));
#216084=CARTESIAN_POINT('Ctrl Pts',(62.5134793937744,-6.2673170675176,2.8027875326841));
#216085=CARTESIAN_POINT('Ctrl Pts',(62.5022494248193,-6.25949391181267,
2.82191817723497));
#216086=CARTESIAN_POINT('Ctrl Pts',(62.4904862126941,-6.25357708651515,
2.84159092315994));
#216087=CARTESIAN_POINT('Ctrl Pts',(62.4783706704684,-6.24962081353253,
2.8615123381799));
#216088=CARTESIAN_POINT('Ctrl Pts',(62.4703445484942,-6.24699992138176,
2.87470957721967));
#216089=CARTESIAN_POINT('Ctrl Pts',(62.4621637089584,-6.24524040122871,
2.88801594388671));
#216090=CARTESIAN_POINT('Ctrl Pts',(62.4538823482276,-6.24436990787956,
2.9013417351602));
#216091=CARTESIAN_POINT('',(62.099536274866,-6.20712349654361,3.47153072139068));
#216092=CARTESIAN_POINT('',(62.4538823482276,-6.24436990787956,2.9013417351602));
#216093=CARTESIAN_POINT('',(62.4081695979768,-0.318048871876943,3.47153072139072));
#216094=CARTESIAN_POINT('Origin',(5.53234440788222E-15,1.85015204418142E-13,
3.47153072139072));
#216095=CARTESIAN_POINT('',(62.7644678366119,-0.318045750792856,2.90134173516023));
#216096=CARTESIAN_POINT('',(62.4081695979768,-0.318048871876944,3.47153072139072));
#216097=CARTESIAN_POINT('Ctrl Pts',(62.7644678366119,-0.318045750792856,
2.90134173516023));
#216098=CARTESIAN_POINT('Ctrl Pts',(62.7767737714904,-0.318045618797943,
2.88164837656825));
#216099=CARTESIAN_POINT('Ctrl Pts',(62.7890393354356,-0.316095234070607,
2.86203734439344));
#216100=CARTESIAN_POINT('Ctrl Pts',(62.8010929413143,-0.312273660577998,
2.8427794597845));
#216101=CARTESIAN_POINT('Ctrl Pts',(62.8133887511215,-0.308375296776985,
2.8231346092043));
#216102=CARTESIAN_POINT('Ctrl Pts',(62.8254649274571,-0.302529834047596,
2.80385576863858));
#216103=CARTESIAN_POINT('Ctrl Pts',(62.8371482135724,-0.294768478452709,
2.78521678519004));
#216104=CARTESIAN_POINT('Ctrl Pts',(62.8483776146134,-0.287308644486815,
2.76730190935176));
#216105=CARTESIAN_POINT('Ctrl Pts',(62.859244860888,-0.278078518363,2.74997687280568));
#216106=CARTESIAN_POINT('Ctrl Pts',(62.8695915013826,-0.267060783352544,
2.73349253346579));
#216107=CARTESIAN_POINT('Ctrl Pts',(62.8775394315778,-0.258597341637506,
2.72082983599833));
#216108=CARTESIAN_POINT('Ctrl Pts',(62.8851801717839,-0.24907818494816,
2.70866321039538));
#216109=CARTESIAN_POINT('Ctrl Pts',(62.8924356323738,-0.238478017627679,
2.69711645335845));
#216110=CARTESIAN_POINT('Ctrl Pts',(62.892454647642,-0.238450236479571,
2.69708619136751));
#216111=CARTESIAN_POINT('Ctrl Pts',(62.8924736601095,-0.238422447083147,
2.69705593387219));
#216112=CARTESIAN_POINT('Ctrl Pts',(62.8924926697742,-0.238394649440984,
2.69702568087571));
#216113=CARTESIAN_POINT('Ctrl Pts',(62.8945308924032,-0.23541417691232,
2.69378194443266));
#216114=CARTESIAN_POINT('Ctrl Pts',(62.8965351787718,-0.232339728999126,
2.690592666247));
#216115=CARTESIAN_POINT('Ctrl Pts',(62.8985027695519,-0.229175397308934,
2.68746219342677));
#216116=CARTESIAN_POINT('Ctrl Pts',(62.9094519648695,-0.211566610930916,
2.67004182396156));
#216117=CARTESIAN_POINT('Ctrl Pts',(62.9192690206948,-0.191177078586518,
2.65443567878009));
#216118=CARTESIAN_POINT('Ctrl Pts',(62.9274935913882,-0.168765047545019,
2.64136852353229));
#216119=CARTESIAN_POINT('Ctrl Pts',(62.9311848926126,-0.158706217642537,
2.63550380329772));
#216120=CARTESIAN_POINT('Ctrl Pts',(62.9345557609572,-0.148239886922649,
2.63014997451123));
#216121=CARTESIAN_POINT('Ctrl Pts',(62.9375663198809,-0.137433186922181,
2.62536981119254));
#216122=CARTESIAN_POINT('Ctrl Pts',(62.9388746680683,-0.132736741273433,
2.62329241687074));
#216123=CARTESIAN_POINT('Ctrl Pts',(62.9401148076313,-0.127976140237919,
2.62132362131427));
#216124=CARTESIAN_POINT('Ctrl Pts',(62.9412833674838,-0.123156980417379,
2.61946873372348));
#216125=CARTESIAN_POINT('Ctrl Pts',(62.9453733269673,-0.106289921045488,
2.61297662715568));
#216126=CARTESIAN_POINT('Ctrl Pts',(62.9485864317704,-0.0887055165508694,
2.60787989113969));
#216127=CARTESIAN_POINT('Ctrl Pts',(62.9507781643242,-0.0706437212499775,
2.60440616886179));
#216128=CARTESIAN_POINT('Ctrl Pts',(62.9518740306011,-0.0616128235995317,
2.60266930772284));
#216129=CARTESIAN_POINT('Ctrl Pts',(62.9527145544237,-0.0524625782499523,
2.60133820040185));
#216130=CARTESIAN_POINT('Ctrl Pts',(62.9532816790167,-0.0432229794973303,
2.60044130723585));
#216131=CARTESIAN_POINT('Ctrl Pts',(62.9535652413132,-0.0386031801210193,
2.59999286065284));
#216132=CARTESIAN_POINT('Ctrl Pts',(62.9537804539255,-0.0339610423939235,
2.59965296768511));
#216133=CARTESIAN_POINT('Ctrl Pts',(62.9539250604562,-0.0293003156014106,
2.59942518630953));
#216134=CARTESIAN_POINT('Ctrl Pts',(62.9540696669868,-0.0246395888088978,
2.59919740493395));
#216135=CARTESIAN_POINT('Ctrl Pts',(62.9541436657296,-0.0199602729506026,
2.59908173791615));
#216136=CARTESIAN_POINT('Ctrl Pts',(62.9541448057648,-0.0152661173106757,
2.59908173516024));
#216137=CARTESIAN_POINT('Origin',(5.71385722241845E-15,1.94016234460786E-13,
2.18253198860262));
#216138=CARTESIAN_POINT('',(-59.1088767419348,0.316922544675878,2.90134173516022));
#216139=CARTESIAN_POINT('Ctrl Pts',(-58.9208513795073,0.015212193456111,
2.59908173516023));
#216140=CARTESIAN_POINT('Ctrl Pts',(-58.9208504012364,0.0190220008287343,
2.59908174371509));
#216141=CARTESIAN_POINT('Ctrl Pts',(-58.9208964366351,0.0228214099819142,
2.59915764355889));
#216142=CARTESIAN_POINT('Ctrl Pts',(-58.9209883940807,0.0266084895331968,
2.59930765775276));
#216143=CARTESIAN_POINT('Ctrl Pts',(-58.9215313038857,0.0489671208155431,
2.60019333020889));
#216144=CARTESIAN_POINT('Ctrl Pts',(-58.9236732325291,0.0708986527649559,
2.60365973324157));
#216145=CARTESIAN_POINT('Ctrl Pts',(-58.9271900305707,0.0919988953574036,
2.6093417708256));
#216146=CARTESIAN_POINT('Ctrl Pts',(-58.9285037892495,0.0998812435911596,
2.61146439091957));
#216147=CARTESIAN_POINT('Ctrl Pts',(-58.93000918782,0.107647933248718,2.61389584429379));
#216148=CARTESIAN_POINT('Ctrl Pts',(-58.9316938830317,0.115279202947081,
2.6166160438525));
#216149=CARTESIAN_POINT('Ctrl Pts',(-58.933008366749,0.121233502390386,
2.61873848000773));
#216150=CARTESIAN_POINT('Ctrl Pts',(-58.9344322364591,0.127104908280178,
2.62103707099785));
#216151=CARTESIAN_POINT('Ctrl Pts',(-58.9359598525093,0.13288357827324,
2.62350262767649));
#216152=CARTESIAN_POINT('Ctrl Pts',(-58.9413065086848,0.153108923248959,
2.63213207605176));
#216153=CARTESIAN_POINT('Ctrl Pts',(-58.9479240485795,0.172198253417896,
2.64280685971912));
#216154=CARTESIAN_POINT('Ctrl Pts',(-58.9555707636545,0.189729578870957,
2.65513293646081));
#216155=CARTESIAN_POINT('Ctrl Pts',(-58.959394121192,0.198495241597488,
2.66129597483166));
#216156=CARTESIAN_POINT('Ctrl Pts',(-58.9634747743348,0.206871403160735,
2.66787183533849));
#216157=CARTESIAN_POINT('Ctrl Pts',(-58.9677825146336,0.2148053148634,2.67481125953859));
#216158=CARTESIAN_POINT('Ctrl Pts',(-58.9720718502312,0.222705329147818,
2.68172103524077));
#216159=CARTESIAN_POINT('Ctrl Pts',(-58.9765861722458,0.23016705507937,
2.68899101329786));
#216160=CARTESIAN_POINT('Ctrl Pts',(-58.9812961520165,0.237137844566841,
2.69657334701272));
#216161=CARTESIAN_POINT('Ctrl Pts',(-58.9813163616197,0.237167754862984,
2.69660588132569));
#216162=CARTESIAN_POINT('Ctrl Pts',(-58.9813365744745,0.237197656536892,
2.69663842081378));
#216163=CARTESIAN_POINT('Ctrl Pts',(-58.9813567905789,0.237227549588143,
2.69667096547378));
#216164=CARTESIAN_POINT('Ctrl Pts',(-58.9908903168205,0.251324537971825,
2.71201840157859));
#216165=CARTESIAN_POINT('Ctrl Pts',(-59.0011093202319,0.263501580511345,
2.7284564593918));
#216166=CARTESIAN_POINT('Ctrl Pts',(-59.011829410383,0.273820596507998,
2.74568723186633));
#216167=CARTESIAN_POINT('Ctrl Pts',(-59.0229394763206,0.28451499800261,
2.76354482593972));
#216168=CARTESIAN_POINT('Ctrl Pts',(-59.034588573653,0.29321400956702,2.78225519316684));
#216169=CARTESIAN_POINT('Ctrl Pts',(-59.0465875206362,0.299936893970986,
2.8015122308497));
#216170=CARTESIAN_POINT('Ctrl Pts',(-59.0584152157231,0.306563827729856,
2.82049442739634));
#216171=CARTESIAN_POINT('Ctrl Pts',(-59.0705837677918,0.311270560392258,
2.84000929088533));
#216172=CARTESIAN_POINT('Ctrl Pts',(-59.082913990599,0.314027284734976,
2.85976644340804));
#216173=CARTESIAN_POINT('Ctrl Pts',(-59.0915108413181,0.31594932199406,
2.87354148166398));
#216174=CARTESIAN_POINT('Ctrl Pts',(-59.1001863397057,0.316922445687917,
2.88743438345212));
#216175=CARTESIAN_POINT('Ctrl Pts',(-59.1088767419348,0.316922544675878,
2.90134173516022));
#216176=CARTESIAN_POINT('',(-59.4651754363832,0.316925998273232,3.47153072139072));
#216177=CARTESIAN_POINT('',(-59.1088767419348,0.316922544675878,2.90134173516022));
#216178=CARTESIAN_POINT('',(-59.1725467709678,5.90061356181237,3.47153072139075));
#216179=CARTESIAN_POINT('Origin',(5.53234440788222E-15,1.85015204418142E-13,
3.47153072139072));
#216180=CARTESIAN_POINT('',(-58.8181995570485,5.8633736414956,2.90134173516027));
#216181=CARTESIAN_POINT('',(-59.1725467709678,5.90061356181236,3.47153072139076));
#216182=CARTESIAN_POINT('',(-58.5996668978649,6.14377718965303,2.59908173516027));
#216183=CARTESIAN_POINT('Ctrl Pts',(-58.8181995570485,5.8633736414956,2.90134173516027));
#216184=CARTESIAN_POINT('Ctrl Pts',(-58.8060365798454,5.8620954050285,2.88176998919727));
#216185=CARTESIAN_POINT('Ctrl Pts',(-58.7937272422245,5.86273454612513,
2.86226752356565));
#216186=CARTESIAN_POINT('Ctrl Pts',(-58.7814443761798,5.86523378400462,
2.84310370499784));
#216187=CARTESIAN_POINT('Ctrl Pts',(-58.7689396367193,5.86777816724704,
2.8235937178835));
#216188=CARTESIAN_POINT('Ctrl Pts',(-58.7564614161378,5.87225032431066,
2.80443322636623));
#216189=CARTESIAN_POINT('Ctrl Pts',(-58.7441787427581,5.8786413544399,2.78589323877821));
#216190=CARTESIAN_POINT('Ctrl Pts',(-58.7324160859235,5.88476180492377,
2.7681381861952));
#216191=CARTESIAN_POINT('Ctrl Pts',(-58.7208319573114,5.89264238981991,
2.750950951982));
#216192=CARTESIAN_POINT('Ctrl Pts',(-58.7095754394624,5.90232005416046,
2.73457771434575));
#216193=CARTESIAN_POINT('Ctrl Pts',(-58.7006223753279,5.91001735013374,
2.7215549795523));
#216194=CARTESIAN_POINT('Ctrl Pts',(-58.6918764318946,5.91885232406616,
2.70904711159798));
#216195=CARTESIAN_POINT('Ctrl Pts',(-58.6834178317481,5.92886364759531,
2.69718956158341));
#216196=CARTESIAN_POINT('Ctrl Pts',(-58.6833947425173,5.92889097525654,
2.69715719432358));
#216197=CARTESIAN_POINT('Ctrl Pts',(-58.683371655605,5.92891831167209,2.69712483219024));
#216198=CARTESIAN_POINT('Ctrl Pts',(-58.6833485710132,5.92894565684157,
2.69709247518652));
#216199=CARTESIAN_POINT('Ctrl Pts',(-58.6787531612542,5.93438921243197,
2.69065122242277));
#216200=CARTESIAN_POINT('Ctrl Pts',(-58.6742527563956,5.94021607194757,
2.68442464469429));
#216201=CARTESIAN_POINT('Ctrl Pts',(-58.6698707672381,5.94639317576856,
2.67844505923581));
#216202=CARTESIAN_POINT('Ctrl Pts',(-58.6611744062938,5.95865206607762,
2.6665781577957));
#216203=CARTESIAN_POINT('Ctrl Pts',(-58.6529445485198,5.97229179622498,
2.65568445664175));
#216204=CARTESIAN_POINT('Ctrl Pts',(-58.6453649253901,5.98706231730018,
2.64601906229516));
#216205=CARTESIAN_POINT('Ctrl Pts',(-58.6396802080428,5.99814020810658,
2.63877001653522));
#216206=CARTESIAN_POINT('Ctrl Pts',(-58.6343612468744,6.00985416873249,
2.63221189387604));
#216207=CARTESIAN_POINT('Ctrl Pts',(-58.6294855649109,6.02209871088772,
2.62645231033236));
#216208=CARTESIAN_POINT('Ctrl Pts',(-58.6276571841746,6.02669041419593,
2.62429246650348));
#216209=CARTESIAN_POINT('Ctrl Pts',(-58.6258911397673,6.03135673055019,
2.62224491711748));
#216210=CARTESIAN_POINT('Ctrl Pts',(-58.6241915206271,6.03609209717129,
2.620315336726));
#216211=CARTESIAN_POINT('Ctrl Pts',(-58.6182428536364,6.05266588034514,
2.61356180535581));
#216212=CARTESIAN_POINT('Ctrl Pts',(-58.6131078911177,6.07008552874948,
2.60825339735349));
#216213=CARTESIAN_POINT('Ctrl Pts',(-58.6089619925611,6.08811254303241,
2.60463337987613));
#216214=CARTESIAN_POINT('Ctrl Pts',(-58.6068890432827,6.09712605017387,
2.60282337113744));
#216215=CARTESIAN_POINT('Ctrl Pts',(-58.6050633610079,6.10629139889381,
2.60143545939118));
#216216=CARTESIAN_POINT('Ctrl Pts',(-58.6035068699781,6.11557877725394,
2.600500050346));
#216217=CARTESIAN_POINT('Ctrl Pts',(-58.6027286244632,6.120222466434,2.6000323458234));
#216218=CARTESIAN_POINT('Ctrl Pts',(-58.6020176767849,6.12489666302712,
2.59967776696069));
#216219=CARTESIAN_POINT('Ctrl Pts',(-58.6013767677628,6.12959764057339,
2.59944011429163));
#216220=CARTESIAN_POINT('Ctrl Pts',(-58.6007358587407,6.13429861811967,
2.59920246162257));
#216221=CARTESIAN_POINT('Ctrl Pts',(-58.600164990065,6.13902637679624,2.5990817379131));
#216222=CARTESIAN_POINT('Ctrl Pts',(-58.5996668978649,6.14377718965303,
2.59908173516027));
#216223=CARTESIAN_POINT('',(-58.5964866834551,6.17403490859001,2.59908173516028));
#216224=CARTESIAN_POINT('Origin',(3.34731138317026E-16,1.91114605089249E-13,
2.59908173516024));
#216225=CARTESIAN_POINT('',(-58.7519447039088,6.49374646112719,2.90134173516027));
#216226=CARTESIAN_POINT('Ctrl Pts',(-58.5964866834551,6.17403490859001,
2.59908173516027));
#216227=CARTESIAN_POINT('Ctrl Pts',(-58.5960874772333,6.17782374318206,
2.59908174371516));
#216228=CARTESIAN_POINT('Ctrl Pts',(-58.5957361140451,6.18160715078384,
2.59915764355894));
#216229=CARTESIAN_POINT('Ctrl Pts',(-58.5954317101325,6.18538309648757,
2.59930765775281));
#216230=CARTESIAN_POINT('Ctrl Pts',(-58.5936345324521,6.20767599437474,
2.60019333020889));
#216231=CARTESIAN_POINT('Ctrl Pts',(-58.5934722580544,6.22971127560576,
2.60365973324126));
#216232=CARTESIAN_POINT('Ctrl Pts',(-58.5947642147754,6.25106353435537,
2.60934177082473));
#216233=CARTESIAN_POINT('Ctrl Pts',(-58.5952468467989,6.25904002743775,
2.61146439091893));
#216234=CARTESIAN_POINT('Ctrl Pts',(-58.595932158504,6.26692152735706,2.61389584429345));
#216235=CARTESIAN_POINT('Ctrl Pts',(-58.5968099398848,6.27468709076421,
2.61661604385256));
#216236=CARTESIAN_POINT('Ctrl Pts',(-58.5974948289522,6.28074617289512,
2.61873848000779));
#216237=CARTESIAN_POINT('Ctrl Pts',(-58.5982971695201,6.2867342495218,2.62103707099791));
#216238=CARTESIAN_POINT('Ctrl Pts',(-58.5992123816356,6.2926409427142,2.62350262767655));
#216239=CARTESIAN_POINT('Ctrl Pts',(-58.6024156240399,6.31331436888757,
2.63213207605182));
#216240=CARTESIAN_POINT('Ctrl Pts',(-58.6070015340112,6.33299084698429,
2.64280685971917));
#216241=CARTESIAN_POINT('Ctrl Pts',(-58.6127738370723,6.35122543337802,
2.65513293646087));
#216242=CARTESIAN_POINT('Ctrl Pts',(-58.6156599886029,6.36034272657488,
2.66129597483171));
#216243=CARTESIAN_POINT('Ctrl Pts',(-58.6188427402045,6.36909954705081,
2.66787183533855));
#216244=CARTESIAN_POINT('Ctrl Pts',(-58.6222975626532,6.37744027742862,
2.67481125953864));
#216245=CARTESIAN_POINT('Ctrl Pts',(-58.6257376244687,6.38574537226665,
2.68172103524082));
#216246=CARTESIAN_POINT('Ctrl Pts',(-58.6294472538099,6.3936380972257,2.6889910132979));
#216247=CARTESIAN_POINT('Ctrl Pts',(-58.6334027859058,6.40106302694644,
2.69657334701276));
#216248=CARTESIAN_POINT('Ctrl Pts',(-58.6334197583214,6.40109488586962,
2.69660588132573));
#216249=CARTESIAN_POINT('Ctrl Pts',(-58.633436734872,6.40112673655768,2.69663842081382));
#216250=CARTESIAN_POINT('Ctrl Pts',(-58.6334537155557,6.40115857900999,
2.69667096547382));
#216251=CARTESIAN_POINT('Ctrl Pts',(-58.6414614796113,6.41617486746512,
2.7120184015799));
#216252=CARTESIAN_POINT('Ctrl Pts',(-58.6503516547099,6.42935337961519,
2.72845645939456));
#216253=CARTESIAN_POINT('Ctrl Pts',(-58.6599343882018,6.44073642151277,
2.74568723187065));
#216254=CARTESIAN_POINT('Ctrl Pts',(-58.6698657226828,6.45253355607693,
2.7635448259456));
#216255=CARTESIAN_POINT('Ctrl Pts',(-58.6805417107313,6.46240257578875,
2.78225519317439));
#216256=CARTESIAN_POINT('Ctrl Pts',(-58.6917721934532,6.47034286301753,
2.80151223085897));
#216257=CARTESIAN_POINT('Ctrl Pts',(-58.7028423919877,6.47816982453123,
2.82049442740706));
#216258=CARTESIAN_POINT('Ctrl Pts',(-58.7144522959237,6.48412273326722,
2.84000929089754));
#216259=CARTESIAN_POINT('Ctrl Pts',(-58.726426816322,6.48815321522669,2.85976644342169));
#216260=CARTESIAN_POINT('Ctrl Pts',(-58.7347756649898,6.49096333895761,
2.87354148167318));
#216261=CARTESIAN_POINT('Ctrl Pts',(-58.7433019189624,6.49283796829162,
2.88743438345675));
#216262=CARTESIAN_POINT('Ctrl Pts',(-58.7519447039089,6.49374646112717,
2.90134173516027));
#216263=CARTESIAN_POINT('',(-59.1062911958297,6.53099325080035,3.47153072139076));
#216264=CARTESIAN_POINT('',(-58.7519447039089,6.4937464611272,2.90134173516027));
#216265=CARTESIAN_POINT('',(-58.2316113004782,12.053504764932,3.4715307213908));
#216266=CARTESIAN_POINT('Origin',(5.53234440788222E-15,1.85015204418142E-13,
3.47153072139072));
#216267=CARTESIAN_POINT('',(-57.8830978693156,11.979429479061,2.90134173516031));
#216268=CARTESIAN_POINT('',(-58.2316113004781,12.053504764932,3.4715307213908));
#216269=CARTESIAN_POINT('',(-57.6364522029208,12.2354540642043,2.59908173516031));
#216270=CARTESIAN_POINT('Ctrl Pts',(-57.8830978693156,11.979429479061,2.90134173516031));
#216271=CARTESIAN_POINT('Ctrl Pts',(-57.8711351342684,11.9768868675913,
2.88176998919809));
#216272=CARTESIAN_POINT('Ctrl Pts',(-57.8588264200507,11.9762358312607,
2.86226752356722));
#216273=CARTESIAN_POINT('Ctrl Pts',(-57.8463495993371,11.9774374689412,
2.84310370500015));
#216274=CARTESIAN_POINT('Ctrl Pts',(-57.8336474016779,11.9786608125864,
2.8235937178865));
#216275=CARTESIAN_POINT('Ctrl Pts',(-57.8207700703895,11.9818041414837,
2.80443322636989));
#216276=CARTESIAN_POINT('Ctrl Pts',(-57.8078866382221,11.9868762719075,
2.78589323878247));
#216277=CARTESIAN_POINT('Ctrl Pts',(-57.7955486571692,11.99173366148,2.76813818619992));
#216278=CARTESIAN_POINT('Ctrl Pts',(-57.7832042421973,11.9983602045449,
2.75095095198714));
#216279=CARTESIAN_POINT('Ctrl Pts',(-57.7709977973496,12.0068082271144,
2.73457771435122));
#216280=CARTESIAN_POINT('Ctrl Pts',(-57.7612891925164,12.0135275064601,
2.72155497955582));
#216281=CARTESIAN_POINT('Ctrl Pts',(-57.7516676540268,12.0213998814549,
2.70904711159967));
#216282=CARTESIAN_POINT('Ctrl Pts',(-57.7422089227118,12.0304721974328,
2.69718956158346));
#216283=CARTESIAN_POINT('Ctrl Pts',(-57.7421831034479,12.0304969619084,
2.69715719432363));
#216284=CARTESIAN_POINT('Ctrl Pts',(-57.7421572855746,12.0305217353328,
2.69712483219029));
#216285=CARTESIAN_POINT('Ctrl Pts',(-57.7421314690941,12.0305465177056,
2.69709247518657));
#216286=CARTESIAN_POINT('Ctrl Pts',(-57.7369922269699,12.0354799018088,
2.69065122242283));
#216287=CARTESIAN_POINT('Ctrl Pts',(-57.7319074031292,12.0408044207743,
2.68442464469433));
#216288=CARTESIAN_POINT('Ctrl Pts',(-57.726903735797,12.0464896431815,2.67844505923586));
#216289=CARTESIAN_POINT('Ctrl Pts',(-57.7169736114625,12.0577723607613,
2.66657815779574));
#216290=CARTESIAN_POINT('Ctrl Pts',(-57.7073630976788,12.0704771166537,
2.65568445664181));
#216291=CARTESIAN_POINT('Ctrl Pts',(-57.698281056648,12.0843744369111,2.64601906229522));
#216292=CARTESIAN_POINT('Ctrl Pts',(-57.6914695258749,12.0947974271042,
2.63877001653528));
#216293=CARTESIAN_POINT('Ctrl Pts',(-57.6849552602293,12.105891234591,2.63221189387608));
#216294=CARTESIAN_POINT('Ctrl Pts',(-57.6788263845868,12.1175590523201,
2.6264523103324));
#216295=CARTESIAN_POINT('Ctrl Pts',(-57.6765280562209,12.1219344839685,
2.62429246650352));
#216296=CARTESIAN_POINT('Ctrl Pts',(-57.674283923512,12.1263906358456,2.62224491711752));
#216297=CARTESIAN_POINT('Ctrl Pts',(-57.6720986344673,12.130922403056,2.62031533672604));
#216298=CARTESIAN_POINT('Ctrl Pts',(-57.6644501228111,12.1467835882925,
2.61356180535585));
#216299=CARTESIAN_POINT('Ctrl Pts',(-57.6575224410761,12.1635710602992,
2.60825339735355));
#216300=CARTESIAN_POINT('Ctrl Pts',(-57.6515149180852,12.1810659563067,
2.60463337987618));
#216301=CARTESIAN_POINT('Ctrl Pts',(-57.6485111565898,12.1898134043104,
2.6028233711375));
#216302=CARTESIAN_POINT('Ctrl Pts',(-57.6457374357765,12.1987377085285,
2.60143545939121));
#216303=CARTESIAN_POINT('Ctrl Pts',(-57.6432186759796,12.2078115120428,
2.60050005034603));
#216304=CARTESIAN_POINT('Ctrl Pts',(-57.6419592960812,12.2123484137999,
2.60003234582343));
#216305=CARTESIAN_POINT('Ctrl Pts',(-57.6407636564617,12.2169226903867,
2.59967776696073));
#216306=CARTESIAN_POINT('Ctrl Pts',(-57.6396348724476,12.221530922251,2.59944011429167));
#216307=CARTESIAN_POINT('Ctrl Pts',(-57.6385060884334,12.2261391541152,
2.59920246162261));
#216308=CARTESIAN_POINT('Ctrl Pts',(-57.637444161687,12.2307813416097,2.59908173791317));
#216309=CARTESIAN_POINT('Ctrl Pts',(-57.6364522029208,12.2354540642043,
2.59908173516031));
#216310=CARTESIAN_POINT('',(-57.6301266171958,12.2652136052659,2.59908173516031));
#216311=CARTESIAN_POINT('Origin',(3.35846787602729E-16,1.91121649021616E-13,
2.59908173516024));
#216312=CARTESIAN_POINT('',(-57.7513140650721,12.599423532447,2.9013417351603));
#216313=CARTESIAN_POINT('Ctrl Pts',(-57.6301266171958,12.2652136052659,
2.59908173516031));
#216314=CARTESIAN_POINT('Ctrl Pts',(-57.62933355681,12.2689399558127,2.5990817437152));
#216315=CARTESIAN_POINT('Ctrl Pts',(-57.6285886446436,12.2726659100577,
2.59915764355898));
#216316=CARTESIAN_POINT('Ctrl Pts',(-57.6278912144856,12.2763893518626,
2.59930765775284));
#216317=CARTESIAN_POINT('Ctrl Pts',(-57.6237736395748,12.2983722707008,
2.60019333020891));
#216318=CARTESIAN_POINT('Ctrl Pts',(-57.6213089400485,12.3202698780616,
2.6036597332411));
#216319=CARTESIAN_POINT('Ctrl Pts',(-57.620361900501,12.3416402131538,2.6093417708243));
#216320=CARTESIAN_POINT('Ctrl Pts',(-57.6200081180516,12.3496234589568,
2.61146439091861));
#216321=CARTESIAN_POINT('Ctrl Pts',(-57.6198658344726,12.3575334177749,
2.6138958442933));
#216322=CARTESIAN_POINT('Ctrl Pts',(-57.6199270848658,12.3653481937526,
2.61661604385262));
#216323=CARTESIAN_POINT('Ctrl Pts',(-57.6199748754952,12.3714456739993,
2.61873848000785));
#216324=CARTESIAN_POINT('Ctrl Pts',(-57.6201468963099,12.3774848147423,
2.62103707099796));
#216325=CARTESIAN_POINT('Ctrl Pts',(-57.6204396772352,12.3834548161674,
2.62350262767661));
#216326=CARTESIAN_POINT('Ctrl Pts',(-57.6214644104741,12.4043498211551,
2.63213207605187));
#216327=CARTESIAN_POINT('Ctrl Pts',(-57.6239684463328,12.424397867568,2.64280685971922));
#216328=CARTESIAN_POINT('Ctrl Pts',(-57.6278030948197,12.443135932958,2.65513293646092));
#216329=CARTESIAN_POINT('Ctrl Pts',(-57.6297204190631,12.452504965653,2.66129597483176));
#216330=CARTESIAN_POINT('Ctrl Pts',(-57.631970398231,12.461546503484,2.66787183533859));
#216331=CARTESIAN_POINT('Ctrl Pts',(-57.634534451072,12.4702026697495,2.67481125953868));
#216332=CARTESIAN_POINT('Ctrl Pts',(-57.6370875490681,12.4788218527842,
2.68172103524086));
#216333=CARTESIAN_POINT('Ctrl Pts',(-57.6399518422608,12.4870591024244,
2.68899101329793));
#216334=CARTESIAN_POINT('Ctrl Pts',(-57.6431095890443,12.4948568232947,
2.69657334701279));
#216335=CARTESIAN_POINT('Ctrl Pts',(-57.6431231383189,12.4948902817918,
2.69660588132577));
#216336=CARTESIAN_POINT('Ctrl Pts',(-57.6431366925668,12.4949237325312,
2.69663842081385));
#216337=CARTESIAN_POINT('Ctrl Pts',(-57.643150251786,12.494957175512,2.69667096547386));
#216338=CARTESIAN_POINT('Ctrl Pts',(-57.6495445189162,12.5107282424394,
2.71201840158057));
#216339=CARTESIAN_POINT('Ctrl Pts',(-57.6570084630825,12.5247638376628,
2.72845645939596));
#216340=CARTESIAN_POINT('Ctrl Pts',(-57.6653488494813,12.537086190472,2.74568723187283));
#216341=CARTESIAN_POINT('Ctrl Pts',(-57.6739926427264,12.5498568062306,
2.7635448259486));
#216342=CARTESIAN_POINT('Ctrl Pts',(-57.6835785531314,12.5607877070446,
2.78225519317828));
#216343=CARTESIAN_POINT('Ctrl Pts',(-57.6939175280725,12.5698584016499,
2.80151223086376));
#216344=CARTESIAN_POINT('Ctrl Pts',(-57.7041089426426,12.5787996370904,
2.82049442741271));
#216345=CARTESIAN_POINT('Ctrl Pts',(-57.7150329979085,12.5859335005865,
2.84000929090405));
#216346=CARTESIAN_POINT('Ctrl Pts',(-57.7265206205463,12.5911935813594,
2.85976644342905));
#216347=CARTESIAN_POINT('Ctrl Pts',(-57.734529995431,12.5948610032589,2.87354148167813));
#216348=CARTESIAN_POINT('Ctrl Pts',(-57.7428135895673,12.5976165994018,
2.88743438345924));
#216349=CARTESIAN_POINT('Ctrl Pts',(-57.7513140650721,12.599423532447,2.9013417351603));
#216350=CARTESIAN_POINT('',(-58.0998260601481,12.6735055745739,3.4715307213908));
#216351=CARTESIAN_POINT('',(-57.7513140650721,12.599423532447,2.9013417351603));
#216352=CARTESIAN_POINT('',(-56.6526781108324,18.074335247489,3.47153072139084));
#216353=CARTESIAN_POINT('Origin',(5.53234440788222E-15,1.85015204418142E-13,
3.47153072139072));
#216354=CARTESIAN_POINT('',(-56.3138168485096,17.9642361803971,2.90134173516035));
#216355=CARTESIAN_POINT('',(-56.6526781108324,18.074335247489,3.47153072139084));
#216356=CARTESIAN_POINT('',(-56.0417604764384,18.1930767435948,2.59908173516036));
#216357=CARTESIAN_POINT('Ctrl Pts',(-56.3138168485096,17.9642361803971,
2.90134173516035));
#216358=CARTESIAN_POINT('Ctrl Pts',(-56.3021854218461,17.9604570513083,
2.88176998919808));
#216359=CARTESIAN_POINT('Ctrl Pts',(-56.2900121878799,17.958522970441,2.86226752356716));
#216360=CARTESIAN_POINT('Ctrl Pts',(-56.2774781111554,17.958413842529,2.84310370500003));
#216361=CARTESIAN_POINT('Ctrl Pts',(-56.2647176232329,17.9583027433683,
2.82359371788659));
#216362=CARTESIAN_POINT('Ctrl Pts',(-56.2515822679736,17.9600828051304,
2.80443322637017));
#216363=CARTESIAN_POINT('Ctrl Pts',(-56.2382392305972,17.9637804645268,
2.78589323878292));
#216364=CARTESIAN_POINT('Ctrl Pts',(-56.2254611028283,17.9673215746115,
2.76813818620094));
#216365=CARTESIAN_POINT('Ctrl Pts',(-56.2124916494903,17.9726214740528,
2.75095095198868));
#216366=CARTESIAN_POINT('Ctrl Pts',(-56.1994690140083,17.9797472965484,
2.73457771435322));
#216367=CARTESIAN_POINT('Ctrl Pts',(-56.1891112379835,17.9854149414352,
2.72155497955712));
#216368=CARTESIAN_POINT('Ctrl Pts',(-56.1787195200274,17.9922384661037,
2.70904711160031));
#216369=CARTESIAN_POINT('Ctrl Pts',(-56.1683642893843,18.0002723763371,
2.6971895615835));
#216370=CARTESIAN_POINT('Ctrl Pts',(-56.1683360229684,18.0002943063023,
2.69715719432367));
#216371=CARTESIAN_POINT('Ctrl Pts',(-56.1683077570002,18.0003162453126,
2.69712483219033));
#216372=CARTESIAN_POINT('Ctrl Pts',(-56.1682794914817,18.000338193368,2.69709247518661));
#216373=CARTESIAN_POINT('Ctrl Pts',(-56.1626527236046,18.0047073547952,
2.69065122242287));
#216374=CARTESIAN_POINT('Ctrl Pts',(-56.1570391911759,18.0094711966667,
2.68442464469436));
#216375=CARTESIAN_POINT('Ctrl Pts',(-56.1514686668952,18.0146022491738,
2.67844505923589));
#216376=CARTESIAN_POINT('Ctrl Pts',(-56.1404135756907,18.0247851782094,
2.66657815779577));
#216377=CARTESIAN_POINT('Ctrl Pts',(-56.1295277006975,18.0364157638827,
2.65568445664184));
#216378=CARTESIAN_POINT('Ctrl Pts',(-56.1190427465077,18.0492876213733,
2.64601906229525));
#216379=CARTESIAN_POINT('Ctrl Pts',(-56.1111790308653,18.0589415144913,
2.63877001653531));
#216380=CARTESIAN_POINT('Ctrl Pts',(-56.1035408324002,18.0692936227627,
2.63221189387612));
#216381=CARTESIAN_POINT('Ctrl Pts',(-56.0962259123228,18.080256881013,2.62645231033244));
#216382=CARTESIAN_POINT('Ctrl Pts',(-56.0934828172938,18.0843681028569,
2.62429246650356));
#216383=CARTESIAN_POINT('Ctrl Pts',(-56.0907851834709,18.0885652677243,
2.62224491711756));
#216384=CARTESIAN_POINT('Ctrl Pts',(-56.0881381670059,18.0928437845341,
2.62031533672608));
#216385=CARTESIAN_POINT('Ctrl Pts',(-56.0788736093784,18.1078185933685,
2.61356180535589));
#216386=CARTESIAN_POINT('Ctrl Pts',(-56.0702291095578,18.1237899619214,
2.60825339735359));
#216387=CARTESIAN_POINT('Ctrl Pts',(-56.0624257818118,18.1405610619117,
2.60463337987622));
#216388=CARTESIAN_POINT('Ctrl Pts',(-56.0585241179387,18.1489466119069,
2.60282337113754));
#216389=CARTESIAN_POINT('Ctrl Pts',(-56.0548327480526,18.1575320950786,
2.60143545939126));
#216390=CARTESIAN_POINT('Ctrl Pts',(-56.0513793155481,18.1662929092569,
2.60050005034608));
#216391=CARTESIAN_POINT('Ctrl Pts',(-56.0496525992959,18.170673316346,2.60003234582348));
#216392=CARTESIAN_POINT('Ctrl Pts',(-56.0479853674132,18.1750975561951,
2.59967776696078));
#216393=CARTESIAN_POINT('Ctrl Pts',(-56.0463810756008,18.1795625536246,
2.59944011429172));
#216394=CARTESIAN_POINT('Ctrl Pts',(-56.0447767837884,18.1840275510541,
2.59920246162266));
#216395=CARTESIAN_POINT('Ctrl Pts',(-56.0432354336628,18.1885333065889,
2.59908173791323));
#216396=CARTESIAN_POINT('Ctrl Pts',(-56.0417604764384,18.1930767435948,
2.59908173516036));
#216397=CARTESIAN_POINT('',(-56.0323588238392,18.2220120550216,2.59908173516035));
#216398=CARTESIAN_POINT('Origin',(3.37692616670652E-16,1.9112853774948E-13,
2.59908173516024));
#216399=CARTESIAN_POINT('',(-56.1179479440989,18.5670586829464,2.90134173516035));
#216400=CARTESIAN_POINT('Ctrl Pts',(-56.0323588238392,18.2220120550216,
2.59908173516036));
#216401=CARTESIAN_POINT('Ctrl Pts',(-56.0311805982249,18.2256350948468,
2.59908174371523));
#216402=CARTESIAN_POINT('Ctrl Pts',(-56.0300502984939,18.2292627734005,
2.59915764355901));
#216403=CARTESIAN_POINT('Ctrl Pts',(-56.0289674832814,18.232892916499,2.59930765775288));
#216404=CARTESIAN_POINT('Ctrl Pts',(-56.0225746241525,18.2543250068297,
2.60019333020893));
#216405=CARTESIAN_POINT('Ctrl Pts',(-56.0178345032614,18.2758450255522,
2.60365973324109));
#216406=CARTESIAN_POINT('Ctrl Pts',(-56.0146588434089,18.296999299124,2.60934177082421));
#216407=CARTESIAN_POINT('Ctrl Pts',(-56.0134725226011,18.3049018315356,
2.61146439091855));
#216408=CARTESIAN_POINT('Ctrl Pts',(-56.0125042026266,18.3127535860879,
2.61389584429327));
#216409=CARTESIAN_POINT('Ctrl Pts',(-56.01174825096,18.3205319543147,2.61661604385263));
#216410=CARTESIAN_POINT('Ctrl Pts',(-56.0111584195474,18.3266010274078,
2.61873848000787));
#216411=CARTESIAN_POINT('Ctrl Pts',(-56.0106982359127,18.3326250661773,
2.62103707099799));
#216412=CARTESIAN_POINT('Ctrl Pts',(-56.0103653778789,18.3385929672501,
2.62350262767664));
#216413=CARTESIAN_POINT('Ctrl Pts',(-56.0092003747605,18.3594806210049,
2.6321320760519));
#216414=CARTESIAN_POINT('Ctrl Pts',(-56.0095951017657,18.3796805851421,
2.64280685971925));
#216415=CARTESIAN_POINT('Ctrl Pts',(-56.0114500824671,18.3987168313629,
2.65513293646094));
#216416=CARTESIAN_POINT('Ctrl Pts',(-56.0123775728178,18.4082349544732,
2.66129597483179));
#216417=CARTESIAN_POINT('Ctrl Pts',(-56.0136701283094,18.4174621486788,
2.66787183533863));
#216418=CARTESIAN_POINT('Ctrl Pts',(-56.0153153192431,18.426338912063,2.67481125953872));
#216419=CARTESIAN_POINT('Ctrl Pts',(-56.016953481144,18.4351777497213,2.6817210352409));
#216420=CARTESIAN_POINT('Ctrl Pts',(-56.0189410563924,18.4436692750118,
2.688991013298));
#216421=CARTESIAN_POINT('Ctrl Pts',(-56.0212664209291,18.4517543535699,
2.69657334701286));
#216422=CARTESIAN_POINT('Ctrl Pts',(-56.0212763986141,18.4517890450628,
2.69660588132583));
#216423=CARTESIAN_POINT('Ctrl Pts',(-56.021286382056,18.4518237293603,2.69663842081391));
#216424=CARTESIAN_POINT('Ctrl Pts',(-56.021296371253,18.4518584064613,2.69667096547392));
#216425=CARTESIAN_POINT('Ctrl Pts',(-56.0260070845284,18.4682114607492,
2.7120184015792));
#216426=CARTESIAN_POINT('Ctrl Pts',(-56.0319630212272,18.4829503621257,
2.72845645939294));
#216427=CARTESIAN_POINT('Ctrl Pts',(-56.0389696815128,18.4960770195692,
2.74568723186805));
#216428=CARTESIAN_POINT('Ctrl Pts',(-56.046231230313,18.5096811989822,2.76354482594212));
#216429=CARTESIAN_POINT('Ctrl Pts',(-56.0546220378327,18.5215542196609,
2.78225519317));
#216430=CARTESIAN_POINT('Ctrl Pts',(-56.0639562290182,18.5316559412141,
2.80151223085363));
#216431=CARTESIAN_POINT('Ctrl Pts',(-56.0731572003518,18.5416134885349,
2.82049442740119));
#216432=CARTESIAN_POINT('Ctrl Pts',(-56.0832757207105,18.5498501466901,
2.84000929089115));
#216433=CARTESIAN_POINT('Ctrl Pts',(-56.0941505847886,18.5562821957317,
2.8597664434148));
#216434=CARTESIAN_POINT('Ctrl Pts',(-56.1017327335067,18.5607667347609,
2.87354148166857));
#216435=CARTESIAN_POINT('Ctrl Pts',(-56.10968291102,18.5643731068268,2.88743438345449));
#216436=CARTESIAN_POINT('Ctrl Pts',(-56.1179479440989,18.5670586829464,
2.90134173516035));
#216437=CARTESIAN_POINT('',(-56.4568070719812,18.6771643191708,3.47153072139084));
#216438=CARTESIAN_POINT('',(-56.1179479440989,18.5670586829464,2.90134173516035));
#216439=CARTESIAN_POINT('',(-54.4530463244694,23.8971395307767,3.47153072139088));
#216440=CARTESIAN_POINT('Origin',(5.53234440788222E-15,1.85015204418142E-13,
3.47153072139072));
#216441=CARTESIAN_POINT('',(-54.1275498658875,23.7522229508827,2.90134173516039));
#216442=CARTESIAN_POINT('',(-54.4530463244694,23.8971395307767,3.47153072139088));
#216443=CARTESIAN_POINT('',(-53.8330634946839,23.9513722670364,2.5990817351604));
#216444=CARTESIAN_POINT('Ctrl Pts',(-54.1275498658875,23.7522229508827,
2.90134173516039));
#216445=CARTESIAN_POINT('Ctrl Pts',(-54.1163771839517,23.7472487091033,
2.88176998919681));
#216446=CARTESIAN_POINT('Ctrl Pts',(-54.1044728027349,23.7440527738937,
2.86226752356458));
#216447=CARTESIAN_POINT('Ctrl Pts',(-54.0920187959662,23.7426340760174,
2.84310370499621));
#216448=CARTESIAN_POINT('Ctrl Pts',(-54.0793398243553,23.7411897512767,
2.82359371788141));
#216449=CARTESIAN_POINT('Ctrl Pts',(-54.0660903588249,23.7415870431748,
2.80443322636371));
#216450=CARTESIAN_POINT('Ctrl Pts',(-54.0524339053478,23.7438697192146,
2.78589323877531));
#216451=CARTESIAN_POINT('Ctrl Pts',(-54.0393556307033,23.7460557526692,
2.76813818619207));
#216452=CARTESIAN_POINT('Ctrl Pts',(-54.0259032350424,23.749970941681,2.75095095197868));
#216453=CARTESIAN_POINT('Ctrl Pts',(-54.012207087644,23.7556964921021,2.73457771434229));
#216454=CARTESIAN_POINT('Ctrl Pts',(-54.0013136223926,23.7602504066258,
2.72155497955013));
#216455=CARTESIAN_POINT('Ctrl Pts',(-53.9902655788102,23.7659503210024,
2.70904711159702));
#216456=CARTESIAN_POINT('Ctrl Pts',(-53.9791273029164,23.772857804287,2.69718956158354));
#216457=CARTESIAN_POINT('Ctrl Pts',(-53.9790968990413,23.7728766594726,
2.69715719432371));
#216458=CARTESIAN_POINT('Ctrl Pts',(-53.979066494666,23.7728955237005,2.69712483219037));
#216459=CARTESIAN_POINT('Ctrl Pts',(-53.9790360897925,23.7729143969709,
2.69709247518665));
#216460=CARTESIAN_POINT('Ctrl Pts',(-53.9729834442088,23.7766714662754,
2.69065122242291));
#216461=CARTESIAN_POINT('Ctrl Pts',(-53.966902706228,23.7808224374043,2.68442464469441));
#216462=CARTESIAN_POINT('Ctrl Pts',(-53.9608263568287,23.7853431031263,
2.67844505923594));
#216463=CARTESIAN_POINT('Ctrl Pts',(-53.9487674206469,23.7943146773162,
2.66657815779582));
#216464=CARTESIAN_POINT('Ctrl Pts',(-53.9367254523685,23.80474366564,2.65568445664189));
#216465=CARTESIAN_POINT('Ctrl Pts',(-53.924952460372,23.8164490335996,2.64601906229531));
#216466=CARTESIAN_POINT('Ctrl Pts',(-53.9161227163745,23.8252280595693,
2.63877001653537));
#216467=CARTESIAN_POINT('Ctrl Pts',(-53.9074442707905,23.8347250487607,
2.63221189387617));
#216468=CARTESIAN_POINT('Ctrl Pts',(-53.8990234500734,23.8448636317806,
2.62645231033249));
#216469=CARTESIAN_POINT('Ctrl Pts',(-53.8958656423045,23.848665600413,2.62429246650361));
#216470=CARTESIAN_POINT('Ctrl Pts',(-53.8927440632083,23.8525577932541,
2.62224491711761));
#216471=CARTESIAN_POINT('Ctrl Pts',(-53.8896643205892,23.8565361833379,
2.62031533672612));
#216472=CARTESIAN_POINT('Ctrl Pts',(-53.8788852214227,23.8704605486311,
2.61356180535593));
#216473=CARTESIAN_POINT('Ctrl Pts',(-53.8686186144654,23.8854408280738,
2.60825339735363));
#216474=CARTESIAN_POINT('Ctrl Pts',(-53.8591049768559,23.901304384366,2.60463337987626));
#216475=CARTESIAN_POINT('Ctrl Pts',(-53.8543481580512,23.9092361625121,
2.60282337113758));
#216476=CARTESIAN_POINT('Ctrl Pts',(-53.8497795825132,23.9173887602871,
2.6014354593913));
#216477=CARTESIAN_POINT('Ctrl Pts',(-53.8454293138303,23.9257405998159,
2.60050005034611));
#216478=CARTESIAN_POINT('Ctrl Pts',(-53.8432541794888,23.9299165195804,
2.60003234582352));
#216479=CARTESIAN_POINT('Ctrl Pts',(-53.8411336218843,23.934142249794,2.5996777669608));
#216480=CARTESIAN_POINT('Ctrl Pts',(-53.8390713992305,23.9384150933427,
2.59944011429174));
#216481=CARTESIAN_POINT('Ctrl Pts',(-53.8370091765767,23.9426879368913,
2.59920246162268));
#216482=CARTESIAN_POINT('Ctrl Pts',(-53.8350052904264,23.9470078944659,
2.59908173791324));
#216483=CARTESIAN_POINT('Ctrl Pts',(-53.8330634946839,23.9513722670364,
2.59908173516039));
#216484=CARTESIAN_POINT('',(-53.8206887816837,23.9791663275012,2.59908173516039));
#216485=CARTESIAN_POINT('Origin',(3.40248402231255E-16,1.91135195798496E-13,
2.59908173516024));
#216486=CARTESIAN_POINT('',(-53.8697418420146,24.3312692531087,2.90134173516039));
#216487=CARTESIAN_POINT('Ctrl Pts',(-53.8206887816837,23.9791663275012,
2.59908173516039));
#216488=CARTESIAN_POINT('Ctrl Pts',(-53.8191382997273,23.9826463618224,
2.59908174371529));
#216489=CARTESIAN_POINT('Ctrl Pts',(-53.817634996232,23.9861360190795,2.59915764355906));
#216490=CARTESIAN_POINT('Ctrl Pts',(-53.816178659515,23.9896330908641,2.59930765775292));
#216491=CARTESIAN_POINT('Ctrl Pts',(-53.8075805576711,24.0102795382192,
2.60019333020891));
#216492=CARTESIAN_POINT('Ctrl Pts',(-53.8006169491722,24.0311861904733,
2.60365973324058));
#216493=CARTESIAN_POINT('Ctrl Pts',(-53.7952474622088,24.0518926318752,
2.60934177082291));
#216494=CARTESIAN_POINT('Ctrl Pts',(-53.793241600621,24.0596278690981,2.61146439091757));
#216495=CARTESIAN_POINT('Ctrl Pts',(-53.791457853367,24.0673353939202,2.61389584429274));
#216496=CARTESIAN_POINT('Ctrl Pts',(-53.7898929820049,24.0749921329677,
2.61661604385268));
#216497=CARTESIAN_POINT('Ctrl Pts',(-53.7886719908666,24.0809663048721,
2.61873848000792));
#216498=CARTESIAN_POINT('Ctrl Pts',(-53.7875846446508,24.0869092410388,
2.62103707099803));
#216499=CARTESIAN_POINT('Ctrl Pts',(-53.78662979452,24.0928096561863,2.62350262767668));
#216500=CARTESIAN_POINT('Ctrl Pts',(-53.7832878190623,24.1134611092026,
2.63213207605195));
#216501=CARTESIAN_POINT('Ctrl Pts',(-53.7815689125024,24.1335916760301,
2.6428068597193));
#216502=CARTESIAN_POINT('Ctrl Pts',(-53.7814239018616,24.1527175379843,
2.655132936461));
#216503=CARTESIAN_POINT('Ctrl Pts',(-53.7813513965412,24.1622804689615,
2.66129597483185));
#216504=CARTESIAN_POINT('Ctrl Pts',(-53.7816723668479,24.1715922244709,
2.66787183533867));
#216505=CARTESIAN_POINT('Ctrl Pts',(-53.7823806708182,24.1805923292966,
2.67481125953876));
#216506=CARTESIAN_POINT('Ctrl Pts',(-53.7830859485794,24.1895539814234,
2.68172103524095));
#216507=CARTESIAN_POINT('Ctrl Pts',(-53.7841750295932,24.1982067474363,
2.68899101329804));
#216508=CARTESIAN_POINT('Ctrl Pts',(-53.7856425347025,24.2064906018697,
2.6965733470129));
#216509=CARTESIAN_POINT('Ctrl Pts',(-53.7856488314803,24.206526146271,2.69660588132587));
#216510=CARTESIAN_POINT('Ctrl Pts',(-53.7856551347356,24.2065616841181,
2.69663842081396));
#216511=CARTESIAN_POINT('Ctrl Pts',(-53.7856614444666,24.2065972154097,
2.69667096547396));
#216512=CARTESIAN_POINT('Ctrl Pts',(-53.7886369923274,24.2233530895752,
2.71201840157957));
#216513=CARTESIAN_POINT('Ctrl Pts',(-53.7930196670707,24.2386338146185,
2.72845645939369));
#216514=CARTESIAN_POINT('Ctrl Pts',(-53.7986158348079,24.2524209582917,
2.74568723186921));
#216515=CARTESIAN_POINT('Ctrl Pts',(-53.8044155801161,24.2667096511237,
2.76354482594357));
#216516=CARTESIAN_POINT('Ctrl Pts',(-53.8115193533084,24.2793947083685,
2.78225519317175));
#216517=CARTESIAN_POINT('Ctrl Pts',(-53.8197464933879,24.2904167802946,
2.80151223085569));
#216518=CARTESIAN_POINT('Ctrl Pts',(-53.8278562137185,24.3012815425233,
2.82049442740332));
#216519=CARTESIAN_POINT('Ctrl Pts',(-53.8370583385447,24.3105307527869,
2.84000929089333));
#216520=CARTESIAN_POINT('Ctrl Pts',(-53.8472012967776,24.3180642992209,
2.85976644341703));
#216521=CARTESIAN_POINT('Ctrl Pts',(-53.8542731477182,24.3233168218295,
2.87354148167009));
#216522=CARTESIAN_POINT('Ctrl Pts',(-53.8618028047969,24.3277344576498,
2.88743438345526));
#216523=CARTESIAN_POINT('Ctrl Pts',(-53.8697418420146,24.3312692531087,
2.90134173516039));
#216524=CARTESIAN_POINT('',(-54.1952354911873,24.4761921430391,3.47153072139088));
#216525=CARTESIAN_POINT('',(-53.8697418420146,24.3312692531087,2.90134173516039));
#216526=CARTESIAN_POINT('',(-51.6568155675429,29.4581217525673,3.47153072139092));
#216527=CARTESIAN_POINT('Origin',(5.53234440788222E-15,1.85015204418142E-13,
3.47153072139072));
#216528=CARTESIAN_POINT('',(-51.3482501200167,29.2799753962461,2.90134173516043));
#216529=CARTESIAN_POINT('',(-51.6568155675429,29.4581217525673,3.47153072139092));
#216530=CARTESIAN_POINT('',(-51.0345602039888,29.4472515437734,2.59908173516043));
#216531=CARTESIAN_POINT('Ctrl Pts',(-51.3482501200167,29.2799753962461,
2.90134173516043));
#216532=CARTESIAN_POINT('Ctrl Pts',(-51.3376585930506,29.2738605406102,
2.88176998919663));
#216533=CARTESIAN_POINT('Ctrl Pts',(-51.3261534914758,29.2694377663933,
2.86226752356419));
#216534=CARTESIAN_POINT('Ctrl Pts',(-51.313916003368,29.2667250421033,2.84310370499561));
#216535=CARTESIAN_POINT('Ctrl Pts',(-51.3014574615356,29.2639633161063,
2.82359371788049));
#216536=CARTESIAN_POINT('Ctrl Pts',(-51.2882390496519,29.2629734853269,
2.80443322636248));
#216537=CARTESIAN_POINT('Ctrl Pts',(-51.2744188030369,29.263816168533,2.7858932387738));
#216538=CARTESIAN_POINT('Ctrl Pts',(-51.2611836698312,29.264623174717,2.7681381861901));
#216539=CARTESIAN_POINT('Ctrl Pts',(-51.2473957191101,29.2671107576683,
2.75095095197629));
#216540=CARTESIAN_POINT('Ctrl Pts',(-51.2331761176528,29.2713733056852,
2.73457771433953));
#216541=CARTESIAN_POINT('Ctrl Pts',(-51.2218663142576,29.2747635962062,
2.72155497954838));
#216542=CARTESIAN_POINT('Ctrl Pts',(-51.2102829897242,29.2792774508374,
2.70904711159621));
#216543=CARTESIAN_POINT('Ctrl Pts',(-51.1984837018592,29.2849828273428,
2.69718956158358));
#216544=CARTESIAN_POINT('Ctrl Pts',(-51.1984514936361,29.2849984011674,
2.69715719432375));
#216545=CARTESIAN_POINT('Ctrl Pts',(-51.1984192839704,29.2850139839325,
2.69712483219041));
#216546=CARTESIAN_POINT('Ctrl Pts',(-51.198387072864,29.2850295756385,2.69709247518669));
#216547=CARTESIAN_POINT('Ctrl Pts',(-51.1919748636254,29.2881333895826,
2.69065122242294));
#216548=CARTESIAN_POINT('Ctrl Pts',(-51.1854935419303,29.2916260110607,
2.68442464469444));
#216549=CARTESIAN_POINT('Ctrl Pts',(-51.1789779411679,29.2954867606378,
2.67844505923596));
#216550=CARTESIAN_POINT('Ctrl Pts',(-51.1660472802371,29.303148685538,2.66657815779585));
#216551=CARTESIAN_POINT('Ctrl Pts',(-51.152981152998,29.3122618143336,2.65568445664191));
#216552=CARTESIAN_POINT('Ctrl Pts',(-51.1400491105586,29.3226724463013,
2.64601906229532));
#216553=CARTESIAN_POINT('Ctrl Pts',(-51.130350078729,29.330480420277,2.63877001653539));
#216554=CARTESIAN_POINT('Ctrl Pts',(-51.1207264688922,29.3390182393876,
2.6322118938762));
#216555=CARTESIAN_POINT('Ctrl Pts',(-51.1112920078093,29.3482210667398,
2.62645231033252));
#216556=CARTESIAN_POINT('Ctrl Pts',(-51.1077540849032,29.3516721269969,
2.62429246650364));
#216557=CARTESIAN_POINT('Ctrl Pts',(-51.1042427612074,29.3552167041325,
2.62224491711764));
#216558=CARTESIAN_POINT('Ctrl Pts',(-51.100764034739,29.3588513794159,2.62031533672616));
#216559=CARTESIAN_POINT('Ctrl Pts',(-51.0885884920994,29.3715727429078,
2.61356180535597));
#216560=CARTESIAN_POINT('Ctrl Pts',(-51.0768122610998,29.3853978061641,
2.60825339735367));
#216561=CARTESIAN_POINT('Ctrl Pts',(-51.0656925470314,29.4001800143157,
2.6046333798763));
#216562=CARTESIAN_POINT('Ctrl Pts',(-51.0601326899972,29.4075711183915,
2.60282337113762));
#216563=CARTESIAN_POINT('Ctrl Pts',(-51.0547369630769,29.4152015092025,
2.60143545939133));
#216564=CARTESIAN_POINT('Ctrl Pts',(-51.0495375206696,29.4230528695804,
2.60050005034615));
#216565=CARTESIAN_POINT('Ctrl Pts',(-51.046937799466,29.4269785497693,2.60003234582355));
#216566=CARTESIAN_POINT('Ctrl Pts',(-51.0443871494124,29.430959472363,2.59967776696084));
#216567=CARTESIAN_POINT('Ctrl Pts',(-51.0418895900602,29.4349933478627,
2.59944011429178));
#216568=CARTESIAN_POINT('Ctrl Pts',(-51.039392030708,29.4390272233624,2.59920246162272));
#216569=CARTESIAN_POINT('Ctrl Pts',(-51.0369475635291,29.4431140526175,
2.59908173791332));
#216570=CARTESIAN_POINT('Ctrl Pts',(-51.0345602039888,29.4472515437734,
2.59908173516043));
#216571=CARTESIAN_POINT('',(-51.0193480105329,29.4735998357337,2.59908173516043));
#216572=CARTESIAN_POINT('Origin',(3.434861425631E-16,1.91141550221685E-13,
2.59908173516024));
#216573=CARTESIAN_POINT('',(-51.031327575341,29.8289013456885,2.90134173516044));
#216574=CARTESIAN_POINT('Ctrl Pts',(-51.0193480105329,29.4735998357337,
2.59908173516043));
#216575=CARTESIAN_POINT('Ctrl Pts',(-51.0174422596392,29.4768987365664,
2.59908174371533));
#216576=CARTESIAN_POINT('Ctrl Pts',(-51.0155824228873,29.4802121391118,
2.5991576435591));
#216577=CARTESIAN_POINT('Ctrl Pts',(-51.0137685205956,29.4835378249322,
2.59930765775296));
#216578=CARTESIAN_POINT('Ctrl Pts',(-51.0030593786377,29.5031724225187,
2.60019333020908));
#216579=CARTESIAN_POINT('Ctrl Pts',(-50.9939485772814,29.5232366506522,
2.60365973324168));
#216580=CARTESIAN_POINT('Ctrl Pts',(-50.9864440924292,29.5432683957837,
2.60934177082554));
#216581=CARTESIAN_POINT('Ctrl Pts',(-50.9836406667025,29.5507515889354,
2.61146439091959));
#216582=CARTESIAN_POINT('Ctrl Pts',(-50.9810610352785,29.5582304387677,
2.6138958442939));
#216583=CARTESIAN_POINT('Ctrl Pts',(-50.9787043892802,29.5656816597958,
2.61661604385273));
#216584=CARTESIAN_POINT('Ctrl Pts',(-50.9768656158506,29.5714954762341,
2.61873848000796));
#216585=CARTESIAN_POINT('Ctrl Pts',(-50.9751630202463,29.5772921977456,
2.62103707099807));
#216586=CARTESIAN_POINT('Ctrl Pts',(-50.9735966395564,29.5830604807848,
2.62350262767672));
#216587=CARTESIAN_POINT('Ctrl Pts',(-50.9681143071419,29.6032494714219,
2.63213207605199));
#216588=CARTESIAN_POINT('Ctrl Pts',(-50.9643005997168,29.6230900862367,
2.64280685971934));
#216589=CARTESIAN_POINT('Ctrl Pts',(-50.9621571865007,29.6420960169786,
2.65513293646104));
#216590=CARTESIAN_POINT('Ctrl Pts',(-50.9610854798927,29.6515989823495,
2.66129597483189));
#216591=CARTESIAN_POINT('Ctrl Pts',(-50.9604313483968,29.6608932776209,
2.66787183533872));
#216592=CARTESIAN_POINT('Ctrl Pts',(-50.9601950050771,29.6699181168562,
2.67481125953881));
#216593=CARTESIAN_POINT('Ctrl Pts',(-50.9599596715278,29.6789043977155,
2.68172103524099));
#216594=CARTESIAN_POINT('Ctrl Pts',(-50.9601383261075,29.6876236029356,
2.68899101329808));
#216595=CARTESIAN_POINT('Ctrl Pts',(-50.9607318934965,29.6960154736015,
2.69657334701294));
#216596=CARTESIAN_POINT('Ctrl Pts',(-50.9607344403782,29.6960514814794,
2.69660588132591));
#216597=CARTESIAN_POINT('Ctrl Pts',(-50.960736994387,29.6960874835161,2.696638420814));
#216598=CARTESIAN_POINT('Ctrl Pts',(-50.9607395555213,29.69612347971,2.69667096547401));
#216599=CARTESIAN_POINT('Ctrl Pts',(-50.9619473372423,29.713098592887,2.71201840157792));
#216600=CARTESIAN_POINT('Ctrl Pts',(-50.964708732528,29.728753722774,2.72845645939011));
#216601=CARTESIAN_POINT('Ctrl Pts',(-50.968833094931,29.743050297844,2.74568723186355));
#216602=CARTESIAN_POINT('Ctrl Pts',(-50.973107493523,29.7578669541847,2.76354482593593));
#216603=CARTESIAN_POINT('Ctrl Pts',(-50.9788464019613,29.771225067853,2.78225519316198));
#216604=CARTESIAN_POINT('Ctrl Pts',(-50.9858763526649,29.7830467300249,
2.80151223084375));
#216605=CARTESIAN_POINT('Ctrl Pts',(-50.9928059701984,29.7946996705526,
2.82049442738965));
#216606=CARTESIAN_POINT('Ctrl Pts',(-51.0009908790854,29.8048600966415,
2.8400092908779));
#216607=CARTESIAN_POINT('Ctrl Pts',(-51.0102908030987,29.8134126013573,
2.8597664433999));
#216608=CARTESIAN_POINT('Ctrl Pts',(-51.0167748755856,29.8193755598118,
2.87354148165858));
#216609=CARTESIAN_POINT('Ctrl Pts',(-51.0238015157341,29.8245560588468,
2.88743438344952));
#216610=CARTESIAN_POINT('Ctrl Pts',(-51.031327575341,29.8289013456885,2.90134173516043));
#216611=CARTESIAN_POINT('',(-51.3398895692699,30.0070536838157,3.47153072139092));
#216612=CARTESIAN_POINT('',(-51.031327575341,29.8289013456885,2.90134173516044));
#216613=CARTESIAN_POINT('',(-48.2946219293748,34.6963546279285,3.47153072139096));
#216614=CARTESIAN_POINT('Origin',(5.53234440788222E-15,1.85015204418142E-13,
3.47153072139072));
#216615=CARTESIAN_POINT('',(-48.0063682005189,34.4869303039396,2.90134173516046));
#216616=CARTESIAN_POINT('',(-48.2946219293748,34.6963546279284,3.47153072139096));
#216617=CARTESIAN_POINT('',(-47.6769115920306,34.6205005703634,2.59908173516047));
#216618=CARTESIAN_POINT('Ctrl Pts',(-48.0063682005189,34.4869303039396,
2.90134173516046));
#216619=CARTESIAN_POINT('Ctrl Pts',(-47.9964738715098,34.479741830086,2.88176998919909));
#216620=CARTESIAN_POINT('Ctrl Pts',(-47.985494101879,34.4741406737021,2.86226752356907));
#216621=CARTESIAN_POINT('Ctrl Pts',(-47.9736072089144,34.4701636441736,
2.84310370500279));
#216622=CARTESIAN_POINT('Ctrl Pts',(-47.9615055952539,34.4661147749682,
2.82359371788992));
#216623=CARTESIAN_POINT('Ctrl Pts',(-47.9484630607056,34.4637486663041,
2.80443322637404));
#216624=CARTESIAN_POINT('Ctrl Pts',(-47.9346304384691,34.463142124062,2.78589323878727));
#216625=CARTESIAN_POINT('Ctrl Pts',(-47.9213834535936,34.4625612612459,
2.76813818620531));
#216626=CARTESIAN_POINT('Ctrl Pts',(-47.907411011488,34.4635939836559,2.75095095199305));
#216627=CARTESIAN_POINT('Ctrl Pts',(-47.8928237489035,34.4663468278986,
2.73457771435755));
#216628=CARTESIAN_POINT('Ctrl Pts',(-47.8812215199315,34.4685363496847,
2.72155497955993));
#216629=CARTESIAN_POINT('Ctrl Pts',(-47.8692298237685,34.4718146898359,
2.70904711160169));
#216630=CARTESIAN_POINT('Ctrl Pts',(-47.8568987993929,34.4762554502657,
2.6971895615836));
#216631=CARTESIAN_POINT('Ctrl Pts',(-47.8568651397019,34.4762675720992,
2.69715719432378));
#216632=CARTESIAN_POINT('Ctrl Pts',(-47.8568314776416,34.4762797026734,
2.69712483219044));
#216633=CARTESIAN_POINT('Ctrl Pts',(-47.8567978132139,34.4762918419889,
2.69709247518672));
#216634=CARTESIAN_POINT('Ctrl Pts',(-47.8500962938266,34.4787083945376,
2.69065122242297));
#216635=CARTESIAN_POINT('Ctrl Pts',(-47.843285399134,34.4815044004731,2.68442464469447));
#216636=CARTESIAN_POINT('Ctrl Pts',(-47.836401933294,34.4846629347251,2.678445059236));
#216637=CARTESIAN_POINT('Ctrl Pts',(-47.8227412186412,34.4909312646828,
2.66657815779588));
#216638=CARTESIAN_POINT('Ctrl Pts',(-47.8087940876657,34.4986286886042,
2.65568445664195));
#216639=CARTESIAN_POINT('Ctrl Pts',(-47.7948446809467,34.5076305235176,
2.64601906229537));
#216640=CARTESIAN_POINT('Ctrl Pts',(-47.7843826259074,34.5143818997027,
2.63877001653543));
#216641=CARTESIAN_POINT('Ctrl Pts',(-47.7739192901009,34.5218670065995,
2.63221189387623));
#216642=CARTESIAN_POINT('Ctrl Pts',(-47.7635745545821,34.5300332501818,
2.62645231033255));
#216643=CARTESIAN_POINT('Ctrl Pts',(-47.7596952787625,34.5330955915252,
2.62429246650367));
#216644=CARTESIAN_POINT('Ctrl Pts',(-47.7558326812644,34.5362537178264,
2.62224491711768));
#216645=CARTESIAN_POINT('Ctrl Pts',(-47.7519930846017,34.5395048560464,
2.6203153367262));
#216646=CARTESIAN_POINT('Ctrl Pts',(-47.7385544962822,34.5508838398164,
2.61356180535601));
#216647=CARTESIAN_POINT('Ctrl Pts',(-47.7253976640914,34.5634022166003,
2.6082533973537));
#216648=CARTESIAN_POINT('Ctrl Pts',(-47.7127937034783,34.5769411196454,
2.60463337987634));
#216649=CARTESIAN_POINT('Ctrl Pts',(-47.7064917231718,34.5837105711679,
2.60282337113765));
#216650=CARTESIAN_POINT('Ctrl Pts',(-47.7003279615826,34.5907351548565,
2.60143545939137));
#216651=CARTESIAN_POINT('Ctrl Pts',(-47.69433631163,34.598000014936,2.60050005034618));
#216652=CARTESIAN_POINT('Ctrl Pts',(-47.6913404866537,34.6016324449758,
2.60003234582359));
#216653=CARTESIAN_POINT('Ctrl Pts',(-47.6883876896069,34.6053249441285,
2.59967776696089));
#216654=CARTESIAN_POINT('Ctrl Pts',(-47.6854821573391,34.6090756555952,
2.59944011429183));
#216655=CARTESIAN_POINT('Ctrl Pts',(-47.6825766250713,34.6128263670618,
2.59920246162277));
#216656=CARTESIAN_POINT('Ctrl Pts',(-47.6797183589578,34.6166352918409,
2.59908173791336));
#216657=CARTESIAN_POINT('Ctrl Pts',(-47.6769115920305,34.6205005703634,
2.59908173516047));
#216658=CARTESIAN_POINT('',(-47.6590285860937,34.6451144164185,2.59908173516047));
#216659=CARTESIAN_POINT('Origin',(3.4737036430558E-16,1.91147531398658E-13,
2.59908173516024));
#216660=CARTESIAN_POINT('',(-47.6338034047601,34.999721753026,2.90134173516047));
#216661=CARTESIAN_POINT('Ctrl Pts',(-47.6590285860937,34.6451144164185,
2.59908173516047));
#216662=CARTESIAN_POINT('Ctrl Pts',(-47.6567884460683,34.648196040315,2.59908174371537));
#216663=CARTESIAN_POINT('Ctrl Pts',(-47.6545924528205,34.651296885817,2.59915764355913));
#216664=CARTESIAN_POINT('Ctrl Pts',(-47.6524408584473,34.6544147487634,
2.599307657753));
#216665=CARTESIAN_POINT('Ctrl Pts',(-47.6397380079787,34.6728223758155,
2.60019333020899));
#216666=CARTESIAN_POINT('Ctrl Pts',(-47.6285798336134,34.6918243519402,
2.60365973324072));
#216667=CARTESIAN_POINT('Ctrl Pts',(-47.6190225715802,34.710961928804,2.60934177082314));
#216668=CARTESIAN_POINT('Ctrl Pts',(-47.615452296631,34.7181110904602,2.61146439091776));
#216669=CARTESIAN_POINT('Ctrl Pts',(-47.6121050440164,34.7252793254648,
2.61389584429288));
#216670=CARTESIAN_POINT('Ctrl Pts',(-47.6089824432867,34.7324433913425,
2.61661604385275));
#216671=CARTESIAN_POINT('Ctrl Pts',(-47.6065460335524,34.7380331549252,
2.61873848000798));
#216672=CARTESIAN_POINT('Ctrl Pts',(-47.6042468425534,34.7436201516877,
2.6210370709981));
#216673=CARTESIAN_POINT('Ctrl Pts',(-47.602086092899,34.7491931041024,2.62350262767674));
#216674=CARTESIAN_POINT('Ctrl Pts',(-47.5945234691089,34.7686984375539,
2.63213207605201));
#216675=CARTESIAN_POINT('Ctrl Pts',(-47.5886567445952,34.7880317224284,
2.64280685971936));
#216676=CARTESIAN_POINT('Ctrl Pts',(-47.5845384124876,34.8067094890034,
2.65513293646106));
#216677=CARTESIAN_POINT('Ctrl Pts',(-47.5824792464338,34.8160483722909,
2.66129597483191));
#216678=CARTESIAN_POINT('Ctrl Pts',(-47.5808571799367,34.8252233770803,
2.66787183533875));
#216679=CARTESIAN_POINT('Ctrl Pts',(-47.579678778754,34.834174072698,2.67481125953884));
#216680=CARTESIAN_POINT('Ctrl Pts',(-47.5785054122578,34.8430865267163,
2.68172103524103));
#216681=CARTESIAN_POINT('Ctrl Pts',(-47.5777716830264,34.8517766417065,
2.68899101329812));
#216682=CARTESIAN_POINT('Ctrl Pts',(-47.5774848094465,34.8601845855139,
2.69657334701298));
#216683=CARTESIAN_POINT('Ctrl Pts',(-47.577483578528,34.8602206623585,2.69660588132595));
#216684=CARTESIAN_POINT('Ctrl Pts',(-47.5774823553081,34.8602567341388,
2.69663842081403));
#216685=CARTESIAN_POINT('Ctrl Pts',(-47.5774811397854,34.8602928008533,
2.69667096547404));
#216686=CARTESIAN_POINT('Ctrl Pts',(-47.5769079226575,34.8773011701528,
2.71201840157922));
#216687=CARTESIAN_POINT('Ctrl Pts',(-47.5780177840617,34.8931591840073,
2.72845645939285));
#216688=CARTESIAN_POINT('Ctrl Pts',(-47.5806251537543,34.9078085542082,
2.74568723186784));
#216689=CARTESIAN_POINT('Ctrl Pts',(-47.5833273744258,34.9229908396723,
2.7635448259414));
#216690=CARTESIAN_POINT('Ctrl Pts',(-47.5876385414298,34.9368756554767,
2.78225519316872));
#216691=CARTESIAN_POINT('Ctrl Pts',(-47.5933942811485,34.9493673872906,
2.80151223085178));
#216692=CARTESIAN_POINT('Ctrl Pts',(-47.5990678735466,34.9616808340626,
2.82049442739819));
#216693=CARTESIAN_POINT('Ctrl Pts',(-47.6061458909216,34.972641156222,2.84000929088694));
#216694=CARTESIAN_POINT('Ctrl Pts',(-47.6145008888038,34.9821189161873,
2.85976644340938));
#216695=CARTESIAN_POINT('Ctrl Pts',(-47.6203261419784,34.9887269790624,
2.87354148166497));
#216696=CARTESIAN_POINT('Ctrl Pts',(-47.6267727798526,34.9946135826766,
2.88743438345274));
#216697=CARTESIAN_POINT('Ctrl Pts',(-47.6338034047602,34.999721753026,2.90134173516047));
#216698=CARTESIAN_POINT('',(-47.9220530736689,35.2091516650527,3.47153072139096));
#216699=CARTESIAN_POINT('',(-47.6338034047601,34.999721753026,2.90134173516047));
#216700=CARTESIAN_POINT('',(-44.4033023070491,39.554446981307,3.47153072139099));
#216701=CARTESIAN_POINT('Origin',(5.53234440788222E-15,1.85015204418142E-13,
3.47153072139072));
#216702=CARTESIAN_POINT('',(-44.1385184650378,39.3160391863689,2.9013417351605));
#216703=CARTESIAN_POINT('',(-44.4033023070491,39.554446981307,3.47153072139099));
#216704=CARTESIAN_POINT('',(-43.7969047596348,39.4144401478989,2.5990817351605));
#216705=CARTESIAN_POINT('Ctrl Pts',(-44.1385184650378,39.3160391863689,
2.9013417351605));
#216706=CARTESIAN_POINT('Ctrl Pts',(-44.1294297383223,39.30785585272,2.88176998919681));
#216707=CARTESIAN_POINT('Ctrl Pts',(-44.1190955972863,39.3011376816097,
2.86226752356449));
#216708=CARTESIAN_POINT('Ctrl Pts',(-44.1076895347485,39.2959399200101,
2.84310370499602));
#216709=CARTESIAN_POINT('Ctrl Pts',(-44.0960774370682,39.2906482678547,
2.82359371788097));
#216710=CARTESIAN_POINT('Ctrl Pts',(-44.0833536765897,39.2869318048881,
2.80443322636304));
#216711=CARTESIAN_POINT('Ctrl Pts',(-44.0696602318316,39.2848826826031,
2.78589323877442));
#216712=CARTESIAN_POINT('Ctrl Pts',(-44.0565465320208,39.2829203148427,
2.76813818619067));
#216713=CARTESIAN_POINT('Ctrl Pts',(-44.0425426835264,39.2824868619908,
2.75095095197682));
#216714=CARTESIAN_POINT('Ctrl Pts',(-44.0277475809121,39.2836998417248,
2.73457771434002));
#216715=CARTESIAN_POINT('Ctrl Pts',(-44.0159800428216,39.284664605917,2.72155497954872));
#216716=CARTESIAN_POINT('Ctrl Pts',(-44.0037113585722,39.2866715134056,
2.70904711159642));
#216717=CARTESIAN_POINT('Ctrl Pts',(-43.9909836989806,39.2897990038552,
2.69718956158366));
#216718=CARTESIAN_POINT('Ctrl Pts',(-43.9909489566042,39.2898075408882,
2.69715719432383));
#216719=CARTESIAN_POINT('Ctrl Pts',(-43.990914210958,39.2898160863664,2.69712483219049));
#216720=CARTESIAN_POINT('Ctrl Pts',(-43.9908794620435,39.2898246402906,
2.69709247518676));
#216721=CARTESIAN_POINT('Ctrl Pts',(-43.9839620557563,39.2915274551885,
2.69065122242303));
#216722=CARTESIAN_POINT('Ctrl Pts',(-43.9768962096537,39.2935962119552,
2.68442464469453));
#216723=CARTESIAN_POINT('Ctrl Pts',(-43.9697202954283,39.2960179253199,
2.67844505923606));
#216724=CARTESIAN_POINT('Ctrl Pts',(-43.955479196702,39.3008239832004,2.66657815779594));
#216725=CARTESIAN_POINT('Ctrl Pts',(-43.9408038696757,39.3070213676603,
2.655684456642));
#216726=CARTESIAN_POINT('Ctrl Pts',(-43.9259899312961,39.3145157795323,
2.64601906229541));
#216727=CARTESIAN_POINT('Ctrl Pts',(-43.9148794775114,39.3201365884364,
2.63877001653547));
#216728=CARTESIAN_POINT('Ctrl Pts',(-43.9036910542319,39.3264869747219,
2.63221189387627));
#216729=CARTESIAN_POINT('Ctrl Pts',(-43.8925493833644,39.3335271634608,
2.6264523103326));
#216730=CARTESIAN_POINT('Ctrl Pts',(-43.888371256789,39.3361672342378,2.62429246650372));
#216731=CARTESIAN_POINT('Ctrl Pts',(-43.8841997049151,39.3389043086121,
2.62224491711771));
#216732=CARTESIAN_POINT('Ctrl Pts',(-43.8800413054826,39.341736289618,2.62031533672623));
#216733=CARTESIAN_POINT('Ctrl Pts',(-43.865486907469,39.3516482231388,2.61356180535604));
#216734=CARTESIAN_POINT('Ctrl Pts',(-43.8510936230937,39.3627227594944,
2.60825339735373));
#216735=CARTESIAN_POINT('Ctrl Pts',(-43.8371435075661,39.374870022378,2.60463337987637));
#216736=CARTESIAN_POINT('Ctrl Pts',(-43.8301684498022,39.3809436538199,
2.60282337113768));
#216737=CARTESIAN_POINT('Ctrl Pts',(-43.8233041850059,39.3872854675772,
2.6014354593914));
#216738=CARTESIAN_POINT('Ctrl Pts',(-43.8165859732786,39.393884232031,2.60050005034622));
#216739=CARTESIAN_POINT('Ctrl Pts',(-43.813226867415,39.397183614258,2.60003234582362));
#216740=CARTESIAN_POINT('Ctrl Pts',(-43.8099042748374,39.4005472341764,
2.59967776696092));
#216741=CARTESIAN_POINT('Ctrl Pts',(-43.8066226032736,39.4039736880302,
2.59944011429186));
#216742=CARTESIAN_POINT('Ctrl Pts',(-43.8033409317098,39.4074001418841,
2.5992024616228));
#216743=CARTESIAN_POINT('Ctrl Pts',(-43.8001001824232,39.4108894308103,
2.59908173791338));
#216744=CARTESIAN_POINT('Ctrl Pts',(-43.7969047596348,39.4144401478989,
2.5990817351605));
#216745=CARTESIAN_POINT('',(-43.7765468711724,39.4370498736008,2.5990817351605));
#216746=CARTESIAN_POINT('Origin',(3.51858511112454E-16,1.91153073798388E-13,
2.59908173516023));
#216747=CARTESIAN_POINT('',(-43.7143933160625,39.7870778846747,2.9013417351605));
#216748=CARTESIAN_POINT('Ctrl Pts',(-43.7765468711724,39.4370498736008,
2.5990817351605));
#216749=CARTESIAN_POINT('Ctrl Pts',(-43.7739968854581,39.4398804576448,
2.59908174371538));
#216750=CARTESIAN_POINT('Ctrl Pts',(-43.771488795476,39.4427347725911,2.59915764355917));
#216751=CARTESIAN_POINT('Ctrl Pts',(-43.7690230823394,39.4456106527047,
2.59930765775303));
#216752=CARTESIAN_POINT('Ctrl Pts',(-43.7544656984466,39.4625896314113,
2.60019333020903));
#216753=CARTESIAN_POINT('Ctrl Pts',(-43.7413824023646,39.4803211659033,
2.60365973324078));
#216754=CARTESIAN_POINT('Ctrl Pts',(-43.7298770745125,39.4983548992053,
2.60934177082323));
#216755=CARTESIAN_POINT('Ctrl Pts',(-43.7255790670215,39.505091701652,2.61146439091784));
#216756=CARTESIAN_POINT('Ctrl Pts',(-43.7215008664177,39.5118707851432,
2.61389584429295));
#216757=CARTESIAN_POINT('Ctrl Pts',(-43.7176465228246,39.5186692048627,
2.6166160438528));
#216758=CARTESIAN_POINT('Ctrl Pts',(-43.7146391706003,39.5239736729702,
2.61873848000803));
#216759=CARTESIAN_POINT('Ctrl Pts',(-43.7117685746243,39.529289732678,2.62103707099814));
#216760=CARTESIAN_POINT('Ctrl Pts',(-43.7090371296309,39.5346062960354,
2.62350262767678));
#216761=CARTESIAN_POINT('Ctrl Pts',(-43.699477072154,39.5532142677863,2.63213207605205));
#216762=CARTESIAN_POINT('Ctrl Pts',(-43.6916216076132,39.5718284032055,
2.6428068597194));
#216763=CARTESIAN_POINT('Ctrl Pts',(-43.6855734779224,39.5899733680945,
2.6551329364611));
#216764=CARTESIAN_POINT('Ctrl Pts',(-43.682549413077,39.599045850539,2.66129597483194));
#216765=CARTESIAN_POINT('Ctrl Pts',(-43.6799771832788,39.6080010415739,
2.66787183533878));
#216766=CARTESIAN_POINT('Ctrl Pts',(-43.677869635043,39.6167795278797,2.67481125953887));
#216767=CARTESIAN_POINT('Ctrl Pts',(-43.6757710912487,39.6255205083456,
2.68172103524106));
#216768=CARTESIAN_POINT('Ctrl Pts',(-43.6741330170973,39.6340863223877,
2.68899101329813));
#216769=CARTESIAN_POINT('Ctrl Pts',(-43.6729688455954,39.6424182201447,
2.69657334701299));
#216770=CARTESIAN_POINT('Ctrl Pts',(-43.6729638503629,39.6424539706906,
2.69660588132596));
#216771=CARTESIAN_POINT('Ctrl Pts',(-43.6729588633162,39.6424897170046,
2.69663842081405));
#216772=CARTESIAN_POINT('Ctrl Pts',(-43.672953884454,39.6425254590851,2.69667096547406));
#216773=CARTESIAN_POINT('Ctrl Pts',(-43.6706059487636,39.659380737255,2.71201840158148));
#216774=CARTESIAN_POINT('Ctrl Pts',(-43.6700521164124,39.6752678913595,
2.72845645939766));
#216775=CARTESIAN_POINT('Ctrl Pts',(-43.6711139265066,39.6901095551267,
2.74568723187539));
#216776=CARTESIAN_POINT('Ctrl Pts',(-43.6722143631627,39.7054911294186,
2.76354482595175));
#216777=CARTESIAN_POINT('Ctrl Pts',(-43.6750505546851,39.7197505224127,
2.78225519318207));
#216778=CARTESIAN_POINT('Ctrl Pts',(-43.6794690223308,39.7327754618416,
2.8015122308682));
#216779=CARTESIAN_POINT('Ctrl Pts',(-43.683824428529,39.7456145061593,2.82049442741723));
#216780=CARTESIAN_POINT('Ctrl Pts',(-43.6897180061537,39.7572546408068,
2.84000929090864));
#216781=CARTESIAN_POINT('Ctrl Pts',(-43.697036538801,39.7675538157007,2.85976644343369));
#216782=CARTESIAN_POINT('Ctrl Pts',(-43.7021391499695,39.7747345836734,
2.87354148168132));
#216783=CARTESIAN_POINT('Ctrl Pts',(-43.7079351548543,39.781262797003,2.88743438346094));
#216784=CARTESIAN_POINT('Ctrl Pts',(-43.7143933160625,39.7870778846747,
2.9013417351605));
#216785=CARTESIAN_POINT('',(-43.9791725362585,40.0254908126588,3.471530721391));
#216786=CARTESIAN_POINT('',(-43.7143933160625,39.7870778846747,2.90134173516051));
#216787=CARTESIAN_POINT('',(-40.025490812659,43.9791725362583,3.47153072139102));
#216788=CARTESIAN_POINT('Origin',(5.53234440788222E-15,1.85015204418142E-13,
3.47153072139072));
#216789=CARTESIAN_POINT('',(-39.7870778846749,43.7143933160623,2.90134173516053));
#216790=CARTESIAN_POINT('',(-40.025490812659,43.9791725362582,3.47153072139102));
#216791=CARTESIAN_POINT('',(-39.437049873601,43.7765468711722,2.59908173516053));
#216792=CARTESIAN_POINT('Ctrl Pts',(-39.7870778846749,43.7143933160623,
2.90134173516053));
#216793=CARTESIAN_POINT('Ctrl Pts',(-39.7788943382465,43.7053047809347,
2.8817699891974));
#216794=CARTESIAN_POINT('Ctrl Pts',(-39.769319048819,43.6975432007871,2.86226752356563));
#216795=CARTESIAN_POINT('Ctrl Pts',(-39.7585187839181,43.6911816548805,
2.8431037049977));
#216796=CARTESIAN_POINT('Ctrl Pts',(-39.7475234267921,43.6847051962234,
2.82359371788292));
#216797=CARTESIAN_POINT('Ctrl Pts',(-39.7352578445677,43.6796790973,2.80443322636524));
#216798=CARTESIAN_POINT('Ctrl Pts',(-39.7218536055365,43.6762098455838,
2.78589323877684));
#216799=CARTESIAN_POINT('Ctrl Pts',(-39.7090168672317,43.6728874729903,
2.76813818619297));
#216800=CARTESIAN_POINT('Ctrl Pts',(-39.6951350414451,43.6709925938754,
2.75095095197898));
#216801=CARTESIAN_POINT('Ctrl Pts',(-39.6802941970433,43.6706524194393,
2.73457771434204));
#216802=CARTESIAN_POINT('Ctrl Pts',(-39.6684902774387,43.6703818558792,
2.72155497955002));
#216803=CARTESIAN_POINT('Ctrl Pts',(-39.6560790233689,43.6710953426077,
2.70904711159703));
#216804=CARTESIAN_POINT('Ctrl Pts',(-39.643094175457,43.6728752976394,2.69718956158366));
#216805=CARTESIAN_POINT('Ctrl Pts',(-39.6430587310401,43.6728801563384,
2.69715719432384));
#216806=CARTESIAN_POINT('Ctrl Pts',(-39.6430232824884,43.6728850230946,
2.6971248321905));
#216807=CARTESIAN_POINT('Ctrl Pts',(-39.6429878298037,43.6728898979089,
2.69709247518678));
#216808=CARTESIAN_POINT('Ctrl Pts',(-39.6359303251673,43.6738603187596,
2.69065122242303));
#216809=CARTESIAN_POINT('Ctrl Pts',(-39.6286869425433,43.6751791606255,
2.68442464469454));
#216810=CARTESIAN_POINT('Ctrl Pts',(-39.6212972007503,43.6768375203045,
2.67844505923606));
#216811=CARTESIAN_POINT('Ctrl Pts',(-39.6066317464083,43.680128649932,2.66657815779595));
#216812=CARTESIAN_POINT('Ctrl Pts',(-39.5913890092851,43.6847580950894,
2.65568445664202));
#216813=CARTESIAN_POINT('Ctrl Pts',(-39.5758728438538,43.6906629735752,
2.64601906229543));
#216814=CARTESIAN_POINT('Ctrl Pts',(-39.5642357197804,43.6950916324396,
2.63877001653549));
#216815=CARTESIAN_POINT('Ctrl Pts',(-39.5524447917348,43.7002377219528,
2.63221189387629));
#216816=CARTESIAN_POINT('Ctrl Pts',(-39.540628255996,43.7060747220671,2.62645231033261));
#216817=CARTESIAN_POINT('Ctrl Pts',(-39.5361970550939,43.70826359711,2.62429246650373));
#216818=CARTESIAN_POINT('Ctrl Pts',(-39.5317622532395,43.7105496315976,
2.62224491711774));
#216819=CARTESIAN_POINT('Ctrl Pts',(-39.5273306113316,43.712931427613,2.62031533672625));
#216820=CARTESIAN_POINT('Ctrl Pts',(-39.5118198646542,43.7212677136667,
2.61356180535607));
#216821=CARTESIAN_POINT('Ctrl Pts',(-39.4963478239301,43.7307770746562,
2.60825339735376));
#216822=CARTESIAN_POINT('Ctrl Pts',(-39.4812043938728,43.7413996094243,
2.60463337987639));
#216823=CARTESIAN_POINT('Ctrl Pts',(-39.4736326788442,43.7467108768083,
2.60282337113771));
#216824=CARTESIAN_POINT('Ctrl Pts',(-39.4661431171622,43.7523004383957,
2.60143545939144));
#216825=CARTESIAN_POINT('Ctrl Pts',(-39.4587719497939,43.7581608097797,
2.60050005034626));
#216826=CARTESIAN_POINT('Ctrl Pts',(-39.4550863661098,43.7610909954717,
2.60003234582367));
#216827=CARTESIAN_POINT('Ctrl Pts',(-39.4514303810208,43.764088883632,2.59967776696095));
#216828=CARTESIAN_POINT('Ctrl Pts',(-39.4478085248414,43.7671535389277,
2.59944011429189));
#216829=CARTESIAN_POINT('Ctrl Pts',(-39.444186668662,43.7702181942233,2.59920246162283));
#216830=CARTESIAN_POINT('Ctrl Pts',(-39.4405989425298,43.7733496179168,
2.59908173791343));
#216831=CARTESIAN_POINT('Ctrl Pts',(-39.437049873601,43.7765468711722,2.59908173516054));
#216832=CARTESIAN_POINT('',(-39.4144401478992,43.7969047596346,2.59908173516053));
#216833=CARTESIAN_POINT('Origin',(3.56901409908097E-16,1.91158116697184E-13,
2.59908173516024));
#216834=CARTESIAN_POINT('',(-39.3160391863692,44.1385184650376,2.90134173516053));
#216835=CARTESIAN_POINT('Ctrl Pts',(-39.4144401478992,43.7969047596346,
2.59908173516053));
#216836=CARTESIAN_POINT('Ctrl Pts',(-39.4116082546731,43.799453291355,2.59908174371542));
#216837=CARTESIAN_POINT('Ctrl Pts',(-39.4088155471153,43.8020298032738,
2.5991576435592));
#216838=CARTESIAN_POINT('Ctrl Pts',(-39.4060627300845,43.8046321918102,
2.59930765775307));
#216839=CARTESIAN_POINT('Ctrl Pts',(-39.3898103065118,43.8199964969273,
2.60019333020906));
#216840=CARTESIAN_POINT('Ctrl Pts',(-39.374945232043,43.8362633193841,2.60365973324077));
#216841=CARTESIAN_POINT('Ctrl Pts',(-39.3616178931518,43.8529956277683,
2.60934177082315));
#216842=CARTESIAN_POINT('Ctrl Pts',(-39.3566392429883,43.8592462611882,
2.61146439091779));
#216843=CARTESIAN_POINT('Ctrl Pts',(-39.3518747760143,43.8655619201089,
2.61389584429293));
#216844=CARTESIAN_POINT('Ctrl Pts',(-39.3473309185526,43.8719202087612,
2.61661604385284));
#216845=CARTESIAN_POINT('Ctrl Pts',(-39.3437855730188,43.8768812645309,
2.61873848000807));
#216846=CARTESIAN_POINT('Ctrl Pts',(-39.3403750229161,43.8818681433213,
2.62103707099818));
#216847=CARTESIAN_POINT('Ctrl Pts',(-39.3371028088665,43.8868700682407,
2.62350262767683));
#216848=CARTESIAN_POINT('Ctrl Pts',(-39.3256500596931,43.9043768054586,
2.6321320760521));
#216849=CARTESIAN_POINT('Ctrl Pts',(-39.3158919212385,43.9220678510596,
2.64280685971945));
#216850=CARTESIAN_POINT('Ctrl Pts',(-39.3079802585391,43.9394812142302,
2.65513293646114));
#216851=CARTESIAN_POINT('Ctrl Pts',(-39.3040244271894,43.9481878958155,
2.66129597483199));
#216852=CARTESIAN_POINT('Ctrl Pts',(-39.3005302159781,43.9568251581489,
2.66787183533882));
#216853=CARTESIAN_POINT('Ctrl Pts',(-39.2975166114287,43.9653352562099,
2.67481125953891));
#216854=CARTESIAN_POINT('Ctrl Pts',(-39.2945158824213,43.9738089951123,
2.6817210352411));
#216855=CARTESIAN_POINT('Ctrl Pts',(-39.291991410433,43.982156659355,2.68899101329819));
#216856=CARTESIAN_POINT('Ctrl Pts',(-39.2899626959158,43.9903212250463,
2.69657334701305));
#216857=CARTESIAN_POINT('Ctrl Pts',(-39.2899539910981,43.9903562576029,
2.69660588132602));
#216858=CARTESIAN_POINT('Ctrl Pts',(-39.2899452948636,43.9903912868066,
2.69663842081411));
#216859=CARTESIAN_POINT('Ctrl Pts',(-39.2899366072115,43.9904263126555,
2.69667096547411));
#216860=CARTESIAN_POINT('Ctrl Pts',(-39.2858396774342,44.0069438297351,
2.71201840157854));
#216861=CARTESIAN_POINT('Ctrl Pts',(-39.2836282192305,44.0226860610995,
2.72845645939131));
#216862=CARTESIAN_POINT('Ctrl Pts',(-39.2831328363115,44.0375574100545,
2.74568723186538));
#216863=CARTESIAN_POINT('Ctrl Pts',(-39.2826194323367,44.0529697494231,
2.76354482593832));
#216864=CARTESIAN_POINT('Ctrl Pts',(-39.2839495744673,44.0674474907097,
2.78225519316498));
#216865=CARTESIAN_POINT('Ctrl Pts',(-39.2869823603806,44.0808629337889,
2.80151223084737));
#216866=CARTESIAN_POINT('Ctrl Pts',(-39.289971861634,44.0940869083944,2.82049442739379));
#216867=CARTESIAN_POINT('Ctrl Pts',(-39.2946164282351,44.1062793237782,
2.84000929088258));
#216868=CARTESIAN_POINT('Ctrl Pts',(-39.3008183122678,44.1172870736854,
2.85976644340509));
#216869=CARTESIAN_POINT('Ctrl Pts',(-39.305142376159,44.1249618727701,2.8735414816621));
#216870=CARTESIAN_POINT('Ctrl Pts',(-39.3102242458182,44.1320601713533,
2.88743438345134));
#216871=CARTESIAN_POINT('Ctrl Pts',(-39.3160391863692,44.1385184650376,
2.90134173516053));
#216872=CARTESIAN_POINT('',(-39.5544469813073,44.4033023070489,3.47153072139102));
#216873=CARTESIAN_POINT('',(-39.3160391863692,44.1385184650376,2.90134173516054));
#216874=CARTESIAN_POINT('',(-35.209151665053,47.9220530736687,3.47153072139105));
#216875=CARTESIAN_POINT('Origin',(5.53234440788222E-15,1.85015204418142E-13,
3.47153072139072));
#216876=CARTESIAN_POINT('',(-34.9997217530263,47.63380340476,2.90134173516056));
#216877=CARTESIAN_POINT('',(-35.209151665053,47.9220530736687,3.47153072139105));
#216878=CARTESIAN_POINT('',(-34.6451144164188,47.6590285860936,2.59908173516056));
#216879=CARTESIAN_POINT('Ctrl Pts',(-34.9997217530262,47.63380340476,2.90134173516056));
#216880=CARTESIAN_POINT('Ctrl Pts',(-34.9925330475312,47.6239092440466,
2.88176998919708));
#216881=CARTESIAN_POINT('Ctrl Pts',(-34.983821518586,47.6151892923579,2.86226752356497));
#216882=CARTESIAN_POINT('Ctrl Pts',(-34.9737453812837,47.6077336605724,
2.8431037049967));
#216883=CARTESIAN_POINT('Ctrl Pts',(-34.9634872321452,47.6001433528501,
2.82359371788197));
#216884=CARTESIAN_POINT('Ctrl Pts',(-34.9518142124603,47.5938626849615,
2.80443322636432));
#216885=CARTESIAN_POINT('Ctrl Pts',(-34.9388460388037,47.589011313662,2.78589323877598));
#216886=CARTESIAN_POINT('Ctrl Pts',(-34.9264269039965,47.584365336845,2.76813818619268));
#216887=CARTESIAN_POINT('Ctrl Pts',(-34.9128191931065,47.5810297921593,
2.75095095197925));
#216888=CARTESIAN_POINT('Ctrl Pts',(-34.8980952063149,47.5791401905754,
2.73457771434281));
#216889=CARTESIAN_POINT('Ctrl Pts',(-34.88638423141,47.5776372636139,2.72155497955052));
#216890=CARTESIAN_POINT('Ctrl Pts',(-34.8739663878171,47.5770495124722,
2.7090471115973));
#216891=CARTESIAN_POINT('Ctrl Pts',(-34.8608666162964,47.577462430526,2.69718956158371));
#216892=CARTESIAN_POINT('Ctrl Pts',(-34.8608308581753,47.5774635576581,
2.69715719432388));
#216893=CARTESIAN_POINT('Ctrl Pts',(-34.8607950951,47.5774646923711,2.69712483219054));
#216894=CARTESIAN_POINT('Ctrl Pts',(-34.8607593270719,47.577465834666,2.69709247518681));
#216895=CARTESIAN_POINT('Ctrl Pts',(-34.8536390475841,47.5776932293355,
2.69065122242307));
#216896=CARTESIAN_POINT('Ctrl Pts',(-34.8462974884545,47.5782477067932,
2.68442464469458));
#216897=CARTESIAN_POINT('Ctrl Pts',(-34.8387748826515,47.5791245434507,
2.67844505923611));
#216898=CARTESIAN_POINT('Ctrl Pts',(-34.8238457504804,47.5808646865203,
2.66657815779599));
#216899=CARTESIAN_POINT('Ctrl Pts',(-34.8082026058779,47.5838754712052,
2.65568445664205));
#216900=CARTESIAN_POINT('Ctrl Pts',(-34.7921542117505,47.5881261212206,
2.64601906229547));
#216901=CARTESIAN_POINT('Ctrl Pts',(-34.780117916155,47.5913141087321,2.63877001653553));
#216902=CARTESIAN_POINT('Ctrl Pts',(-34.7678536672182,47.5951995198394,
2.63221189387632));
#216903=CARTESIAN_POINT('Ctrl Pts',(-34.7554917310465,47.5997693799344,
2.62645231033264));
#216904=CARTESIAN_POINT('Ctrl Pts',(-34.7508560049822,47.60148307747,2.62429246650376));
#216905=CARTESIAN_POINT('Ctrl Pts',(-34.7462065417643,47.6032930257988,
2.62224491711777));
#216906=CARTESIAN_POINT('Ctrl Pts',(-34.7415502113773,47.605198541368,2.62031533672629));
#216907=CARTESIAN_POINT('Ctrl Pts',(-34.7252530550225,47.6118678458601,
2.6135618053561));
#216908=CARTESIAN_POINT('Ctrl Pts',(-34.7088717728655,47.6197078449347,
2.6082533973538));
#216909=CARTESIAN_POINT('Ctrl Pts',(-34.6927009428672,47.6286892688734,
2.60463337987643));
#216910=CARTESIAN_POINT('Ctrl Pts',(-34.684615527868,47.6331799808427,2.60282337113774));
#216911=CARTESIAN_POINT('Ctrl Pts',(-34.6765827265055,47.6379560498536,
2.60143545939147));
#216912=CARTESIAN_POINT('Ctrl Pts',(-34.6686393635484,47.6430138207125,
2.60050005034628));
#216913=CARTESIAN_POINT('Ctrl Pts',(-34.6646676820698,47.645542706142,2.60003234582369));
#216914=CARTESIAN_POINT('Ctrl Pts',(-34.6607183602073,47.6481420170542,
2.59967776696097));
#216915=CARTESIAN_POINT('Ctrl Pts',(-34.6567960012265,47.6508112967869,
2.59944011429191));
#216916=CARTESIAN_POINT('Ctrl Pts',(-34.6528736422457,47.6534805765195,
2.59920246162285));
#216917=CARTESIAN_POINT('Ctrl Pts',(-34.6489782471461,47.6562198264472,
2.59908173791348));
#216918=CARTESIAN_POINT('Ctrl Pts',(-34.6451144164188,47.6590285860936,
2.59908173516056));
#216919=CARTESIAN_POINT('',(-34.6205005703637,47.6769115920304,2.59908173516056));
#216920=CARTESIAN_POINT('Origin',(3.62443809638014E-16,1.9116260484399E-13,
2.59908173516024));
#216921=CARTESIAN_POINT('',(-34.4869303039399,48.0063682005187,2.90134173516056));
#216922=CARTESIAN_POINT('Ctrl Pts',(-34.6205005703637,47.6769115920304,
2.59908173516056));
#216923=CARTESIAN_POINT('Ctrl Pts',(-34.6174177964407,47.6791501491803,
2.59908174371546));
#216924=CARTESIAN_POINT('Ctrl Pts',(-34.6143710687957,47.6814206292679,
2.59915764355922));
#216925=CARTESIAN_POINT('Ctrl Pts',(-34.61136130831,47.6837210139136,2.59930765775308));
#216926=CARTESIAN_POINT('Ctrl Pts',(-34.5935919100066,47.6973023109027,
2.6001933302093));
#216927=CARTESIAN_POINT('Ctrl Pts',(-34.5771079220135,47.7119261986175,
2.60365973324256));
#216928=CARTESIAN_POINT('Ctrl Pts',(-34.5621045891938,47.7271737594161,
2.60934177082752));
#216929=CARTESIAN_POINT('Ctrl Pts',(-34.5564998434951,47.7328697405577,
2.61146439092112));
#216930=CARTESIAN_POINT('Ctrl Pts',(-34.5511013106521,47.7386527792229,
2.61389584429479));
#216931=CARTESIAN_POINT('Ctrl Pts',(-34.5459177227788,47.744501274063,2.61661604385282));
#216932=CARTESIAN_POINT('Ctrl Pts',(-34.5418732274829,47.7490645631296,
2.61873848000805));
#216933=CARTESIAN_POINT('Ctrl Pts',(-34.537960089954,47.7536676237151,2.62103707099818));
#216934=CARTESIAN_POINT('Ctrl Pts',(-34.5341829579102,47.7583001080604,
2.62350262767682));
#216935=CARTESIAN_POINT('Ctrl Pts',(-34.5209629957568,47.7745138032688,
2.63213207605209));
#216936=CARTESIAN_POINT('Ctrl Pts',(-34.5094090955955,47.7910879322539,
2.64280685971945));
#216937=CARTESIAN_POINT('Ctrl Pts',(-34.4997205817196,47.8075789092552,
2.65513293646115));
#216938=CARTESIAN_POINT('Ctrl Pts',(-34.4948763247817,47.8158243977558,
2.661295974832));
#216939=CARTESIAN_POINT('Ctrl Pts',(-34.4904984154664,47.8240490997342,
2.66787183533883));
#216940=CARTESIAN_POINT('Ctrl Pts',(-34.4866117722854,47.8321975711351,
2.67481125953893));
#216941=CARTESIAN_POINT('Ctrl Pts',(-34.4827417346799,47.8403112284174,
2.68172103524111));
#216942=CARTESIAN_POINT('Ctrl Pts',(-34.4793585234982,47.8483492841045,
2.68899101329819));
#216943=CARTESIAN_POINT('Ctrl Pts',(-34.4764874929864,47.8562570650397,
2.69657334701305));
#216944=CARTESIAN_POINT('Ctrl Pts',(-34.4764751739553,47.8562909957832,
2.69660588132602));
#216945=CARTESIAN_POINT('Ctrl Pts',(-34.4764628638109,47.8563249240892,
2.69663842081411));
#216946=CARTESIAN_POINT('Ctrl Pts',(-34.4764505625524,47.8563588499558,
2.69667096547411));
#216947=CARTESIAN_POINT('Ctrl Pts',(-34.4706495255077,47.8723576365753,
2.71201840157889));
#216948=CARTESIAN_POINT('Ctrl Pts',(-34.4668046706504,47.8877824700219,
2.72845645939207));
#216949=CARTESIAN_POINT('Ctrl Pts',(-34.4647575222379,47.9025205705564,
2.74568723186657));
#216950=CARTESIAN_POINT('Ctrl Pts',(-34.4626359025942,47.9177948141892,
2.76354482593998));
#216951=CARTESIAN_POINT('Ctrl Pts',(-34.4624454220188,47.9323322826072,
2.78225519316713));
#216952=CARTESIAN_POINT('Ctrl Pts',(-34.4640592983646,47.9459912469369,
2.80151223085002));
#216953=CARTESIAN_POINT('Ctrl Pts',(-34.4656501410737,47.9594552671979,
2.82049442739673));
#216954=CARTESIAN_POINT('Ctrl Pts',(-34.4689948098096,47.9720663806638,
2.8400092908858));
#216955=CARTESIAN_POINT('Ctrl Pts',(-34.4740120960911,47.9836621023726,
2.85976644340858));
#216956=CARTESIAN_POINT('Ctrl Pts',(-34.4775102373536,47.9917468458577,
2.87354148166445));
#216957=CARTESIAN_POINT('Ctrl Pts',(-34.4818222937561,47.9993374592438,
2.88743438345252));
#216958=CARTESIAN_POINT('Ctrl Pts',(-34.4869303039399,48.0063682005187,
2.90134173516055));
#216959=CARTESIAN_POINT('',(-34.6963546279287,48.2946219293746,3.47153072139105));
#216960=CARTESIAN_POINT('',(-34.4869303039399,48.0063682005187,2.90134173516056));
#216961=CARTESIAN_POINT('',(-30.007053683816,51.3398895692697,3.47153072139107));
#216962=CARTESIAN_POINT('Origin',(5.53234440788222E-15,1.85015204418142E-13,
3.47153072139072));
#216963=CARTESIAN_POINT('',(-29.8289013456888,51.0313275753409,2.90134173516058));
#216964=CARTESIAN_POINT('',(-30.007053683816,51.3398895692697,3.47153072139107));
#216965=CARTESIAN_POINT('',(-29.473599835734,51.0193480105328,2.59908173516058));
#216966=CARTESIAN_POINT('Ctrl Pts',(-29.8289013456888,51.0313275753409,
2.90134173516058));
#216967=CARTESIAN_POINT('Ctrl Pts',(-29.8227862420895,51.0207361915371,
2.88176998919749));
#216968=CARTESIAN_POINT('Ctrl Pts',(-29.8150339189614,51.0111534059229,
2.86226752356577));
#216969=CARTESIAN_POINT('Ctrl Pts',(-29.8057923055269,51.0026853737207,
2.84310370499788));
#216970=CARTESIAN_POINT('Ctrl Pts',(-29.7963837548049,50.994064377933,2.82359371788349));
#216971=CARTESIAN_POINT('Ctrl Pts',(-29.7854311897062,50.9865979533909,
2.80443322636617));
#216972=CARTESIAN_POINT('Ctrl Pts',(-29.7730411634487,50.9804176151473,
2.78589323877811));
#216973=CARTESIAN_POINT('Ctrl Pts',(-29.7611756987788,50.9744989364009,
2.7681381861951));
#216974=CARTESIAN_POINT('Ctrl Pts',(-29.7479911917134,50.9697592710701,
2.7509509519819));
#216975=CARTESIAN_POINT('Ctrl Pts',(-29.7335453816122,50.9663409452088,
2.73457771434565));
#216976=CARTESIAN_POINT('Ctrl Pts',(-29.7220556592981,50.9636221212279,
2.72155497955235));
#216977=CARTESIAN_POINT('Ctrl Pts',(-29.7097672786746,50.9617395717404,
2.70904711159817));
#216978=CARTESIAN_POINT('Ctrl Pts',(-29.6966961073823,50.9607809287996,
2.69718956158373));
#216979=CARTESIAN_POINT('Ctrl Pts',(-29.6966604273306,50.9607783120158,
2.6971571943239));
#216980=CARTESIAN_POINT('Ctrl Pts',(-29.6966247415593,50.9607757022533,
2.69712483219056));
#216981=CARTESIAN_POINT('Ctrl Pts',(-29.6965890500698,50.9607730995136,
2.69709247518683));
#216982=CARTESIAN_POINT('Ctrl Pts',(-29.6894840070028,50.9602549766185,
2.6906512224231));
#216983=CARTESIAN_POINT('Ctrl Pts',(-29.6821247070256,50.9600390146968,
2.6844246446946));
#216984=CARTESIAN_POINT('Ctrl Pts',(-29.6745516564559,50.9601247215271,
2.67844505923613));
#216985=CARTESIAN_POINT('Ctrl Pts',(-29.6595224131521,50.9602948126671,
2.66657815779601));
#216986=CARTESIAN_POINT('Ctrl Pts',(-29.6436502506361,50.9616539500925,
2.65568445664207));
#216987=CARTESIAN_POINT('Ctrl Pts',(-29.6272454573769,50.9642038006262,
2.64601906229549));
#216988=CARTESIAN_POINT('Ctrl Pts',(-29.6149418624325,50.9661161885266,
2.63877001653555));
#216989=CARTESIAN_POINT('Ctrl Pts',(-29.6023386622825,50.9686983518508,
2.63221189387636));
#216990=CARTESIAN_POINT('Ctrl Pts',(-29.5895667656375,50.971951003583,2.62645231033268));
#216991=CARTESIAN_POINT('Ctrl Pts',(-29.5847773043957,50.9731707479826,
2.6242924665038));
#216992=CARTESIAN_POINT('Ctrl Pts',(-29.5799641203064,50.9744847799798,
2.6222449171178));
#216993=CARTESIAN_POINT('Ctrl Pts',(-29.5751341171702,50.9758931378755,
2.62031533672632));
#216994=CARTESIAN_POINT('Ctrl Pts',(-29.5582291061936,50.9808223905105,
2.61356180535613));
#216995=CARTESIAN_POINT('Ctrl Pts',(-29.5411180593589,50.9869071309996,
2.60825339735382));
#216996=CARTESIAN_POINT('Ctrl Pts',(-29.524097000417,50.9941490417487,2.60463337987645));
#216997=CARTESIAN_POINT('Ctrl Pts',(-29.5155864709461,50.9977699971232,
2.60282337113777));
#216998=CARTESIAN_POINT('Ctrl Pts',(-29.5070984389558,51.0016802459462,
2.6014354593915));
#216999=CARTESIAN_POINT('Ctrl Pts',(-29.4986699095566,51.0058800022841,
2.60050005034631));
#217000=CARTESIAN_POINT('Ctrl Pts',(-29.494455644857,51.007979880453,2.60003234582372));
#217001=CARTESIAN_POINT('Ctrl Pts',(-29.4902562558177,51.0101521355229,
2.59967776696102));
#217002=CARTESIAN_POINT('Ctrl Pts',(-29.4860763682213,51.0123967945052,
2.59944011429196));
#217003=CARTESIAN_POINT('Ctrl Pts',(-29.481896480625,51.0146414534876,2.5992024616229));
#217004=CARTESIAN_POINT('Ctrl Pts',(-29.4777360953218,51.0169585178539,
2.59908173791349));
#217005=CARTESIAN_POINT('Ctrl Pts',(-29.473599835734,51.0193480105328,2.59908173516058));
#217006=CARTESIAN_POINT('',(-29.4472515437738,51.0345602039887,2.59908173516058));
#217007=CARTESIAN_POINT('Origin',(3.68424986610942E-16,1.91166489065733E-13,
2.59908173516024));
#217008=CARTESIAN_POINT('',(-29.2799753962465,51.3482501200166,2.90134173516058));
#217009=CARTESIAN_POINT('Ctrl Pts',(-29.4472515437738,51.0345602039887,
2.59908173516058));
#217010=CARTESIAN_POINT('Ctrl Pts',(-29.4439516646701,51.0364642604676,
2.5990817437155));
#217011=CARTESIAN_POINT('Ctrl Pts',(-29.4406842975234,51.0384038328689,
2.59915764355925));
#217012=CARTESIAN_POINT('Ctrl Pts',(-29.4374505691487,51.0403770101285,
2.59930765775312));
#217013=CARTESIAN_POINT('Ctrl Pts',(-29.4183588813685,51.0520264994517,
2.60019333020917));
#217014=CARTESIAN_POINT('Ctrl Pts',(-29.4004365818796,51.0648472300434,
2.60365973324133));
#217015=CARTESIAN_POINT('Ctrl Pts',(-29.3839216347905,51.0784429877824,
2.60934177082445));
#217016=CARTESIAN_POINT('Ctrl Pts',(-29.3777522003165,51.0835219102907,
2.61146439091879));
#217017=CARTESIAN_POINT('Ctrl Pts',(-29.3717787490535,51.0887089685256,
2.6138958442935));
#217018=CARTESIAN_POINT('Ctrl Pts',(-29.3660122232361,51.0939835922269,
2.61661604385286));
#217019=CARTESIAN_POINT('Ctrl Pts',(-29.3615128905151,51.0980991182406,
2.61873848000809));
#217020=CARTESIAN_POINT('Ctrl Pts',(-29.3571400387136,51.1022679285262,
2.62103707099819));
#217021=CARTESIAN_POINT('Ctrl Pts',(-29.3528993717246,51.1064802178294,
2.62350262767684));
#217022=CARTESIAN_POINT('Ctrl Pts',(-29.3380570372632,51.1212232303906,
2.6321320760521));
#217023=CARTESIAN_POINT('Ctrl Pts',(-29.324833962343,51.1364988531344,2.64280685971946));
#217024=CARTESIAN_POINT('Ctrl Pts',(-29.3134747466761,51.1518867653714,
2.65513293646116));
#217025=CARTESIAN_POINT('Ctrl Pts',(-29.3077951388427,51.1595807214899,
2.66129597483201));
#217026=CARTESIAN_POINT('Ctrl Pts',(-29.3025814967141,51.1673027515572,
2.66787183533885));
#217027=CARTESIAN_POINT('Ctrl Pts',(-29.2978643977776,51.1750003199402,
2.67481125953895));
#217028=CARTESIAN_POINT('Ctrl Pts',(-29.2931674525158,51.1826650006753,
2.68172103524113));
#217029=CARTESIAN_POINT('Ctrl Pts',(-29.2889625693103,51.1903053811865,
2.68899101329822));
#217030=CARTESIAN_POINT('Ctrl Pts',(-29.2852806784151,51.197869738063,2.69657334701308));
#217031=CARTESIAN_POINT('Ctrl Pts',(-29.2852648801404,51.1979021952409,
2.69660588132605));
#217032=CARTESIAN_POINT('Ctrl Pts',(-29.2852490909586,51.1979346509236,
2.69663842081414));
#217033=CARTESIAN_POINT('Ctrl Pts',(-29.285233310869,51.1979671051091,2.69667096547414));
#217034=CARTESIAN_POINT('Ctrl Pts',(-29.2777917239323,51.2132718752146,
2.71201840157962));
#217035=CARTESIAN_POINT('Ctrl Pts',(-29.2723555974557,51.2282103130406,
2.7284564593936));
#217036=CARTESIAN_POINT('Ctrl Pts',(-29.268779112536,51.2426536914413,2.74568723186895));
#217037=CARTESIAN_POINT('Ctrl Pts',(-29.2650725221322,51.2576224915288,
2.76354482594299));
#217038=CARTESIAN_POINT('Ctrl Pts',(-29.2633635057959,51.2720604115324,
2.78225519317082));
#217039=CARTESIAN_POINT('Ctrl Pts',(-29.2635407906072,51.2858132466409,
2.8015122308544));
#217040=CARTESIAN_POINT('Ctrl Pts',(-29.2637155451665,51.2993697979339,
2.82049442740137));
#217041=CARTESIAN_POINT('Ctrl Pts',(-29.2657236711467,51.3122614394839,
2.8400092908907));
#217042=CARTESIAN_POINT('Ctrl Pts',(-29.2695013892387,51.3243180878406,
2.85976644341372));
#217043=CARTESIAN_POINT('Ctrl Pts',(-29.2721352815049,51.3327241975842,
2.87354148166792));
#217044=CARTESIAN_POINT('Ctrl Pts',(-29.2756302808585,51.3407239614242,
2.88743438345427));
#217045=CARTESIAN_POINT('Ctrl Pts',(-29.2799753962465,51.3482501200166,
2.90134173516058));
#217046=CARTESIAN_POINT('',(-29.4581217525676,51.6568155675428,3.47153072139108));
#217047=CARTESIAN_POINT('',(-29.2799753962465,51.3482501200166,2.90134173516058));
#217048=CARTESIAN_POINT('',(-24.4761921430394,54.1952354911873,3.4715307213911));
#217049=CARTESIAN_POINT('Origin',(5.53234440788222E-15,1.85015204418142E-13,
3.47153072139072));
#217050=CARTESIAN_POINT('',(-24.331269253109,53.8697418420146,2.9013417351606));
#217051=CARTESIAN_POINT('',(-24.4761921430394,54.1952354911873,3.4715307213911));
#217052=CARTESIAN_POINT('',(-23.9791663275016,53.8206887816837,2.59908173516061));
#217053=CARTESIAN_POINT('Ctrl Pts',(-24.331269253109,53.8697418420146,2.9013417351606));
#217054=CARTESIAN_POINT('Ctrl Pts',(-24.32629474976,53.8585692765371,2.881769989197));
#217055=CARTESIAN_POINT('Ctrl Pts',(-24.319586568523,53.8482286480016,2.86226752356478));
#217056=CARTESIAN_POINT('Ctrl Pts',(-24.3112807320066,53.8388409929152,
2.8431037049964));
#217057=CARTESIAN_POINT('Ctrl Pts',(-24.3028248617511,53.8292837624956,
2.8235937178814));
#217058=CARTESIAN_POINT('Ctrl Pts',(-24.292712749833,53.8207133850096,2.80443322636351));
#217059=CARTESIAN_POINT('Ctrl Pts',(-24.2810366186942,53.8132717929009,
2.78589323877493));
#217060=CARTESIAN_POINT('Ctrl Pts',(-24.2698548246746,53.8061452585079,
2.76813818619129));
#217061=CARTESIAN_POINT('Ctrl Pts',(-24.2572379736511,53.8000534012972,
2.75095095197752));
#217062=CARTESIAN_POINT('Ctrl Pts',(-24.2432286115574,53.7951438030521,
2.7345777143408));
#217063=CARTESIAN_POINT('Ctrl Pts',(-24.2320860256382,53.7912388700573,
2.72155497954925));
#217064=CARTESIAN_POINT('Ctrl Pts',(-24.2200617420557,53.7880821478308,
2.7090471115967));
#217065=CARTESIAN_POINT('Ctrl Pts',(-24.2071623814825,53.7857624469883,
2.69718956158374));
#217066=CARTESIAN_POINT('Ctrl Pts',(-24.2071271704182,53.7857561149585,
2.69715719432391));
#217067=CARTESIAN_POINT('Ctrl Pts',(-24.2070919529318,53.7857497893138,
2.69712483219057));
#217068=CARTESIAN_POINT('Ctrl Pts',(-24.2070567290244,53.7857434700556,
2.69709247518685));
#217069=CARTESIAN_POINT('Ctrl Pts',(-24.2000447667167,53.7844855062587,
2.69065122242311));
#217070=CARTESIAN_POINT('Ctrl Pts',(-24.1927483559227,53.7835014710817,
2.68442464469462));
#217071=CARTESIAN_POINT('Ctrl Pts',(-24.1852078325131,53.7827951090626,
2.67844505923615));
#217072=CARTESIAN_POINT('Ctrl Pts',(-24.1702431416111,53.7813932847189,
2.66657815779603));
#217073=CARTESIAN_POINT('Ctrl Pts',(-24.1543158599157,53.7810858838908,
2.6556844566421));
#217074=CARTESIAN_POINT('Ctrl Pts',(-24.1377344018726,53.781906998247,2.64601906229551));
#217075=CARTESIAN_POINT('Ctrl Pts',(-24.1252983083403,53.7825228340141,
2.63877001653557));
#217076=CARTESIAN_POINT('Ctrl Pts',(-24.1124942402751,53.7837734588335,
2.63221189387637));
#217077=CARTESIAN_POINT('Ctrl Pts',(-24.0994523147292,53.7856732654699,
2.62645231033269));
#217078=CARTESIAN_POINT('Ctrl Pts',(-24.0945615926495,53.7863856929585,
2.6242924665038));
#217079=CARTESIAN_POINT('Ctrl Pts',(-24.089637421941,53.7871894118147,2.62224491711781));
#217080=CARTESIAN_POINT('Ctrl Pts',(-24.0846866645808,53.7880851817731,
2.62031533672632));
#217081=CARTESIAN_POINT('Ctrl Pts',(-24.06735901382,53.7912203766274,2.61356180535613));
#217082=CARTESIAN_POINT('Ctrl Pts',(-24.0497056745176,53.7954831928409,
2.60825339735384));
#217083=CARTESIAN_POINT('Ctrl Pts',(-24.0320208729158,53.8009062465108,
2.60463337987647));
#217084=CARTESIAN_POINT('Ctrl Pts',(-24.023178472115,53.8036177733458,2.60282337113778));
#217085=CARTESIAN_POINT('Ctrl Pts',(-24.0143282061515,53.8066193604765,
2.6014354593915));
#217086=CARTESIAN_POINT('Ctrl Pts',(-24.0055068550422,53.809915088884,2.60050005034632));
#217087=CARTESIAN_POINT('Ctrl Pts',(-24.0010961794875,53.8115629530877,
2.60003234582373));
#217088=CARTESIAN_POINT('Ctrl Pts',(-23.9966927326565,53.8132843526341,
2.59967776696101));
#217089=CARTESIAN_POINT('Ctrl Pts',(-23.9923011121677,53.8150797979126,
2.59944011429195));
#217090=CARTESIAN_POINT('Ctrl Pts',(-23.987909491679,53.8168752431911,2.59920246162289));
#217091=CARTESIAN_POINT('Ctrl Pts',(-23.9835296982243,53.8187447357541,
2.59908173791349));
#217092=CARTESIAN_POINT('Ctrl Pts',(-23.9791663275016,53.8206887816837,
2.59908173516061));
#217093=CARTESIAN_POINT('',(-23.9513722670367,53.8330634946838,2.5990817351606));
#217094=CARTESIAN_POINT('Origin',(3.74779409800327E-16,1.91169726806065E-13,
2.59908173516024));
#217095=CARTESIAN_POINT('',(-23.752222950883,54.1275498658874,2.9013417351606));
#217096=CARTESIAN_POINT('Ctrl Pts',(-23.9513722670367,53.8330634946838,
2.5990817351606));
#217097=CARTESIAN_POINT('Ctrl Pts',(-23.9478914369184,53.8346121892504,
2.5990817437155));
#217098=CARTESIAN_POINT('Ctrl Pts',(-23.9444392282283,53.8361996036044,
2.59915764355927));
#217099=CARTESIAN_POINT('Ctrl Pts',(-23.9410169613692,53.8378239549349,
2.59930765775313));
#217100=CARTESIAN_POINT('Ctrl Pts',(-23.9208121566366,53.8474140023513,
2.60019333020913));
#217101=CARTESIAN_POINT('Ctrl Pts',(-23.9016479061139,53.8582911092149,
2.60365973324093));
#217102=CARTESIAN_POINT('Ctrl Pts',(-23.8838022859705,53.8700861059294,
2.60934177082346));
#217103=CARTESIAN_POINT('Ctrl Pts',(-23.877135756338,53.8744923240646,2.61146439091803));
#217104=CARTESIAN_POINT('Ctrl Pts',(-23.8706528330389,53.8790265713715,
2.61389584429309));
#217105=CARTESIAN_POINT('Ctrl Pts',(-23.8643665485424,53.883669534051,2.61661604385287));
#217106=CARTESIAN_POINT('Ctrl Pts',(-23.8594616740271,53.8872922064475,
2.6187384800081));
#217107=CARTESIAN_POINT('Ctrl Pts',(-23.8546770178326,53.8909810920752,
2.62103707099821));
#217108=CARTESIAN_POINT('Ctrl Pts',(-23.8500192775333,53.8947270356133,
2.62350262767686));
#217109=CARTESIAN_POINT('Ctrl Pts',(-23.8337171864861,53.9078378379965,
2.63213207605213));
#217110=CARTESIAN_POINT('Ctrl Pts',(-23.818969811583,53.9216475915795,2.64280685971948));
#217111=CARTESIAN_POINT('Ctrl Pts',(-23.806064348069,53.9357638458657,2.65513293646118));
#217112=CARTESIAN_POINT('Ctrl Pts',(-23.7996116163121,53.9428219730087,
2.66129597483203));
#217113=CARTESIAN_POINT('Ctrl Pts',(-23.7936193631243,53.9499567269876,
2.66787183533887));
#217114=CARTESIAN_POINT('Ctrl Pts',(-23.7881234899554,53.9571190561827,
2.67481125953896));
#217115=CARTESIAN_POINT('Ctrl Pts',(-23.7826510977526,53.9642507845245,
2.68172103524115));
#217116=CARTESIAN_POINT('Ctrl Pts',(-23.7776706121036,53.9714097802522,
2.68899101329824));
#217117=CARTESIAN_POINT('Ctrl Pts',(-23.773218200392,53.978547836393,2.6965733470131));
#217118=CARTESIAN_POINT('Ctrl Pts',(-23.773199095963,53.9785784643977,2.69660588132608));
#217119=CARTESIAN_POINT('Ctrl Pts',(-23.7731800007333,53.9786090918658,
2.69663842081416));
#217120=CARTESIAN_POINT('Ctrl Pts',(-23.7731609147026,53.9786397187955,
2.69667096547416));
#217121=CARTESIAN_POINT('Ctrl Pts',(-23.7641603094577,53.9930827901226,
2.71201840158019));
#217122=CARTESIAN_POINT('Ctrl Pts',(-23.757192470701,54.007371163677,2.72845645939479));
#217123=CARTESIAN_POINT('Ctrl Pts',(-23.7521258339913,54.0213615752674,
2.74568723187081));
#217124=CARTESIAN_POINT('Ctrl Pts',(-23.7468748830075,54.0358609305036,
2.76354482594575));
#217125=CARTESIAN_POINT('Ctrl Pts',(-23.7436660552509,54.05004111722,2.78225519317455));
#217126=CARTESIAN_POINT('Ctrl Pts',(-23.7424048061584,54.0637371441683,
2.80151223085914));
#217127=CARTESIAN_POINT('Ctrl Pts',(-23.7411615579203,54.0772376980811,
2.82049442740744));
#217128=CARTESIAN_POINT('Ctrl Pts',(-23.7418111396966,54.0902686241933,
2.84000929089815));
#217129=CARTESIAN_POINT('Ctrl Pts',(-23.7443079001293,54.1026541040363,
2.85976644342254));
#217130=CARTESIAN_POINT('Ctrl Pts',(-23.7460486859244,54.1112894809403,
2.87354148167386));
#217131=CARTESIAN_POINT('Ctrl Pts',(-23.7486883362847,54.1196107481466,
2.88743438345726));
#217132=CARTESIAN_POINT('Ctrl Pts',(-23.7522229508831,54.1275498658874,
2.9013417351606));
#217133=CARTESIAN_POINT('',(-23.8971395307771,54.4530463244693,3.4715307213911));
#217134=CARTESIAN_POINT('',(-23.752222950883,54.1275498658874,2.9013417351606));
#217135=CARTESIAN_POINT('',(-18.6771643191712,56.4568070719812,3.47153072139111));
#217136=CARTESIAN_POINT('Origin',(5.53234440788222E-15,1.85015204418142E-13,
3.47153072139072));
#217137=CARTESIAN_POINT('',(-18.5670586829468,56.1179479440989,2.90134173516062));
#217138=CARTESIAN_POINT('',(-18.6771643191712,56.4568070719812,3.47153072139112));
#217139=CARTESIAN_POINT('',(-18.2220120550219,56.0323588238392,2.59908173516062));
#217140=CARTESIAN_POINT('Ctrl Pts',(-18.5670586829468,56.1179479440989,
2.90134173516062));
#217141=CARTESIAN_POINT('Ctrl Pts',(-18.5632792815475,56.1063166059136,
2.88176998919699));
#217142=CARTESIAN_POINT('Ctrl Pts',(-18.5576887384392,56.0953314285471,
2.86226752356472));
#217143=CARTESIAN_POINT('Ctrl Pts',(-18.5504096793241,56.0851270036903,
2.84310370499631));
#217144=CARTESIAN_POINT('Ctrl Pts',(-18.5429991338194,56.0747382496557,
2.82359371788145));
#217145=CARTESIAN_POINT('Ctrl Pts',(-18.5338382654968,56.0651578180751,
2.80443322636368));
#217146=CARTESIAN_POINT('Ctrl Pts',(-18.5230039556137,56.0565365037418,
2.78589323877522));
#217147=CARTESIAN_POINT('Ctrl Pts',(-18.5126283423204,56.0482801935046,
2.76813818619188));
#217148=CARTESIAN_POINT('Ctrl Pts',(-18.5007173801999,56.0409028880764,
2.7509509519784));
#217149=CARTESIAN_POINT('Ctrl Pts',(-18.4872979556178,56.0345558080332,
2.73457771434192));
#217150=CARTESIAN_POINT('Ctrl Pts',(-18.476624586595,56.0295075492868,2.72155497954998));
#217151=CARTESIAN_POINT('Ctrl Pts',(-18.4649961406192,56.02511124003,2.70904711159707));
#217152=CARTESIAN_POINT('Ctrl Pts',(-18.4524099188568,56.0214558964135,
2.69718956158377));
#217153=CARTESIAN_POINT('Ctrl Pts',(-18.4523755625598,56.0214459185128,
2.69715719432394));
#217154=CARTESIAN_POINT('Ctrl Pts',(-18.4523411992083,56.0214359462908,
2.6971248321906));
#217155=CARTESIAN_POINT('Ctrl Pts',(-18.4523068288036,56.0214259797493,
2.69709247518687));
#217156=CARTESIAN_POINT('Ctrl Pts',(-18.4454647717816,56.0194419575651,
2.69065122242314));
#217157=CARTESIAN_POINT('Ctrl Pts',(-18.4383111911742,56.0177006304281,
2.68442464469464));
#217158=CARTESIAN_POINT('Ctrl Pts',(-18.4308858104772,56.0162099386099,
2.67844505923617));
#217159=CARTESIAN_POINT('Ctrl Pts',(-18.4161496282622,56.0132515574634,
2.66657815779605));
#217160=CARTESIAN_POINT('Ctrl Pts',(-18.4003417300186,56.0112809863295,
2.65568445664211));
#217161=CARTESIAN_POINT('Ctrl Pts',(-18.3837652771157,56.0103643682073,
2.64601906229553));
#217162=CARTESIAN_POINT('Ctrl Pts',(-18.3713329374386,56.0096769046157,
2.63877001653558));
#217163=CARTESIAN_POINT('Ctrl Pts',(-18.3584682855075,56.009582288823,2.63221189387638));
#217164=CARTESIAN_POINT('Ctrl Pts',(-18.3452992211262,56.0101084356845,
2.6264523103327));
#217165=CARTESIAN_POINT('Ctrl Pts',(-18.3403608219832,56.0103057407576,
2.62429246650382));
#217166=CARTESIAN_POINT('Ctrl Pts',(-18.3353796149,56.0105903407607,2.62224491711782));
#217167=CARTESIAN_POINT('Ctrl Pts',(-18.3303623448494,56.0109637085387,
2.62031533672634));
#217168=CARTESIAN_POINT('Ctrl Pts',(-18.3128018996724,56.0122704957615,
2.61356180535615));
#217169=CARTESIAN_POINT('Ctrl Pts',(-18.2947996815818,56.014664683393,2.60825339735385));
#217170=CARTESIAN_POINT('Ctrl Pts',(-18.2766448957073,56.0182094638728,
2.60463337987648));
#217171=CARTESIAN_POINT('Ctrl Pts',(-18.2675675027701,56.0199818541128,
2.6028233711378));
#217172=CARTESIAN_POINT('Ctrl Pts',(-18.2584519681994,56.0220418935344,
2.60143545939152));
#217173=CARTESIAN_POINT('Ctrl Pts',(-18.2493344439487,56.0243974853215,
2.60050005034633));
#217174=CARTESIAN_POINT('Ctrl Pts',(-18.2447756818233,56.025575281215,2.60003234582374));
#217175=CARTESIAN_POINT('Ctrl Pts',(-18.2402164222855,56.0268269652242,
2.59967776696103));
#217176=CARTESIAN_POINT('Ctrl Pts',(-18.2356611844174,56.0281535255247,
2.59944011429197));
#217177=CARTESIAN_POINT('Ctrl Pts',(-18.2311059465494,56.0294800858251,
2.59920246162291));
#217178=CARTESIAN_POINT('Ctrl Pts',(-18.2265547308768,56.030881524033,2.59908173791348));
#217179=CARTESIAN_POINT('Ctrl Pts',(-18.2220120550219,56.0323588238392,
2.59908173516062));
#217180=CARTESIAN_POINT('',(-18.1930767435952,56.0417604764384,2.59908173516062));
#217181=CARTESIAN_POINT('Origin',(3.81437458815951E-16,1.91172282591625E-13,
2.59908173516023));
#217182=CARTESIAN_POINT('',(-17.9642361803975,56.3138168485096,2.90134173516061));
#217183=CARTESIAN_POINT('Ctrl Pts',(-18.1930767435952,56.0417604764384,
2.59908173516062));
#217184=CARTESIAN_POINT('Ctrl Pts',(-18.1894530991653,56.042936841271,2.59908174371553));
#217185=CARTESIAN_POINT('Ctrl Pts',(-18.1858538720526,56.0441547055337,
2.59915764355928));
#217186=CARTESIAN_POINT('Ctrl Pts',(-18.1822805617811,56.045412434202,2.59930765775314));
#217187=CARTESIAN_POINT('Ctrl Pts',(-18.1611840081645,56.0528379691456,
2.60019333020911));
#217188=CARTESIAN_POINT('Ctrl Pts',(-18.1409877741468,56.0616522804226,
2.6036597332407));
#217189=CARTESIAN_POINT('Ctrl Pts',(-18.1220070012975,56.0715172876609,
2.60934177082289));
#217190=CARTESIAN_POINT('Ctrl Pts',(-18.1149164164007,56.0752025259747,
2.6114643909176));
#217191=CARTESIAN_POINT('Ctrl Pts',(-18.10799504933,56.0790342841908,2.61389584429285));
#217192=CARTESIAN_POINT('Ctrl Pts',(-18.1012578800032,56.0829947165772,
2.61661604385289));
#217193=CARTESIAN_POINT('Ctrl Pts',(-18.0960012025252,56.0860848445997,
2.61873848000813));
#217194=CARTESIAN_POINT('Ctrl Pts',(-18.0908571636321,56.0892533893667,
2.62103707099824));
#217195=CARTESIAN_POINT('Ctrl Pts',(-18.0858333812,56.0924919457983,2.62350262767689));
#217196=CARTESIAN_POINT('Ctrl Pts',(-18.0682501426879,56.1038268933091,
2.63213207605216));
#217197=CARTESIAN_POINT('Ctrl Pts',(-18.0521400431274,56.1160194751812,
2.64280685971951));
#217198=CARTESIAN_POINT('Ctrl Pts',(-18.0378297267253,56.1287094108805,
2.65513293646121));
#217199=CARTESIAN_POINT('Ctrl Pts',(-18.0306745685242,56.1350543787301,
2.66129597483206));
#217200=CARTESIAN_POINT('Ctrl Pts',(-18.0239693566573,56.141523686763,2.6678718353389));
#217201=CARTESIAN_POINT('Ctrl Pts',(-18.0177549231924,56.1480723047927,
2.67481125953899));
#217202=CARTESIAN_POINT('Ctrl Pts',(-18.0115670407226,56.154592944033,2.68172103524118));
#217203=CARTESIAN_POINT('Ctrl Pts',(-18.0058655198732,56.1611921195218,
2.68899101329827));
#217204=CARTESIAN_POINT('Ctrl Pts',(-18.0006913688997,56.1678256688902,
2.69657334701313));
#217205=CARTESIAN_POINT('Ctrl Pts',(-18.0006691676285,56.1678541321548,
2.6966058813261));
#217206=CARTESIAN_POINT('Ctrl Pts',(-18.0006469755623,56.1678825958475,
2.69663842081419));
#217207=CARTESIAN_POINT('Ctrl Pts',(-18.000624792701,56.1679110599662,2.69667096547419));
#217208=CARTESIAN_POINT('Ctrl Pts',(-17.9901637816629,56.1813341912024,
2.71201840157986));
#217209=CARTESIAN_POINT('Ctrl Pts',(-17.9817405717259,56.1948159540735,
2.72845645939404));
#217210=CARTESIAN_POINT('Ctrl Pts',(-17.9752392943583,56.2082001169759,
2.74568723186962));
#217211=CARTESIAN_POINT('Ctrl Pts',(-17.9685015133122,56.2220711693896,
2.76354482594404));
#217212=CARTESIAN_POINT('Ctrl Pts',(-17.9638280307234,56.2358382617248,
2.78225519317228));
#217213=CARTESIAN_POINT('Ctrl Pts',(-17.9611420662355,56.2493274239746,
2.80151223085629));
#217214=CARTESIAN_POINT('Ctrl Pts',(-17.9584944364875,56.2626240656124,
2.82049442740399));
#217215=CARTESIAN_POINT('Ctrl Pts',(-17.9577783571051,56.2756515067325,
2.84000929089407));
#217216=CARTESIAN_POINT('Ctrl Pts',(-17.9589668048478,56.2882301201518,
2.85976644341784));
#217217=CARTESIAN_POINT('Ctrl Pts',(-17.9597954117585,56.2970001532227,
2.8735414816707));
#217218=CARTESIAN_POINT('Ctrl Pts',(-17.9615507925646,56.3055517542533,
2.88743438345568));
#217219=CARTESIAN_POINT('Ctrl Pts',(-17.9642361803975,56.3138168485096,
2.9013417351606));
#217220=CARTESIAN_POINT('',(-18.0743352474894,56.6526781108324,3.47153072139111));
#217221=CARTESIAN_POINT('',(-17.9642361803975,56.3138168485096,2.90134173516061));
#217222=CARTESIAN_POINT('',(-12.6735055745743,58.0998260601481,3.47153072139113));
#217223=CARTESIAN_POINT('Origin',(5.53234440788222E-15,1.85015204418142E-13,
3.47153072139072));
#217224=CARTESIAN_POINT('',(-12.5994235324474,57.7513140650721,2.90134173516064));
#217225=CARTESIAN_POINT('',(-12.6735055745743,58.0998260601481,3.47153072139113));
#217226=CARTESIAN_POINT('',(-12.2652136052663,57.6301266171959,2.59908173516063));
#217227=CARTESIAN_POINT('Ctrl Pts',(-12.5994235324474,57.7513140650721,
2.90134173516064));
#217228=CARTESIAN_POINT('Ctrl Pts',(-12.5968806409108,57.7393513895546,
2.88176998919802));
#217229=CARTESIAN_POINT('Ctrl Pts',(-12.5924689870918,57.7278420192598,
2.86226752356677));
#217230=CARTESIAN_POINT('Ctrl Pts',(-12.5862964562735,57.7169326264472,
2.84310370499932));
#217231=CARTESIAN_POINT('Ctrl Pts',(-12.5800124270075,57.7058261701611,
2.82359371788539));
#217232=CARTESIAN_POINT('Ctrl Pts',(-12.5719031706713,57.6953406496997,
2.80443322636852));
#217233=CARTESIAN_POINT('Ctrl Pts',(-12.5620293850107,57.685634070066,2.78589323878086));
#217234=CARTESIAN_POINT('Ctrl Pts',(-12.5525736298349,57.6763384418474,
2.76813818619826));
#217235=CARTESIAN_POINT('Ctrl Pts',(-12.5414990556115,57.667756515504,2.75095095198544));
#217236=CARTESIAN_POINT('Ctrl Pts',(-12.5288165945656,57.6600414936,2.73457771434951));
#217237=CARTESIAN_POINT('Ctrl Pts',(-12.5187293821024,57.65390521888,2.72155497955484));
#217238=CARTESIAN_POINT('Ctrl Pts',(-12.5076241774191,57.648317489476,2.70904711159938));
#217239=CARTESIAN_POINT('Ctrl Pts',(-12.495488991745,57.6433665517942,2.69718956158379));
#217240=CARTESIAN_POINT('Ctrl Pts',(-12.49545586663,57.6433530373425,2.69715719432396));
#217241=CARTESIAN_POINT('Ctrl Pts',(-12.4954227339057,57.6433395278011,
2.69712483219062));
#217242=CARTESIAN_POINT('Ctrl Pts',(-12.4953895935729,57.6433260231718,
2.6970924751869));
#217243=CARTESIAN_POINT('Ctrl Pts',(-12.4887924048451,57.6406376799627,
2.69065122242315));
#217244=CARTESIAN_POINT('Ctrl Pts',(-12.4818600305505,57.6381581392101,
2.68442464469466));
#217245=CARTESIAN_POINT('Ctrl Pts',(-12.4746311465908,57.6358994499242,
2.67844505923618));
#217246=CARTESIAN_POINT('Ctrl Pts',(-12.4602849257588,57.6314169246178,
2.66657815779607));
#217247=CARTESIAN_POINT('Ctrl Pts',(-12.4447696056082,57.6278047731679,
2.65568445664213));
#217248=CARTESIAN_POINT('Ctrl Pts',(-12.4283797729325,57.6251604652273,
2.64601906229555));
#217249=CARTESIAN_POINT('Ctrl Pts',(-12.4160873984258,57.6231772342719,
2.63877001653561));
#217250=CARTESIAN_POINT('Ctrl Pts',(-12.4033031104474,57.6217384144976,
2.63221189387641));
#217251=CARTESIAN_POINT('Ctrl Pts',(-12.3901511902558,57.6208851370091,
2.62645231033273));
#217252=CARTESIAN_POINT('Ctrl Pts',(-12.3852192201839,57.6205651579509,
2.62429246650384));
#217253=CARTESIAN_POINT('Ctrl Pts',(-12.3802355518734,57.6203275209639,
2.62224491711784));
#217254=CARTESIAN_POINT('Ctrl Pts',(-12.3752067393931,57.6201743958659,
2.62031533672636));
#217255=CARTESIAN_POINT('Ctrl Pts',(-12.3576058957119,57.6196384580229,
2.61356180535617));
#217256=CARTESIAN_POINT('Ctrl Pts',(-12.3394520349016,57.6201377858516,
2.60825339735387));
#217257=CARTESIAN_POINT('Ctrl Pts',(-12.3210261723876,57.6217654557846,
2.6046333798765));
#217258=CARTESIAN_POINT('Ctrl Pts',(-12.3118132411305,57.6225792907512,
2.60282337113782));
#217259=CARTESIAN_POINT('Ctrl Pts',(-12.302532309657,57.6236752122408,2.60143545939154));
#217260=CARTESIAN_POINT('Ctrl Pts',(-12.2932185057685,57.6250648590508,
2.60050005034635));
#217261=CARTESIAN_POINT('Ctrl Pts',(-12.2885616038243,57.6257596824558,
2.60003234582376));
#217262=CARTESIAN_POINT('Ctrl Pts',(-12.2838964837812,57.626527937216,2.59967776696105));
#217263=CARTESIAN_POINT('Ctrl Pts',(-12.2792275366732,57.6273710784661,
2.59944011429199));
#217264=CARTESIAN_POINT('Ctrl Pts',(-12.2745585895652,57.6282142197163,
2.59920246162293));
#217265=CARTESIAN_POINT('Ctrl Pts',(-12.2698858157461,57.6291322491188,
2.59908173791354));
#217266=CARTESIAN_POINT('Ctrl Pts',(-12.2652136052663,57.6301266171959,
2.59908173516064));
#217267=CARTESIAN_POINT('',(-12.2354540642047,57.6364522029208,2.59908173516064));
#217268=CARTESIAN_POINT('Origin',(3.88326186679512E-16,1.91174128420693E-13,
2.59908173516024));
#217269=CARTESIAN_POINT('',(-11.9794294790614,57.8830978693157,2.90134173516063));
#217270=CARTESIAN_POINT('Ctrl Pts',(-12.2354540642047,57.6364522029208,
2.59908173516064));
#217271=CARTESIAN_POINT('Ctrl Pts',(-12.2317273068699,57.63724334952,2.59908174371556));
#217272=CARTESIAN_POINT('Ctrl Pts',(-12.2280204952201,57.638078320516,2.59915764355931));
#217273=CARTESIAN_POINT('Ctrl Pts',(-12.2243352914713,57.6389556465835,
2.59930765775318));
#217274=CARTESIAN_POINT('Ctrl Pts',(-12.2025781272232,57.6441353133407,
2.60019333020927));
#217275=CARTESIAN_POINT('Ctrl Pts',(-12.1815711838732,57.6507902575936,
2.60365973324169));
#217276=CARTESIAN_POINT('Ctrl Pts',(-12.1616632156344,57.6586171922739,
2.60934177082526));
#217277=CARTESIAN_POINT('Ctrl Pts',(-12.1542262614087,57.6615410745228,
2.61146439091942));
#217278=CARTESIAN_POINT('Ctrl Pts',(-12.1469422825158,57.6646283621018,
2.61389584429389));
#217279=CARTESIAN_POINT('Ctrl Pts',(-12.1398280421989,57.6678628728675,
2.61661604385293));
#217280=CARTESIAN_POINT('Ctrl Pts',(-12.1342771550166,57.6703866004267,
2.61873848000816));
#217281=CARTESIAN_POINT('Ctrl Pts',(-12.1288300925915,57.6730000890934,
2.62103707099826));
#217282=CARTESIAN_POINT('Ctrl Pts',(-12.1234953096383,57.6756957761166,
2.62350262767691));
#217283=CARTESIAN_POINT('Ctrl Pts',(-12.104823569302,57.685130680698,2.63213207605218));
#217284=CARTESIAN_POINT('Ctrl Pts',(-12.0875272507061,57.6955725063807,
2.64280685971954));
#217285=CARTESIAN_POINT('Ctrl Pts',(-12.071968868237,57.7066970899021,2.65513293646124));
#217286=CARTESIAN_POINT('Ctrl Pts',(-12.0641896770024,57.7122593816628,
2.66129597483209));
#217287=CARTESIAN_POINT('Ctrl Pts',(-12.0568449701605,57.717992364657,2.66787183533892));
#217288=CARTESIAN_POINT('Ctrl Pts',(-12.0499800630333,57.7238555234918,
2.67481125953901));
#217289=CARTESIAN_POINT('Ctrl Pts',(-12.0431444860318,57.7296936321426,
2.68172103524119));
#217290=CARTESIAN_POINT('Ctrl Pts',(-12.0367843970375,57.735660685445,2.68899101329828));
#217291=CARTESIAN_POINT('Ctrl Pts',(-12.0309451958829,57.7417170494859,
2.69657334701314));
#217292=CARTESIAN_POINT('Ctrl Pts',(-12.0309201410113,57.741743036161,2.69660588132611));
#217293=CARTESIAN_POINT('Ctrl Pts',(-12.0308950952495,57.741769024224,2.6966384208142));
#217294=CARTESIAN_POINT('Ctrl Pts',(-12.0308700585976,57.7417950136728,
2.6966709654742));
#217295=CARTESIAN_POINT('Ctrl Pts',(-12.0190632547925,57.7540511381832,
2.71201840157942));
#217296=CARTESIAN_POINT('Ctrl Pts',(-12.009276960126,57.7665785813559,2.72845645939309));
#217297=CARTESIAN_POINT('Ctrl Pts',(-12.0014122714559,57.7792098558806,
2.74568723186812));
#217298=CARTESIAN_POINT('Ctrl Pts',(-11.9932614808867,57.7923006313189,
2.76354482594205));
#217299=CARTESIAN_POINT('Ctrl Pts',(-11.9871745471191,57.8055037941284,
2.78225519316977));
#217300=CARTESIAN_POINT('Ctrl Pts',(-11.9830932952248,57.8186383015954,
2.80151223085323));
#217301=CARTESIAN_POINT('Ctrl Pts',(-11.9790702919525,57.8315853501699,
2.82049442740046));
#217302=CARTESIAN_POINT('Ctrl Pts',(-11.9769963969271,57.8444665749267,
2.84000929089006));
#217303=CARTESIAN_POINT('Ctrl Pts',(-11.9768635110977,57.8571005080016,
2.85976644341336));
#217304=CARTESIAN_POINT('Ctrl Pts',(-11.9767708607331,57.8659091109217,
2.87354148166769));
#217305=CARTESIAN_POINT('Ctrl Pts',(-11.9776227396652,57.8745973526462,
2.88743438345419));
#217306=CARTESIAN_POINT('Ctrl Pts',(-11.9794294790615,57.8830978693157,
2.90134173516063));
#217307=CARTESIAN_POINT('',(-12.0535047649324,58.2316113004782,3.47153072139112));
#217308=CARTESIAN_POINT('',(-11.9794294790614,57.8830978693157,2.90134173516064));
#217309=CARTESIAN_POINT('',(-6.53099325080075,59.1062911958298,3.47153072139113));
#217310=CARTESIAN_POINT('Origin',(5.53234440788222E-15,1.85015204418142E-13,
3.47153072139072));
#217311=CARTESIAN_POINT('',(-6.4937464611276,58.751944703909,2.90134173516065));
#217312=CARTESIAN_POINT('',(-6.53099325080075,59.1062911958298,3.47153072139113));
#217313=CARTESIAN_POINT('',(-6.1740349085904,58.5964866834552,2.59908173516065));
#217314=CARTESIAN_POINT('Ctrl Pts',(-6.4937464611276,58.751944703909,2.90134173516065));
#217315=CARTESIAN_POINT('Ctrl Pts',(-6.49246793990533,58.7397817566342,
2.88176998919662));
#217316=CARTESIAN_POINT('Ctrl Pts',(-6.48928351037726,58.7278742924791,
2.86226752356397));
#217317=CARTESIAN_POINT('Ctrl Pts',(-6.4842851353939,58.7163794573001,2.84310370499519));
#217318=CARTESIAN_POINT('Ctrl Pts',(-6.47919647150507,58.7046769834205,
2.82359371787983));
#217319=CARTESIAN_POINT('Ctrl Pts',(-6.47222767386301,58.6934012556334,
2.8044332263616));
#217320=CARTESIAN_POINT('Ctrl Pts',(-6.46342259168489,58.6827157580163,
2.78589323877272));
#217321=CARTESIAN_POINT('Ctrl Pts',(-6.45499029385684,58.6724826566635,
2.76813818618886));
#217322=CARTESIAN_POINT('Ctrl Pts',(-6.4448734428809,58.662790134785,2.7509509519749));
#217323=CARTESIAN_POINT('Ctrl Pts',(-6.43306689706553,58.6537916984143,
2.73457771433802));
#217324=CARTESIAN_POINT('Ctrl Pts',(-6.42367635877643,58.6466346380341,
2.72155497954749));
#217325=CARTESIAN_POINT('Ctrl Pts',(-6.4132160663368,58.6399167088188,2.70904711159589));
#217326=CARTESIAN_POINT('Ctrl Pts',(-6.40166487239057,58.6337244205834,
2.69718956158378));
#217327=CARTESIAN_POINT('Ctrl Pts',(-6.40163334138329,58.633707517648,2.69715719432396));
#217328=CARTESIAN_POINT('Ctrl Pts',(-6.40160180229505,58.6336906188005,
2.69712483219062));
#217329=CARTESIAN_POINT('Ctrl Pts',(-6.40157025512662,58.6336737240429,
2.6970924751869));
#217330=CARTESIAN_POINT('Ctrl Pts',(-6.39529021487341,58.6303105138596,
2.69065122242315));
#217331=CARTESIAN_POINT('Ctrl Pts',(-6.38865499943491,58.6271199258589,
2.68442464469466));
#217332=CARTESIAN_POINT('Ctrl Pts',(-6.38170181337804,58.6241179857778,
2.67844505923619));
#217333=CARTESIAN_POINT('Ctrl Pts',(-6.36790273412669,58.6181604277967,
2.66657815779607));
#217334=CARTESIAN_POINT('Ctrl Pts',(-6.35284998116341,58.612946271518,2.65568445664214));
#217335=CARTESIAN_POINT('Ctrl Pts',(-6.33682633915145,58.6086032453502,
2.64601906229556));
#217336=CARTESIAN_POINT('Ctrl Pts',(-6.32480860764249,58.6053459757243,
2.63877001653562));
#217337=CARTESIAN_POINT('Ctrl Pts',(-6.31224475095125,58.602578715979,2.63221189387642));
#217338=CARTESIAN_POINT('Ctrl Pts',(-6.2992540701391,58.6003553628272,2.62645231033274));
#217339=CARTESIAN_POINT('Ctrl Pts',(-6.29438256483455,58.5995216053953,
2.62429246650386));
#217340=CARTESIAN_POINT('Ctrl Pts',(-6.28945103740957,58.5987643350185,
2.62224491711786));
#217341=CARTESIAN_POINT('Ctrl Pts',(-6.28446577922136,58.5980863947152,
2.62031533672637));
#217342=CARTESIAN_POINT('Ctrl Pts',(-6.26701737556263,58.5957136036536,
2.61356180535618));
#217343=CARTESIAN_POINT('Ctrl Pts',(-6.24891076953076,58.5943126009393,
2.60825339735388));
#217344=CARTESIAN_POINT('Ctrl Pts',(-6.23041570798265,58.5940053272332,
2.60463337987651));
#217345=CARTESIAN_POINT('Ctrl Pts',(-6.2211681772086,58.5938516903802,2.60282337113783));
#217346=CARTESIAN_POINT('Ctrl Pts',(-6.21182353265963,58.5939714867927,
2.60143545939156));
#217347=CARTESIAN_POINT('Ctrl Pts',(-6.20241549311782,58.5943799633644,
2.60050005034637));
#217348=CARTESIAN_POINT('Ctrl Pts',(-6.19771147334692,58.5945842016503,
2.60003234582378));
#217349=CARTESIAN_POINT('Ctrl Pts',(-6.19299160483011,58.5948606100014,
2.59967776696106));
#217350=CARTESIAN_POINT('Ctrl Pts',(-6.18826010244368,58.5952110945693,
2.599440114292));
#217351=CARTESIAN_POINT('Ctrl Pts',(-6.18352860005725,58.5955615791371,
2.59920246162294));
#217352=CARTESIAN_POINT('Ctrl Pts',(-6.17878546397933,58.5959861416121,
2.59908173791359));
#217353=CARTESIAN_POINT('Ctrl Pts',(-6.1740349085904,58.5964866834552,2.59908173516065));
#217354=CARTESIAN_POINT('',(-6.14377718965342,58.599666897865,2.59908173516065));
#217355=CARTESIAN_POINT('Origin',(3.95370119046986E-16,1.91175244069979E-13,
2.59908173516024));
#217356=CARTESIAN_POINT('',(-5.863373641496,58.8181995570487,2.90134173516065));
#217357=CARTESIAN_POINT('Ctrl Pts',(-6.14377718965342,58.599666897865,2.59908173516065));
#217358=CARTESIAN_POINT('Ctrl Pts',(-6.13998815054705,58.6000641582632,
2.59908174371554));
#217359=CARTESIAN_POINT('Ctrl Pts',(-6.13621436696423,58.6005070878752,
2.59915764355931));
#217360=CARTESIAN_POINT('Ctrl Pts',(-6.13245764560145,58.6009943991741,
2.59930765775317));
#217361=CARTESIAN_POINT('Ctrl Pts',(-6.11027824677063,58.6038714482308,
2.60019333020922));
#217362=CARTESIAN_POINT('Ctrl Pts',(-6.08869075055971,58.6082941124961,
2.60365973324127));
#217363=CARTESIAN_POINT('Ctrl Pts',(-6.06807370280082,58.613997221082,2.60934177082423));
#217364=CARTESIAN_POINT('Ctrl Pts',(-6.06037186006897,58.6161277126016,
2.61146439091863));
#217365=CARTESIAN_POINT('Ctrl Pts',(-6.05280507414697,58.6184367045764,
2.61389584429346));
#217366=CARTESIAN_POINT('Ctrl Pts',(-6.04539170794193,58.6209098557465,
2.61661604385295));
#217367=CARTESIAN_POINT('Ctrl Pts',(-6.03960742773695,58.6228395323551,
2.61873848000818));
#217368=CARTESIAN_POINT('Ctrl Pts',(-6.03391702093564,58.6248693309928,
2.6210370709983));
#217369=CARTESIAN_POINT('Ctrl Pts',(-6.02832968645963,58.6269926140966,
2.62350262767695));
#217370=CARTESIAN_POINT('Ctrl Pts',(-6.00877401579357,58.6344241049596,
2.63213207605221));
#217371=CARTESIAN_POINT('Ctrl Pts',(-5.99048098024846,58.6430007716256,
2.64280685971957));
#217372=CARTESIAN_POINT('Ctrl Pts',(-5.97384499260641,58.652438119704,2.65513293646127));
#217373=CARTESIAN_POINT('Ctrl Pts',(-5.96552699878538,58.6571567937432,
2.66129597483211));
#217374=CARTESIAN_POINT('Ctrl Pts',(-5.95762326711374,58.6620906399374,
2.66787183533894));
#217375=CARTESIAN_POINT('Ctrl Pts',(-5.95018309968312,58.6672041015821,
2.67481125953903));
#217376=CARTESIAN_POINT('Ctrl Pts',(-5.942774720162,58.6722957161035,2.68172103524121));
#217377=CARTESIAN_POINT('Ctrl Pts',(-5.93582574548873,58.6775652709346,
2.6889910132983));
#217378=CARTESIAN_POINT('Ctrl Pts',(-5.92938546966289,58.6829780948562,
2.69657334701315));
#217379=CARTESIAN_POINT('Ctrl Pts',(-5.92935783569725,58.6830013202264,
2.69660588132613));
#217380=CARTESIAN_POINT('Ctrl Pts',(-5.92933021064649,58.6830245479291,
2.69663842081421));
#217381=CARTESIAN_POINT('Ctrl Pts',(-5.92930259451082,58.6830477779622,
2.69667096547422));
#217382=CARTESIAN_POINT('Ctrl Pts',(-5.91627935575166,58.6940026150824,
2.71201840157949));
#217383=CARTESIAN_POINT('Ctrl Pts',(-5.90523719704773,58.7054384852681,
2.72845645939321));
#217384=CARTESIAN_POINT('Ctrl Pts',(-5.89609526424982,58.7171784805286,
2.74568723186831));
#217385=CARTESIAN_POINT('Ctrl Pts',(-5.8866207659247,58.7293455537166,2.7635448259422));
#217386=CARTESIAN_POINT('Ctrl Pts',(-5.87918707069841,58.741840130386,2.78225519316988));
#217387=CARTESIAN_POINT('Ctrl Pts',(-5.87375524644771,58.7544760786581,
2.80151223085331));
#217388=CARTESIAN_POINT('Ctrl Pts',(-5.86840094651688,58.766931683596,2.82049442740043));
#217389=CARTESIAN_POINT('Ctrl Pts',(-5.8649919578766,58.7795255625957,2.84000929088992));
#217390=CARTESIAN_POINT('Ctrl Pts',(-5.86353919440033,58.7920763953117,
2.85976644341311));
#217391=CARTESIAN_POINT('Ctrl Pts',(-5.86252630185741,58.8008270591832,
2.87354148166754));
#217392=CARTESIAN_POINT('Ctrl Pts',(-5.86246534555161,58.8095567514062,
2.88743438345412));
#217393=CARTESIAN_POINT('Ctrl Pts',(-5.863373641496,58.8181995570487,2.90134173516065));
#217394=CARTESIAN_POINT('',(-5.90061356181277,59.1725467709679,3.47153072139113));
#217395=CARTESIAN_POINT('',(-5.863373641496,58.8181995570487,2.90134173516065));
#217396=CARTESIAN_POINT('',(-0.316925998273249,59.4651754363834,3.47153072139114));
#217397=CARTESIAN_POINT('Origin',(5.53234440788222E-15,1.85015204418142E-13,
3.47153072139072));
#217398=CARTESIAN_POINT('',(-0.316922544675889,59.108876741935,2.90134173516065));
#217399=CARTESIAN_POINT('',(-0.316925998273249,59.4651754363834,3.47153072139114));
#217400=CARTESIAN_POINT('',(-0.0152121934561199,58.9208513795075,2.59908173516064));
#217401=CARTESIAN_POINT('Ctrl Pts',(-0.316922544675889,59.108876741935,
2.90134173516064));
#217402=CARTESIAN_POINT('Ctrl Pts',(-0.316922401514067,59.0966467827009,
2.88176998919896));
#217403=CARTESIAN_POINT('Ctrl Pts',(-0.315000085554109,59.0844716853568,
2.86226752356863));
#217404=CARTESIAN_POINT('Ctrl Pts',(-0.311230629649539,59.0725173476332,
2.84310370500206));
#217405=CARTESIAN_POINT('Ctrl Pts',(-0.30739308360589,59.060347070915,2.82359371788902));
#217406=CARTESIAN_POINT('Ctrl Pts',(-0.301641096265653,59.0484046750375,
2.80443322637298));
#217407=CARTESIAN_POINT('Ctrl Pts',(-0.29400118789602,59.0368573319866,
2.78589323878608));
#217408=CARTESIAN_POINT('Ctrl Pts',(-0.286684733438416,59.0257988735011,
2.76813818620413));
#217409=CARTESIAN_POINT('Ctrl Pts',(-0.277636448050035,59.0151019493871,
2.75095095199189));
#217410=CARTESIAN_POINT('Ctrl Pts',(-0.266835172456312,59.0049186873026,
2.73457771435643));
#217411=CARTESIAN_POINT('Ctrl Pts',(-0.258244193038573,58.9968192555073,
2.72155497955927));
#217412=CARTESIAN_POINT('Ctrl Pts',(-0.248543417988618,58.9890447295132,
2.70904711160149));
#217413=CARTESIAN_POINT('Ctrl Pts',(-0.237702773059694,58.9816789347252,
2.6971895615838));
#217414=CARTESIAN_POINT('Ctrl Pts',(-0.237673181620435,58.9816588284981,
2.69715719432397));
#217415=CARTESIAN_POINT('Ctrl Pts',(-0.237643581717174,58.9816387254918,
2.69712483219063));
#217416=CARTESIAN_POINT('Ctrl Pts',(-0.237613973350488,58.9816186257084,
2.69709247518691));
#217417=CARTESIAN_POINT('Ctrl Pts',(-0.231719887006982,58.9776173965854,
2.69065122242317));
#217418=CARTESIAN_POINT('Ctrl Pts',(-0.225454527233559,58.9737507180864,
2.68442464469466));
#217419=CARTESIAN_POINT('Ctrl Pts',(-0.218853219640928,58.9700384170938,
2.67844505923619));
#217420=CARTESIAN_POINT('Ctrl Pts',(-0.205752467570126,58.9626710986901,
2.66657815779607));
#217421=CARTESIAN_POINT('Ctrl Pts',(-0.191327202905629,58.9559120649698,
2.65568445664213));
#217422=CARTESIAN_POINT('Ctrl Pts',(-0.175845309932447,58.9499179036783,
2.64601906229555));
#217423=CARTESIAN_POINT('Ctrl Pts',(-0.164233890202561,58.9454222827096,
2.63877001653561));
#217424=CARTESIAN_POINT('Ctrl Pts',(-0.152028117041498,58.9413569016701,
2.63221189387641));
#217425=CARTESIAN_POINT('Ctrl Pts',(-0.139341004226338,58.9377878323774,
2.62645231033273));
#217426=CARTESIAN_POINT('Ctrl Pts',(-0.134583336920653,58.9364494313926,
2.62429246650385));
#217427=CARTESIAN_POINT('Ctrl Pts',(-0.129757981227663,58.935180824439,
2.62224491711786));
#217428=CARTESIAN_POINT('Ctrl Pts',(-0.124870896863517,58.9339854965862,
2.62031533672638));
#217429=CARTESIAN_POINT('Ctrl Pts',(-0.107766101589008,58.9298018491014,
2.61356180535619));
#217430=CARTESIAN_POINT('Ctrl Pts',(-0.0899051301002618,58.9265158655231,
2.60825339735388));
#217431=CARTESIAN_POINT('Ctrl Pts',(-0.0715435052827858,58.9242770147328,
2.60463337987651));
#217432=CARTESIAN_POINT('Ctrl Pts',(-0.0623626928740478,58.9231575893377,
2.60282337113783));
#217433=CARTESIAN_POINT('Ctrl Pts',(-0.0530567171307718,58.9222999481583,
2.60143545939156));
#217434=CARTESIAN_POINT('Ctrl Pts',(-0.0436575183856266,58.921722779137,
2.60050005034638));
#217435=CARTESIAN_POINT('Ctrl Pts',(-0.038957919013054,58.9214341946264,
2.60003234582378));
#217436=CARTESIAN_POINT('Ctrl Pts',(-0.0342350138896582,58.9212157281807,
2.59967776696107));
#217437=CARTESIAN_POINT('Ctrl Pts',(-0.0294927955550828,58.9210697160841,
2.59944011429201));
#217438=CARTESIAN_POINT('Ctrl Pts',(-0.0247505772205072,58.9209237039874,
2.59920246162295));
#217439=CARTESIAN_POINT('Ctrl Pts',(-0.0199890456752399,58.9208501479393,
2.59908173791352));
#217440=CARTESIAN_POINT('Ctrl Pts',(-0.0152121934561203,58.9208513795075,
2.59908173516065));
#217441=CARTESIAN_POINT('',(0.0152121934557198,58.9208513795075,2.59908173516064));
#217442=CARTESIAN_POINT('Origin',(4.02492081121313E-16,1.91175617316195E-13,
2.59908173516023));
#217443=CARTESIAN_POINT('',(0.316922544675488,59.108876741935,2.90134173516064));
#217444=CARTESIAN_POINT('Ctrl Pts',(0.0152121934557198,58.9208513795075,
2.59908173516065));
#217445=CARTESIAN_POINT('Ctrl Pts',(0.0190220008283435,58.9208504012366,
2.59908174371555));
#217446=CARTESIAN_POINT('Ctrl Pts',(0.0228214099815236,58.9208964366353,
2.59915764355931));
#217447=CARTESIAN_POINT('Ctrl Pts',(0.0266084895328065,58.9209883940809,
2.59930765775317));
#217448=CARTESIAN_POINT('Ctrl Pts',(0.048967120812902,58.9215313038858,
2.60019333020922));
#217449=CARTESIAN_POINT('Ctrl Pts',(0.070898652760156,58.9236732325288,
2.6036597332413));
#217450=CARTESIAN_POINT('Ctrl Pts',(0.0919988953506439,58.9271900305698,
2.60934177082431));
#217451=CARTESIAN_POINT('Ctrl Pts',(0.0998812435866003,58.9285037892489,
2.6114643909187));
#217452=CARTESIAN_POINT('Ctrl Pts',(0.107647933246302,58.9300091878198,
2.61389584429349));
#217453=CARTESIAN_POINT('Ctrl Pts',(0.115279202946735,58.9316938830319,
2.61661604385294));
#217454=CARTESIAN_POINT('Ctrl Pts',(0.121233502390038,58.9330083667492,
2.61873848000818));
#217455=CARTESIAN_POINT('Ctrl Pts',(0.127104908279827,58.9344322364593,
2.6210370709983));
#217456=CARTESIAN_POINT('Ctrl Pts',(0.132883578272888,58.9359598525095,
2.62350262767694));
#217457=CARTESIAN_POINT('Ctrl Pts',(0.1531089232486,58.9413065086851,2.63213207605221));
#217458=CARTESIAN_POINT('Ctrl Pts',(0.17219825341753,58.9479240485797,2.64280685971956));
#217459=CARTESIAN_POINT('Ctrl Pts',(0.189729578870585,58.9555707636547,
2.65513293646126));
#217460=CARTESIAN_POINT('Ctrl Pts',(0.198495241597112,58.9593941211922,
2.6612959748321));
#217461=CARTESIAN_POINT('Ctrl Pts',(0.206871403160357,58.963474774335,2.66787183533893));
#217462=CARTESIAN_POINT('Ctrl Pts',(0.214805314863019,58.9677825146338,
2.67481125953902));
#217463=CARTESIAN_POINT('Ctrl Pts',(0.222705329147433,58.9720718502314,
2.68172103524121));
#217464=CARTESIAN_POINT('Ctrl Pts',(0.230167055078982,58.976586172246,2.68899101329828));
#217465=CARTESIAN_POINT('Ctrl Pts',(0.23713784456645,58.9812961520167,2.69657334701314));
#217466=CARTESIAN_POINT('Ctrl Pts',(0.237167754862593,58.9813163616199,
2.69660588132611));
#217467=CARTESIAN_POINT('Ctrl Pts',(0.237197656536502,58.9813365744747,
2.6966384208142));
#217468=CARTESIAN_POINT('Ctrl Pts',(0.237227549587754,58.9813567905791,
2.69667096547421));
#217469=CARTESIAN_POINT('Ctrl Pts',(0.251324537972172,58.9908903168212,
2.71201840157982));
#217470=CARTESIAN_POINT('Ctrl Pts',(0.263501580512235,59.0011093202332,
2.72845645939393));
#217471=CARTESIAN_POINT('Ctrl Pts',(0.273820596509237,59.0118294103849,
2.74568723186944));
#217472=CARTESIAN_POINT('Ctrl Pts',(0.284514998004185,59.0229394763231,
2.76354482594379));
#217473=CARTESIAN_POINT('Ctrl Pts',(0.293214009568733,59.0345885736561,
2.78225519317196));
#217474=CARTESIAN_POINT('Ctrl Pts',(0.299936893972635,59.04658752064,2.80151223085589));
#217475=CARTESIAN_POINT('Ctrl Pts',(0.3065638277314,59.0584152157275,2.82049442740346));
#217476=CARTESIAN_POINT('Ctrl Pts',(0.311270560393525,59.0705837677967,
2.8400092908934));
#217477=CARTESIAN_POINT('Ctrl Pts',(0.314027284735791,59.0829139906045,
2.85976644341704));
#217478=CARTESIAN_POINT('Ctrl Pts',(0.315949321994076,59.0915108413219,
2.87354148167017));
#217479=CARTESIAN_POINT('Ctrl Pts',(0.316922445687527,59.1001863397077,
2.88743438345543));
#217480=CARTESIAN_POINT('Ctrl Pts',(0.316922544675488,59.108876741935,2.90134173516064));
#217481=CARTESIAN_POINT('',(0.316925998272844,59.4651754363834,3.47153072139114));
#217482=CARTESIAN_POINT('',(0.316922544675488,59.108876741935,2.90134173516064));
#217483=CARTESIAN_POINT('',(5.90061356181238,59.1725467709679,3.47153072139113));
#217484=CARTESIAN_POINT('Origin',(5.53234440788222E-15,1.85015204418142E-13,
3.47153072139072));
#217485=CARTESIAN_POINT('',(5.86337364149561,58.8181995570487,2.90134173516065));
#217486=CARTESIAN_POINT('',(5.90061356181238,59.1725467709679,3.47153072139113));
#217487=CARTESIAN_POINT('',(6.14377718965303,58.599666897865,2.59908173516064));
#217488=CARTESIAN_POINT('Ctrl Pts',(5.86337364149561,58.8181995570487,2.90134173516065));
#217489=CARTESIAN_POINT('Ctrl Pts',(5.86209540502863,58.8060365798462,2.88176998919861));
#217490=CARTESIAN_POINT('Ctrl Pts',(5.86273454612518,58.7937272422258,2.86226752356793));
#217491=CARTESIAN_POINT('Ctrl Pts',(5.86523378400438,58.7814443761818,2.84310370500102));
#217492=CARTESIAN_POINT('Ctrl Pts',(5.86777816724649,58.768939636722,2.82359371788768));
#217493=CARTESIAN_POINT('Ctrl Pts',(5.8722503243096,58.7564614161411,2.80443322637135));
#217494=CARTESIAN_POINT('Ctrl Pts',(5.87864135443809,58.744178742762,2.78589323878419));
#217495=CARTESIAN_POINT('Ctrl Pts',(5.88476180492122,58.732416085928,2.76813818620209));
#217496=CARTESIAN_POINT('Ctrl Pts',(5.89264238981639,58.7208319573166,2.75095095198971));
#217497=CARTESIAN_POINT('Ctrl Pts',(5.90232005415578,58.7095754394681,2.73457771435415));
#217498=CARTESIAN_POINT('Ctrl Pts',(5.91001735013015,58.7006223753317,2.72155497955782));
#217499=CARTESIAN_POINT('Ctrl Pts',(5.91885232406413,58.6918764318965,2.7090471116008));
#217500=CARTESIAN_POINT('Ctrl Pts',(5.92886364759533,58.6834178317482,2.6971895615838));
#217501=CARTESIAN_POINT('Ctrl Pts',(5.92889097525656,58.6833947425175,2.69715719432397));
#217502=CARTESIAN_POINT('Ctrl Pts',(5.92891831167211,58.6833716556052,2.69712483219063));
#217503=CARTESIAN_POINT('Ctrl Pts',(5.92894565684159,58.6833485710134,2.6970924751869));
#217504=CARTESIAN_POINT('Ctrl Pts',(5.93438921243199,58.6787531612544,2.69065122242316));
#217505=CARTESIAN_POINT('Ctrl Pts',(5.94021607194757,58.6742527563958,2.68442464469467));
#217506=CARTESIAN_POINT('Ctrl Pts',(5.94639317576856,58.6698707672383,2.6784450592362));
#217507=CARTESIAN_POINT('Ctrl Pts',(5.95865206607762,58.661174406294,2.66657815779608));
#217508=CARTESIAN_POINT('Ctrl Pts',(5.97229179622498,58.65294454852,2.65568445664214));
#217509=CARTESIAN_POINT('Ctrl Pts',(5.98706231730018,58.6453649253903,2.64601906229556));
#217510=CARTESIAN_POINT('Ctrl Pts',(5.99814020810658,58.639680208043,2.63877001653562));
#217511=CARTESIAN_POINT('Ctrl Pts',(6.0098541687325,58.6343612468746,2.63221189387641));
#217512=CARTESIAN_POINT('Ctrl Pts',(6.02209871088772,58.6294855649111,2.62645231033273));
#217513=CARTESIAN_POINT('Ctrl Pts',(6.02669041419593,58.6276571841747,2.62429246650385));
#217514=CARTESIAN_POINT('Ctrl Pts',(6.03135673055019,58.6258911397674,2.62224491711786));
#217515=CARTESIAN_POINT('Ctrl Pts',(6.03609209717129,58.6241915206272,2.62031533672638));
#217516=CARTESIAN_POINT('Ctrl Pts',(6.05266588034514,58.6182428536365,2.61356180535619));
#217517=CARTESIAN_POINT('Ctrl Pts',(6.07008552874948,58.6131078911179,2.60825339735388));
#217518=CARTESIAN_POINT('Ctrl Pts',(6.08811254303241,58.6089619925612,2.60463337987651));
#217519=CARTESIAN_POINT('Ctrl Pts',(6.09712605017387,58.6068890432829,2.60282337113783));
#217520=CARTESIAN_POINT('Ctrl Pts',(6.10629139889382,58.6050633610081,2.60143545939155));
#217521=CARTESIAN_POINT('Ctrl Pts',(6.11557877725394,58.6035068699783,2.60050005034636));
#217522=CARTESIAN_POINT('Ctrl Pts',(6.120222466434,58.6027286244634,2.60003234582377));
#217523=CARTESIAN_POINT('Ctrl Pts',(6.12489666302712,58.602017676785,2.59967776696106));
#217524=CARTESIAN_POINT('Ctrl Pts',(6.12959764057339,58.6013767677629,2.599440114292));
#217525=CARTESIAN_POINT('Ctrl Pts',(6.13429861811967,58.6007358587408,2.59920246162294));
#217526=CARTESIAN_POINT('Ctrl Pts',(6.13902637679625,58.6001649900653,2.59908173791355));
#217527=CARTESIAN_POINT('Ctrl Pts',(6.14377718965303,58.599666897865,2.59908173516065));
#217528=CARTESIAN_POINT('',(6.17403490859001,58.5964866834553,2.59908173516065));
#217529=CARTESIAN_POINT('Origin',(5.66232193761676E-15,1.85922536175558E-13,
2.59908173516024));
#217530=CARTESIAN_POINT('',(6.49374646112721,58.7519447039091,2.90134173516065));
#217531=CARTESIAN_POINT('Ctrl Pts',(6.17403490859001,58.5964866834553,2.59908173516065));
#217532=CARTESIAN_POINT('Ctrl Pts',(6.17782374318207,58.5960874772335,2.59908174371556));
#217533=CARTESIAN_POINT('Ctrl Pts',(6.18160715078386,58.5957361140453,2.59915764355931));
#217534=CARTESIAN_POINT('Ctrl Pts',(6.18538309648759,58.5954317101327,2.59930765775318));
#217535=CARTESIAN_POINT('Ctrl Pts',(6.20767599437387,58.5936345324523,2.60019333020923));
#217536=CARTESIAN_POINT('Ctrl Pts',(6.22971127560402,58.5934722580546,2.60365973324136));
#217537=CARTESIAN_POINT('Ctrl Pts',(6.25106353435283,58.5947642147754,2.60934177082444));
#217538=CARTESIAN_POINT('Ctrl Pts',(6.25904002743607,58.595246846799,2.6114643909188));
#217539=CARTESIAN_POINT('Ctrl Pts',(6.26692152735623,58.5959321585041,2.61389584429355));
#217540=CARTESIAN_POINT('Ctrl Pts',(6.27468709076422,58.596809939885,2.61661604385295));
#217541=CARTESIAN_POINT('Ctrl Pts',(6.28074617289512,58.5974948289523,2.61873848000818));
#217542=CARTESIAN_POINT('Ctrl Pts',(6.2867342495218,58.5982971695203,2.62103707099828));
#217543=CARTESIAN_POINT('Ctrl Pts',(6.2926409427142,58.5992123816358,2.62350262767693));
#217544=CARTESIAN_POINT('Ctrl Pts',(6.31331436888758,58.6024156240401,2.63213207605219));
#217545=CARTESIAN_POINT('Ctrl Pts',(6.33299084698429,58.6070015340114,2.64280685971955));
#217546=CARTESIAN_POINT('Ctrl Pts',(6.35122543337802,58.6127738370725,2.65513293646125));
#217547=CARTESIAN_POINT('Ctrl Pts',(6.36034272657489,58.615659988603,2.6612959748321));
#217548=CARTESIAN_POINT('Ctrl Pts',(6.36909954705082,58.6188427402047,2.66787183533892));
#217549=CARTESIAN_POINT('Ctrl Pts',(6.37744027742863,58.6222975626534,2.67481125953901));
#217550=CARTESIAN_POINT('Ctrl Pts',(6.38574537226666,58.6257376244688,2.6817210352412));
#217551=CARTESIAN_POINT('Ctrl Pts',(6.39363809722571,58.6294472538101,2.68899101329829));
#217552=CARTESIAN_POINT('Ctrl Pts',(6.40106302694645,58.6334027859059,2.69657334701315));
#217553=CARTESIAN_POINT('Ctrl Pts',(6.40109488586963,58.6334197583216,2.69660588132612));
#217554=CARTESIAN_POINT('Ctrl Pts',(6.40112673655769,58.6334367348722,2.6966384208142));
#217555=CARTESIAN_POINT('Ctrl Pts',(6.40115857901,58.6334537155559,2.69667096547421));
#217556=CARTESIAN_POINT('Ctrl Pts',(6.41617486746507,58.6414614796115,2.71201840158023));
#217557=CARTESIAN_POINT('Ctrl Pts',(6.42935337961508,58.65035165471,2.72845645939482));
#217558=CARTESIAN_POINT('Ctrl Pts',(6.4407364215126,58.6599343882018,2.74568723187084));
#217559=CARTESIAN_POINT('Ctrl Pts',(6.45253355607674,58.6698657226829,2.76354482594574));
#217560=CARTESIAN_POINT('Ctrl Pts',(6.46240257578854,58.6805417107313,2.78225519317451));
#217561=CARTESIAN_POINT('Ctrl Pts',(6.47034286301732,58.6917721934532,2.80151223085904));
#217562=CARTESIAN_POINT('Ctrl Pts',(6.47816982453107,58.7028423919878,2.82049442740721));
#217563=CARTESIAN_POINT('Ctrl Pts',(6.48412273326709,58.7144522959238,2.84000929089776));
#217564=CARTESIAN_POINT('Ctrl Pts',(6.48815321522661,58.7264268163221,2.85976644342199));
#217565=CARTESIAN_POINT('Ctrl Pts',(6.49096333895756,58.7347756649899,2.8735414816735));
#217566=CARTESIAN_POINT('Ctrl Pts',(6.49283796829161,58.7433019189626,2.8874343834571));
#217567=CARTESIAN_POINT('Ctrl Pts',(6.49374646112721,58.7519447039091,2.90134173516065));
#217568=CARTESIAN_POINT('',(6.53099325080036,59.1062911958298,3.47153072139114));
#217569=CARTESIAN_POINT('',(6.49374646112721,58.7519447039091,2.90134173516065));
#217570=CARTESIAN_POINT('',(12.053504764932,58.2316113004783,3.47153072139113));
#217571=CARTESIAN_POINT('Origin',(5.53234440788222E-15,1.85015204418142E-13,
3.47153072139072));
#217572=CARTESIAN_POINT('',(11.9794294790611,57.8830978693158,2.90134173516064));
#217573=CARTESIAN_POINT('',(12.053504764932,58.2316113004783,3.47153072139113));
#217574=CARTESIAN_POINT('',(12.2354540642043,57.6364522029209,2.59908173516063));
#217575=CARTESIAN_POINT('Ctrl Pts',(11.9794294790611,57.8830978693158,2.90134173516064));
#217576=CARTESIAN_POINT('Ctrl Pts',(11.9768868675913,57.8711351342684,2.88176998919826));
#217577=CARTESIAN_POINT('Ctrl Pts',(11.9762358312606,57.8588264200507,2.86226752356724));
#217578=CARTESIAN_POINT('Ctrl Pts',(11.9774374689412,57.8463495993369,2.84310370500002));
#217579=CARTESIAN_POINT('Ctrl Pts',(11.9786608125865,57.8336474016777,2.82359371788621));
#217580=CARTESIAN_POINT('Ctrl Pts',(11.9818041414838,57.8207700703892,2.80443322636944));
#217581=CARTESIAN_POINT('Ctrl Pts',(11.9868762719078,57.8078866382217,2.78589323878188));
#217582=CARTESIAN_POINT('Ctrl Pts',(11.9917336614803,57.7955486571686,2.76813818619916));
#217583=CARTESIAN_POINT('Ctrl Pts',(11.9983602045454,57.7832042421965,2.75095095198623));
#217584=CARTESIAN_POINT('Ctrl Pts',(12.0068082271151,57.7709977973487,2.73457771435019));
#217585=CARTESIAN_POINT('Ctrl Pts',(12.0135275064606,57.7612891925159,2.72155497955527));
#217586=CARTESIAN_POINT('Ctrl Pts',(12.0213998814552,57.7516676540266,2.70904711159958));
#217587=CARTESIAN_POINT('Ctrl Pts',(12.0304721974328,57.742208922712,2.69718956158378));
#217588=CARTESIAN_POINT('Ctrl Pts',(12.0304969619084,57.742183103448,2.69715719432395));
#217589=CARTESIAN_POINT('Ctrl Pts',(12.0305217353328,57.7421572855747,2.69712483219061));
#217590=CARTESIAN_POINT('Ctrl Pts',(12.0305465177057,57.7421314690942,2.69709247518689));
#217591=CARTESIAN_POINT('Ctrl Pts',(12.0354799018088,57.7369922269701,2.69065122242315));
#217592=CARTESIAN_POINT('Ctrl Pts',(12.0408044207743,57.7319074031294,2.68442464469465));
#217593=CARTESIAN_POINT('Ctrl Pts',(12.0464896431816,57.7269037357971,2.67844505923618));
#217594=CARTESIAN_POINT('Ctrl Pts',(12.0577723607613,57.7169736114626,2.66657815779606));
#217595=CARTESIAN_POINT('Ctrl Pts',(12.0704771166537,57.7073630976789,2.65568445664212));
#217596=CARTESIAN_POINT('Ctrl Pts',(12.0843744369111,57.6982810566481,2.64601906229554));
#217597=CARTESIAN_POINT('Ctrl Pts',(12.0947974271042,57.691469525875,2.6387700165356));
#217598=CARTESIAN_POINT('Ctrl Pts',(12.105891234591,57.6849552602295,2.6322118938764));
#217599=CARTESIAN_POINT('Ctrl Pts',(12.1175590523201,57.678826384587,2.62645231033272));
#217600=CARTESIAN_POINT('Ctrl Pts',(12.1219344839685,57.676528056221,2.62429246650384));
#217601=CARTESIAN_POINT('Ctrl Pts',(12.1263906358456,57.6742839235121,2.62224491711785));
#217602=CARTESIAN_POINT('Ctrl Pts',(12.130922403056,57.6720986344675,2.62031533672637));
#217603=CARTESIAN_POINT('Ctrl Pts',(12.1467835882925,57.6644501228113,2.61356180535618));
#217604=CARTESIAN_POINT('Ctrl Pts',(12.1635710602992,57.6575224410762,2.60825339735387));
#217605=CARTESIAN_POINT('Ctrl Pts',(12.1810659563067,57.6515149180854,2.6046333798765));
#217606=CARTESIAN_POINT('Ctrl Pts',(12.1898134043104,57.6485111565899,2.60282337113781));
#217607=CARTESIAN_POINT('Ctrl Pts',(12.1987377085285,57.6457374357766,2.60143545939154));
#217608=CARTESIAN_POINT('Ctrl Pts',(12.2078115120428,57.6432186759798,2.60050005034636));
#217609=CARTESIAN_POINT('Ctrl Pts',(12.2123484137999,57.6419592960813,2.60003234582376));
#217610=CARTESIAN_POINT('Ctrl Pts',(12.2169226903867,57.6407636564619,2.59967776696105));
#217611=CARTESIAN_POINT('Ctrl Pts',(12.221530922251,57.6396348724477,2.59944011429199));
#217612=CARTESIAN_POINT('Ctrl Pts',(12.2261391541152,57.6385060884335,2.59920246162293));
#217613=CARTESIAN_POINT('Ctrl Pts',(12.2307813416097,57.6374441616871,2.59908173791356));
#217614=CARTESIAN_POINT('Ctrl Pts',(12.2354540642043,57.6364522029209,2.59908173516064));
#217615=CARTESIAN_POINT('',(12.2652136052659,57.630126617196,2.59908173516063));
#217616=CARTESIAN_POINT('Origin',(5.66936586998423E-15,1.85921420526272E-13,
2.59908173516023));
#217617=CARTESIAN_POINT('',(12.599423532447,57.7513140650722,2.90134173516063));
#217618=CARTESIAN_POINT('Ctrl Pts',(12.2652136052659,57.630126617196,2.59908173516064));
#217619=CARTESIAN_POINT('Ctrl Pts',(12.2689399558127,57.6293335568101,2.59908174371554));
#217620=CARTESIAN_POINT('Ctrl Pts',(12.2726659100577,57.6285886446437,2.59915764355929));
#217621=CARTESIAN_POINT('Ctrl Pts',(12.2763893518626,57.6278912144858,2.59930765775316));
#217622=CARTESIAN_POINT('Ctrl Pts',(12.2983722707008,57.623773639575,2.60019333020922));
#217623=CARTESIAN_POINT('Ctrl Pts',(12.3202698780615,57.6213089400487,2.60365973324141));
#217624=CARTESIAN_POINT('Ctrl Pts',(12.3416402131536,57.6203619005011,2.60934177082459));
#217625=CARTESIAN_POINT('Ctrl Pts',(12.3496234589567,57.6200081180517,2.61146439091891));
#217626=CARTESIAN_POINT('Ctrl Pts',(12.3575334177749,57.6198658344727,2.6138958442936));
#217627=CARTESIAN_POINT('Ctrl Pts',(12.3653481937526,57.6199270848659,2.61661604385293));
#217628=CARTESIAN_POINT('Ctrl Pts',(12.3714456739993,57.6199748754953,2.61873848000816));
#217629=CARTESIAN_POINT('Ctrl Pts',(12.3774848147423,57.62014689631,2.62103707099827));
#217630=CARTESIAN_POINT('Ctrl Pts',(12.3834548161673,57.6204396772354,2.62350262767692));
#217631=CARTESIAN_POINT('Ctrl Pts',(12.404349821155,57.6214644104742,2.63213207605218));
#217632=CARTESIAN_POINT('Ctrl Pts',(12.4243978675679,57.6239684463329,2.64280685971954));
#217633=CARTESIAN_POINT('Ctrl Pts',(12.443135932958,57.6278030948198,2.65513293646124));
#217634=CARTESIAN_POINT('Ctrl Pts',(12.452504965653,57.6297204190633,2.66129597483208));
#217635=CARTESIAN_POINT('Ctrl Pts',(12.461546503484,57.6319703982312,2.66787183533892));
#217636=CARTESIAN_POINT('Ctrl Pts',(12.4702026697495,57.6345344510721,2.67481125953901));
#217637=CARTESIAN_POINT('Ctrl Pts',(12.4788218527842,57.6370875490683,2.6817210352412));
#217638=CARTESIAN_POINT('Ctrl Pts',(12.4870591024244,57.6399518422609,2.68899101329827));
#217639=CARTESIAN_POINT('Ctrl Pts',(12.4948568232946,57.6431095890445,2.69657334701313));
#217640=CARTESIAN_POINT('Ctrl Pts',(12.4948902817918,57.6431231383191,2.6966058813261));
#217641=CARTESIAN_POINT('Ctrl Pts',(12.4949237325312,57.643136692567,2.69663842081419));
#217642=CARTESIAN_POINT('Ctrl Pts',(12.494957175512,57.6431502517861,2.69667096547419));
#217643=CARTESIAN_POINT('Ctrl Pts',(12.5107282424387,57.6495445189161,2.7120184015802));
#217644=CARTESIAN_POINT('Ctrl Pts',(12.5247638376615,57.657008463082,2.72845645939476));
#217645=CARTESIAN_POINT('Ctrl Pts',(12.5370861904703,57.6653488494803,2.74568723187076));
#217646=CARTESIAN_POINT('Ctrl Pts',(12.5498568062284,57.6739926427249,2.76354482594561));
#217647=CARTESIAN_POINT('Ctrl Pts',(12.5607877070422,57.6835785531293,2.7822551931743));
#217648=CARTESIAN_POINT('Ctrl Pts',(12.5698584016474,57.6939175280698,2.80151223085877));
#217649=CARTESIAN_POINT('Ctrl Pts',(12.5787996370878,57.7041089426393,2.8204944274068));
#217650=CARTESIAN_POINT('Ctrl Pts',(12.585933500584,57.7150329979046,2.84000929089722));
#217651=CARTESIAN_POINT('Ctrl Pts',(12.5911935813573,57.7265206205418,2.85976644342131));
#217652=CARTESIAN_POINT('Ctrl Pts',(12.5948610032578,57.7345299954279,2.87354148167304));
#217653=CARTESIAN_POINT('Ctrl Pts',(12.5976165994014,57.7428135895658,2.88743438345685));
#217654=CARTESIAN_POINT('Ctrl Pts',(12.599423532447,57.7513140650722,2.90134173516062));
#217655=CARTESIAN_POINT('',(12.6735055745739,58.0998260601482,3.47153072139113));
#217656=CARTESIAN_POINT('',(12.599423532447,57.7513140650722,2.90134173516063));
#217657=CARTESIAN_POINT('',(18.074335247489,56.6526781108326,3.47153072139111));
#217658=CARTESIAN_POINT('Origin',(5.53234440788222E-15,1.85015204418142E-13,
3.47153072139072));
#217659=CARTESIAN_POINT('',(17.9642361803971,56.3138168485097,2.90134173516062));
#217660=CARTESIAN_POINT('',(18.074335247489,56.6526781108326,3.47153072139112));
#217661=CARTESIAN_POINT('',(18.1930767435948,56.0417604764385,2.59908173516062));
#217662=CARTESIAN_POINT('Ctrl Pts',(17.9642361803971,56.3138168485097,2.90134173516062));
#217663=CARTESIAN_POINT('Ctrl Pts',(17.9604570513084,56.3021854218465,2.8817699891988));
#217664=CARTESIAN_POINT('Ctrl Pts',(17.9585229704411,56.2900121878806,2.86226752356833));
#217665=CARTESIAN_POINT('Ctrl Pts',(17.9584138425289,56.2774781111564,2.84310370500163));
#217666=CARTESIAN_POINT('Ctrl Pts',(17.9583027433682,56.2647176232342,2.82359371788858));
#217667=CARTESIAN_POINT('Ctrl Pts',(17.9600828051301,56.2515822679753,2.80443322637254));
#217668=CARTESIAN_POINT('Ctrl Pts',(17.9637804645263,56.2382392305991,2.78589323878563));
#217669=CARTESIAN_POINT('Ctrl Pts',(17.9673215746107,56.2254611028304,2.76813818620392));
#217670=CARTESIAN_POINT('Ctrl Pts',(17.9726214740518,56.2124916494927,2.7509509519919));
#217671=CARTESIAN_POINT('Ctrl Pts',(17.979747296547,56.1994690140109,2.73457771435663));
#217672=CARTESIAN_POINT('Ctrl Pts',(17.9854149414341,56.1891112379853,2.7215549795594));
#217673=CARTESIAN_POINT('Ctrl Pts',(17.9922384661031,56.1787195200284,2.70904711160154));
#217674=CARTESIAN_POINT('Ctrl Pts',(18.0002723763371,56.1683642893845,2.69718956158378));
#217675=CARTESIAN_POINT('Ctrl Pts',(18.0002943063023,56.1683360229685,2.69715719432395));
#217676=CARTESIAN_POINT('Ctrl Pts',(18.0003162453126,56.1683077570003,2.6971248321906));
#217677=CARTESIAN_POINT('Ctrl Pts',(18.000338193368,56.1682794914818,2.69709247518688));
#217678=CARTESIAN_POINT('Ctrl Pts',(18.0047073547953,56.1626527236047,2.69065122242314));
#217679=CARTESIAN_POINT('Ctrl Pts',(18.0094711966667,56.157039191176,2.68442464469463));
#217680=CARTESIAN_POINT('Ctrl Pts',(18.0146022491738,56.1514686668953,2.67844505923616));
#217681=CARTESIAN_POINT('Ctrl Pts',(18.0247851782094,56.1404135756909,2.66657815779605));
#217682=CARTESIAN_POINT('Ctrl Pts',(18.0364157638827,56.1295277006976,2.65568445664212));
#217683=CARTESIAN_POINT('Ctrl Pts',(18.0492876213733,56.1190427465078,2.64601906229553));
#217684=CARTESIAN_POINT('Ctrl Pts',(18.0589415144913,56.1111790308655,2.63877001653559));
#217685=CARTESIAN_POINT('Ctrl Pts',(18.0692936227627,56.1035408324003,2.63221189387639));
#217686=CARTESIAN_POINT('Ctrl Pts',(18.080256881013,56.0962259123229,2.62645231033271));
#217687=CARTESIAN_POINT('Ctrl Pts',(18.0843681028569,56.0934828172939,2.62429246650383));
#217688=CARTESIAN_POINT('Ctrl Pts',(18.0885652677243,56.090785183471,2.62224491711783));
#217689=CARTESIAN_POINT('Ctrl Pts',(18.0928437845341,56.088138167006,2.62031533672635));
#217690=CARTESIAN_POINT('Ctrl Pts',(18.1078185933686,56.0788736093786,2.61356180535616));
#217691=CARTESIAN_POINT('Ctrl Pts',(18.1237899619214,56.0702291095579,2.60825339735387));
#217692=CARTESIAN_POINT('Ctrl Pts',(18.1405610619117,56.0624257818119,2.6046333798765));
#217693=CARTESIAN_POINT('Ctrl Pts',(18.1489466119069,56.0585241179389,2.60282337113782));
#217694=CARTESIAN_POINT('Ctrl Pts',(18.1575320950786,56.0548327480527,2.60143545939154));
#217695=CARTESIAN_POINT('Ctrl Pts',(18.1662929092569,56.0513793155482,2.60050005034635));
#217696=CARTESIAN_POINT('Ctrl Pts',(18.170673316346,56.049652599296,2.60003234582376));
#217697=CARTESIAN_POINT('Ctrl Pts',(18.1750975561951,56.0479853674133,2.59967776696105));
#217698=CARTESIAN_POINT('Ctrl Pts',(18.1795625536246,56.0463810756009,2.59944011429199));
#217699=CARTESIAN_POINT('Ctrl Pts',(18.1840275510541,56.0447767837885,2.59920246162293));
#217700=CARTESIAN_POINT('Ctrl Pts',(18.1885333065889,56.043235433663,2.59908173791354));
#217701=CARTESIAN_POINT('Ctrl Pts',(18.1930767435948,56.0417604764385,2.59908173516063));
#217702=CARTESIAN_POINT('',(18.2220120550216,56.0323588238393,2.59908173516062));
#217703=CARTESIAN_POINT('Origin',(5.6762545978478E-15,1.85919574697204E-13,
2.59908173516023));
#217704=CARTESIAN_POINT('',(18.5670586829464,56.117947944099,2.90134173516062));
#217705=CARTESIAN_POINT('Ctrl Pts',(18.2220120550216,56.0323588238393,2.59908173516063));
#217706=CARTESIAN_POINT('Ctrl Pts',(18.2256350948468,56.031180598225,2.59908174371555));
#217707=CARTESIAN_POINT('Ctrl Pts',(18.2292627734005,56.030050298494,2.59915764355929));
#217708=CARTESIAN_POINT('Ctrl Pts',(18.232892916499,56.0289674832815,2.59930765775315));
#217709=CARTESIAN_POINT('Ctrl Pts',(18.2543250068308,56.0225746241523,2.60019333020925));
#217710=CARTESIAN_POINT('Ctrl Pts',(18.2758450255544,56.0178345032611,2.60365973324173));
#217711=CARTESIAN_POINT('Ctrl Pts',(18.2969992991273,56.0146588434085,2.60934177082538));
#217712=CARTESIAN_POINT('Ctrl Pts',(18.3049018315378,56.0134725226009,2.61146439091951));
#217713=CARTESIAN_POINT('Ctrl Pts',(18.312753586089,56.0125042026267,2.61389584429393));
#217714=CARTESIAN_POINT('Ctrl Pts',(18.3205319543147,56.0117482509602,2.61661604385292));
#217715=CARTESIAN_POINT('Ctrl Pts',(18.3266010274077,56.0111584195475,2.61873848000815));
#217716=CARTESIAN_POINT('Ctrl Pts',(18.3326250661772,56.0106982359128,2.62103707099826));
#217717=CARTESIAN_POINT('Ctrl Pts',(18.3385929672501,56.010365377879,2.62350262767691));
#217718=CARTESIAN_POINT('Ctrl Pts',(18.3594806210049,56.0092003747606,2.63213207605218));
#217719=CARTESIAN_POINT('Ctrl Pts',(18.3796805851421,56.0095951017658,2.64280685971953));
#217720=CARTESIAN_POINT('Ctrl Pts',(18.3987168313629,56.0114500824672,2.65513293646122));
#217721=CARTESIAN_POINT('Ctrl Pts',(18.4082349544733,56.012377572818,2.66129597483207));
#217722=CARTESIAN_POINT('Ctrl Pts',(18.4174621486788,56.0136701283095,2.6678718353389));
#217723=CARTESIAN_POINT('Ctrl Pts',(18.426338912063,56.0153153192432,2.67481125953899));
#217724=CARTESIAN_POINT('Ctrl Pts',(18.4351777497213,56.0169534811442,2.68172103524118));
#217725=CARTESIAN_POINT('Ctrl Pts',(18.4436692750119,56.0189410563925,2.68899101329826));
#217726=CARTESIAN_POINT('Ctrl Pts',(18.4517543535699,56.0212664209292,2.69657334701312));
#217727=CARTESIAN_POINT('Ctrl Pts',(18.4517890450628,56.0212763986143,2.69660588132609));
#217728=CARTESIAN_POINT('Ctrl Pts',(18.4518237293603,56.0212863820561,2.69663842081418));
#217729=CARTESIAN_POINT('Ctrl Pts',(18.4518584064613,56.0212963712531,2.69667096547418));
#217730=CARTESIAN_POINT('Ctrl Pts',(18.4682114607491,56.0260070845285,2.71201840157933));
#217731=CARTESIAN_POINT('Ctrl Pts',(18.4829503621255,56.0319630212272,2.72845645939292));
#217732=CARTESIAN_POINT('Ctrl Pts',(18.496077019569,56.0389696815127,2.74568723186786));
#217733=CARTESIAN_POINT('Ctrl Pts',(18.5096811989819,56.0462312303128,2.76354482594163));
#217734=CARTESIAN_POINT('Ctrl Pts',(18.5215542196605,56.0546220378322,2.78225519316918));
#217735=CARTESIAN_POINT('Ctrl Pts',(18.5316559412137,56.0639562290176,2.80151223085247));
#217736=CARTESIAN_POINT('Ctrl Pts',(18.5416134885343,56.0731572003508,2.82049442739942));
#217737=CARTESIAN_POINT('Ctrl Pts',(18.5498501466894,56.0832757207091,2.84000929088874));
#217738=CARTESIAN_POINT('Ctrl Pts',(18.5562821957309,56.0941505847868,2.85976644341176));
#217739=CARTESIAN_POINT('Ctrl Pts',(18.5607667347605,56.1017327335055,2.87354148166662));
#217740=CARTESIAN_POINT('Ctrl Pts',(18.5643731068268,56.1096829110195,2.88743438345364));
#217741=CARTESIAN_POINT('Ctrl Pts',(18.5670586829464,56.117947944099,2.90134173516062));
#217742=CARTESIAN_POINT('',(18.6771643191709,56.4568070719813,3.47153072139112));
#217743=CARTESIAN_POINT('',(18.5670586829464,56.117947944099,2.90134173516062));
#217744=CARTESIAN_POINT('',(23.8971395307767,54.4530463244695,3.4715307213911));
#217745=CARTESIAN_POINT('Origin',(5.53234440788222E-15,1.85015204418142E-13,
3.47153072139072));
#217746=CARTESIAN_POINT('',(23.7522229508827,54.1275498658876,2.90134173516061));
#217747=CARTESIAN_POINT('',(23.8971395307767,54.4530463244695,3.4715307213911));
#217748=CARTESIAN_POINT('',(23.9513722670364,53.833063494684,2.59908173516061));
#217749=CARTESIAN_POINT('Ctrl Pts',(23.7522229508827,54.1275498658876,2.90134173516061));
#217750=CARTESIAN_POINT('Ctrl Pts',(23.7472487091033,54.1163771839518,2.88176998919702));
#217751=CARTESIAN_POINT('Ctrl Pts',(23.7440527738937,54.1044728027351,2.8622675235648));
#217752=CARTESIAN_POINT('Ctrl Pts',(23.7426340760174,54.0920187959664,2.84310370499643));
#217753=CARTESIAN_POINT('Ctrl Pts',(23.7411897512766,54.0793398243554,2.8235937178816));
#217754=CARTESIAN_POINT('Ctrl Pts',(23.7415870431748,54.0660903588251,2.80443322636387));
#217755=CARTESIAN_POINT('Ctrl Pts',(23.7438697192146,54.0524339053479,2.78589323877544));
#217756=CARTESIAN_POINT('Ctrl Pts',(23.7460557526692,54.0393556307033,2.76813818619217));
#217757=CARTESIAN_POINT('Ctrl Pts',(23.749970941681,54.0259032350424,2.75095095197874));
#217758=CARTESIAN_POINT('Ctrl Pts',(23.7556964921022,54.0122070876439,2.73457771434232));
#217759=CARTESIAN_POINT('Ctrl Pts',(23.7602504066259,54.0013136223926,2.72155497955023));
#217760=CARTESIAN_POINT('Ctrl Pts',(23.7659503210024,53.9902655788103,2.70904711159718));
#217761=CARTESIAN_POINT('Ctrl Pts',(23.772857804287,53.9791273029166,2.69718956158376));
#217762=CARTESIAN_POINT('Ctrl Pts',(23.7728766594726,53.9790968990415,2.69715719432393));
#217763=CARTESIAN_POINT('Ctrl Pts',(23.7728955237005,53.9790664946661,2.69712483219059));
#217764=CARTESIAN_POINT('Ctrl Pts',(23.7729143969709,53.9790360897926,2.69709247518687));
#217765=CARTESIAN_POINT('Ctrl Pts',(23.7766714662753,53.9729834442089,2.69065122242313));
#217766=CARTESIAN_POINT('Ctrl Pts',(23.7808224374043,53.9669027062281,2.68442464469463));
#217767=CARTESIAN_POINT('Ctrl Pts',(23.7853431031263,53.9608263568288,2.67844505923616));
#217768=CARTESIAN_POINT('Ctrl Pts',(23.7943146773162,53.948767420647,2.66657815779604));
#217769=CARTESIAN_POINT('Ctrl Pts',(23.8047436656399,53.9367254523687,2.6556844566421));
#217770=CARTESIAN_POINT('Ctrl Pts',(23.8164490335996,53.9249524603721,2.64601906229552));
#217771=CARTESIAN_POINT('Ctrl Pts',(23.8252280595693,53.9161227163746,2.63877001653558));
#217772=CARTESIAN_POINT('Ctrl Pts',(23.8347250487607,53.9074442707907,2.63221189387639));
#217773=CARTESIAN_POINT('Ctrl Pts',(23.8448636317806,53.8990234500736,2.62645231033271));
#217774=CARTESIAN_POINT('Ctrl Pts',(23.848665600413,53.8958656423046,2.62429246650383));
#217775=CARTESIAN_POINT('Ctrl Pts',(23.8525577932542,53.8927440632084,2.62224491711782));
#217776=CARTESIAN_POINT('Ctrl Pts',(23.8565361833379,53.8896643205894,2.62031533672634));
#217777=CARTESIAN_POINT('Ctrl Pts',(23.8704605486311,53.8788852214228,2.61356180535615));
#217778=CARTESIAN_POINT('Ctrl Pts',(23.8854408280738,53.8686186144655,2.60825339735384));
#217779=CARTESIAN_POINT('Ctrl Pts',(23.901304384366,53.859104976856,2.60463337987647));
#217780=CARTESIAN_POINT('Ctrl Pts',(23.9092361625121,53.8543481580513,2.60282337113779));
#217781=CARTESIAN_POINT('Ctrl Pts',(23.9173887602871,53.8497795825133,2.60143545939151));
#217782=CARTESIAN_POINT('Ctrl Pts',(23.9257405998159,53.8454293138304,2.60050005034632));
#217783=CARTESIAN_POINT('Ctrl Pts',(23.9299165195804,53.8432541794889,2.60003234582373));
#217784=CARTESIAN_POINT('Ctrl Pts',(23.934142249794,53.8411336218844,2.59967776696103));
#217785=CARTESIAN_POINT('Ctrl Pts',(23.9384150933427,53.8390713992306,2.59944011429197));
#217786=CARTESIAN_POINT('Ctrl Pts',(23.9426879368913,53.8370091765768,2.59920246162291));
#217787=CARTESIAN_POINT('Ctrl Pts',(23.9470078944659,53.8350052904266,2.59908173791346));
#217788=CARTESIAN_POINT('Ctrl Pts',(23.9513722670364,53.833063494684,2.59908173516062));
#217789=CARTESIAN_POINT('',(23.9791663275012,53.8206887816839,2.59908173516061));
#217790=CARTESIAN_POINT('Origin',(5.68291264686342E-15,1.85917018911644E-13,
2.59908173516024));
#217791=CARTESIAN_POINT('',(24.3312692531087,53.8697418420147,2.90134173516062));
#217792=CARTESIAN_POINT('Ctrl Pts',(23.9791663275012,53.8206887816838,2.59908173516062));
#217793=CARTESIAN_POINT('Ctrl Pts',(23.9826463618224,53.8191382997274,2.59908174371552));
#217794=CARTESIAN_POINT('Ctrl Pts',(23.9861360190795,53.8176349962321,2.59915764355927));
#217795=CARTESIAN_POINT('Ctrl Pts',(23.9896330908641,53.8161786595151,2.59930765775314));
#217796=CARTESIAN_POINT('Ctrl Pts',(24.0102795382193,53.8075805576712,2.60019333020912));
#217797=CARTESIAN_POINT('Ctrl Pts',(24.0311861904735,53.8006169491722,2.60365973324083));
#217798=CARTESIAN_POINT('Ctrl Pts',(24.0518926318755,53.7952474622088,2.60934177082319));
#217799=CARTESIAN_POINT('Ctrl Pts',(24.0596278690982,53.7932416006211,2.61146439091783));
#217800=CARTESIAN_POINT('Ctrl Pts',(24.0673353939203,53.7914578533671,2.61389584429299));
#217801=CARTESIAN_POINT('Ctrl Pts',(24.0749921329676,53.789892982005,2.6166160438529));
#217802=CARTESIAN_POINT('Ctrl Pts',(24.0809663048721,53.7886719908667,2.61873848000813));
#217803=CARTESIAN_POINT('Ctrl Pts',(24.0869092410387,53.7875846446509,2.62103707099824));
#217804=CARTESIAN_POINT('Ctrl Pts',(24.0928096561863,53.7866297945201,2.62350262767689));
#217805=CARTESIAN_POINT('Ctrl Pts',(24.1134611092026,53.7832878190624,2.63213207605215));
#217806=CARTESIAN_POINT('Ctrl Pts',(24.1335916760301,53.7815689125025,2.64280685971951));
#217807=CARTESIAN_POINT('Ctrl Pts',(24.1527175379843,53.7814239018617,2.65513293646121));
#217808=CARTESIAN_POINT('Ctrl Pts',(24.1622804689615,53.7813513965413,2.66129597483206));
#217809=CARTESIAN_POINT('Ctrl Pts',(24.1715922244709,53.781672366848,2.66787183533889));
#217810=CARTESIAN_POINT('Ctrl Pts',(24.1805923292966,53.7823806708183,2.67481125953899));
#217811=CARTESIAN_POINT('Ctrl Pts',(24.1895539814234,53.7830859485795,2.68172103524117));
#217812=CARTESIAN_POINT('Ctrl Pts',(24.1982067474363,53.7841750295933,2.68899101329827));
#217813=CARTESIAN_POINT('Ctrl Pts',(24.2064906018697,53.7856425347027,2.69657334701313));
#217814=CARTESIAN_POINT('Ctrl Pts',(24.206526146271,53.7856488314805,2.6966058813261));
#217815=CARTESIAN_POINT('Ctrl Pts',(24.2065616841181,53.7856551347357,2.69663842081418));
#217816=CARTESIAN_POINT('Ctrl Pts',(24.2065972154097,53.7856614444667,2.69667096547419));
#217817=CARTESIAN_POINT('Ctrl Pts',(24.2233530895743,53.7886369923274,2.71201840157898));
#217818=CARTESIAN_POINT('Ctrl Pts',(24.2386338146169,53.7930196670704,2.72845645939216));
#217819=CARTESIAN_POINT('Ctrl Pts',(24.2524209582896,53.7986158348071,2.74568723186666));
#217820=CARTESIAN_POINT('Ctrl Pts',(24.2667096511209,53.8044155801148,2.76354482593984));
#217821=CARTESIAN_POINT('Ctrl Pts',(24.2793947083652,53.8115193533064,2.78225519316674));
#217822=CARTESIAN_POINT('Ctrl Pts',(24.2904167802911,53.8197464933851,2.80151223084937));
#217823=CARTESIAN_POINT('Ctrl Pts',(24.3012815425194,53.8278562137149,2.82049442739556));
#217824=CARTESIAN_POINT('Ctrl Pts',(24.3105307527829,53.8370583385401,2.84000929088409));
#217825=CARTESIAN_POINT('Ctrl Pts',(24.318064299217,53.847201296772,2.85976644340634));
#217826=CARTESIAN_POINT('Ctrl Pts',(24.3233168218273,53.8542731477143,2.87354148166297));
#217827=CARTESIAN_POINT('Ctrl Pts',(24.3277344576489,53.8618028047949,2.88743438345181));
#217828=CARTESIAN_POINT('Ctrl Pts',(24.3312692531087,53.8697418420148,2.90134173516062));
#217829=CARTESIAN_POINT('',(24.4761921430391,54.1952354911874,3.4715307213911));
#217830=CARTESIAN_POINT('',(24.3312692531087,53.8697418420147,2.90134173516061));
#217831=CARTESIAN_POINT('',(29.4581217525673,51.656815567543,3.47153072139109));
#217832=CARTESIAN_POINT('Origin',(5.53234440788222E-15,1.85015204418142E-13,
3.47153072139072));
#217833=CARTESIAN_POINT('',(29.2799753962461,51.3482501200168,2.90134173516058));
#217834=CARTESIAN_POINT('',(29.4581217525673,51.656815567543,3.47153072139109));
#217835=CARTESIAN_POINT('',(29.4472515437734,51.0345602039889,2.59908173516059));
#217836=CARTESIAN_POINT('Ctrl Pts',(29.2799753962461,51.3482501200168,2.90134173516059));
#217837=CARTESIAN_POINT('Ctrl Pts',(29.2738605406109,51.337658593052,2.88176998919915));
#217838=CARTESIAN_POINT('Ctrl Pts',(29.2694377663943,51.3261534914787,2.86226752356906));
#217839=CARTESIAN_POINT('Ctrl Pts',(29.2667250421043,51.3139160033725,2.84310370500273));
#217840=CARTESIAN_POINT('Ctrl Pts',(29.2639633161072,51.3014574615418,2.8235937178899));
#217841=CARTESIAN_POINT('Ctrl Pts',(29.2629734853273,51.2882390496599,2.80443322637407));
#217842=CARTESIAN_POINT('Ctrl Pts',(29.2638161685324,51.274418803047,2.78589323878736));
#217843=CARTESIAN_POINT('Ctrl Pts',(29.2646231747155,51.2611836698432,2.76813818620555));
#217844=CARTESIAN_POINT('Ctrl Pts',(29.2671107576654,51.2473957191241,2.75095095199344));
#217845=CARTESIAN_POINT('Ctrl Pts',(29.2713733056804,51.2331761176688,2.73457771435808));
#217846=CARTESIAN_POINT('Ctrl Pts',(29.274763596202,51.2218663142685,2.72155497956031));
#217847=CARTESIAN_POINT('Ctrl Pts',(29.2792774508348,51.2102829897298,2.70904711160195));
#217848=CARTESIAN_POINT('Ctrl Pts',(29.2849828273429,51.1984837018593,2.69718956158373));
#217849=CARTESIAN_POINT('Ctrl Pts',(29.2849984011674,51.1984514936362,2.69715719432391));
#217850=CARTESIAN_POINT('Ctrl Pts',(29.2850139839325,51.1984192839705,2.69712483219057));
#217851=CARTESIAN_POINT('Ctrl Pts',(29.2850295756385,51.1983870728641,2.69709247518685));
#217852=CARTESIAN_POINT('Ctrl Pts',(29.2881333895826,51.1919748636255,2.69065122242311));
#217853=CARTESIAN_POINT('Ctrl Pts',(29.2916260110607,51.1854935419304,2.68442464469461));
#217854=CARTESIAN_POINT('Ctrl Pts',(29.2954867606378,51.178977941168,2.67844505923613));
#217855=CARTESIAN_POINT('Ctrl Pts',(29.3031486855379,51.1660472802372,2.66657815779602));
#217856=CARTESIAN_POINT('Ctrl Pts',(29.3122618143336,51.1529811529981,2.65568445664209));
#217857=CARTESIAN_POINT('Ctrl Pts',(29.3226724463013,51.1400491105587,2.6460190622955));
#217858=CARTESIAN_POINT('Ctrl Pts',(29.330480420277,51.1303500787291,2.63877001653556));
#217859=CARTESIAN_POINT('Ctrl Pts',(29.3390182393876,51.1207264688923,2.63221189387636));
#217860=CARTESIAN_POINT('Ctrl Pts',(29.3482210667398,51.1112920078094,2.62645231033268));
#217861=CARTESIAN_POINT('Ctrl Pts',(29.3516721269969,51.1077540849033,2.6242924665038));
#217862=CARTESIAN_POINT('Ctrl Pts',(29.3552167041325,51.1042427612075,2.6222449171178));
#217863=CARTESIAN_POINT('Ctrl Pts',(29.3588513794159,51.1007640347391,2.62031533672632));
#217864=CARTESIAN_POINT('Ctrl Pts',(29.3715727429078,51.0885884920995,2.61356180535613));
#217865=CARTESIAN_POINT('Ctrl Pts',(29.3853978061641,51.0768122610999,2.60825339735383));
#217866=CARTESIAN_POINT('Ctrl Pts',(29.4001800143157,51.0656925470315,2.60463337987646));
#217867=CARTESIAN_POINT('Ctrl Pts',(29.4075711183915,51.0601326899973,2.60282337113778));
#217868=CARTESIAN_POINT('Ctrl Pts',(29.4152015092025,51.054736963077,2.60143545939149));
#217869=CARTESIAN_POINT('Ctrl Pts',(29.4230528695803,51.0495375206697,2.60050005034631));
#217870=CARTESIAN_POINT('Ctrl Pts',(29.4269785497693,51.046937799466,2.60003234582371));
#217871=CARTESIAN_POINT('Ctrl Pts',(29.430959472363,51.0443871494125,2.59967776696101));
#217872=CARTESIAN_POINT('Ctrl Pts',(29.4349933478627,51.0418895900603,2.59944011429195));
#217873=CARTESIAN_POINT('Ctrl Pts',(29.4390272233624,51.0393920307081,2.59920246162289));
#217874=CARTESIAN_POINT('Ctrl Pts',(29.4431140526175,51.0369475635292,2.59908173791351));
#217875=CARTESIAN_POINT('Ctrl Pts',(29.4472515437734,51.0345602039889,2.59908173516059));
#217876=CARTESIAN_POINT('',(29.4735998357337,51.019348010533,2.59908173516059));
#217877=CARTESIAN_POINT('Origin',(5.68926707005281E-15,1.85913781171312E-13,
2.59908173516024));
#217878=CARTESIAN_POINT('',(29.8289013456884,51.0313275753411,2.90134173516059));
#217879=CARTESIAN_POINT('Ctrl Pts',(29.4735998357337,51.019348010533,2.59908173516059));
#217880=CARTESIAN_POINT('Ctrl Pts',(29.4768987365664,51.0174422596393,2.59908174371551));
#217881=CARTESIAN_POINT('Ctrl Pts',(29.4802121391118,51.0155824228874,2.59915764355925));
#217882=CARTESIAN_POINT('Ctrl Pts',(29.4835378249322,51.0137685205957,2.59930765775312));
#217883=CARTESIAN_POINT('Ctrl Pts',(29.5031724225188,51.0030593786377,2.60019333020924));
#217884=CARTESIAN_POINT('Ctrl Pts',(29.5232366506524,50.9939485772814,2.60365973324187));
#217885=CARTESIAN_POINT('Ctrl Pts',(29.543268395784,50.9864440924292,2.60934177082577));
#217886=CARTESIAN_POINT('Ctrl Pts',(29.5507515889356,50.9836406667026,2.6114643909198));
#217887=CARTESIAN_POINT('Ctrl Pts',(29.5582304387678,50.9810610352786,2.61389584429407));
#217888=CARTESIAN_POINT('Ctrl Pts',(29.5656816597958,50.9787043892803,2.61661604385287));
#217889=CARTESIAN_POINT('Ctrl Pts',(29.571495476234,50.9768656158507,2.6187384800081));
#217890=CARTESIAN_POINT('Ctrl Pts',(29.5772921977456,50.9751630202464,2.62103707099821));
#217891=CARTESIAN_POINT('Ctrl Pts',(29.5830604807848,50.9735966395565,2.62350262767686));
#217892=CARTESIAN_POINT('Ctrl Pts',(29.6032494714218,50.968114307142,2.63213207605213));
#217893=CARTESIAN_POINT('Ctrl Pts',(29.6230900862367,50.9643005997169,2.64280685971949));
#217894=CARTESIAN_POINT('Ctrl Pts',(29.6420960169785,50.9621571865008,2.65513293646119));
#217895=CARTESIAN_POINT('Ctrl Pts',(29.6515989823495,50.9610854798928,2.66129597483204));
#217896=CARTESIAN_POINT('Ctrl Pts',(29.6608932776209,50.9604313483969,2.66787183533886));
#217897=CARTESIAN_POINT('Ctrl Pts',(29.6699181168562,50.9601950050772,2.67481125953896));
#217898=CARTESIAN_POINT('Ctrl Pts',(29.6789043977155,50.9599596715279,2.68172103524114));
#217899=CARTESIAN_POINT('Ctrl Pts',(29.6876236029356,50.9601383261076,2.68899101329823));
#217900=CARTESIAN_POINT('Ctrl Pts',(29.6960154736015,50.9607318934966,2.69657334701309));
#217901=CARTESIAN_POINT('Ctrl Pts',(29.6960514814794,50.9607344403783,2.69660588132607));
#217902=CARTESIAN_POINT('Ctrl Pts',(29.6960874835161,50.9607369943871,2.69663842081415));
#217903=CARTESIAN_POINT('Ctrl Pts',(29.69612347971,50.9607395555214,2.69667096547416));
#217904=CARTESIAN_POINT('Ctrl Pts',(29.7130985928877,50.9619473372424,2.71201840157874));
#217905=CARTESIAN_POINT('Ctrl Pts',(29.7287537227754,50.9647087325283,2.72845645939168));
#217906=CARTESIAN_POINT('Ctrl Pts',(29.7430502978459,50.9688330949316,2.74568723186593));
#217907=CARTESIAN_POINT('Ctrl Pts',(29.7578669541872,50.9731074935238,2.76354482593901));
#217908=CARTESIAN_POINT('Ctrl Pts',(29.7712250678558,50.9788464019624,2.78225519316582));
#217909=CARTESIAN_POINT('Ctrl Pts',(29.7830467300279,50.9858763526664,2.80151223084835));
#217910=CARTESIAN_POINT('Ctrl Pts',(29.7946996705556,50.9928059702003,2.82049442739468));
#217911=CARTESIAN_POINT('Ctrl Pts',(29.8048600966444,51.0009908790876,2.84000929088337));
#217912=CARTESIAN_POINT('Ctrl Pts',(29.81341260136,51.0102908031014,2.85976644340578));
#217913=CARTESIAN_POINT('Ctrl Pts',(29.8193755598134,51.0167748755875,2.87354148166258));
#217914=CARTESIAN_POINT('Ctrl Pts',(29.8245560588475,51.0238015157352,2.8874343834516));
#217915=CARTESIAN_POINT('Ctrl Pts',(29.8289013456884,51.0313275753411,2.90134173516059));
#217916=CARTESIAN_POINT('',(30.0070536838157,51.3398895692699,3.47153072139108));
#217917=CARTESIAN_POINT('',(29.8289013456884,51.0313275753411,2.90134173516059));
#217918=CARTESIAN_POINT('',(34.6963546279284,48.2946219293749,3.47153072139107));
#217919=CARTESIAN_POINT('Origin',(5.53234440788222E-15,1.85015204418142E-13,
3.47153072139072));
#217920=CARTESIAN_POINT('',(34.4869303039396,48.006368200519,2.90134173516058));
#217921=CARTESIAN_POINT('',(34.6963546279284,48.2946219293749,3.47153072139107));
#217922=CARTESIAN_POINT('',(34.6205005703634,47.6769115920306,2.59908173516057));
#217923=CARTESIAN_POINT('Ctrl Pts',(34.4869303039396,48.006368200519,2.90134173516058));
#217924=CARTESIAN_POINT('Ctrl Pts',(34.4797418300859,47.9964738715098,2.88176998919899));
#217925=CARTESIAN_POINT('Ctrl Pts',(34.4741406737019,47.9854941018789,2.86226752356877));
#217926=CARTESIAN_POINT('Ctrl Pts',(34.4701636441734,47.9736072089142,2.84310370500229));
#217927=CARTESIAN_POINT('Ctrl Pts',(34.466114774968,47.9615055952534,2.82359371788922));
#217928=CARTESIAN_POINT('Ctrl Pts',(34.4637486663039,47.948463060705,2.80443322637314));
#217929=CARTESIAN_POINT('Ctrl Pts',(34.4631421240619,47.9346304384684,2.7858932387862));
#217930=CARTESIAN_POINT('Ctrl Pts',(34.4625612612459,47.9213834535926,2.76813818620404));
#217931=CARTESIAN_POINT('Ctrl Pts',(34.463593983656,47.9074110114868,2.75095095199161));
#217932=CARTESIAN_POINT('Ctrl Pts',(34.4663468278988,47.8928237489021,2.73457771435597));
#217933=CARTESIAN_POINT('Ctrl Pts',(34.4685363496849,47.8812215199305,2.72155497955895));
#217934=CARTESIAN_POINT('Ctrl Pts',(34.4718146898361,47.8692298237681,2.70904711160129));
#217935=CARTESIAN_POINT('Ctrl Pts',(34.4762554502657,47.856898799393,2.69718956158372));
#217936=CARTESIAN_POINT('Ctrl Pts',(34.4762675720992,47.856865139702,2.69715719432389));
#217937=CARTESIAN_POINT('Ctrl Pts',(34.4762797026733,47.8568314776417,2.69712483219055));
#217938=CARTESIAN_POINT('Ctrl Pts',(34.4762918419889,47.856797813214,2.69709247518683));
#217939=CARTESIAN_POINT('Ctrl Pts',(34.4787083945376,47.8500962938267,2.69065122242308));
#217940=CARTESIAN_POINT('Ctrl Pts',(34.4815044004731,47.8432853991341,2.68442464469459));
#217941=CARTESIAN_POINT('Ctrl Pts',(34.4846629347251,47.836401933294,2.67844505923611));
#217942=CARTESIAN_POINT('Ctrl Pts',(34.4909312646828,47.8227412186413,2.66657815779599));
#217943=CARTESIAN_POINT('Ctrl Pts',(34.4986286886042,47.8087940876658,2.65568445664205));
#217944=CARTESIAN_POINT('Ctrl Pts',(34.5076305235176,47.7948446809468,2.64601906229547));
#217945=CARTESIAN_POINT('Ctrl Pts',(34.5143818997026,47.7843826259075,2.63877001653553));
#217946=CARTESIAN_POINT('Ctrl Pts',(34.5218670065994,47.7739192901009,2.63221189387634));
#217947=CARTESIAN_POINT('Ctrl Pts',(34.5300332501818,47.7635745545821,2.62645231033266));
#217948=CARTESIAN_POINT('Ctrl Pts',(34.5330955915252,47.7596952787626,2.62429246650378));
#217949=CARTESIAN_POINT('Ctrl Pts',(34.5362537178264,47.7558326812645,2.62224491711778));
#217950=CARTESIAN_POINT('Ctrl Pts',(34.5395048560464,47.7519930846018,2.6203153367263));
#217951=CARTESIAN_POINT('Ctrl Pts',(34.5508838398164,47.7385544962823,2.61356180535611));
#217952=CARTESIAN_POINT('Ctrl Pts',(34.5634022166002,47.7253976640915,2.60825339735381));
#217953=CARTESIAN_POINT('Ctrl Pts',(34.5769411196453,47.7127937034784,2.60463337987644));
#217954=CARTESIAN_POINT('Ctrl Pts',(34.5837105711679,47.7064917231719,2.60282337113776));
#217955=CARTESIAN_POINT('Ctrl Pts',(34.5907351548565,47.7003279615827,2.60143545939147));
#217956=CARTESIAN_POINT('Ctrl Pts',(34.598000014936,47.6943363116301,2.60050005034629));
#217957=CARTESIAN_POINT('Ctrl Pts',(34.6016324449757,47.6913404866537,2.60003234582369));
#217958=CARTESIAN_POINT('Ctrl Pts',(34.6053249441285,47.688387689607,2.59967776696099));
#217959=CARTESIAN_POINT('Ctrl Pts',(34.6090756555951,47.6854821573392,2.59944011429193));
#217960=CARTESIAN_POINT('Ctrl Pts',(34.6128263670618,47.6825766250714,2.59920246162287));
#217961=CARTESIAN_POINT('Ctrl Pts',(34.6166352918409,47.6797183589579,2.5990817379135));
#217962=CARTESIAN_POINT('Ctrl Pts',(34.6205005703634,47.6769115920306,2.59908173516058));
#217963=CARTESIAN_POINT('',(34.6451144164185,47.6590285860938,2.59908173516057));
#217964=CARTESIAN_POINT('Origin',(5.69524824702573E-15,1.85909896949569E-13,
2.59908173516024));
#217965=CARTESIAN_POINT('',(34.9997217530259,47.6338034047602,2.90134173516056));
#217966=CARTESIAN_POINT('Ctrl Pts',(34.6451144164185,47.6590285860938,2.59908173516057));
#217967=CARTESIAN_POINT('Ctrl Pts',(34.648196040315,47.6567884460683,2.59908174371547));
#217968=CARTESIAN_POINT('Ctrl Pts',(34.651296885817,47.6545924528205,2.59915764355924));
#217969=CARTESIAN_POINT('Ctrl Pts',(34.6544147487634,47.6524408584473,2.5993076577531));
#217970=CARTESIAN_POINT('Ctrl Pts',(34.672822375816,47.6397380079784,2.60019333020912));
#217971=CARTESIAN_POINT('Ctrl Pts',(34.6918243519411,47.6285798336129,2.603659733241));
#217972=CARTESIAN_POINT('Ctrl Pts',(34.7109619288054,47.6190225715796,2.60934177082367));
#217973=CARTESIAN_POINT('Ctrl Pts',(34.7181110904612,47.6154522966306,2.61146439091819));
#217974=CARTESIAN_POINT('Ctrl Pts',(34.7252793254653,47.6121050440163,2.61389584429317));
#217975=CARTESIAN_POINT('Ctrl Pts',(34.7324433913425,47.6089824432868,2.61661604385286));
#217976=CARTESIAN_POINT('Ctrl Pts',(34.7380331549252,47.6065460335524,2.61873848000809));
#217977=CARTESIAN_POINT('Ctrl Pts',(34.7436201516877,47.6042468425534,2.62103707099821));
#217978=CARTESIAN_POINT('Ctrl Pts',(34.7491931041024,47.6020860928991,2.62350262767686));
#217979=CARTESIAN_POINT('Ctrl Pts',(34.768698437554,47.594523469109,2.63213207605212));
#217980=CARTESIAN_POINT('Ctrl Pts',(34.7880317224284,47.5886567445953,2.64280685971947));
#217981=CARTESIAN_POINT('Ctrl Pts',(34.8067094890034,47.5845384124877,2.65513293646117));
#217982=CARTESIAN_POINT('Ctrl Pts',(34.8160483722909,47.5824792464338,2.66129597483202));
#217983=CARTESIAN_POINT('Ctrl Pts',(34.8252233770803,47.5808571799368,2.66787183533885));
#217984=CARTESIAN_POINT('Ctrl Pts',(34.8341740726979,47.5796787787541,2.67481125953894));
#217985=CARTESIAN_POINT('Ctrl Pts',(34.8430865267162,47.5785054122579,2.68172103524112));
#217986=CARTESIAN_POINT('Ctrl Pts',(34.8517766417065,47.5777716830265,2.68899101329822));
#217987=CARTESIAN_POINT('Ctrl Pts',(34.8601845855138,47.5774848094466,2.69657334701308));
#217988=CARTESIAN_POINT('Ctrl Pts',(34.8602206623585,47.5774835785281,2.69660588132605));
#217989=CARTESIAN_POINT('Ctrl Pts',(34.8602567341388,47.5774823553082,2.69663842081414));
#217990=CARTESIAN_POINT('Ctrl Pts',(34.8602928008533,47.5774811397855,2.69667096547414));
#217991=CARTESIAN_POINT('Ctrl Pts',(34.8773011701531,47.5769079226576,2.71201840157965));
#217992=CARTESIAN_POINT('Ctrl Pts',(34.8931591840079,47.5780177840619,2.72845645939364));
#217993=CARTESIAN_POINT('Ctrl Pts',(34.907808554209,47.5806251537546,2.74568723186902));
#217994=CARTESIAN_POINT('Ctrl Pts',(34.9229908396734,47.5833273744263,2.76354482594315));
#217995=CARTESIAN_POINT('Ctrl Pts',(34.9368756554781,47.5876385414306,2.78225519317108));
#217996=CARTESIAN_POINT('Ctrl Pts',(34.9493673872922,47.5933942811496,2.80151223085477));
#217997=CARTESIAN_POINT('Ctrl Pts',(34.9616808340646,47.5990678735481,2.82049442740203));
#217998=CARTESIAN_POINT('Ctrl Pts',(34.9726411562242,47.6061458909237,2.84000929089166));
#217999=CARTESIAN_POINT('Ctrl Pts',(34.9821189161897,47.6145008888064,2.85976644341498));
#218000=CARTESIAN_POINT('Ctrl Pts',(34.9887269790637,47.6203261419803,2.87354148166876));
#218001=CARTESIAN_POINT('Ctrl Pts',(34.9946135826771,47.6267727798537,2.88743438345469));
#218002=CARTESIAN_POINT('Ctrl Pts',(34.9997217530259,47.6338034047602,2.90134173516057));
#218003=CARTESIAN_POINT('',(35.2091516650527,47.922053073669,3.47153072139106));
#218004=CARTESIAN_POINT('',(34.9997217530259,47.6338034047602,2.90134173516056));
#218005=CARTESIAN_POINT('',(39.554446981307,44.4033023070492,3.47153072139104));
#218006=CARTESIAN_POINT('Origin',(5.53234440788222E-15,1.85015204418142E-13,
3.47153072139072));
#218007=CARTESIAN_POINT('',(39.3160391863689,44.1385184650378,2.90134173516055));
#218008=CARTESIAN_POINT('',(39.554446981307,44.4033023070492,3.47153072139104));
#218009=CARTESIAN_POINT('',(39.4144401478989,43.7969047596349,2.59908173516054));
#218010=CARTESIAN_POINT('Ctrl Pts',(39.3160391863689,44.1385184650378,2.90134173516055));
#218011=CARTESIAN_POINT('Ctrl Pts',(39.3078558527201,44.1294297383226,2.88176998919738));
#218012=CARTESIAN_POINT('Ctrl Pts',(39.30113768161,44.1190955972869,2.86226752356559));
#218013=CARTESIAN_POINT('Ctrl Pts',(39.2959399200105,44.1076895347495,2.84310370499762));
#218014=CARTESIAN_POINT('Ctrl Pts',(39.2906482678552,44.0960774370696,2.8235937178831));
#218015=CARTESIAN_POINT('Ctrl Pts',(39.2869318048885,44.0833536765915,2.80443322636566));
#218016=CARTESIAN_POINT('Ctrl Pts',(39.2848826826034,44.0696602318339,2.78589323877748));
#218017=CARTESIAN_POINT('Ctrl Pts',(39.2829203148429,44.0565465320237,2.76813818619431));
#218018=CARTESIAN_POINT('Ctrl Pts',(39.2824868619908,44.0425426835299,2.75095095198097));
#218019=CARTESIAN_POINT('Ctrl Pts',(39.2836998417244,44.0277475809163,2.73457771434461));
#218020=CARTESIAN_POINT('Ctrl Pts',(39.2846646059165,44.0159800428246,2.72155497955166));
#218021=CARTESIAN_POINT('Ctrl Pts',(39.2866715134052,44.0037113585737,2.70904711159781));
#218022=CARTESIAN_POINT('Ctrl Pts',(39.2897990038552,43.9909836989807,2.69718956158368));
#218023=CARTESIAN_POINT('Ctrl Pts',(39.2898075408882,43.9909489566043,2.69715719432385));
#218024=CARTESIAN_POINT('Ctrl Pts',(39.2898160863664,43.990914210958,2.69712483219051));
#218025=CARTESIAN_POINT('Ctrl Pts',(39.2898246402906,43.9908794620436,2.69709247518679));
#218026=CARTESIAN_POINT('Ctrl Pts',(39.2915274551884,43.9839620557564,2.69065122242305));
#218027=CARTESIAN_POINT('Ctrl Pts',(39.2935962119552,43.9768962096538,2.68442464469456));
#218028=CARTESIAN_POINT('Ctrl Pts',(39.2960179253199,43.9697202954283,2.67844505923608));
#218029=CARTESIAN_POINT('Ctrl Pts',(39.3008239832004,43.955479196702,2.66657815779597));
#218030=CARTESIAN_POINT('Ctrl Pts',(39.3070213676603,43.9408038696757,2.65568445664204));
#218031=CARTESIAN_POINT('Ctrl Pts',(39.3145157795323,43.9259899312962,2.64601906229545));
#218032=CARTESIAN_POINT('Ctrl Pts',(39.3201365884363,43.9148794775115,2.63877001653551));
#218033=CARTESIAN_POINT('Ctrl Pts',(39.3264869747219,43.903691054232,2.63221189387631));
#218034=CARTESIAN_POINT('Ctrl Pts',(39.3335271634607,43.8925493833644,2.62645231033263));
#218035=CARTESIAN_POINT('Ctrl Pts',(39.3361672342378,43.888371256789,2.62429246650375));
#218036=CARTESIAN_POINT('Ctrl Pts',(39.338904308612,43.8841997049151,2.62224491711776));
#218037=CARTESIAN_POINT('Ctrl Pts',(39.341736289618,43.8800413054827,2.62031533672627));
#218038=CARTESIAN_POINT('Ctrl Pts',(39.3516482231388,43.865486907469,2.61356180535609));
#218039=CARTESIAN_POINT('Ctrl Pts',(39.3627227594944,43.8510936230938,2.60825339735378));
#218040=CARTESIAN_POINT('Ctrl Pts',(39.374870022378,43.8371435075661,2.60463337987641));
#218041=CARTESIAN_POINT('Ctrl Pts',(39.3809436538198,43.8301684498023,2.60282337113772));
#218042=CARTESIAN_POINT('Ctrl Pts',(39.3872854675771,43.8233041850059,2.60143545939144));
#218043=CARTESIAN_POINT('Ctrl Pts',(39.393884232031,43.8165859732787,2.60050005034625));
#218044=CARTESIAN_POINT('Ctrl Pts',(39.3971836142579,43.8132268674151,2.60003234582366));
#218045=CARTESIAN_POINT('Ctrl Pts',(39.4005472341763,43.8099042748374,2.59967776696096));
#218046=CARTESIAN_POINT('Ctrl Pts',(39.4039736880302,43.8066226032737,2.5994401142919));
#218047=CARTESIAN_POINT('Ctrl Pts',(39.4074001418841,43.8033409317099,2.59920246162284));
#218048=CARTESIAN_POINT('Ctrl Pts',(39.4108894308102,43.8001001824233,2.59908173791343));
#218049=CARTESIAN_POINT('Ctrl Pts',(39.4144401478989,43.7969047596349,2.59908173516055));
#218050=CARTESIAN_POINT('',(39.4370498736007,43.7765468711725,2.59908173516054));
#218051=CARTESIAN_POINT('Origin',(5.70079064675565E-15,1.85905408802762E-13,
2.59908173516024));
#218052=CARTESIAN_POINT('',(39.7870778846746,43.7143933160626,2.90134173516054));
#218053=CARTESIAN_POINT('Ctrl Pts',(39.4370498736007,43.7765468711725,2.59908173516055));
#218054=CARTESIAN_POINT('Ctrl Pts',(39.4398804576448,43.7739968854582,2.59908174371544));
#218055=CARTESIAN_POINT('Ctrl Pts',(39.4427347725911,43.771488795476,2.59915764355922));
#218056=CARTESIAN_POINT('Ctrl Pts',(39.4456106527046,43.7690230823394,2.59930765775308));
#218057=CARTESIAN_POINT('Ctrl Pts',(39.4625896314097,43.7544656984479,2.600193330209));
#218058=CARTESIAN_POINT('Ctrl Pts',(39.4803211659001,43.7413824023669,2.6036597332402));
#218059=CARTESIAN_POINT('Ctrl Pts',(39.4983548992005,43.7298770745156,2.60934177082175));
#218060=CARTESIAN_POINT('Ctrl Pts',(39.5050917016488,43.7255790670235,2.61146439091671));
#218061=CARTESIAN_POINT('Ctrl Pts',(39.5118707851416,43.7215008664186,2.61389584429233));
#218062=CARTESIAN_POINT('Ctrl Pts',(39.5186692048627,43.7176465228246,2.61661604385282));
#218063=CARTESIAN_POINT('Ctrl Pts',(39.5239736729701,43.7146391706004,2.61873848000805));
#218064=CARTESIAN_POINT('Ctrl Pts',(39.5292897326779,43.7117685746244,2.62103707099818));
#218065=CARTESIAN_POINT('Ctrl Pts',(39.5346062960353,43.709037129631,2.62350262767683));
#218066=CARTESIAN_POINT('Ctrl Pts',(39.5532142677863,43.6994770721541,2.6321320760521));
#218067=CARTESIAN_POINT('Ctrl Pts',(39.5718284032055,43.6916216076132,2.64280685971944));
#218068=CARTESIAN_POINT('Ctrl Pts',(39.5899733680945,43.6855734779225,2.65513293646114));
#218069=CARTESIAN_POINT('Ctrl Pts',(39.599045850539,43.6825494130771,2.66129597483199));
#218070=CARTESIAN_POINT('Ctrl Pts',(39.6080010415738,43.6799771832789,2.66787183533882));
#218071=CARTESIAN_POINT('Ctrl Pts',(39.6167795278796,43.6778696350431,2.67481125953892));
#218072=CARTESIAN_POINT('Ctrl Pts',(39.6255205083456,43.6757710912488,2.6817210352411));
#218073=CARTESIAN_POINT('Ctrl Pts',(39.6340863223877,43.6741330170974,2.68899101329819));
#218074=CARTESIAN_POINT('Ctrl Pts',(39.6424182201447,43.6729688455955,2.69657334701305));
#218075=CARTESIAN_POINT('Ctrl Pts',(39.6424539706905,43.672963850363,2.69660588132602));
#218076=CARTESIAN_POINT('Ctrl Pts',(39.6424897170046,43.6729588633163,2.69663842081411));
#218077=CARTESIAN_POINT('Ctrl Pts',(39.6425254590851,43.6729538844541,2.69667096547411));
#218078=CARTESIAN_POINT('Ctrl Pts',(39.6593807372542,43.6706059487638,2.71201840158091));
#218079=CARTESIAN_POINT('Ctrl Pts',(39.6752678913581,43.6700521164126,2.72845645939637));
#218080=CARTESIAN_POINT('Ctrl Pts',(39.6901095551247,43.6711139265067,2.74568723187333));
#218081=CARTESIAN_POINT('Ctrl Pts',(39.7054911294161,43.6722143631628,2.76354482594909));
#218082=CARTESIAN_POINT('Ctrl Pts',(39.7197505224098,43.6750505546849,2.78225519317877));
#218083=CARTESIAN_POINT('Ctrl Pts',(39.7327754618385,43.6794690223303,2.80151223086424));
#218084=CARTESIAN_POINT('Ctrl Pts',(39.7456145061562,43.6838244285283,2.82049442741313));
#218085=CARTESIAN_POINT('Ctrl Pts',(39.7572546408038,43.6897180061528,2.84000929090442));
#218086=CARTESIAN_POINT('Ctrl Pts',(39.767553815698,43.6970365387998,2.85976644342937));
#218087=CARTESIAN_POINT('Ctrl Pts',(39.7747345836717,43.7021391499686,2.87354148167843));
#218088=CARTESIAN_POINT('Ctrl Pts',(39.7812627970021,43.7079351548539,2.88743438345951));
#218089=CARTESIAN_POINT('Ctrl Pts',(39.7870778846746,43.7143933160626,2.90134173516054));
#218090=CARTESIAN_POINT('',(40.0254908126588,43.9791725362585,3.47153072139104));
#218091=CARTESIAN_POINT('',(39.7870778846746,43.7143933160626,2.90134173516055));
#218092=CARTESIAN_POINT('',(43.9791725362582,40.0254908126591,3.47153072139101));
#218093=CARTESIAN_POINT('Origin',(5.53234440788222E-15,1.85015204418142E-13,
3.47153072139072));
#218094=CARTESIAN_POINT('',(43.7143933160623,39.787077884675,2.90134173516052));
#218095=CARTESIAN_POINT('',(43.9791725362582,40.0254908126591,3.47153072139101));
#218096=CARTESIAN_POINT('',(43.7765468711722,39.4370498736011,2.59908173516051));
#218097=CARTESIAN_POINT('Ctrl Pts',(43.7143933160623,39.787077884675,2.90134173516052));
#218098=CARTESIAN_POINT('Ctrl Pts',(43.7053047809347,39.7788943382461,2.88176998919692));
#218099=CARTESIAN_POINT('Ctrl Pts',(43.697543200787,39.7693190488182,2.8622675235647));
#218100=CARTESIAN_POINT('Ctrl Pts',(43.6911816548804,39.7585187839169,2.84310370499633));
#218101=CARTESIAN_POINT('Ctrl Pts',(43.6847051962234,39.7475234267907,2.8235937178814));
#218102=CARTESIAN_POINT('Ctrl Pts',(43.6796790972999,39.7352578445662,2.80443322636358));
#218103=CARTESIAN_POINT('Ctrl Pts',(43.6762098455837,39.7218536055349,2.78589323877506));
#218104=CARTESIAN_POINT('Ctrl Pts',(43.6728874729904,39.7090168672304,2.76813818619159));
#218105=CARTESIAN_POINT('Ctrl Pts',(43.6709925938755,39.6951350414441,2.75095095197799));
#218106=CARTESIAN_POINT('Ctrl Pts',(43.6706524194393,39.6802941970427,2.73457771434141));
#218107=CARTESIAN_POINT('Ctrl Pts',(43.6703818558792,39.6684902774383,2.72155497954961));
#218108=CARTESIAN_POINT('Ctrl Pts',(43.6710953426077,39.6560790233687,2.70904711159683));
#218109=CARTESIAN_POINT('Ctrl Pts',(43.6728752976394,39.6430941754571,2.69718956158366));
#218110=CARTESIAN_POINT('Ctrl Pts',(43.6728801563384,39.6430587310402,2.69715719432383));
#218111=CARTESIAN_POINT('Ctrl Pts',(43.6728850230946,39.6430232824885,2.69712483219048));
#218112=CARTESIAN_POINT('Ctrl Pts',(43.6728898979089,39.6429878298037,2.69709247518676));
#218113=CARTESIAN_POINT('Ctrl Pts',(43.6738603187595,39.6359303251674,2.69065122242302));
#218114=CARTESIAN_POINT('Ctrl Pts',(43.6751791606255,39.6286869425433,2.68442464469454));
#218115=CARTESIAN_POINT('Ctrl Pts',(43.6768375203044,39.6212972007503,2.67844505923606));
#218116=CARTESIAN_POINT('Ctrl Pts',(43.6801286499319,39.6066317464083,2.66657815779595));
#218117=CARTESIAN_POINT('Ctrl Pts',(43.6847580950893,39.5913890092851,2.65568445664201));
#218118=CARTESIAN_POINT('Ctrl Pts',(43.6906629735752,39.5758728438539,2.64601906229542));
#218119=CARTESIAN_POINT('Ctrl Pts',(43.6950916324396,39.5642357197805,2.63877001653548));
#218120=CARTESIAN_POINT('Ctrl Pts',(43.7002377219528,39.5524447917348,2.63221189387629));
#218121=CARTESIAN_POINT('Ctrl Pts',(43.7060747220671,39.540628255996,2.62645231033261));
#218122=CARTESIAN_POINT('Ctrl Pts',(43.70826359711,39.536197055094,2.62429246650373));
#218123=CARTESIAN_POINT('Ctrl Pts',(43.7105496315976,39.5317622532395,2.62224491711773));
#218124=CARTESIAN_POINT('Ctrl Pts',(43.7129314276129,39.5273306113317,2.62031533672625));
#218125=CARTESIAN_POINT('Ctrl Pts',(43.7212677136666,39.5118198646543,2.61356180535606));
#218126=CARTESIAN_POINT('Ctrl Pts',(43.7307770746562,39.4963478239302,2.60825339735375));
#218127=CARTESIAN_POINT('Ctrl Pts',(43.7413996094243,39.4812043938729,2.60463337987638));
#218128=CARTESIAN_POINT('Ctrl Pts',(43.7467108768083,39.4736326788442,2.6028233711377));
#218129=CARTESIAN_POINT('Ctrl Pts',(43.7523004383956,39.4661431171622,2.60143545939142));
#218130=CARTESIAN_POINT('Ctrl Pts',(43.7581608097796,39.4587719497939,2.60050005034623));
#218131=CARTESIAN_POINT('Ctrl Pts',(43.7610909954716,39.4550863661098,2.60003234582364));
#218132=CARTESIAN_POINT('Ctrl Pts',(43.764088883632,39.4514303810209,2.59967776696093));
#218133=CARTESIAN_POINT('Ctrl Pts',(43.7671535389276,39.4478085248415,2.59944011429187));
#218134=CARTESIAN_POINT('Ctrl Pts',(43.7702181942233,39.4441866686621,2.59920246162281));
#218135=CARTESIAN_POINT('Ctrl Pts',(43.7733496179168,39.4405989425298,2.59908173791339));
#218136=CARTESIAN_POINT('Ctrl Pts',(43.7765468711722,39.4370498736011,2.59908173516052));
#218137=CARTESIAN_POINT('',(43.7969047596346,39.4144401478992,2.59908173516051));
#218138=CARTESIAN_POINT('Origin',(5.7058335455513E-15,1.85900365903967E-13,
2.59908173516024));
#218139=CARTESIAN_POINT('',(44.1385184650375,39.3160391863693,2.90134173516051));
#218140=CARTESIAN_POINT('Ctrl Pts',(43.7969047596346,39.4144401478992,2.59908173516051));
#218141=CARTESIAN_POINT('Ctrl Pts',(43.799453291355,39.4116082546732,2.59908174371542));
#218142=CARTESIAN_POINT('Ctrl Pts',(43.8020298032738,39.4088155471154,2.59915764355919));
#218143=CARTESIAN_POINT('Ctrl Pts',(43.8046321918101,39.4060627300845,2.59930765775305));
#218144=CARTESIAN_POINT('Ctrl Pts',(43.8199964969283,39.3898103065108,2.6001933302091));
#218145=CARTESIAN_POINT('Ctrl Pts',(43.8362633193862,39.374945232041,2.60365973324122));
#218146=CARTESIAN_POINT('Ctrl Pts',(43.8529956277716,39.3616178931491,2.60934177082429));
#218147=CARTESIAN_POINT('Ctrl Pts',(43.8592462611905,39.3566392429866,2.61146439091865));
#218148=CARTESIAN_POINT('Ctrl Pts',(43.86556192011,39.3518747760135,2.6138958442934));
#218149=CARTESIAN_POINT('Ctrl Pts',(43.8719202087612,39.3473309185527,2.61661604385281));
#218150=CARTESIAN_POINT('Ctrl Pts',(43.8768812645308,39.3437855730189,2.61873848000804));
#218151=CARTESIAN_POINT('Ctrl Pts',(43.8818681433212,39.3403750229161,2.62103707099816));
#218152=CARTESIAN_POINT('Ctrl Pts',(43.8868700682407,39.3371028088665,2.6235026276768));
#218153=CARTESIAN_POINT('Ctrl Pts',(43.9043768054586,39.3256500596931,2.63213207605207));
#218154=CARTESIAN_POINT('Ctrl Pts',(43.9220678510596,39.3158919212386,2.64280685971942));
#218155=CARTESIAN_POINT('Ctrl Pts',(43.9394812142302,39.3079802585392,2.65513293646112));
#218156=CARTESIAN_POINT('Ctrl Pts',(43.9481878958155,39.3040244271895,2.66129597483196));
#218157=CARTESIAN_POINT('Ctrl Pts',(43.9568251581489,39.3005302159781,2.6678718353388));
#218158=CARTESIAN_POINT('Ctrl Pts',(43.9653352562098,39.2975166114287,2.67481125953889));
#218159=CARTESIAN_POINT('Ctrl Pts',(43.9738089951123,39.2945158824213,2.68172103524107));
#218160=CARTESIAN_POINT('Ctrl Pts',(43.982156659355,39.291991410433,2.68899101329814));
#218161=CARTESIAN_POINT('Ctrl Pts',(43.9903212250463,39.2899626959158,2.69657334701299));
#218162=CARTESIAN_POINT('Ctrl Pts',(43.9903562576029,39.2899539910981,2.69660588132597));
#218163=CARTESIAN_POINT('Ctrl Pts',(43.9903912868066,39.2899452948636,2.69663842081406));
#218164=CARTESIAN_POINT('Ctrl Pts',(43.9904263126554,39.2899366072115,2.69667096547406));
#218165=CARTESIAN_POINT('Ctrl Pts',(44.0069438297388,39.2858396774333,2.71201840158195));
#218166=CARTESIAN_POINT('Ctrl Pts',(44.0226860611066,39.2836282192295,2.72845645939866));
#218167=CARTESIAN_POINT('Ctrl Pts',(44.0375574100645,39.2831328363111,2.74568723187695));
#218168=CARTESIAN_POINT('Ctrl Pts',(44.0529697494363,39.282619432337,2.76354482595429));
#218169=CARTESIAN_POINT('Ctrl Pts',(44.0674474907255,39.283949574469,2.78225519318566));
#218170=CARTESIAN_POINT('Ctrl Pts',(44.0808629338068,39.2869823603845,2.80151223087286));
#218171=CARTESIAN_POINT('Ctrl Pts',(44.094086908414,39.28997186164,2.82049442742354));
#218172=CARTESIAN_POINT('Ctrl Pts',(44.1062793237989,39.2946164282438,2.84000929091666));
#218173=CARTESIAN_POINT('Ctrl Pts',(44.1172870737068,39.3008183122797,2.8597664434434));
#218174=CARTESIAN_POINT('Ctrl Pts',(44.1249618727833,39.3051423761684,2.87354148168786));
#218175=CARTESIAN_POINT('Ctrl Pts',(44.1320601713592,39.3102242458236,2.88743438346422));
#218176=CARTESIAN_POINT('Ctrl Pts',(44.1385184650375,39.3160391863692,2.90134173516051));
#218177=CARTESIAN_POINT('',(44.4033023070489,39.5544469813073,3.471530721391));
#218178=CARTESIAN_POINT('',(44.1385184650375,39.3160391863692,2.90134173516052));
#218179=CARTESIAN_POINT('',(47.9220530736687,35.209151665053,3.47153072139097));
#218180=CARTESIAN_POINT('Origin',(5.53234440788222E-15,1.85015204418142E-13,
3.47153072139072));
#218181=CARTESIAN_POINT('',(47.6338034047599,34.9997217530263,2.90134173516048));
#218182=CARTESIAN_POINT('',(47.9220530736687,35.209151665053,3.47153072139097));
#218183=CARTESIAN_POINT('',(47.6590285860935,34.6451144164188,2.59908173516048));
#218184=CARTESIAN_POINT('Ctrl Pts',(47.6338034047599,34.9997217530263,2.90134173516048));
#218185=CARTESIAN_POINT('Ctrl Pts',(47.6239092440469,34.992533047532,2.88176998919812));
#218186=CARTESIAN_POINT('Ctrl Pts',(47.6151892923585,34.9838215185875,2.86226752356711));
#218187=CARTESIAN_POINT('Ctrl Pts',(47.6077336605733,34.9737453812859,2.84310370499989));
#218188=CARTESIAN_POINT('Ctrl Pts',(47.6001433528511,34.9634872321481,2.82359371788591));
#218189=CARTESIAN_POINT('Ctrl Pts',(47.5938626849626,34.9518142124638,2.80443322636898));
#218190=CARTESIAN_POINT('Ctrl Pts',(47.5890113136631,34.9388460388079,2.78589323878128));
#218191=CARTESIAN_POINT('Ctrl Pts',(47.5843653368459,34.926426904001,2.76813818619804));
#218192=CARTESIAN_POINT('Ctrl Pts',(47.5810297921601,34.9128191931112,2.75095095198462));
#218193=CARTESIAN_POINT('Ctrl Pts',(47.5791401905759,34.8980952063199,2.73457771434816));
#218194=CARTESIAN_POINT('Ctrl Pts',(47.5776372636139,34.8863842314135,2.72155497955392));
#218195=CARTESIAN_POINT('Ctrl Pts',(47.5770495124721,34.873966387819,2.70904711159887));
#218196=CARTESIAN_POINT('Ctrl Pts',(47.5774624305259,34.8608666162964,2.69718956158364));
#218197=CARTESIAN_POINT('Ctrl Pts',(47.5774635576581,34.8608308581754,2.69715719432381));
#218198=CARTESIAN_POINT('Ctrl Pts',(47.577464692371,34.8607950951,2.69712483219046));
#218199=CARTESIAN_POINT('Ctrl Pts',(47.5774658346659,34.8607593270719,2.69709247518674));
#218200=CARTESIAN_POINT('Ctrl Pts',(47.5776932293355,34.8536390475842,2.690651222423));
#218201=CARTESIAN_POINT('Ctrl Pts',(47.5782477067931,34.8462974884545,2.6844246446945));
#218202=CARTESIAN_POINT('Ctrl Pts',(47.5791245434507,34.8387748826515,2.67844505923603));
#218203=CARTESIAN_POINT('Ctrl Pts',(47.5808646865202,34.8238457504805,2.66657815779591));
#218204=CARTESIAN_POINT('Ctrl Pts',(47.5838754712052,34.808202605878,2.65568445664198));
#218205=CARTESIAN_POINT('Ctrl Pts',(47.5881261212205,34.7921542117506,2.64601906229539));
#218206=CARTESIAN_POINT('Ctrl Pts',(47.591314108732,34.780117916155,2.63877001653545));
#218207=CARTESIAN_POINT('Ctrl Pts',(47.5951995198393,34.7678536672182,2.63221189387625));
#218208=CARTESIAN_POINT('Ctrl Pts',(47.5997693799344,34.7554917310466,2.62645231033257));
#218209=CARTESIAN_POINT('Ctrl Pts',(47.60148307747,34.7508560049822,2.62429246650369));
#218210=CARTESIAN_POINT('Ctrl Pts',(47.6032930257987,34.7462065417644,2.62224491711769));
#218211=CARTESIAN_POINT('Ctrl Pts',(47.6051985413679,34.7415502113773,2.62031533672621));
#218212=CARTESIAN_POINT('Ctrl Pts',(47.6118678458601,34.7252530550225,2.61356180535602));
#218213=CARTESIAN_POINT('Ctrl Pts',(47.6197078449347,34.7088717728655,2.60825339735371));
#218214=CARTESIAN_POINT('Ctrl Pts',(47.6286892688733,34.6927009428672,2.60463337987634));
#218215=CARTESIAN_POINT('Ctrl Pts',(47.6331799808426,34.6846155278681,2.60282337113766));
#218216=CARTESIAN_POINT('Ctrl Pts',(47.6379560498536,34.6765827265055,2.60143545939139));
#218217=CARTESIAN_POINT('Ctrl Pts',(47.6430138207125,34.6686393635484,2.6005000503462));
#218218=CARTESIAN_POINT('Ctrl Pts',(47.6455427061419,34.6646676820698,2.6000323458236));
#218219=CARTESIAN_POINT('Ctrl Pts',(47.6481420170542,34.6607183602073,2.59967776696091));
#218220=CARTESIAN_POINT('Ctrl Pts',(47.6508112967868,34.6567960012265,2.59944011429185));
#218221=CARTESIAN_POINT('Ctrl Pts',(47.6534805765195,34.6528736422458,2.59920246162279));
#218222=CARTESIAN_POINT('Ctrl Pts',(47.6562198264472,34.6489782471461,2.59908173791339));
#218223=CARTESIAN_POINT('Ctrl Pts',(47.6590285860935,34.6451144164188,2.59908173516049));
#218224=CARTESIAN_POINT('',(47.6769115920304,34.6205005703637,2.59908173516048));
#218225=CARTESIAN_POINT('Origin',(5.71032169235817E-15,1.85894823504237E-13,
2.59908173516024));
#218226=CARTESIAN_POINT('',(48.0063682005187,34.4869303039399,2.90134173516047));
#218227=CARTESIAN_POINT('Ctrl Pts',(47.6769115920304,34.6205005703637,2.59908173516048));
#218228=CARTESIAN_POINT('Ctrl Pts',(47.6791501491803,34.6174177964407,2.59908174371533));
#218229=CARTESIAN_POINT('Ctrl Pts',(47.6814206292678,34.6143710687957,2.59915764355915));
#218230=CARTESIAN_POINT('Ctrl Pts',(47.6837210139136,34.61136130831,2.59930765775302));
#218231=CARTESIAN_POINT('Ctrl Pts',(47.6973023109003,34.5935919100098,2.60019333020907));
#218232=CARTESIAN_POINT('Ctrl Pts',(47.7119261986122,34.5771079220194,2.60365973324124));
#218233=CARTESIAN_POINT('Ctrl Pts',(47.7271737594079,34.5621045892019,2.60934177082439));
#218234=CARTESIAN_POINT('Ctrl Pts',(47.7328697405521,34.5564998435003,2.61146439091872));
#218235=CARTESIAN_POINT('Ctrl Pts',(47.7386527792201,34.5511013106546,2.61389584429343));
#218236=CARTESIAN_POINT('Ctrl Pts',(47.744501274063,34.5459177227788,2.61661604385277));
#218237=CARTESIAN_POINT('Ctrl Pts',(47.7490645631296,34.541873227483,2.618738480008));
#218238=CARTESIAN_POINT('Ctrl Pts',(47.7536676237151,34.537960089954,2.62103707099811));
#218239=CARTESIAN_POINT('Ctrl Pts',(47.7583001080603,34.5341829579102,2.62350262767675));
#218240=CARTESIAN_POINT('Ctrl Pts',(47.7745138032687,34.5209629957568,2.63213207605202));
#218241=CARTESIAN_POINT('Ctrl Pts',(47.7910879322539,34.5094090955955,2.64280685971938));
#218242=CARTESIAN_POINT('Ctrl Pts',(47.8075789092551,34.4997205817196,2.65513293646107));
#218243=CARTESIAN_POINT('Ctrl Pts',(47.8158243977558,34.4948763247817,2.66129597483192));
#218244=CARTESIAN_POINT('Ctrl Pts',(47.8240490997342,34.4904984154664,2.66787183533875));
#218245=CARTESIAN_POINT('Ctrl Pts',(47.8321975711351,34.4866117722855,2.67481125953884));
#218246=CARTESIAN_POINT('Ctrl Pts',(47.8403112284174,34.4827417346799,2.68172103524103));
#218247=CARTESIAN_POINT('Ctrl Pts',(47.8483492841045,34.4793585234982,2.68899101329811));
#218248=CARTESIAN_POINT('Ctrl Pts',(47.8562570650397,34.4764874929865,2.69657334701297));
#218249=CARTESIAN_POINT('Ctrl Pts',(47.8562909957831,34.4764751739553,2.69660588132594));
#218250=CARTESIAN_POINT('Ctrl Pts',(47.8563249240891,34.4764628638109,2.69663842081403));
#218251=CARTESIAN_POINT('Ctrl Pts',(47.8563588499558,34.4764505625524,2.69667096547403));
#218252=CARTESIAN_POINT('Ctrl Pts',(47.8723576365775,34.4706495255069,2.71201840158102));
#218253=CARTESIAN_POINT('Ctrl Pts',(47.8877824700263,34.4668046706493,2.72845645939671));
#218254=CARTESIAN_POINT('Ctrl Pts',(47.9025205705626,34.4647575222371,2.7456872318739));
#218255=CARTESIAN_POINT('Ctrl Pts',(47.9177948141974,34.4626359025937,2.76354482595019));
#218256=CARTESIAN_POINT('Ctrl Pts',(47.9323322826173,34.4624454220191,2.78225519318044));
#218257=CARTESIAN_POINT('Ctrl Pts',(47.9459912469484,34.4640592983662,2.80151223086651));
#218258=CARTESIAN_POINT('Ctrl Pts',(47.9594552672108,34.4656501410767,2.82049442741633));
#218259=CARTESIAN_POINT('Ctrl Pts',(47.972066380678,34.4689948098143,2.84000929090859));
#218260=CARTESIAN_POINT('Ctrl Pts',(47.9836621023876,34.474012096098,2.8597664434345));
#218261=CARTESIAN_POINT('Ctrl Pts',(47.9917468458671,34.4775102373592,2.87354148168186));
#218262=CARTESIAN_POINT('Ctrl Pts',(47.9993374592481,34.4818222937595,2.88743438346119));
#218263=CARTESIAN_POINT('Ctrl Pts',(48.0063682005187,34.4869303039399,2.90134173516047));
#218264=CARTESIAN_POINT('',(48.2946219293746,34.6963546279288,3.47153072139097));
#218265=CARTESIAN_POINT('',(48.0063682005187,34.4869303039399,2.90134173516048));
#218266=CARTESIAN_POINT('',(51.3398895692697,30.007053683816,3.47153072139094));
#218267=CARTESIAN_POINT('Origin',(5.53234440788222E-15,1.85015204418142E-13,
3.47153072139072));
#218268=CARTESIAN_POINT('',(51.0313275753408,29.8289013456888,2.90134173516045));
#218269=CARTESIAN_POINT('',(51.3398895692697,30.007053683816,3.47153072139094));
#218270=CARTESIAN_POINT('',(51.0193480105327,29.473599835734,2.59908173516044));
#218271=CARTESIAN_POINT('Ctrl Pts',(51.0313275753408,29.8289013456888,2.90134173516045));
#218272=CARTESIAN_POINT('Ctrl Pts',(51.0207361915367,29.8227862420893,2.88176998919671));
#218273=CARTESIAN_POINT('Ctrl Pts',(51.0111534059222,29.8150339189608,2.86226752356434));
#218274=CARTESIAN_POINT('Ctrl Pts',(51.0026853737198,29.8057923055259,2.84310370499583));
#218275=CARTESIAN_POINT('Ctrl Pts',(50.9940643779319,29.7963837548036,2.82359371788082));
#218276=CARTESIAN_POINT('Ctrl Pts',(50.9865979533897,29.7854311897043,2.80443322636292));
#218277=CARTESIAN_POINT('Ctrl Pts',(50.980417615146,29.7730411634463,2.78589323877433));
#218278=CARTESIAN_POINT('Ctrl Pts',(50.9744989363996,29.7611756987759,2.76813818619093));
#218279=CARTESIAN_POINT('Ctrl Pts',(50.9697592710689,29.74799119171,2.75095095197738));
#218280=CARTESIAN_POINT('Ctrl Pts',(50.9663409452077,29.7335453816081,2.73457771434086));
#218281=CARTESIAN_POINT('Ctrl Pts',(50.9636221212274,29.7220556592952,2.72155497954923));
#218282=CARTESIAN_POINT('Ctrl Pts',(50.9617395717402,29.709767278673,2.70904711159661));
#218283=CARTESIAN_POINT('Ctrl Pts',(50.9607809287995,29.6966961073823,2.69718956158359));
#218284=CARTESIAN_POINT('Ctrl Pts',(50.9607783120157,29.6966604273306,2.69715719432376));
#218285=CARTESIAN_POINT('Ctrl Pts',(50.9607757022532,29.6966247415593,2.69712483219041));
#218286=CARTESIAN_POINT('Ctrl Pts',(50.9607730995135,29.6965890500699,2.69709247518669));
#218287=CARTESIAN_POINT('Ctrl Pts',(50.9602549766184,29.6894840070028,2.69065122242295));
#218288=CARTESIAN_POINT('Ctrl Pts',(50.9600390146967,29.6821247070257,2.68442464469445));
#218289=CARTESIAN_POINT('Ctrl Pts',(50.960124721527,29.674551656456,2.67844505923598));
#218290=CARTESIAN_POINT('Ctrl Pts',(50.960294812667,29.6595224131521,2.66657815779586));
#218291=CARTESIAN_POINT('Ctrl Pts',(50.9616539500924,29.6436502506362,2.65568445664193));
#218292=CARTESIAN_POINT('Ctrl Pts',(50.9642038006262,29.627245457377,2.64601906229534));
#218293=CARTESIAN_POINT('Ctrl Pts',(50.9661161885265,29.6149418624326,2.6387700165354));
#218294=CARTESIAN_POINT('Ctrl Pts',(50.9686983518507,29.6023386622825,2.63221189387621));
#218295=CARTESIAN_POINT('Ctrl Pts',(50.9719510035829,29.5895667656375,2.62645231033253));
#218296=CARTESIAN_POINT('Ctrl Pts',(50.9731707479825,29.5847773043957,2.62429246650365));
#218297=CARTESIAN_POINT('Ctrl Pts',(50.9744847799798,29.5799641203064,2.62224491711765));
#218298=CARTESIAN_POINT('Ctrl Pts',(50.9758931378754,29.5751341171702,2.62031533672617));
#218299=CARTESIAN_POINT('Ctrl Pts',(50.9808223905104,29.5582291061936,2.61356180535598));
#218300=CARTESIAN_POINT('Ctrl Pts',(50.9869071309995,29.5411180593589,2.60825339735368));
#218301=CARTESIAN_POINT('Ctrl Pts',(50.9941490417486,29.5240970004171,2.60463337987631));
#218302=CARTESIAN_POINT('Ctrl Pts',(50.9977699971231,29.5155864709462,2.60282337113763));
#218303=CARTESIAN_POINT('Ctrl Pts',(51.0016802459462,29.5070984389558,2.60143545939135));
#218304=CARTESIAN_POINT('Ctrl Pts',(51.005880002284,29.4986699095566,2.60050005034617));
#218305=CARTESIAN_POINT('Ctrl Pts',(51.0079798804529,29.4944556448571,2.60003234582357));
#218306=CARTESIAN_POINT('Ctrl Pts',(51.0101521355228,29.4902562558177,2.59967776696086));
#218307=CARTESIAN_POINT('Ctrl Pts',(51.0123967945051,29.4860763682213,2.5994401142918));
#218308=CARTESIAN_POINT('Ctrl Pts',(51.0146414534875,29.481896480625,2.59920246162274));
#218309=CARTESIAN_POINT('Ctrl Pts',(51.0169585178538,29.4777360953218,2.59908173791333));
#218310=CARTESIAN_POINT('Ctrl Pts',(51.0193480105327,29.473599835734,2.59908173516044));
#218311=CARTESIAN_POINT('',(51.0345602039887,29.4472515437738,2.59908173516044));
#218312=CARTESIAN_POINT('Origin',(5.71420591410065E-15,1.85888842327264E-13,
2.59908173516023));
#218313=CARTESIAN_POINT('',(51.3482501200165,29.2799753962465,2.90134173516044));
#218314=CARTESIAN_POINT('Ctrl Pts',(51.0345602039887,29.4472515437738,2.59908173516044));
#218315=CARTESIAN_POINT('Ctrl Pts',(51.0364642604675,29.4439516646701,2.59908174371532));
#218316=CARTESIAN_POINT('Ctrl Pts',(51.0384038328688,29.4406842975235,2.5991576435591));
#218317=CARTESIAN_POINT('Ctrl Pts',(51.0403770101285,29.4374505691487,2.59930765775297));
#218318=CARTESIAN_POINT('Ctrl Pts',(51.0520264994527,29.4183588813669,2.6001933302091));
#218319=CARTESIAN_POINT('Ctrl Pts',(51.0648472300456,29.4004365818765,2.60365973324178));
#218320=CARTESIAN_POINT('Ctrl Pts',(51.0784429877858,29.3839216347863,2.60934177082578));
#218321=CARTESIAN_POINT('Ctrl Pts',(51.0835219102931,29.3777522003137,2.61146439091977));
#218322=CARTESIAN_POINT('Ctrl Pts',(51.0887089685267,29.3717787490522,2.613895844294));
#218323=CARTESIAN_POINT('Ctrl Pts',(51.0939835922269,29.366012223236,2.61661604385274));
#218324=CARTESIAN_POINT('Ctrl Pts',(51.0980991182406,29.361512890515,2.61873848000797));
#218325=CARTESIAN_POINT('Ctrl Pts',(51.1022679285261,29.3571400387136,2.62103707099808));
#218326=CARTESIAN_POINT('Ctrl Pts',(51.1064802178293,29.3528993717246,2.62350262767673));
#218327=CARTESIAN_POINT('Ctrl Pts',(51.1212232303905,29.3380570372631,2.63213207605199));
#218328=CARTESIAN_POINT('Ctrl Pts',(51.1364988531343,29.3248339623429,2.64280685971935));
#218329=CARTESIAN_POINT('Ctrl Pts',(51.1518867653713,29.3134747466761,2.65513293646105));
#218330=CARTESIAN_POINT('Ctrl Pts',(51.1595807214898,29.3077951388427,2.66129597483189));
#218331=CARTESIAN_POINT('Ctrl Pts',(51.1673027515571,29.3025814967141,2.66787183533873));
#218332=CARTESIAN_POINT('Ctrl Pts',(51.1750003199401,29.2978643977776,2.67481125953882));
#218333=CARTESIAN_POINT('Ctrl Pts',(51.1826650006752,29.2931674525158,2.681721035241));
#218334=CARTESIAN_POINT('Ctrl Pts',(51.1903053811865,29.2889625693103,2.68899101329808));
#218335=CARTESIAN_POINT('Ctrl Pts',(51.1978697380629,29.2852806784151,2.69657334701294));
#218336=CARTESIAN_POINT('Ctrl Pts',(51.1979021952408,29.2852648801404,2.69660588132591));
#218337=CARTESIAN_POINT('Ctrl Pts',(51.1979346509235,29.2852490909586,2.696638420814));
#218338=CARTESIAN_POINT('Ctrl Pts',(51.1979671051091,29.285233310869,2.69667096547401));
#218339=CARTESIAN_POINT('Ctrl Pts',(51.2132718752135,29.2777917239328,2.71201840157856));
#218340=CARTESIAN_POINT('Ctrl Pts',(51.2282103130388,29.2723555974563,2.72845645939148));
#218341=CARTESIAN_POINT('Ctrl Pts',(51.2426536914386,29.2687791125366,2.7456872318657));
#218342=CARTESIAN_POINT('Ctrl Pts',(51.2576224915253,29.2650725221328,2.76354482593858));
#218343=CARTESIAN_POINT('Ctrl Pts',(51.2720604115281,29.2633635057962,2.78225519316517));
#218344=CARTESIAN_POINT('Ctrl Pts',(51.285813246636,29.2635407906071,2.80151223084747));
#218345=CARTESIAN_POINT('Ctrl Pts',(51.2993697979284,29.263715545166,2.82049442739328));
#218346=CARTESIAN_POINT('Ctrl Pts',(51.3122614394779,29.2657236711455,2.84000929088141));
#218347=CARTESIAN_POINT('Ctrl Pts',(51.3243180878342,29.2695013892367,2.85976644340326));
#218348=CARTESIAN_POINT('Ctrl Pts',(51.3327241975802,29.2721352815031,2.87354148166084));
#218349=CARTESIAN_POINT('Ctrl Pts',(51.3407239614222,29.2756302808574,2.88743438345066));
#218350=CARTESIAN_POINT('Ctrl Pts',(51.3482501200165,29.2799753962465,2.90134173516044));
#218351=CARTESIAN_POINT('',(51.6568155675427,29.4581217525676,3.47153072139093));
#218352=CARTESIAN_POINT('',(51.3482501200165,29.2799753962465,2.90134173516044));
#218353=CARTESIAN_POINT('',(54.1952354911872,24.4761921430395,3.4715307213909));
#218354=CARTESIAN_POINT('Origin',(5.53234440788222E-15,1.85015204418142E-13,
3.47153072139072));
#218355=CARTESIAN_POINT('',(53.8697418420145,24.3312692531091,2.90134173516041));
#218356=CARTESIAN_POINT('',(54.1952354911872,24.4761921430394,3.4715307213909));
#218357=CARTESIAN_POINT('',(53.8206887816836,23.9791663275016,2.5990817351604));
#218358=CARTESIAN_POINT('Ctrl Pts',(53.8697418420145,24.3312692531091,2.90134173516041));
#218359=CARTESIAN_POINT('Ctrl Pts',(53.8585692765374,24.3262947497599,2.88176998919737));
#218360=CARTESIAN_POINT('Ctrl Pts',(53.8482286480022,24.3195865685231,2.86226752356569));
#218361=CARTESIAN_POINT('Ctrl Pts',(53.838840992916,24.311280732007,2.84310370499783));
#218362=CARTESIAN_POINT('Ctrl Pts',(53.8292837624968,24.3028248617519,2.82359371788356));
#218363=CARTESIAN_POINT('Ctrl Pts',(53.820713385011,24.2927127498343,2.80443322636636));
#218364=CARTESIAN_POINT('Ctrl Pts',(53.8132717929024,24.2810366186963,2.78589323877841));
#218365=CARTESIAN_POINT('Ctrl Pts',(53.8061452585096,24.2698548246775,2.76813818619556));
#218366=CARTESIAN_POINT('Ctrl Pts',(53.800053401299,24.2572379736549,2.75095095198253));
#218367=CARTESIAN_POINT('Ctrl Pts',(53.7951438030538,24.2432286115624,2.73457771434643));
#218368=CARTESIAN_POINT('Ctrl Pts',(53.7912388700582,24.2320860256417,2.72155497955279));
#218369=CARTESIAN_POINT('Ctrl Pts',(53.788082147831,24.2200617420577,2.70904711159829));
#218370=CARTESIAN_POINT('Ctrl Pts',(53.7857624469883,24.2071623814825,2.69718956158356));
#218371=CARTESIAN_POINT('Ctrl Pts',(53.7857561149585,24.2071271704182,2.69715719432374));
#218372=CARTESIAN_POINT('Ctrl Pts',(53.7857497893137,24.2070919529318,2.69712483219039));
#218373=CARTESIAN_POINT('Ctrl Pts',(53.7857434700555,24.2070567290244,2.69709247518667));
#218374=CARTESIAN_POINT('Ctrl Pts',(53.7844855062586,24.2000447667167,2.69065122242293));
#218375=CARTESIAN_POINT('Ctrl Pts',(53.7835014710816,24.1927483559227,2.68442464469441));
#218376=CARTESIAN_POINT('Ctrl Pts',(53.7827951090625,24.1852078325131,2.67844505923594));
#218377=CARTESIAN_POINT('Ctrl Pts',(53.7813932847188,24.1702431416111,2.66657815779583));
#218378=CARTESIAN_POINT('Ctrl Pts',(53.7810858838907,24.1543158599158,2.6556844566419));
#218379=CARTESIAN_POINT('Ctrl Pts',(53.7819069982469,24.1377344018726,2.64601906229531));
#218380=CARTESIAN_POINT('Ctrl Pts',(53.782522834014,24.1252983083403,2.63877001653537));
#218381=CARTESIAN_POINT('Ctrl Pts',(53.7837734588334,24.1124942402751,2.63221189387617));
#218382=CARTESIAN_POINT('Ctrl Pts',(53.7856732654698,24.0994523147292,2.62645231033249));
#218383=CARTESIAN_POINT('Ctrl Pts',(53.7863856929584,24.0945615926495,2.62429246650361));
#218384=CARTESIAN_POINT('Ctrl Pts',(53.7871894118146,24.089637421941,2.62224491711761));
#218385=CARTESIAN_POINT('Ctrl Pts',(53.788085181773,24.0846866645808,2.62031533672613));
#218386=CARTESIAN_POINT('Ctrl Pts',(53.7912203766273,24.06735901382,2.61356180535594));
#218387=CARTESIAN_POINT('Ctrl Pts',(53.7954831928409,24.0497056745176,2.60825339735364));
#218388=CARTESIAN_POINT('Ctrl Pts',(53.8009062465108,24.0320208729158,2.60463337987627));
#218389=CARTESIAN_POINT('Ctrl Pts',(53.8036177733457,24.023178472115,2.60282337113758));
#218390=CARTESIAN_POINT('Ctrl Pts',(53.8066193604764,24.0143282061515,2.60143545939131));
#218391=CARTESIAN_POINT('Ctrl Pts',(53.8099150888839,24.0055068550422,2.60050005034612));
#218392=CARTESIAN_POINT('Ctrl Pts',(53.8115629530876,24.0010961794876,2.60003234582353));
#218393=CARTESIAN_POINT('Ctrl Pts',(53.813284352634,23.9966927326565,2.59967776696082));
#218394=CARTESIAN_POINT('Ctrl Pts',(53.8150797979125,23.9923011121677,2.59944011429176));
#218395=CARTESIAN_POINT('Ctrl Pts',(53.816875243191,23.987909491679,2.5992024616227));
#218396=CARTESIAN_POINT('Ctrl Pts',(53.818744735754,23.9835296982243,2.59908173791327));
#218397=CARTESIAN_POINT('Ctrl Pts',(53.8206887816836,23.9791663275016,2.59908173516041));
#218398=CARTESIAN_POINT('',(53.8330634946837,23.9513722670367,2.5990817351604));
#218399=CARTESIAN_POINT('Origin',(5.71744365443249E-15,1.85882487904075E-13,
2.59908173516024));
#218400=CARTESIAN_POINT('',(54.1275498658873,23.752222950883,2.9013417351604));
#218401=CARTESIAN_POINT('Ctrl Pts',(53.8330634946837,23.9513722670367,2.59908173516041));
#218402=CARTESIAN_POINT('Ctrl Pts',(53.8346121892503,23.9478914369184,2.59908174371528));
#218403=CARTESIAN_POINT('Ctrl Pts',(53.8361996036043,23.9444392282283,2.59915764355907));
#218404=CARTESIAN_POINT('Ctrl Pts',(53.8378239549348,23.9410169613692,2.59930765775294));
#218405=CARTESIAN_POINT('Ctrl Pts',(53.8474140023518,23.9208121566354,2.600193330209));
#218406=CARTESIAN_POINT('Ctrl Pts',(53.8582911092161,23.9016479061115,2.60365973324117));
#218407=CARTESIAN_POINT('Ctrl Pts',(53.8700861059314,23.8838022859672,2.60934177082432));
#218408=CARTESIAN_POINT('Ctrl Pts',(53.874492324066,23.8771357563359,2.61146439091865));
#218409=CARTESIAN_POINT('Ctrl Pts',(53.8790265713722,23.8706528330379,2.61389584429335));
#218410=CARTESIAN_POINT('Ctrl Pts',(53.8836695340509,23.8643665485424,2.61661604385269));
#218411=CARTESIAN_POINT('Ctrl Pts',(53.8872922064474,23.8594616740271,2.61873848000792));
#218412=CARTESIAN_POINT('Ctrl Pts',(53.8909810920751,23.8546770178326,2.62103707099804));
#218413=CARTESIAN_POINT('Ctrl Pts',(53.8947270356132,23.8500192775333,2.62350262767669));
#218414=CARTESIAN_POINT('Ctrl Pts',(53.9078378379965,23.8337171864861,2.63213207605195));
#218415=CARTESIAN_POINT('Ctrl Pts',(53.9216475915795,23.818969811583,2.6428068597193));
#218416=CARTESIAN_POINT('Ctrl Pts',(53.9357638458656,23.806064348069,2.655132936461));
#218417=CARTESIAN_POINT('Ctrl Pts',(53.9428219730086,23.7996116163121,2.66129597483185));
#218418=CARTESIAN_POINT('Ctrl Pts',(53.9499567269876,23.7936193631243,2.66787183533868));
#218419=CARTESIAN_POINT('Ctrl Pts',(53.9571190561826,23.7881234899554,2.67481125953877));
#218420=CARTESIAN_POINT('Ctrl Pts',(53.9642507845244,23.7826510977526,2.68172103524096));
#218421=CARTESIAN_POINT('Ctrl Pts',(53.9714097802521,23.7776706121036,2.68899101329806));
#218422=CARTESIAN_POINT('Ctrl Pts',(53.9785478363929,23.773218200392,2.69657334701291));
#218423=CARTESIAN_POINT('Ctrl Pts',(53.9785784643976,23.773199095963,2.69660588132589));
#218424=CARTESIAN_POINT('Ctrl Pts',(53.9786090918658,23.7731800007334,2.69663842081398));
#218425=CARTESIAN_POINT('Ctrl Pts',(53.9786397187954,23.7731609147026,2.69667096547398));
#218426=CARTESIAN_POINT('Ctrl Pts',(53.9930827901208,23.7641603094588,2.71201840157812));
#218427=CARTESIAN_POINT('Ctrl Pts',(54.0073711636735,23.7571924707026,2.72845645939056));
#218428=CARTESIAN_POINT('Ctrl Pts',(54.0213615752623,23.7521258339931,2.74568723186427));
#218429=CARTESIAN_POINT('Ctrl Pts',(54.0358609304966,23.7468748830093,2.76354482593661));
#218430=CARTESIAN_POINT('Ctrl Pts',(54.0500411172113,23.7436660552523,2.78225519316262));
#218431=CARTESIAN_POINT('Ctrl Pts',(54.0637371441579,23.7424048061589,2.80151223084434));
#218432=CARTESIAN_POINT('Ctrl Pts',(54.0772376980691,23.74116155792,2.82049442738965));
#218433=CARTESIAN_POINT('Ctrl Pts',(54.0902686241798,23.7418111396949,2.84000929087727));
#218434=CARTESIAN_POINT('Ctrl Pts',(54.1026541040215,23.7443079001259,2.85976644339863));
#218435=CARTESIAN_POINT('Ctrl Pts',(54.1112894809308,23.746048685921,2.87354148165772));
#218436=CARTESIAN_POINT('Ctrl Pts',(54.1196107481421,23.7486883362824,2.88743438344908));
#218437=CARTESIAN_POINT('Ctrl Pts',(54.1275498658873,23.752222950883,2.9013417351604));
#218438=CARTESIAN_POINT('',(54.4530463244692,23.8971395307771,3.47153072139089));
#218439=CARTESIAN_POINT('',(54.1275498658873,23.752222950883,2.9013417351604));
#218440=CARTESIAN_POINT('',(56.4568070719811,18.6771643191712,3.47153072139086));
#218441=CARTESIAN_POINT('Origin',(5.53234440788222E-15,1.85015204418142E-13,
3.47153072139072));
#218442=CARTESIAN_POINT('',(56.1179479440988,18.5670586829468,2.90134173516037));
#218443=CARTESIAN_POINT('',(56.4568070719811,18.6771643191712,3.47153072139086));
#218444=CARTESIAN_POINT('',(56.0323588238391,18.2220120550219,2.59908173516037));
#218445=CARTESIAN_POINT('Ctrl Pts',(56.1179479440988,18.5670586829468,2.90134173516037));
#218446=CARTESIAN_POINT('Ctrl Pts',(56.1063166059132,18.5632792815473,2.88176998919632));
#218447=CARTESIAN_POINT('Ctrl Pts',(56.0953314285466,18.5576887384388,2.86226752356364));
#218448=CARTESIAN_POINT('Ctrl Pts',(56.0851270036896,18.5504096793235,2.84310370499483));
#218449=CARTESIAN_POINT('Ctrl Pts',(56.0747382496548,18.5429991338186,2.82359371787964));
#218450=CARTESIAN_POINT('Ctrl Pts',(56.0651578180741,18.5338382654957,2.80443322636156));
#218451=CARTESIAN_POINT('Ctrl Pts',(56.0565365037408,18.5230039556123,2.78589323877282));
#218452=CARTESIAN_POINT('Ctrl Pts',(56.0482801935035,18.5126283423189,2.76813818618936));
#218453=CARTESIAN_POINT('Ctrl Pts',(56.0409028880753,18.5007173801981,2.75095095197577));
#218454=CARTESIAN_POINT('Ctrl Pts',(56.0345558080321,18.4872979556158,2.73457771433922));
#218455=CARTESIAN_POINT('Ctrl Pts',(56.0295075492861,18.4766245865935,2.72155497954816));
#218456=CARTESIAN_POINT('Ctrl Pts',(56.0251112400296,18.4649961406184,2.70904711159607));
#218457=CARTESIAN_POINT('Ctrl Pts',(56.0214558964134,18.4524099188568,2.69718956158351));
#218458=CARTESIAN_POINT('Ctrl Pts',(56.0214459185126,18.4523755625597,2.69715719432368));
#218459=CARTESIAN_POINT('Ctrl Pts',(56.0214359462907,18.4523411992083,2.69712483219034));
#218460=CARTESIAN_POINT('Ctrl Pts',(56.0214259797492,18.4523068288036,2.69709247518662));
#218461=CARTESIAN_POINT('Ctrl Pts',(56.019441957565,18.4454647717816,2.69065122242288));
#218462=CARTESIAN_POINT('Ctrl Pts',(56.017700630428,18.4383111911741,2.68442464469438));
#218463=CARTESIAN_POINT('Ctrl Pts',(56.0162099386098,18.4308858104772,2.67844505923591));
#218464=CARTESIAN_POINT('Ctrl Pts',(56.0132515574632,18.4161496282621,2.66657815779579));
#218465=CARTESIAN_POINT('Ctrl Pts',(56.0112809863294,18.4003417300186,2.65568445664185));
#218466=CARTESIAN_POINT('Ctrl Pts',(56.0103643682072,18.3837652771157,2.64601906229527));
#218467=CARTESIAN_POINT('Ctrl Pts',(56.0096769046155,18.3713329374386,2.63877001653533));
#218468=CARTESIAN_POINT('Ctrl Pts',(56.0095822888229,18.3584682855075,2.63221189387613));
#218469=CARTESIAN_POINT('Ctrl Pts',(56.0101084356844,18.3452992211262,2.62645231033245));
#218470=CARTESIAN_POINT('Ctrl Pts',(56.0103057407575,18.3403608219831,2.62429246650357));
#218471=CARTESIAN_POINT('Ctrl Pts',(56.0105903407606,18.3353796149,2.62224491711757));
#218472=CARTESIAN_POINT('Ctrl Pts',(56.0109637085386,18.3303623448494,2.62031533672609));
#218473=CARTESIAN_POINT('Ctrl Pts',(56.0122704957614,18.3128018996724,2.6135618053559));
#218474=CARTESIAN_POINT('Ctrl Pts',(56.0146646833929,18.2947996815818,2.60825339735361));
#218475=CARTESIAN_POINT('Ctrl Pts',(56.0182094638727,18.2766448957073,2.60463337987624));
#218476=CARTESIAN_POINT('Ctrl Pts',(56.0199818541126,18.2675675027701,2.60282337113756));
#218477=CARTESIAN_POINT('Ctrl Pts',(56.0220418935343,18.2584519681994,2.60143545939127));
#218478=CARTESIAN_POINT('Ctrl Pts',(56.0243974853213,18.2493344439487,2.60050005034609));
#218479=CARTESIAN_POINT('Ctrl Pts',(56.0255752812149,18.2447756818233,2.6000323458235));
#218480=CARTESIAN_POINT('Ctrl Pts',(56.0268269652241,18.2402164222855,2.59967776696078));
#218481=CARTESIAN_POINT('Ctrl Pts',(56.0281535255245,18.2356611844174,2.59944011429172));
#218482=CARTESIAN_POINT('Ctrl Pts',(56.029480085825,18.2311059465494,2.59920246162266));
#218483=CARTESIAN_POINT('Ctrl Pts',(56.0308815240328,18.2265547308768,2.59908173791323));
#218484=CARTESIAN_POINT('Ctrl Pts',(56.0323588238391,18.2220120550219,2.59908173516037));
#218485=CARTESIAN_POINT('',(56.0417604764383,18.1930767435952,2.59908173516037));
#218486=CARTESIAN_POINT('Origin',(5.71999943999309E-15,1.85875829855059E-13,
2.59908173516024));
#218487=CARTESIAN_POINT('',(56.3138168485095,17.9642361803975,2.90134173516037));
#218488=CARTESIAN_POINT('Ctrl Pts',(56.0417604764383,18.1930767435951,2.59908173516037));
#218489=CARTESIAN_POINT('Ctrl Pts',(56.0429368412708,18.1894530991653,2.59908174371526));
#218490=CARTESIAN_POINT('Ctrl Pts',(56.0441547055336,18.1858538720526,2.59915764355904));
#218491=CARTESIAN_POINT('Ctrl Pts',(56.0454124342019,18.1822805617811,2.5993076577529));
#218492=CARTESIAN_POINT('Ctrl Pts',(56.0528379691459,18.1611840081634,2.60019333020892));
#218493=CARTESIAN_POINT('Ctrl Pts',(56.0616522804234,18.1409877741446,2.60365973324084));
#218494=CARTESIAN_POINT('Ctrl Pts',(56.0715172876624,18.1220070012944,2.60934177082357));
#218495=CARTESIAN_POINT('Ctrl Pts',(56.0752025259757,18.1149164163987,2.61146439091806));
#218496=CARTESIAN_POINT('Ctrl Pts',(56.0790342841913,18.107995049329,2.61389584429301));
#218497=CARTESIAN_POINT('Ctrl Pts',(56.0829947165771,18.1012578800032,2.61661604385265));
#218498=CARTESIAN_POINT('Ctrl Pts',(56.0860848445996,18.0960012025252,2.61873848000788));
#218499=CARTESIAN_POINT('Ctrl Pts',(56.0892533893666,18.090857163632,2.621037070998));
#218500=CARTESIAN_POINT('Ctrl Pts',(56.0924919457982,18.0858333812,2.62350262767665));
#218501=CARTESIAN_POINT('Ctrl Pts',(56.103826893309,18.0682501426879,2.63213207605191));
#218502=CARTESIAN_POINT('Ctrl Pts',(56.1160194751811,18.0521400431274,2.64280685971927));
#218503=CARTESIAN_POINT('Ctrl Pts',(56.1287094108803,18.0378297267253,2.65513293646097));
#218504=CARTESIAN_POINT('Ctrl Pts',(56.13505437873,18.0306745685242,2.66129597483182));
#218505=CARTESIAN_POINT('Ctrl Pts',(56.1415236867628,18.0239693566572,2.66787183533864));
#218506=CARTESIAN_POINT('Ctrl Pts',(56.1480723047925,18.0177549231924,2.67481125953873));
#218507=CARTESIAN_POINT('Ctrl Pts',(56.1545929440329,18.0115670407226,2.68172103524091));
#218508=CARTESIAN_POINT('Ctrl Pts',(56.1611921195217,18.0058655198732,2.68899101329801));
#218509=CARTESIAN_POINT('Ctrl Pts',(56.1678256688901,18.0006913688997,2.69657334701286));
#218510=CARTESIAN_POINT('Ctrl Pts',(56.1678541321547,18.0006691676285,2.69660588132584));
#218511=CARTESIAN_POINT('Ctrl Pts',(56.1678825958474,18.0006469755623,2.69663842081393));
#218512=CARTESIAN_POINT('Ctrl Pts',(56.1679110599661,18.000624792701,2.69667096547393));
#218513=CARTESIAN_POINT('Ctrl Pts',(56.1813341912022,17.990163781663,2.71201840157953));
#218514=CARTESIAN_POINT('Ctrl Pts',(56.1948159540733,17.9817405717259,2.72845645939364));
#218515=CARTESIAN_POINT('Ctrl Pts',(56.2082001169757,17.9752392943583,2.74568723186914));
#218516=CARTESIAN_POINT('Ctrl Pts',(56.2220711693892,17.9685015133122,2.76354482594343));
#218517=CARTESIAN_POINT('Ctrl Pts',(56.2358382617244,17.9638280307234,2.78225519317152));
#218518=CARTESIAN_POINT('Ctrl Pts',(56.2493274239741,17.9611420662354,2.80151223085537));
#218519=CARTESIAN_POINT('Ctrl Pts',(56.2626240656117,17.9584944364873,2.82049442740277));
#218520=CARTESIAN_POINT('Ctrl Pts',(56.2756515067316,17.9577783571049,2.84000929089254));
#218521=CARTESIAN_POINT('Ctrl Pts',(56.2882301201508,17.9589668048475,2.859766443416));
#218522=CARTESIAN_POINT('Ctrl Pts',(56.297000153222,17.9597954117583,2.87354148166938));
#218523=CARTESIAN_POINT('Ctrl Pts',(56.3055517542529,17.9615507925644,2.8874343834549));
#218524=CARTESIAN_POINT('Ctrl Pts',(56.3138168485095,17.9642361803975,2.90134173516036));
#218525=CARTESIAN_POINT('',(56.6526781108323,18.0743352474894,3.47153072139086));
#218526=CARTESIAN_POINT('',(56.3138168485095,17.9642361803975,2.90134173516037));
#218527=CARTESIAN_POINT('',(58.099826060148,12.6735055745743,3.47153072139082));
#218528=CARTESIAN_POINT('Origin',(5.53234440788222E-15,1.85015204418142E-13,
3.47153072139072));
#218529=CARTESIAN_POINT('',(57.751314065072,12.5994235324474,2.90134173516033));
#218530=CARTESIAN_POINT('',(58.099826060148,12.6735055745743,3.47153072139082));
#218531=CARTESIAN_POINT('',(57.6301266171957,12.2652136052663,2.59908173516032));
#218532=CARTESIAN_POINT('Ctrl Pts',(57.751314065072,12.5994235324474,2.90134173516032));
#218533=CARTESIAN_POINT('Ctrl Pts',(57.739351389555,12.596880640911,2.88176998919846));
#218534=CARTESIAN_POINT('Ctrl Pts',(57.7278420192606,12.5924689870922,2.86226752356795));
#218535=CARTESIAN_POINT('Ctrl Pts',(57.7169326264483,12.5862964562743,2.8431037050012));
#218536=CARTESIAN_POINT('Ctrl Pts',(57.7058261701626,12.5800124270087,2.82359371788796));
#218537=CARTESIAN_POINT('Ctrl Pts',(57.6953406497014,12.5719031706729,2.80443322637173));
#218538=CARTESIAN_POINT('Ctrl Pts',(57.685634070068,12.562029385013,2.78589323878465));
#218539=CARTESIAN_POINT('Ctrl Pts',(57.6763384418496,12.5525736298376,2.76813818620248));
#218540=CARTESIAN_POINT('Ctrl Pts',(57.6677565155063,12.5414990556149,2.75095095199004));
#218541=CARTESIAN_POINT('Ctrl Pts',(57.6600414936023,12.5288165945697,2.73457771435441));
#218542=CARTESIAN_POINT('Ctrl Pts',(57.6539052188813,12.5187293821054,2.72155497955787));
#218543=CARTESIAN_POINT('Ctrl Pts',(57.6483174894765,12.5076241774207,2.70904711160065));
#218544=CARTESIAN_POINT('Ctrl Pts',(57.643366551794,12.495488991745,2.69718956158348));
#218545=CARTESIAN_POINT('Ctrl Pts',(57.6433530373424,12.49545586663,2.69715719432365));
#218546=CARTESIAN_POINT('Ctrl Pts',(57.643339527801,12.4954227339057,2.69712483219031));
#218547=CARTESIAN_POINT('Ctrl Pts',(57.6433260231716,12.4953895935729,2.69709247518659));
#218548=CARTESIAN_POINT('Ctrl Pts',(57.6406376799625,12.4887924048451,2.69065122242284));
#218549=CARTESIAN_POINT('Ctrl Pts',(57.63815813921,12.4818600305504,2.68442464469433));
#218550=CARTESIAN_POINT('Ctrl Pts',(57.6358994499241,12.4746311465908,2.67844505923586));
#218551=CARTESIAN_POINT('Ctrl Pts',(57.6314169246176,12.4602849257588,2.66657815779574));
#218552=CARTESIAN_POINT('Ctrl Pts',(57.6278047731677,12.4447696056082,2.65568445664181));
#218553=CARTESIAN_POINT('Ctrl Pts',(57.6251604652272,12.4283797729325,2.64601906229522));
#218554=CARTESIAN_POINT('Ctrl Pts',(57.6231772342717,12.4160873984258,2.63877001653528));
#218555=CARTESIAN_POINT('Ctrl Pts',(57.6217384144975,12.4033031104474,2.63221189387609));
#218556=CARTESIAN_POINT('Ctrl Pts',(57.620885137009,12.3901511902558,2.62645231033241));
#218557=CARTESIAN_POINT('Ctrl Pts',(57.6205651579508,12.3852192201839,2.62429246650353));
#218558=CARTESIAN_POINT('Ctrl Pts',(57.6203275209637,12.3802355518734,2.62224491711753));
#218559=CARTESIAN_POINT('Ctrl Pts',(57.6201743958657,12.375206739393,2.62031533672604));
#218560=CARTESIAN_POINT('Ctrl Pts',(57.6196384580227,12.3576058957119,2.61356180535586));
#218561=CARTESIAN_POINT('Ctrl Pts',(57.6201377858514,12.3394520349016,2.60825339735356));
#218562=CARTESIAN_POINT('Ctrl Pts',(57.6217654557845,12.3210261723876,2.60463337987619));
#218563=CARTESIAN_POINT('Ctrl Pts',(57.622579290751,12.3118132411305,2.6028233711375));
#218564=CARTESIAN_POINT('Ctrl Pts',(57.6236752122407,12.302532309657,2.60143545939122));
#218565=CARTESIAN_POINT('Ctrl Pts',(57.6250648590507,12.2932185057685,2.60050005034604));
#218566=CARTESIAN_POINT('Ctrl Pts',(57.6257596824557,12.2885616038243,2.60003234582344));
#218567=CARTESIAN_POINT('Ctrl Pts',(57.6265279372158,12.2838964837812,2.59967776696074));
#218568=CARTESIAN_POINT('Ctrl Pts',(57.627371078466,12.2792275366732,2.59944011429168));
#218569=CARTESIAN_POINT('Ctrl Pts',(57.6282142197161,12.2745585895652,2.59920246162262));
#218570=CARTESIAN_POINT('Ctrl Pts',(57.6291322491186,12.2698858157461,2.5990817379132));
#218571=CARTESIAN_POINT('Ctrl Pts',(57.6301266171957,12.2652136052663,2.59908173516033));
#218572=CARTESIAN_POINT('',(57.6364522029207,12.2354540642047,2.59908173516032));
#218573=CARTESIAN_POINT('Origin',(5.72184526906101E-15,1.85868941127195E-13,
2.59908173516024));
#218574=CARTESIAN_POINT('',(57.8830978693156,11.9794294790614,2.90134173516032));
#218575=CARTESIAN_POINT('Ctrl Pts',(57.6364522029207,12.2354540642047,2.59908173516033));
#218576=CARTESIAN_POINT('Ctrl Pts',(57.6372433495199,12.2317273068699,2.59908174371527));
#218577=CARTESIAN_POINT('Ctrl Pts',(57.6380783205158,12.2280204952201,2.59915764355899));
#218578=CARTESIAN_POINT('Ctrl Pts',(57.6389556465834,12.2243352914713,2.59930765775286));
#218579=CARTESIAN_POINT('Ctrl Pts',(57.6441353133405,12.2025781272235,2.60019333020894));
#218580=CARTESIAN_POINT('Ctrl Pts',(57.6507902575933,12.1815711838737,2.6036597332413));
#218581=CARTESIAN_POINT('Ctrl Pts',(57.6586171922735,12.1616632156351,2.60934177082476));
#218582=CARTESIAN_POINT('Ctrl Pts',(57.6615410745225,12.1542262614092,2.61146439091896));
#218583=CARTESIAN_POINT('Ctrl Pts',(57.6646283621015,12.146942282516,2.61389584429349));
#218584=CARTESIAN_POINT('Ctrl Pts',(57.6678628728673,12.1398280421989,2.6166160438526));
#218585=CARTESIAN_POINT('Ctrl Pts',(57.6703866004265,12.1342771550166,2.61873848000783));
#218586=CARTESIAN_POINT('Ctrl Pts',(57.6730000890932,12.1288300925915,2.62103707099796));
#218587=CARTESIAN_POINT('Ctrl Pts',(57.6756957761165,12.1234953096383,2.62350262767661));
#218588=CARTESIAN_POINT('Ctrl Pts',(57.6851306806979,12.104823569302,2.63213207605187));
#218589=CARTESIAN_POINT('Ctrl Pts',(57.6955725063806,12.0875272507062,2.64280685971922));
#218590=CARTESIAN_POINT('Ctrl Pts',(57.7066970899019,12.071968868237,2.65513293646092));
#218591=CARTESIAN_POINT('Ctrl Pts',(57.7122593816626,12.0641896770024,2.66129597483177));
#218592=CARTESIAN_POINT('Ctrl Pts',(57.7179923646568,12.0568449701605,2.6678718353386));
#218593=CARTESIAN_POINT('Ctrl Pts',(57.7238555234916,12.0499800630333,2.67481125953869));
#218594=CARTESIAN_POINT('Ctrl Pts',(57.7296936321425,12.0431444860318,2.68172103524088));
#218595=CARTESIAN_POINT('Ctrl Pts',(57.7356606854448,12.0367843970375,2.68899101329797));
#218596=CARTESIAN_POINT('Ctrl Pts',(57.7417170494857,12.0309451958829,2.69657334701283));
#218597=CARTESIAN_POINT('Ctrl Pts',(57.7417430361608,12.0309201410113,2.6966058813258));
#218598=CARTESIAN_POINT('Ctrl Pts',(57.7417690242238,12.0308950952495,2.69663842081389));
#218599=CARTESIAN_POINT('Ctrl Pts',(57.7417950136727,12.0308700585976,2.69667096547389));
#218600=CARTESIAN_POINT('Ctrl Pts',(57.7540511381823,12.0190632547933,2.71201840157817));
#218601=CARTESIAN_POINT('Ctrl Pts',(57.7665785813542,12.0092769601272,2.72845645939077));
#218602=CARTESIAN_POINT('Ctrl Pts',(57.7792098558781,12.0014122714574,2.74568723186465));
#218603=CARTESIAN_POINT('Ctrl Pts',(57.7923006313156,11.9932614808885,2.76354482593735));
#218604=CARTESIAN_POINT('Ctrl Pts',(57.8055037941242,11.9871745471209,2.78225519316374));
#218605=CARTESIAN_POINT('Ctrl Pts',(57.8186383015904,11.9830932952263,2.80151223084585));
#218606=CARTESIAN_POINT('Ctrl Pts',(57.8315853501642,11.9790702919537,2.82049442739185));
#218607=CARTESIAN_POINT('Ctrl Pts',(57.8444665749203,11.9769963969278,2.84000929088019));
#218608=CARTESIAN_POINT('Ctrl Pts',(57.8571005079945,11.9768635110977,2.85976644340226));
#218609=CARTESIAN_POINT('Ctrl Pts',(57.865909110917,11.9767708607326,2.87354148166013));
#218610=CARTESIAN_POINT('Ctrl Pts',(57.8745973526438,11.9776227396647,2.88743438345024));
#218611=CARTESIAN_POINT('Ctrl Pts',(57.8830978693156,11.9794294790614,2.90134173516032));
#218612=CARTESIAN_POINT('',(58.2316113004781,12.0535047649324,3.47153072139081));
#218613=CARTESIAN_POINT('',(57.8830978693156,11.9794294790614,2.90134173516032));
#218614=CARTESIAN_POINT('',(59.1062911958296,6.53099325080074,3.47153072139077));
#218615=CARTESIAN_POINT('Origin',(5.53234440788222E-15,1.85015204418142E-13,
3.47153072139072));
#218616=CARTESIAN_POINT('',(58.7519447039088,6.49374646112759,2.90134173516028));
#218617=CARTESIAN_POINT('',(59.1062911958296,6.53099325080074,3.47153072139077));
#218618=CARTESIAN_POINT('',(58.5964866834551,6.17403490859039,2.59908173516028));
#218619=CARTESIAN_POINT('Ctrl Pts',(58.7519447039088,6.49374646112759,2.90134173516028));
#218620=CARTESIAN_POINT('Ctrl Pts',(58.7397817566352,6.49246793990547,2.88176998919804));
#218621=CARTESIAN_POINT('Ctrl Pts',(58.7278742924811,6.48928351037784,2.86226752356716));
#218622=CARTESIAN_POINT('Ctrl Pts',(58.7163794573031,6.48428513539526,2.84310370500006));
#218623=CARTESIAN_POINT('Ctrl Pts',(58.7046769834245,6.47919647150722,2.82359371788643));
#218624=CARTESIAN_POINT('Ctrl Pts',(58.6934012556383,6.47222767386629,2.80443322636984));
#218625=CARTESIAN_POINT('Ctrl Pts',(58.6827157580219,6.46342259168963,2.78589323878244));
#218626=CARTESIAN_POINT('Ctrl Pts',(58.6724826566698,6.45499029386298,2.76813818619996));
#218627=CARTESIAN_POINT('Ctrl Pts',(58.662790134792,6.44487344288875,2.75095095198725));
#218628=CARTESIAN_POINT('Ctrl Pts',(58.6537916984216,6.43306689707541,2.73457771435139));
#218629=CARTESIAN_POINT('Ctrl Pts',(58.6466346380387,6.42367635878376,2.72155497955592));
#218630=CARTESIAN_POINT('Ctrl Pts',(58.6399167088208,6.41321606634085,2.7090471115997));
#218631=CARTESIAN_POINT('Ctrl Pts',(58.6337244205833,6.40166487239056,2.69718956158343));
#218632=CARTESIAN_POINT('Ctrl Pts',(58.6337075176479,6.40163334138328,2.6971571943236));
#218633=CARTESIAN_POINT('Ctrl Pts',(58.6336906188004,6.40160180229503,2.69712483219026));
#218634=CARTESIAN_POINT('Ctrl Pts',(58.6336737240427,6.4015702551266,2.69709247518654));
#218635=CARTESIAN_POINT('Ctrl Pts',(58.6303105138594,6.39529021487339,2.69065122242279));
#218636=CARTESIAN_POINT('Ctrl Pts',(58.6271199258587,6.3886549994349,2.6844246446943));
#218637=CARTESIAN_POINT('Ctrl Pts',(58.6241179857776,6.38170181337803,2.67844505923582));
#218638=CARTESIAN_POINT('Ctrl Pts',(58.6181604277966,6.36790273412668,2.66657815779571));
#218639=CARTESIAN_POINT('Ctrl Pts',(58.6129462715178,6.3528499811634,2.65568445664178));
#218640=CARTESIAN_POINT('Ctrl Pts',(58.60860324535,6.33682633915144,2.6460190622952));
#218641=CARTESIAN_POINT('Ctrl Pts',(58.6053459757242,6.32480860764248,2.63877001653526));
#218642=CARTESIAN_POINT('Ctrl Pts',(58.6025787159788,6.31224475095124,2.63221189387606));
#218643=CARTESIAN_POINT('Ctrl Pts',(58.600355362827,6.29925407013909,2.62645231033238));
#218644=CARTESIAN_POINT('Ctrl Pts',(58.5995216053951,6.29438256483454,2.6242924665035));
#218645=CARTESIAN_POINT('Ctrl Pts',(58.5987643350184,6.28945103740957,2.6222449171175));
#218646=CARTESIAN_POINT('Ctrl Pts',(58.5980863947151,6.28446577922136,2.62031533672602));
#218647=CARTESIAN_POINT('Ctrl Pts',(58.5957136036535,6.26701737556262,2.61356180535583));
#218648=CARTESIAN_POINT('Ctrl Pts',(58.5943126009392,6.24891076953075,2.60825339735352));
#218649=CARTESIAN_POINT('Ctrl Pts',(58.5940053272331,6.23041570798264,2.60463337987615));
#218650=CARTESIAN_POINT('Ctrl Pts',(58.59385169038,6.22116817720859,2.60282337113747));
#218651=CARTESIAN_POINT('Ctrl Pts',(58.5939714867925,6.21182353265962,2.60143545939119));
#218652=CARTESIAN_POINT('Ctrl Pts',(58.5943799633642,6.20241549311782,2.600500050346));
#218653=CARTESIAN_POINT('Ctrl Pts',(58.5945842016501,6.19771147334691,2.60003234582341));
#218654=CARTESIAN_POINT('Ctrl Pts',(58.5948606100012,6.19299160483011,2.5996777669607));
#218655=CARTESIAN_POINT('Ctrl Pts',(58.5952110945691,6.18826010244367,2.59944011429164));
#218656=CARTESIAN_POINT('Ctrl Pts',(58.595561579137,6.18352860005724,2.59920246162258));
#218657=CARTESIAN_POINT('Ctrl Pts',(58.5959861416118,6.17878546397932,2.59908173791315));
#218658=CARTESIAN_POINT('Ctrl Pts',(58.5964866834551,6.17403490859039,2.59908173516029));
#218659=CARTESIAN_POINT('',(58.5996668978648,6.14377718965341,2.59908173516028));
#218660=CARTESIAN_POINT('Origin',(5.72296091834672E-15,1.85861897194828E-13,
2.59908173516023));
#218661=CARTESIAN_POINT('',(58.8181995570485,5.86337364149599,2.90134173516027));
#218662=CARTESIAN_POINT('Ctrl Pts',(58.5996668978648,6.14377718965341,2.59908173516029));
#218663=CARTESIAN_POINT('Ctrl Pts',(58.600064158263,6.13998815054705,2.59908174371518));
#218664=CARTESIAN_POINT('Ctrl Pts',(58.6005070878751,6.13621436696423,2.59915764355894));
#218665=CARTESIAN_POINT('Ctrl Pts',(58.6009943991739,6.13245764560146,2.5993076577528));
#218666=CARTESIAN_POINT('Ctrl Pts',(58.6038714482307,6.11027824676951,2.60019333020889));
#218667=CARTESIAN_POINT('Ctrl Pts',(58.6082941124964,6.0886907505575,2.60365973324126));
#218668=CARTESIAN_POINT('Ctrl Pts',(58.6139972210827,6.06807370279766,2.60934177082473));
#218669=CARTESIAN_POINT('Ctrl Pts',(58.6161277126021,6.0603718600669,2.61146439091893));
#218670=CARTESIAN_POINT('Ctrl Pts',(58.6184367045766,6.05280507414597,2.61389584429346));
#218671=CARTESIAN_POINT('Ctrl Pts',(58.6209098557463,6.04539170794194,2.61661604385258));
#218672=CARTESIAN_POINT('Ctrl Pts',(58.6228395323549,6.03960742773696,2.61873848000781));
#218673=CARTESIAN_POINT('Ctrl Pts',(58.6248693309927,6.03391702093566,2.62103707099793));
#218674=CARTESIAN_POINT('Ctrl Pts',(58.6269926140964,6.02832968645964,2.62350262767658));
#218675=CARTESIAN_POINT('Ctrl Pts',(58.6344241049594,6.00877401579358,2.63213207605185));
#218676=CARTESIAN_POINT('Ctrl Pts',(58.6430007716254,5.99048098024846,2.64280685971919));
#218677=CARTESIAN_POINT('Ctrl Pts',(58.6524381197038,5.97384499260641,2.65513293646089));
#218678=CARTESIAN_POINT('Ctrl Pts',(58.657156793743,5.96552699878538,2.66129597483174));
#218679=CARTESIAN_POINT('Ctrl Pts',(58.6620906399372,5.95762326711374,2.66787183533857));
#218680=CARTESIAN_POINT('Ctrl Pts',(58.667204101582,5.95018309968312,2.67481125953866));
#218681=CARTESIAN_POINT('Ctrl Pts',(58.6722957161033,5.942774720162,2.68172103524084));
#218682=CARTESIAN_POINT('Ctrl Pts',(58.6775652709345,5.93582574548871,2.68899101329792));
#218683=CARTESIAN_POINT('Ctrl Pts',(58.682978094856,5.92938546966287,2.69657334701278));
#218684=CARTESIAN_POINT('Ctrl Pts',(58.6830013202262,5.92935783569723,2.69660588132575));
#218685=CARTESIAN_POINT('Ctrl Pts',(58.6830245479289,5.92933021064647,2.69663842081383));
#218686=CARTESIAN_POINT('Ctrl Pts',(58.6830477779621,5.92930259451081,2.69667096547384));
#218687=CARTESIAN_POINT('Ctrl Pts',(58.6940026150825,5.91627935575131,2.71201840157951));
#218688=CARTESIAN_POINT('Ctrl Pts',(58.7054384852685,5.90523719704714,2.7284564593937));
#218689=CARTESIAN_POINT('Ctrl Pts',(58.7171784805293,5.8960952642491,2.74568723186929));
#218690=CARTESIAN_POINT('Ctrl Pts',(58.7293455537178,5.8866207659238,2.76354482594377));
#218691=CARTESIAN_POINT('Ctrl Pts',(58.7418401303876,5.87918707069746,2.78225519317208));
#218692=CARTESIAN_POINT('Ctrl Pts',(58.7544760786601,5.87375524644683,2.80151223085615));
#218693=CARTESIAN_POINT('Ctrl Pts',(58.7669316835984,5.86840094651606,2.82049442740392));
#218694=CARTESIAN_POINT('Ctrl Pts',(58.7795255625985,5.86499195787596,2.84000929089408));
#218695=CARTESIAN_POINT('Ctrl Pts',(58.7920763953149,5.86353919439998,2.85976644341793));
#218696=CARTESIAN_POINT('Ctrl Pts',(58.8008270591852,5.86252630185742,2.87354148167065));
#218697=CARTESIAN_POINT('Ctrl Pts',(58.8095567514071,5.86246534555174,2.88743438345549));
#218698=CARTESIAN_POINT('Ctrl Pts',(58.8181995570485,5.86337364149599,2.90134173516027));
#218699=CARTESIAN_POINT('',(59.1725467709677,5.90061356181276,3.47153072139077));
#218700=CARTESIAN_POINT('',(58.8181995570485,5.86337364149599,2.90134173516028));
#218701=CARTESIAN_POINT('',(59.4651754363832,0.316925998273232,3.47153072139073));
#218702=CARTESIAN_POINT('Origin',(5.53234440788222E-15,1.85015204418142E-13,
3.47153072139072));
#218703=CARTESIAN_POINT('',(59.1088767419348,0.316922544675878,2.90134173516024));
#218704=CARTESIAN_POINT('',(59.4651754363832,0.316925998273232,3.47153072139073));
#218705=CARTESIAN_POINT('',(58.9208513795073,0.0152121934561109,2.59908173516024));
#218706=CARTESIAN_POINT('Ctrl Pts',(59.1088767419348,0.316922544675878,
2.90134173516024));
#218707=CARTESIAN_POINT('Ctrl Pts',(59.0966467827006,0.316922401514052,
2.88176998919844));
#218708=CARTESIAN_POINT('Ctrl Pts',(59.0844716853565,0.315000085554071,
2.86226752356799));
#218709=CARTESIAN_POINT('Ctrl Pts',(59.0725173476328,0.311230629649457,
2.84310370500131));
#218710=CARTESIAN_POINT('Ctrl Pts',(59.0603470709145,0.307393083605762,
2.82359371788815));
#218711=CARTESIAN_POINT('Ctrl Pts',(59.048404675037,0.301641096265457,2.804433226372));
#218712=CARTESIAN_POINT('Ctrl Pts',(59.036857331986,0.294001187895731,2.785893238785));
#218713=CARTESIAN_POINT('Ctrl Pts',(59.0257988735004,0.286684733438041,
2.76813818620296));
#218714=CARTESIAN_POINT('Ctrl Pts',(59.0151019493863,0.277636448049551,
2.75095095199063));
#218715=CARTESIAN_POINT('Ctrl Pts',(59.0049186873018,0.266835172455698,
2.7345777143551));
#218716=CARTESIAN_POINT('Ctrl Pts',(58.9968192555067,0.258244193038107,
2.72155497955828));
#218717=CARTESIAN_POINT('Ctrl Pts',(58.9890447295129,0.248543417988351,
2.7090471116008));
#218718=CARTESIAN_POINT('Ctrl Pts',(58.981678934725,0.237702773059678,2.69718956158338));
#218719=CARTESIAN_POINT('Ctrl Pts',(58.9816588284979,0.23767318162042,2.69715719432356));
#218720=CARTESIAN_POINT('Ctrl Pts',(58.9816387254916,0.23764358171716,2.69712483219022));
#218721=CARTESIAN_POINT('Ctrl Pts',(58.9816186257082,0.237613973350474,
2.6970924751865));
#218722=CARTESIAN_POINT('Ctrl Pts',(58.9776173965852,0.231719887006966,
2.69065122242275));
#218723=CARTESIAN_POINT('Ctrl Pts',(58.9737507180862,0.225454527233545,
2.68442464469425));
#218724=CARTESIAN_POINT('Ctrl Pts',(58.9700384170936,0.218853219640912,
2.67844505923578));
#218725=CARTESIAN_POINT('Ctrl Pts',(58.9626710986899,0.20575246757011,2.66657815779566));
#218726=CARTESIAN_POINT('Ctrl Pts',(58.9559120649696,0.191327202905614,
2.65568445664172));
#218727=CARTESIAN_POINT('Ctrl Pts',(58.9499179036781,0.175845309932433,
2.64601906229514));
#218728=CARTESIAN_POINT('Ctrl Pts',(58.9454222827095,0.164233890202547,
2.6387700165352));
#218729=CARTESIAN_POINT('Ctrl Pts',(58.9413569016699,0.152028117041484,
2.632211893876));
#218730=CARTESIAN_POINT('Ctrl Pts',(58.9377878323772,0.139341004226325,
2.62645231033232));
#218731=CARTESIAN_POINT('Ctrl Pts',(58.9364494313924,0.13458333692064,2.62429246650344));
#218732=CARTESIAN_POINT('Ctrl Pts',(58.9351808244388,0.12975798122765,2.62224491711744));
#218733=CARTESIAN_POINT('Ctrl Pts',(58.933985496586,0.124870896863504,2.62031533672596));
#218734=CARTESIAN_POINT('Ctrl Pts',(58.9298018491012,0.107766101588996,
2.61356180535577));
#218735=CARTESIAN_POINT('Ctrl Pts',(58.9265158655229,0.0899051301002505,
2.60825339735347));
#218736=CARTESIAN_POINT('Ctrl Pts',(58.9242770147326,0.0715435052827752,
2.6046333798761));
#218737=CARTESIAN_POINT('Ctrl Pts',(58.9231575893375,0.0623626928740375,
2.60282337113742));
#218738=CARTESIAN_POINT('Ctrl Pts',(58.9222999481582,0.0530567171307616,
2.60143545939114));
#218739=CARTESIAN_POINT('Ctrl Pts',(58.9217227791368,0.0436575183856167,
2.60050005034595));
#218740=CARTESIAN_POINT('Ctrl Pts',(58.9214341946262,0.0389579190130443,
2.60003234582336));
#218741=CARTESIAN_POINT('Ctrl Pts',(58.9212157281805,0.0342350138896486,
2.59967776696065));
#218742=CARTESIAN_POINT('Ctrl Pts',(58.9210697160839,0.0294927955550733,
2.59944011429159));
#218743=CARTESIAN_POINT('Ctrl Pts',(58.9209237039872,0.024750577220498,
2.59920246162253));
#218744=CARTESIAN_POINT('Ctrl Pts',(58.9208501479391,0.0199890456752306,
2.5990817379131));
#218745=CARTESIAN_POINT('Ctrl Pts',(58.9208513795073,0.0152121934561115,
2.59908173516024));
#218746=CARTESIAN_POINT('',(58.9208533432504,1.98323206572159E-13,2.59908173516024));
#218747=CARTESIAN_POINT('Origin',(4.7062627014205E-16,1.91107483127175E-13,
2.59908173516023));
#218748=CARTESIAN_POINT('',(58.6605641730809,2.0120008167586E-13,2.18253198860263));
#218749=CARTESIAN_POINT('',(58.9208513795073,-0.0152121934557287,2.59908173516024));
#218750=CARTESIAN_POINT('Origin',(4.7062627014205E-16,1.91107483127175E-13,
2.59908173516023));
#218751=CARTESIAN_POINT('',(59.1088767419348,-0.316922544675487,2.90134173516023));
#218752=CARTESIAN_POINT('Ctrl Pts',(58.9208513795073,-0.0152121934557287,
2.59908173516024));
#218753=CARTESIAN_POINT('Ctrl Pts',(58.9208504012364,-0.0190220008283522,
2.59908174371513));
#218754=CARTESIAN_POINT('Ctrl Pts',(58.9208964366351,-0.022821409981532,
2.5991576435589));
#218755=CARTESIAN_POINT('Ctrl Pts',(58.9209883940807,-0.0266084895328146,
2.59930765775277));
#218756=CARTESIAN_POINT('Ctrl Pts',(58.9215313038857,-0.0489671208145109,
2.60019333020887));
#218757=CARTESIAN_POINT('Ctrl Pts',(58.9236732325289,-0.070898652763302,
2.60365973324139));
#218758=CARTESIAN_POINT('Ctrl Pts',(58.9271900305704,-0.0919988953551827,
2.60934177082511));
#218759=CARTESIAN_POINT('Ctrl Pts',(58.9285037892493,-0.0998812435895791,
2.61146439091921));
#218760=CARTESIAN_POINT('Ctrl Pts',(58.9300091878199,-0.107647933247761,
2.61389584429359));
#218761=CARTESIAN_POINT('Ctrl Pts',(58.9316938830317,-0.115279202946726,
2.61661604385252));
#218762=CARTESIAN_POINT('Ctrl Pts',(58.933008366749,-0.12123350239003,2.61873848000775));
#218763=CARTESIAN_POINT('Ctrl Pts',(58.9344322364591,-0.12710490827982,
2.62103707099787));
#218764=CARTESIAN_POINT('Ctrl Pts',(58.9359598525093,-0.132883578272882,
2.62350262767652));
#218765=CARTESIAN_POINT('Ctrl Pts',(58.9413065086849,-0.153108923248597,
2.63213207605179));
#218766=CARTESIAN_POINT('Ctrl Pts',(58.9479240485795,-0.172198253417529,
2.64280685971914));
#218767=CARTESIAN_POINT('Ctrl Pts',(58.9555707636545,-0.189729578870587,
2.65513293646084));
#218768=CARTESIAN_POINT('Ctrl Pts',(58.959394121192,-0.198495241597116,
2.66129597483169));
#218769=CARTESIAN_POINT('Ctrl Pts',(58.9634747743348,-0.206871403160361,
2.66787183533852));
#218770=CARTESIAN_POINT('Ctrl Pts',(58.9677825146337,-0.214805314863025,
2.67481125953861));
#218771=CARTESIAN_POINT('Ctrl Pts',(58.9720718502312,-0.222705329147438,
2.68172103524079));
#218772=CARTESIAN_POINT('Ctrl Pts',(58.9765861722458,-0.230167055078992,
2.68899101329788));
#218773=CARTESIAN_POINT('Ctrl Pts',(58.9812961520165,-0.23713784456646,
2.69657334701273));
#218774=CARTESIAN_POINT('Ctrl Pts',(58.9813163616197,-0.237167754862604,
2.69660588132571));
#218775=CARTESIAN_POINT('Ctrl Pts',(58.9813365744745,-0.237197656536514,
2.6966384208138));
#218776=CARTESIAN_POINT('Ctrl Pts',(58.9813567905789,-0.237227549587767,
2.69667096547381));
#218777=CARTESIAN_POINT('Ctrl Pts',(58.9908903168207,-0.251324537971755,
2.71201840157895));
#218778=CARTESIAN_POINT('Ctrl Pts',(59.0011093202324,-0.263501580511499,
2.72845645939253));
#218779=CARTESIAN_POINT('Ctrl Pts',(59.0118294103837,-0.273820596508295,
2.74568723186747));
#218780=CARTESIAN_POINT('Ctrl Pts',(59.0229394763216,-0.284514998003045,
2.76354482594125));
#218781=CARTESIAN_POINT('Ctrl Pts',(59.0345885736542,-0.293214009567509,
2.78225519316881));
#218782=CARTESIAN_POINT('Ctrl Pts',(59.0465875206378,-0.299936893971445,
2.80151223085212));
#218783=CARTESIAN_POINT('Ctrl Pts',(59.0584152157249,-0.306563827730263,
2.82049442739912));
#218784=CARTESIAN_POINT('Ctrl Pts',(59.0705837677937,-0.311270560392544,
2.84000929088849));
#218785=CARTESIAN_POINT('Ctrl Pts',(59.0829139906012,-0.314027284735069,
2.85976644341157));
#218786=CARTESIAN_POINT('Ctrl Pts',(59.0915108413196,-0.315949321993822,
2.87354148166636));
#218787=CARTESIAN_POINT('Ctrl Pts',(59.1001863397065,-0.316922445687508,
2.88743438345332));
#218788=CARTESIAN_POINT('Ctrl Pts',(59.1088767419348,-0.316922544675462,
2.90134173516024));
#218789=CARTESIAN_POINT('',(59.4651754363832,-0.316925998272862,3.47153072139072));
#218790=CARTESIAN_POINT('',(59.1088767419348,-0.3169225446755,2.90134173516023));
#218791=CARTESIAN_POINT('',(59.1725467709678,-5.90061356181158,3.47153072139069));
#218792=CARTESIAN_POINT('Origin',(5.53234440788222E-15,1.85015204418142E-13,
3.47153072139072));
#218793=CARTESIAN_POINT('',(58.8181995570486,-5.86337364149481,2.90134173516019));
#218794=CARTESIAN_POINT('',(59.1725467709678,-5.90061356181158,3.47153072139069));
#218795=CARTESIAN_POINT('',(58.5996668978649,-6.14377718965223,2.5990817351602));
#218796=CARTESIAN_POINT('Ctrl Pts',(58.8181995570486,-5.86337364149481,
2.9013417351602));
#218797=CARTESIAN_POINT('Ctrl Pts',(58.8060365798459,-5.86209540502774,
2.88176998919788));
#218798=CARTESIAN_POINT('Ctrl Pts',(58.7937272422254,-5.86273454612429,
2.86226752356692));
#218799=CARTESIAN_POINT('Ctrl Pts',(58.7814443761811,-5.86523378400357,
2.84310370499975));
#218800=CARTESIAN_POINT('Ctrl Pts',(58.7689396367211,-5.86777816724576,
2.82359371788606));
#218801=CARTESIAN_POINT('Ctrl Pts',(58.75646141614,-5.87225032430905,2.80443322636941));
#218802=CARTESIAN_POINT('Ctrl Pts',(58.7441787427607,-5.8786413544378,2.78589323878195));
#218803=CARTESIAN_POINT('Ctrl Pts',(58.7324160859264,-5.88476180492122,
2.76813818619945));
#218804=CARTESIAN_POINT('Ctrl Pts',(58.7208319573147,-5.89264238981678,
2.75095095198671));
#218805=CARTESIAN_POINT('Ctrl Pts',(58.709575439466,-5.90232005415664,2.73457771435083));
#218806=CARTESIAN_POINT('Ctrl Pts',(58.7006223753302,-5.91001735013063,
2.72155497955553));
#218807=CARTESIAN_POINT('Ctrl Pts',(58.6918764318957,-5.91885232406405,
2.70904711159948));
#218808=CARTESIAN_POINT('Ctrl Pts',(58.6834178317481,-5.92886364759452,
2.69718956158335));
#218809=CARTESIAN_POINT('Ctrl Pts',(58.6833947425173,-5.92889097525576,
2.69715719432352));
#218810=CARTESIAN_POINT('Ctrl Pts',(58.683371655605,-5.92891831167131,2.69712483219017));
#218811=CARTESIAN_POINT('Ctrl Pts',(58.6833485710132,-5.92894565684079,
2.69709247518645));
#218812=CARTESIAN_POINT('Ctrl Pts',(58.6787531612542,-5.93438921243119,
2.69065122242271));
#218813=CARTESIAN_POINT('Ctrl Pts',(58.6742527563957,-5.94021607194678,
2.68442464469422));
#218814=CARTESIAN_POINT('Ctrl Pts',(58.6698707672382,-5.94639317576777,
2.67844505923575));
#218815=CARTESIAN_POINT('Ctrl Pts',(58.6611744062939,-5.95865206607682,
2.66657815779563));
#218816=CARTESIAN_POINT('Ctrl Pts',(58.6529445485199,-5.97229179622419,
2.65568445664168));
#218817=CARTESIAN_POINT('Ctrl Pts',(58.6453649253902,-5.98706231729939,
2.6460190622951));
#218818=CARTESIAN_POINT('Ctrl Pts',(58.6396802080429,-5.99814020810579,
2.63877001653516));
#218819=CARTESIAN_POINT('Ctrl Pts',(58.6343612468745,-6.0098541687317,2.63221189387596));
#218820=CARTESIAN_POINT('Ctrl Pts',(58.6294855649109,-6.02209871088692,
2.62645231033228));
#218821=CARTESIAN_POINT('Ctrl Pts',(58.6276571841746,-6.02669041419513,
2.6242924665034));
#218822=CARTESIAN_POINT('Ctrl Pts',(58.6258911397673,-6.0313567305494,2.62224491711741));
#218823=CARTESIAN_POINT('Ctrl Pts',(58.6241915206271,-6.0360920971705,2.62031533672592));
#218824=CARTESIAN_POINT('Ctrl Pts',(58.6182428536364,-6.05266588034435,
2.61356180535573));
#218825=CARTESIAN_POINT('Ctrl Pts',(58.6131078911178,-6.07008552874868,
2.60825339735344));
#218826=CARTESIAN_POINT('Ctrl Pts',(58.6089619925611,-6.08811254303161,
2.60463337987607));
#218827=CARTESIAN_POINT('Ctrl Pts',(58.6068890432828,-6.09712605017307,
2.60282337113739));
#218828=CARTESIAN_POINT('Ctrl Pts',(58.6050633610079,-6.10629139889302,
2.6014354593911));
#218829=CARTESIAN_POINT('Ctrl Pts',(58.6035068699781,-6.11557877725314,
2.60050005034591));
#218830=CARTESIAN_POINT('Ctrl Pts',(58.6027286244632,-6.1202224664332,2.60003234582332));
#218831=CARTESIAN_POINT('Ctrl Pts',(58.6020176767849,-6.12489666302632,
2.59967776696062));
#218832=CARTESIAN_POINT('Ctrl Pts',(58.6013767677628,-6.1295976405726,2.59944011429156));
#218833=CARTESIAN_POINT('Ctrl Pts',(58.6007358587407,-6.13429861811887,
2.5992024616225));
#218834=CARTESIAN_POINT('Ctrl Pts',(58.6001649900651,-6.13902637679545,
2.59908173791307));
#218835=CARTESIAN_POINT('Ctrl Pts',(58.5996668978649,-6.14377718965223,
2.5990817351602));
#218836=CARTESIAN_POINT('',(58.5964866834552,-6.17403490858921,2.59908173516019));
#218837=CARTESIAN_POINT('Origin',(5.72296091834672E-15,1.85847653270679E-13,
2.59908173516024));
#218838=CARTESIAN_POINT('',(58.7519447039089,-6.49374646112641,2.90134173516019));
#218839=CARTESIAN_POINT('Ctrl Pts',(58.5964866834552,-6.17403490858921,
2.5990817351602));
#218840=CARTESIAN_POINT('Ctrl Pts',(58.5960874772333,-6.17782374318127,
2.5990817437151));
#218841=CARTESIAN_POINT('Ctrl Pts',(58.5957361140452,-6.18160715078305,
2.59915764355886));
#218842=CARTESIAN_POINT('Ctrl Pts',(58.5954317101325,-6.18538309648678,
2.59930765775272));
#218843=CARTESIAN_POINT('Ctrl Pts',(58.5936345324522,-6.20767599437294,
2.60019333020876));
#218844=CARTESIAN_POINT('Ctrl Pts',(58.5934722580545,-6.22971127560298,
2.60365973324086));
#218845=CARTESIAN_POINT('Ctrl Pts',(58.5947642147753,-6.25106353435168,
2.60934177082389));
#218846=CARTESIAN_POINT('Ctrl Pts',(58.5952468467988,-6.25904002743504,
2.61146439091827));
#218847=CARTESIAN_POINT('Ctrl Pts',(58.595932158504,-6.26692152735531,2.61389584429305));
#218848=CARTESIAN_POINT('Ctrl Pts',(58.5968099398849,-6.2746870907634,2.61661604385248));
#218849=CARTESIAN_POINT('Ctrl Pts',(58.5974948289522,-6.28074617289431,
2.61873848000772));
#218850=CARTESIAN_POINT('Ctrl Pts',(58.5982971695202,-6.28673424952099,
2.62103707099783));
#218851=CARTESIAN_POINT('Ctrl Pts',(58.5992123816357,-6.29264094271338,
2.62350262767647));
#218852=CARTESIAN_POINT('Ctrl Pts',(58.6024156240399,-6.31331436888676,
2.63213207605174));
#218853=CARTESIAN_POINT('Ctrl Pts',(58.6070015340113,-6.33299084698348,
2.6428068597191));
#218854=CARTESIAN_POINT('Ctrl Pts',(58.6127738370724,-6.35122543337721,
2.6551329364608));
#218855=CARTESIAN_POINT('Ctrl Pts',(58.6156599886029,-6.36034272657408,
2.66129597483165));
#218856=CARTESIAN_POINT('Ctrl Pts',(58.6188427402045,-6.36909954705002,
2.66787183533847));
#218857=CARTESIAN_POINT('Ctrl Pts',(58.6222975626533,-6.37744027742783,
2.67481125953856));
#218858=CARTESIAN_POINT('Ctrl Pts',(58.6257376244687,-6.38574537226586,
2.68172103524075));
#218859=CARTESIAN_POINT('Ctrl Pts',(58.62944725381,-6.3936380972249,2.68899101329783));
#218860=CARTESIAN_POINT('Ctrl Pts',(58.6334027859058,-6.40106302694565,
2.69657334701269));
#218861=CARTESIAN_POINT('Ctrl Pts',(58.6334197583214,-6.40109488586883,
2.69660588132566));
#218862=CARTESIAN_POINT('Ctrl Pts',(58.6334367348721,-6.40112673655689,
2.69663842081375));
#218863=CARTESIAN_POINT('Ctrl Pts',(58.6334537155558,-6.4011585790092,2.69667096547375));
#218864=CARTESIAN_POINT('Ctrl Pts',(58.6414614796112,-6.41617486746407,
2.71201840157957));
#218865=CARTESIAN_POINT('Ctrl Pts',(58.6503516547096,-6.42935337961396,
2.72845645939393));
#218866=CARTESIAN_POINT('Ctrl Pts',(58.6599343882013,-6.44073642151141,
2.74568723186971));
#218867=CARTESIAN_POINT('Ctrl Pts',(58.6698657226822,-6.45253355607543,
2.7635448259443));
#218868=CARTESIAN_POINT('Ctrl Pts',(58.6805417107305,-6.46240257578718,
2.78225519317272));
#218869=CARTESIAN_POINT('Ctrl Pts',(58.691772193452,-6.47034286301596,2.80151223085691));
#218870=CARTESIAN_POINT('Ctrl Pts',(58.7028423919864,-6.47816982452966,
2.82049442740461));
#218871=CARTESIAN_POINT('Ctrl Pts',(58.7144522959221,-6.4841227332657,2.84000929089469));
#218872=CARTESIAN_POINT('Ctrl Pts',(58.7264268163201,-6.48815321522529,
2.85976644341845));
#218873=CARTESIAN_POINT('Ctrl Pts',(58.7347756649885,-6.49096333895657,
2.87354148167098));
#218874=CARTESIAN_POINT('Ctrl Pts',(58.7433019189618,-6.49283796829079,
2.88743438345561));
#218875=CARTESIAN_POINT('Ctrl Pts',(58.7519447039089,-6.49374646112638,
2.90134173516019));
#218876=CARTESIAN_POINT('',(59.1062911958297,-6.53099325079957,3.47153072139068));
#218877=CARTESIAN_POINT('',(58.7519447039089,-6.49374646112642,2.90134173516019));
#218878=CARTESIAN_POINT('',(58.2316113004783,-12.0535047649312,3.47153072139065));
#218879=CARTESIAN_POINT('Origin',(5.53234440788222E-15,1.85015204418142E-13,
3.47153072139072));
#218880=CARTESIAN_POINT('',(57.8830978693157,-11.9794294790603,2.90134173516016));
#218881=CARTESIAN_POINT('',(58.2316113004783,-12.0535047649312,3.47153072139065));
#218882=CARTESIAN_POINT('',(57.6364522029208,-12.2354540642035,2.59908173516015));
#218883=CARTESIAN_POINT('Ctrl Pts',(57.8830978693157,-11.9794294790603,
2.90134173516015));
#218884=CARTESIAN_POINT('Ctrl Pts',(57.8711351342685,-11.9768868675905,
2.88176998919795));
#218885=CARTESIAN_POINT('Ctrl Pts',(57.8588264200508,-11.9762358312599,
2.86226752356711));
#218886=CARTESIAN_POINT('Ctrl Pts',(57.8463495993372,-11.9774374689404,
2.84310370500005));
#218887=CARTESIAN_POINT('Ctrl Pts',(57.8336474016781,-11.9786608125856,
2.8235937178864));
#218888=CARTESIAN_POINT('Ctrl Pts',(57.8207700703897,-11.9818041414829,
2.8044332263698));
#218889=CARTESIAN_POINT('Ctrl Pts',(57.8078866382223,-11.9868762719067,
2.78589323878238));
#218890=CARTESIAN_POINT('Ctrl Pts',(57.7955486571693,-11.9917336614792,
2.7681381861998));
#218891=CARTESIAN_POINT('Ctrl Pts',(57.7832042421973,-11.9983602045441,
2.75095095198698));
#218892=CARTESIAN_POINT('Ctrl Pts',(57.7709977973496,-12.0068082271136,
2.73457771435104));
#218893=CARTESIAN_POINT('Ctrl Pts',(57.7612891925165,-12.0135275064593,
2.72155497955564));
#218894=CARTESIAN_POINT('Ctrl Pts',(57.7516676540269,-12.0213998814541,
2.7090471115995));
#218895=CARTESIAN_POINT('Ctrl Pts',(57.7422089227119,-12.030472197432,2.6971895615833));
#218896=CARTESIAN_POINT('Ctrl Pts',(57.7421831034479,-12.0304969619077,
2.69715719432347));
#218897=CARTESIAN_POINT('Ctrl Pts',(57.7421572855747,-12.030521735332,2.69712483219013));
#218898=CARTESIAN_POINT('Ctrl Pts',(57.7421314690942,-12.0305465177049,
2.69709247518641));
#218899=CARTESIAN_POINT('Ctrl Pts',(57.73699222697,-12.035479901808,2.69065122242267));
#218900=CARTESIAN_POINT('Ctrl Pts',(57.7319074031293,-12.0408044207735,
2.68442464469416));
#218901=CARTESIAN_POINT('Ctrl Pts',(57.726903735797,-12.0464896431808,2.67844505923569));
#218902=CARTESIAN_POINT('Ctrl Pts',(57.7169736114625,-12.0577723607605,
2.66657815779557));
#218903=CARTESIAN_POINT('Ctrl Pts',(57.7073630976789,-12.070477116653,2.65568445664164));
#218904=CARTESIAN_POINT('Ctrl Pts',(57.6982810566481,-12.0843744369104,
2.64601906229505));
#218905=CARTESIAN_POINT('Ctrl Pts',(57.691469525875,-12.0947974271034,2.63877001653511));
#218906=CARTESIAN_POINT('Ctrl Pts',(57.6849552602294,-12.1058912345902,
2.63221189387592));
#218907=CARTESIAN_POINT('Ctrl Pts',(57.6788263845869,-12.1175590523193,
2.62645231033224));
#218908=CARTESIAN_POINT('Ctrl Pts',(57.676528056221,-12.1219344839678,2.62429246650336));
#218909=CARTESIAN_POINT('Ctrl Pts',(57.6742839235121,-12.1263906358448,
2.62224491711736));
#218910=CARTESIAN_POINT('Ctrl Pts',(57.6720986344674,-12.1309224030552,
2.62031533672588));
#218911=CARTESIAN_POINT('Ctrl Pts',(57.6644501228112,-12.1467835882917,
2.61356180535569));
#218912=CARTESIAN_POINT('Ctrl Pts',(57.6575224410762,-12.1635710602984,
2.60825339735338));
#218913=CARTESIAN_POINT('Ctrl Pts',(57.6515149180853,-12.1810659563059,
2.60463337987601));
#218914=CARTESIAN_POINT('Ctrl Pts',(57.6485111565899,-12.1898134043097,
2.60282337113733));
#218915=CARTESIAN_POINT('Ctrl Pts',(57.6457374357766,-12.1987377085277,
2.60143545939106));
#218916=CARTESIAN_POINT('Ctrl Pts',(57.6432186759797,-12.207811512042,2.60050005034587));
#218917=CARTESIAN_POINT('Ctrl Pts',(57.6419592960813,-12.2123484137991,
2.60003234582328));
#218918=CARTESIAN_POINT('Ctrl Pts',(57.6407636564618,-12.216922690386,2.59967776696058));
#218919=CARTESIAN_POINT('Ctrl Pts',(57.6396348724477,-12.2215309222502,
2.59944011429152));
#218920=CARTESIAN_POINT('Ctrl Pts',(57.6385060884335,-12.2261391541144,
2.59920246162246));
#218921=CARTESIAN_POINT('Ctrl Pts',(57.637444161687,-12.2307813416089,2.59908173791303));
#218922=CARTESIAN_POINT('Ctrl Pts',(57.6364522029208,-12.2354540642035,
2.59908173516016));
#218923=CARTESIAN_POINT('',(57.6301266171959,-12.2652136052652,2.59908173516015));
#218924=CARTESIAN_POINT('Origin',(5.72184526906101E-15,1.85840609338312E-13,
2.59908173516024));
#218925=CARTESIAN_POINT('',(57.7513140650722,-12.5994235324463,2.90134173516015));
#218926=CARTESIAN_POINT('Ctrl Pts',(57.6301266171959,-12.2652136052652,
2.59908173516016));
#218927=CARTESIAN_POINT('Ctrl Pts',(57.6293335568101,-12.268939955812,2.59908174371505));
#218928=CARTESIAN_POINT('Ctrl Pts',(57.6285886446437,-12.272665910057,2.59915764355882));
#218929=CARTESIAN_POINT('Ctrl Pts',(57.6278912144857,-12.2763893518618,
2.59930765775268));
#218930=CARTESIAN_POINT('Ctrl Pts',(57.6237736395747,-12.2983722707009,
2.60019333020878));
#218931=CARTESIAN_POINT('Ctrl Pts',(57.6213089400484,-12.3202698780625,
2.60365973324121));
#218932=CARTESIAN_POINT('Ctrl Pts',(57.6203619005009,-12.3416402131555,
2.60934177082479));
#218933=CARTESIAN_POINT('Ctrl Pts',(57.6200081180516,-12.3496234589577,
2.61146439091895));
#218934=CARTESIAN_POINT('Ctrl Pts',(57.6198658344727,-12.3575334177749,
2.61389584429341));
#218935=CARTESIAN_POINT('Ctrl Pts',(57.6199270848659,-12.3653481937518,
2.61661604385244));
#218936=CARTESIAN_POINT('Ctrl Pts',(57.6199748754953,-12.3714456739986,
2.61873848000767));
#218937=CARTESIAN_POINT('Ctrl Pts',(57.62014689631,-12.3774848147415,2.62103707099779));
#218938=CARTESIAN_POINT('Ctrl Pts',(57.6204396772353,-12.3834548161666,
2.62350262767644));
#218939=CARTESIAN_POINT('Ctrl Pts',(57.6214644104742,-12.4043498211543,
2.6321320760517));
#218940=CARTESIAN_POINT('Ctrl Pts',(57.6239684463329,-12.4243978675672,
2.64280685971906));
#218941=CARTESIAN_POINT('Ctrl Pts',(57.6278030948198,-12.4431359329572,
2.65513293646075));
#218942=CARTESIAN_POINT('Ctrl Pts',(57.6297204190632,-12.4525049656522,
2.6612959748316));
#218943=CARTESIAN_POINT('Ctrl Pts',(57.6319703982311,-12.4615465034833,
2.66787183533843));
#218944=CARTESIAN_POINT('Ctrl Pts',(57.6345344510721,-12.4702026697488,
2.67481125953852));
#218945=CARTESIAN_POINT('Ctrl Pts',(57.6370875490682,-12.4788218527834,
2.68172103524071));
#218946=CARTESIAN_POINT('Ctrl Pts',(57.6399518422609,-12.4870591024237,
2.68899101329778));
#218947=CARTESIAN_POINT('Ctrl Pts',(57.6431095890444,-12.4948568232939,
2.69657334701264));
#218948=CARTESIAN_POINT('Ctrl Pts',(57.6431231383191,-12.4948902817911,
2.69660588132561));
#218949=CARTESIAN_POINT('Ctrl Pts',(57.6431366925669,-12.4949237325305,
2.6966384208137));
#218950=CARTESIAN_POINT('Ctrl Pts',(57.6431502517861,-12.4949571755113,
2.69667096547371));
#218951=CARTESIAN_POINT('Ctrl Pts',(57.6495445189161,-12.510728242438,2.71201840157977));
#218952=CARTESIAN_POINT('Ctrl Pts',(57.657008463082,-12.5247638376608,2.72845645939442));
#218953=CARTESIAN_POINT('Ctrl Pts',(57.6653488494803,-12.5370861904697,
2.74568723187049));
#218954=CARTESIAN_POINT('Ctrl Pts',(57.673992642725,-12.5498568062279,2.76354482594546));
#218955=CARTESIAN_POINT('Ctrl Pts',(57.6835785531295,-12.5607877070417,
2.78225519317428));
#218956=CARTESIAN_POINT('Ctrl Pts',(57.69391752807,-12.5698584016469,2.80151223085888));
#218957=CARTESIAN_POINT('Ctrl Pts',(57.7041089426397,-12.5787996370874,
2.82049442740705));
#218958=CARTESIAN_POINT('Ctrl Pts',(57.715032997905,-12.5859335005836,2.8400092908976));
#218959=CARTESIAN_POINT('Ctrl Pts',(57.7265206205423,-12.5911935813568,
2.85976644342183));
#218960=CARTESIAN_POINT('Ctrl Pts',(57.7345299954283,-12.5948610032571,
2.87354148167323));
#218961=CARTESIAN_POINT('Ctrl Pts',(57.742813589566,-12.5976165994007,2.88743438345671));
#218962=CARTESIAN_POINT('Ctrl Pts',(57.7513140650722,-12.5994235324462,
2.90134173516015));
#218963=CARTESIAN_POINT('',(58.0998260601482,-12.6735055745731,3.47153072139064));
#218964=CARTESIAN_POINT('',(57.7513140650722,-12.5994235324462,2.90134173516015));
#218965=CARTESIAN_POINT('',(56.6526781108326,-18.0743352474882,3.4715307213906));
#218966=CARTESIAN_POINT('Origin',(5.53234440788222E-15,1.85015204418142E-13,
3.47153072139072));
#218967=CARTESIAN_POINT('',(56.3138168485097,-17.9642361803963,2.90134173516012));
#218968=CARTESIAN_POINT('',(56.6526781108326,-18.0743352474882,3.4715307213906));
#218969=CARTESIAN_POINT('',(56.0417604764386,-18.193076743594,2.59908173516011));
#218970=CARTESIAN_POINT('Ctrl Pts',(56.3138168485097,-17.9642361803963,
2.90134173516011));
#218971=CARTESIAN_POINT('Ctrl Pts',(56.3021854218467,-17.9604570513074,
2.88176998919846));
#218972=CARTESIAN_POINT('Ctrl Pts',(56.2900121878809,-17.95852297044,2.86226752356817));
#218973=CARTESIAN_POINT('Ctrl Pts',(56.2774781111569,-17.9584138425278,
2.84310370500164));
#218974=CARTESIAN_POINT('Ctrl Pts',(56.2647176232347,-17.958302743367,2.82359371788856));
#218975=CARTESIAN_POINT('Ctrl Pts',(56.2515822679757,-17.9600828051289,
2.80443322637249));
#218976=CARTESIAN_POINT('Ctrl Pts',(56.2382392305995,-17.9637804645252,
2.78589323878555));
#218977=CARTESIAN_POINT('Ctrl Pts',(56.2254611028306,-17.9673215746097,
2.76813818620352));
#218978=CARTESIAN_POINT('Ctrl Pts',(56.2124916494926,-17.9726214740509,
2.7509509519912));
#218979=CARTESIAN_POINT('Ctrl Pts',(56.1994690140106,-17.9797472965464,
2.73457771435566));
#218980=CARTESIAN_POINT('Ctrl Pts',(56.1891112379851,-17.9854149414334,
2.72155497955859));
#218981=CARTESIAN_POINT('Ctrl Pts',(56.1787195200283,-17.9922384661024,
2.70904711160088));
#218982=CARTESIAN_POINT('Ctrl Pts',(56.1683642893845,-18.0002723763363,
2.69718956158326));
#218983=CARTESIAN_POINT('Ctrl Pts',(56.1683360229685,-18.0002943063015,
2.69715719432343));
#218984=CARTESIAN_POINT('Ctrl Pts',(56.1683077570003,-18.0003162453118,
2.69712483219009));
#218985=CARTESIAN_POINT('Ctrl Pts',(56.1682794914818,-18.0003381933673,
2.69709247518637));
#218986=CARTESIAN_POINT('Ctrl Pts',(56.1626527236048,-18.0047073547945,
2.69065122242262));
#218987=CARTESIAN_POINT('Ctrl Pts',(56.157039191176,-18.009471196666,2.68442464469411));
#218988=CARTESIAN_POINT('Ctrl Pts',(56.1514686668953,-18.0146022491731,
2.67844505923564));
#218989=CARTESIAN_POINT('Ctrl Pts',(56.1404135756909,-18.0247851782086,
2.66657815779552));
#218990=CARTESIAN_POINT('Ctrl Pts',(56.1295277006976,-18.036415763882,2.6556844566416));
#218991=CARTESIAN_POINT('Ctrl Pts',(56.1190427465078,-18.0492876213726,
2.64601906229501));
#218992=CARTESIAN_POINT('Ctrl Pts',(56.1111790308655,-18.0589415144906,
2.63877001653507));
#218993=CARTESIAN_POINT('Ctrl Pts',(56.1035408324003,-18.069293622762,2.63221189387587));
#218994=CARTESIAN_POINT('Ctrl Pts',(56.096225912323,-18.0802568810123,2.62645231033219));
#218995=CARTESIAN_POINT('Ctrl Pts',(56.0934828172939,-18.0843681028561,
2.62429246650331));
#218996=CARTESIAN_POINT('Ctrl Pts',(56.090785183471,-18.0885652677235,2.62224491711732));
#218997=CARTESIAN_POINT('Ctrl Pts',(56.088138167006,-18.0928437845334,2.62031533672584));
#218998=CARTESIAN_POINT('Ctrl Pts',(56.0788736093786,-18.1078185933678,
2.61356180535565));
#218999=CARTESIAN_POINT('Ctrl Pts',(56.0702291095579,-18.1237899619206,
2.60825339735334));
#219000=CARTESIAN_POINT('Ctrl Pts',(56.0624257818119,-18.1405610619109,
2.60463337987597));
#219001=CARTESIAN_POINT('Ctrl Pts',(56.0585241179389,-18.1489466119061,
2.60282337113729));
#219002=CARTESIAN_POINT('Ctrl Pts',(56.0548327480528,-18.1575320950778,
2.60143545939101));
#219003=CARTESIAN_POINT('Ctrl Pts',(56.0513793155483,-18.1662929092561,
2.60050005034582));
#219004=CARTESIAN_POINT('Ctrl Pts',(56.049652599296,-18.1706733163452,2.60003234582323));
#219005=CARTESIAN_POINT('Ctrl Pts',(56.0479853674133,-18.1750975561943,
2.59967776696052));
#219006=CARTESIAN_POINT('Ctrl Pts',(56.046381075601,-18.1795625536238,2.59944011429146));
#219007=CARTESIAN_POINT('Ctrl Pts',(56.0447767837886,-18.1840275510534,
2.5992024616224));
#219008=CARTESIAN_POINT('Ctrl Pts',(56.0432354336629,-18.1885333065881,
2.59908173791296));
#219009=CARTESIAN_POINT('Ctrl Pts',(56.0417604764386,-18.193076743594,2.59908173516011));
#219010=CARTESIAN_POINT('',(56.0323588238394,-18.2220120550208,2.59908173516011));
#219011=CARTESIAN_POINT('Origin',(5.71999943999309E-15,1.85833720610448E-13,
2.59908173516024));
#219012=CARTESIAN_POINT('',(56.1179479440991,-18.5670586829457,2.90134173516011));
#219013=CARTESIAN_POINT('Ctrl Pts',(56.0323588238394,-18.2220120550208,
2.59908173516011));
#219014=CARTESIAN_POINT('Ctrl Pts',(56.031180598225,-18.225635094846,2.59908174371501));
#219015=CARTESIAN_POINT('Ctrl Pts',(56.030050298494,-18.2292627733998,2.59915764355878));
#219016=CARTESIAN_POINT('Ctrl Pts',(56.0289674832815,-18.2328929164982,
2.59930765775265));
#219017=CARTESIAN_POINT('Ctrl Pts',(56.0225746241531,-18.2543250068274,
2.60019333020864));
#219018=CARTESIAN_POINT('Ctrl Pts',(56.0178345032622,-18.2758450255484,
2.60365973324037));
#219019=CARTESIAN_POINT('Ctrl Pts',(56.0146588434097,-18.2969992991187,
2.60934177082277));
#219020=CARTESIAN_POINT('Ctrl Pts',(56.0134725226016,-18.3049018315318,
2.6114643909174));
#219021=CARTESIAN_POINT('Ctrl Pts',(56.0125042026269,-18.3127535860857,
2.61389584429253));
#219022=CARTESIAN_POINT('Ctrl Pts',(56.0117482509602,-18.320531954314,2.61661604385242));
#219023=CARTESIAN_POINT('Ctrl Pts',(56.0111584195475,-18.326601027407,2.61873848000765));
#219024=CARTESIAN_POINT('Ctrl Pts',(56.0106982359128,-18.3326250661765,
2.62103707099775));
#219025=CARTESIAN_POINT('Ctrl Pts',(56.010365377879,-18.3385929672493,2.6235026276764));
#219026=CARTESIAN_POINT('Ctrl Pts',(56.0092003747606,-18.3594806210041,
2.63213207605167));
#219027=CARTESIAN_POINT('Ctrl Pts',(56.0095951017658,-18.3796805851414,
2.64280685971903));
#219028=CARTESIAN_POINT('Ctrl Pts',(56.0114500824673,-18.3987168313621,
2.65513293646072));
#219029=CARTESIAN_POINT('Ctrl Pts',(56.012377572818,-18.4082349544725,2.66129597483157));
#219030=CARTESIAN_POINT('Ctrl Pts',(56.0136701283095,-18.417462148678,2.6678718353384));
#219031=CARTESIAN_POINT('Ctrl Pts',(56.0153153192432,-18.4263389120622,
2.67481125953849));
#219032=CARTESIAN_POINT('Ctrl Pts',(56.0169534811442,-18.4351777497205,
2.68172103524067));
#219033=CARTESIAN_POINT('Ctrl Pts',(56.0189410563926,-18.4436692750111,
2.68899101329776));
#219034=CARTESIAN_POINT('Ctrl Pts',(56.0212664209293,-18.4517543535692,
2.69657334701262));
#219035=CARTESIAN_POINT('Ctrl Pts',(56.0212763986143,-18.451789045062,2.69660588132559));
#219036=CARTESIAN_POINT('Ctrl Pts',(56.0212863820562,-18.4518237293595,
2.69663842081367));
#219037=CARTESIAN_POINT('Ctrl Pts',(56.0212963712531,-18.4518584064605,
2.69667096547368));
#219038=CARTESIAN_POINT('Ctrl Pts',(56.0260070845286,-18.4682114607488,
2.71201840157927));
#219039=CARTESIAN_POINT('Ctrl Pts',(56.0319630212276,-18.4829503621255,
2.72845645939336));
#219040=CARTESIAN_POINT('Ctrl Pts',(56.0389696815133,-18.4960770195693,
2.74568723186885));
#219041=CARTESIAN_POINT('Ctrl Pts',(56.0462312303137,-18.5096811989825,
2.7635448259432));
#219042=CARTESIAN_POINT('Ctrl Pts',(56.0546220378335,-18.5215542196613,
2.78225519317137));
#219043=CARTESIAN_POINT('Ctrl Pts',(56.0639562290192,-18.5316559412145,
2.8015122308553));
#219044=CARTESIAN_POINT('Ctrl Pts',(56.0731572003529,-18.5416134885352,
2.82049442740297));
#219045=CARTESIAN_POINT('Ctrl Pts',(56.0832757207117,-18.5498501466904,
2.84000929089302));
#219046=CARTESIAN_POINT('Ctrl Pts',(56.0941505847899,-18.5562821957318,
2.85976644341677));
#219047=CARTESIAN_POINT('Ctrl Pts',(56.1017327335077,-18.5607667347606,
2.87354148166982));
#219048=CARTESIAN_POINT('Ctrl Pts',(56.1096829110206,-18.5643731068263,
2.88743438345499));
#219049=CARTESIAN_POINT('Ctrl Pts',(56.1179479440991,-18.5670586829457,
2.90134173516011));
#219050=CARTESIAN_POINT('',(56.4568070719814,-18.6771643191701,3.4715307213906));
#219051=CARTESIAN_POINT('',(56.1179479440991,-18.5670586829457,2.90134173516011));
#219052=CARTESIAN_POINT('',(54.4530463244696,-23.897139530776,3.47153072139056));
#219053=CARTESIAN_POINT('Origin',(5.53234440788222E-15,1.85015204418142E-13,
3.47153072139072));
#219054=CARTESIAN_POINT('',(54.1275498658877,-23.7522229508819,2.90134173516007));
#219055=CARTESIAN_POINT('',(54.4530463244695,-23.897139530776,3.47153072139056));
#219056=CARTESIAN_POINT('',(53.8330634946841,-23.9513722670356,2.59908173516007));
#219057=CARTESIAN_POINT('Ctrl Pts',(54.1275498658877,-23.7522229508819,
2.90134173516007));
#219058=CARTESIAN_POINT('Ctrl Pts',(54.1163771839526,-23.7472487091029,
2.8817699891978));
#219059=CARTESIAN_POINT('Ctrl Pts',(54.1044728027367,-23.7440527738934,
2.86226752356688));
#219060=CARTESIAN_POINT('Ctrl Pts',(54.0920187959689,-23.742634076017,2.84310370499975));
#219061=CARTESIAN_POINT('Ctrl Pts',(54.0793398243589,-23.7411897512761,
2.82359371788624));
#219062=CARTESIAN_POINT('Ctrl Pts',(54.0660903588296,-23.7415870431739,
2.80443322636975));
#219063=CARTESIAN_POINT('Ctrl Pts',(54.0524339053535,-23.743869719213,2.78589323878245));
#219064=CARTESIAN_POINT('Ctrl Pts',(54.03935563071,-23.746055752667,2.7681381862003));
#219065=CARTESIAN_POINT('Ctrl Pts',(54.0259032350502,-23.7499709416779,
2.75095095198788));
#219066=CARTESIAN_POINT('Ctrl Pts',(54.0122070876528,-23.7556964920978,
2.73457771435229));
#219067=CARTESIAN_POINT('Ctrl Pts',(54.0013136223986,-23.7602504066221,
2.72155497955642));
#219068=CARTESIAN_POINT('Ctrl Pts',(53.9902655788133,-23.7659503209998,
2.70904711159983));
#219069=CARTESIAN_POINT('Ctrl Pts',(53.9791273029166,-23.7728578042863,
2.69718956158322));
#219070=CARTESIAN_POINT('Ctrl Pts',(53.9790968990415,-23.7728766594719,
2.69715719432339));
#219071=CARTESIAN_POINT('Ctrl Pts',(53.9790664946662,-23.7728955236998,
2.69712483219005));
#219072=CARTESIAN_POINT('Ctrl Pts',(53.9790360897926,-23.7729143969702,
2.69709247518633));
#219073=CARTESIAN_POINT('Ctrl Pts',(53.972983444209,-23.7766714662746,2.69065122242259));
#219074=CARTESIAN_POINT('Ctrl Pts',(53.9669027062282,-23.7808224374036,
2.6844246446941));
#219075=CARTESIAN_POINT('Ctrl Pts',(53.9608263568289,-23.7853431031255,
2.67844505923562));
#219076=CARTESIAN_POINT('Ctrl Pts',(53.9487674206471,-23.7943146773155,
2.6665781577955));
#219077=CARTESIAN_POINT('Ctrl Pts',(53.9367254523687,-23.8047436656392,
2.65568445664157));
#219078=CARTESIAN_POINT('Ctrl Pts',(53.9249524603721,-23.8164490335988,
2.64601906229499));
#219079=CARTESIAN_POINT('Ctrl Pts',(53.9161227163747,-23.8252280595685,
2.63877001653505));
#219080=CARTESIAN_POINT('Ctrl Pts',(53.9074442707907,-23.83472504876,2.63221189387585));
#219081=CARTESIAN_POINT('Ctrl Pts',(53.8990234500736,-23.8448636317798,
2.62645231033217));
#219082=CARTESIAN_POINT('Ctrl Pts',(53.8958656423047,-23.8486656004123,
2.62429246650329));
#219083=CARTESIAN_POINT('Ctrl Pts',(53.8927440632084,-23.8525577932534,
2.62224491711729));
#219084=CARTESIAN_POINT('Ctrl Pts',(53.8896643205894,-23.8565361833372,
2.6203153367258));
#219085=CARTESIAN_POINT('Ctrl Pts',(53.8788852214228,-23.8704605486303,
2.61356180535561));
#219086=CARTESIAN_POINT('Ctrl Pts',(53.8686186144656,-23.8854408280731,
2.60825339735331));
#219087=CARTESIAN_POINT('Ctrl Pts',(53.8591049768561,-23.9013043843653,
2.60463337987594));
#219088=CARTESIAN_POINT('Ctrl Pts',(53.8543481580514,-23.9092361625114,
2.60282337113726));
#219089=CARTESIAN_POINT('Ctrl Pts',(53.8497795825134,-23.9173887602863,
2.60143545939098));
#219090=CARTESIAN_POINT('Ctrl Pts',(53.8454293138304,-23.9257405998152,
2.6005000503458));
#219091=CARTESIAN_POINT('Ctrl Pts',(53.843254179489,-23.9299165195797,2.60003234582321));
#219092=CARTESIAN_POINT('Ctrl Pts',(53.8411336218844,-23.9341422497933,
2.59967776696049));
#219093=CARTESIAN_POINT('Ctrl Pts',(53.8390713992306,-23.9384150933419,
2.59944011429143));
#219094=CARTESIAN_POINT('Ctrl Pts',(53.8370091765769,-23.9426879368906,
2.59920246162237));
#219095=CARTESIAN_POINT('Ctrl Pts',(53.8350052904266,-23.9470078944651,
2.59908173791295));
#219096=CARTESIAN_POINT('Ctrl Pts',(53.8330634946841,-23.9513722670356,
2.59908173516008));
#219097=CARTESIAN_POINT('',(53.8206887816839,-23.9791663275005,2.59908173516007));
#219098=CARTESIAN_POINT('Origin',(5.71744365443249E-15,1.85827062561433E-13,
2.59908173516024));
#219099=CARTESIAN_POINT('',(53.8697418420148,-24.331269253108,2.90134173516007));
#219100=CARTESIAN_POINT('Ctrl Pts',(53.8206887816839,-23.9791663275005,
2.59908173516008));
#219101=CARTESIAN_POINT('Ctrl Pts',(53.8191382997274,-23.9826463618216,
2.59908174371494));
#219102=CARTESIAN_POINT('Ctrl Pts',(53.8176349962322,-23.9861360190788,
2.59915764355873));
#219103=CARTESIAN_POINT('Ctrl Pts',(53.8161786595152,-23.9896330908633,
2.5993076577526));
#219104=CARTESIAN_POINT('Ctrl Pts',(53.8075805576709,-24.0102795382194,
2.60019333020862));
#219105=CARTESIAN_POINT('Ctrl Pts',(53.8006169491717,-24.0311861904745,
2.60365973324056));
#219106=CARTESIAN_POINT('Ctrl Pts',(53.7952474622082,-24.0518926318772,
2.60934177082334));
#219107=CARTESIAN_POINT('Ctrl Pts',(53.7932416006208,-24.0596278690992,
2.61146439091781));
#219108=CARTESIAN_POINT('Ctrl Pts',(53.791457853367,-24.0673353939204,2.61389584429273));
#219109=CARTESIAN_POINT('Ctrl Pts',(53.7898929820051,-24.0749921329669,
2.61661604385235));
#219110=CARTESIAN_POINT('Ctrl Pts',(53.7886719908667,-24.0809663048713,
2.61873848000758));
#219111=CARTESIAN_POINT('Ctrl Pts',(53.7875846446509,-24.086909241038,2.62103707099769));
#219112=CARTESIAN_POINT('Ctrl Pts',(53.7866297945202,-24.0928096561855,
2.62350262767634));
#219113=CARTESIAN_POINT('Ctrl Pts',(53.7832878190625,-24.1134611092019,
2.63213207605161));
#219114=CARTESIAN_POINT('Ctrl Pts',(53.7815689125025,-24.1335916760293,
2.64280685971896));
#219115=CARTESIAN_POINT('Ctrl Pts',(53.7814239018617,-24.1527175379836,
2.65513293646066));
#219116=CARTESIAN_POINT('Ctrl Pts',(53.7813513965413,-24.1622804689607,
2.66129597483151));
#219117=CARTESIAN_POINT('Ctrl Pts',(53.7816723668481,-24.1715922244702,
2.66787183533835));
#219118=CARTESIAN_POINT('Ctrl Pts',(53.7823806708184,-24.1805923292959,
2.67481125953844));
#219119=CARTESIAN_POINT('Ctrl Pts',(53.7830859485795,-24.1895539814227,
2.68172103524063));
#219120=CARTESIAN_POINT('Ctrl Pts',(53.7841750295933,-24.1982067474356,
2.68899101329771));
#219121=CARTESIAN_POINT('Ctrl Pts',(53.7856425347027,-24.206490601869,2.69657334701257));
#219122=CARTESIAN_POINT('Ctrl Pts',(53.7856488314805,-24.2065261462703,
2.69660588132554));
#219123=CARTESIAN_POINT('Ctrl Pts',(53.7856551347357,-24.2065616841174,
2.69663842081363));
#219124=CARTESIAN_POINT('Ctrl Pts',(53.7856614444667,-24.206597215409,2.69667096547363));
#219125=CARTESIAN_POINT('Ctrl Pts',(53.7886369923276,-24.2233530895744,
2.71201840157921));
#219126=CARTESIAN_POINT('Ctrl Pts',(53.7930196670709,-24.2386338146178,
2.7284564593933));
#219127=CARTESIAN_POINT('Ctrl Pts',(53.798615834808,-24.2524209582909,2.74568723186877));
#219128=CARTESIAN_POINT('Ctrl Pts',(53.8044155801162,-24.2667096511229,
2.76354482594304));
#219129=CARTESIAN_POINT('Ctrl Pts',(53.8115193533084,-24.2793947083677,
2.78225519317111));
#219130=CARTESIAN_POINT('Ctrl Pts',(53.8197464933878,-24.2904167802938,
2.80151223085494));
#219131=CARTESIAN_POINT('Ctrl Pts',(53.8278562137183,-24.3012815425224,
2.82049442740233));
#219132=CARTESIAN_POINT('Ctrl Pts',(53.8370583385443,-24.3105307527859,
2.84000929089209));
#219133=CARTESIAN_POINT('Ctrl Pts',(53.8472012967771,-24.3180642992199,
2.85976644341553));
#219134=CARTESIAN_POINT('Ctrl Pts',(53.8542731477179,-24.3233168218286,
2.87354148166897));
#219135=CARTESIAN_POINT('Ctrl Pts',(53.8618028047968,-24.327734457649,2.88743438345454));
#219136=CARTESIAN_POINT('Ctrl Pts',(53.8697418420148,-24.331269253108,2.90134173516007));
#219137=CARTESIAN_POINT('',(54.1952354911875,-24.4761921430384,3.47153072139056));
#219138=CARTESIAN_POINT('',(53.8697418420148,-24.331269253108,2.90134173516007));
#219139=CARTESIAN_POINT('',(51.6568155675431,-29.4581217525665,3.47153072139052));
#219140=CARTESIAN_POINT('Origin',(5.53234440788222E-15,1.85015204418142E-13,
3.47153072139072));
#219141=CARTESIAN_POINT('',(51.3482501200169,-29.2799753962454,2.90134173516004));
#219142=CARTESIAN_POINT('',(51.6568155675431,-29.4581217525665,3.47153072139052));
#219143=CARTESIAN_POINT('',(51.0345602039891,-29.4472515437727,2.59908173516003));
#219144=CARTESIAN_POINT('Ctrl Pts',(51.3482501200169,-29.2799753962454,
2.90134173516004));
#219145=CARTESIAN_POINT('Ctrl Pts',(51.3376585930517,-29.2738605406098,
2.88176998919757));
#219146=CARTESIAN_POINT('Ctrl Pts',(51.3261534914777,-29.269437766393,2.86226752356645));
#219147=CARTESIAN_POINT('Ctrl Pts',(51.3139160033708,-29.266725042103,2.84310370499914));
#219148=CARTESIAN_POINT('Ctrl Pts',(51.3014574615393,-29.2639633161059,
2.82359371788522));
#219149=CARTESIAN_POINT('Ctrl Pts',(51.2882390496566,-29.2629734853262,
2.80443322636835));
#219150=CARTESIAN_POINT('Ctrl Pts',(51.2744188030426,-29.2638161685318,
2.78589323878069));
#219151=CARTESIAN_POINT('Ctrl Pts',(51.2611836698378,-29.2646231747154,
2.76813818619779));
#219152=CARTESIAN_POINT('Ctrl Pts',(51.2473957191175,-29.267110757666,2.75095095198469));
#219153=CARTESIAN_POINT('Ctrl Pts',(51.2331761176611,-29.271373305682,2.73457771434851));
#219154=CARTESIAN_POINT('Ctrl Pts',(51.2218663142633,-29.2747635962033,
2.72155497955398));
#219155=CARTESIAN_POINT('Ctrl Pts',(51.2102829897272,-29.2792774508354,
2.70904711159866));
#219156=CARTESIAN_POINT('Ctrl Pts',(51.1984837018595,-29.2849828273421,
2.69718956158318));
#219157=CARTESIAN_POINT('Ctrl Pts',(51.1984514936364,-29.2849984011667,
2.69715719432336));
#219158=CARTESIAN_POINT('Ctrl Pts',(51.1984192839706,-29.2850139839317,
2.69712483219002));
#219159=CARTESIAN_POINT('Ctrl Pts',(51.1983870728642,-29.2850295756377,
2.6970924751863));
#219160=CARTESIAN_POINT('Ctrl Pts',(51.1919748636256,-29.2881333895818,
2.69065122242256));
#219161=CARTESIAN_POINT('Ctrl Pts',(51.1854935419305,-29.29162601106,2.68442464469405));
#219162=CARTESIAN_POINT('Ctrl Pts',(51.1789779411681,-29.2954867606371,
2.67844505923558));
#219163=CARTESIAN_POINT('Ctrl Pts',(51.1660472802373,-29.3031486855372,
2.66657815779546));
#219164=CARTESIAN_POINT('Ctrl Pts',(51.1529811529982,-29.3122618143328,
2.65568445664152));
#219165=CARTESIAN_POINT('Ctrl Pts',(51.1400491105588,-29.3226724463005,
2.64601906229494));
#219166=CARTESIAN_POINT('Ctrl Pts',(51.1303500787293,-29.3304804202763,
2.638770016535));
#219167=CARTESIAN_POINT('Ctrl Pts',(51.1207264688924,-29.3390182393868,
2.63221189387581));
#219168=CARTESIAN_POINT('Ctrl Pts',(51.1112920078095,-29.3482210667391,
2.62645231033213));
#219169=CARTESIAN_POINT('Ctrl Pts',(51.1077540849034,-29.3516721269962,
2.62429246650325));
#219170=CARTESIAN_POINT('Ctrl Pts',(51.1042427612076,-29.3552167041318,
2.62224491711724));
#219171=CARTESIAN_POINT('Ctrl Pts',(51.1007640347392,-29.3588513794152,
2.62031533672576));
#219172=CARTESIAN_POINT('Ctrl Pts',(51.0885884920996,-29.371572742907,2.61356180535557));
#219173=CARTESIAN_POINT('Ctrl Pts',(51.0768122611,-29.3853978061634,2.60825339735327));
#219174=CARTESIAN_POINT('Ctrl Pts',(51.0656925470316,-29.4001800143149,
2.6046333798759));
#219175=CARTESIAN_POINT('Ctrl Pts',(51.0601326899974,-29.4075711183907,
2.60282337113721));
#219176=CARTESIAN_POINT('Ctrl Pts',(51.0547369630771,-29.4152015092018,
2.60143545939095));
#219177=CARTESIAN_POINT('Ctrl Pts',(51.0495375206698,-29.4230528695796,
2.60050005034576));
#219178=CARTESIAN_POINT('Ctrl Pts',(51.0469377994662,-29.4269785497685,
2.60003234582316));
#219179=CARTESIAN_POINT('Ctrl Pts',(51.0443871494126,-29.4309594723622,
2.59967776696045));
#219180=CARTESIAN_POINT('Ctrl Pts',(51.0418895900604,-29.4349933478619,
2.59944011429139));
#219181=CARTESIAN_POINT('Ctrl Pts',(51.0393920307082,-29.4390272233617,
2.59920246162233));
#219182=CARTESIAN_POINT('Ctrl Pts',(51.0369475635293,-29.4431140526167,
2.59908173791293));
#219183=CARTESIAN_POINT('Ctrl Pts',(51.0345602039891,-29.4472515437727,
2.59908173516004));
#219184=CARTESIAN_POINT('',(51.0193480105331,-29.4735998357329,2.59908173516003));
#219185=CARTESIAN_POINT('Origin',(5.71420591410065E-15,1.85820708138243E-13,
2.59908173516023));
#219186=CARTESIAN_POINT('',(51.0313275753413,-29.8289013456877,2.90134173516003));
#219187=CARTESIAN_POINT('Ctrl Pts',(51.0193480105332,-29.4735998357329,
2.59908173516004));
#219188=CARTESIAN_POINT('Ctrl Pts',(51.0174422596394,-29.4768987365657,
2.59908174371493));
#219189=CARTESIAN_POINT('Ctrl Pts',(51.0155824228875,-29.4802121391111,
2.59915764355871));
#219190=CARTESIAN_POINT('Ctrl Pts',(51.0137685205959,-29.4835378249314,
2.59930765775257));
#219191=CARTESIAN_POINT('Ctrl Pts',(51.003059378638,-29.5031724225179,2.60019333020868));
#219192=CARTESIAN_POINT('Ctrl Pts',(50.9939485772817,-29.5232366506513,
2.60365973324125));
#219193=CARTESIAN_POINT('Ctrl Pts',(50.9864440924295,-29.5432683957827,
2.60934177082507));
#219194=CARTESIAN_POINT('Ctrl Pts',(50.9836406667028,-29.5507515889345,
2.61146439091913));
#219195=CARTESIAN_POINT('Ctrl Pts',(50.9810610352787,-29.5582304387669,
2.61389584429345));
#219196=CARTESIAN_POINT('Ctrl Pts',(50.9787043892804,-29.565681659795,2.61661604385232));
#219197=CARTESIAN_POINT('Ctrl Pts',(50.9768656158508,-29.5714954762333,
2.61873848000755));
#219198=CARTESIAN_POINT('Ctrl Pts',(50.9751630202465,-29.5772921977449,
2.62103707099767));
#219199=CARTESIAN_POINT('Ctrl Pts',(50.9735966395567,-29.583060480784,2.62350262767631));
#219200=CARTESIAN_POINT('Ctrl Pts',(50.9681143071422,-29.6032494714211,
2.63213207605158));
#219201=CARTESIAN_POINT('Ctrl Pts',(50.964300599717,-29.623090086236,2.64280685971894));
#219202=CARTESIAN_POINT('Ctrl Pts',(50.9621571865009,-29.6420960169778,
2.65513293646064));
#219203=CARTESIAN_POINT('Ctrl Pts',(50.9610854798929,-29.6515989823488,
2.66129597483149));
#219204=CARTESIAN_POINT('Ctrl Pts',(50.960431348397,-29.6608932776201,2.66787183533831));
#219205=CARTESIAN_POINT('Ctrl Pts',(50.9601950050773,-29.6699181168554,
2.6748112595384));
#219206=CARTESIAN_POINT('Ctrl Pts',(50.959959671528,-29.6789043977148,2.68172103524059));
#219207=CARTESIAN_POINT('Ctrl Pts',(50.9601383261077,-29.6876236029349,
2.68899101329768));
#219208=CARTESIAN_POINT('Ctrl Pts',(50.9607318934967,-29.6960154736008,
2.69657334701254));
#219209=CARTESIAN_POINT('Ctrl Pts',(50.9607344403784,-29.6960514814787,
2.69660588132551));
#219210=CARTESIAN_POINT('Ctrl Pts',(50.9607369943872,-29.6960874835153,
2.69663842081359));
#219211=CARTESIAN_POINT('Ctrl Pts',(50.9607395555215,-29.6961234797093,
2.6966709654736));
#219212=CARTESIAN_POINT('Ctrl Pts',(50.9619473372425,-29.7130985928864,
2.71201840157765));
#219213=CARTESIAN_POINT('Ctrl Pts',(50.9647087325282,-29.7287537227736,
2.72845645938998));
#219214=CARTESIAN_POINT('Ctrl Pts',(50.9688330949313,-29.7430502978437,
2.74568723186358));
#219215=CARTESIAN_POINT('Ctrl Pts',(50.9731074935233,-29.7578669541845,
2.76354482593602));
#219216=CARTESIAN_POINT('Ctrl Pts',(50.9788464019616,-29.7712250678528,
2.78225519316214));
#219217=CARTESIAN_POINT('Ctrl Pts',(50.9858763526652,-29.7830467300247,
2.80151223084397));
#219218=CARTESIAN_POINT('Ctrl Pts',(50.9928059701987,-29.7946996705523,
2.82049442738972));
#219219=CARTESIAN_POINT('Ctrl Pts',(51.0009908790856,-29.8048600966411,
2.84000929087781));
#219220=CARTESIAN_POINT('Ctrl Pts',(51.0102908030989,-29.8134126013568,
2.85976644339964));
#219221=CARTESIAN_POINT('Ctrl Pts',(51.0167748755858,-29.8193755598113,
2.87354148165827));
#219222=CARTESIAN_POINT('Ctrl Pts',(51.0238015157343,-29.8245560588462,
2.88743438344917));
#219223=CARTESIAN_POINT('Ctrl Pts',(51.0313275753413,-29.8289013456877,
2.90134173516003));
#219224=CARTESIAN_POINT('',(51.3398895692701,-30.007053683815,3.47153072139052));
#219225=CARTESIAN_POINT('',(51.0313275753413,-29.8289013456877,2.90134173516003));
#219226=CARTESIAN_POINT('',(48.2946219293751,-34.6963546279277,3.47153072139049));
#219227=CARTESIAN_POINT('Origin',(5.53234440788222E-15,1.85015204418142E-13,
3.47153072139072));
#219228=CARTESIAN_POINT('',(48.0063682005191,-34.4869303039389,2.90134173516));
#219229=CARTESIAN_POINT('',(48.2946219293751,-34.6963546279277,3.47153072139049));
#219230=CARTESIAN_POINT('',(47.6769115920308,-34.6205005703627,2.59908173516));
#219231=CARTESIAN_POINT('Ctrl Pts',(48.0063682005191,-34.4869303039389,
2.90134173516));
#219232=CARTESIAN_POINT('Ctrl Pts',(47.9964738715105,-34.4797418300855,
2.88176998919937));
#219233=CARTESIAN_POINT('Ctrl Pts',(47.9854941018801,-34.4741406737017,
2.86226752357008));
#219234=CARTESIAN_POINT('Ctrl Pts',(47.9736072089161,-34.4701636441732,
2.84310370500451));
#219235=CARTESIAN_POINT('Ctrl Pts',(47.961505595256,-34.4661147749679,2.82359371789228));
#219236=CARTESIAN_POINT('Ctrl Pts',(47.9484630607083,-34.4637486663037,
2.80443322637702));
#219237=CARTESIAN_POINT('Ctrl Pts',(47.9346304384724,-34.4631421240614,
2.78589323879081));
#219238=CARTESIAN_POINT('Ctrl Pts',(47.9213834535972,-34.462561261245,2.76813818620915));
#219239=CARTESIAN_POINT('Ctrl Pts',(47.9074110114921,-34.4635939836547,
2.75095095199715));
#219240=CARTESIAN_POINT('Ctrl Pts',(47.8928237489081,-34.4663468278971,
2.73457771436186));
#219241=CARTESIAN_POINT('Ctrl Pts',(47.8812215199347,-34.4685363496832,
2.72155497956252));
#219242=CARTESIAN_POINT('Ctrl Pts',(47.8692298237703,-34.4718146898347,
2.70904711160269));
#219243=CARTESIAN_POINT('Ctrl Pts',(47.8568987993932,-34.476255450265,2.69718956158315));
#219244=CARTESIAN_POINT('Ctrl Pts',(47.8568651397022,-34.4762675720985,
2.69715719432332));
#219245=CARTESIAN_POINT('Ctrl Pts',(47.8568314776419,-34.4762797026727,
2.69712483218998));
#219246=CARTESIAN_POINT('Ctrl Pts',(47.8567978132142,-34.4762918419882,
2.69709247518626));
#219247=CARTESIAN_POINT('Ctrl Pts',(47.8500962938269,-34.4787083945369,
2.69065122242252));
#219248=CARTESIAN_POINT('Ctrl Pts',(47.8432853991343,-34.4815044004724,
2.68442464469402));
#219249=CARTESIAN_POINT('Ctrl Pts',(47.8364019332942,-34.4846629347244,
2.67844505923554));
#219250=CARTESIAN_POINT('Ctrl Pts',(47.8227412186415,-34.4909312646821,
2.66657815779542));
#219251=CARTESIAN_POINT('Ctrl Pts',(47.808794087666,-34.4986286886035,2.65568445664149));
#219252=CARTESIAN_POINT('Ctrl Pts',(47.794844680947,-34.5076305235169,2.64601906229491));
#219253=CARTESIAN_POINT('Ctrl Pts',(47.7843826259077,-34.5143818997019,
2.63877001653497));
#219254=CARTESIAN_POINT('Ctrl Pts',(47.7739192901011,-34.5218670065987,
2.63221189387577));
#219255=CARTESIAN_POINT('Ctrl Pts',(47.7635745545823,-34.5300332501811,
2.62645231033209));
#219256=CARTESIAN_POINT('Ctrl Pts',(47.7596952787628,-34.5330955915245,
2.62429246650321));
#219257=CARTESIAN_POINT('Ctrl Pts',(47.7558326812647,-34.5362537178257,
2.62224491711721));
#219258=CARTESIAN_POINT('Ctrl Pts',(47.751993084602,-34.5395048560457,2.62031533672573));
#219259=CARTESIAN_POINT('Ctrl Pts',(47.7385544962824,-34.5508838398157,
2.61356180535554));
#219260=CARTESIAN_POINT('Ctrl Pts',(47.7253976640916,-34.5634022165996,
2.60825339735323));
#219261=CARTESIAN_POINT('Ctrl Pts',(47.7127937034786,-34.5769411196446,
2.60463337987586));
#219262=CARTESIAN_POINT('Ctrl Pts',(47.7064917231721,-34.5837105711672,
2.60282337113718));
#219263=CARTESIAN_POINT('Ctrl Pts',(47.7003279615829,-34.5907351548558,
2.6014354593909));
#219264=CARTESIAN_POINT('Ctrl Pts',(47.6943363116302,-34.5980000149353,
2.60050005034571));
#219265=CARTESIAN_POINT('Ctrl Pts',(47.6913404866539,-34.601632444975,2.60003234582311));
#219266=CARTESIAN_POINT('Ctrl Pts',(47.6883876896072,-34.6053249441278,
2.59967776696041));
#219267=CARTESIAN_POINT('Ctrl Pts',(47.6854821573394,-34.6090756555945,
2.59944011429135));
#219268=CARTESIAN_POINT('Ctrl Pts',(47.6825766250716,-34.6128263670611,
2.59920246162229));
#219269=CARTESIAN_POINT('Ctrl Pts',(47.679718358958,-34.6166352918402,2.59908173791286));
#219270=CARTESIAN_POINT('Ctrl Pts',(47.6769115920308,-34.6205005703627,
2.59908173516));
#219271=CARTESIAN_POINT('',(47.659028586094,-34.6451144164178,2.59908173516));
#219272=CARTESIAN_POINT('Origin',(5.71032169235817E-15,1.8581472696127E-13,
2.59908173516024));
#219273=CARTESIAN_POINT('',(47.6338034047604,-34.9997217530253,2.90134173515999));
#219274=CARTESIAN_POINT('Ctrl Pts',(47.659028586094,-34.6451144164178,2.59908173516));
#219275=CARTESIAN_POINT('Ctrl Pts',(47.6567884460685,-34.6481960403143,
2.59908174371483));
#219276=CARTESIAN_POINT('Ctrl Pts',(47.6545924528207,-34.6512968858163,
2.59915764355865));
#219277=CARTESIAN_POINT('Ctrl Pts',(47.6524408584475,-34.6544147487627,
2.59930765775252));
#219278=CARTESIAN_POINT('Ctrl Pts',(47.6397380079788,-34.6728223758151,
2.60019333020852));
#219279=CARTESIAN_POINT('Ctrl Pts',(47.6285798336134,-34.69182435194,2.60365973324032));
#219280=CARTESIAN_POINT('Ctrl Pts',(47.6190225715801,-34.710961928804,2.60934177082287));
#219281=CARTESIAN_POINT('Ctrl Pts',(47.615452296631,-34.71811109046,2.61146439091744));
#219282=CARTESIAN_POINT('Ctrl Pts',(47.6121050440166,-34.7252793254644,
2.6138958442925));
#219283=CARTESIAN_POINT('Ctrl Pts',(47.608982443287,-34.7324433913419,2.61661604385228));
#219284=CARTESIAN_POINT('Ctrl Pts',(47.6065460335526,-34.7380331549245,
2.61873848000751));
#219285=CARTESIAN_POINT('Ctrl Pts',(47.6042468425536,-34.743620151687,2.62103707099763));
#219286=CARTESIAN_POINT('Ctrl Pts',(47.6020860928993,-34.7491931041017,
2.62350262767627));
#219287=CARTESIAN_POINT('Ctrl Pts',(47.5945234691092,-34.7686984375533,
2.63213207605154));
#219288=CARTESIAN_POINT('Ctrl Pts',(47.5886567445954,-34.7880317224277,
2.64280685971889));
#219289=CARTESIAN_POINT('Ctrl Pts',(47.5845384124878,-34.8067094890027,
2.65513293646059));
#219290=CARTESIAN_POINT('Ctrl Pts',(47.582479246434,-34.8160483722902,2.66129597483144));
#219291=CARTESIAN_POINT('Ctrl Pts',(47.580857179937,-34.8252233770796,2.66787183533828));
#219292=CARTESIAN_POINT('Ctrl Pts',(47.5796787787543,-34.8341740726973,
2.67481125953837));
#219293=CARTESIAN_POINT('Ctrl Pts',(47.578505412258,-34.8430865267156,2.68172103524056));
#219294=CARTESIAN_POINT('Ctrl Pts',(47.5777716830267,-34.8517766417058,
2.68899101329765));
#219295=CARTESIAN_POINT('Ctrl Pts',(47.5774848094468,-34.8601845855132,
2.6965733470125));
#219296=CARTESIAN_POINT('Ctrl Pts',(47.5774835785283,-34.8602206623578,
2.69660588132548));
#219297=CARTESIAN_POINT('Ctrl Pts',(47.5774823553084,-34.8602567341381,
2.69663842081356));
#219298=CARTESIAN_POINT('Ctrl Pts',(47.5774811397857,-34.8602928008526,
2.69667096547357));
#219299=CARTESIAN_POINT('Ctrl Pts',(47.5769079226578,-34.8773011701513,
2.71201840157807));
#219300=CARTESIAN_POINT('Ctrl Pts',(47.578017784062,-34.8931591840051,2.72845645939092));
#219301=CARTESIAN_POINT('Ctrl Pts',(47.5806251537543,-34.9078085542054,
2.74568723186507));
#219302=CARTESIAN_POINT('Ctrl Pts',(47.5833273744258,-34.922990839669,2.76354482593811));
#219303=CARTESIAN_POINT('Ctrl Pts',(47.5876385414295,-34.9368756554732,
2.78225519316489));
#219304=CARTESIAN_POINT('Ctrl Pts',(47.5933942811479,-34.9493673872869,
2.80151223084739));
#219305=CARTESIAN_POINT('Ctrl Pts',(47.599067873546,-34.9616808340591,2.8204944273939));
#219306=CARTESIAN_POINT('Ctrl Pts',(47.6061458909209,-34.9726411562187,
2.84000929088276));
#219307=CARTESIAN_POINT('Ctrl Pts',(47.6145008888029,-34.9821189161845,
2.85976644340536));
#219308=CARTESIAN_POINT('Ctrl Pts',(47.6203261419778,-34.9887269790603,
2.87354148166211));
#219309=CARTESIAN_POINT('Ctrl Pts',(47.6267727798524,-34.9946135826752,
2.88743438345107));
#219310=CARTESIAN_POINT('Ctrl Pts',(47.6338034047604,-34.9997217530253,
2.90134173515999));
#219311=CARTESIAN_POINT('',(47.9220530736691,-35.209151665052,3.47153072139048));
#219312=CARTESIAN_POINT('',(47.6338034047604,-34.9997217530253,2.90134173515999));
#219313=CARTESIAN_POINT('',(44.4033023070494,-39.5544469813064,3.47153072139045));
#219314=CARTESIAN_POINT('Origin',(5.53234440788222E-15,1.85015204418142E-13,
3.47153072139072));
#219315=CARTESIAN_POINT('',(44.1385184650381,-39.3160391863683,2.90134173515996));
#219316=CARTESIAN_POINT('',(44.4033023070494,-39.5544469813064,3.47153072139045));
#219317=CARTESIAN_POINT('',(43.7969047596351,-39.4144401478983,2.59908173515996));
#219318=CARTESIAN_POINT('Ctrl Pts',(44.1385184650381,-39.3160391863683,
2.90134173515997));
#219319=CARTESIAN_POINT('Ctrl Pts',(44.1294297383231,-39.3078558527201,
2.88176998919776));
#219320=CARTESIAN_POINT('Ctrl Pts',(44.1190955972879,-39.3011376816103,
2.8622675235669));
#219321=CARTESIAN_POINT('Ctrl Pts',(44.1076895347511,-39.2959399200109,
2.84310370499984));
#219322=CARTESIAN_POINT('Ctrl Pts',(44.0960774370719,-39.2906482678558,
2.82359371788642));
#219323=CARTESIAN_POINT('Ctrl Pts',(44.0833536765948,-39.2869318048891,
2.80443322637003));
#219324=CARTESIAN_POINT('Ctrl Pts',(44.0696602318382,-39.2848826826036,
2.78589323878281));
#219325=CARTESIAN_POINT('Ctrl Pts',(44.0565465320292,-39.2829203148429,
2.76813818620078));
#219326=CARTESIAN_POINT('Ctrl Pts',(44.0425426835367,-39.2824868619903,
2.75095095198847));
#219327=CARTESIAN_POINT('Ctrl Pts',(44.0277475809245,-39.2836998417232,
2.73457771435298));
#219328=CARTESIAN_POINT('Ctrl Pts',(44.0159800428303,-39.284664605915,2.72155497955682));
#219329=CARTESIAN_POINT('Ctrl Pts',(44.0037113585768,-39.2866715134038,
2.70904711159996));
#219330=CARTESIAN_POINT('Ctrl Pts',(43.9909836989808,-39.2897990038545,
2.69718956158311));
#219331=CARTESIAN_POINT('Ctrl Pts',(43.9909489566045,-39.2898075408876,
2.69715719432328));
#219332=CARTESIAN_POINT('Ctrl Pts',(43.9909142109582,-39.2898160863657,
2.69712483218994));
#219333=CARTESIAN_POINT('Ctrl Pts',(43.9908794620438,-39.28982464029,2.69709247518622));
#219334=CARTESIAN_POINT('Ctrl Pts',(43.9839620557566,-39.2915274551878,
2.69065122242248));
#219335=CARTESIAN_POINT('Ctrl Pts',(43.976896209654,-39.2935962119545,2.68442464469397));
#219336=CARTESIAN_POINT('Ctrl Pts',(43.9697202954285,-39.2960179253192,
2.67844505923549));
#219337=CARTESIAN_POINT('Ctrl Pts',(43.9554791967022,-39.3008239831998,
2.66657815779538));
#219338=CARTESIAN_POINT('Ctrl Pts',(43.9408038696759,-39.3070213676597,
2.65568445664144));
#219339=CARTESIAN_POINT('Ctrl Pts',(43.9259899312963,-39.3145157795317,
2.64601906229486));
#219340=CARTESIAN_POINT('Ctrl Pts',(43.9148794775117,-39.3201365884357,
2.63877001653492));
#219341=CARTESIAN_POINT('Ctrl Pts',(43.9036910542322,-39.3264869747212,
2.63221189387573));
#219342=CARTESIAN_POINT('Ctrl Pts',(43.8925493833646,-39.3335271634601,
2.62645231033205));
#219343=CARTESIAN_POINT('Ctrl Pts',(43.8883712567893,-39.3361672342372,
2.62429246650317));
#219344=CARTESIAN_POINT('Ctrl Pts',(43.8841997049153,-39.3389043086114,
2.62224491711717));
#219345=CARTESIAN_POINT('Ctrl Pts',(43.8800413054829,-39.3417362896173,
2.62031533672569));
#219346=CARTESIAN_POINT('Ctrl Pts',(43.8654869074692,-39.3516482231381,
2.6135618053555));
#219347=CARTESIAN_POINT('Ctrl Pts',(43.851093623094,-39.3627227594938,2.6082533973532));
#219348=CARTESIAN_POINT('Ctrl Pts',(43.8371435075663,-39.3748700223774,
2.60463337987583));
#219349=CARTESIAN_POINT('Ctrl Pts',(43.8301684498025,-39.3809436538192,
2.60282337113715));
#219350=CARTESIAN_POINT('Ctrl Pts',(43.8233041850061,-39.3872854675765,
2.60143545939088));
#219351=CARTESIAN_POINT('Ctrl Pts',(43.8165859732789,-39.3938842320304,
2.60050005034569));
#219352=CARTESIAN_POINT('Ctrl Pts',(43.8132268674153,-39.3971836142573,
2.6000323458231));
#219353=CARTESIAN_POINT('Ctrl Pts',(43.8099042748376,-39.4005472341757,
2.59967776696038));
#219354=CARTESIAN_POINT('Ctrl Pts',(43.8066226032739,-39.4039736880296,
2.59944011429132));
#219355=CARTESIAN_POINT('Ctrl Pts',(43.8033409317101,-39.4074001418835,
2.59920246162226));
#219356=CARTESIAN_POINT('Ctrl Pts',(43.8001001824234,-39.4108894308096,
2.5990817379128));
#219357=CARTESIAN_POINT('Ctrl Pts',(43.7969047596351,-39.4144401478983,
2.59908173515997));
#219358=CARTESIAN_POINT('',(43.7765468711727,-39.4370498736001,2.59908173515996));
#219359=CARTESIAN_POINT('Origin',(5.7058335455513E-15,1.8580918456154E-13,
2.59908173516024));
#219360=CARTESIAN_POINT('',(43.7143933160628,-39.787077884674,2.90134173515997));
#219361=CARTESIAN_POINT('Ctrl Pts',(43.7765468711727,-39.4370498736001,
2.59908173515997));
#219362=CARTESIAN_POINT('Ctrl Pts',(43.7739968854584,-39.4398804576441,
2.59908174371481));
#219363=CARTESIAN_POINT('Ctrl Pts',(43.7714887954762,-39.4427347725904,
2.59915764355863));
#219364=CARTESIAN_POINT('Ctrl Pts',(43.7690230823397,-39.445610652704,2.59930765775249));
#219365=CARTESIAN_POINT('Ctrl Pts',(43.7544656984445,-39.4625896314133,
2.60019333020863));
#219366=CARTESIAN_POINT('Ctrl Pts',(43.7413824023606,-39.4803211659083,
2.60365973324136));
#219367=CARTESIAN_POINT('Ctrl Pts',(43.7298770745073,-39.4983548992134,
2.60934177082543));
#219368=CARTESIAN_POINT('Ctrl Pts',(43.7255790670182,-39.5050917016572,
2.6114643909194));
#219369=CARTESIAN_POINT('Ctrl Pts',(43.7215008664163,-39.5118707851455,
2.61389584429358));
#219370=CARTESIAN_POINT('Ctrl Pts',(43.7176465228248,-39.5186692048621,
2.61661604385227));
#219371=CARTESIAN_POINT('Ctrl Pts',(43.7146391706006,-39.5239736729695,
2.6187384800075));
#219372=CARTESIAN_POINT('Ctrl Pts',(43.7117685746246,-39.5292897326773,
2.62103707099761));
#219373=CARTESIAN_POINT('Ctrl Pts',(43.7090371296312,-39.5346062960347,
2.62350262767626));
#219374=CARTESIAN_POINT('Ctrl Pts',(43.6994770721543,-39.5532142677857,
2.63213207605152));
#219375=CARTESIAN_POINT('Ctrl Pts',(43.6916216076134,-39.5718284032049,
2.64280685971888));
#219376=CARTESIAN_POINT('Ctrl Pts',(43.6855734779227,-39.5899733680939,
2.65513293646057));
#219377=CARTESIAN_POINT('Ctrl Pts',(43.6825494130773,-39.5990458505383,
2.66129597483142));
#219378=CARTESIAN_POINT('Ctrl Pts',(43.6799771832791,-39.6080010415732,
2.66787183533825));
#219379=CARTESIAN_POINT('Ctrl Pts',(43.6778696350433,-39.616779527879,2.67481125953834));
#219380=CARTESIAN_POINT('Ctrl Pts',(43.675771091249,-39.625520508345,2.68172103524052));
#219381=CARTESIAN_POINT('Ctrl Pts',(43.6741330170976,-39.634086322387,2.68899101329759));
#219382=CARTESIAN_POINT('Ctrl Pts',(43.6729688455957,-39.6424182201441,
2.69657334701245));
#219383=CARTESIAN_POINT('Ctrl Pts',(43.6729638503632,-39.6424539706899,
2.69660588132542));
#219384=CARTESIAN_POINT('Ctrl Pts',(43.6729588633165,-39.6424897170039,
2.6966384208135));
#219385=CARTESIAN_POINT('Ctrl Pts',(43.6729538844543,-39.6425254590845,
2.69667096547351));
#219386=CARTESIAN_POINT('Ctrl Pts',(43.6706059487642,-39.6593807372523,
2.71201840157909));
#219387=CARTESIAN_POINT('Ctrl Pts',(43.6700521164129,-39.675267891355,2.72845645939318));
#219388=CARTESIAN_POINT('Ctrl Pts',(43.6711139265067,-39.6901095551206,
2.74568723186866));
#219389=CARTESIAN_POINT('Ctrl Pts',(43.6722143631624,-39.7054911294111,
2.76354482594304));
#219390=CARTESIAN_POINT('Ctrl Pts',(43.675050554684,-39.719750522404,2.78225519317123));
#219391=CARTESIAN_POINT('Ctrl Pts',(43.6794690223286,-39.7327754618321,
2.80151223085518));
#219392=CARTESIAN_POINT('Ctrl Pts',(43.6838244285259,-39.7456145061494,
2.8204944274028));
#219393=CARTESIAN_POINT('Ctrl Pts',(43.6897180061495,-39.7572546407968,
2.8400092908928));
#219394=CARTESIAN_POINT('Ctrl Pts',(43.6970365387954,-39.767553815691,2.85976644341649));
#219395=CARTESIAN_POINT('Ctrl Pts',(43.7021391499654,-39.7747345836671,
2.87354148166958));
#219396=CARTESIAN_POINT('Ctrl Pts',(43.7079351548522,-39.7812627969998,
2.88743438345479));
#219397=CARTESIAN_POINT('Ctrl Pts',(43.7143933160628,-39.787077884674,2.90134173515996));
#219398=CARTESIAN_POINT('',(43.9791725362587,-40.0254908126581,3.47153072139045));
#219399=CARTESIAN_POINT('',(43.7143933160628,-39.787077884674,2.90134173515997));
#219400=CARTESIAN_POINT('',(40.0254908126594,-43.9791725362576,3.47153072139042));
#219401=CARTESIAN_POINT('Origin',(5.53234440788222E-15,1.85015204418142E-13,
3.47153072139072));
#219402=CARTESIAN_POINT('',(39.7870778846752,-43.7143933160617,2.90134173515994));
#219403=CARTESIAN_POINT('',(40.0254908126594,-43.9791725362576,3.47153072139042));
#219404=CARTESIAN_POINT('',(39.4370498736014,-43.7765468711716,2.59908173515993));
#219405=CARTESIAN_POINT('Ctrl Pts',(39.7870778846752,-43.7143933160617,
2.90134173515994));
#219406=CARTESIAN_POINT('Ctrl Pts',(39.7788943382472,-43.7053047809349,
2.8817699891982));
#219407=CARTESIAN_POINT('Ctrl Pts',(39.7693190488203,-43.6975432007878,
2.86226752356781));
#219408=CARTESIAN_POINT('Ctrl Pts',(39.7585187839203,-43.6911816548816,
2.84310370500119));
#219409=CARTESIAN_POINT('Ctrl Pts',(39.7475234267954,-43.6847051962249,
2.82359371788803));
#219410=CARTESIAN_POINT('Ctrl Pts',(39.7352578445723,-43.6796790973015,
2.80443322637188));
#219411=CARTESIAN_POINT('Ctrl Pts',(39.7218536055427,-43.6762098455851,
2.78589323878489));
#219412=CARTESIAN_POINT('Ctrl Pts',(39.7090168672396,-43.6728874729914,
2.76813818620265));
#219413=CARTESIAN_POINT('Ctrl Pts',(39.6951350414549,-43.670992593876,2.75095095199014));
#219414=CARTESIAN_POINT('Ctrl Pts',(39.6802941970553,-43.670652419439,2.73457771435445));
#219415=CARTESIAN_POINT('Ctrl Pts',(39.6684902774472,-43.6703818558782,
2.72155497955776));
#219416=CARTESIAN_POINT('Ctrl Pts',(39.6560790233735,-43.6710953426065,
2.70904711160041));
#219417=CARTESIAN_POINT('Ctrl Pts',(39.6430941754573,-43.6728752976388,
2.6971895615831));
#219418=CARTESIAN_POINT('Ctrl Pts',(39.6430587310404,-43.6728801563378,
2.69715719432327));
#219419=CARTESIAN_POINT('Ctrl Pts',(39.6430232824887,-43.672885023094,2.69712483218993));
#219420=CARTESIAN_POINT('Ctrl Pts',(39.642987829804,-43.6728898979083,2.69709247518621));
#219421=CARTESIAN_POINT('Ctrl Pts',(39.6359303251676,-43.673860318759,2.69065122242247));
#219422=CARTESIAN_POINT('Ctrl Pts',(39.6286869425436,-43.6751791606249,
2.68442464469395));
#219423=CARTESIAN_POINT('Ctrl Pts',(39.6212972007506,-43.6768375203038,
2.67844505923548));
#219424=CARTESIAN_POINT('Ctrl Pts',(39.6066317464086,-43.6801286499313,
2.66657815779536));
#219425=CARTESIAN_POINT('Ctrl Pts',(39.5913890092854,-43.6847580950887,
2.65568445664143));
#219426=CARTESIAN_POINT('Ctrl Pts',(39.5758728438542,-43.6906629735746,
2.64601906229485));
#219427=CARTESIAN_POINT('Ctrl Pts',(39.5642357197808,-43.695091632439,2.63877001653491));
#219428=CARTESIAN_POINT('Ctrl Pts',(39.5524447917351,-43.7002377219522,
2.63221189387571));
#219429=CARTESIAN_POINT('Ctrl Pts',(39.5406282559963,-43.7060747220665,
2.62645231033202));
#219430=CARTESIAN_POINT('Ctrl Pts',(39.5361970550943,-43.7082635971094,
2.62429246650314));
#219431=CARTESIAN_POINT('Ctrl Pts',(39.5317622532398,-43.7105496315969,
2.62224491711714));
#219432=CARTESIAN_POINT('Ctrl Pts',(39.527330611332,-43.7129314276123,2.62031533672566));
#219433=CARTESIAN_POINT('Ctrl Pts',(39.5118198646546,-43.721267713666,2.61356180535547));
#219434=CARTESIAN_POINT('Ctrl Pts',(39.4963478239305,-43.7307770746556,
2.60825339735317));
#219435=CARTESIAN_POINT('Ctrl Pts',(39.4812043938732,-43.7413996094237,
2.6046333798758));
#219436=CARTESIAN_POINT('Ctrl Pts',(39.4736326788445,-43.7467108768077,
2.60282337113712));
#219437=CARTESIAN_POINT('Ctrl Pts',(39.4661431171625,-43.752300438395,2.60143545939084));
#219438=CARTESIAN_POINT('Ctrl Pts',(39.4587719497942,-43.758160809779,2.60050005034565));
#219439=CARTESIAN_POINT('Ctrl Pts',(39.4550863661101,-43.761090995471,2.60003234582306));
#219440=CARTESIAN_POINT('Ctrl Pts',(39.4514303810211,-43.7640888836314,
2.59967776696035));
#219441=CARTESIAN_POINT('Ctrl Pts',(39.4478085248418,-43.767153538927,2.59944011429129));
#219442=CARTESIAN_POINT('Ctrl Pts',(39.4441866686624,-43.7702181942226,
2.59920246162223));
#219443=CARTESIAN_POINT('Ctrl Pts',(39.4405989425301,-43.7733496179162,
2.59908173791281));
#219444=CARTESIAN_POINT('Ctrl Pts',(39.4370498736014,-43.7765468711716,
2.59908173515994));
#219445=CARTESIAN_POINT('',(39.4144401478995,-43.796904759634,2.59908173515993));
#219446=CARTESIAN_POINT('Origin',(5.70079064675565E-15,1.85804141662745E-13,
2.59908173516024));
#219447=CARTESIAN_POINT('',(39.3160391863695,-44.1385184650369,2.90134173515993));
#219448=CARTESIAN_POINT('Ctrl Pts',(39.4144401478995,-43.796904759634,2.59908173515994));
#219449=CARTESIAN_POINT('Ctrl Pts',(39.4116082546734,-43.7994532913544,
2.59908174371479));
#219450=CARTESIAN_POINT('Ctrl Pts',(39.4088155471157,-43.8020298032732,
2.5991576435586));
#219451=CARTESIAN_POINT('Ctrl Pts',(39.4060627300848,-43.8046321918096,
2.59930765775247));
#219452=CARTESIAN_POINT('Ctrl Pts',(39.3898103065133,-43.8199964969256,
2.6001933302084));
#219453=CARTESIAN_POINT('Ctrl Pts',(39.3749452320453,-43.8362633193812,
2.60365973323969));
#219454=CARTESIAN_POINT('Ctrl Pts',(39.3616178931548,-43.8529956277642,
2.60934177082139));
#219455=CARTESIAN_POINT('Ctrl Pts',(39.3566392429903,-43.8592462611853,
2.6114643909163));
#219456=CARTESIAN_POINT('Ctrl Pts',(39.3518747760154,-43.8655619201071,
2.61389584429184));
#219457=CARTESIAN_POINT('Ctrl Pts',(39.347330918553,-43.8719202087606,2.61661604385224));
#219458=CARTESIAN_POINT('Ctrl Pts',(39.3437855730191,-43.8768812645303,
2.61873848000747));
#219459=CARTESIAN_POINT('Ctrl Pts',(39.3403750229164,-43.8818681433207,
2.62103707099758));
#219460=CARTESIAN_POINT('Ctrl Pts',(39.3371028088668,-43.8868700682401,
2.62350262767623));
#219461=CARTESIAN_POINT('Ctrl Pts',(39.3256500596934,-43.904376805458,2.63213207605149));
#219462=CARTESIAN_POINT('Ctrl Pts',(39.3158919212388,-43.922067851059,2.64280685971885));
#219463=CARTESIAN_POINT('Ctrl Pts',(39.3079802585394,-43.9394812142296,
2.65513293646054));
#219464=CARTESIAN_POINT('Ctrl Pts',(39.3040244271897,-43.9481878958149,
2.66129597483139));
#219465=CARTESIAN_POINT('Ctrl Pts',(39.3005302159784,-43.9568251581483,
2.66787183533822));
#219466=CARTESIAN_POINT('Ctrl Pts',(39.297516611429,-43.9653352562093,2.67481125953831));
#219467=CARTESIAN_POINT('Ctrl Pts',(39.2945158824216,-43.9738089951117,
2.68172103524049));
#219468=CARTESIAN_POINT('Ctrl Pts',(39.2919914104334,-43.9821566593544,
2.68899101329759));
#219469=CARTESIAN_POINT('Ctrl Pts',(39.2899626959162,-43.9903212250457,
2.69657334701244));
#219470=CARTESIAN_POINT('Ctrl Pts',(39.2899539910984,-43.9903562576023,
2.69660588132542));
#219471=CARTESIAN_POINT('Ctrl Pts',(39.289945294864,-43.990391286806,2.6966384208135));
#219472=CARTESIAN_POINT('Ctrl Pts',(39.2899366072118,-43.9904263126548,
2.69667096547351));
#219473=CARTESIAN_POINT('Ctrl Pts',(39.2858396774343,-44.0069438297352,
2.71201840157866));
#219474=CARTESIAN_POINT('Ctrl Pts',(39.2836282192306,-44.0226860611004,
2.72845645939226));
#219475=CARTESIAN_POINT('Ctrl Pts',(39.2831328363118,-44.0375574100559,
2.74568723186722));
#219476=CARTESIAN_POINT('Ctrl Pts',(39.2826194323372,-44.0529697494253,
2.76354482594117));
#219477=CARTESIAN_POINT('Ctrl Pts',(39.2839495744681,-44.0674474907124,
2.78225519316891));
#219478=CARTESIAN_POINT('Ctrl Pts',(39.2869823603819,-44.0808629337922,
2.80151223085242));
#219479=CARTESIAN_POINT('Ctrl Pts',(39.2899718616358,-44.0940869083981,
2.82049442739997));
#219480=CARTESIAN_POINT('Ctrl Pts',(39.2946164282376,-44.1062793237822,
2.84000929088993));
#219481=CARTESIAN_POINT('Ctrl Pts',(39.300818312271,-44.1172870736897,2.85976644341359));
#219482=CARTESIAN_POINT('Ctrl Pts',(39.3051423761616,-44.1249618727725,
2.87354148166762));
#219483=CARTESIAN_POINT('Ctrl Pts',(39.3102242458198,-44.132060171354,2.8874343834538));
#219484=CARTESIAN_POINT('Ctrl Pts',(39.3160391863695,-44.1385184650369,
2.90134173515994));
#219485=CARTESIAN_POINT('',(39.5544469813076,-44.4033023070483,3.47153072139042));
#219486=CARTESIAN_POINT('',(39.3160391863695,-44.1385184650369,2.90134173515993));
#219487=CARTESIAN_POINT('',(35.2091516650533,-47.9220530736681,3.47153072139039));
#219488=CARTESIAN_POINT('Origin',(5.53234440788222E-15,1.85015204418142E-13,
3.47153072139072));
#219489=CARTESIAN_POINT('',(34.9997217530266,-47.6338034047594,2.90134173515991));
#219490=CARTESIAN_POINT('',(35.2091516650533,-47.9220530736681,3.47153072139039));
#219491=CARTESIAN_POINT('',(34.6451144164191,-47.659028586093,2.5990817351599));
#219492=CARTESIAN_POINT('Ctrl Pts',(34.9997217530266,-47.6338034047594,
2.90134173515991));
#219493=CARTESIAN_POINT('Ctrl Pts',(34.9925330475321,-47.6239092440466,
2.88176998919768));
#219494=CARTESIAN_POINT('Ctrl Pts',(34.9838215185876,-47.6151892923583,
2.86226752356681));
#219495=CARTESIAN_POINT('Ctrl Pts',(34.9737453812861,-47.6077336605731,
2.84310370499972));
#219496=CARTESIAN_POINT('Ctrl Pts',(34.9634872321484,-47.6001433528511,
2.82359371788609));
#219497=CARTESIAN_POINT('Ctrl Pts',(34.9518142124644,-47.5938626849626,
2.80443322636949));
#219498=CARTESIAN_POINT('Ctrl Pts',(34.9388460388088,-47.5890113136631,
2.78589323878208));
#219499=CARTESIAN_POINT('Ctrl Pts',(34.9264269040025,-47.5843653368459,
2.76813818619949));
#219500=CARTESIAN_POINT('Ctrl Pts',(34.9128191931135,-47.5810297921601,
2.75095095198667));
#219501=CARTESIAN_POINT('Ctrl Pts',(34.898095206323,-47.5791401905757,2.73457771435072));
#219502=CARTESIAN_POINT('Ctrl Pts',(34.8863842314158,-47.5776372636135,
2.72155497955536));
#219503=CARTESIAN_POINT('Ctrl Pts',(34.8739663878203,-47.5770495124715,
2.70904711159925));
#219504=CARTESIAN_POINT('Ctrl Pts',(34.8608666162967,-47.5774624305254,
2.69718956158306));
#219505=CARTESIAN_POINT('Ctrl Pts',(34.8608308581757,-47.5774635576576,
2.69715719432324));
#219506=CARTESIAN_POINT('Ctrl Pts',(34.8607950951003,-47.5774646923705,
2.69712483218989));
#219507=CARTESIAN_POINT('Ctrl Pts',(34.8607593270722,-47.5774658346654,
2.69709247518617));
#219508=CARTESIAN_POINT('Ctrl Pts',(34.8536390475845,-47.577693229335,2.69065122242243));
#219509=CARTESIAN_POINT('Ctrl Pts',(34.8462974884548,-47.5782477067926,
2.68442464469393));
#219510=CARTESIAN_POINT('Ctrl Pts',(34.8387748826518,-47.5791245434502,
2.67844505923545));
#219511=CARTESIAN_POINT('Ctrl Pts',(34.8238457504807,-47.5808646865197,
2.66657815779533));
#219512=CARTESIAN_POINT('Ctrl Pts',(34.8082026058782,-47.5838754712046,
2.65568445664141));
#219513=CARTESIAN_POINT('Ctrl Pts',(34.7921542117508,-47.58812612122,2.64601906229482));
#219514=CARTESIAN_POINT('Ctrl Pts',(34.7801179161553,-47.5913141087315,
2.63877001653488));
#219515=CARTESIAN_POINT('Ctrl Pts',(34.7678536672185,-47.5951995198388,
2.63221189387568));
#219516=CARTESIAN_POINT('Ctrl Pts',(34.7554917310468,-47.5997693799338,
2.626452310332));
#219517=CARTESIAN_POINT('Ctrl Pts',(34.7508560049825,-47.6014830774695,
2.62429246650311));
#219518=CARTESIAN_POINT('Ctrl Pts',(34.7462065417646,-47.6032930257982,
2.62224491711712));
#219519=CARTESIAN_POINT('Ctrl Pts',(34.7415502113776,-47.6051985413674,
2.62031533672564));
#219520=CARTESIAN_POINT('Ctrl Pts',(34.7252530550228,-47.6118678458595,
2.61356180535545));
#219521=CARTESIAN_POINT('Ctrl Pts',(34.7088717728658,-47.6197078449341,
2.60825339735313));
#219522=CARTESIAN_POINT('Ctrl Pts',(34.6927009428675,-47.6286892688728,
2.60463337987577));
#219523=CARTESIAN_POINT('Ctrl Pts',(34.6846155278684,-47.6331799808421,
2.60282337113708));
#219524=CARTESIAN_POINT('Ctrl Pts',(34.6765827265058,-47.6379560498531,
2.60143545939082));
#219525=CARTESIAN_POINT('Ctrl Pts',(34.6686393635487,-47.6430138207119,
2.60050005034563));
#219526=CARTESIAN_POINT('Ctrl Pts',(34.6646676820701,-47.6455427061414,
2.60003234582304));
#219527=CARTESIAN_POINT('Ctrl Pts',(34.6607183602076,-47.6481420170537,
2.59967776696033));
#219528=CARTESIAN_POINT('Ctrl Pts',(34.6567960012268,-47.6508112967863,
2.59944011429127));
#219529=CARTESIAN_POINT('Ctrl Pts',(34.6528736422461,-47.653480576519,2.59920246162221));
#219530=CARTESIAN_POINT('Ctrl Pts',(34.6489782471464,-47.6562198264466,
2.59908173791277));
#219531=CARTESIAN_POINT('Ctrl Pts',(34.6451144164191,-47.659028586093,2.59908173515991));
#219532=CARTESIAN_POINT('',(34.620500570364,-47.6769115920298,2.5990817351599));
#219533=CARTESIAN_POINT('Origin',(5.69524824702573E-15,1.85799653515938E-13,
2.59908173516023));
#219534=CARTESIAN_POINT('',(34.4869303039402,-48.0063682005181,2.90134173515989));
#219535=CARTESIAN_POINT('Ctrl Pts',(34.620500570364,-47.6769115920298,2.59908173515991));
#219536=CARTESIAN_POINT('Ctrl Pts',(34.617417796441,-47.6791501491797,2.59908174371474));
#219537=CARTESIAN_POINT('Ctrl Pts',(34.614371068796,-47.6814206292673,2.59915764355858));
#219538=CARTESIAN_POINT('Ctrl Pts',(34.6113613083103,-47.6837210139131,
2.59930765775244));
#219539=CARTESIAN_POINT('Ctrl Pts',(34.5935919100092,-47.6973023109004,
2.60019333020854));
#219540=CARTESIAN_POINT('Ctrl Pts',(34.577107922018,-47.7119261986131,2.60365973324102));
#219541=CARTESIAN_POINT('Ctrl Pts',(34.5621045891999,-47.7271737594097,
2.60934177082469));
#219542=CARTESIAN_POINT('Ctrl Pts',(34.5564998434991,-47.7328697405531,
2.61146439091881));
#219543=CARTESIAN_POINT('Ctrl Pts',(34.5511013106542,-47.7386527792204,
2.61389584429323));
#219544=CARTESIAN_POINT('Ctrl Pts',(34.5459177227791,-47.7445012740624,
2.6166160438522));
#219545=CARTESIAN_POINT('Ctrl Pts',(34.5418732274832,-47.7490645631291,
2.61873848000743));
#219546=CARTESIAN_POINT('Ctrl Pts',(34.5379600899543,-47.7536676237146,
2.62103707099754));
#219547=CARTESIAN_POINT('Ctrl Pts',(34.5341829579105,-47.7583001080598,
2.62350262767619));
#219548=CARTESIAN_POINT('Ctrl Pts',(34.5209629957571,-47.7745138032682,
2.63213207605145));
#219549=CARTESIAN_POINT('Ctrl Pts',(34.5094090955958,-47.7910879322534,
2.6428068597188));
#219550=CARTESIAN_POINT('Ctrl Pts',(34.4997205817199,-47.8075789092546,
2.6551329364605));
#219551=CARTESIAN_POINT('Ctrl Pts',(34.494876324782,-47.8158243977553,2.66129597483135));
#219552=CARTESIAN_POINT('Ctrl Pts',(34.4904984154667,-47.8240490997336,
2.66787183533818));
#219553=CARTESIAN_POINT('Ctrl Pts',(34.4866117722857,-47.8321975711346,
2.67481125953827));
#219554=CARTESIAN_POINT('Ctrl Pts',(34.4827417346802,-47.8403112284169,
2.68172103524046));
#219555=CARTESIAN_POINT('Ctrl Pts',(34.4793585234985,-47.8483492841039,
2.68899101329756));
#219556=CARTESIAN_POINT('Ctrl Pts',(34.4764874929868,-47.8562570650391,
2.69657334701241));
#219557=CARTESIAN_POINT('Ctrl Pts',(34.4764751739556,-47.8562909957826,
2.69660588132538));
#219558=CARTESIAN_POINT('Ctrl Pts',(34.4764628638112,-47.8563249240885,
2.69663842081347));
#219559=CARTESIAN_POINT('Ctrl Pts',(34.4764505625528,-47.8563588499552,
2.69667096547348));
#219560=CARTESIAN_POINT('Ctrl Pts',(34.4706495255088,-47.8723576365726,
2.71201840157626));
#219561=CARTESIAN_POINT('Ctrl Pts',(34.4668046706517,-47.8877824700173,
2.72845645938716));
#219562=CARTESIAN_POINT('Ctrl Pts',(34.464757522239,-47.90252057055,2.7456872318592));
#219563=CARTESIAN_POINT('Ctrl Pts',(34.4626359025951,-47.9177948141809,
2.76354482592991));
#219564=CARTESIAN_POINT('Ctrl Pts',(34.462445422019,-47.9323322825973,2.78225519315416));
#219565=CARTESIAN_POINT('Ctrl Pts',(34.4640592983636,-47.9459912469255,
2.80151223083409));
#219566=CARTESIAN_POINT('Ctrl Pts',(34.4656501410715,-47.9594552671851,
2.82049442737791));
#219567=CARTESIAN_POINT('Ctrl Pts',(34.4689948098058,-47.97206638065,2.84000929086404));
#219568=CARTESIAN_POINT('Ctrl Pts',(34.4740120960853,-47.983662102358,2.85976644338393));
#219569=CARTESIAN_POINT('Ctrl Pts',(34.4775102373488,-47.9917468458484,
2.87354148164767));
#219570=CARTESIAN_POINT('Ctrl Pts',(34.4818222937534,-47.9993374592392,
2.88743438344379));
#219571=CARTESIAN_POINT('Ctrl Pts',(34.4869303039402,-48.0063682005181,
2.90134173515989));
#219572=CARTESIAN_POINT('',(34.6963546279291,-48.2946219293741,3.47153072139039));
#219573=CARTESIAN_POINT('',(34.4869303039402,-48.0063682005181,2.90134173515989));
#219574=CARTESIAN_POINT('',(30.0070536838164,-51.3398895692692,3.47153072139037));
#219575=CARTESIAN_POINT('Origin',(5.53234440788222E-15,1.85015204418142E-13,
3.47153072139072));
#219576=CARTESIAN_POINT('',(29.8289013456892,-51.0313275753403,2.90134173515987));
#219577=CARTESIAN_POINT('',(30.0070536838164,-51.3398895692692,3.47153072139037));
#219578=CARTESIAN_POINT('',(29.4735998357344,-51.0193480105322,2.59908173515988));
#219579=CARTESIAN_POINT('Ctrl Pts',(29.8289013456892,-51.0313275753403,
2.90134173515987));
#219580=CARTESIAN_POINT('Ctrl Pts',(29.82278624209,-51.0207361915368,2.8817699891973));
#219581=CARTESIAN_POINT('Ctrl Pts',(29.8150339189621,-51.0111534059229,
2.8622675235661));
#219582=CARTESIAN_POINT('Ctrl Pts',(29.8057923055279,-51.0026853737208,
2.84310370499869));
#219583=CARTESIAN_POINT('Ctrl Pts',(29.7963837548063,-50.9940643779333,
2.82359371788484));
#219584=CARTESIAN_POINT('Ctrl Pts',(29.785431189708,-50.9865979533913,2.80443322636804));
#219585=CARTESIAN_POINT('Ctrl Pts',(29.7730411634511,-50.9804176151478,
2.78589323878044));
#219586=CARTESIAN_POINT('Ctrl Pts',(29.7611756987818,-50.9744989364014,
2.76813818619798));
#219587=CARTESIAN_POINT('Ctrl Pts',(29.747991191717,-50.9697592710706,2.75095095198528));
#219588=CARTESIAN_POINT('Ctrl Pts',(29.7335453816165,-50.9663409452091,
2.73457771434945));
#219589=CARTESIAN_POINT('Ctrl Pts',(29.7220556593013,-50.9636221212278,
2.72155497955453));
#219590=CARTESIAN_POINT('Ctrl Pts',(29.7097672786764,-50.9617395717399,
2.70904711159883));
#219591=CARTESIAN_POINT('Ctrl Pts',(29.6966961073826,-50.960780928799,2.69718956158301));
#219592=CARTESIAN_POINT('Ctrl Pts',(29.6966604273309,-50.9607783120152,
2.69715719432319));
#219593=CARTESIAN_POINT('Ctrl Pts',(29.6966247415596,-50.9607757022527,
2.69712483218985));
#219594=CARTESIAN_POINT('Ctrl Pts',(29.6965890500702,-50.960773099513,2.69709247518613));
#219595=CARTESIAN_POINT('Ctrl Pts',(29.6894840070031,-50.9602549766179,
2.69065122242238));
#219596=CARTESIAN_POINT('Ctrl Pts',(29.682124707026,-50.9600390146962,2.68442464469389));
#219597=CARTESIAN_POINT('Ctrl Pts',(29.6745516564563,-50.9601247215265,
2.67844505923542));
#219598=CARTESIAN_POINT('Ctrl Pts',(29.6595224131524,-50.9602948126665,
2.6665781577953));
#219599=CARTESIAN_POINT('Ctrl Pts',(29.6436502506365,-50.9616539500919,
2.65568445664136));
#219600=CARTESIAN_POINT('Ctrl Pts',(29.6272454573773,-50.9642038006257,
2.64601906229478));
#219601=CARTESIAN_POINT('Ctrl Pts',(29.6149418624329,-50.966116188526,2.63877001653484));
#219602=CARTESIAN_POINT('Ctrl Pts',(29.6023386622828,-50.9686983518502,
2.63221189387565));
#219603=CARTESIAN_POINT('Ctrl Pts',(29.5895667656379,-50.9719510035824,
2.62645231033197));
#219604=CARTESIAN_POINT('Ctrl Pts',(29.584777304396,-50.973170747982,2.62429246650308));
#219605=CARTESIAN_POINT('Ctrl Pts',(29.5799641203068,-50.9744847799793,
2.62224491711709));
#219606=CARTESIAN_POINT('Ctrl Pts',(29.5751341171706,-50.9758931378749,
2.62031533672561));
#219607=CARTESIAN_POINT('Ctrl Pts',(29.5582291061939,-50.9808223905099,
2.61356180535542));
#219608=CARTESIAN_POINT('Ctrl Pts',(29.5411180593592,-50.986907130999,2.60825339735312));
#219609=CARTESIAN_POINT('Ctrl Pts',(29.5240970004174,-50.9941490417481,
2.60463337987575));
#219610=CARTESIAN_POINT('Ctrl Pts',(29.5155864709465,-50.9977699971226,
2.60282337113707));
#219611=CARTESIAN_POINT('Ctrl Pts',(29.5070984389562,-51.0016802459457,
2.60143545939079));
#219612=CARTESIAN_POINT('Ctrl Pts',(29.498669909557,-51.0058800022835,2.6005000503456));
#219613=CARTESIAN_POINT('Ctrl Pts',(29.4944556448574,-51.0079798804524,
2.60003234582301));
#219614=CARTESIAN_POINT('Ctrl Pts',(29.490256255818,-51.0101521355223,2.59967776696029));
#219615=CARTESIAN_POINT('Ctrl Pts',(29.4860763682217,-51.0123967945046,
2.59944011429123));
#219616=CARTESIAN_POINT('Ctrl Pts',(29.4818964806253,-51.014641453487,2.59920246162217));
#219617=CARTESIAN_POINT('Ctrl Pts',(29.4777360953222,-51.0169585178533,
2.59908173791271));
#219618=CARTESIAN_POINT('Ctrl Pts',(29.4735998357344,-51.0193480105322,
2.59908173515988));
#219619=CARTESIAN_POINT('',(29.4472515437741,-51.0345602039881,2.59908173515987));
#219620=CARTESIAN_POINT('Origin',(5.68926707005281E-15,1.85795769294195E-13,
2.59908173516024));
#219621=CARTESIAN_POINT('',(29.2799753962469,-51.348250120016,2.90134173515988));
#219622=CARTESIAN_POINT('Ctrl Pts',(29.4472515437741,-51.0345602039881,
2.59908173515988));
#219623=CARTESIAN_POINT('Ctrl Pts',(29.4439516646705,-51.036464260467,2.59908174371475));
#219624=CARTESIAN_POINT('Ctrl Pts',(29.4406842975238,-51.0384038328683,
2.59915764355853));
#219625=CARTESIAN_POINT('Ctrl Pts',(29.437450569149,-51.0403770101279,2.59930765775239));
#219626=CARTESIAN_POINT('Ctrl Pts',(29.4183588813692,-51.0520264994509,
2.60019333020843));
#219627=CARTESIAN_POINT('Ctrl Pts',(29.4004365818807,-51.0648472300424,
2.60365973324047));
#219628=CARTESIAN_POINT('Ctrl Pts',(29.3839216347919,-51.078442987781,2.60934177082339));
#219629=CARTESIAN_POINT('Ctrl Pts',(29.3777522003175,-51.0835219102896,
2.61146439091781));
#219630=CARTESIAN_POINT('Ctrl Pts',(29.3717787490542,-51.0887089685247,
2.61389584429265));
#219631=CARTESIAN_POINT('Ctrl Pts',(29.3660122232364,-51.0939835922264,
2.61661604385216));
#219632=CARTESIAN_POINT('Ctrl Pts',(29.3615128905154,-51.0980991182401,
2.61873848000739));
#219633=CARTESIAN_POINT('Ctrl Pts',(29.357140038714,-51.1022679285256,2.62103707099751));
#219634=CARTESIAN_POINT('Ctrl Pts',(29.352899371725,-51.1064802178288,2.62350262767616));
#219635=CARTESIAN_POINT('Ctrl Pts',(29.3380570372635,-51.12122323039,2.63213207605142));
#219636=CARTESIAN_POINT('Ctrl Pts',(29.3248339623433,-51.1364988531338,
2.64280685971877));
#219637=CARTESIAN_POINT('Ctrl Pts',(29.3134747466765,-51.1518867653708,
2.65513293646047));
#219638=CARTESIAN_POINT('Ctrl Pts',(29.307795138843,-51.1595807214893,2.66129597483132));
#219639=CARTESIAN_POINT('Ctrl Pts',(29.3025814967145,-51.1673027515566,
2.66787183533815));
#219640=CARTESIAN_POINT('Ctrl Pts',(29.297864397778,-51.1750003199397,2.67481125953824));
#219641=CARTESIAN_POINT('Ctrl Pts',(29.2931674525162,-51.1826650006747,
2.68172103524043));
#219642=CARTESIAN_POINT('Ctrl Pts',(29.2889625693107,-51.190305381186,2.68899101329752));
#219643=CARTESIAN_POINT('Ctrl Pts',(29.2852806784154,-51.1978697380624,
2.69657334701238));
#219644=CARTESIAN_POINT('Ctrl Pts',(29.2852648801408,-51.1979021952403,
2.69660588132535));
#219645=CARTESIAN_POINT('Ctrl Pts',(29.2852490909589,-51.197934650923,2.69663842081344));
#219646=CARTESIAN_POINT('Ctrl Pts',(29.2852333108693,-51.1979671051086,
2.69667096547344));
#219647=CARTESIAN_POINT('Ctrl Pts',(29.2777917239327,-51.213271875214,2.71201840157896));
#219648=CARTESIAN_POINT('Ctrl Pts',(29.272355597456,-51.2282103130401,2.72845645939298));
#219649=CARTESIAN_POINT('Ctrl Pts',(29.2687791125364,-51.2426536914408,
2.74568723186839));
#219650=CARTESIAN_POINT('Ctrl Pts',(29.2650725221326,-51.2576224915284,
2.76354482594258));
#219651=CARTESIAN_POINT('Ctrl Pts',(29.2633635057963,-51.2720604115321,
2.78225519317057));
#219652=CARTESIAN_POINT('Ctrl Pts',(29.2635407906078,-51.2858132466407,
2.80151223085432));
#219653=CARTESIAN_POINT('Ctrl Pts',(29.2637155451671,-51.2993697979339,
2.82049442740165));
#219654=CARTESIAN_POINT('Ctrl Pts',(29.2657236711474,-51.3122614394841,
2.84000929089134));
#219655=CARTESIAN_POINT('Ctrl Pts',(29.2695013892396,-51.324318087841,2.85976644341472));
#219656=CARTESIAN_POINT('Ctrl Pts',(29.2721352815056,-51.3327241975843,
2.87354148166836));
#219657=CARTESIAN_POINT('Ctrl Pts',(29.2756302808591,-51.3407239614239,
2.88743438345414));
#219658=CARTESIAN_POINT('Ctrl Pts',(29.2799753962468,-51.348250120016,2.90134173515988));
#219659=CARTESIAN_POINT('',(29.458121752568,-51.6568155675422,3.47153072139037));
#219660=CARTESIAN_POINT('',(29.2799753962469,-51.348250120016,2.90134173515988));
#219661=CARTESIAN_POINT('',(24.4761921430398,-54.1952354911867,3.47153072139034));
#219662=CARTESIAN_POINT('Origin',(5.53234440788222E-15,1.85015204418142E-13,
3.47153072139072));
#219663=CARTESIAN_POINT('',(24.3312692531094,-53.869741842014,2.90134173515986));
#219664=CARTESIAN_POINT('',(24.4761921430398,-54.1952354911867,3.47153072139034));
#219665=CARTESIAN_POINT('',(23.979166327502,-53.8206887816831,2.59908173515986));
#219666=CARTESIAN_POINT('Ctrl Pts',(24.3312692531094,-53.869741842014,2.90134173515986));
#219667=CARTESIAN_POINT('Ctrl Pts',(24.3262947497604,-53.8585692765372,
2.88176998919721));
#219668=CARTESIAN_POINT('Ctrl Pts',(24.3195865685237,-53.8482286480022,
2.86226752356593));
#219669=CARTESIAN_POINT('Ctrl Pts',(24.3112807320078,-53.8388409929162,
2.84310370499844));
#219670=CARTESIAN_POINT('Ctrl Pts',(24.3028248617529,-53.8292837624971,
2.82359371788458));
#219671=CARTESIAN_POINT('Ctrl Pts',(24.2927127498357,-53.8207133850115,
2.80443322636777));
#219672=CARTESIAN_POINT('Ctrl Pts',(24.281036618698,-53.813271792903,2.78589323878017));
#219673=CARTESIAN_POINT('Ctrl Pts',(24.2698548246797,-53.8061452585103,
2.76813818619776));
#219674=CARTESIAN_POINT('Ctrl Pts',(24.2572379736576,-53.8000534012996,
2.75095095198512));
#219675=CARTESIAN_POINT('Ctrl Pts',(24.2432286115656,-53.7951438030544,
2.73457771434934));
#219676=CARTESIAN_POINT('Ctrl Pts',(24.2320860256442,-53.7912388700583,
2.72155497955446));
#219677=CARTESIAN_POINT('Ctrl Pts',(24.2200617420592,-53.7880821478308,
2.7090471115988));
#219678=CARTESIAN_POINT('Ctrl Pts',(24.2071623814828,-53.7857624469878,
2.69718956158302));
#219679=CARTESIAN_POINT('Ctrl Pts',(24.2071271704186,-53.785756114958,2.69715719432319));
#219680=CARTESIAN_POINT('Ctrl Pts',(24.2070919529321,-53.7857497893133,
2.69712483218985));
#219681=CARTESIAN_POINT('Ctrl Pts',(24.2070567290248,-53.7857434700551,
2.69709247518612));
#219682=CARTESIAN_POINT('Ctrl Pts',(24.2000447667171,-53.7844855062582,
2.69065122242238));
#219683=CARTESIAN_POINT('Ctrl Pts',(24.192748355923,-53.7835014710811,2.68442464469388));
#219684=CARTESIAN_POINT('Ctrl Pts',(24.1852078325135,-53.7827951090621,
2.67844505923541));
#219685=CARTESIAN_POINT('Ctrl Pts',(24.1702431416115,-53.7813932847184,
2.66657815779529));
#219686=CARTESIAN_POINT('Ctrl Pts',(24.1543158599161,-53.7810858838903,
2.65568445664136));
#219687=CARTESIAN_POINT('Ctrl Pts',(24.137734401873,-53.7819069982464,2.64601906229478));
#219688=CARTESIAN_POINT('Ctrl Pts',(24.1252983083406,-53.7825228340135,
2.63877001653484));
#219689=CARTESIAN_POINT('Ctrl Pts',(24.1124942402755,-53.7837734588329,
2.63221189387564));
#219690=CARTESIAN_POINT('Ctrl Pts',(24.0994523147296,-53.7856732654693,
2.62645231033196));
#219691=CARTESIAN_POINT('Ctrl Pts',(24.0945615926499,-53.786385692958,2.62429246650308));
#219692=CARTESIAN_POINT('Ctrl Pts',(24.0896374219413,-53.7871894118142,
2.62224491711709));
#219693=CARTESIAN_POINT('Ctrl Pts',(24.0846866645811,-53.7880851817726,
2.6203153367256));
#219694=CARTESIAN_POINT('Ctrl Pts',(24.0673590138204,-53.7912203766269,
2.61356180535542));
#219695=CARTESIAN_POINT('Ctrl Pts',(24.0497056745179,-53.7954831928404,
2.6082533973531));
#219696=CARTESIAN_POINT('Ctrl Pts',(24.0320208729162,-53.8009062465103,
2.60463337987573));
#219697=CARTESIAN_POINT('Ctrl Pts',(24.0231784721153,-53.8036177733453,
2.60282337113705));
#219698=CARTESIAN_POINT('Ctrl Pts',(24.0143282061519,-53.806619360476,2.60143545939077));
#219699=CARTESIAN_POINT('Ctrl Pts',(24.0055068550426,-53.8099150888835,
2.60050005034559));
#219700=CARTESIAN_POINT('Ctrl Pts',(24.0010961794879,-53.8115629530872,
2.60003234582299));
#219701=CARTESIAN_POINT('Ctrl Pts',(23.9966927326568,-53.8132843526336,
2.59967776696028));
#219702=CARTESIAN_POINT('Ctrl Pts',(23.9923011121681,-53.8150797979121,
2.59944011429122));
#219703=CARTESIAN_POINT('Ctrl Pts',(23.9879094916794,-53.8168752431906,
2.59920246162216));
#219704=CARTESIAN_POINT('Ctrl Pts',(23.9835296982247,-53.8187447357535,
2.59908173791273));
#219705=CARTESIAN_POINT('Ctrl Pts',(23.979166327502,-53.8206887816831,2.59908173515986));
#219706=CARTESIAN_POINT('',(23.9513722670371,-53.8330634946833,2.59908173515986));
#219707=CARTESIAN_POINT('Origin',(5.68291264686342E-15,1.85792531553863E-13,
2.59908173516024));
#219708=CARTESIAN_POINT('',(23.7522229508834,-54.1275498658869,2.90134173515986));
#219709=CARTESIAN_POINT('Ctrl Pts',(23.9513722670371,-53.8330634946833,
2.59908173515986));
#219710=CARTESIAN_POINT('Ctrl Pts',(23.9478914369187,-53.8346121892499,
2.59908174371477));
#219711=CARTESIAN_POINT('Ctrl Pts',(23.9444392282286,-53.8361996036039,
2.59915764355854));
#219712=CARTESIAN_POINT('Ctrl Pts',(23.9410169613696,-53.8378239549344,
2.5993076577524));
#219713=CARTESIAN_POINT('Ctrl Pts',(23.9208121566327,-53.8474140023528,
2.60019333020859));
#219714=CARTESIAN_POINT('Ctrl Pts',(23.9016479061061,-53.858291109219,2.60365973324168));
#219715=CARTESIAN_POINT('Ctrl Pts',(23.8838022859594,-53.8700861059364,
2.60934177082638));
#219716=CARTESIAN_POINT('Ctrl Pts',(23.877135756331,-53.8744923240693,2.61146439092009));
#219717=CARTESIAN_POINT('Ctrl Pts',(23.8706528330356,-53.8790265713737,
2.61389584429392));
#219718=CARTESIAN_POINT('Ctrl Pts',(23.8643665485428,-53.8836695340505,
2.61661604385215));
#219719=CARTESIAN_POINT('Ctrl Pts',(23.8594616740275,-53.887292206447,2.61873848000738));
#219720=CARTESIAN_POINT('Ctrl Pts',(23.8546770178329,-53.8909810920747,
2.62103707099751));
#219721=CARTESIAN_POINT('Ctrl Pts',(23.8500192775337,-53.8947270356128,
2.62350262767616));
#219722=CARTESIAN_POINT('Ctrl Pts',(23.8337171864864,-53.907837837996,2.63213207605142));
#219723=CARTESIAN_POINT('Ctrl Pts',(23.8189698115833,-53.921647591579,2.64280685971878));
#219724=CARTESIAN_POINT('Ctrl Pts',(23.8060643480694,-53.9357638458652,
2.65513293646048));
#219725=CARTESIAN_POINT('Ctrl Pts',(23.7996116163124,-53.9428219730082,
2.66129597483132));
#219726=CARTESIAN_POINT('Ctrl Pts',(23.7936193631247,-53.9499567269871,
2.66787183533814));
#219727=CARTESIAN_POINT('Ctrl Pts',(23.7881234899558,-53.9571190561822,
2.67481125953823));
#219728=CARTESIAN_POINT('Ctrl Pts',(23.7826510977529,-53.964250784524,2.68172103524042));
#219729=CARTESIAN_POINT('Ctrl Pts',(23.777670612104,-53.9714097802517,2.68899101329751));
#219730=CARTESIAN_POINT('Ctrl Pts',(23.7732182003924,-53.9785478363925,
2.69657334701237));
#219731=CARTESIAN_POINT('Ctrl Pts',(23.7731990959634,-53.9785784643972,
2.69660588132534));
#219732=CARTESIAN_POINT('Ctrl Pts',(23.7731800007337,-53.9786090918653,
2.69663842081342));
#219733=CARTESIAN_POINT('Ctrl Pts',(23.773160914703,-53.978639718795,2.69667096547343));
#219734=CARTESIAN_POINT('Ctrl Pts',(23.7641603094591,-53.9930827901205,
2.7120184015777));
#219735=CARTESIAN_POINT('Ctrl Pts',(23.7571924707029,-54.0073711636733,
2.72845645939029));
#219736=CARTESIAN_POINT('Ctrl Pts',(23.7521258339934,-54.0213615752622,
2.74568723186417));
#219737=CARTESIAN_POINT('Ctrl Pts',(23.7468748830096,-54.0358609304967,
2.76354482593678));
#219738=CARTESIAN_POINT('Ctrl Pts',(23.7436660552526,-54.0500411172115,
2.78225519316308));
#219739=CARTESIAN_POINT('Ctrl Pts',(23.7424048061593,-54.0637371441584,
2.8015122308451));
#219740=CARTESIAN_POINT('Ctrl Pts',(23.7411615579205,-54.0772376980698,
2.82049442739081));
#219741=CARTESIAN_POINT('Ctrl Pts',(23.7418111396955,-54.0902686241807,
2.84000929087886));
#219742=CARTESIAN_POINT('Ctrl Pts',(23.7443079001267,-54.1026541040226,
2.85976644340064));
#219743=CARTESIAN_POINT('Ctrl Pts',(23.7460486859218,-54.1112894809313,
2.87354148165889));
#219744=CARTESIAN_POINT('Ctrl Pts',(23.7486883362831,-54.1196107481421,
2.88743438344939));
#219745=CARTESIAN_POINT('Ctrl Pts',(23.7522229508834,-54.1275498658869,
2.90134173515986));
#219746=CARTESIAN_POINT('',(23.8971395307774,-54.4530463244688,3.47153072139034));
#219747=CARTESIAN_POINT('',(23.7522229508834,-54.1275498658869,2.90134173515986));
#219748=CARTESIAN_POINT('',(18.6771643191716,-56.4568070719807,3.47153072139033));
#219749=CARTESIAN_POINT('Origin',(5.53234440788222E-15,1.85015204418142E-13,
3.47153072139072));
#219750=CARTESIAN_POINT('',(18.5670586829472,-56.1179479440984,2.90134173515985));
#219751=CARTESIAN_POINT('',(18.6771643191716,-56.4568070719807,3.47153072139033));
#219752=CARTESIAN_POINT('',(18.2220120550223,-56.0323588238387,2.59908173515985));
#219753=CARTESIAN_POINT('Ctrl Pts',(18.5670586829472,-56.1179479440984,
2.90134173515985));
#219754=CARTESIAN_POINT('Ctrl Pts',(18.5632792815482,-56.1063166059137,
2.88176998919726));
#219755=CARTESIAN_POINT('Ctrl Pts',(18.5576887384403,-56.0953314285478,
2.86226752356603));
#219756=CARTESIAN_POINT('Ctrl Pts',(18.5504096793258,-56.0851270036914,
2.8431037049986));
#219757=CARTESIAN_POINT('Ctrl Pts',(18.5429991338217,-56.0747382496572,
2.82359371788465));
#219758=CARTESIAN_POINT('Ctrl Pts',(18.5338382654998,-56.065157818077,2.80443322636776));
#219759=CARTESIAN_POINT('Ctrl Pts',(18.5230039556175,-56.0565365037439,
2.78589323878008));
#219760=CARTESIAN_POINT('Ctrl Pts',(18.5126283423249,-56.0482801935068,
2.76813818619733));
#219761=CARTESIAN_POINT('Ctrl Pts',(18.5007173802052,-56.0409028880787,
2.75095095198438));
#219762=CARTESIAN_POINT('Ctrl Pts',(18.4872979556241,-56.0345558080355,
2.73457771434832));
#219763=CARTESIAN_POINT('Ctrl Pts',(18.4766245865996,-56.0295075492879,
2.7215549795538));
#219764=CARTESIAN_POINT('Ctrl Pts',(18.4649961406218,-56.0251112400301,
2.70904711159847));
#219765=CARTESIAN_POINT('Ctrl Pts',(18.4524099188571,-56.021455896413,2.69718956158299));
#219766=CARTESIAN_POINT('Ctrl Pts',(18.4523755625601,-56.0214459185123,
2.69715719432317));
#219767=CARTESIAN_POINT('Ctrl Pts',(18.4523411992087,-56.0214359462903,
2.69712483218983));
#219768=CARTESIAN_POINT('Ctrl Pts',(18.4523068288039,-56.0214259797488,
2.69709247518611));
#219769=CARTESIAN_POINT('Ctrl Pts',(18.4454647717819,-56.0194419575647,
2.69065122242236));
#219770=CARTESIAN_POINT('Ctrl Pts',(18.4383111911745,-56.0177006304276,
2.68442464469387));
#219771=CARTESIAN_POINT('Ctrl Pts',(18.4308858104775,-56.0162099386094,
2.6784450592354));
#219772=CARTESIAN_POINT('Ctrl Pts',(18.4161496282625,-56.0132515574629,
2.66657815779528));
#219773=CARTESIAN_POINT('Ctrl Pts',(18.4003417300189,-56.011280986329,2.65568445664134));
#219774=CARTESIAN_POINT('Ctrl Pts',(18.3837652771161,-56.0103643682068,
2.64601906229475));
#219775=CARTESIAN_POINT('Ctrl Pts',(18.371332937439,-56.0096769046152,2.63877001653481));
#219776=CARTESIAN_POINT('Ctrl Pts',(18.3584682855079,-56.0095822888225,
2.63221189387562));
#219777=CARTESIAN_POINT('Ctrl Pts',(18.3452992211265,-56.010108435684,2.62645231033194));
#219778=CARTESIAN_POINT('Ctrl Pts',(18.3403608219835,-56.0103057407571,
2.62429246650306));
#219779=CARTESIAN_POINT('Ctrl Pts',(18.3353796149004,-56.0105903407603,
2.62224491711705));
#219780=CARTESIAN_POINT('Ctrl Pts',(18.3303623448498,-56.0109637085382,
2.62031533672557));
#219781=CARTESIAN_POINT('Ctrl Pts',(18.3128018996728,-56.012270495761,2.61356180535538));
#219782=CARTESIAN_POINT('Ctrl Pts',(18.2947996815822,-56.0146646833925,
2.60825339735308));
#219783=CARTESIAN_POINT('Ctrl Pts',(18.2766448957077,-56.0182094638723,
2.60463337987572));
#219784=CARTESIAN_POINT('Ctrl Pts',(18.2675675027704,-56.0199818541123,
2.60282337113703));
#219785=CARTESIAN_POINT('Ctrl Pts',(18.2584519681998,-56.022041893534,2.60143545939075));
#219786=CARTESIAN_POINT('Ctrl Pts',(18.2493344439491,-56.024397485321,2.60050005034556));
#219787=CARTESIAN_POINT('Ctrl Pts',(18.2447756818237,-56.0255752812145,
2.60003234582297));
#219788=CARTESIAN_POINT('Ctrl Pts',(18.2402164222858,-56.0268269652237,
2.59967776696028));
#219789=CARTESIAN_POINT('Ctrl Pts',(18.2356611844178,-56.0281535255242,
2.59944011429122));
#219790=CARTESIAN_POINT('Ctrl Pts',(18.2311059465498,-56.0294800858246,
2.59920246162216));
#219791=CARTESIAN_POINT('Ctrl Pts',(18.2265547308772,-56.0308815240325,
2.59908173791271));
#219792=CARTESIAN_POINT('Ctrl Pts',(18.2220120550223,-56.0323588238387,
2.59908173515985));
#219793=CARTESIAN_POINT('',(18.1930767435955,-56.0417604764379,2.59908173515985));
#219794=CARTESIAN_POINT('Origin',(5.6762545978478E-15,1.85789975768303E-13,
2.59908173516024));
#219795=CARTESIAN_POINT('',(17.9642361803979,-56.3138168485091,2.90134173515985));
#219796=CARTESIAN_POINT('Ctrl Pts',(18.1930767435955,-56.0417604764379,
2.59908173515985));
#219797=CARTESIAN_POINT('Ctrl Pts',(18.1894530991656,-56.0429368412704,
2.59908174371471));
#219798=CARTESIAN_POINT('Ctrl Pts',(18.185853872053,-56.0441547055333,2.59915764355852));
#219799=CARTESIAN_POINT('Ctrl Pts',(18.1822805617814,-56.0454124342016,
2.59930765775238));
#219800=CARTESIAN_POINT('Ctrl Pts',(18.161184008162,-56.0528379691462,2.60019333020848));
#219801=CARTESIAN_POINT('Ctrl Pts',(18.1409877741415,-56.0616522804246,
2.60365973324091));
#219802=CARTESIAN_POINT('Ctrl Pts',(18.1220070012899,-56.0715172876645,
2.60934177082451));
#219803=CARTESIAN_POINT('Ctrl Pts',(18.1149164163959,-56.0752025259771,
2.61146439091866));
#219804=CARTESIAN_POINT('Ctrl Pts',(18.1079950493278,-56.0790342841918,
2.61389584429311));
#219805=CARTESIAN_POINT('Ctrl Pts',(18.1012578800036,-56.0829947165767,
2.61661604385213));
#219806=CARTESIAN_POINT('Ctrl Pts',(18.0960012025255,-56.0860848445992,
2.61873848000736));
#219807=CARTESIAN_POINT('Ctrl Pts',(18.0908571636324,-56.0892533893662,
2.62103707099748));
#219808=CARTESIAN_POINT('Ctrl Pts',(18.0858333812004,-56.0924919457979,
2.62350262767612));
#219809=CARTESIAN_POINT('Ctrl Pts',(18.0682501426882,-56.1038268933086,
2.63213207605139));
#219810=CARTESIAN_POINT('Ctrl Pts',(18.0521400431278,-56.1160194751807,
2.64280685971874));
#219811=CARTESIAN_POINT('Ctrl Pts',(18.0378297267257,-56.12870941088,2.65513293646044));
#219812=CARTESIAN_POINT('Ctrl Pts',(18.0306745685246,-56.1350543787296,
2.66129597483129));
#219813=CARTESIAN_POINT('Ctrl Pts',(18.0239693566576,-56.1415236867625,
2.66787183533812));
#219814=CARTESIAN_POINT('Ctrl Pts',(18.0177549231928,-56.1480723047922,
2.67481125953821));
#219815=CARTESIAN_POINT('Ctrl Pts',(18.011567040723,-56.1545929440325,2.6817210352404));
#219816=CARTESIAN_POINT('Ctrl Pts',(18.0058655198736,-56.1611921195213,
2.68899101329749));
#219817=CARTESIAN_POINT('Ctrl Pts',(18.0006913689001,-56.1678256688897,
2.69657334701235));
#219818=CARTESIAN_POINT('Ctrl Pts',(18.0006691676289,-56.1678541321544,
2.69660588132532));
#219819=CARTESIAN_POINT('Ctrl Pts',(18.0006469755627,-56.167882595847,2.69663842081341));
#219820=CARTESIAN_POINT('Ctrl Pts',(18.0006247927013,-56.1679110599657,
2.69667096547341));
#219821=CARTESIAN_POINT('Ctrl Pts',(17.9901637816639,-56.1813341912011,
2.71201840157821));
#219822=CARTESIAN_POINT('Ctrl Pts',(17.9817405717272,-56.1948159540715,
2.7284564593914));
#219823=CARTESIAN_POINT('Ctrl Pts',(17.9752392943597,-56.2082001169732,
2.74568723186593));
#219824=CARTESIAN_POINT('Ctrl Pts',(17.9685015133137,-56.2220711693861,
2.76354482593923));
#219825=CARTESIAN_POINT('Ctrl Pts',(17.9638280307249,-56.2358382617205,
2.78225519316626));
#219826=CARTESIAN_POINT('Ctrl Pts',(17.9611420662366,-56.2493274239697,
2.80151223084904));
#219827=CARTESIAN_POINT('Ctrl Pts',(17.9584944364883,-56.2626240656068,
2.82049442739549));
#219828=CARTESIAN_POINT('Ctrl Pts',(17.9577783571054,-56.2756515067261,
2.8400092908843));
#219829=CARTESIAN_POINT('Ctrl Pts',(17.9589668048474,-56.2882301201448,
2.85976644340682));
#219830=CARTESIAN_POINT('Ctrl Pts',(17.9597954117579,-56.297000153218,2.87354148166304));
#219831=CARTESIAN_POINT('Ctrl Pts',(17.9615507925642,-56.3055517542508,
2.88743438345146));
#219832=CARTESIAN_POINT('Ctrl Pts',(17.9642361803979,-56.3138168485091,
2.90134173515985));
#219833=CARTESIAN_POINT('',(18.0743352474898,-56.652678110832,3.47153072139033));
#219834=CARTESIAN_POINT('',(17.9642361803979,-56.3138168485091,2.90134173515984));
#219835=CARTESIAN_POINT('',(12.6735055745747,-58.0998260601477,3.47153072139032));
#219836=CARTESIAN_POINT('Origin',(5.53234440788222E-15,1.85015204418142E-13,
3.47153072139072));
#219837=CARTESIAN_POINT('',(12.5994235324478,-57.7513140650717,2.90134173515983));
#219838=CARTESIAN_POINT('',(12.6735055745747,-58.0998260601477,3.47153072139032));
#219839=CARTESIAN_POINT('',(12.2652136052667,-57.6301266171954,2.59908173515984));
#219840=CARTESIAN_POINT('Ctrl Pts',(12.5994235324478,-57.7513140650717,
2.90134173515983));
#219841=CARTESIAN_POINT('Ctrl Pts',(12.5968806409114,-57.7393513895545,
2.88176998919773));
#219842=CARTESIAN_POINT('Ctrl Pts',(12.5924689870926,-57.72784201926,2.86226752356698));
#219843=CARTESIAN_POINT('Ctrl Pts',(12.5862964562745,-57.7169326264476,
2.84310370500001));
#219844=CARTESIAN_POINT('Ctrl Pts',(12.5800124270088,-57.7058261701617,
2.82359371788647));
#219845=CARTESIAN_POINT('Ctrl Pts',(12.5719031706729,-57.6953406497004,
2.80443322636996));
#219846=CARTESIAN_POINT('Ctrl Pts',(12.5620293850127,-57.6856340700669,
2.78589323878263));
#219847=CARTESIAN_POINT('Ctrl Pts',(12.552573629837,-57.6763384418483,2.76813818620015));
#219848=CARTESIAN_POINT('Ctrl Pts',(12.5414990556139,-57.6677565155049,
2.75095095198743));
#219849=CARTESIAN_POINT('Ctrl Pts',(12.5288165945683,-57.6600414936009,
2.73457771435156));
#219850=CARTESIAN_POINT('Ctrl Pts',(12.5187293821045,-57.6539052188803,
2.72155497955587));
#219851=CARTESIAN_POINT('Ctrl Pts',(12.5076241774204,-57.6483174894759,
2.70904711159944));
#219852=CARTESIAN_POINT('Ctrl Pts',(12.4954889917454,-57.6433665517937,
2.69718956158298));
#219853=CARTESIAN_POINT('Ctrl Pts',(12.4954558666304,-57.6433530373421,
2.69715719432315));
#219854=CARTESIAN_POINT('Ctrl Pts',(12.4954227339061,-57.6433395278007,
2.69712483218981));
#219855=CARTESIAN_POINT('Ctrl Pts',(12.4953895935733,-57.6433260231713,
2.69709247518609));
#219856=CARTESIAN_POINT('Ctrl Pts',(12.4887924048456,-57.6406376799622,
2.69065122242235));
#219857=CARTESIAN_POINT('Ctrl Pts',(12.4818600305509,-57.6381581392096,
2.68442464469384));
#219858=CARTESIAN_POINT('Ctrl Pts',(12.4746311465912,-57.6358994499237,
2.67844505923537));
#219859=CARTESIAN_POINT('Ctrl Pts',(12.4602849257593,-57.6314169246173,
2.66657815779526));
#219860=CARTESIAN_POINT('Ctrl Pts',(12.4447696056087,-57.6278047731674,
2.65568445664133));
#219861=CARTESIAN_POINT('Ctrl Pts',(12.428379772933,-57.6251604652268,2.64601906229475));
#219862=CARTESIAN_POINT('Ctrl Pts',(12.4160873984262,-57.6231772342714,
2.63877001653481));
#219863=CARTESIAN_POINT('Ctrl Pts',(12.4033031104479,-57.6217384144971,
2.63221189387561));
#219864=CARTESIAN_POINT('Ctrl Pts',(12.3901511902562,-57.6208851370086,
2.62645231033193));
#219865=CARTESIAN_POINT('Ctrl Pts',(12.3852192201843,-57.6205651579504,
2.62429246650305));
#219866=CARTESIAN_POINT('Ctrl Pts',(12.3802355518738,-57.6203275209634,
2.62224491711704));
#219867=CARTESIAN_POINT('Ctrl Pts',(12.3752067393935,-57.6201743958654,
2.62031533672556));
#219868=CARTESIAN_POINT('Ctrl Pts',(12.3576058957123,-57.6196384580224,
2.61356180535537));
#219869=CARTESIAN_POINT('Ctrl Pts',(12.339452034902,-57.6201377858511,2.60825339735307));
#219870=CARTESIAN_POINT('Ctrl Pts',(12.321026172388,-57.6217654557842,2.60463337987571));
#219871=CARTESIAN_POINT('Ctrl Pts',(12.3118132411309,-57.6225792907507,
2.60282337113702));
#219872=CARTESIAN_POINT('Ctrl Pts',(12.3025323096574,-57.6236752122404,
2.60143545939074));
#219873=CARTESIAN_POINT('Ctrl Pts',(12.293218505769,-57.6250648590504,2.60050005034555));
#219874=CARTESIAN_POINT('Ctrl Pts',(12.2885616038247,-57.6257596824554,
2.60003234582296));
#219875=CARTESIAN_POINT('Ctrl Pts',(12.2838964837817,-57.6265279372155,
2.59967776696024));
#219876=CARTESIAN_POINT('Ctrl Pts',(12.2792275366736,-57.6273710784657,
2.59944011429118));
#219877=CARTESIAN_POINT('Ctrl Pts',(12.2745585895656,-57.6282142197158,
2.59920246162212));
#219878=CARTESIAN_POINT('Ctrl Pts',(12.2698858157465,-57.6291322491183,
2.5990817379127));
#219879=CARTESIAN_POINT('Ctrl Pts',(12.2652136052667,-57.6301266171954,
2.59908173515984));
#219880=CARTESIAN_POINT('',(12.2354540642051,-57.6364522029204,2.59908173515984));
#219881=CARTESIAN_POINT('Origin',(5.66936586998424E-15,1.85788129939235E-13,
2.59908173516024));
#219882=CARTESIAN_POINT('',(11.9794294790619,-57.8830978693153,2.90134173515983));
#219883=CARTESIAN_POINT('Ctrl Pts',(12.2354540642051,-57.6364522029204,
2.59908173515984));
#219884=CARTESIAN_POINT('Ctrl Pts',(12.2317273068703,-57.6372433495196,
2.59908174371473));
#219885=CARTESIAN_POINT('Ctrl Pts',(12.2280204952205,-57.6380783205155,
2.5991576435585));
#219886=CARTESIAN_POINT('Ctrl Pts',(12.2243352914717,-57.6389556465831,
2.59930765775236));
#219887=CARTESIAN_POINT('Ctrl Pts',(12.2025781272246,-57.64413531334,2.60019333020842));
#219888=CARTESIAN_POINT('Ctrl Pts',(12.1815711838755,-57.6507902575926,
2.60365973324057));
#219889=CARTESIAN_POINT('Ctrl Pts',(12.1616632156375,-57.6586171922724,
2.6093417708237));
#219890=CARTESIAN_POINT('Ctrl Pts',(12.1542262614109,-57.6615410745216,
2.61146439091804));
#219891=CARTESIAN_POINT('Ctrl Pts',(12.146942282517,-57.6646283621009,2.61389584429276));
#219892=CARTESIAN_POINT('Ctrl Pts',(12.1398280421993,-57.667862872867,2.61661604385213));
#219893=CARTESIAN_POINT('Ctrl Pts',(12.134277155017,-57.6703866004262,2.61873848000736));
#219894=CARTESIAN_POINT('Ctrl Pts',(12.1288300925919,-57.6730000890929,
2.62103707099748));
#219895=CARTESIAN_POINT('Ctrl Pts',(12.1234953096387,-57.6756957761162,
2.62350262767613));
#219896=CARTESIAN_POINT('Ctrl Pts',(12.1048235693024,-57.6851306806976,
2.63213207605139));
#219897=CARTESIAN_POINT('Ctrl Pts',(12.0875272507065,-57.6955725063803,
2.64280685971875));
#219898=CARTESIAN_POINT('Ctrl Pts',(12.0719688682374,-57.7066970899016,
2.65513293646045));
#219899=CARTESIAN_POINT('Ctrl Pts',(12.0641896770028,-57.7122593816623,
2.6612959748313));
#219900=CARTESIAN_POINT('Ctrl Pts',(12.0568449701609,-57.7179923646565,
2.66787183533812));
#219901=CARTESIAN_POINT('Ctrl Pts',(12.0499800630337,-57.7238555234913,
2.67481125953821));
#219902=CARTESIAN_POINT('Ctrl Pts',(12.0431444860322,-57.7296936321422,
2.68172103524039));
#219903=CARTESIAN_POINT('Ctrl Pts',(12.0367843970379,-57.7356606854445,
2.68899101329748));
#219904=CARTESIAN_POINT('Ctrl Pts',(12.0309451958833,-57.7417170494854,
2.69657334701234));
#219905=CARTESIAN_POINT('Ctrl Pts',(12.0309201410117,-57.7417430361605,
2.69660588132531));
#219906=CARTESIAN_POINT('Ctrl Pts',(12.0308950952499,-57.7417690242235,
2.6966384208134));
#219907=CARTESIAN_POINT('Ctrl Pts',(12.030870058598,-57.7417950136724,2.69667096547341));
#219908=CARTESIAN_POINT('Ctrl Pts',(12.0190632547926,-57.7540511381831,
2.71201840157904));
#219909=CARTESIAN_POINT('Ctrl Pts',(12.0092769601259,-57.7665785813561,
2.72845645939319));
#219910=CARTESIAN_POINT('Ctrl Pts',(12.0014122714556,-57.7792098558812,
2.74568723186873));
#219911=CARTESIAN_POINT('Ctrl Pts',(11.9932614808864,-57.7923006313198,
2.7635448259431));
#219912=CARTESIAN_POINT('Ctrl Pts',(11.9871745471188,-57.8055037941296,
2.78225519317128));
#219913=CARTESIAN_POINT('Ctrl Pts',(11.9830932952246,-57.8186383015968,
2.80151223085522));
#219914=CARTESIAN_POINT('Ctrl Pts',(11.9790702919523,-57.8315853501716,
2.82049442740278));
#219915=CARTESIAN_POINT('Ctrl Pts',(11.9769963969271,-57.8444665749285,
2.84000929089272));
#219916=CARTESIAN_POINT('Ctrl Pts',(11.976863511098,-57.8571005080036,2.85976644341635));
#219917=CARTESIAN_POINT('Ctrl Pts',(11.9767708607336,-57.8659091109228,
2.87354148166945));
#219918=CARTESIAN_POINT('Ctrl Pts',(11.9776227396658,-57.8745973526465,
2.88743438345466));
#219919=CARTESIAN_POINT('Ctrl Pts',(11.9794294790619,-57.8830978693152,
2.90134173515983));
#219920=CARTESIAN_POINT('',(12.0535047649328,-58.2316113004778,3.47153072139032));
#219921=CARTESIAN_POINT('',(11.9794294790618,-57.8830978693153,2.90134173515983));
#219922=CARTESIAN_POINT('',(6.53099325080115,-59.1062911958294,3.47153072139031));
#219923=CARTESIAN_POINT('Origin',(5.53234440788222E-15,1.85015204418142E-13,
3.47153072139072));
#219924=CARTESIAN_POINT('',(6.493746461128,-58.7519447039086,2.90134173515983));
#219925=CARTESIAN_POINT('',(6.53099325080115,-59.1062911958294,3.47153072139031));
#219926=CARTESIAN_POINT('',(6.17403490859079,-58.5964866834548,2.59908173515983));
#219927=CARTESIAN_POINT('Ctrl Pts',(6.49374646112799,-58.7519447039086,
2.90134173515983));
#219928=CARTESIAN_POINT('Ctrl Pts',(6.49246793990574,-58.7397817566341,
2.88176998919634));
#219929=CARTESIAN_POINT('Ctrl Pts',(6.48928351037779,-58.7278742924794,
2.86226752356423));
#219930=CARTESIAN_POINT('Ctrl Pts',(6.48428513539465,-58.7163794573007,
2.84310370499596));
#219931=CARTESIAN_POINT('Ctrl Pts',(6.47919647150606,-58.7046769834214,
2.82359371788115));
#219932=CARTESIAN_POINT('Ctrl Pts',(6.47222767386437,-58.6934012556346,
2.80443322636344));
#219933=CARTESIAN_POINT('Ctrl Pts',(6.46342259168671,-58.6827157580177,
2.78589323877503));
#219934=CARTESIAN_POINT('Ctrl Pts',(6.45499029385914,-58.6724826566651,
2.76813818619166));
#219935=CARTESIAN_POINT('Ctrl Pts',(6.44487344288378,-58.6627901347869,
2.75095095197815));
#219936=CARTESIAN_POINT('Ctrl Pts',(6.43306689706911,-58.6537916984163,
2.73457771434164));
#219937=CARTESIAN_POINT('Ctrl Pts',(6.42367635877919,-58.6466346380352,
2.72155497954951));
#219938=CARTESIAN_POINT('Ctrl Pts',(6.41321606633851,-58.6399167088191,
2.70904711159642));
#219939=CARTESIAN_POINT('Ctrl Pts',(6.40166487239097,-58.633724420583,2.69718956158297));
#219940=CARTESIAN_POINT('Ctrl Pts',(6.40163334138369,-58.6337075176476,
2.69715719432314));
#219941=CARTESIAN_POINT('Ctrl Pts',(6.40160180229544,-58.6336906188001,
2.6971248321898));
#219942=CARTESIAN_POINT('Ctrl Pts',(6.40157025512701,-58.6336737240425,
2.69709247518608));
#219943=CARTESIAN_POINT('Ctrl Pts',(6.3952902148738,-58.6303105138591,2.69065122242233));
#219944=CARTESIAN_POINT('Ctrl Pts',(6.3886549994353,-58.6271199258585,2.68442464469384));
#219945=CARTESIAN_POINT('Ctrl Pts',(6.38170181337843,-58.6241179857774,
2.67844505923537));
#219946=CARTESIAN_POINT('Ctrl Pts',(6.36790273412708,-58.6181604277963,
2.66657815779525));
#219947=CARTESIAN_POINT('Ctrl Pts',(6.3528499811638,-58.6129462715176,2.65568445664132));
#219948=CARTESIAN_POINT('Ctrl Pts',(6.33682633915184,-58.6086032453497,
2.64601906229474));
#219949=CARTESIAN_POINT('Ctrl Pts',(6.32480860764288,-58.6053459757239,
2.6387700165348));
#219950=CARTESIAN_POINT('Ctrl Pts',(6.31224475095164,-58.6025787159785,
2.6322118938756));
#219951=CARTESIAN_POINT('Ctrl Pts',(6.29925407013949,-58.6003553628267,
2.62645231033192));
#219952=CARTESIAN_POINT('Ctrl Pts',(6.29438256483494,-58.5995216053948,
2.62429246650304));
#219953=CARTESIAN_POINT('Ctrl Pts',(6.28945103740996,-58.5987643350181,
2.62224491711704));
#219954=CARTESIAN_POINT('Ctrl Pts',(6.28446577922175,-58.5980863947148,
2.62031533672556));
#219955=CARTESIAN_POINT('Ctrl Pts',(6.26701737556302,-58.5957136036532,
2.61356180535537));
#219956=CARTESIAN_POINT('Ctrl Pts',(6.24891076953115,-58.5943126009389,
2.60825339735306));
#219957=CARTESIAN_POINT('Ctrl Pts',(6.23041570798304,-58.5940053272328,
2.60463337987569));
#219958=CARTESIAN_POINT('Ctrl Pts',(6.22116817720899,-58.5938516903798,
2.60282337113701));
#219959=CARTESIAN_POINT('Ctrl Pts',(6.21182353266003,-58.5939714867922,
2.60143545939073));
#219960=CARTESIAN_POINT('Ctrl Pts',(6.20241549311822,-58.594379963364,2.60050005034555));
#219961=CARTESIAN_POINT('Ctrl Pts',(6.19771147334731,-58.5945842016499,
2.60003234582295));
#219962=CARTESIAN_POINT('Ctrl Pts',(6.19299160483051,-58.5948606100009,
2.59967776696025));
#219963=CARTESIAN_POINT('Ctrl Pts',(6.18826010244408,-58.5952110945688,
2.59944011429119));
#219964=CARTESIAN_POINT('Ctrl Pts',(6.18352860005764,-58.5955615791367,
2.59920246162213));
#219965=CARTESIAN_POINT('Ctrl Pts',(6.17878546397971,-58.5959861416116,
2.59908173791268));
#219966=CARTESIAN_POINT('Ctrl Pts',(6.17403490859079,-58.5964866834548,
2.59908173515983));
#219967=CARTESIAN_POINT('',(6.14377718965381,-58.5996668978646,2.59908173515983));
#219968=CARTESIAN_POINT('Origin',(5.66232193761676E-15,1.85787014289949E-13,
2.59908173516024));
#219969=CARTESIAN_POINT('',(5.8633736414964,-58.8181995570482,2.90134173515983));
#219970=CARTESIAN_POINT('Ctrl Pts',(6.14377718965381,-58.5996668978646,
2.59908173515983));
#219971=CARTESIAN_POINT('Ctrl Pts',(6.13998815054745,-58.6000641582627,
2.59908174371469));
#219972=CARTESIAN_POINT('Ctrl Pts',(6.13621436696463,-58.6005070878748,
2.5991576435585));
#219973=CARTESIAN_POINT('Ctrl Pts',(6.13245764560185,-58.6009943991737,
2.59930765775236));
#219974=CARTESIAN_POINT('Ctrl Pts',(6.11027824677107,-58.6038714482303,
2.6001933302084));
#219975=CARTESIAN_POINT('Ctrl Pts',(6.08869075056017,-58.6082941124956,
2.60365973324044));
#219976=CARTESIAN_POINT('Ctrl Pts',(6.06807370280131,-58.6139972210815,
2.60934177082338));
#219977=CARTESIAN_POINT('Ctrl Pts',(6.06037186006944,-58.6161277126012,
2.6114643909178));
#219978=CARTESIAN_POINT('Ctrl Pts',(6.05280507414744,-58.618436704576,2.61389584429262));
#219979=CARTESIAN_POINT('Ctrl Pts',(6.04539170794238,-58.6209098557461,
2.61661604385212));
#219980=CARTESIAN_POINT('Ctrl Pts',(6.03960742773739,-58.6228395323547,
2.61873848000735));
#219981=CARTESIAN_POINT('Ctrl Pts',(6.03391702093609,-58.6248693309924,
2.62103707099746));
#219982=CARTESIAN_POINT('Ctrl Pts',(6.02832968646007,-58.6269926140961,
2.62350262767611));
#219983=CARTESIAN_POINT('Ctrl Pts',(6.008774015794,-58.6344241049591,2.63213207605137));
#219984=CARTESIAN_POINT('Ctrl Pts',(5.99048098024888,-58.6430007716252,
2.64280685971873));
#219985=CARTESIAN_POINT('Ctrl Pts',(5.97384499260682,-58.6524381197036,
2.65513293646042));
#219986=CARTESIAN_POINT('Ctrl Pts',(5.9655269987858,-58.6571567937428,2.66129597483127));
#219987=CARTESIAN_POINT('Ctrl Pts',(5.95762326711415,-58.662090639937,2.6678718353381));
#219988=CARTESIAN_POINT('Ctrl Pts',(5.95018309968352,-58.6672041015817,
2.67481125953819));
#219989=CARTESIAN_POINT('Ctrl Pts',(5.9427747201624,-58.672295716103,2.68172103524038));
#219990=CARTESIAN_POINT('Ctrl Pts',(5.93582574548912,-58.6775652709342,
2.68899101329747));
#219991=CARTESIAN_POINT('Ctrl Pts',(5.92938546966327,-58.6829780948558,
2.69657334701233));
#219992=CARTESIAN_POINT('Ctrl Pts',(5.92935783569763,-58.683001320226,2.6966058813253));
#219993=CARTESIAN_POINT('Ctrl Pts',(5.92933021064688,-58.6830245479287,
2.69663842081338));
#219994=CARTESIAN_POINT('Ctrl Pts',(5.92930259451121,-58.6830477779618,
2.69667096547339));
#219995=CARTESIAN_POINT('Ctrl Pts',(5.91627935575179,-58.6940026150822,
2.71201840157897));
#219996=CARTESIAN_POINT('Ctrl Pts',(5.90523719704766,-58.7054384852681,
2.72845645939305));
#219997=CARTESIAN_POINT('Ctrl Pts',(5.89609526424964,-58.7171784805289,
2.74568723186852));
#219998=CARTESIAN_POINT('Ctrl Pts',(5.88662076592438,-58.7293455537172,
2.76354482594282));
#219999=CARTESIAN_POINT('Ctrl Pts',(5.87918707069805,-58.7418401303869,
2.78225519317093));
#220000=CARTESIAN_POINT('Ctrl Pts',(5.87375524644739,-58.7544760786592,
2.8015122308548));
#220001=CARTESIAN_POINT('Ctrl Pts',(5.86840094651664,-58.7669316835973,
2.82049442740227));
#220002=CARTESIAN_POINT('Ctrl Pts',(5.86499195787649,-58.7795255625973,
2.84000929089211));
#220003=CARTESIAN_POINT('Ctrl Pts',(5.86353919440045,-58.7920763953135,
2.85976644341564));
#220004=CARTESIAN_POINT('Ctrl Pts',(5.86252630185777,-58.8008270591842,
2.87354148166896));
#220005=CARTESIAN_POINT('Ctrl Pts',(5.86246534555209,-58.8095567514065,
2.88743438345442));
#220006=CARTESIAN_POINT('Ctrl Pts',(5.86337364149643,-58.8181995570482,
2.90134173515983));
#220007=CARTESIAN_POINT('',(5.90061356181316,-59.1725467709675,3.47153072139031));
#220008=CARTESIAN_POINT('',(5.86337364149639,-58.8181995570482,2.90134173515982));
#220009=CARTESIAN_POINT('',(0.316925998273675,-59.465175436383,3.4715307213903));
#220010=CARTESIAN_POINT('Origin',(5.53234440788222E-15,1.85015204418142E-13,
3.47153072139072));
#220011=CARTESIAN_POINT('',(0.316922544676313,-59.1088767419346,2.90134173515982));
#220012=CARTESIAN_POINT('',(0.316925998273675,-59.465175436383,3.47153072139031));
#220013=CARTESIAN_POINT('Ctrl Pts',(0.316922544676314,-59.1088767419346,
2.90134173515982));
#220014=CARTESIAN_POINT('Ctrl Pts',(0.316922401514487,-59.0966467827005,
2.88176998919813));
#220015=CARTESIAN_POINT('Ctrl Pts',(0.315000085554525,-59.0844716853564,
2.8622675235678));
#220016=CARTESIAN_POINT('Ctrl Pts',(0.311230629649952,-59.0725173476328,
2.84310370500122));
#220017=CARTESIAN_POINT('Ctrl Pts',(0.307393083606301,-59.0603470709146,
2.82359371788818));
#220018=CARTESIAN_POINT('Ctrl Pts',(0.301641096266063,-59.0484046750371,
2.80443322637214));
#220019=CARTESIAN_POINT('Ctrl Pts',(0.294001187896427,-59.0368573319862,
2.78589323878523));
#220020=CARTESIAN_POINT('Ctrl Pts',(0.286684733438826,-59.0257988735007,
2.76813818620329));
#220021=CARTESIAN_POINT('Ctrl Pts',(0.277636448050448,-59.0151019493867,
2.75095095199105));
#220022=CARTESIAN_POINT('Ctrl Pts',(0.26683517245673,-59.0049186873022,
2.7345777143556));
#220023=CARTESIAN_POINT('Ctrl Pts',(0.258244193038992,-58.9968192555069,
2.72155497955845));
#220024=CARTESIAN_POINT('Ctrl Pts',(0.248543417989038,-58.9890447295128,
2.70904711160066));
#220025=CARTESIAN_POINT('Ctrl Pts',(0.237702773060113,-58.9816789347248,
2.69718956158297));
#220026=CARTESIAN_POINT('Ctrl Pts',(0.237673181620855,-58.9816588284977,
2.69715719432314));
#220027=CARTESIAN_POINT('Ctrl Pts',(0.237643581717596,-58.9816387254914,
2.6971248321898));
#220028=CARTESIAN_POINT('Ctrl Pts',(0.23761397335091,-58.981618625708,2.69709247518608));
#220029=CARTESIAN_POINT('Ctrl Pts',(0.231719887007404,-58.977617396585,
2.69065122242234));
#220030=CARTESIAN_POINT('Ctrl Pts',(0.225454527233984,-58.973750718086,
2.68442464469383));
#220031=CARTESIAN_POINT('Ctrl Pts',(0.218853219641353,-58.9700384170934,
2.67844505923535));
#220032=CARTESIAN_POINT('Ctrl Pts',(0.20575246757055,-58.9626710986897,
2.66657815779524));
#220033=CARTESIAN_POINT('Ctrl Pts',(0.191327202906053,-58.9559120649694,
2.65568445664132));
#220034=CARTESIAN_POINT('Ctrl Pts',(0.175845309932871,-58.9499179036779,
2.64601906229473));
#220035=CARTESIAN_POINT('Ctrl Pts',(0.164233890202985,-58.9454222827093,
2.63877001653479));
#220036=CARTESIAN_POINT('Ctrl Pts',(0.152028117041922,-58.9413569016697,
2.63221189387559));
#220037=CARTESIAN_POINT('Ctrl Pts',(0.139341004226762,-58.937787832377,
2.62645231033191));
#220038=CARTESIAN_POINT('Ctrl Pts',(0.134583336921077,-58.9364494313922,
2.62429246650303));
#220039=CARTESIAN_POINT('Ctrl Pts',(0.129757981228087,-58.9351808244386,
2.62224491711703));
#220040=CARTESIAN_POINT('Ctrl Pts',(0.124870896863941,-58.9339854965858,
2.62031533672554));
#220041=CARTESIAN_POINT('Ctrl Pts',(0.107766101589432,-58.929801849101,
2.61356180535535));
#220042=CARTESIAN_POINT('Ctrl Pts',(0.0899051301006859,-58.9265158655227,
2.60825339735305));
#220043=CARTESIAN_POINT('Ctrl Pts',(0.0715435052832096,-58.9242770147324,
2.60463337987569));
#220044=CARTESIAN_POINT('Ctrl Pts',(0.0623626928744716,-58.9231575893373,
2.602823371137));
#220045=CARTESIAN_POINT('Ctrl Pts',(0.0530567171311952,-58.922299948158,
2.60143545939073));
#220046=CARTESIAN_POINT('Ctrl Pts',(0.0436575183860499,-58.9217227791367,
2.60050005034554));
#220047=CARTESIAN_POINT('Ctrl Pts',(0.0389579190134772,-58.921434194626,
2.60003234582295));
#220048=CARTESIAN_POINT('Ctrl Pts',(0.0342350138900813,-58.9212157281803,
2.59967776696023));
#220049=CARTESIAN_POINT('Ctrl Pts',(0.0294927955555056,-58.9210697160837,
2.59944011429117));
#220050=CARTESIAN_POINT('Ctrl Pts',(0.02475057722093,-58.9209237039871,
2.59920246162211));
#220051=CARTESIAN_POINT('Ctrl Pts',(0.0199890456756626,-58.920850147939,
2.5990817379127));
#220052=CARTESIAN_POINT('Ctrl Pts',(0.015212193456543,-58.9208513795071,
2.59908173515982));
#220053=CARTESIAN_POINT('',(-0.316922544675051,-59.1088767419346,2.90134173515982));
#220054=CARTESIAN_POINT('Ctrl Pts',(-0.015212193455297,-58.9208513795071,
2.59908173515982));
#220055=CARTESIAN_POINT('Ctrl Pts',(-0.0190220008279213,-58.9208504012362,
2.59908174371469));
#220056=CARTESIAN_POINT('Ctrl Pts',(-0.022821409981102,-58.9208964366349,
2.59915764355849));
#220057=CARTESIAN_POINT('Ctrl Pts',(-0.0266084895323855,-58.9209883940805,
2.59930765775236));
#220058=CARTESIAN_POINT('Ctrl Pts',(-0.0489671208120116,-58.9215313038854,
2.60019333020838));
#220059=CARTESIAN_POINT('Ctrl Pts',(-0.0708986527588113,-58.9236732325283,
2.60365973324034));
#220060=CARTESIAN_POINT('Ctrl Pts',(-0.0919988953488922,-58.9271900305692,
2.60934177082313));
#220061=CARTESIAN_POINT('Ctrl Pts',(-0.0998812435853016,-58.9285037892484,
2.6114643909176));
#220062=CARTESIAN_POINT('Ctrl Pts',(-0.107647933245444,-58.9300091878193,
2.61389584429252));
#220063=CARTESIAN_POINT('Ctrl Pts',(-0.115279202946303,-58.9316938830315,
2.61661604385212));
#220064=CARTESIAN_POINT('Ctrl Pts',(-0.121233502389606,-58.9330083667488,
2.61873848000735));
#220065=CARTESIAN_POINT('Ctrl Pts',(-0.127104908279396,-58.9344322364589,
2.62103707099747));
#220066=CARTESIAN_POINT('Ctrl Pts',(-0.132883578272457,-58.9359598525091,
2.62350262767611));
#220067=CARTESIAN_POINT('Ctrl Pts',(-0.15310892324817,-58.9413065086847,
2.63213207605138));
#220068=CARTESIAN_POINT('Ctrl Pts',(-0.172198253417102,-58.9479240485793,
2.64280685971873));
#220069=CARTESIAN_POINT('Ctrl Pts',(-0.189729578870158,-58.9555707636543,
2.65513293646042));
#220070=CARTESIAN_POINT('Ctrl Pts',(-0.198495241596686,-58.9593941211918,
2.66129597483127));
#220071=CARTESIAN_POINT('Ctrl Pts',(-0.206871403159931,-58.9634747743346,
2.6678718353381));
#220072=CARTESIAN_POINT('Ctrl Pts',(-0.214805314862594,-58.9677825146335,
2.67481125953819));
#220073=CARTESIAN_POINT('Ctrl Pts',(-0.222705329147009,-58.972071850231,
2.68172103524038));
#220074=CARTESIAN_POINT('Ctrl Pts',(-0.230167055078558,-58.9765861722456,
2.68899101329746));
#220075=CARTESIAN_POINT('Ctrl Pts',(-0.237137844566027,-58.9812961520163,
2.69657334701232));
#220076=CARTESIAN_POINT('Ctrl Pts',(-0.23716775486217,-58.9813163616195,
2.69660588132529));
#220077=CARTESIAN_POINT('Ctrl Pts',(-0.237197656536079,-58.9813365744743,
2.69663842081338));
#220078=CARTESIAN_POINT('Ctrl Pts',(-0.23722754958733,-58.9813567905787,
2.69667096547338));
#220079=CARTESIAN_POINT('Ctrl Pts',(-0.251324537971816,-58.9908903168209,
2.71201840157907));
#220080=CARTESIAN_POINT('Ctrl Pts',(-0.26350158051193,-59.0011093202329,
2.72845645939327));
#220081=CARTESIAN_POINT('Ctrl Pts',(-0.273820596508964,-59.0118294103847,
2.74568723186887));
#220082=CARTESIAN_POINT('Ctrl Pts',(-0.284514998003945,-59.0229394763229,
2.76354482594332));
#220083=CARTESIAN_POINT('Ctrl Pts',(-0.293214009568506,-59.034588573656,
2.78225519317159));
#220084=CARTESIAN_POINT('Ctrl Pts',(-0.2999368939724,-59.04658752064,2.80151223085562));
#220085=CARTESIAN_POINT('Ctrl Pts',(-0.306563827731156,-59.0584152157275,
2.82049442740328));
#220086=CARTESIAN_POINT('Ctrl Pts',(-0.311270560393252,-59.0705837677968,
2.84000929089333));
#220087=CARTESIAN_POINT('Ctrl Pts',(-0.314027284735468,-59.0829139906047,
2.85976644341707));
#220088=CARTESIAN_POINT('Ctrl Pts',(-0.315949321993669,-59.0915108413219,
2.87354148166992));
#220089=CARTESIAN_POINT('Ctrl Pts',(-0.316922445687073,-59.1001863397075,
2.88743438345489));
#220090=CARTESIAN_POINT('Ctrl Pts',(-0.316922544675027,-59.1088767419346,
2.90134173515982));
#220091=CARTESIAN_POINT('',(-0.316925998272418,-59.465175436383,3.47153072139031));
#220092=CARTESIAN_POINT('',(-0.316922544675064,-59.1088767419346,2.90134173515982));
#220093=CARTESIAN_POINT('',(-5.90061356181196,-59.1725467709676,3.47153072139031));
#220094=CARTESIAN_POINT('Origin',(5.53234440788222E-15,1.85015204418142E-13,
3.47153072139072));
#220095=CARTESIAN_POINT('',(-5.8633736414952,-58.8181995570483,2.90134173515982));
#220096=CARTESIAN_POINT('',(-5.90061356181196,-59.1725467709676,3.47153072139031));
#220097=CARTESIAN_POINT('',(-6.14377718965262,-58.5996668978647,2.59908173515982));
#220098=CARTESIAN_POINT('Ctrl Pts',(-5.8633736414952,-58.8181995570483,
2.90134173515982));
#220099=CARTESIAN_POINT('Ctrl Pts',(-5.86209540502805,-58.8060365798449,
2.88176998919624));
#220100=CARTESIAN_POINT('Ctrl Pts',(-5.86273454612475,-58.7937272422236,
2.86226752356404));
#220101=CARTESIAN_POINT('Ctrl Pts',(-5.86523378400442,-58.7814443761786,
2.84310370499567));
#220102=CARTESIAN_POINT('Ctrl Pts',(-5.86777816724702,-58.7689396367177,
2.82359371788075));
#220103=CARTESIAN_POINT('Ctrl Pts',(-5.87225032431096,-58.7564614161358,
2.80443322636292));
#220104=CARTESIAN_POINT('Ctrl Pts',(-5.87864135444063,-58.7441787427558,
2.7858932387744));
#220105=CARTESIAN_POINT('Ctrl Pts',(-5.88476180492493,-58.7324160859207,
2.76813818619086));
#220106=CARTESIAN_POINT('Ctrl Pts',(-5.89264238982162,-58.7208319573083,
2.75095095197719));
#220107=CARTESIAN_POINT('Ctrl Pts',(-5.90232005416286,-58.7095754394589,
2.73457771434054));
#220108=CARTESIAN_POINT('Ctrl Pts',(-5.91001735013549,-58.7006223753256,
2.72155497954881));
#220109=CARTESIAN_POINT('Ctrl Pts',(-5.91885232406698,-58.6918764318934,
2.70904711159609));
#220110=CARTESIAN_POINT('Ctrl Pts',(-5.92886364759491,-58.6834178317479,
2.69718956158297));
#220111=CARTESIAN_POINT('Ctrl Pts',(-5.92889097525615,-58.6833947425171,
2.69715719432314));
#220112=CARTESIAN_POINT('Ctrl Pts',(-5.92891831167169,-58.6833716556048,
2.6971248321898));
#220113=CARTESIAN_POINT('Ctrl Pts',(-5.92894565684117,-58.683348571013,
2.69709247518608));
#220114=CARTESIAN_POINT('Ctrl Pts',(-5.93438921243157,-58.678753161254,
2.69065122242233));
#220115=CARTESIAN_POINT('Ctrl Pts',(-5.94021607194716,-58.6742527563955,
2.68442464469383));
#220116=CARTESIAN_POINT('Ctrl Pts',(-5.94639317576815,-58.6698707672379,
2.67844505923536));
#220117=CARTESIAN_POINT('Ctrl Pts',(-5.95865206607721,-58.6611744062937,
2.66657815779524));
#220118=CARTESIAN_POINT('Ctrl Pts',(-5.97229179622458,-58.6529445485197,
2.65568445664132));
#220119=CARTESIAN_POINT('Ctrl Pts',(-5.98706231729978,-58.64536492539,2.64601906229473));
#220120=CARTESIAN_POINT('Ctrl Pts',(-5.99814020810618,-58.6396802080427,
2.63877001653479));
#220121=CARTESIAN_POINT('Ctrl Pts',(-6.00985416873209,-58.6343612468743,
2.63221189387559));
#220122=CARTESIAN_POINT('Ctrl Pts',(-6.02209871088731,-58.6294855649107,
2.62645231033191));
#220123=CARTESIAN_POINT('Ctrl Pts',(-6.02669041419552,-58.6276571841744,
2.62429246650303));
#220124=CARTESIAN_POINT('Ctrl Pts',(-6.03135673054979,-58.6258911397671,
2.62224491711703));
#220125=CARTESIAN_POINT('Ctrl Pts',(-6.03609209717089,-58.6241915206269,
2.62031533672554));
#220126=CARTESIAN_POINT('Ctrl Pts',(-6.05266588034474,-58.6182428536362,
2.61356180535535));
#220127=CARTESIAN_POINT('Ctrl Pts',(-6.07008552874908,-58.6131078911175,
2.60825339735306));
#220128=CARTESIAN_POINT('Ctrl Pts',(-6.088112543032,-58.6089619925609,2.60463337987569));
#220129=CARTESIAN_POINT('Ctrl Pts',(-6.09712605017347,-58.6068890432826,
2.60282337113701));
#220130=CARTESIAN_POINT('Ctrl Pts',(-6.10629139889341,-58.6050633610077,
2.60143545939073));
#220131=CARTESIAN_POINT('Ctrl Pts',(-6.11557877725353,-58.6035068699779,
2.60050005034554));
#220132=CARTESIAN_POINT('Ctrl Pts',(-6.12022246643359,-58.602728624463,
2.60003234582295));
#220133=CARTESIAN_POINT('Ctrl Pts',(-6.12489666302672,-58.6020176767847,
2.59967776696024));
#220134=CARTESIAN_POINT('Ctrl Pts',(-6.12959764057299,-58.6013767677626,
2.59944011429119));
#220135=CARTESIAN_POINT('Ctrl Pts',(-6.13429861811926,-58.6007358587405,
2.59920246162213));
#220136=CARTESIAN_POINT('Ctrl Pts',(-6.13902637679584,-58.6001649900649,
2.59908173791266));
#220137=CARTESIAN_POINT('Ctrl Pts',(-6.14377718965262,-58.5996668978647,
2.59908173515982));
#220138=CARTESIAN_POINT('',(-6.17403490858961,-58.5964866834549,2.59908173515982));
#220139=CARTESIAN_POINT('Origin',(3.95370119046988E-16,1.9103972218437E-13,
2.59908173516024));
#220140=CARTESIAN_POINT('',(-6.4937464611268,-58.7519447039087,2.90134173515982));
#220141=CARTESIAN_POINT('Ctrl Pts',(-6.17403490858961,-58.5964866834549,
2.59908173515983));
#220142=CARTESIAN_POINT('Ctrl Pts',(-6.17782374318166,-58.5960874772331,
2.5990817437147));
#220143=CARTESIAN_POINT('Ctrl Pts',(-6.18160715078344,-58.595736114045,
2.5991576435585));
#220144=CARTESIAN_POINT('Ctrl Pts',(-6.18538309648717,-58.5954317101323,
2.59930765775236));
#220145=CARTESIAN_POINT('Ctrl Pts',(-6.20767599437393,-58.593634532452,
2.60019333020843));
#220146=CARTESIAN_POINT('Ctrl Pts',(-6.22971127560455,-58.5934722580542,
2.60365973324068));
#220147=CARTESIAN_POINT('Ctrl Pts',(-6.2510635343538,-58.5947642147752,
2.60934177082398));
#220148=CARTESIAN_POINT('Ctrl Pts',(-6.25904002743657,-58.5952468467987,
2.61146439091825));
#220149=CARTESIAN_POINT('Ctrl Pts',(-6.26692152735626,-58.5959321585038,
2.61389584429287));
#220150=CARTESIAN_POINT('Ctrl Pts',(-6.27468709076379,-58.5968099398847,
2.61661604385211));
#220151=CARTESIAN_POINT('Ctrl Pts',(-6.2807461728947,-58.597494828952,2.61873848000734));
#220152=CARTESIAN_POINT('Ctrl Pts',(-6.28673424952138,-58.59829716952,2.62103707099745));
#220153=CARTESIAN_POINT('Ctrl Pts',(-6.29264094271378,-58.5992123816355,
2.6235026276761));
#220154=CARTESIAN_POINT('Ctrl Pts',(-6.31331436888716,-58.6024156240397,
2.63213207605136));
#220155=CARTESIAN_POINT('Ctrl Pts',(-6.33299084698388,-58.6070015340111,
2.64280685971873));
#220156=CARTESIAN_POINT('Ctrl Pts',(-6.35122543337761,-58.6127738370721,
2.65513293646043));
#220157=CARTESIAN_POINT('Ctrl Pts',(-6.36034272657447,-58.6156599886027,
2.66129597483128));
#220158=CARTESIAN_POINT('Ctrl Pts',(-6.36909954705041,-58.6188427402043,
2.6678718353381));
#220159=CARTESIAN_POINT('Ctrl Pts',(-6.37744027742822,-58.6222975626531,
2.67481125953819));
#220160=CARTESIAN_POINT('Ctrl Pts',(-6.38574537226625,-58.6257376244685,
2.68172103524038));
#220161=CARTESIAN_POINT('Ctrl Pts',(-6.39363809722528,-58.6294472538098,
2.68899101329747));
#220162=CARTESIAN_POINT('Ctrl Pts',(-6.40106302694602,-58.6334027859056,
2.69657334701232));
#220163=CARTESIAN_POINT('Ctrl Pts',(-6.40109488586921,-58.6334197583212,
2.6966058813253));
#220164=CARTESIAN_POINT('Ctrl Pts',(-6.40112673655726,-58.6334367348719,
2.69663842081339));
#220165=CARTESIAN_POINT('Ctrl Pts',(-6.40115857900958,-58.6334537155556,
2.69667096547339));
#220166=CARTESIAN_POINT('Ctrl Pts',(-6.41617486746338,-58.6414614796105,
2.71201840157812));
#220167=CARTESIAN_POINT('Ctrl Pts',(-6.42935337961243,-58.6503516547081,
2.72845645939122));
#220168=CARTESIAN_POINT('Ctrl Pts',(-6.44073642150931,-58.6599343881991,
2.74568723186565));
#220169=CARTESIAN_POINT('Ctrl Pts',(-6.45253355607274,-58.6698657226791,
2.76354482593886));
#220170=CARTESIAN_POINT('Ctrl Pts',(-6.46240257578417,-58.6805417107265,
2.78225519316581));
#220171=CARTESIAN_POINT('Ctrl Pts',(-6.47034286301293,-58.6917721934471,
2.80151223084849));
#220172=CARTESIAN_POINT('Ctrl Pts',(-6.4781698245267,-58.7028423919807,
2.82049442739492));
#220173=CARTESIAN_POINT('Ctrl Pts',(-6.48412273326305,-58.7144522959155,
2.84000929088371));
#220174=CARTESIAN_POINT('Ctrl Pts',(-6.48815321522321,-58.7264268163128,
2.85976644340622));
#220175=CARTESIAN_POINT('Ctrl Pts',(-6.49096333895585,-58.7347756649834,
2.87354148166263));
#220176=CARTESIAN_POINT('Ctrl Pts',(-6.49283796829092,-58.7433019189591,
2.88743438345124));
#220177=CARTESIAN_POINT('Ctrl Pts',(-6.49374646112681,-58.7519447039087,
2.90134173515981));
#220178=CARTESIAN_POINT('',(-6.53099325079995,-59.1062911958295,3.47153072139031));
#220179=CARTESIAN_POINT('',(-6.49374646112681,-58.7519447039087,2.90134173515982));
#220180=CARTESIAN_POINT('',(-12.0535047649316,-58.231611300478,3.47153072139032));
#220181=CARTESIAN_POINT('Origin',(5.53234440788222E-15,1.85015204418142E-13,
3.47153072139072));
#220182=CARTESIAN_POINT('',(-11.9794294790606,-57.8830978693155,2.90134173515983));
#220183=CARTESIAN_POINT('',(-12.0535047649316,-58.231611300478,3.47153072139032));
#220184=CARTESIAN_POINT('',(-12.2354540642039,-57.6364522029206,2.59908173515983));
#220185=CARTESIAN_POINT('Ctrl Pts',(-11.9794294790606,-57.8830978693155,
2.90134173515983));
#220186=CARTESIAN_POINT('Ctrl Pts',(-11.9768868675909,-57.8711351342679,
2.8817699891971));
#220187=CARTESIAN_POINT('Ctrl Pts',(-11.9762358312604,-57.8588264200499,
2.86226752356573));
#220188=CARTESIAN_POINT('Ctrl Pts',(-11.9774374689411,-57.8463495993359,
2.84310370499817));
#220189=CARTESIAN_POINT('Ctrl Pts',(-11.9786608125864,-57.8336474016765,
2.82359371788415));
#220190=CARTESIAN_POINT('Ctrl Pts',(-11.9818041414839,-57.8207700703878,
2.80443322636717));
#220191=CARTESIAN_POINT('Ctrl Pts',(-11.986876271908,-57.8078866382202,
2.78589323877943));
#220192=CARTESIAN_POINT('Ctrl Pts',(-11.9917336614806,-57.7955486571671,
2.76813818619671));
#220193=CARTESIAN_POINT('Ctrl Pts',(-11.9983602045457,-57.783204242195,
2.75095095198379));
#220194=CARTESIAN_POINT('Ctrl Pts',(-12.0068082271156,-57.7709977973472,
2.73457771434777));
#220195=CARTESIAN_POINT('Ctrl Pts',(-12.0135275064609,-57.7612891925148,
2.72155497955344));
#220196=CARTESIAN_POINT('Ctrl Pts',(-12.0213998814552,-57.751667654026,
2.70904711159829));
#220197=CARTESIAN_POINT('Ctrl Pts',(-12.0304721974324,-57.7422089227117,
2.69718956158298));
#220198=CARTESIAN_POINT('Ctrl Pts',(-12.030496961908,-57.7421831034477,
2.69715719432316));
#220199=CARTESIAN_POINT('Ctrl Pts',(-12.0305217353324,-57.7421572855745,
2.69712483218981));
#220200=CARTESIAN_POINT('Ctrl Pts',(-12.0305465177052,-57.7421314690939,
2.69709247518609));
#220201=CARTESIAN_POINT('Ctrl Pts',(-12.0354799018083,-57.7369922269698,
2.69065122242235));
#220202=CARTESIAN_POINT('Ctrl Pts',(-12.0408044207739,-57.7319074031291,
2.68442464469384));
#220203=CARTESIAN_POINT('Ctrl Pts',(-12.0464896431811,-57.7269037357968,
2.67844505923537));
#220204=CARTESIAN_POINT('Ctrl Pts',(-12.0577723607609,-57.7169736114624,
2.66657815779526));
#220205=CARTESIAN_POINT('Ctrl Pts',(-12.0704771166533,-57.7073630976787,
2.65568445664133));
#220206=CARTESIAN_POINT('Ctrl Pts',(-12.0843744369107,-57.6982810566479,
2.64601906229474));
#220207=CARTESIAN_POINT('Ctrl Pts',(-12.0947974271037,-57.6914695258748,
2.6387700165348));
#220208=CARTESIAN_POINT('Ctrl Pts',(-12.1058912345906,-57.6849552602292,
2.6322118938756));
#220209=CARTESIAN_POINT('Ctrl Pts',(-12.1175590523197,-57.6788263845867,
2.62645231033191));
#220210=CARTESIAN_POINT('Ctrl Pts',(-12.1219344839681,-57.6765280562207,
2.62429246650303));
#220211=CARTESIAN_POINT('Ctrl Pts',(-12.1263906358452,-57.6742839235119,
2.62224491711704));
#220212=CARTESIAN_POINT('Ctrl Pts',(-12.1309224030556,-57.6720986344672,
2.62031533672556));
#220213=CARTESIAN_POINT('Ctrl Pts',(-12.146783588292,-57.664450122811,2.61356180535537));
#220214=CARTESIAN_POINT('Ctrl Pts',(-12.1635710602988,-57.657522441076,
2.60825339735306));
#220215=CARTESIAN_POINT('Ctrl Pts',(-12.1810659563062,-57.6515149180851,
2.6046333798757));
#220216=CARTESIAN_POINT('Ctrl Pts',(-12.18981340431,-57.6485111565897,2.60282337113701));
#220217=CARTESIAN_POINT('Ctrl Pts',(-12.1987377085281,-57.6457374357763,
2.60143545939073));
#220218=CARTESIAN_POINT('Ctrl Pts',(-12.2078115120423,-57.6432186759795,
2.60050005034555));
#220219=CARTESIAN_POINT('Ctrl Pts',(-12.2123484137995,-57.6419592960811,
2.60003234582295));
#220220=CARTESIAN_POINT('Ctrl Pts',(-12.2169226903863,-57.6407636564616,
2.59967776696024));
#220221=CARTESIAN_POINT('Ctrl Pts',(-12.2215309222505,-57.6396348724474,
2.59944011429118));
#220222=CARTESIAN_POINT('Ctrl Pts',(-12.2261391541148,-57.6385060884332,
2.59920246162212));
#220223=CARTESIAN_POINT('Ctrl Pts',(-12.2307813416093,-57.6374441616868,
2.5990817379127));
#220224=CARTESIAN_POINT('Ctrl Pts',(-12.2354540642039,-57.6364522029206,
2.59908173515984));
#220225=CARTESIAN_POINT('',(-12.2652136052655,-57.6301266171957,2.59908173515984));
#220226=CARTESIAN_POINT('Origin',(3.88326186679512E-16,1.91040837833656E-13,
2.59908173516024));
#220227=CARTESIAN_POINT('',(-12.5994235324466,-57.7513140650719,2.90134173515983));
#220228=CARTESIAN_POINT('Ctrl Pts',(-12.2652136052655,-57.6301266171957,
2.59908173515984));
#220229=CARTESIAN_POINT('Ctrl Pts',(-12.2689399558123,-57.6293335568098,
2.59908174371468));
#220230=CARTESIAN_POINT('Ctrl Pts',(-12.2726659100573,-57.6285886446434,
2.5991576435585));
#220231=CARTESIAN_POINT('Ctrl Pts',(-12.2763893518622,-57.6278912144855,
2.59930765775236));
#220232=CARTESIAN_POINT('Ctrl Pts',(-12.2983722706983,-57.6237736395751,
2.60019333020834));
#220233=CARTESIAN_POINT('Ctrl Pts',(-12.3202698780571,-57.6213089400488,
2.60365973323998));
#220234=CARTESIAN_POINT('Ctrl Pts',(-12.3416402131473,-57.6203619005011,
2.60934177082223));
#220235=CARTESIAN_POINT('Ctrl Pts',(-12.3496234589524,-57.6200081180515,
2.61146439091692));
#220236=CARTESIAN_POINT('Ctrl Pts',(-12.3575334177725,-57.6198658344725,
2.61389584429214));
#220237=CARTESIAN_POINT('Ctrl Pts',(-12.3653481937522,-57.6199270848657,
2.61661604385214));
#220238=CARTESIAN_POINT('Ctrl Pts',(-12.3714456739989,-57.6199748754951,
2.61873848000737));
#220239=CARTESIAN_POINT('Ctrl Pts',(-12.3774848147419,-57.6201468963097,
2.62103707099747));
#220240=CARTESIAN_POINT('Ctrl Pts',(-12.3834548161669,-57.6204396772351,
2.62350262767612));
#220241=CARTESIAN_POINT('Ctrl Pts',(-12.4043498211546,-57.6214644104739,
2.63213207605139));
#220242=CARTESIAN_POINT('Ctrl Pts',(-12.4243978675675,-57.6239684463326,
2.64280685971874));
#220243=CARTESIAN_POINT('Ctrl Pts',(-12.4431359329576,-57.6278030948195,
2.65513293646044));
#220244=CARTESIAN_POINT('Ctrl Pts',(-12.4525049656526,-57.629720419063,
2.66129597483128));
#220245=CARTESIAN_POINT('Ctrl Pts',(-12.4615465034836,-57.6319703982309,
2.66787183533812));
#220246=CARTESIAN_POINT('Ctrl Pts',(-12.4702026697491,-57.6345344510719,
2.67481125953822));
#220247=CARTESIAN_POINT('Ctrl Pts',(-12.4788218527838,-57.637087549068,
2.6817210352404));
#220248=CARTESIAN_POINT('Ctrl Pts',(-12.487059102424,-57.6399518422607,
2.68899101329748));
#220249=CARTESIAN_POINT('Ctrl Pts',(-12.4948568232942,-57.6431095890442,
2.69657334701234));
#220250=CARTESIAN_POINT('Ctrl Pts',(-12.4948902817914,-57.6431231383188,
2.69660588132531));
#220251=CARTESIAN_POINT('Ctrl Pts',(-12.4949237325308,-57.6431366925667,
2.6966384208134));
#220252=CARTESIAN_POINT('Ctrl Pts',(-12.4949571755116,-57.6431502517858,
2.6966709654734));
#220253=CARTESIAN_POINT('Ctrl Pts',(-12.5107282424373,-57.6495445189154,
2.71201840157843));
#220254=CARTESIAN_POINT('Ctrl Pts',(-12.5247638376593,-57.6570084630808,
2.72845645939189));
#220255=CARTESIAN_POINT('Ctrl Pts',(-12.5370861904675,-57.6653488494784,
2.74568723186669));
#220256=CARTESIAN_POINT('Ctrl Pts',(-12.549856806225,-57.6739926427224,
2.76354482594026));
#220257=CARTESIAN_POINT('Ctrl Pts',(-12.5607877070384,-57.683578553126,
2.78225519316758));
#220258=CARTESIAN_POINT('Ctrl Pts',(-12.5698584016435,-57.6939175280655,
2.80151223085064));
#220259=CARTESIAN_POINT('Ctrl Pts',(-12.5787996370839,-57.7041089426343,
2.82049442739735));
#220260=CARTESIAN_POINT('Ctrl Pts',(-12.5859335005802,-57.7150329978987,
2.84000929088641));
#220261=CARTESIAN_POINT('Ctrl Pts',(-12.5911935813539,-57.7265206205349,
2.85976644340919));
#220262=CARTESIAN_POINT('Ctrl Pts',(-12.5948610032559,-57.7345299954231,
2.87354148166462));
#220263=CARTESIAN_POINT('Ctrl Pts',(-12.5976165994005,-57.7428135895632,
2.88743438345224));
#220264=CARTESIAN_POINT('Ctrl Pts',(-12.5994235324466,-57.7513140650719,
2.90134173515982));
#220265=CARTESIAN_POINT('',(-12.6735055745735,-58.0998260601479,3.47153072139032));
#220266=CARTESIAN_POINT('',(-12.5994235324466,-57.7513140650719,2.90134173515983));
#220267=CARTESIAN_POINT('',(-18.0743352474886,-56.6526781108323,3.47153072139033));
#220268=CARTESIAN_POINT('Origin',(5.53234440788222E-15,1.85015204418142E-13,
3.47153072139072));
#220269=CARTESIAN_POINT('',(-17.9642361803967,-56.3138168485095,2.90134173515983));
#220270=CARTESIAN_POINT('',(-18.0743352474886,-56.6526781108323,3.47153072139033));
#220271=CARTESIAN_POINT('',(-18.1930767435944,-56.0417604764383,2.59908173515983));
#220272=CARTESIAN_POINT('Ctrl Pts',(-17.9642361803967,-56.3138168485095,
2.90134173515983));
#220273=CARTESIAN_POINT('Ctrl Pts',(-17.9604570513079,-56.3021854218459,
2.88176998919747));
#220274=CARTESIAN_POINT('Ctrl Pts',(-17.9585229704406,-56.2900121878797,
2.86226752356647));
#220275=CARTESIAN_POINT('Ctrl Pts',(-17.9584138425285,-56.2774781111551,
2.84310370499926));
#220276=CARTESIAN_POINT('Ctrl Pts',(-17.9583027433679,-56.2647176232326,
2.8235937178857));
#220277=CARTESIAN_POINT('Ctrl Pts',(-17.96008280513,-56.2515822679732,2.80443322636917));
#220278=CARTESIAN_POINT('Ctrl Pts',(-17.9637804645265,-56.2382392305966,
2.78589323878182));
#220279=CARTESIAN_POINT('Ctrl Pts',(-17.9673215746112,-56.2254611028276,
2.76813818619968));
#220280=CARTESIAN_POINT('Ctrl Pts',(-17.9726214740526,-56.2124916494895,
2.75095095198728));
#220281=CARTESIAN_POINT('Ctrl Pts',(-17.9797472965484,-56.1994690140074,
2.7345777143517));
#220282=CARTESIAN_POINT('Ctrl Pts',(-17.9854149414351,-56.1891112379828,
2.72155497955596));
#220283=CARTESIAN_POINT('Ctrl Pts',(-17.9922384661036,-56.1787195200271,
2.70904711159949));
#220284=CARTESIAN_POINT('Ctrl Pts',(-18.0002723763367,-56.1683642893842,
2.69718956158298));
#220285=CARTESIAN_POINT('Ctrl Pts',(-18.0002943063019,-56.1683360229683,
2.69715719432316));
#220286=CARTESIAN_POINT('Ctrl Pts',(-18.0003162453122,-56.168307757,2.69712483218981));
#220287=CARTESIAN_POINT('Ctrl Pts',(-18.0003381933676,-56.1682794914815,
2.69709247518609));
#220288=CARTESIAN_POINT('Ctrl Pts',(-18.0047073547948,-56.1626527236045,
2.69065122242235));
#220289=CARTESIAN_POINT('Ctrl Pts',(-18.0094711966663,-56.1570391911757,
2.68442464469385));
#220290=CARTESIAN_POINT('Ctrl Pts',(-18.0146022491734,-56.1514686668951,
2.67844505923538));
#220291=CARTESIAN_POINT('Ctrl Pts',(-18.024785178209,-56.1404135756906,
2.66657815779526));
#220292=CARTESIAN_POINT('Ctrl Pts',(-18.0364157638823,-56.1295277006974,
2.65568445664133));
#220293=CARTESIAN_POINT('Ctrl Pts',(-18.049287621373,-56.1190427465076,
2.64601906229474));
#220294=CARTESIAN_POINT('Ctrl Pts',(-18.0589415144909,-56.1111790308652,
2.6387700165348));
#220295=CARTESIAN_POINT('Ctrl Pts',(-18.0692936227623,-56.1035408324,2.6322118938756));
#220296=CARTESIAN_POINT('Ctrl Pts',(-18.0802568810126,-56.0962259123227,
2.62645231033192));
#220297=CARTESIAN_POINT('Ctrl Pts',(-18.0843681028565,-56.0934828172937,
2.62429246650304));
#220298=CARTESIAN_POINT('Ctrl Pts',(-18.0885652677239,-56.0907851834708,
2.62224491711704));
#220299=CARTESIAN_POINT('Ctrl Pts',(-18.0928437845337,-56.0881381670058,
2.62031533672556));
#220300=CARTESIAN_POINT('Ctrl Pts',(-18.1078185933682,-56.0788736093783,
2.61356180535537));
#220301=CARTESIAN_POINT('Ctrl Pts',(-18.123789961921,-56.0702291095577,
2.60825339735306));
#220302=CARTESIAN_POINT('Ctrl Pts',(-18.1405610619113,-56.0624257818116,
2.60463337987569));
#220303=CARTESIAN_POINT('Ctrl Pts',(-18.1489466119065,-56.0585241179386,
2.60282337113701));
#220304=CARTESIAN_POINT('Ctrl Pts',(-18.1575320950781,-56.0548327480525,
2.60143545939074));
#220305=CARTESIAN_POINT('Ctrl Pts',(-18.1662929092565,-56.051379315548,
2.60050005034556));
#220306=CARTESIAN_POINT('Ctrl Pts',(-18.1706733163456,-56.0496525992958,
2.60003234582296));
#220307=CARTESIAN_POINT('Ctrl Pts',(-18.1750975561947,-56.0479853674131,
2.59967776696025));
#220308=CARTESIAN_POINT('Ctrl Pts',(-18.1795625536242,-56.0463810756007,
2.59944011429119));
#220309=CARTESIAN_POINT('Ctrl Pts',(-18.1840275510537,-56.0447767837883,
2.59920246162213));
#220310=CARTESIAN_POINT('Ctrl Pts',(-18.1885333065885,-56.0432354336627,
2.59908173791271));
#220311=CARTESIAN_POINT('Ctrl Pts',(-18.1930767435944,-56.0417604764383,
2.59908173515984));
#220312=CARTESIAN_POINT('',(-18.2220120550212,-56.0323588238391,2.59908173515983));
#220313=CARTESIAN_POINT('Origin',(3.81437458815951E-16,1.91042683662724E-13,
2.59908173516023));
#220314=CARTESIAN_POINT('',(-18.567058682946,-56.1179479440988,2.90134173515983));
#220315=CARTESIAN_POINT('Ctrl Pts',(-18.2220120550212,-56.0323588238391,
2.59908173515984));
#220316=CARTESIAN_POINT('Ctrl Pts',(-18.2256350948464,-56.0311805982248,
2.59908174371473));
#220317=CARTESIAN_POINT('Ctrl Pts',(-18.2292627734001,-56.0300502984937,
2.5991576435585));
#220318=CARTESIAN_POINT('Ctrl Pts',(-18.2328929164986,-56.0289674832812,
2.59930765775237));
#220319=CARTESIAN_POINT('Ctrl Pts',(-18.2543250068291,-56.0225746241524,
2.60019333020841));
#220320=CARTESIAN_POINT('Ctrl Pts',(-18.2758450255513,-56.0178345032614,
2.6036597332405));
#220321=CARTESIAN_POINT('Ctrl Pts',(-18.2969992991229,-56.0146588434089,
2.60934177082352));
#220322=CARTESIAN_POINT('Ctrl Pts',(-18.3049018315347,-56.013472522601,
2.6114643909179));
#220323=CARTESIAN_POINT('Ctrl Pts',(-18.3127535860873,-56.0125042026265,
2.61389584429268));
#220324=CARTESIAN_POINT('Ctrl Pts',(-18.3205319543143,-56.0117482509599,
2.61661604385212));
#220325=CARTESIAN_POINT('Ctrl Pts',(-18.3266010274073,-56.0111584195472,
2.61873848000736));
#220326=CARTESIAN_POINT('Ctrl Pts',(-18.3326250661768,-56.0106982359126,
2.62103707099747));
#220327=CARTESIAN_POINT('Ctrl Pts',(-18.3385929672496,-56.0103653778788,
2.62350262767612));
#220328=CARTESIAN_POINT('Ctrl Pts',(-18.3594806210044,-56.0092003747603,
2.63213207605138));
#220329=CARTESIAN_POINT('Ctrl Pts',(-18.3796805851417,-56.0095951017655,
2.64280685971873));
#220330=CARTESIAN_POINT('Ctrl Pts',(-18.3987168313625,-56.011450082467,
2.65513293646043));
#220331=CARTESIAN_POINT('Ctrl Pts',(-18.4082349544728,-56.0123775728177,
2.66129597483128));
#220332=CARTESIAN_POINT('Ctrl Pts',(-18.4174621486784,-56.0136701283092,
2.66787183533812));
#220333=CARTESIAN_POINT('Ctrl Pts',(-18.4263389120626,-56.0153153192429,
2.67481125953821));
#220334=CARTESIAN_POINT('Ctrl Pts',(-18.4351777497209,-56.0169534811439,
2.6817210352404));
#220335=CARTESIAN_POINT('Ctrl Pts',(-18.4436692750114,-56.0189410563923,
2.68899101329748));
#220336=CARTESIAN_POINT('Ctrl Pts',(-18.4517543535695,-56.021266420929,
2.69657334701234));
#220337=CARTESIAN_POINT('Ctrl Pts',(-18.4517890450624,-56.021276398614,
2.69660588132531));
#220338=CARTESIAN_POINT('Ctrl Pts',(-18.4518237293599,-56.0212863820559,
2.6966384208134));
#220339=CARTESIAN_POINT('Ctrl Pts',(-18.4518584064609,-56.0212963712528,
2.6966709654734));
#220340=CARTESIAN_POINT('Ctrl Pts',(-18.4682114607484,-56.0260070845282,
2.71201840157833));
#220341=CARTESIAN_POINT('Ctrl Pts',(-18.4829503621247,-56.0319630212268,
2.72845645939167));
#220342=CARTESIAN_POINT('Ctrl Pts',(-18.4960770195681,-56.0389696815121,
2.74568723186634));
#220343=CARTESIAN_POINT('Ctrl Pts',(-18.5096811989808,-56.0462312303121,
2.76354482593977));
#220344=CARTESIAN_POINT('Ctrl Pts',(-18.5215542196593,-56.0546220378313,
2.78225519316695));
#220345=CARTESIAN_POINT('Ctrl Pts',(-18.5316559412124,-56.0639562290164,
2.80151223084986));
#220346=CARTESIAN_POINT('Ctrl Pts',(-18.5416134885329,-56.0731572003494,
2.8204944273964));
#220347=CARTESIAN_POINT('Ctrl Pts',(-18.549850146688,-56.0832757207075,
2.84000929088528));
#220348=CARTESIAN_POINT('Ctrl Pts',(-18.5562821957296,-56.0941505847849,
2.85976644340788));
#220349=CARTESIAN_POINT('Ctrl Pts',(-18.5607667347597,-56.101732733504,
2.87354148166375));
#220350=CARTESIAN_POINT('Ctrl Pts',(-18.5643731068262,-56.1096829110186,
2.88743438345181));
#220351=CARTESIAN_POINT('Ctrl Pts',(-18.567058682946,-56.1179479440988,
2.90134173515983));
#220352=CARTESIAN_POINT('',(-18.6771643191705,-56.4568070719811,3.47153072139032));
#220353=CARTESIAN_POINT('',(-18.567058682946,-56.1179479440988,2.90134173515984));
#220354=CARTESIAN_POINT('',(-23.8971395307763,-54.4530463244693,3.47153072139034));
#220355=CARTESIAN_POINT('Origin',(5.53234440788222E-15,1.85015204418142E-13,
3.47153072139072));
#220356=CARTESIAN_POINT('',(-23.7522229508823,-54.1275498658874,2.90134173515985));
#220357=CARTESIAN_POINT('',(-23.8971395307763,-54.4530463244693,3.47153072139034));
#220358=CARTESIAN_POINT('',(-23.951372267036,-53.8330634946838,2.59908173515985));
#220359=CARTESIAN_POINT('Ctrl Pts',(-23.7522229508823,-54.1275498658874,
2.90134173515985));
#220360=CARTESIAN_POINT('Ctrl Pts',(-23.7472487091031,-54.1163771839526,
2.88176998919785));
#220361=CARTESIAN_POINT('Ctrl Pts',(-23.7440527738936,-54.1044728027369,
2.86226752356721));
#220362=CARTESIAN_POINT('Ctrl Pts',(-23.7426340760171,-54.0920187959693,
2.84310370500034));
#220363=CARTESIAN_POINT('Ctrl Pts',(-23.7411897512761,-54.0793398243594,
2.82359371788689));
#220364=CARTESIAN_POINT('Ctrl Pts',(-23.7415870431738,-54.0660903588301,
2.80443322637046));
#220365=CARTESIAN_POINT('Ctrl Pts',(-23.7438697192129,-54.052433905354,
2.78589323878321));
#220366=CARTESIAN_POINT('Ctrl Pts',(-23.746055752667,-54.0393556307103,
2.76813818620075));
#220367=CARTESIAN_POINT('Ctrl Pts',(-23.749970941678,-54.0259032350503,
2.75095095198804));
#220368=CARTESIAN_POINT('Ctrl Pts',(-23.755696492098,-54.0122070876526,
2.73457771435218));
#220369=CARTESIAN_POINT('Ctrl Pts',(-23.7602504066224,-54.0013136223984,
2.72155497955627));
#220370=CARTESIAN_POINT('Ctrl Pts',(-23.7659503210002,-53.9902655788131,
2.70904711159964));
#220371=CARTESIAN_POINT('Ctrl Pts',(-23.7728578042866,-53.9791273029163,
2.697189561583));
#220372=CARTESIAN_POINT('Ctrl Pts',(-23.7728766594722,-53.9790968990412,
2.69715719432317));
#220373=CARTESIAN_POINT('Ctrl Pts',(-23.7728955237001,-53.9790664946659,
2.69712483218983));
#220374=CARTESIAN_POINT('Ctrl Pts',(-23.7729143969706,-53.9790360897924,
2.69709247518611));
#220375=CARTESIAN_POINT('Ctrl Pts',(-23.776671466275,-53.9729834442087,
2.69065122242236));
#220376=CARTESIAN_POINT('Ctrl Pts',(-23.780822437404,-53.9669027062279,
2.68442464469386));
#220377=CARTESIAN_POINT('Ctrl Pts',(-23.7853431031259,-53.9608263568286,
2.67844505923539));
#220378=CARTESIAN_POINT('Ctrl Pts',(-23.7943146773159,-53.9487674206468,
2.66657815779527));
#220379=CARTESIAN_POINT('Ctrl Pts',(-23.8047436656396,-53.9367254523684,
2.65568445664134));
#220380=CARTESIAN_POINT('Ctrl Pts',(-23.8164490335992,-53.9249524603718,
2.64601906229476));
#220381=CARTESIAN_POINT('Ctrl Pts',(-23.8252280595689,-53.9161227163744,
2.63877001653482));
#220382=CARTESIAN_POINT('Ctrl Pts',(-23.8347250487603,-53.9074442707904,
2.63221189387562));
#220383=CARTESIAN_POINT('Ctrl Pts',(-23.8448636317802,-53.8990234500733,
2.62645231033194));
#220384=CARTESIAN_POINT('Ctrl Pts',(-23.8486656004127,-53.8958656423044,
2.62429246650306));
#220385=CARTESIAN_POINT('Ctrl Pts',(-23.8525577932538,-53.8927440632082,
2.62224491711707));
#220386=CARTESIAN_POINT('Ctrl Pts',(-23.8565361833376,-53.8896643205891,
2.62031533672558));
#220387=CARTESIAN_POINT('Ctrl Pts',(-23.8704605486307,-53.8788852214226,
2.6135618053554));
#220388=CARTESIAN_POINT('Ctrl Pts',(-23.8854408280735,-53.8686186144653,
2.60825339735309));
#220389=CARTESIAN_POINT('Ctrl Pts',(-23.9013043843656,-53.8591049768558,
2.60463337987572));
#220390=CARTESIAN_POINT('Ctrl Pts',(-23.9092361625117,-53.8543481580511,
2.60282337113704));
#220391=CARTESIAN_POINT('Ctrl Pts',(-23.9173887602867,-53.8497795825131,
2.60143545939075));
#220392=CARTESIAN_POINT('Ctrl Pts',(-23.9257405998156,-53.8454293138302,
2.60050005034556));
#220393=CARTESIAN_POINT('Ctrl Pts',(-23.92991651958,-53.8432541794887,2.60003234582297));
#220394=CARTESIAN_POINT('Ctrl Pts',(-23.9341422497936,-53.8411336218842,
2.59967776696026));
#220395=CARTESIAN_POINT('Ctrl Pts',(-23.9384150933423,-53.8390713992304,
2.5994401142912));
#220396=CARTESIAN_POINT('Ctrl Pts',(-23.942687936891,-53.8370091765766,
2.59920246162214));
#220397=CARTESIAN_POINT('Ctrl Pts',(-23.9470078944655,-53.8350052904263,
2.59908173791272));
#220398=CARTESIAN_POINT('Ctrl Pts',(-23.951372267036,-53.8330634946838,
2.59908173515985));
#220399=CARTESIAN_POINT('',(-23.9791663275009,-53.8206887816836,2.59908173515985));
#220400=CARTESIAN_POINT('Origin',(3.74779409800327E-16,1.91045239448285E-13,
2.59908173516024));
#220401=CARTESIAN_POINT('',(-24.3312692531083,-53.8697418420145,2.90134173515984));
#220402=CARTESIAN_POINT('Ctrl Pts',(-23.9791663275009,-53.8206887816836,
2.59908173515985));
#220403=CARTESIAN_POINT('Ctrl Pts',(-23.982646361822,-53.8191382997272,
2.59908174371477));
#220404=CARTESIAN_POINT('Ctrl Pts',(-23.9861360190791,-53.8176349962319,
2.59915764355852));
#220405=CARTESIAN_POINT('Ctrl Pts',(-23.9896330908637,-53.8161786595149,
2.59930765775239));
#220406=CARTESIAN_POINT('Ctrl Pts',(-24.0102795382214,-53.80758055767,2.60019333020848));
#220407=CARTESIAN_POINT('Ctrl Pts',(-24.031186190478,-53.8006169491704,
2.60365973324088));
#220408=CARTESIAN_POINT('Ctrl Pts',(-24.0518926318823,-53.7952474622067,
2.60934177082442));
#220409=CARTESIAN_POINT('Ctrl Pts',(-24.0596278691027,-53.7932416006198,
2.61146439091859));
#220410=CARTESIAN_POINT('Ctrl Pts',(-24.0673353939223,-53.7914578533664,
2.61389584429308));
#220411=CARTESIAN_POINT('Ctrl Pts',(-24.0749921329673,-53.7898929820048,
2.61661604385214));
#220412=CARTESIAN_POINT('Ctrl Pts',(-24.0809663048717,-53.7886719908665,
2.61873848000737));
#220413=CARTESIAN_POINT('Ctrl Pts',(-24.0869092410384,-53.7875846446507,
2.62103707099748));
#220414=CARTESIAN_POINT('Ctrl Pts',(-24.0928096561859,-53.7866297945199,
2.62350262767613));
#220415=CARTESIAN_POINT('Ctrl Pts',(-24.1134611092023,-53.7832878190622,
2.63213207605139));
#220416=CARTESIAN_POINT('Ctrl Pts',(-24.1335916760297,-53.7815689125022,
2.64280685971875));
#220417=CARTESIAN_POINT('Ctrl Pts',(-24.152717537984,-53.7814239018615,
2.65513293646044));
#220418=CARTESIAN_POINT('Ctrl Pts',(-24.1622804689611,-53.7813513965411,
2.66129597483129));
#220419=CARTESIAN_POINT('Ctrl Pts',(-24.1715922244705,-53.7816723668478,
2.66787183533813));
#220420=CARTESIAN_POINT('Ctrl Pts',(-24.1805923292962,-53.7823806708181,
2.67481125953822));
#220421=CARTESIAN_POINT('Ctrl Pts',(-24.1895539814231,-53.7830859485793,
2.6817210352404));
#220422=CARTESIAN_POINT('Ctrl Pts',(-24.198206747436,-53.784175029593,2.68899101329747));
#220423=CARTESIAN_POINT('Ctrl Pts',(-24.2064906018693,-53.7856425347024,
2.69657334701233));
#220424=CARTESIAN_POINT('Ctrl Pts',(-24.2065261462707,-53.7856488314802,
2.6966058813253));
#220425=CARTESIAN_POINT('Ctrl Pts',(-24.2065616841178,-53.7856551347354,
2.69663842081339));
#220426=CARTESIAN_POINT('Ctrl Pts',(-24.2065972154094,-53.7856614444664,
2.6966709654734));
#220427=CARTESIAN_POINT('Ctrl Pts',(-24.2233530895763,-53.7886369923275,
2.71201840158033));
#220428=CARTESIAN_POINT('Ctrl Pts',(-24.2386338146209,-53.7930196670714,
2.72845645939597));
#220429=CARTESIAN_POINT('Ctrl Pts',(-24.252420958295,-53.7986158348092,
2.74568723187311));
#220430=CARTESIAN_POINT('Ctrl Pts',(-24.266709651128,-53.8044155801181,
2.76354482594914));
#220431=CARTESIAN_POINT('Ctrl Pts',(-24.2793947083735,-53.8115193533113,
2.78225519317911));
#220432=CARTESIAN_POINT('Ctrl Pts',(-24.2904167803,-53.8197464933919,2.80151223086488));
#220433=CARTESIAN_POINT('Ctrl Pts',(-24.3012815425289,-53.8278562137235,
2.82049442741405));
#220434=CARTESIAN_POINT('Ctrl Pts',(-24.3105307527925,-53.8370583385507,
2.84000929090562));
#220435=CARTESIAN_POINT('Ctrl Pts',(-24.3180642992262,-53.8472012967848,
2.85976644343084));
#220436=CARTESIAN_POINT('Ctrl Pts',(-24.3233168218323,-53.8542731477233,
2.87354148167919));
#220437=CARTESIAN_POINT('Ctrl Pts',(-24.3277344576507,-53.8618028047995,
2.88743438345954));
#220438=CARTESIAN_POINT('Ctrl Pts',(-24.3312692531083,-53.8697418420145,
2.90134173515984));
#220439=CARTESIAN_POINT('',(-24.4761921430387,-54.1952354911872,3.47153072139034));
#220440=CARTESIAN_POINT('',(-24.3312692531083,-53.8697418420145,2.90134173515984));
#220441=CARTESIAN_POINT('',(-29.4581217525669,-51.6568155675428,3.47153072139036));
#220442=CARTESIAN_POINT('Origin',(5.53234440788222E-15,1.85015204418142E-13,
3.47153072139072));
#220443=CARTESIAN_POINT('',(-29.2799753962458,-51.3482501200166,2.90134173515987));
#220444=CARTESIAN_POINT('',(-29.4581217525669,-51.6568155675428,3.47153072139035));
#220445=CARTESIAN_POINT('',(-29.4472515437731,-51.0345602039888,2.59908173515987));
#220446=CARTESIAN_POINT('Ctrl Pts',(-29.2799753962458,-51.3482501200166,
2.90134173515987));
#220447=CARTESIAN_POINT('Ctrl Pts',(-29.2738605406103,-51.3376585930513,
2.88176998919738));
#220448=CARTESIAN_POINT('Ctrl Pts',(-29.2694377663935,-51.3261534914773,
2.86226752356625));
#220449=CARTESIAN_POINT('Ctrl Pts',(-29.2667250421036,-51.3139160033703,
2.84310370499892));
#220450=CARTESIAN_POINT('Ctrl Pts',(-29.2639633161065,-51.3014574615389,
2.82359371788513));
#220451=CARTESIAN_POINT('Ctrl Pts',(-29.2629734853268,-51.2882390496563,
2.80443322636838));
#220452=CARTESIAN_POINT('Ctrl Pts',(-29.2638161685324,-51.2744188030425,
2.78589323878084));
#220453=CARTESIAN_POINT('Ctrl Pts',(-29.2646231747158,-51.2611836698379,
2.76813818619833));
#220454=CARTESIAN_POINT('Ctrl Pts',(-29.2671107576663,-51.247395719118,
2.75095095198559));
#220455=CARTESIAN_POINT('Ctrl Pts',(-29.2713733056821,-51.233176117662,
2.73457771434972));
#220456=CARTESIAN_POINT('Ctrl Pts',(-29.2747635962034,-51.2218663142638,
2.7215549795547));
#220457=CARTESIAN_POINT('Ctrl Pts',(-29.2792774508355,-51.2102829897273,
2.70904711159891));
#220458=CARTESIAN_POINT('Ctrl Pts',(-29.2849828273425,-51.1984837018591,
2.69718956158302));
#220459=CARTESIAN_POINT('Ctrl Pts',(-29.2849984011671,-51.1984514936361,
2.69715719432319));
#220460=CARTESIAN_POINT('Ctrl Pts',(-29.2850139839321,-51.1984192839703,
2.69712483218985));
#220461=CARTESIAN_POINT('Ctrl Pts',(-29.2850295756381,-51.1983870728639,
2.69709247518613));
#220462=CARTESIAN_POINT('Ctrl Pts',(-29.2881333895822,-51.1919748636253,
2.69065122242239));
#220463=CARTESIAN_POINT('Ctrl Pts',(-29.2916260110603,-51.1854935419302,
2.68442464469389));
#220464=CARTESIAN_POINT('Ctrl Pts',(-29.2954867606375,-51.1789779411678,
2.67844505923542));
#220465=CARTESIAN_POINT('Ctrl Pts',(-29.3031486855376,-51.166047280237,
2.6665781577953));
#220466=CARTESIAN_POINT('Ctrl Pts',(-29.3122618143332,-51.1529811529979,
2.65568445664136));
#220467=CARTESIAN_POINT('Ctrl Pts',(-29.3226724463009,-51.1400491105585,
2.64601906229477));
#220468=CARTESIAN_POINT('Ctrl Pts',(-29.3304804202767,-51.130350078729,
2.63877001653483));
#220469=CARTESIAN_POINT('Ctrl Pts',(-29.3390182393872,-51.1207264688921,
2.63221189387563));
#220470=CARTESIAN_POINT('Ctrl Pts',(-29.3482210667394,-51.1112920078092,
2.62645231033195));
#220471=CARTESIAN_POINT('Ctrl Pts',(-29.3516721269965,-51.1077540849031,
2.62429246650307));
#220472=CARTESIAN_POINT('Ctrl Pts',(-29.3552167041322,-51.1042427612073,
2.62224491711707));
#220473=CARTESIAN_POINT('Ctrl Pts',(-29.3588513794155,-51.1007640347389,
2.62031533672559));
#220474=CARTESIAN_POINT('Ctrl Pts',(-29.3715727429074,-51.0885884920993,
2.6135618053554));
#220475=CARTESIAN_POINT('Ctrl Pts',(-29.3853978061638,-51.0768122610997,
2.6082533973531));
#220476=CARTESIAN_POINT('Ctrl Pts',(-29.4001800143153,-51.0656925470313,
2.60463337987573));
#220477=CARTESIAN_POINT('Ctrl Pts',(-29.4075711183911,-51.0601326899971,
2.60282337113705));
#220478=CARTESIAN_POINT('Ctrl Pts',(-29.4152015092021,-51.0547369630768,
2.60143545939077));
#220479=CARTESIAN_POINT('Ctrl Pts',(-29.42305286958,-51.0495375206695,2.60050005034558));
#220480=CARTESIAN_POINT('Ctrl Pts',(-29.4269785497689,-51.0469377994659,
2.60003234582299));
#220481=CARTESIAN_POINT('Ctrl Pts',(-29.4309594723626,-51.0443871494124,
2.59967776696029));
#220482=CARTESIAN_POINT('Ctrl Pts',(-29.4349933478623,-51.0418895900601,
2.59944011429123));
#220483=CARTESIAN_POINT('Ctrl Pts',(-29.439027223362,-51.0393920307079,
2.59920246162217));
#220484=CARTESIAN_POINT('Ctrl Pts',(-29.4431140526171,-51.036947563529,
2.59908173791276));
#220485=CARTESIAN_POINT('Ctrl Pts',(-29.4472515437731,-51.0345602039888,
2.59908173515987));
#220486=CARTESIAN_POINT('',(-29.4735998357333,-51.0193480105328,2.59908173515987));
#220487=CARTESIAN_POINT('Origin',(3.68424986610945E-16,1.91048477188617E-13,
2.59908173516023));
#220488=CARTESIAN_POINT('',(-29.8289013456881,-51.031327575341,2.90134173515987));
#220489=CARTESIAN_POINT('Ctrl Pts',(-29.4735998357333,-51.0193480105328,
2.59908173515987));
#220490=CARTESIAN_POINT('Ctrl Pts',(-29.4768987365661,-51.0174422596391,
2.59908174371478));
#220491=CARTESIAN_POINT('Ctrl Pts',(-29.4802121391114,-51.0155824228872,
2.59915764355853));
#220492=CARTESIAN_POINT('Ctrl Pts',(-29.4835378249318,-51.0137685205955,
2.5993076577524));
#220493=CARTESIAN_POINT('Ctrl Pts',(-29.5031724225193,-51.0030593786371,
2.60019333020856));
#220494=CARTESIAN_POINT('Ctrl Pts',(-29.5232366506538,-50.9939485772804,
2.60365973324146));
#220495=CARTESIAN_POINT('Ctrl Pts',(-29.5432683957864,-50.986444092428,
2.60934177082582));
#220496=CARTESIAN_POINT('Ctrl Pts',(-29.550751588937,-50.9836406667018,
2.61146439091966));
#220497=CARTESIAN_POINT('Ctrl Pts',(-29.5582304387683,-50.9810610352781,
2.61389584429368));
#220498=CARTESIAN_POINT('Ctrl Pts',(-29.5656816597954,-50.9787043892801,
2.61661604385215));
#220499=CARTESIAN_POINT('Ctrl Pts',(-29.5714954762337,-50.9768656158505,
2.61873848000738));
#220500=CARTESIAN_POINT('Ctrl Pts',(-29.5772921977452,-50.9751630202462,
2.62103707099751));
#220501=CARTESIAN_POINT('Ctrl Pts',(-29.5830604807844,-50.9735966395564,
2.62350262767616));
#220502=CARTESIAN_POINT('Ctrl Pts',(-29.6032494714215,-50.9681143071419,
2.63213207605142));
#220503=CARTESIAN_POINT('Ctrl Pts',(-29.6230900862363,-50.9643005997167,
2.64280685971877));
#220504=CARTESIAN_POINT('Ctrl Pts',(-29.6420960169782,-50.9621571865007,
2.65513293646047));
#220505=CARTESIAN_POINT('Ctrl Pts',(-29.6515989823491,-50.9610854798926,
2.66129597483132));
#220506=CARTESIAN_POINT('Ctrl Pts',(-29.6608932776205,-50.9604313483967,
2.66787183533815));
#220507=CARTESIAN_POINT('Ctrl Pts',(-29.6699181168558,-50.9601950050771,
2.67481125953824));
#220508=CARTESIAN_POINT('Ctrl Pts',(-29.6789043977152,-50.9599596715277,
2.68172103524042));
#220509=CARTESIAN_POINT('Ctrl Pts',(-29.6876236029352,-50.9601383261074,
2.68899101329751));
#220510=CARTESIAN_POINT('Ctrl Pts',(-29.6960154736012,-50.9607318934964,
2.69657334701236));
#220511=CARTESIAN_POINT('Ctrl Pts',(-29.6960514814791,-50.9607344403781,
2.69660588132534));
#220512=CARTESIAN_POINT('Ctrl Pts',(-29.6960874835157,-50.9607369943869,
2.69663842081342));
#220513=CARTESIAN_POINT('Ctrl Pts',(-29.6961234797097,-50.9607395555212,
2.69667096547343));
#220514=CARTESIAN_POINT('Ctrl Pts',(-29.7130985928885,-50.9619473372423,
2.71201840157905));
#220515=CARTESIAN_POINT('Ctrl Pts',(-29.7287537227772,-50.9647087325284,
2.7284564593932));
#220516=CARTESIAN_POINT('Ctrl Pts',(-29.7430502978486,-50.9688330949321,
2.74568723186873));
#220517=CARTESIAN_POINT('Ctrl Pts',(-29.7578669541906,-50.9731074935248,
2.76354482594296));
#220518=CARTESIAN_POINT('Ctrl Pts',(-29.7712250678598,-50.978846401964,
2.78225519317099));
#220519=CARTESIAN_POINT('Ctrl Pts',(-29.7830467300322,-50.9858763526687,
2.80151223085477));
#220520=CARTESIAN_POINT('Ctrl Pts',(-29.79469967056,-50.9928059702031,2.8204944274019));
#220521=CARTESIAN_POINT('Ctrl Pts',(-29.8048600966487,-51.000990879091,
2.84000929089138));
#220522=CARTESIAN_POINT('Ctrl Pts',(-29.813412601364,-51.0102908031055,
2.85976644341455));
#220523=CARTESIAN_POINT('Ctrl Pts',(-29.8193755598157,-51.0167748755905,
2.87354148166824));
#220524=CARTESIAN_POINT('Ctrl Pts',(-29.8245560588483,-51.0238015157366,
2.88743438345408));
#220525=CARTESIAN_POINT('Ctrl Pts',(-29.8289013456881,-51.031327575341,
2.90134173515987));
#220526=CARTESIAN_POINT('',(-30.0070536838153,-51.3398895692698,3.47153072139036));
#220527=CARTESIAN_POINT('',(-29.8289013456881,-51.031327575341,2.90134173515987));
#220528=CARTESIAN_POINT('',(-34.6963546279281,-48.2946219293748,3.47153072139038));
#220529=CARTESIAN_POINT('Origin',(5.53234440788222E-15,1.85015204418142E-13,
3.47153072139072));
#220530=CARTESIAN_POINT('',(-34.4869303039392,-48.0063682005188,2.90134173515989));
#220531=CARTESIAN_POINT('',(-34.6963546279281,-48.2946219293748,3.47153072139038));
#220532=CARTESIAN_POINT('',(-34.620500570363,-47.6769115920305,2.5990817351599));
#220533=CARTESIAN_POINT('Ctrl Pts',(-34.4869303039392,-48.0063682005188,
2.90134173515989));
#220534=CARTESIAN_POINT('Ctrl Pts',(-34.479741830085,-47.9964738715085,
2.88176998919639));
#220535=CARTESIAN_POINT('Ctrl Pts',(-34.4741406737007,-47.9854941018764,
2.86226752356426));
#220536=CARTESIAN_POINT('Ctrl Pts',(-34.4701636441721,-47.9736072089104,
2.84310370499598));
#220537=CARTESIAN_POINT('Ctrl Pts',(-34.4661147749668,-47.9615055952483,
2.8235937178812));
#220538=CARTESIAN_POINT('Ctrl Pts',(-34.4637486663029,-47.9484630606985,
2.80443322636351));
#220539=CARTESIAN_POINT('Ctrl Pts',(-34.4631421240615,-47.9346304384603,
2.78589323877512));
#220540=CARTESIAN_POINT('Ctrl Pts',(-34.4625612612459,-47.9213834535833,
2.76813818619183));
#220541=CARTESIAN_POINT('Ctrl Pts',(-34.4635939836568,-47.9074110114761,
2.75095095197838));
#220542=CARTESIAN_POINT('Ctrl Pts',(-34.4663468279008,-47.89282374889,2.73457771434193));
#220543=CARTESIAN_POINT('Ctrl Pts',(-34.4685363496869,-47.8812215199222,
2.72155497954972));
#220544=CARTESIAN_POINT('Ctrl Pts',(-34.4718146898373,-47.8692298237637,
2.70904711159655));
#220545=CARTESIAN_POINT('Ctrl Pts',(-34.4762554502653,-47.8568987993929,
2.69718956158302));
#220546=CARTESIAN_POINT('Ctrl Pts',(-34.4762675720988,-47.8568651397018,
2.6971571943232));
#220547=CARTESIAN_POINT('Ctrl Pts',(-34.476279702673,-47.8568314776415,
2.69712483218986));
#220548=CARTESIAN_POINT('Ctrl Pts',(-34.4762918419885,-47.8567978132139,
2.69709247518615));
#220549=CARTESIAN_POINT('Ctrl Pts',(-34.4787083945372,-47.8500962938265,
2.6906512224224));
#220550=CARTESIAN_POINT('Ctrl Pts',(-34.4815044004727,-47.843285399134,
2.68442464469391));
#220551=CARTESIAN_POINT('Ctrl Pts',(-34.4846629347248,-47.8364019332939,
2.67844505923543));
#220552=CARTESIAN_POINT('Ctrl Pts',(-34.4909312646825,-47.8227412186412,
2.66657815779531));
#220553=CARTESIAN_POINT('Ctrl Pts',(-34.4986286886039,-47.8087940876657,
2.65568445664138));
#220554=CARTESIAN_POINT('Ctrl Pts',(-34.5076305235173,-47.7948446809466,
2.64601906229479));
#220555=CARTESIAN_POINT('Ctrl Pts',(-34.5143818997023,-47.7843826259073,
2.63877001653485));
#220556=CARTESIAN_POINT('Ctrl Pts',(-34.5218670065991,-47.7739192901008,
2.63221189387566));
#220557=CARTESIAN_POINT('Ctrl Pts',(-34.5300332501815,-47.763574554582,
2.62645231033198));
#220558=CARTESIAN_POINT('Ctrl Pts',(-34.5330955915248,-47.7596952787624,
2.6242924665031));
#220559=CARTESIAN_POINT('Ctrl Pts',(-34.5362537178261,-47.7558326812644,
2.6222449171171));
#220560=CARTESIAN_POINT('Ctrl Pts',(-34.5395048560461,-47.7519930846016,
2.62031533672562));
#220561=CARTESIAN_POINT('Ctrl Pts',(-34.5508838398161,-47.7385544962821,
2.61356180535543));
#220562=CARTESIAN_POINT('Ctrl Pts',(-34.5634022165999,-47.7253976640913,
2.60825339735312));
#220563=CARTESIAN_POINT('Ctrl Pts',(-34.576941119645,-47.7127937034783,
2.60463337987576));
#220564=CARTESIAN_POINT('Ctrl Pts',(-34.5837105711675,-47.7064917231718,
2.60282337113707));
#220565=CARTESIAN_POINT('Ctrl Pts',(-34.5907351548561,-47.7003279615826,
2.6014354593908));
#220566=CARTESIAN_POINT('Ctrl Pts',(-34.5980000149356,-47.6943363116299,
2.60050005034561));
#220567=CARTESIAN_POINT('Ctrl Pts',(-34.6016324449754,-47.6913404866536,
2.60003234582302));
#220568=CARTESIAN_POINT('Ctrl Pts',(-34.6053249441282,-47.6883876896068,
2.59967776696031));
#220569=CARTESIAN_POINT('Ctrl Pts',(-34.6090756555948,-47.6854821573391,
2.59944011429125));
#220570=CARTESIAN_POINT('Ctrl Pts',(-34.6128263670615,-47.6825766250713,
2.59920246162219));
#220571=CARTESIAN_POINT('Ctrl Pts',(-34.6166352918405,-47.6797183589577,
2.59908173791276));
#220572=CARTESIAN_POINT('Ctrl Pts',(-34.620500570363,-47.6769115920305,
2.5990817351599));
#220573=CARTESIAN_POINT('',(-34.6451144164181,-47.6590285860937,2.59908173515989));
#220574=CARTESIAN_POINT('Origin',(3.62443809638016E-16,1.91052361410359E-13,
2.59908173516024));
#220575=CARTESIAN_POINT('',(-34.9997217530256,-47.6338034047601,2.9013417351599));
#220576=CARTESIAN_POINT('Ctrl Pts',(-34.6451144164181,-47.6590285860937,
2.59908173515989));
#220577=CARTESIAN_POINT('Ctrl Pts',(-34.6481960403147,-47.6567884460682,
2.59908174371476));
#220578=CARTESIAN_POINT('Ctrl Pts',(-34.6512968858166,-47.6545924528204,
2.59915764355856));
#220579=CARTESIAN_POINT('Ctrl Pts',(-34.654414748763,-47.6524408584472,
2.59930765775242));
#220580=CARTESIAN_POINT('Ctrl Pts',(-34.672822375818,-47.6397380079767,
2.60019333020855));
#220581=CARTESIAN_POINT('Ctrl Pts',(-34.6918243519456,-47.62857983361,2.60365973324119));
#220582=CARTESIAN_POINT('Ctrl Pts',(-34.7109619288123,-47.6190225715758,
2.60934177082513));
#220583=CARTESIAN_POINT('Ctrl Pts',(-34.7181110904657,-47.6154522966282,
2.61146439091915));
#220584=CARTESIAN_POINT('Ctrl Pts',(-34.7252793254674,-47.6121050440151,
2.61389584429341));
#220585=CARTESIAN_POINT('Ctrl Pts',(-34.7324433913422,-47.6089824432867,
2.61661604385218));
#220586=CARTESIAN_POINT('Ctrl Pts',(-34.7380331549248,-47.6065460335523,
2.61873848000741));
#220587=CARTESIAN_POINT('Ctrl Pts',(-34.7436201516873,-47.6042468425533,
2.62103707099753));
#220588=CARTESIAN_POINT('Ctrl Pts',(-34.7491931041021,-47.602086092899,
2.62350262767618));
#220589=CARTESIAN_POINT('Ctrl Pts',(-34.7686984375536,-47.5945234691089,
2.63213207605145));
#220590=CARTESIAN_POINT('Ctrl Pts',(-34.788031722428,-47.5886567445951,
2.64280685971879));
#220591=CARTESIAN_POINT('Ctrl Pts',(-34.8067094890031,-47.5845384124875,
2.65513293646049));
#220592=CARTESIAN_POINT('Ctrl Pts',(-34.8160483722906,-47.5824792464337,
2.66129597483134));
#220593=CARTESIAN_POINT('Ctrl Pts',(-34.8252233770799,-47.5808571799367,
2.66787183533817));
#220594=CARTESIAN_POINT('Ctrl Pts',(-34.8341740726976,-47.579678778754,
2.67481125953826));
#220595=CARTESIAN_POINT('Ctrl Pts',(-34.8430865267159,-47.5785054122577,
2.68172103524045));
#220596=CARTESIAN_POINT('Ctrl Pts',(-34.8517766417061,-47.5777716830264,
2.68899101329754));
#220597=CARTESIAN_POINT('Ctrl Pts',(-34.8601845855135,-47.5774848094464,
2.6965733470124));
#220598=CARTESIAN_POINT('Ctrl Pts',(-34.8602206623581,-47.577483578528,
2.69660588132537));
#220599=CARTESIAN_POINT('Ctrl Pts',(-34.8602567341385,-47.577482355308,
2.69663842081345));
#220600=CARTESIAN_POINT('Ctrl Pts',(-34.8602928008529,-47.5774811397854,
2.69667096547346));
#220601=CARTESIAN_POINT('Ctrl Pts',(-34.8773011701517,-47.5769079226575,
2.71201840157799));
#220602=CARTESIAN_POINT('Ctrl Pts',(-34.8931591840055,-47.5780177840616,
2.72845645939089));
#220603=CARTESIAN_POINT('Ctrl Pts',(-34.9078085542059,-47.580625153754,
2.74568723186509));
#220604=CARTESIAN_POINT('Ctrl Pts',(-34.9229908396696,-47.5833273744254,
2.76354482593811));
#220605=CARTESIAN_POINT('Ctrl Pts',(-34.9368756554737,-47.5876385414291,
2.78225519316485));
#220606=CARTESIAN_POINT('Ctrl Pts',(-34.9493673872874,-47.5933942811475,
2.80151223084732));
#220607=CARTESIAN_POINT('Ctrl Pts',(-34.9616808340595,-47.5990678735455,
2.82049442739359));
#220608=CARTESIAN_POINT('Ctrl Pts',(-34.972641156219,-47.6061458909203,
2.84000929088222));
#220609=CARTESIAN_POINT('Ctrl Pts',(-34.9821189161847,-47.6145008888021,
2.85976644340457));
#220610=CARTESIAN_POINT('Ctrl Pts',(-34.9887269790606,-47.6203261419772,
2.87354148166155));
#220611=CARTESIAN_POINT('Ctrl Pts',(-34.9946135826755,-47.6267727798519,
2.88743438345074));
#220612=CARTESIAN_POINT('Ctrl Pts',(-34.9997217530256,-47.6338034047601,
2.90134173515989));
#220613=CARTESIAN_POINT('',(-35.2091516650524,-47.9220530736688,3.47153072139038));
#220614=CARTESIAN_POINT('',(-34.9997217530256,-47.6338034047601,2.9013417351599));
#220615=CARTESIAN_POINT('',(-39.5544469813067,-44.4033023070491,3.47153072139041));
#220616=CARTESIAN_POINT('Origin',(5.53234440788222E-15,1.85015204418142E-13,
3.47153072139072));
#220617=CARTESIAN_POINT('',(-39.3160391863686,-44.1385184650377,2.90134173515991));
#220618=CARTESIAN_POINT('',(-39.5544469813067,-44.4033023070491,3.47153072139041));
#220619=CARTESIAN_POINT('',(-39.4144401478986,-43.7969047596348,2.59908173515993));
#220620=CARTESIAN_POINT('Ctrl Pts',(-39.3160391863686,-44.1385184650377,
2.90134173515992));
#220621=CARTESIAN_POINT('Ctrl Pts',(-39.3078558527196,-44.1294297383224,
2.88176998919639));
#220622=CARTESIAN_POINT('Ctrl Pts',(-39.3011376816092,-44.1190955972866,
2.86226752356423));
#220623=CARTESIAN_POINT('Ctrl Pts',(-39.2959399200097,-44.107689534749,
2.84310370499592));
#220624=CARTESIAN_POINT('Ctrl Pts',(-39.2906482678543,-44.0960774370687,
2.82359371788089));
#220625=CARTESIAN_POINT('Ctrl Pts',(-39.2869318048876,-44.0833536765902,
2.80443322636297));
#220626=CARTESIAN_POINT('Ctrl Pts',(-39.2848826826026,-44.0696602318321,
2.78589323877437));
#220627=CARTESIAN_POINT('Ctrl Pts',(-39.2829203148422,-44.0565465320211,
2.76813818619038));
#220628=CARTESIAN_POINT('Ctrl Pts',(-39.2824868619903,-44.0425426835265,
2.75095095197631));
#220629=CARTESIAN_POINT('Ctrl Pts',(-39.2836998417244,-44.027747580912,
2.73457771433931));
#220630=CARTESIAN_POINT('Ctrl Pts',(-39.2846646059167,-44.0159800428215,
2.72155497954806));
#220631=CARTESIAN_POINT('Ctrl Pts',(-39.2866715134052,-44.0037113585721,
2.70904711159579));
#220632=CARTESIAN_POINT('Ctrl Pts',(-39.2897990038549,-43.9909836989805,
2.69718956158308));
#220633=CARTESIAN_POINT('Ctrl Pts',(-39.2898075408879,-43.9909489566042,
2.69715719432325));
#220634=CARTESIAN_POINT('Ctrl Pts',(-39.2898160863661,-43.9909142109579,
2.6971248321899));
#220635=CARTESIAN_POINT('Ctrl Pts',(-39.2898246402903,-43.9908794620435,
2.69709247518618));
#220636=CARTESIAN_POINT('Ctrl Pts',(-39.2915274551881,-43.9839620557563,
2.69065122242244));
#220637=CARTESIAN_POINT('Ctrl Pts',(-39.2935962119549,-43.9768962096537,
2.68442464469393));
#220638=CARTESIAN_POINT('Ctrl Pts',(-39.2960179253196,-43.9697202954282,
2.67844505923546));
#220639=CARTESIAN_POINT('Ctrl Pts',(-39.3008239832001,-43.9554791967019,
2.66657815779534));
#220640=CARTESIAN_POINT('Ctrl Pts',(-39.30702136766,-43.9408038696756,2.65568445664141));
#220641=CARTESIAN_POINT('Ctrl Pts',(-39.314515779532,-43.925989931296,2.64601906229483));
#220642=CARTESIAN_POINT('Ctrl Pts',(-39.320136588436,-43.9148794775113,
2.63877001653489));
#220643=CARTESIAN_POINT('Ctrl Pts',(-39.3264869747216,-43.9036910542319,
2.63221189387569));
#220644=CARTESIAN_POINT('Ctrl Pts',(-39.3335271634604,-43.8925493833643,
2.62645231033201));
#220645=CARTESIAN_POINT('Ctrl Pts',(-39.3361672342375,-43.888371256789,
2.62429246650313));
#220646=CARTESIAN_POINT('Ctrl Pts',(-39.3389043086117,-43.884199704915,
2.62224491711713));
#220647=CARTESIAN_POINT('Ctrl Pts',(-39.3417362896177,-43.8800413054826,
2.62031533672564));
#220648=CARTESIAN_POINT('Ctrl Pts',(-39.3516482231385,-43.8654869074689,
2.61356180535546));
#220649=CARTESIAN_POINT('Ctrl Pts',(-39.3627227594941,-43.8510936230937,
2.60825339735315));
#220650=CARTESIAN_POINT('Ctrl Pts',(-39.3748700223777,-43.837143507566,
2.60463337987578));
#220651=CARTESIAN_POINT('Ctrl Pts',(-39.3809436538195,-43.8301684498022,
2.6028233711371));
#220652=CARTESIAN_POINT('Ctrl Pts',(-39.3872854675768,-43.8233041850058,
2.60143545939083));
#220653=CARTESIAN_POINT('Ctrl Pts',(-39.3938842320307,-43.8165859732786,
2.60050005034564));
#220654=CARTESIAN_POINT('Ctrl Pts',(-39.3971836142576,-43.8132268674149,
2.60003234582305));
#220655=CARTESIAN_POINT('Ctrl Pts',(-39.400547234176,-43.8099042748373,
2.59967776696034));
#220656=CARTESIAN_POINT('Ctrl Pts',(-39.4039736880299,-43.8066226032736,
2.59944011429128));
#220657=CARTESIAN_POINT('Ctrl Pts',(-39.4074001418838,-43.8033409317098,
2.59920246162222));
#220658=CARTESIAN_POINT('Ctrl Pts',(-39.4108894308099,-43.8001001824231,
2.59908173791277));
#220659=CARTESIAN_POINT('Ctrl Pts',(-39.4144401478986,-43.7969047596348,
2.59908173515992));
#220660=CARTESIAN_POINT('',(-39.4370498736004,-43.7765468711724,2.59908173515992));
#220661=CARTESIAN_POINT('Origin',(3.56901409908096E-16,1.91056849557166E-13,
2.59908173516024));
#220662=CARTESIAN_POINT('',(-39.7870778846743,-43.7143933160625,2.90134173515992));
#220663=CARTESIAN_POINT('Ctrl Pts',(-39.4370498736004,-43.7765468711724,
2.59908173515992));
#220664=CARTESIAN_POINT('Ctrl Pts',(-39.4398804576444,-43.7739968854581,
2.59908174371479));
#220665=CARTESIAN_POINT('Ctrl Pts',(-39.4427347725907,-43.7714887954759,
2.59915764355859));
#220666=CARTESIAN_POINT('Ctrl Pts',(-39.4456106527043,-43.7690230823394,
2.59930765775246));
#220667=CARTESIAN_POINT('Ctrl Pts',(-39.462589631414,-43.7544656984439,
2.60019333020861));
#220668=CARTESIAN_POINT('Ctrl Pts',(-39.4803211659094,-43.7413824023598,
2.60365973324145));
#220669=CARTESIAN_POINT('Ctrl Pts',(-39.4983548992148,-43.7298770745062,
2.60934177082573));
#220670=CARTESIAN_POINT('Ctrl Pts',(-39.5050917016582,-43.7255790670175,
2.61146439091961));
#220671=CARTESIAN_POINT('Ctrl Pts',(-39.5118707851462,-43.7215008664158,
2.61389584429367));
#220672=CARTESIAN_POINT('Ctrl Pts',(-39.5186692048624,-43.7176465228245,
2.6166160438522));
#220673=CARTESIAN_POINT('Ctrl Pts',(-39.5239736729698,-43.7146391706003,
2.61873848000744));
#220674=CARTESIAN_POINT('Ctrl Pts',(-39.5292897326776,-43.7117685746243,
2.62103707099755));
#220675=CARTESIAN_POINT('Ctrl Pts',(-39.534606296035,-43.7090371296309,
2.62350262767619));
#220676=CARTESIAN_POINT('Ctrl Pts',(-39.553214267786,-43.6994770721539,
2.63213207605146));
#220677=CARTESIAN_POINT('Ctrl Pts',(-39.5718284032052,-43.6916216076131,
2.64280685971882));
#220678=CARTESIAN_POINT('Ctrl Pts',(-39.5899733680942,-43.6855734779223,
2.65513293646052));
#220679=CARTESIAN_POINT('Ctrl Pts',(-39.5990458505387,-43.682549413077,
2.66129597483137));
#220680=CARTESIAN_POINT('Ctrl Pts',(-39.6080010415735,-43.6799771832788,
2.6678718353382));
#220681=CARTESIAN_POINT('Ctrl Pts',(-39.6167795278794,-43.677869635043,
2.67481125953829));
#220682=CARTESIAN_POINT('Ctrl Pts',(-39.6255205083453,-43.6757710912487,
2.68172103524048));
#220683=CARTESIAN_POINT('Ctrl Pts',(-39.6340863223874,-43.6741330170973,
2.68899101329756));
#220684=CARTESIAN_POINT('Ctrl Pts',(-39.6424182201444,-43.6729688455954,
2.69657334701241));
#220685=CARTESIAN_POINT('Ctrl Pts',(-39.6424539706902,-43.6729638503629,
2.69660588132539));
#220686=CARTESIAN_POINT('Ctrl Pts',(-39.6424897170043,-43.6729588633161,
2.69663842081348));
#220687=CARTESIAN_POINT('Ctrl Pts',(-39.6425254590848,-43.672953884454,
2.69667096547348));
#220688=CARTESIAN_POINT('Ctrl Pts',(-39.6593807372517,-43.670605948764,
2.71201840157821));
#220689=CARTESIAN_POINT('Ctrl Pts',(-39.6752678913536,-43.6700521164126,
2.72845645939134));
#220690=CARTESIAN_POINT('Ctrl Pts',(-39.6901095551185,-43.6711139265061,
2.74568723186578));
#220691=CARTESIAN_POINT('Ctrl Pts',(-39.7054911294082,-43.6722143631616,
2.76354482593897));
#220692=CARTESIAN_POINT('Ctrl Pts',(-39.7197505224005,-43.6750505546826,
2.78225519316589));
#220693=CARTESIAN_POINT('Ctrl Pts',(-39.7327754618281,-43.6794690223266,
2.80151223084853));
#220694=CARTESIAN_POINT('Ctrl Pts',(-39.7456145061449,-43.6838244285232,
2.82049442739476));
#220695=CARTESIAN_POINT('Ctrl Pts',(-39.7572546407919,-43.689718006146,
2.84000929088333));
#220696=CARTESIAN_POINT('Ctrl Pts',(-39.7675538156858,-43.697036538791,
2.85976644340562));
#220697=CARTESIAN_POINT('Ctrl Pts',(-39.7747345836642,-43.7021391499619,
2.87354148166226));
#220698=CARTESIAN_POINT('Ctrl Pts',(-39.7812627969987,-43.7079351548501,
2.88743438345111));
#220699=CARTESIAN_POINT('Ctrl Pts',(-39.7870778846743,-43.7143933160625,
2.90134173515992));
#220700=CARTESIAN_POINT('',(-40.0254908126584,-43.9791725362584,3.47153072139041));
#220701=CARTESIAN_POINT('',(-39.7870778846743,-43.7143933160625,2.90134173515992));
#220702=CARTESIAN_POINT('',(-43.9791725362579,-40.025490812659,3.47153072139043));
#220703=CARTESIAN_POINT('Origin',(5.53234440788222E-15,1.85015204418142E-13,
3.47153072139072));
#220704=CARTESIAN_POINT('',(-43.714393316062,-39.7870778846749,2.90134173515995));
#220705=CARTESIAN_POINT('',(-43.9791725362579,-40.025490812659,3.47153072139043));
#220706=CARTESIAN_POINT('',(-43.7765468711719,-39.437049873601,2.59908173515996));
#220707=CARTESIAN_POINT('Ctrl Pts',(-43.714393316062,-39.7870778846749,
2.90134173515995));
#220708=CARTESIAN_POINT('Ctrl Pts',(-43.7053047809348,-39.7788943382464,
2.88176998919728));
#220709=CARTESIAN_POINT('Ctrl Pts',(-43.6975432007875,-39.769319048819,
2.86226752356597));
#220710=CARTESIAN_POINT('Ctrl Pts',(-43.691181654881,-39.7585187839184,
2.84310370499846));
#220711=CARTESIAN_POINT('Ctrl Pts',(-43.6847051962242,-39.7475234267928,
2.82359371788444));
#220712=CARTESIAN_POINT('Ctrl Pts',(-43.6796790973008,-39.735257844569,
2.80443322636747));
#220713=CARTESIAN_POINT('Ctrl Pts',(-43.6762098455845,-39.7218536055386,
2.78589323877973));
#220714=CARTESIAN_POINT('Ctrl Pts',(-43.672887472991,-39.7090168672348,
2.76813818619693));
#220715=CARTESIAN_POINT('Ctrl Pts',(-43.6709925938758,-39.6951350414494,
2.75095095198392));
#220716=CARTESIAN_POINT('Ctrl Pts',(-43.6706524194392,-39.6802941970489,
2.73457771434783));
#220717=CARTESIAN_POINT('Ctrl Pts',(-43.6703818558787,-39.6684902774427,
2.72155497955352));
#220718=CARTESIAN_POINT('Ctrl Pts',(-43.6710953426071,-39.656079023371,
2.70904711159839));
#220719=CARTESIAN_POINT('Ctrl Pts',(-43.6728752976391,-39.643094175457,
2.6971895615831));
#220720=CARTESIAN_POINT('Ctrl Pts',(-43.6728801563381,-39.6430587310401,
2.69715719432327));
#220721=CARTESIAN_POINT('Ctrl Pts',(-43.6728850230943,-39.6430232824884,
2.69712483218993));
#220722=CARTESIAN_POINT('Ctrl Pts',(-43.6728898979086,-39.6429878298036,
2.69709247518621));
#220723=CARTESIAN_POINT('Ctrl Pts',(-43.6738603187593,-39.6359303251673,
2.69065122242247));
#220724=CARTESIAN_POINT('Ctrl Pts',(-43.6751791606252,-39.6286869425433,
2.68442464469396));
#220725=CARTESIAN_POINT('Ctrl Pts',(-43.6768375203041,-39.6212972007503,
2.67844505923549));
#220726=CARTESIAN_POINT('Ctrl Pts',(-43.6801286499316,-39.6066317464083,
2.66657815779537));
#220727=CARTESIAN_POINT('Ctrl Pts',(-43.684758095089,-39.591389009285,2.65568445664145));
#220728=CARTESIAN_POINT('Ctrl Pts',(-43.6906629735749,-39.5758728438538,
2.64601906229486));
#220729=CARTESIAN_POINT('Ctrl Pts',(-43.6950916324393,-39.5642357197804,
2.63877001653492));
#220730=CARTESIAN_POINT('Ctrl Pts',(-43.7002377219525,-39.5524447917348,
2.63221189387572));
#220731=CARTESIAN_POINT('Ctrl Pts',(-43.7060747220668,-39.540628255996,
2.62645231033204));
#220732=CARTESIAN_POINT('Ctrl Pts',(-43.7082635971097,-39.5361970550939,
2.62429246650316));
#220733=CARTESIAN_POINT('Ctrl Pts',(-43.7105496315973,-39.5317622532394,
2.62224491711717));
#220734=CARTESIAN_POINT('Ctrl Pts',(-43.7129314276126,-39.5273306113316,
2.62031533672568));
#220735=CARTESIAN_POINT('Ctrl Pts',(-43.7212677136663,-39.5118198646542,
2.6135618053555));
#220736=CARTESIAN_POINT('Ctrl Pts',(-43.7307770746559,-39.4963478239301,
2.60825339735318));
#220737=CARTESIAN_POINT('Ctrl Pts',(-43.741399609424,-39.4812043938728,
2.60463337987581));
#220738=CARTESIAN_POINT('Ctrl Pts',(-43.746710876808,-39.4736326788442,
2.60282337113713));
#220739=CARTESIAN_POINT('Ctrl Pts',(-43.7523004383953,-39.4661431171622,
2.60143545939086));
#220740=CARTESIAN_POINT('Ctrl Pts',(-43.7581608097794,-39.4587719497939,
2.60050005034567));
#220741=CARTESIAN_POINT('Ctrl Pts',(-43.7610909954714,-39.4550863661097,
2.60003234582308));
#220742=CARTESIAN_POINT('Ctrl Pts',(-43.7640888836317,-39.4514303810208,
2.59967776696037));
#220743=CARTESIAN_POINT('Ctrl Pts',(-43.7671535389273,-39.4478085248414,
2.59944011429131));
#220744=CARTESIAN_POINT('Ctrl Pts',(-43.770218194223,-39.444186668662,2.59920246162225));
#220745=CARTESIAN_POINT('Ctrl Pts',(-43.7733496179165,-39.4405989425297,
2.59908173791279));
#220746=CARTESIAN_POINT('Ctrl Pts',(-43.7765468711719,-39.437049873601,
2.59908173515996));
#220747=CARTESIAN_POINT('',(-43.7969047596343,-39.4144401478991,2.59908173515995));
#220748=CARTESIAN_POINT('Origin',(3.51858511112452E-16,1.91061892455961E-13,
2.59908173516024));
#220749=CARTESIAN_POINT('',(-44.1385184650372,-39.3160391863692,2.90134173515995));
#220750=CARTESIAN_POINT('Ctrl Pts',(-43.7969047596343,-39.4144401478991,
2.59908173515995));
#220751=CARTESIAN_POINT('Ctrl Pts',(-43.7994532913547,-39.4116082546731,
2.59908174371483));
#220752=CARTESIAN_POINT('Ctrl Pts',(-43.8020298032735,-39.4088155471153,
2.59915764355862));
#220753=CARTESIAN_POINT('Ctrl Pts',(-43.8046321918099,-39.4060627300844,
2.59930765775248));
#220754=CARTESIAN_POINT('Ctrl Pts',(-43.8199964969259,-39.3898103065129,
2.60019333020841));
#220755=CARTESIAN_POINT('Ctrl Pts',(-43.8362633193816,-39.3749452320449,
2.60365973323973));
#220756=CARTESIAN_POINT('Ctrl Pts',(-43.8529956277646,-39.3616178931544,
2.60934177082144));
#220757=CARTESIAN_POINT('Ctrl Pts',(-43.8592462611857,-39.35663924299,2.61146439091634));
#220758=CARTESIAN_POINT('Ctrl Pts',(-43.8655619201074,-39.3518747760151,
2.61389584429187));
#220759=CARTESIAN_POINT('Ctrl Pts',(-43.8719202087609,-39.3473309185526,
2.61661604385226));
#220760=CARTESIAN_POINT('Ctrl Pts',(-43.8768812645306,-39.3437855730188,
2.61873848000749));
#220761=CARTESIAN_POINT('Ctrl Pts',(-43.881868143321,-39.340375022916,2.6210370709976));
#220762=CARTESIAN_POINT('Ctrl Pts',(-43.8868700682404,-39.3371028088665,
2.62350262767625));
#220763=CARTESIAN_POINT('Ctrl Pts',(-43.9043768054583,-39.325650059693,
2.63213207605151));
#220764=CARTESIAN_POINT('Ctrl Pts',(-43.9220678510593,-39.3158919212385,
2.64280685971886));
#220765=CARTESIAN_POINT('Ctrl Pts',(-43.9394812142299,-39.3079802585391,
2.65513293646056));
#220766=CARTESIAN_POINT('Ctrl Pts',(-43.9481878958152,-39.3040244271894,
2.6612959748314));
#220767=CARTESIAN_POINT('Ctrl Pts',(-43.9568251581486,-39.3005302159781,
2.66787183533823));
#220768=CARTESIAN_POINT('Ctrl Pts',(-43.9653352562096,-39.2975166114286,
2.67481125953832));
#220769=CARTESIAN_POINT('Ctrl Pts',(-43.973808995112,-39.2945158824213,
2.6817210352405));
#220770=CARTESIAN_POINT('Ctrl Pts',(-43.9821566593547,-39.291991410433,
2.6889910132976));
#220771=CARTESIAN_POINT('Ctrl Pts',(-43.990321225046,-39.2899626959158,
2.69657334701245));
#220772=CARTESIAN_POINT('Ctrl Pts',(-43.9903562576026,-39.2899539910981,
2.69660588132543));
#220773=CARTESIAN_POINT('Ctrl Pts',(-43.9903912868063,-39.2899452948636,
2.69663842081351));
#220774=CARTESIAN_POINT('Ctrl Pts',(-43.9904263126551,-39.2899366072114,
2.69667096547352));
#220775=CARTESIAN_POINT('Ctrl Pts',(-44.0069438297366,-39.2858396774337,
2.71201840157964));
#220776=CARTESIAN_POINT('Ctrl Pts',(-44.0226860611028,-39.2836282192298,
2.72845645939433));
#220777=CARTESIAN_POINT('Ctrl Pts',(-44.0375574100593,-39.2831328363111,
2.74568723187047));
#220778=CARTESIAN_POINT('Ctrl Pts',(-44.0529697494292,-39.2826194323365,
2.76354482594518));
#220779=CARTESIAN_POINT('Ctrl Pts',(-44.0674474907168,-39.2839495744676,
2.78225519317373));
#220780=CARTESIAN_POINT('Ctrl Pts',(-44.080862933797,-39.2869823603817,
2.80151223085806));
#220781=CARTESIAN_POINT('Ctrl Pts',(-44.0940869084027,-39.2899718616359,
2.82049442740554));
#220782=CARTESIAN_POINT('Ctrl Pts',(-44.1062793237865,-39.2946164282379,
2.84000929089538));
#220783=CARTESIAN_POINT('Ctrl Pts',(-44.1172870736935,-39.3008183122717,
2.8597664434189));
#220784=CARTESIAN_POINT('Ctrl Pts',(-44.1249618727751,-39.3051423761621,
2.87354148167119));
#220785=CARTESIAN_POINT('Ctrl Pts',(-44.1320601713554,-39.3102242458199,
2.8874343834556));
#220786=CARTESIAN_POINT('Ctrl Pts',(-44.1385184650372,-39.3160391863692,
2.90134173515995));
#220787=CARTESIAN_POINT('',(-44.4033023070486,-39.5544469813073,3.47153072139044));
#220788=CARTESIAN_POINT('',(-44.1385184650372,-39.3160391863692,2.90134173515995));
#220789=CARTESIAN_POINT('',(-47.9220530736684,-35.209151665053,3.47153072139047));
#220790=CARTESIAN_POINT('Origin',(5.53234440788222E-15,1.85015204418142E-13,
3.47153072139072));
#220791=CARTESIAN_POINT('',(-47.6338034047597,-34.9997217530262,2.90134173515998));
#220792=CARTESIAN_POINT('',(-47.9220530736684,-35.209151665053,3.47153072139047));
#220793=CARTESIAN_POINT('',(-47.6590285860933,-34.6451144164188,2.59908173515998));
#220794=CARTESIAN_POINT('Ctrl Pts',(-47.6338034047597,-34.9997217530262,
2.90134173515998));
#220795=CARTESIAN_POINT('Ctrl Pts',(-47.6239092440466,-34.9925330475314,
2.8817699891971));
#220796=CARTESIAN_POINT('Ctrl Pts',(-47.6151892923582,-34.9838215185865,
2.86226752356558));
#220797=CARTESIAN_POINT('Ctrl Pts',(-47.6077336605729,-34.9737453812845,
2.84310370499787));
#220798=CARTESIAN_POINT('Ctrl Pts',(-47.6001433528508,-34.9634872321464,
2.82359371788377));
#220799=CARTESIAN_POINT('Ctrl Pts',(-47.5938626849622,-34.9518142124621,
2.80443322636672));
#220800=CARTESIAN_POINT('Ctrl Pts',(-47.5890113136627,-34.938846038806,
2.78589323877891));
#220801=CARTESIAN_POINT('Ctrl Pts',(-47.5843653368456,-34.9264269039996,
2.76813818619628));
#220802=CARTESIAN_POINT('Ctrl Pts',(-47.5810297921599,-34.9128191931104,
2.75095095198344));
#220803=CARTESIAN_POINT('Ctrl Pts',(-47.5791401905757,-34.8980952063196,
2.73457771434749));
#220804=CARTESIAN_POINT('Ctrl Pts',(-47.5776372636137,-34.8863842314133,
2.72155497955331));
#220805=CARTESIAN_POINT('Ctrl Pts',(-47.5770495124718,-34.8739663878189,
2.70904711159831));
#220806=CARTESIAN_POINT('Ctrl Pts',(-47.5774624305257,-34.8608666162964,
2.69718956158313));
#220807=CARTESIAN_POINT('Ctrl Pts',(-47.5774635576578,-34.8608308581753,
2.6971571943233));
#220808=CARTESIAN_POINT('Ctrl Pts',(-47.5774646923707,-34.8607950951,2.69712483218996));
#220809=CARTESIAN_POINT('Ctrl Pts',(-47.5774658346656,-34.8607593270719,
2.69709247518623));
#220810=CARTESIAN_POINT('Ctrl Pts',(-47.5776932293352,-34.8536390475841,
2.69065122242249));
#220811=CARTESIAN_POINT('Ctrl Pts',(-47.5782477067929,-34.8462974884545,
2.684424644694));
#220812=CARTESIAN_POINT('Ctrl Pts',(-47.5791245434504,-34.8387748826514,
2.67844505923552));
#220813=CARTESIAN_POINT('Ctrl Pts',(-47.58086468652,-34.8238457504804,2.66657815779541));
#220814=CARTESIAN_POINT('Ctrl Pts',(-47.5838754712049,-34.8082026058779,
2.65568445664148));
#220815=CARTESIAN_POINT('Ctrl Pts',(-47.5881261212203,-34.7921542117505,
2.64601906229489));
#220816=CARTESIAN_POINT('Ctrl Pts',(-47.5913141087318,-34.780117916155,
2.63877001653495));
#220817=CARTESIAN_POINT('Ctrl Pts',(-47.5951995198391,-34.7678536672182,
2.63221189387577));
#220818=CARTESIAN_POINT('Ctrl Pts',(-47.5997693799341,-34.7554917310465,
2.62645231033209));
#220819=CARTESIAN_POINT('Ctrl Pts',(-47.6014830774698,-34.7508560049821,
2.62429246650321));
#220820=CARTESIAN_POINT('Ctrl Pts',(-47.6032930257985,-34.7462065417643,
2.62224491711719));
#220821=CARTESIAN_POINT('Ctrl Pts',(-47.6051985413677,-34.7415502113772,
2.62031533672571));
#220822=CARTESIAN_POINT('Ctrl Pts',(-47.6118678458598,-34.7252530550225,
2.61356180535552));
#220823=CARTESIAN_POINT('Ctrl Pts',(-47.6197078449344,-34.7088717728654,
2.60825339735324));
#220824=CARTESIAN_POINT('Ctrl Pts',(-47.6286892688731,-34.6927009428671,
2.60463337987587));
#220825=CARTESIAN_POINT('Ctrl Pts',(-47.6331799808424,-34.684615527868,
2.60282337113719));
#220826=CARTESIAN_POINT('Ctrl Pts',(-47.6379560498533,-34.6765827265055,
2.6014354593909));
#220827=CARTESIAN_POINT('Ctrl Pts',(-47.6430138207122,-34.6686393635484,
2.60050005034571));
#220828=CARTESIAN_POINT('Ctrl Pts',(-47.6455427061417,-34.6646676820698,
2.60003234582312));
#220829=CARTESIAN_POINT('Ctrl Pts',(-47.6481420170539,-34.6607183602072,
2.5996777669604));
#220830=CARTESIAN_POINT('Ctrl Pts',(-47.6508112967866,-34.6567960012265,
2.59944011429134));
#220831=CARTESIAN_POINT('Ctrl Pts',(-47.6534805765192,-34.6528736422457,
2.59920246162228));
#220832=CARTESIAN_POINT('Ctrl Pts',(-47.6562198264469,-34.648978247146,
2.59908173791283));
#220833=CARTESIAN_POINT('Ctrl Pts',(-47.6590285860933,-34.6451144164188,
2.59908173515999));
#220834=CARTESIAN_POINT('',(-47.6769115920301,-34.6205005703637,2.59908173515998));
#220835=CARTESIAN_POINT('Origin',(3.4737036430558E-16,1.91067434855691E-13,
2.59908173516024));
#220836=CARTESIAN_POINT('',(-48.0063682005184,-34.4869303039399,2.90134173515999));
#220837=CARTESIAN_POINT('Ctrl Pts',(-47.6769115920301,-34.6205005703637,
2.59908173515998));
#220838=CARTESIAN_POINT('Ctrl Pts',(-47.67915014918,-34.6174177964407,2.59908174371487));
#220839=CARTESIAN_POINT('Ctrl Pts',(-47.6814206292676,-34.6143710687956,
2.59915764355865));
#220840=CARTESIAN_POINT('Ctrl Pts',(-47.6837210139133,-34.61136130831,2.59930765775252));
#220841=CARTESIAN_POINT('Ctrl Pts',(-47.6973023109009,-34.5935919100086,
2.60019333020864));
#220842=CARTESIAN_POINT('Ctrl Pts',(-47.7119261986139,-34.5771079220171,
2.60365973324122));
#220843=CARTESIAN_POINT('Ctrl Pts',(-47.7271737594107,-34.5621045891988,
2.60934177082506));
#220844=CARTESIAN_POINT('Ctrl Pts',(-47.7328697405539,-34.5564998434983,
2.61146439091911));
#220845=CARTESIAN_POINT('Ctrl Pts',(-47.7386527792209,-34.5511013106536,
2.61389584429342));
#220846=CARTESIAN_POINT('Ctrl Pts',(-47.7445012740627,-34.5459177227787,
2.61661604385227));
#220847=CARTESIAN_POINT('Ctrl Pts',(-47.7490645631293,-34.5418732274829,
2.6187384800075));
#220848=CARTESIAN_POINT('Ctrl Pts',(-47.7536676237148,-34.537960089954,
2.62103707099762));
#220849=CARTESIAN_POINT('Ctrl Pts',(-47.7583001080601,-34.5341829579102,
2.62350262767627));
#220850=CARTESIAN_POINT('Ctrl Pts',(-47.7745138032685,-34.5209629957568,
2.63213207605153));
#220851=CARTESIAN_POINT('Ctrl Pts',(-47.7910879322537,-34.5094090955954,
2.64280685971889));
#220852=CARTESIAN_POINT('Ctrl Pts',(-47.8075789092549,-34.4997205817196,
2.65513293646059));
#220853=CARTESIAN_POINT('Ctrl Pts',(-47.8158243977556,-34.4948763247816,
2.66129597483143));
#220854=CARTESIAN_POINT('Ctrl Pts',(-47.8240490997339,-34.4904984154664,
2.66787183533825));
#220855=CARTESIAN_POINT('Ctrl Pts',(-47.8321975711348,-34.4866117722854,
2.67481125953835));
#220856=CARTESIAN_POINT('Ctrl Pts',(-47.8403112284171,-34.4827417346799,
2.68172103524053));
#220857=CARTESIAN_POINT('Ctrl Pts',(-47.8483492841042,-34.4793585234982,
2.68899101329763));
#220858=CARTESIAN_POINT('Ctrl Pts',(-47.8562570650394,-34.4764874929864,
2.69657334701249));
#220859=CARTESIAN_POINT('Ctrl Pts',(-47.8562909957829,-34.4764751739553,
2.69660588132546));
#220860=CARTESIAN_POINT('Ctrl Pts',(-47.8563249240889,-34.4764628638109,
2.69663842081354));
#220861=CARTESIAN_POINT('Ctrl Pts',(-47.8563588499555,-34.4764505625524,
2.69667096547355));
#220862=CARTESIAN_POINT('Ctrl Pts',(-47.872357636575,-34.4706495255077,
2.71201840157839));
#220863=CARTESIAN_POINT('Ctrl Pts',(-47.8877824700218,-34.4668046706503,
2.72845645939164));
#220864=CARTESIAN_POINT('Ctrl Pts',(-47.9025205705563,-34.4647575222378,
2.74568723186622));
#220865=CARTESIAN_POINT('Ctrl Pts',(-47.917794814189,-34.4626359025941,
2.76354482593952));
#220866=CARTESIAN_POINT('Ctrl Pts',(-47.932332282607,-34.4624454220187,
2.78225519316656));
#220867=CARTESIAN_POINT('Ctrl Pts',(-47.9459912469366,-34.4640592983644,
2.80151223084933));
#220868=CARTESIAN_POINT('Ctrl Pts',(-47.9594552671974,-34.4656501410735,
2.82049442739569));
#220869=CARTESIAN_POINT('Ctrl Pts',(-47.9720663806631,-34.4689948098093,
2.8400092908844));
#220870=CARTESIAN_POINT('Ctrl Pts',(-47.9836621023717,-34.4740120960907,
2.85976644340683));
#220871=CARTESIAN_POINT('Ctrl Pts',(-47.9917468458571,-34.4775102373532,
2.87354148166309));
#220872=CARTESIAN_POINT('Ctrl Pts',(-47.9993374592434,-34.4818222937559,
2.88743438345156));
#220873=CARTESIAN_POINT('Ctrl Pts',(-48.0063682005184,-34.4869303039399,
2.90134173515999));
#220874=CARTESIAN_POINT('',(-48.2946219293743,-34.6963546279287,3.47153072139047));
#220875=CARTESIAN_POINT('',(-48.0063682005184,-34.4869303039399,2.90134173515999));
#220876=CARTESIAN_POINT('',(-51.3398895692695,-30.007053683816,3.4715307213905));
#220877=CARTESIAN_POINT('Origin',(5.53234440788222E-15,1.85015204418142E-13,
3.47153072139072));
#220878=CARTESIAN_POINT('',(-51.0313275753406,-29.8289013456888,2.90134173516002));
#220879=CARTESIAN_POINT('',(-51.3398895692695,-30.007053683816,3.4715307213905));
#220880=CARTESIAN_POINT('',(-51.0193480105325,-29.473599835734,2.59908173516003));
#220881=CARTESIAN_POINT('Ctrl Pts',(-51.0313275753406,-29.8289013456888,
2.90134173516002));
#220882=CARTESIAN_POINT('Ctrl Pts',(-51.0207361915371,-29.8227862420897,
2.8817699891976));
#220883=CARTESIAN_POINT('Ctrl Pts',(-51.0111534059233,-29.8150339189619,
2.86226752356654));
#220884=CARTESIAN_POINT('Ctrl Pts',(-51.0026853737213,-29.8057923055278,
2.84310370499927));
#220885=CARTESIAN_POINT('Ctrl Pts',(-50.9940643779338,-29.7963837548062,
2.82359371788554));
#220886=CARTESIAN_POINT('Ctrl Pts',(-50.9865979533919,-29.7854311897081,
2.80443322636885));
#220887=CARTESIAN_POINT('Ctrl Pts',(-50.9804176151483,-29.7730411634513,
2.78589323878137));
#220888=CARTESIAN_POINT('Ctrl Pts',(-50.9744989364019,-29.761175698782,
2.76813818619886));
#220889=CARTESIAN_POINT('Ctrl Pts',(-50.9697592710711,-29.7479911917172,
2.75095095198612));
#220890=CARTESIAN_POINT('Ctrl Pts',(-50.9663409452096,-29.7335453816167,
2.73457771435025));
#220891=CARTESIAN_POINT('Ctrl Pts',(-50.9636221212281,-29.7220556593013,
2.7215549795551));
#220892=CARTESIAN_POINT('Ctrl Pts',(-50.9617395717402,-29.7097672786763,
2.70904711159918));
#220893=CARTESIAN_POINT('Ctrl Pts',(-50.9607809287993,-29.6966961073822,
2.69718956158317));
#220894=CARTESIAN_POINT('Ctrl Pts',(-50.9607783120155,-29.6966604273305,
2.69715719432334));
#220895=CARTESIAN_POINT('Ctrl Pts',(-50.960775702253,-29.6966247415593,
2.69712483219));
#220896=CARTESIAN_POINT('Ctrl Pts',(-50.9607730995133,-29.6965890500698,
2.69709247518628));
#220897=CARTESIAN_POINT('Ctrl Pts',(-50.9602549766182,-29.6894840070028,
2.69065122242254));
#220898=CARTESIAN_POINT('Ctrl Pts',(-50.9600390146965,-29.6821247070256,
2.68442464469403));
#220899=CARTESIAN_POINT('Ctrl Pts',(-50.9601247215267,-29.6745516564559,
2.67844505923556));
#220900=CARTESIAN_POINT('Ctrl Pts',(-50.9602948126667,-29.6595224131521,
2.66657815779545));
#220901=CARTESIAN_POINT('Ctrl Pts',(-50.9616539500922,-29.6436502506361,
2.65568445664151));
#220902=CARTESIAN_POINT('Ctrl Pts',(-50.964203800626,-29.6272454573769,
2.64601906229493));
#220903=CARTESIAN_POINT('Ctrl Pts',(-50.9661161885263,-29.6149418624325,
2.63877001653499));
#220904=CARTESIAN_POINT('Ctrl Pts',(-50.9686983518505,-29.6023386622825,
2.63221189387579));
#220905=CARTESIAN_POINT('Ctrl Pts',(-50.9719510035827,-29.5895667656375,
2.62645231033211));
#220906=CARTESIAN_POINT('Ctrl Pts',(-50.9731707479823,-29.5847773043956,
2.62429246650323));
#220907=CARTESIAN_POINT('Ctrl Pts',(-50.9744847799795,-29.5799641203064,
2.62224491711723));
#220908=CARTESIAN_POINT('Ctrl Pts',(-50.9758931378752,-29.5751341171702,
2.62031533672575));
#220909=CARTESIAN_POINT('Ctrl Pts',(-50.9808223905102,-29.5582291061935,
2.61356180535556));
#220910=CARTESIAN_POINT('Ctrl Pts',(-50.9869071309993,-29.5411180593588,
2.60825339735326));
#220911=CARTESIAN_POINT('Ctrl Pts',(-50.9941490417484,-29.524097000417,
2.60463337987589));
#220912=CARTESIAN_POINT('Ctrl Pts',(-50.9977699971229,-29.5155864709461,
2.60282337113721));
#220913=CARTESIAN_POINT('Ctrl Pts',(-51.0016802459459,-29.5070984389558,
2.60143545939093));
#220914=CARTESIAN_POINT('Ctrl Pts',(-51.0058800022838,-29.4986699095566,
2.60050005034575));
#220915=CARTESIAN_POINT('Ctrl Pts',(-51.0079798804527,-29.494455644857,
2.60003234582315));
#220916=CARTESIAN_POINT('Ctrl Pts',(-51.0101521355226,-29.4902562558177,
2.59967776696044));
#220917=CARTESIAN_POINT('Ctrl Pts',(-51.0123967945049,-29.4860763682213,
2.59944011429138));
#220918=CARTESIAN_POINT('Ctrl Pts',(-51.0146414534873,-29.4818964806249,
2.59920246162232));
#220919=CARTESIAN_POINT('Ctrl Pts',(-51.0169585178536,-29.4777360953218,
2.59908173791288));
#220920=CARTESIAN_POINT('Ctrl Pts',(-51.0193480105325,-29.473599835734,
2.59908173516002));
#220921=CARTESIAN_POINT('',(-51.0345602039884,-29.4472515437738,2.59908173516002));
#220922=CARTESIAN_POINT('Origin',(3.43486142563102E-16,1.91073416032664E-13,
2.59908173516024));
#220923=CARTESIAN_POINT('',(-51.3482501200163,-29.2799753962465,2.90134173516002));
#220924=CARTESIAN_POINT('Ctrl Pts',(-51.0345602039884,-29.4472515437738,
2.59908173516002));
#220925=CARTESIAN_POINT('Ctrl Pts',(-51.0364642604673,-29.4439516646701,
2.59908174371488));
#220926=CARTESIAN_POINT('Ctrl Pts',(-51.0384038328686,-29.4406842975234,
2.59915764355868));
#220927=CARTESIAN_POINT('Ctrl Pts',(-51.0403770101282,-29.4374505691487,
2.59930765775255));
#220928=CARTESIAN_POINT('Ctrl Pts',(-51.0520264994499,-29.418358881371,
2.60019333020849));
#220929=CARTESIAN_POINT('Ctrl Pts',(-51.0648472300398,-29.4004365818843,
2.60365973323985));
#220930=CARTESIAN_POINT('Ctrl Pts',(-51.0784429877767,-29.383921634797,
2.60934177082164));
#220931=CARTESIAN_POINT('Ctrl Pts',(-51.0835219102868,-29.3777522003207,
2.61146439091651));
#220932=CARTESIAN_POINT('Ctrl Pts',(-51.0887089685234,-29.3717787490555,
2.61389584429199));
#220933=CARTESIAN_POINT('Ctrl Pts',(-51.0939835922267,-29.366012223236,
2.61661604385232));
#220934=CARTESIAN_POINT('Ctrl Pts',(-51.0980991182404,-29.361512890515,
2.61873848000755));
#220935=CARTESIAN_POINT('Ctrl Pts',(-51.1022679285259,-29.3571400387136,
2.62103707099765));
#220936=CARTESIAN_POINT('Ctrl Pts',(-51.1064802178291,-29.3528993717246,
2.6235026276763));
#220937=CARTESIAN_POINT('Ctrl Pts',(-51.1212232303903,-29.3380570372631,
2.63213207605156));
#220938=CARTESIAN_POINT('Ctrl Pts',(-51.1364988531341,-29.3248339623429,
2.64280685971893));
#220939=CARTESIAN_POINT('Ctrl Pts',(-51.1518867653711,-29.3134747466761,
2.65513293646063));
#220940=CARTESIAN_POINT('Ctrl Pts',(-51.1595807214896,-29.3077951388426,
2.66129597483147));
#220941=CARTESIAN_POINT('Ctrl Pts',(-51.1673027515569,-29.3025814967141,
2.6678718353383));
#220942=CARTESIAN_POINT('Ctrl Pts',(-51.1750003199399,-29.2978643977776,
2.67481125953839));
#220943=CARTESIAN_POINT('Ctrl Pts',(-51.182665000675,-29.2931674525158,
2.68172103524058));
#220944=CARTESIAN_POINT('Ctrl Pts',(-51.1903053811862,-29.2889625693103,
2.68899101329765));
#220945=CARTESIAN_POINT('Ctrl Pts',(-51.1978697380627,-29.2852806784151,
2.69657334701251));
#220946=CARTESIAN_POINT('Ctrl Pts',(-51.1979021952406,-29.2852648801404,
2.69660588132548));
#220947=CARTESIAN_POINT('Ctrl Pts',(-51.1979346509233,-29.2852490909586,
2.69663842081357));
#220948=CARTESIAN_POINT('Ctrl Pts',(-51.1979671051089,-29.285233310869,
2.69667096547357));
#220949=CARTESIAN_POINT('Ctrl Pts',(-51.2132718752151,-29.2777917239319,
2.71201840157988));
#220950=CARTESIAN_POINT('Ctrl Pts',(-51.2282103130419,-29.2723555974551,
2.72845645939479));
#220951=CARTESIAN_POINT('Ctrl Pts',(-51.2426536914433,-29.2687791125354,
2.74568723187116));
#220952=CARTESIAN_POINT('Ctrl Pts',(-51.2576224915316,-29.2650725221316,
2.7635448259463));
#220953=CARTESIAN_POINT('Ctrl Pts',(-51.2720604115359,-29.2633635057956,
2.78225519317531));
#220954=CARTESIAN_POINT('Ctrl Pts',(-51.285813246645,-29.2635407906074,
2.80151223086009));
#220955=CARTESIAN_POINT('Ctrl Pts',(-51.2993697979386,-29.2637155451671,
2.82049442740827));
#220956=CARTESIAN_POINT('Ctrl Pts',(-51.3122614394892,-29.2657236711479,
2.84000929089882));
#220957=CARTESIAN_POINT('Ctrl Pts',(-51.3243180878463,-29.2695013892407,
2.85976644342305));
#220958=CARTESIAN_POINT('Ctrl Pts',(-51.3327241975877,-29.2721352815066,
2.87354148167401));
#220959=CARTESIAN_POINT('Ctrl Pts',(-51.3407239614257,-29.2756302808596,
2.88743438345704));
#220960=CARTESIAN_POINT('Ctrl Pts',(-51.3482501200163,-29.2799753962465,
2.90134173516001));
#220961=CARTESIAN_POINT('',(-51.6568155675425,-29.4581217525676,3.47153072139051));
#220962=CARTESIAN_POINT('',(-51.3482501200163,-29.2799753962465,2.90134173516002));
#220963=CARTESIAN_POINT('',(-54.195235491187,-24.4761921430394,3.47153072139054));
#220964=CARTESIAN_POINT('Origin',(5.53234440788222E-15,1.85015204418142E-13,
3.47153072139072));
#220965=CARTESIAN_POINT('',(-53.8697418420143,-24.331269253109,2.90134173516006));
#220966=CARTESIAN_POINT('',(-54.195235491187,-24.4761921430394,3.47153072139055));
#220967=CARTESIAN_POINT('',(-53.8206887816834,-23.9791663275016,2.59908173516006));
#220968=CARTESIAN_POINT('Ctrl Pts',(-53.8697418420143,-24.331269253109,
2.90134173516006));
#220969=CARTESIAN_POINT('Ctrl Pts',(-53.8585692765376,-24.32629474976,2.88176998919761));
#220970=CARTESIAN_POINT('Ctrl Pts',(-53.8482286480027,-24.3195865685234,
2.86226752356651));
#220971=CARTESIAN_POINT('Ctrl Pts',(-53.8388409929167,-24.3112807320076,
2.84310370499922));
#220972=CARTESIAN_POINT('Ctrl Pts',(-53.8292837624978,-24.3028248617528,
2.82359371788556));
#220973=CARTESIAN_POINT('Ctrl Pts',(-53.8207133850122,-24.2927127498358,
2.80443322636894));
#220974=CARTESIAN_POINT('Ctrl Pts',(-53.8132717929037,-24.2810366186984,
2.78589323878152));
#220975=CARTESIAN_POINT('Ctrl Pts',(-53.806145258511,-24.2698548246802,
2.76813818619927));
#220976=CARTESIAN_POINT('Ctrl Pts',(-53.8000534013004,-24.2572379736583,
2.75095095198677));
#220977=CARTESIAN_POINT('Ctrl Pts',(-53.7951438030552,-24.2432286115666,
2.73457771435111));
#220978=CARTESIAN_POINT('Ctrl Pts',(-53.7912388700589,-24.2320860256448,
2.72155497955566));
#220979=CARTESIAN_POINT('Ctrl Pts',(-53.7880821478312,-24.2200617420593,
2.70904711159946));
#220980=CARTESIAN_POINT('Ctrl Pts',(-53.7857624469881,-24.2071623814824,
2.69718956158321));
#220981=CARTESIAN_POINT('Ctrl Pts',(-53.7857561149583,-24.2071271704182,
2.69715719432338));
#220982=CARTESIAN_POINT('Ctrl Pts',(-53.7857497893135,-24.2070919529317,
2.69712483219004));
#220983=CARTESIAN_POINT('Ctrl Pts',(-53.7857434700554,-24.2070567290244,
2.69709247518632));
#220984=CARTESIAN_POINT('Ctrl Pts',(-53.7844855062584,-24.2000447667167,
2.69065122242259));
#220985=CARTESIAN_POINT('Ctrl Pts',(-53.7835014710814,-24.1927483559227,
2.68442464469408));
#220986=CARTESIAN_POINT('Ctrl Pts',(-53.7827951090624,-24.1852078325131,
2.67844505923561));
#220987=CARTESIAN_POINT('Ctrl Pts',(-53.7813932847187,-24.1702431416111,
2.66657815779549));
#220988=CARTESIAN_POINT('Ctrl Pts',(-53.7810858838905,-24.1543158599158,
2.65568445664155));
#220989=CARTESIAN_POINT('Ctrl Pts',(-53.7819069982467,-24.1377344018726,
2.64601906229496));
#220990=CARTESIAN_POINT('Ctrl Pts',(-53.7825228340138,-24.1252983083403,
2.63877001653502));
#220991=CARTESIAN_POINT('Ctrl Pts',(-53.7837734588332,-24.1124942402751,
2.63221189387583));
#220992=CARTESIAN_POINT('Ctrl Pts',(-53.7856732654696,-24.0994523147292,
2.62645231033215));
#220993=CARTESIAN_POINT('Ctrl Pts',(-53.7863856929583,-24.0945615926495,
2.62429246650327));
#220994=CARTESIAN_POINT('Ctrl Pts',(-53.7871894118144,-24.089637421941,
2.62224491711727));
#220995=CARTESIAN_POINT('Ctrl Pts',(-53.7880851817728,-24.0846866645808,
2.62031533672578));
#220996=CARTESIAN_POINT('Ctrl Pts',(-53.7912203766271,-24.06735901382,2.61356180535559));
#220997=CARTESIAN_POINT('Ctrl Pts',(-53.7954831928407,-24.0497056745176,
2.6082533973533));
#220998=CARTESIAN_POINT('Ctrl Pts',(-53.8009062465106,-24.0320208729158,
2.60463337987593));
#220999=CARTESIAN_POINT('Ctrl Pts',(-53.8036177733455,-24.023178472115,
2.60282337113724));
#221000=CARTESIAN_POINT('Ctrl Pts',(-53.8066193604762,-24.0143282061515,
2.60143545939096));
#221001=CARTESIAN_POINT('Ctrl Pts',(-53.8099150888837,-24.0055068550422,
2.60050005034577));
#221002=CARTESIAN_POINT('Ctrl Pts',(-53.8115629530875,-24.0010961794875,
2.60003234582318));
#221003=CARTESIAN_POINT('Ctrl Pts',(-53.8132843526338,-23.9966927326564,
2.59967776696048));
#221004=CARTESIAN_POINT('Ctrl Pts',(-53.8150797979123,-23.9923011121677,
2.59944011429142));
#221005=CARTESIAN_POINT('Ctrl Pts',(-53.8168752431908,-23.987909491679,
2.59920246162236));
#221006=CARTESIAN_POINT('Ctrl Pts',(-53.8187447357538,-23.9835296982243,
2.59908173791293));
#221007=CARTESIAN_POINT('Ctrl Pts',(-53.8206887816834,-23.9791663275016,
2.59908173516006));
#221008=CARTESIAN_POINT('',(-53.8330634946836,-23.9513722670367,2.59908173516006));
#221009=CARTESIAN_POINT('Origin',(3.40248402231257E-16,1.91079770455854E-13,
2.59908173516024));
#221010=CARTESIAN_POINT('',(-54.1275498658872,-23.752222950883,2.90134173516006));
#221011=CARTESIAN_POINT('Ctrl Pts',(-53.8330634946836,-23.9513722670367,
2.59908173516006));
#221012=CARTESIAN_POINT('Ctrl Pts',(-53.8346121892501,-23.9478914369183,
2.59908174371493));
#221013=CARTESIAN_POINT('Ctrl Pts',(-53.8361996036041,-23.9444392282282,
2.59915764355872));
#221014=CARTESIAN_POINT('Ctrl Pts',(-53.8378239549346,-23.9410169613692,
2.59930765775258));
#221015=CARTESIAN_POINT('Ctrl Pts',(-53.8474140023514,-23.9208121566358,
2.60019333020862));
#221016=CARTESIAN_POINT('Ctrl Pts',(-53.8582911092154,-23.9016479061124,
2.60365973324066));
#221017=CARTESIAN_POINT('Ctrl Pts',(-53.8700861059304,-23.8838022859684,
2.60934177082359));
#221018=CARTESIAN_POINT('Ctrl Pts',(-53.8744923240653,-23.8771357563367,
2.61146439091801));
#221019=CARTESIAN_POINT('Ctrl Pts',(-53.8790265713717,-23.8706528330382,
2.61389584429284));
#221020=CARTESIAN_POINT('Ctrl Pts',(-53.8836695340507,-23.8643665485424,
2.61661604385234));
#221021=CARTESIAN_POINT('Ctrl Pts',(-53.8872922064472,-23.8594616740271,
2.61873848000757));
#221022=CARTESIAN_POINT('Ctrl Pts',(-53.8909810920749,-23.8546770178325,
2.62103707099769));
#221023=CARTESIAN_POINT('Ctrl Pts',(-53.894727035613,-23.8500192775333,
2.62350262767634));
#221024=CARTESIAN_POINT('Ctrl Pts',(-53.9078378379963,-23.833717186486,
2.63213207605161));
#221025=CARTESIAN_POINT('Ctrl Pts',(-53.9216475915793,-23.8189698115829,
2.64280685971896));
#221026=CARTESIAN_POINT('Ctrl Pts',(-53.9357638458654,-23.806064348069,
2.65513293646066));
#221027=CARTESIAN_POINT('Ctrl Pts',(-53.9428219730085,-23.799611616312,
2.66129597483151));
#221028=CARTESIAN_POINT('Ctrl Pts',(-53.9499567269874,-23.7936193631243,
2.66787183533834));
#221029=CARTESIAN_POINT('Ctrl Pts',(-53.9571190561825,-23.7881234899554,
2.67481125953843));
#221030=CARTESIAN_POINT('Ctrl Pts',(-53.9642507845242,-23.7826510977525,
2.68172103524061));
#221031=CARTESIAN_POINT('Ctrl Pts',(-53.9714097802519,-23.7776706121036,
2.68899101329771));
#221032=CARTESIAN_POINT('Ctrl Pts',(-53.9785478363928,-23.773218200392,
2.69657334701256));
#221033=CARTESIAN_POINT('Ctrl Pts',(-53.9785784643974,-23.773199095963,
2.69660588132554));
#221034=CARTESIAN_POINT('Ctrl Pts',(-53.9786090918656,-23.7731800007333,
2.69663842081363));
#221035=CARTESIAN_POINT('Ctrl Pts',(-53.9786397187952,-23.7731609147026,
2.69667096547363));
#221036=CARTESIAN_POINT('Ctrl Pts',(-53.993082790121,-23.7641603094586,
2.71201840157815));
#221037=CARTESIAN_POINT('Ctrl Pts',(-54.007371163674,-23.7571924707023,
2.72845645939101));
#221038=CARTESIAN_POINT('Ctrl Pts',(-54.0213615752631,-23.7521258339928,
2.74568723186518));
#221039=CARTESIAN_POINT('Ctrl Pts',(-54.0358609304978,-23.746874883009,
2.76354482593813));
#221040=CARTESIAN_POINT('Ctrl Pts',(-54.0500411172129,-23.7436660552521,
2.78225519316479));
#221041=CARTESIAN_POINT('Ctrl Pts',(-54.0637371441599,-23.7424048061589,
2.80151223084718));
#221042=CARTESIAN_POINT('Ctrl Pts',(-54.0772376980716,-23.7411615579202,
2.82049442739336));
#221043=CARTESIAN_POINT('Ctrl Pts',(-54.0902686241828,-23.7418111396954,
2.84000929088188));
#221044=CARTESIAN_POINT('Ctrl Pts',(-54.1026541040249,-23.7443079001269,
2.85976644340412));
#221045=CARTESIAN_POINT('Ctrl Pts',(-54.1112894809329,-23.746048685922,
2.87354148166129));
#221046=CARTESIAN_POINT('Ctrl Pts',(-54.119610748143,-23.748688336283,2.8874343834507));
#221047=CARTESIAN_POINT('Ctrl Pts',(-54.1275498658872,-23.752222950883,
2.90134173516006));
#221048=CARTESIAN_POINT('',(-54.4530463244691,-23.8971395307771,3.47153072139055));
#221049=CARTESIAN_POINT('',(-54.1275498658872,-23.752222950883,2.90134173516006));
#221050=CARTESIAN_POINT('',(-56.456807071981,-18.6771643191712,3.47153072139058));
#221051=CARTESIAN_POINT('Origin',(5.53234440788222E-15,1.85015204418142E-13,
3.47153072139072));
#221052=CARTESIAN_POINT('',(-56.1179479440987,-18.5670586829468,2.9013417351601));
#221053=CARTESIAN_POINT('',(-56.456807071981,-18.6771643191712,3.47153072139059));
#221054=CARTESIAN_POINT('',(-56.032358823839,-18.2220120550219,2.5990817351601));
#221055=CARTESIAN_POINT('Ctrl Pts',(-56.1179479440987,-18.5670586829468,
2.9013417351601));
#221056=CARTESIAN_POINT('Ctrl Pts',(-56.106316605913,-18.5632792815474,
2.88176998919588));
#221057=CARTESIAN_POINT('Ctrl Pts',(-56.0953314285462,-18.5576887384388,
2.86226752356303));
#221058=CARTESIAN_POINT('Ctrl Pts',(-56.0851270036891,-18.5504096793234,
2.84310370499407));
#221059=CARTESIAN_POINT('Ctrl Pts',(-56.0747382496542,-18.5429991338184,
2.82359371787864));
#221060=CARTESIAN_POINT('Ctrl Pts',(-56.0651578180735,-18.5338382654954,
2.80443322636034));
#221061=CARTESIAN_POINT('Ctrl Pts',(-56.05653650374,-18.5230039556117,2.7858932387714));
#221062=CARTESIAN_POINT('Ctrl Pts',(-56.0482801935027,-18.512628342318,
2.76813818618766));
#221063=CARTESIAN_POINT('Ctrl Pts',(-56.0409028880744,-18.500717380197,
2.75095095197381));
#221064=CARTESIAN_POINT('Ctrl Pts',(-56.0345558080313,-18.4872979556143,
2.73457771433704));
#221065=CARTESIAN_POINT('Ctrl Pts',(-56.0295075492856,-18.4766245865924,
2.72155497954667));
#221066=CARTESIAN_POINT('Ctrl Pts',(-56.0251112400293,-18.4649961406178,
2.70904711159522));
#221067=CARTESIAN_POINT('Ctrl Pts',(-56.0214558964132,-18.4524099188568,
2.69718956158324));
#221068=CARTESIAN_POINT('Ctrl Pts',(-56.0214459185125,-18.4523755625598,
2.69715719432342));
#221069=CARTESIAN_POINT('Ctrl Pts',(-56.0214359462906,-18.4523411992083,
2.69712483219007));
#221070=CARTESIAN_POINT('Ctrl Pts',(-56.021425979749,-18.4523068288036,
2.69709247518635));
#221071=CARTESIAN_POINT('Ctrl Pts',(-56.0194419575649,-18.4454647717816,
2.69065122242261));
#221072=CARTESIAN_POINT('Ctrl Pts',(-56.0177006304279,-18.4383111911741,
2.68442464469413));
#221073=CARTESIAN_POINT('Ctrl Pts',(-56.0162099386096,-18.4308858104772,
2.67844505923565));
#221074=CARTESIAN_POINT('Ctrl Pts',(-56.0132515574631,-18.4161496282621,
2.66657815779553));
#221075=CARTESIAN_POINT('Ctrl Pts',(-56.0112809863292,-18.4003417300186,
2.65568445664159));
#221076=CARTESIAN_POINT('Ctrl Pts',(-56.010364368207,-18.3837652771157,
2.64601906229501));
#221077=CARTESIAN_POINT('Ctrl Pts',(-56.0096769046154,-18.3713329374386,
2.63877001653507));
#221078=CARTESIAN_POINT('Ctrl Pts',(-56.0095822888227,-18.3584682855075,
2.63221189387587));
#221079=CARTESIAN_POINT('Ctrl Pts',(-56.0101084356843,-18.3452992211262,
2.62645231033219));
#221080=CARTESIAN_POINT('Ctrl Pts',(-56.0103057407573,-18.3403608219831,
2.6242924665033));
#221081=CARTESIAN_POINT('Ctrl Pts',(-56.0105903407605,-18.3353796149,2.62224491711731));
#221082=CARTESIAN_POINT('Ctrl Pts',(-56.0109637085384,-18.3303623448494,
2.62031533672582));
#221083=CARTESIAN_POINT('Ctrl Pts',(-56.0122704957612,-18.3128018996725,
2.61356180535563));
#221084=CARTESIAN_POINT('Ctrl Pts',(-56.0146646833927,-18.2947996815818,
2.60825339735333));
#221085=CARTESIAN_POINT('Ctrl Pts',(-56.0182094638726,-18.2766448957073,
2.60463337987597));
#221086=CARTESIAN_POINT('Ctrl Pts',(-56.0199818541125,-18.26756750277,2.60282337113728));
#221087=CARTESIAN_POINT('Ctrl Pts',(-56.0220418935342,-18.2584519681994,
2.601435459391));
#221088=CARTESIAN_POINT('Ctrl Pts',(-56.0243974853212,-18.2493344439487,
2.60050005034582));
#221089=CARTESIAN_POINT('Ctrl Pts',(-56.0255752812147,-18.2447756818233,
2.60003234582322));
#221090=CARTESIAN_POINT('Ctrl Pts',(-56.0268269652239,-18.2402164222855,
2.59967776696052));
#221091=CARTESIAN_POINT('Ctrl Pts',(-56.0281535255244,-18.2356611844174,
2.59944011429146));
#221092=CARTESIAN_POINT('Ctrl Pts',(-56.0294800858248,-18.2311059465494,
2.5992024616224));
#221093=CARTESIAN_POINT('Ctrl Pts',(-56.0308815240327,-18.2265547308768,
2.59908173791298));
#221094=CARTESIAN_POINT('Ctrl Pts',(-56.032358823839,-18.2220120550219,
2.5990817351601));
#221095=CARTESIAN_POINT('',(-56.0417604764382,-18.1930767435951,2.5990817351601));
#221096=CARTESIAN_POINT('Origin',(3.37692616670652E-16,1.91086428504869E-13,
2.59908173516024));
#221097=CARTESIAN_POINT('',(-56.3138168485094,-17.9642361803975,2.9013417351601));
#221098=CARTESIAN_POINT('Ctrl Pts',(-56.0417604764382,-18.1930767435951,
2.59908173516011));
#221099=CARTESIAN_POINT('Ctrl Pts',(-56.0429368412707,-18.1894530991653,
2.59908174371499));
#221100=CARTESIAN_POINT('Ctrl Pts',(-56.0441547055335,-18.1858538720526,
2.59915764355877));
#221101=CARTESIAN_POINT('Ctrl Pts',(-56.0454124342018,-18.1822805617811,
2.59930765775263));
#221102=CARTESIAN_POINT('Ctrl Pts',(-56.0528379691454,-18.1611840081647,
2.6001933302086));
#221103=CARTESIAN_POINT('Ctrl Pts',(-56.0616522804222,-18.140987774147,
2.60365973324016));
#221104=CARTESIAN_POINT('Ctrl Pts',(-56.0715172876605,-18.1220070012978,
2.60934177082228));
#221105=CARTESIAN_POINT('Ctrl Pts',(-56.0752025259743,-18.1149164164009,
2.61146439091702));
#221106=CARTESIAN_POINT('Ctrl Pts',(-56.0790342841905,-18.10799504933,2.61389584429231));
#221107=CARTESIAN_POINT('Ctrl Pts',(-56.082994716577,-18.1012578800032,
2.6166160438524));
#221108=CARTESIAN_POINT('Ctrl Pts',(-56.0860848445995,-18.0960012025251,
2.61873848000763));
#221109=CARTESIAN_POINT('Ctrl Pts',(-56.0892533893664,-18.090857163632,
2.62103707099775));
#221110=CARTESIAN_POINT('Ctrl Pts',(-56.0924919457981,-18.0858333812,2.62350262767639));
#221111=CARTESIAN_POINT('Ctrl Pts',(-56.1038268933089,-18.0682501426878,
2.63213207605166));
#221112=CARTESIAN_POINT('Ctrl Pts',(-56.116019475181,-18.0521400431274,
2.64280685971901));
#221113=CARTESIAN_POINT('Ctrl Pts',(-56.1287094108802,-18.0378297267253,
2.6551329364607));
#221114=CARTESIAN_POINT('Ctrl Pts',(-56.1350543787298,-18.0306745685242,
2.66129597483155));
#221115=CARTESIAN_POINT('Ctrl Pts',(-56.1415236867627,-18.0239693566572,
2.66787183533838));
#221116=CARTESIAN_POINT('Ctrl Pts',(-56.1480723047924,-18.0177549231924,
2.67481125953847));
#221117=CARTESIAN_POINT('Ctrl Pts',(-56.1545929440327,-18.0115670407226,
2.68172103524065));
#221118=CARTESIAN_POINT('Ctrl Pts',(-56.1611921195216,-18.0058655198732,
2.68899101329776));
#221119=CARTESIAN_POINT('Ctrl Pts',(-56.1678256688899,-18.0006913688997,
2.69657334701261));
#221120=CARTESIAN_POINT('Ctrl Pts',(-56.1678541321546,-18.0006691676285,
2.69660588132558));
#221121=CARTESIAN_POINT('Ctrl Pts',(-56.1678825958473,-18.0006469755623,
2.69663842081367));
#221122=CARTESIAN_POINT('Ctrl Pts',(-56.1679110599659,-18.000624792701,
2.69667096547367));
#221123=CARTESIAN_POINT('Ctrl Pts',(-56.1813341912018,-17.9901637816632,
2.71201840157894));
#221124=CARTESIAN_POINT('Ctrl Pts',(-56.1948159540726,-17.9817405717263,
2.72845645939267));
#221125=CARTESIAN_POINT('Ctrl Pts',(-56.2082001169746,-17.9752392943588,
2.74568723186776));
#221126=CARTESIAN_POINT('Ctrl Pts',(-56.2220711693879,-17.9685015133128,
2.7635448259417));
#221127=CARTESIAN_POINT('Ctrl Pts',(-56.2358382617228,-17.963828030724,
2.78225519316943));
#221128=CARTESIAN_POINT('Ctrl Pts',(-56.2493274239724,-17.9611420662359,
2.80151223085291));
#221129=CARTESIAN_POINT('Ctrl Pts',(-56.2626240656099,-17.9584944364878,
2.82049442740019));
#221130=CARTESIAN_POINT('Ctrl Pts',(-56.2756515067297,-17.9577783571051,
2.84000929088984));
#221131=CARTESIAN_POINT('Ctrl Pts',(-56.2882301201489,-17.9589668048476,
2.85976644341319));
#221132=CARTESIAN_POINT('Ctrl Pts',(-56.2970001532207,-17.9597954117582,
2.87354148166741));
#221133=CARTESIAN_POINT('Ctrl Pts',(-56.3055517542522,-17.9615507925643,
2.88743438345378));
#221134=CARTESIAN_POINT('Ctrl Pts',(-56.3138168485093,-17.9642361803975,
2.9013417351601));
#221135=CARTESIAN_POINT('',(-56.6526781108322,-18.0743352474894,3.47153072139059));
#221136=CARTESIAN_POINT('',(-56.3138168485094,-17.9642361803975,2.90134173516011));
#221137=CARTESIAN_POINT('',(-58.0998260601479,-12.6735055745743,3.47153072139063));
#221138=CARTESIAN_POINT('Origin',(5.53234440788222E-15,1.85015204418142E-13,
3.47153072139072));
#221139=CARTESIAN_POINT('',(-57.7513140650719,-12.5994235324474,2.90134173516015));
#221140=CARTESIAN_POINT('',(-58.0998260601479,-12.6735055745743,3.47153072139063));
#221141=CARTESIAN_POINT('',(-57.6301266171956,-12.2652136052663,2.59908173516014));
#221142=CARTESIAN_POINT('Ctrl Pts',(-57.7513140650719,-12.5994235324474,
2.90134173516015));
#221143=CARTESIAN_POINT('Ctrl Pts',(-57.7393513895546,-12.596880640911,
2.88176998919789));
#221144=CARTESIAN_POINT('Ctrl Pts',(-57.72784201926,-12.5924689870921,2.86226752356699));
#221145=CARTESIAN_POINT('Ctrl Pts',(-57.7169326264476,-12.5862964562739,
2.84310370499987));
#221146=CARTESIAN_POINT('Ctrl Pts',(-57.7058261701616,-12.5800124270081,
2.82359371788624));
#221147=CARTESIAN_POINT('Ctrl Pts',(-57.6953406497003,-12.5719031706721,
2.80443322636963));
#221148=CARTESIAN_POINT('Ctrl Pts',(-57.6856340700667,-12.5620293850118,
2.78589323878222));
#221149=CARTESIAN_POINT('Ctrl Pts',(-57.6763384418482,-12.5525736298361,
2.7681381861997));
#221150=CARTESIAN_POINT('Ctrl Pts',(-57.6677565155047,-12.541499055613,
2.75095095198695));
#221151=CARTESIAN_POINT('Ctrl Pts',(-57.6600414936007,-12.5288165945673,
2.73457771435106));
#221152=CARTESIAN_POINT('Ctrl Pts',(-57.6539052188803,-12.5187293821036,
2.72155497955566));
#221153=CARTESIAN_POINT('Ctrl Pts',(-57.648317489476,-12.5076241774198,
2.70904711159951));
#221154=CARTESIAN_POINT('Ctrl Pts',(-57.6433665517939,-12.495488991745,
2.69718956158329));
#221155=CARTESIAN_POINT('Ctrl Pts',(-57.6433530373423,-12.49545586663,2.69715719432346));
#221156=CARTESIAN_POINT('Ctrl Pts',(-57.6433395278009,-12.4954227339057,
2.69712483219012));
#221157=CARTESIAN_POINT('Ctrl Pts',(-57.6433260231715,-12.4953895935729,
2.6970924751864));
#221158=CARTESIAN_POINT('Ctrl Pts',(-57.6406376799624,-12.4887924048451,
2.69065122242266));
#221159=CARTESIAN_POINT('Ctrl Pts',(-57.6381581392099,-12.4818600305505,
2.68442464469416));
#221160=CARTESIAN_POINT('Ctrl Pts',(-57.635899449924,-12.4746311465908,
2.67844505923568));
#221161=CARTESIAN_POINT('Ctrl Pts',(-57.6314169246175,-12.4602849257589,
2.66657815779556));
#221162=CARTESIAN_POINT('Ctrl Pts',(-57.6278047731676,-12.4447696056083,
2.65568445664162));
#221163=CARTESIAN_POINT('Ctrl Pts',(-57.625160465227,-12.4283797729326,
2.64601906229503));
#221164=CARTESIAN_POINT('Ctrl Pts',(-57.6231772342716,-12.4160873984258,
2.63877001653509));
#221165=CARTESIAN_POINT('Ctrl Pts',(-57.6217384144973,-12.4033031104475,
2.63221189387591));
#221166=CARTESIAN_POINT('Ctrl Pts',(-57.6208851370088,-12.3901511902558,
2.62645231033223));
#221167=CARTESIAN_POINT('Ctrl Pts',(-57.6205651579507,-12.3852192201839,
2.62429246650335));
#221168=CARTESIAN_POINT('Ctrl Pts',(-57.6203275209636,-12.3802355518734,
2.62224491711735));
#221169=CARTESIAN_POINT('Ctrl Pts',(-57.6201743958656,-12.3752067393931,
2.62031533672586));
#221170=CARTESIAN_POINT('Ctrl Pts',(-57.6196384580226,-12.3576058957119,
2.61356180535568));
#221171=CARTESIAN_POINT('Ctrl Pts',(-57.6201377858513,-12.3394520349017,
2.60825339735338));
#221172=CARTESIAN_POINT('Ctrl Pts',(-57.6217654557844,-12.3210261723876,
2.60463337987601));
#221173=CARTESIAN_POINT('Ctrl Pts',(-57.6225792907509,-12.3118132411305,
2.60282337113733));
#221174=CARTESIAN_POINT('Ctrl Pts',(-57.6236752122406,-12.302532309657,
2.60143545939105));
#221175=CARTESIAN_POINT('Ctrl Pts',(-57.6250648590506,-12.2932185057686,
2.60050005034586));
#221176=CARTESIAN_POINT('Ctrl Pts',(-57.6257596824556,-12.2885616038243,
2.60003234582327));
#221177=CARTESIAN_POINT('Ctrl Pts',(-57.6265279372157,-12.2838964837813,
2.59967776696056));
#221178=CARTESIAN_POINT('Ctrl Pts',(-57.6273710784659,-12.2792275366732,
2.5994401142915));
#221179=CARTESIAN_POINT('Ctrl Pts',(-57.628214219716,-12.2745585895652,
2.59920246162244));
#221180=CARTESIAN_POINT('Ctrl Pts',(-57.6291322491185,-12.2698858157461,
2.59908173791297));
#221181=CARTESIAN_POINT('Ctrl Pts',(-57.6301266171956,-12.2652136052663,
2.59908173516014));
#221182=CARTESIAN_POINT('',(-57.6364522029206,-12.2354540642047,2.59908173516014));
#221183=CARTESIAN_POINT('Origin',(3.35846787602732E-16,1.91093317232733E-13,
2.59908173516024));
#221184=CARTESIAN_POINT('',(-57.8830978693155,-11.9794294790614,2.90134173516013));
#221185=CARTESIAN_POINT('Ctrl Pts',(-57.6364522029206,-12.2354540642047,
2.59908173516014));
#221186=CARTESIAN_POINT('Ctrl Pts',(-57.6372433495198,-12.2317273068699,
2.59908174371504));
#221187=CARTESIAN_POINT('Ctrl Pts',(-57.6380783205157,-12.2280204952201,
2.59915764355881));
#221188=CARTESIAN_POINT('Ctrl Pts',(-57.6389556465833,-12.2243352914713,
2.59930765775268));
#221189=CARTESIAN_POINT('Ctrl Pts',(-57.6441353133411,-12.2025781272208,
2.60019333020887));
#221190=CARTESIAN_POINT('Ctrl Pts',(-57.6507902575949,-12.1815711838685,
2.60365973324197));
#221191=CARTESIAN_POINT('Ctrl Pts',(-57.6586171922763,-12.1616632156277,
2.60934177082667));
#221192=CARTESIAN_POINT('Ctrl Pts',(-57.6615410745244,-12.1542262614044,
2.61146439092037));
#221193=CARTESIAN_POINT('Ctrl Pts',(-57.6646283621025,-12.1469422825137,
2.61389584429419));
#221194=CARTESIAN_POINT('Ctrl Pts',(-57.6678628728672,-12.1398280421989,
2.61661604385241));
#221195=CARTESIAN_POINT('Ctrl Pts',(-57.6703866004264,-12.1342771550166,
2.61873848000764));
#221196=CARTESIAN_POINT('Ctrl Pts',(-57.6730000890932,-12.1288300925915,
2.62103707099777));
#221197=CARTESIAN_POINT('Ctrl Pts',(-57.6756957761164,-12.1234953096383,
2.62350262767642));
#221198=CARTESIAN_POINT('Ctrl Pts',(-57.6851306806978,-12.104823569302,
2.63213207605169));
#221199=CARTESIAN_POINT('Ctrl Pts',(-57.6955725063805,-12.0875272507062,
2.64280685971904));
#221200=CARTESIAN_POINT('Ctrl Pts',(-57.7066970899018,-12.071968868237,
2.65513293646074));
#221201=CARTESIAN_POINT('Ctrl Pts',(-57.7122593816625,-12.0641896770024,
2.66129597483159));
#221202=CARTESIAN_POINT('Ctrl Pts',(-57.7179923646567,-12.0568449701606,
2.66787183533841));
#221203=CARTESIAN_POINT('Ctrl Pts',(-57.7238555234915,-12.0499800630333,
2.67481125953851));
#221204=CARTESIAN_POINT('Ctrl Pts',(-57.7296936321424,-12.0431444860318,
2.68172103524069));
#221205=CARTESIAN_POINT('Ctrl Pts',(-57.7356606854447,-12.0367843970375,
2.68899101329778));
#221206=CARTESIAN_POINT('Ctrl Pts',(-57.7417170494856,-12.0309451958829,
2.69657334701263));
#221207=CARTESIAN_POINT('Ctrl Pts',(-57.7417430361608,-12.0309201410113,
2.69660588132561));
#221208=CARTESIAN_POINT('Ctrl Pts',(-57.7417690242238,-12.0308950952495,
2.6966384208137));
#221209=CARTESIAN_POINT('Ctrl Pts',(-57.7417950136726,-12.0308700585976,
2.6966709654737));
#221210=CARTESIAN_POINT('Ctrl Pts',(-57.7540511381828,-12.0190632547927,
2.71201840157874));
#221211=CARTESIAN_POINT('Ctrl Pts',(-57.7665785813554,-12.0092769601263,
2.7284564593922));
#221212=CARTESIAN_POINT('Ctrl Pts',(-57.7792098558799,-12.0014122714562,
2.745687231867));
#221213=CARTESIAN_POINT('Ctrl Pts',(-57.792300631318,-11.9932614808871,
2.76354482594064));
#221214=CARTESIAN_POINT('Ctrl Pts',(-57.8055037941273,-11.9871745471194,
2.78225519316803));
#221215=CARTESIAN_POINT('Ctrl Pts',(-57.8186383015941,-11.9830932952251,
2.80151223085117));
#221216=CARTESIAN_POINT('Ctrl Pts',(-57.8315853501684,-11.9790702919526,
2.820494427398));
#221217=CARTESIAN_POINT('Ctrl Pts',(-57.8444665749249,-11.9769963969271,
2.8400092908872));
#221218=CARTESIAN_POINT('Ctrl Pts',(-57.8571005079996,-11.9768635110976,
2.8597664434101));
#221219=CARTESIAN_POINT('Ctrl Pts',(-57.8659091109203,-11.9767708607329,
2.87354148166534));
#221220=CARTESIAN_POINT('Ctrl Pts',(-57.8745973526454,-11.977622739665,
2.88743438345275));
#221221=CARTESIAN_POINT('Ctrl Pts',(-57.8830978693155,-11.9794294790614,
2.90134173516013));
#221222=CARTESIAN_POINT('',(-58.231611300478,-12.0535047649324,3.47153072139063));
#221223=CARTESIAN_POINT('',(-57.8830978693155,-11.9794294790614,2.90134173516013));
#221224=CARTESIAN_POINT('',(-59.1062911958296,-6.53099325080078,3.47153072139067));
#221225=CARTESIAN_POINT('Origin',(5.53234440788222E-15,1.85015204418142E-13,
3.47153072139072));
#221226=CARTESIAN_POINT('',(-58.7519447039088,-6.49374646112762,2.90134173516018));
#221227=CARTESIAN_POINT('',(-59.1062911958296,-6.53099325080078,3.47153072139067));
#221228=CARTESIAN_POINT('',(-58.596486683455,-6.17403490859042,2.59908173516019));
#221229=CARTESIAN_POINT('Ctrl Pts',(-58.7519447039088,-6.49374646112762,
2.90134173516018));
#221230=CARTESIAN_POINT('Ctrl Pts',(-58.7397817566354,-6.49246793990548,
2.88176998919848));
#221231=CARTESIAN_POINT('Ctrl Pts',(-58.7278742924817,-6.48928351037797,
2.86226752356812));
#221232=CARTESIAN_POINT('Ctrl Pts',(-58.716379457304,-6.48428513539561,
2.84310370500153));
#221233=CARTESIAN_POINT('Ctrl Pts',(-58.7046769834257,-6.47919647150781,
2.82359371788848));
#221234=CARTESIAN_POINT('Ctrl Pts',(-58.6934012556399,-6.47222767386725,
2.80443322637243));
#221235=CARTESIAN_POINT('Ctrl Pts',(-58.6827157580237,-6.46342259169109,
2.78589323878551));
#221236=CARTESIAN_POINT('Ctrl Pts',(-58.6724826566719,-6.45499029386492,
2.76813818620355));
#221237=CARTESIAN_POINT('Ctrl Pts',(-58.6627901347942,-6.44487344289129,
2.75095095199129));
#221238=CARTESIAN_POINT('Ctrl Pts',(-58.6537916984241,-6.43306689707866,
2.73457771435581));
#221239=CARTESIAN_POINT('Ctrl Pts',(-58.6466346380402,-6.42367635878618,
2.72155497955872));
#221240=CARTESIAN_POINT('Ctrl Pts',(-58.6399167088215,-6.4132160663422,
2.70904711160098));
#221241=CARTESIAN_POINT('Ctrl Pts',(-58.6337244205832,-6.40166487239058,
2.69718956158333));
#221242=CARTESIAN_POINT('Ctrl Pts',(-58.6337075176478,-6.4016333413833,
2.69715719432351));
#221243=CARTESIAN_POINT('Ctrl Pts',(-58.6336906188003,-6.40160180229505,
2.69712483219017));
#221244=CARTESIAN_POINT('Ctrl Pts',(-58.6336737240427,-6.40157025512662,
2.69709247518644));
#221245=CARTESIAN_POINT('Ctrl Pts',(-58.6303105138594,-6.39529021487341,
2.6906512224227));
#221246=CARTESIAN_POINT('Ctrl Pts',(-58.6271199258587,-6.38865499943493,
2.6844246446942));
#221247=CARTESIAN_POINT('Ctrl Pts',(-58.6241179857776,-6.38170181337806,
2.67844505923572));
#221248=CARTESIAN_POINT('Ctrl Pts',(-58.6181604277965,-6.36790273412671,
2.6665781577956));
#221249=CARTESIAN_POINT('Ctrl Pts',(-58.6129462715177,-6.35284998116343,
2.65568445664167));
#221250=CARTESIAN_POINT('Ctrl Pts',(-58.6086032453499,-6.33682633915147,
2.64601906229508));
#221251=CARTESIAN_POINT('Ctrl Pts',(-58.6053459757241,-6.3248086076425,
2.63877001653514));
#221252=CARTESIAN_POINT('Ctrl Pts',(-58.6025787159787,-6.31224475095126,
2.63221189387594));
#221253=CARTESIAN_POINT('Ctrl Pts',(-58.6003553628269,-6.29925407013912,
2.62645231033226));
#221254=CARTESIAN_POINT('Ctrl Pts',(-58.599521605395,-6.29438256483457,
2.62429246650338));
#221255=CARTESIAN_POINT('Ctrl Pts',(-58.5987643350183,-6.28945103740959,
2.62224491711737));
#221256=CARTESIAN_POINT('Ctrl Pts',(-58.598086394715,-6.28446577922139,
2.62031533672589));
#221257=CARTESIAN_POINT('Ctrl Pts',(-58.5957136036534,-6.26701737556265,
2.6135618053557));
#221258=CARTESIAN_POINT('Ctrl Pts',(-58.5943126009391,-6.24891076953078,
2.60825339735341));
#221259=CARTESIAN_POINT('Ctrl Pts',(-58.594005327233,-6.23041570798267,
2.60463337987604));
#221260=CARTESIAN_POINT('Ctrl Pts',(-58.59385169038,-6.22116817720862,2.60282337113736));
#221261=CARTESIAN_POINT('Ctrl Pts',(-58.5939714867924,-6.21182353265965,
2.60143545939109));
#221262=CARTESIAN_POINT('Ctrl Pts',(-58.5943799633642,-6.20241549311785,
2.60050005034591));
#221263=CARTESIAN_POINT('Ctrl Pts',(-58.5945842016501,-6.19771147334694,
2.60003234582332));
#221264=CARTESIAN_POINT('Ctrl Pts',(-58.5948606100011,-6.19299160483014,
2.5996777669606));
#221265=CARTESIAN_POINT('Ctrl Pts',(-58.5952110945691,-6.1882601024437,
2.59944011429154));
#221266=CARTESIAN_POINT('Ctrl Pts',(-58.595561579137,-6.18352860005727,
2.59920246162248));
#221267=CARTESIAN_POINT('Ctrl Pts',(-58.5959861416118,-6.17878546397934,
2.59908173791308));
#221268=CARTESIAN_POINT('Ctrl Pts',(-58.596486683455,-6.17403490859042,
2.59908173516019));
#221269=CARTESIAN_POINT('',(-58.5996668978648,-6.14377718965343,2.59908173516018));
#221270=CARTESIAN_POINT('Origin',(3.34731138317027E-16,1.911003611651E-13,
2.59908173516024));
#221271=CARTESIAN_POINT('',(-58.8181995570484,-5.86337364149602,2.90134173516017));
#221272=CARTESIAN_POINT('Ctrl Pts',(-58.5996668978648,-6.14377718965343,
2.59908173516018));
#221273=CARTESIAN_POINT('Ctrl Pts',(-58.600064158263,-6.13998815054707,
2.59908174371508));
#221274=CARTESIAN_POINT('Ctrl Pts',(-58.600507087875,-6.13621436696425,
2.59915764355885));
#221275=CARTESIAN_POINT('Ctrl Pts',(-58.6009943991739,-6.13245764560148,
2.59930765775272));
#221276=CARTESIAN_POINT('Ctrl Pts',(-58.6038714482307,-6.11027824676976,
2.60019333020879));
#221277=CARTESIAN_POINT('Ctrl Pts',(-58.6082941124962,-6.08869075055798,
2.60365973324109));
#221278=CARTESIAN_POINT('Ctrl Pts',(-58.6139972210824,-6.06807370279834,
2.60934177082446));
#221279=CARTESIAN_POINT('Ctrl Pts',(-58.6161277126019,-6.06037186006736,
2.6114643909187));
#221280=CARTESIAN_POINT('Ctrl Pts',(-58.6184367045765,-6.05280507414621,
2.61389584429328));
#221281=CARTESIAN_POINT('Ctrl Pts',(-58.6209098557463,-6.04539170794198,
2.61661604385248));
#221282=CARTESIAN_POINT('Ctrl Pts',(-58.6228395323549,-6.039607427737,2.61873848000771));
#221283=CARTESIAN_POINT('Ctrl Pts',(-58.6248693309926,-6.0339170209357,
2.62103707099782));
#221284=CARTESIAN_POINT('Ctrl Pts',(-58.6269926140963,-6.02832968645968,
2.62350262767646));
#221285=CARTESIAN_POINT('Ctrl Pts',(-58.6344241049593,-6.00877401579361,
2.63213207605173));
#221286=CARTESIAN_POINT('Ctrl Pts',(-58.6430007716254,-5.99048098024849,
2.64280685971909));
#221287=CARTESIAN_POINT('Ctrl Pts',(-58.6524381197038,-5.97384499260644,
2.65513293646079));
#221288=CARTESIAN_POINT('Ctrl Pts',(-58.657156793743,-5.96552699878541,
2.66129597483164));
#221289=CARTESIAN_POINT('Ctrl Pts',(-58.6620906399372,-5.95762326711377,
2.66787183533846));
#221290=CARTESIAN_POINT('Ctrl Pts',(-58.6672041015819,-5.95018309968314,
2.67481125953855));
#221291=CARTESIAN_POINT('Ctrl Pts',(-58.6722957161032,-5.94277472016202,
2.68172103524073));
#221292=CARTESIAN_POINT('Ctrl Pts',(-58.6775652709344,-5.93582574548874,
2.68899101329782));
#221293=CARTESIAN_POINT('Ctrl Pts',(-58.682978094856,-5.9293854696629,2.69657334701268));
#221294=CARTESIAN_POINT('Ctrl Pts',(-58.6830013202262,-5.92935783569726,
2.69660588132565));
#221295=CARTESIAN_POINT('Ctrl Pts',(-58.6830245479289,-5.9293302106465,
2.69663842081374));
#221296=CARTESIAN_POINT('Ctrl Pts',(-58.683047777962,-5.92930259451084,
2.69667096547375));
#221297=CARTESIAN_POINT('Ctrl Pts',(-58.694002615082,-5.91627935575193,
2.71201840157873));
#221298=CARTESIAN_POINT('Ctrl Pts',(-58.7054384852674,-5.90523719704818,
2.72845645939213));
#221299=CARTESIAN_POINT('Ctrl Pts',(-58.7171784805277,-5.89609526425038,
2.74568723186687));
#221300=CARTESIAN_POINT('Ctrl Pts',(-58.7293455537156,-5.88662076592534,
2.76354482594046));
#221301=CARTESIAN_POINT('Ctrl Pts',(-58.7418401303848,-5.87918707069908,
2.78225519316782));
#221302=CARTESIAN_POINT('Ctrl Pts',(-58.7544760786566,-5.87375524644833,
2.80151223085092));
#221303=CARTESIAN_POINT('Ctrl Pts',(-58.7669316835944,-5.86840094651743,
2.82049442739782));
#221304=CARTESIAN_POINT('Ctrl Pts',(-58.779525562594,-5.86499195787703,
2.84000929088709));
#221305=CARTESIAN_POINT('Ctrl Pts',(-58.7920763953099,-5.86353919440059,
2.85976644341007));
#221306=CARTESIAN_POINT('Ctrl Pts',(-58.8008270591819,-5.86252630185747,
2.87354148166533));
#221307=CARTESIAN_POINT('Ctrl Pts',(-58.8095567514054,-5.8624653455516,
2.88743438345277));
#221308=CARTESIAN_POINT('Ctrl Pts',(-58.8181995570484,-5.86337364149602,
2.90134173516017));
#221309=CARTESIAN_POINT('',(-59.1725467709677,-5.90061356181279,3.47153072139067));
#221310=CARTESIAN_POINT('',(-58.8181995570484,-5.86337364149602,2.90134173516017));
#221311=CARTESIAN_POINT('',(-59.4651754363832,-0.316925998272859,3.47153072139071));
#221312=CARTESIAN_POINT('Origin',(5.53234440788222E-15,1.85015204418142E-13,
3.47153072139072));
#221313=CARTESIAN_POINT('',(-59.1088767419348,-0.3169225446755,2.90134173516022));
#221314=CARTESIAN_POINT('',(-59.4651754363832,-0.316925998272862,3.47153072139071));
#221315=CARTESIAN_POINT('Ctrl Pts',(-59.1088767419348,-0.3169225446755,
2.90134173516022));
#221316=CARTESIAN_POINT('Ctrl Pts',(-59.0966467827004,-0.316922401513674,
2.88176998919804));
#221317=CARTESIAN_POINT('Ctrl Pts',(-59.084471685356,-0.315000085553621,
2.86226752356721));
#221318=CARTESIAN_POINT('Ctrl Pts',(-59.0725173476321,-0.311230629648864,
2.84310370500017));
#221319=CARTESIAN_POINT('Ctrl Pts',(-59.0603470709135,-0.307393083605022,
2.82359371788663));
#221320=CARTESIAN_POINT('Ctrl Pts',(-59.0484046750358,-0.301641096264493,
2.80443322637013));
#221321=CARTESIAN_POINT('Ctrl Pts',(-59.0368573319846,-0.294001187894466,
2.7858932387828));
#221322=CARTESIAN_POINT('Ctrl Pts',(-59.0257988734988,-0.286684733436473,
2.76813818620042));
#221323=CARTESIAN_POINT('Ctrl Pts',(-59.0151019493846,-0.277636448047603,
2.75095095198779));
#221324=CARTESIAN_POINT('Ctrl Pts',(-59.0049186872999,-0.26683517245329,
2.73457771435201));
#221325=CARTESIAN_POINT('Ctrl Pts',(-58.9968192555055,-0.2582441930362,
2.72155497955629));
#221326=CARTESIAN_POINT('Ctrl Pts',(-58.9890447295123,-0.248543417987119,
2.70904711159986));
#221327=CARTESIAN_POINT('Ctrl Pts',(-58.981678934725,-0.237702773059304,
2.69718956158338));
#221328=CARTESIAN_POINT('Ctrl Pts',(-58.9816588284979,-0.237673181620044,
2.69715719432355));
#221329=CARTESIAN_POINT('Ctrl Pts',(-58.9816387254916,-0.237643581716782,
2.69712483219021));
#221330=CARTESIAN_POINT('Ctrl Pts',(-58.9816186257082,-0.237613973350095,
2.69709247518649));
#221331=CARTESIAN_POINT('Ctrl Pts',(-58.9776173965852,-0.231719887006591,
2.69065122242275));
#221332=CARTESIAN_POINT('Ctrl Pts',(-58.9737507180862,-0.225454527233169,
2.68442464469424));
#221333=CARTESIAN_POINT('Ctrl Pts',(-58.9700384170936,-0.218853219640541,
2.67844505923577));
#221334=CARTESIAN_POINT('Ctrl Pts',(-58.9626710986899,-0.205752467569738,
2.66657815779565));
#221335=CARTESIAN_POINT('Ctrl Pts',(-58.9559120649696,-0.191327202905241,
2.65568445664172));
#221336=CARTESIAN_POINT('Ctrl Pts',(-58.9499179036781,-0.175845309932059,
2.64601906229514));
#221337=CARTESIAN_POINT('Ctrl Pts',(-58.9454222827095,-0.164233890202172,
2.6387700165352));
#221338=CARTESIAN_POINT('Ctrl Pts',(-58.9413569016699,-0.15202811704111,
2.632211893876));
#221339=CARTESIAN_POINT('Ctrl Pts',(-58.9377878323772,-0.139341004225949,
2.62645231033233));
#221340=CARTESIAN_POINT('Ctrl Pts',(-58.9364494313924,-0.134583336920264,
2.62429246650345));
#221341=CARTESIAN_POINT('Ctrl Pts',(-58.9351808244388,-0.129757981227273,
2.62224491711744));
#221342=CARTESIAN_POINT('Ctrl Pts',(-58.933985496586,-0.124870896863128,
2.62031533672596));
#221343=CARTESIAN_POINT('Ctrl Pts',(-58.9298018491012,-0.107766101588619,
2.61356180535577));
#221344=CARTESIAN_POINT('Ctrl Pts',(-58.9265158655229,-0.0899051300998722,
2.60825339735346));
#221345=CARTESIAN_POINT('Ctrl Pts',(-58.9242770147326,-0.0715435052823959,
2.60463337987609));
#221346=CARTESIAN_POINT('Ctrl Pts',(-58.9231575893375,-0.0623626928736577,
2.60282337113741));
#221347=CARTESIAN_POINT('Ctrl Pts',(-58.9222999481582,-0.0530567171303812,
2.60143545939113));
#221348=CARTESIAN_POINT('Ctrl Pts',(-58.9217227791368,-0.0436575183852358,
2.60050005034595));
#221349=CARTESIAN_POINT('Ctrl Pts',(-58.9214341946262,-0.0389579190126632,
2.60003234582335));
#221350=CARTESIAN_POINT('Ctrl Pts',(-58.9212157281805,-0.0342350138892673,
2.59967776696063));
#221351=CARTESIAN_POINT('Ctrl Pts',(-58.9210697160839,-0.0294927955546917,
2.59944011429157));
#221352=CARTESIAN_POINT('Ctrl Pts',(-58.9209237039872,-0.024750577220116,
2.59920246162251));
#221353=CARTESIAN_POINT('Ctrl Pts',(-58.9208501479391,-0.0199890456748488,
2.59908173791312));
#221354=CARTESIAN_POINT('Ctrl Pts',(-58.9208513795073,-0.0152121934557294,
2.59908173516023));
#221355=CARTESIAN_POINT('Origin',(5.49031038273072E-15,1.82930781209959E-13,
3.77003198860263));
#221356=CARTESIAN_POINT('',(56.875,1.74857057214726E-13,3.77003198860264));
#221357=CARTESIAN_POINT('',(-56.875,1.8989595988011E-13,3.77003198860262));
#221358=CARTESIAN_POINT('Origin',(5.49031038273072E-15,1.82930781209959E-13,
3.77003198860263));
#221359=CARTESIAN_POINT('',(-56.875,1.8989595988011E-13,3.77003198860262));
#221360=CARTESIAN_POINT('Origin',(5.49031038273072E-15,1.82930781209959E-13,
3.77003198860263));
#221361=CARTESIAN_POINT('Origin',(0.,-8.93279506303506E-14,42.7590319886026));
#221362=CARTESIAN_POINT('',(56.875,1.87678869229944E-13,4.08753198860264));
#221363=CARTESIAN_POINT('',(56.875,-8.23627719602001E-14,42.7590319886026));
#221364=CARTESIAN_POINT('Origin',(5.44560101479317E-15,1.80713690559794E-13,
4.08753198860262));
#221365=CARTESIAN_POINT('Origin',(60.4792282238308,1.82930781209959E-13,
3.77003198860263));
#221366=CARTESIAN_POINT('',(60.1802756340597,-6.00595296980763,3.77003198860259));
#221367=CARTESIAN_POINT('',(60.1803330762808,-6.00537737563893,3.77003198882083));
#221368=CARTESIAN_POINT('Origin',(5.49031038273072E-15,1.82930781209959E-13,
3.77003198860263));
#221369=CARTESIAN_POINT('',(59.7081718144893,-5.95633285891111,3.77003198860259));
#221370=CARTESIAN_POINT('',(59.70870646733,-5.95638905318906,3.77003198860259));
#221371=CARTESIAN_POINT('',(60.0036905223731,-0.317499999999817,3.77003198860263));
#221372=CARTESIAN_POINT('Origin',(5.49031038273072E-15,1.82930781209959E-13,
3.77003198860263));
#221373=CARTESIAN_POINT('',(60.4783948217626,-0.317500000025078,3.77003198860263));
#221374=CARTESIAN_POINT('',(60.4792282238308,-0.317499999999817,3.77003198860263));
#221375=CARTESIAN_POINT('',(60.4783917836885,-0.318078445377671,3.77003198902516));
#221376=CARTESIAN_POINT('Origin',(5.49031038273072E-15,1.82930781209959E-13,
3.77003198860263));
#221377=CARTESIAN_POINT('Origin',(5.49031038273072E-15,1.82930781209959E-13,
3.77003198860263));
#221378=CARTESIAN_POINT('Origin',(5.49031038273072E-15,1.82930781209959E-13,
3.77003198860263));
#221379=CARTESIAN_POINT('',(60.6410923272405,-0.318076890623181,3.48823028058481));
#221380=CARTESIAN_POINT('',(60.3421421673489,-6.02238575972983,3.48823028074801));
#221381=CARTESIAN_POINT('Origin',(5.52999282761009E-15,1.84898592019556E-13,
3.48823028058481));
#221382=CARTESIAN_POINT('',(60.3421421670676,-6.02238575970175,3.48823028058478));
#221383=CARTESIAN_POINT('',(60.4783917829566,-0.318078445373822,3.77003198860263));
#221384=CARTESIAN_POINT('Origin',(60.71525,1.85785428279622E-13,3.36123028058482));
#221385=CARTESIAN_POINT('',(61.0122769227456,-0.317499999999814,3.36123028058482));
#221386=CARTESIAN_POINT('',(60.7112330730305,-6.06175884541469,3.36123028058478));
#221387=CARTESIAN_POINT('Origin',(5.5478765747851E-15,1.85785428279622E-13,
3.36123028058482));
#221388=CARTESIAN_POINT('',(60.5608532912344,-6.0459532934496,3.36123028058478));
#221389=CARTESIAN_POINT('',(60.561380412237,-6.04600869609946,3.36123028058478));
#221390=CARTESIAN_POINT('',(60.8610688070707,-0.317499999999814,3.36123028058482));
#221391=CARTESIAN_POINT('Origin',(5.5478765747851E-15,1.85785428279622E-13,
3.36123028058482));
#221392=CARTESIAN_POINT('',(60.71525,-0.317499999999814,3.36123028058482));
#221393=CARTESIAN_POINT('Origin',(5.5478765747851E-15,1.85785428279622E-13,
3.36123028058482));
#221394=CARTESIAN_POINT('',(61.0917542093525,-6.10232411255987,3.77003198802717));
#221395=CARTESIAN_POINT('',(61.0918106390013,-6.10175915944532,3.77003198860259));
#221396=CARTESIAN_POINT('Origin',(5.49031038273072E-15,1.82930781209959E-13,
3.77003198860263));
#221397=CARTESIAN_POINT('',(60.9299448846691,-6.08531878138219,3.4882302805848));
#221398=CARTESIAN_POINT('',(61.0917542096815,-6.10232411260822,3.77003198860259));
#221399=CARTESIAN_POINT('',(61.2322532923707,-0.316930737397142,3.48823028042695));
#221400=CARTESIAN_POINT('Origin',(5.52999282761008E-15,1.84898592019556E-13,
3.48823028058484));
#221401=CARTESIAN_POINT('',(61.3949537495049,-0.316932243253077,3.77003198802708));
#221402=CARTESIAN_POINT('',(61.2322532920972,-0.316930737395729,3.48823028058484));
#221403=CARTESIAN_POINT('',(61.3949508163454,-0.317499999999817,3.77003198860263));
#221404=CARTESIAN_POINT('Origin',(5.49031038273072E-15,1.82930781209959E-13,
3.77003198860263));
#221405=CARTESIAN_POINT('Origin',(5.49031038273072E-15,1.82930781209959E-13,
3.77003198860263));
#221406=CARTESIAN_POINT('Origin',(62.2224557307631,1.82930781209959E-13,
3.77003198860263));
#221407=CARTESIAN_POINT('',(61.8696548221181,-0.317499999999817,3.77003198860263));
#221408=CARTESIAN_POINT('',(61.5639141665613,-6.15137923967574,3.77003198860259));
#221409=CARTESIAN_POINT('Origin',(5.49031038273072E-15,1.82930781209959E-13,
3.77003198860263));
#221410=CARTESIAN_POINT('',(61.0923331762718,-6.10181408032554,3.77003198860259));
#221411=CARTESIAN_POINT('',(62.2224557307631,-0.317499999999817,3.77003198860263));
#221412=CARTESIAN_POINT('Origin',(5.57972911860581E-15,1.8736496251029E-13,
3.13503198860263));
#221413=CARTESIAN_POINT('Origin',(59.7081714060831,-5.95632779542196,3.13502491541429));
#221414=CARTESIAN_POINT('Origin',(60.0036895869254,-0.317504993060329,3.13502491541433));
#221415=CARTESIAN_POINT('Origin',(5.57972911860581E-15,1.8736496251029E-13,
3.13503198860263));
#221416=CARTESIAN_POINT('Origin',(61.6018378049622,-6.15533145331055,3.2038202287229));
#221417=CARTESIAN_POINT('Origin',(61.9077842377864,-0.317533537011376,3.20381846780282));
#221418=CARTESIAN_POINT('Origin',(5.51210908043506E-15,1.8401175575949E-13,
3.61523028058481));
#221419=CARTESIAN_POINT('Origin',(60.7269085901928,-6.06344346747399,3.58781461834287));
#221420=CARTESIAN_POINT('Origin',(61.0281367271385,-0.317462907478312,3.58786945047018));
#221421=CARTESIAN_POINT('Origin',(5.51210908043507E-15,1.8401175575949E-13,
3.61523028058481));
#221422=CARTESIAN_POINT('Origin',(60.5450849487963,-6.04425010054694,3.58786923593026));
#221423=CARTESIAN_POINT('Origin',(60.8453028802691,-0.317545368445294,3.5878144026637));
#221424=CARTESIAN_POINT('Origin',(60.4792282238308,1.82930781209959E-13,
3.77003198860263));
#221425=CARTESIAN_POINT('',(58.7584778814678,-12.1649068885782,3.77003198860255));
#221426=CARTESIAN_POINT('',(59.6417962403144,-6.58785426246997,3.77003198860259));
#221427=CARTESIAN_POINT('Origin',(5.49031038273072E-15,1.82930781209959E-13,
3.77003198860263));
#221428=CARTESIAN_POINT('',(60.1139000598801,-6.63747437341682,3.77003198860259));
#221429=CARTESIAN_POINT('',(59.7852323155142,-6.60293000146336,3.77003198860259));
#221430=CARTESIAN_POINT('',(60.1138365744454,-6.63804933242006,3.77003198902532));
#221431=CARTESIAN_POINT('Origin',(5.49031038273072E-15,1.82930781209959E-13,
3.77003198860263));
#221432=CARTESIAN_POINT('',(59.2229260464988,-12.2630370254214,3.77003198882079));
#221433=CARTESIAN_POINT('Origin',(5.49031038273072E-15,1.82930781209959E-13,
3.77003198860263));
#221434=CARTESIAN_POINT('',(59.2228087529784,-12.2636034620779,3.77003198860255));
#221435=CARTESIAN_POINT('Origin',(5.49031038273072E-15,1.82930781209959E-13,
3.77003198860263));
#221436=CARTESIAN_POINT('',(58.7590037315227,-12.1650186614579,3.77003198860255));
#221437=CARTESIAN_POINT('Origin',(5.49031038273072E-15,1.82930781209959E-13,
3.77003198860263));
#221438=CARTESIAN_POINT('',(60.275645989912,-6.65505462397295,3.48823028058477));
#221439=CARTESIAN_POINT('',(60.1138365737176,-6.6380493323397,3.77003198860259));
#221440=CARTESIAN_POINT('',(59.3820708701841,-12.2968658914367,3.48823028074797));
#221441=CARTESIAN_POINT('Origin',(5.52999282761009E-15,1.84898592019556E-13,
3.48823028058481));
#221442=CARTESIAN_POINT('',(59.3820708699072,-12.2968658913794,3.48823028058473));
#221443=CARTESIAN_POINT('Origin',(60.71525,1.85785428279622E-13,3.36123028058482));
#221444=CARTESIAN_POINT('',(59.5971203935661,-12.3431658574201,3.36123028058474));
#221445=CARTESIAN_POINT('',(60.4944777170595,-6.67747469700845,3.36123028058478));
#221446=CARTESIAN_POINT('Origin',(5.5478765747851E-15,1.85785428279622E-13,
3.36123028058482));
#221447=CARTESIAN_POINT('',(60.6448574988555,-6.69328024897355,3.36123028058478));
#221448=CARTESIAN_POINT('',(60.0186752706393,-6.62746584473993,3.36123028058478));
#221449=CARTESIAN_POINT('',(59.7450242491249,-12.3746037924155,3.36123028058474));
#221450=CARTESIAN_POINT('Origin',(5.5478765747851E-15,1.85785428279622E-13,
3.36123028058482));
#221451=CARTESIAN_POINT('',(59.5976388357908,-12.3432760557168,3.36123028058474));
#221452=CARTESIAN_POINT('Origin',(5.5478765747851E-15,1.85785428279622E-13,
3.36123028058482));
#221453=CARTESIAN_POINT('',(59.9600752506739,-12.4208962741577,3.48823028058476));
#221454=CARTESIAN_POINT('',(60.8636883190564,-6.71570789672308,3.48823028042691));
#221455=CARTESIAN_POINT('Origin',(5.52999282761008E-15,1.84898592019556E-13,
3.48823028058484));
#221456=CARTESIAN_POINT('',(61.025497328658,-6.73271622308696,3.77003198802703));
#221457=CARTESIAN_POINT('',(60.8636883187846,-6.71570789669309,3.4882302805848));
#221458=CARTESIAN_POINT('',(61.0254350648263,-6.73328056300417,3.77003198860259));
#221459=CARTESIAN_POINT('Origin',(5.49031038273072E-15,1.82930781209959E-13,
3.77003198860263));
#221460=CARTESIAN_POINT('',(60.119335800013,-12.4541661686656,3.77003198860255));
#221461=CARTESIAN_POINT('Origin',(5.49031038273072E-15,1.82930781209959E-13,
3.77003198860263));
#221462=CARTESIAN_POINT('',(60.1192206258109,-12.4547221284034,3.77003198802712));
#221463=CARTESIAN_POINT('Origin',(5.49031038273072E-15,1.82930781209959E-13,
3.77003198860263));
#221464=CARTESIAN_POINT('',(60.1192206261331,-12.4547221284859,3.77003198860255));
#221465=CARTESIAN_POINT('Origin',(62.2224557307631,1.82930781209959E-13,
3.77003198860263));
#221466=CARTESIAN_POINT('',(61.4975385923863,-6.78290064323459,3.77003198860259));
#221467=CARTESIAN_POINT('',(61.5094129706999,-6.78414869068649,3.77003198860259));
#221468=CARTESIAN_POINT('',(60.5836663843183,-12.5528626811438,3.77003198860255));
#221469=CARTESIAN_POINT('Origin',(5.49031038273072E-15,1.82930781209959E-13,
3.77003198860263));
#221470=CARTESIAN_POINT('',(60.1198497339745,-12.4542754087014,3.77003198860255));
#221471=CARTESIAN_POINT('Origin',(5.57972911860581E-15,1.8736496251029E-13,
3.13503198860263));
#221472=CARTESIAN_POINT('Origin',(59.6417947880742,-6.58785913039715,3.13502491541431));
#221473=CARTESIAN_POINT('Origin',(58.7584780045776,-12.1649018101373,3.13502491541426));
#221474=CARTESIAN_POINT('Origin',(5.57972911860581E-15,1.8736496251029E-13,
3.13503198860263));
#221475=CARTESIAN_POINT('Origin',(61.5354556255543,-6.78691960575202,3.20381846780361));
#221476=CARTESIAN_POINT('Origin',(60.6209691542414,-12.5607573437831,3.20382022872141));
#221477=CARTESIAN_POINT('Origin',(5.51210908043506E-15,1.8401175575949E-13,
3.61523028058481));
#221478=CARTESIAN_POINT('Origin',(60.6606342988055,-6.69490116062973,3.5878694504686));
#221479=CARTESIAN_POINT('Origin',(59.7604378032109,-12.3779177236591,3.58781461833967));
#221480=CARTESIAN_POINT('Origin',(5.51210908043507E-15,1.8401175575949E-13,
3.61523028058481));
#221481=CARTESIAN_POINT('Origin',(60.4787934153613,-6.67587182881982,3.58781440266453));
#221482=CARTESIAN_POINT('Origin',(59.5816164638954,-12.3398237541814,3.58786923593063));
#221483=CARTESIAN_POINT('Origin',(60.4792282238308,1.82930781209959E-13,
3.77003198860263));
#221484=CARTESIAN_POINT('',(57.1650137687749,-18.2401996527036,3.77003198860251));
#221485=CARTESIAN_POINT('',(58.6264539577985,-12.7860306150442,3.77003198860254));
#221486=CARTESIAN_POINT('Origin',(5.49031038273072E-15,1.82930781209959E-13,
3.77003198860263));
#221487=CARTESIAN_POINT('',(59.0907848292992,-12.8847271885934,3.77003198860255));
#221488=CARTESIAN_POINT('',(57.7988642628865,-12.6101209950201,3.77003198860255));
#221489=CARTESIAN_POINT('',(59.0906615920636,-12.8852923618762,3.77003198902547));
#221490=CARTESIAN_POINT('Origin',(5.49031038273072E-15,1.82930781209959E-13,
3.77003198860263));
#221491=CARTESIAN_POINT('',(57.6166602457575,-18.3863402753478,3.77003198882074));
#221492=CARTESIAN_POINT('Origin',(5.49031038273072E-15,1.82930781209959E-13,
3.77003198860263));
#221493=CARTESIAN_POINT('',(57.6164843860299,-18.3868913484936,3.77003198860251));
#221494=CARTESIAN_POINT('Origin',(5.49031038273072E-15,1.82930781209959E-13,
3.77003198860263));
#221495=CARTESIAN_POINT('',(57.1655250547209,-18.2403657795778,3.77003198860251));
#221496=CARTESIAN_POINT('Origin',(5.49031038273072E-15,1.82930781209959E-13,
3.77003198860263));
#221497=CARTESIAN_POINT('',(59.2498070616281,-12.9191181862036,3.48823028058473));
#221498=CARTESIAN_POINT('',(59.0906615913479,-12.8852923617202,3.77003198860254));
#221499=CARTESIAN_POINT('',(57.7713971780683,-18.4366189871523,3.48823028074793));
#221500=CARTESIAN_POINT('Origin',(5.52999282761009E-15,1.84898592019556E-13,
3.48823028058481));
#221501=CARTESIAN_POINT('',(57.771397177799,-18.4366189870664,3.48823028058469));
#221502=CARTESIAN_POINT('Origin',(60.71525,1.85785428279622E-13,3.36123028058482));
#221503=CARTESIAN_POINT('',(57.9804289733666,-18.5051441132832,3.36123028058469));
#221504=CARTESIAN_POINT('',(59.4650964698968,-12.9642895838861,3.36123028058473));
#221505=CARTESIAN_POINT('Origin',(5.5478765747851E-15,1.85785428279622E-13,
3.36123028058482));
#221506=CARTESIAN_POINT('',(59.6130003254557,-12.9957275188814,3.36123028058473));
#221507=CARTESIAN_POINT('',(58.0246834617332,-12.6581203474861,3.36123028058474));
#221508=CARTESIAN_POINT('',(58.1242364370959,-18.5518699907141,3.36123028058469));
#221509=CARTESIAN_POINT('Origin',(5.5478765747851E-15,1.85785428279622E-13,
3.36123028058482));
#221510=CARTESIAN_POINT('',(57.9809330566519,-18.5053078998711,3.36123028058469));
#221511=CARTESIAN_POINT('Origin',(5.5478765747851E-15,1.85785428279622E-13,
3.36123028058482));
#221512=CARTESIAN_POINT('',(58.3332704847798,-18.6203878281138,3.48823028058472));
#221513=CARTESIAN_POINT('',(59.8282880399729,-13.0409063549811,3.48823028042686));
#221514=CARTESIAN_POINT('Origin',(5.52999282761008E-15,1.84898592019556E-13,
3.48823028058484));
#221515=CARTESIAN_POINT('',(59.9874327886719,-13.0747351550701,3.77003198802699));
#221516=CARTESIAN_POINT('',(59.8282880397057,-13.0409063549229,3.48823028058476));
#221517=CARTESIAN_POINT('',(59.9873118763437,-13.0752898951316,3.77003198860254));
#221518=CARTESIAN_POINT('Origin',(5.49031038273072E-15,1.82930781209959E-13,
3.77003198860263));
#221519=CARTESIAN_POINT('',(58.48818093722,-18.6701227271401,3.77003198860251));
#221520=CARTESIAN_POINT('Origin',(5.49031038273072E-15,1.82930781209959E-13,
3.77003198860263));
#221521=CARTESIAN_POINT('',(58.4880082803372,-18.6706636022899,3.77003198802708));
#221522=CARTESIAN_POINT('Origin',(5.49031038273072E-15,1.82930781209959E-13,
3.77003198860263));
#221523=CARTESIAN_POINT('',(58.488008280649,-18.6706636024057,3.77003198860251));
#221524=CARTESIAN_POINT('Origin',(62.2224557307631,1.82930781209959E-13,
3.77003198860263));
#221525=CARTESIAN_POINT('',(60.4516424606491,-13.1739864076097,3.77003198860254));
#221526=CARTESIAN_POINT('',(59.4667368016504,-12.9646382471636,3.77003198860254));
#221527=CARTESIAN_POINT('',(58.9396512752216,-18.8168143322217,3.7700319886025));
#221528=CARTESIAN_POINT('Origin',(5.49031038273072E-15,1.82930781209959E-13,
3.77003198860263));
#221529=CARTESIAN_POINT('',(58.4886806371044,-18.6702850894748,3.77003198860251));
#221530=CARTESIAN_POINT('Origin',(5.57972911860581E-15,1.8736496251029E-13,
3.13503198860263));
#221531=CARTESIAN_POINT('Origin',(58.626452004677,-12.7860353045039,3.13502491541425));
#221532=CARTESIAN_POINT('Origin',(57.165014422052,-18.2401946149514,3.13502491541418));
#221533=CARTESIAN_POINT('Origin',(5.57972911860581E-15,1.8736496251029E-13,
3.13503198860263));
#221534=CARTESIAN_POINT('Origin',(60.4889316843639,-13.1819467630394,3.20381846779961));
#221535=CARTESIAN_POINT('Origin',(58.9759244797151,-18.8285649482862,3.20382022872155));
#221536=CARTESIAN_POINT('Origin',(5.51210908043506E-15,1.8401175575949E-13,
3.61523028058481));
#221537=CARTESIAN_POINT('Origin',(59.6285212670395,-12.9989886756678,3.58786945047026));
#221538=CARTESIAN_POINT('Origin',(58.1392191539775,-18.5567769230171,3.58781461834326));
#221539=CARTESIAN_POINT('Origin',(5.51210908043507E-15,1.8401175575949E-13,
3.61523028058481));
#221540=CARTESIAN_POINT('Origin',(59.4496656337939,-12.9610560404244,3.58781440266666));
#221541=CARTESIAN_POINT('Origin',(57.9653593207604,-18.5001997164921,3.5878692359305));
#221542=CARTESIAN_POINT('Origin',(60.4792282238308,1.82930781209959E-13,
3.77003198860263));
#221543=CARTESIAN_POINT('',(54.9452378026832,-24.1156489724268,3.77003198860246));
#221544=CARTESIAN_POINT('',(56.9687879773468,-18.844120540551,3.7700319886025));
#221545=CARTESIAN_POINT('Origin',(5.49031038273072E-15,1.82930781209959E-13,
3.77003198860263));
#221546=CARTESIAN_POINT('',(57.4202585945868,-18.9908122363893,3.7700319886025));
#221547=CARTESIAN_POINT('',(54.6058629360818,-18.0763596539221,3.77003198860251));
#221548=CARTESIAN_POINT('',(57.4200769557625,-18.9913614317947,3.77003198902511));
#221549=CARTESIAN_POINT('Origin',(5.49031038273072E-15,1.82930781209959E-13,
3.77003198860263));
#221550=CARTESIAN_POINT('',(55.3791342583023,-24.3081989336284,3.7700319888207));
#221551=CARTESIAN_POINT('Origin',(5.49031038273072E-15,1.82930781209959E-13,
3.77003198860263));
#221552=CARTESIAN_POINT('',(55.3789017591236,-24.3087286055908,3.77003198860246));
#221553=CARTESIAN_POINT('Origin',(5.49031038273072E-15,1.82930781209959E-13,
3.77003198860263));
#221554=CARTESIAN_POINT('',(54.9457289227643,-24.1158676331749,3.77003198860246));
#221555=CARTESIAN_POINT('Origin',(5.49031038273072E-15,1.82930781209959E-13,
3.77003198860263));
#221556=CARTESIAN_POINT('',(57.5748148483578,-19.0416371860869,3.48823028058469));
#221557=CARTESIAN_POINT('',(57.4200769550675,-18.9913614315648,3.7700319886025));
#221558=CARTESIAN_POINT('',(55.5277679690275,-24.3743766271342,3.48823028074788));
#221559=CARTESIAN_POINT('Origin',(5.52999282761009E-15,1.84898592019556E-13,
3.48823028058481));
#221560=CARTESIAN_POINT('',(55.5277679687686,-24.3743766270205,3.48823028058465));
#221561=CARTESIAN_POINT('Origin',(60.71525,1.85785428279622E-13,3.36123028058482));
#221562=CARTESIAN_POINT('',(55.7284918401501,-24.4643761377908,3.36123028058465));
#221563=CARTESIAN_POINT('',(57.7842031819385,-19.1090650011306,3.36123028058469));
#221564=CARTESIAN_POINT('Origin',(5.5478765747851E-15,1.85785428279622E-13,
3.36123028058482));
#221565=CARTESIAN_POINT('',(57.9280106456678,-19.1557908785616,3.36123028058469));
#221566=CARTESIAN_POINT('',(54.8193466381482,-18.1457247135482,3.36123028058469));
#221567=CARTESIAN_POINT('',(55.8666273273836,-24.5258780191662,3.36123028058465));
#221568=CARTESIAN_POINT('Origin',(5.5478765747851E-15,1.85785428279622E-13,
3.36123028058482));
#221569=CARTESIAN_POINT('',(55.7289760416541,-24.4645917181899,3.36123028058465));
#221570=CARTESIAN_POINT('Origin',(5.5478765747851E-15,1.85785428279622E-13,
3.36123028058482));
#221571=CARTESIAN_POINT('',(56.0673542004329,-24.6158705164585,3.48823028058468));
#221572=CARTESIAN_POINT('',(58.1373965172492,-19.2232259142289,3.48823028042681));
#221573=CARTESIAN_POINT('Origin',(5.52999282761008E-15,1.84898592019556E-13,
3.48823028058484));
#221574=CARTESIAN_POINT('',(58.2921333818759,-19.27350455263,3.77003198802694));
#221575=CARTESIAN_POINT('',(58.1373965169896,-19.223225914143,3.48823028058471));
#221576=CARTESIAN_POINT('',(58.2919551457919,-19.2740436149875,3.7700319886025));
#221577=CARTESIAN_POINT('Origin',(5.49031038273072E-15,1.82930781209959E-13,
3.77003198860263));
#221578=CARTESIAN_POINT('',(56.2162173246401,-24.6815255140418,3.77003198860246));
#221579=CARTESIAN_POINT('Origin',(5.49031038273072E-15,1.82930781209959E-13,
3.77003198860263));
#221580=CARTESIAN_POINT('',(56.2159890767415,-24.6820453786623,3.77003198802704));
#221581=CARTESIAN_POINT('Origin',(5.49031038273072E-15,1.82930781209959E-13,
3.77003198860263));
#221582=CARTESIAN_POINT('',(56.2159890770395,-24.68204537881,3.77003198860246));
#221583=CARTESIAN_POINT('Origin',(62.2224557307631,1.82930781209959E-13,
3.77003198860263));
#221584=CARTESIAN_POINT('',(58.7434254837935,-19.4207352200692,3.7700319886025));
#221585=CARTESIAN_POINT('',(56.182627028633,-18.5886813639048,3.77003198860251));
#221586=CARTESIAN_POINT('',(56.6498810128385,-24.8746050278044,3.77003198860246));
#221587=CARTESIAN_POINT('Origin',(5.49031038273072E-15,1.82930781209959E-13,
3.77003198860263));
#221588=CARTESIAN_POINT('',(56.2166973156309,-24.6817392197996,3.77003198860246));
#221589=CARTESIAN_POINT('Origin',(5.57972911860581E-15,1.8736496251029E-13,
3.13503198860263));
#221590=CARTESIAN_POINT('Origin',(56.9687855447427,-18.8441250001647,3.13502491541417));
#221591=CARTESIAN_POINT('Origin',(54.94523897897,-24.115644030558,3.1350249154142));
#221592=CARTESIAN_POINT('Origin',(5.57972911860581E-15,1.8736496251029E-13,
3.13503198860263));
#221593=CARTESIAN_POINT('Origin',(58.7796783495195,-19.4325497530921,3.20381846780104));
#221594=CARTESIAN_POINT('Origin',(56.6847272350835,-24.8900828550879,3.20382022872263));
#221595=CARTESIAN_POINT('Origin',(5.51210908043506E-15,1.8401175575949E-13,
3.61523028058481));
#221596=CARTESIAN_POINT('Origin',(57.943105678202,-19.1606565505621,3.58786945047092));
#221597=CARTESIAN_POINT('Origin',(55.8810150532823,-24.5323241911522,3.58781461834182));
#221598=CARTESIAN_POINT('Origin',(5.51210908043507E-15,1.8401175575949E-13,
3.61523028058481));
#221599=CARTESIAN_POINT('Origin',(57.7691948748979,-19.1042362097742,3.58781440266462));
#221600=CARTESIAN_POINT('Origin',(55.7140215708763,-24.4578836192926,3.58786923593034));
#221601=CARTESIAN_POINT('Origin',(60.4792282238308,1.82930781209959E-13,
3.77003198860263));
#221602=CARTESIAN_POINT('',(52.123470313195,-29.7268821954841,3.77003198860243));
#221603=CARTESIAN_POINT('',(54.68696003433,-24.6957503380299,3.77003198860246));
#221604=CARTESIAN_POINT('Origin',(5.49031038273072E-15,1.82930781209959E-13,
3.77003198860263));
#221605=CARTESIAN_POINT('',(55.1206239907505,-24.8888299712403,3.77003198860246));
#221606=CARTESIAN_POINT('',(50.3447265545032,-22.7624634345039,3.77003198860247));
#221607=CARTESIAN_POINT('',(55.1203859404112,-24.8893571716688,3.77003198902525));
#221608=CARTESIAN_POINT('Origin',(5.49031038273072E-15,1.82930781209959E-13,
3.77003198860263));
#221609=CARTESIAN_POINT('',(52.5348628870842,-29.9637318775746,3.77003198882067));
#221610=CARTESIAN_POINT('Origin',(5.49031038273072E-15,1.82930781209959E-13,
3.77003198860263));
#221611=CARTESIAN_POINT('',(52.5345762957642,-29.9642343451567,3.77003198860242));
#221612=CARTESIAN_POINT('Origin',(5.49031038273072E-15,1.82930781209959E-13,
3.77003198860263));
#221613=CARTESIAN_POINT('',(52.123935886597,-29.7271509944131,3.77003198860243));
#221614=CARTESIAN_POINT('Origin',(5.49031038273072E-15,1.82930781209959E-13,
3.77003198860263));
#221615=CARTESIAN_POINT('',(55.2690209153043,-24.9555320242407,3.48823028058464));
#221616=CARTESIAN_POINT('',(55.1203859397437,-24.8893571713674,3.77003198860246));
#221617=CARTESIAN_POINT('',(52.6757649141856,-30.0450834961229,3.48823028074784));
#221618=CARTESIAN_POINT('Origin',(5.52999282761009E-15,1.84898592019556E-13,
3.48823028058481));
#221619=CARTESIAN_POINT('',(52.67576491394,-30.0450834959828,3.48823028058461));
#221620=CARTESIAN_POINT('Origin',(60.71525,1.85785428279622E-13,3.36123028058482));
#221621=CARTESIAN_POINT('',(52.8659816883963,-30.1555713378329,3.36123028058461));
#221622=CARTESIAN_POINT('',(55.470214071797,-25.0444775033939,3.36123028058465));
#221623=CARTESIAN_POINT('Origin',(5.5478765747851E-15,1.85785428279622E-13,
3.36123028058482));
#221624=CARTESIAN_POINT('',(55.6083495590305,-25.1059793847693,3.36123028058465));
#221625=CARTESIAN_POINT('',(50.5417021396889,-22.850162615334,3.36123028058466));
#221626=CARTESIAN_POINT('',(52.9969317578291,-30.2311753956704,3.36123028058461));
#221627=CARTESIAN_POINT('Origin',(5.5478765747851E-15,1.85785428279622E-13,
3.36123028058482));
#221628=CARTESIAN_POINT('',(52.866440703106,-30.1558363500991,3.36123028058461));
#221629=CARTESIAN_POINT('Origin',(5.5478765747851E-15,1.85785428279622E-13,
3.36123028058482));
#221630=CARTESIAN_POINT('',(53.1871522506179,-30.3416565762228,3.48823028058463));
#221631=CARTESIAN_POINT('',(55.8095395122503,-25.1949317876417,3.48823028042678));
#221632=CARTESIAN_POINT('Origin',(5.52999282761008E-15,1.84898592019556E-13,
3.48823028058484));
#221633=CARTESIAN_POINT('',(55.9581731633348,-25.2611094010713,3.7700319880269));
#221634=CARTESIAN_POINT('',(55.809539512001,-25.1949317875292,3.48823028058467));
#221635=CARTESIAN_POINT('',(55.9579395562869,-25.2616268796448,3.77003198860246));
#221636=CARTESIAN_POINT('Origin',(5.49031038273072E-15,1.82930781209959E-13,
3.77003198860263));
#221637=CARTESIAN_POINT('',(53.3283370710516,-30.4225123424703,3.77003198860242));
#221638=CARTESIAN_POINT('Origin',(5.49031038273072E-15,1.82930781209959E-13,
3.77003198860263));
#221639=CARTESIAN_POINT('',(53.328055732869,-30.4230055008159,3.770031988027));
#221640=CARTESIAN_POINT('Origin',(5.49031038273072E-15,1.82930781209959E-13,
3.77003198860263));
#221641=CARTESIAN_POINT('',(53.32805573315,-30.4230055009939,3.77003198860242));
#221642=CARTESIAN_POINT('Origin',(62.2224557307631,1.82930781209959E-13,
3.77003198860263));
#221643=CARTESIAN_POINT('',(56.3916032444854,-25.4547063934074,3.77003198860246));
#221644=CARTESIAN_POINT('',(51.7995637473369,-23.4101986852072,3.77003198860247));
#221645=CARTESIAN_POINT('',(53.7394427993291,-30.6598643453566,3.77003198860242));
#221646=CARTESIAN_POINT('Origin',(5.49031038273072E-15,1.82930781209959E-13,
3.77003198860263));
#221647=CARTESIAN_POINT('',(53.3287920942672,-30.4227750502462,3.77003198860242));
#221648=CARTESIAN_POINT('Origin',(5.57972911860581E-15,1.8736496251029E-13,
3.13503198860263));
#221649=CARTESIAN_POINT('Origin',(54.6869571488954,-24.6957545189369,3.13502491541414));
#221650=CARTESIAN_POINT('Origin',(52.1234719996039,-29.7268774036429,3.13502491541413));
#221651=CARTESIAN_POINT('Origin',(5.57972911860581E-15,1.8736496251029E-13,
3.13503198860263));
#221652=CARTESIAN_POINT('Origin',(56.426422558239,-25.470245661524,3.20381846780071));
#221653=CARTESIAN_POINT('Origin',(53.7724802568203,-30.6788998055451,3.20382022872057));
#221654=CARTESIAN_POINT('Origin',(5.51210908043506E-15,1.8401175575949E-13,
3.61523028058481));
#221655=CARTESIAN_POINT('Origin',(55.6228532981809,-25.1123962626636,3.58786945046893));
#221656=CARTESIAN_POINT('Origin',(53.0105668578093,-30.2390901817304,3.58781461833926));
#221657=CARTESIAN_POINT('Origin',(5.51210908043507E-15,1.8401175575949E-13,
3.61523028058481));
#221658=CARTESIAN_POINT('Origin',(55.4557927279746,-25.0381063693869,3.5878144026651));
#221659=CARTESIAN_POINT('Origin',(52.8522693417503,-30.1476018310214,3.58786923592679));
#221660=CARTESIAN_POINT('Origin',(60.4792282238308,1.82930781209959E-13,
3.77003198860263));
#221661=CARTESIAN_POINT('',(48.7306271754181,-35.0124214764577,3.77003198860239));
#221662=CARTESIAN_POINT('',(51.805970313195,-30.2768083268872,3.77003198860242));
#221663=CARTESIAN_POINT('Origin',(5.49031038273072E-15,1.82930781209959E-13,
3.77003198860263));
#221664=CARTESIAN_POINT('',(52.2170762957395,-30.5141604766039,3.77003198860242));
#221665=CARTESIAN_POINT('',(45.2006711678738,-26.4632370872581,3.77003198860245));
#221666=CARTESIAN_POINT('',(52.2167844420142,-30.5146599059371,3.77003198902529));
#221667=CARTESIAN_POINT('Origin',(5.49031038273072E-15,1.82930781209959E-13,
3.77003198860263));
#221668=CARTESIAN_POINT('',(49.1150085644485,-35.2909759047561,3.77003198882063));
#221669=CARTESIAN_POINT('Origin',(5.49031038273072E-15,1.82930781209959E-13,
3.77003198860263));
#221670=CARTESIAN_POINT('',(49.1146710209414,-35.2914456628179,3.77003198860239));
#221671=CARTESIAN_POINT('Origin',(5.49031038273072E-15,1.82930781209959E-13,
3.77003198860263));
#221672=CARTESIAN_POINT('',(48.7310621012213,-35.0127374685503,3.77003198860239));
#221673=CARTESIAN_POINT('Origin',(5.49031038273072E-15,1.82930781209959E-13,
3.77003198860263));
#221674=CARTESIAN_POINT('',(52.3576880233166,-30.596008831256,3.48823028058461));
#221675=CARTESIAN_POINT('',(52.2167844413819,-30.5146599055676,3.77003198860242));
#221676=CARTESIAN_POINT('',(49.2466351558313,-35.3866101429902,3.4882302807478));
#221677=CARTESIAN_POINT('Origin',(5.52999282761009E-15,1.84898592019556E-13,
3.48823028058481));
#221678=CARTESIAN_POINT('',(49.2466351556017,-35.3866101428252,3.48823028058457));
#221679=CARTESIAN_POINT('Origin',(60.71525,1.85785428279622E-13,3.36123028058482));
#221680=CARTESIAN_POINT('',(49.4242607783465,-35.5163757878388,3.36123028058458));
#221681=CARTESIAN_POINT('',(52.5484816883963,-30.7054974692361,3.36123028058461));
#221682=CARTESIAN_POINT('Origin',(5.5478765747851E-15,1.85785428279622E-13,
3.36123028058482));
#221683=CARTESIAN_POINT('',(52.6794317578291,-30.7811015270735,3.36123028058461));
#221684=CARTESIAN_POINT('',(45.3776875000007,-26.5654375142626,3.36123028058464));
#221685=CARTESIAN_POINT('',(49.5465907136149,-35.6052536882594,3.36123028058457));
#221686=CARTESIAN_POINT('Origin',(5.5478765747851E-15,1.85785428279622E-13,
3.36123028058482));
#221687=CARTESIAN_POINT('',(49.4246895772007,-35.5166873284423,3.36123028058458));
#221688=CARTESIAN_POINT('Origin',(5.5478765747851E-15,1.85785428279622E-13,
3.36123028058482));
#221689=CARTESIAN_POINT('',(49.7242207306179,-35.7350130971381,3.4882302805846));
#221690=CARTESIAN_POINT('',(52.8702215134581,-30.8905967160107,3.48823028042674));
#221691=CARTESIAN_POINT('Origin',(5.52999282761008E-15,1.84898592019556E-13,
3.48823028058484));
#221692=CARTESIAN_POINT('',(53.0111234896157,-30.9719482486873,3.77003198802686));
#221693=CARTESIAN_POINT('',(52.870221513222,-30.8905967158728,3.48823028058463));
#221694=CARTESIAN_POINT('',(53.0108370710516,-30.9724384738734,3.77003198860242));
#221695=CARTESIAN_POINT('Origin',(5.49031038273072E-15,1.82930781209959E-13,
3.77003198860263));
#221696=CARTESIAN_POINT('',(49.8561803968407,-35.8301837593547,3.77003198860238));
#221697=CARTESIAN_POINT('Origin',(5.49031038273072E-15,1.82930781209959E-13,
3.77003198860263));
#221698=CARTESIAN_POINT('',(49.8558490507741,-35.8306448082795,3.77003198802696));
#221699=CARTESIAN_POINT('Origin',(5.49031038273072E-15,1.82930781209959E-13,
3.77003198860263));
#221700=CARTESIAN_POINT('',(49.8558490510349,-35.8306448084859,3.77003198860238));
#221701=CARTESIAN_POINT('Origin',(62.2224557307631,1.82930781209959E-13,
3.77003198860263));
#221702=CARTESIAN_POINT('',(53.4219427993291,-31.2097904767597,3.77003198860242));
#221703=CARTESIAN_POINT('',(46.508091798073,-27.2180767400477,3.77003198860244));
#221704=CARTESIAN_POINT('',(50.2402240048087,-36.1092077731521,3.77003198860238));
#221705=CARTESIAN_POINT('Origin',(5.49031038273072E-15,1.82930781209959E-13,
3.77003198860263));
#221706=CARTESIAN_POINT('',(49.8566054669514,-35.8304925908675,3.77003198860238));
#221707=CARTESIAN_POINT('Origin',(5.57972911860581E-15,1.8736496251029E-13,
3.13503198860263));
#221708=CARTESIAN_POINT('Origin',(51.8059670065433,-30.2768121832808,3.13502491541412));
#221709=CARTESIAN_POINT('Origin',(48.7306293534724,-35.0124168871445,3.13502491541408));
#221710=CARTESIAN_POINT('Origin',(5.57972911860581E-15,1.8736496251029E-13,
3.13503198860263));
#221711=CARTESIAN_POINT('Origin',(53.4549470734263,-31.2288842284957,3.20381846780449));
#221712=CARTESIAN_POINT('Origin',(50.2710907322482,-36.1315923097636,3.20382022872168));
#221713=CARTESIAN_POINT('Origin',(5.51210908043506E-15,1.8401175575949E-13,
3.61523028058481));
#221714=CARTESIAN_POINT('Origin',(52.6931852975928,-30.7889993062039,3.5878694504706));
#221715=CARTESIAN_POINT('Origin',(49.5593237986642,-35.614550372339,3.58781461834505));
#221716=CARTESIAN_POINT('Origin',(5.51210908043507E-15,1.8401175575949E-13,
3.61523028058481));
#221717=CARTESIAN_POINT('Origin',(52.5348053110524,-30.6976537960595,3.58781440266643));
#221718=CARTESIAN_POINT('Origin',(49.4114565896706,-35.5070166082985,3.58786923592949));
#221719=CARTESIAN_POINT('Origin',(60.4792282238308,1.82930781209959E-13,
3.77003198860263));
#221720=CARTESIAN_POINT('',(44.8038810887679,-39.914357340915,3.77003198860236));
#221721=CARTESIAN_POINT('',(48.3573835402124,-35.5261472678858,3.77003198860239));
#221722=CARTESIAN_POINT('Origin',(5.49031038273072E-15,1.82930781209959E-13,
3.77003198860263));
#221723=CARTESIAN_POINT('',(48.7414273857065,-35.8051714542873,3.77003198860238));
#221724=CARTESIAN_POINT('',(39.3975469582356,-29.0164449471017,3.77003198860243));
#221725=CARTESIAN_POINT('',(48.7410849262051,-35.8056376406725,3.77003198902474));
#221726=CARTESIAN_POINT('Origin',(5.49031038273072E-15,1.82930781209959E-13,
3.77003198860263));
#221727=CARTESIAN_POINT('',(45.1570399300043,-40.2315646148135,3.77003198882059));
#221728=CARTESIAN_POINT('Origin',(5.49031038273072E-15,1.82930781209959E-13,
3.77003198860263));
#221729=CARTESIAN_POINT('',(45.1566551325076,-40.2319965165875,3.77003198860235));
#221730=CARTESIAN_POINT('Origin',(5.49031038273072E-15,1.82930781209959E-13,
3.77003198860263));
#221731=CARTESIAN_POINT('',(44.8042806018342,-39.9147170640957,3.77003198860236));
#221732=CARTESIAN_POINT('Origin',(5.49031038273072E-15,1.82930781209959E-13,
3.77003198860263));
#221733=CARTESIAN_POINT('',(48.8727133447948,-35.9012693628897,3.48823028058457));
#221734=CARTESIAN_POINT('',(48.7410849256156,-35.8056376402393,3.77003198860238));
#221735=CARTESIAN_POINT('',(45.2779489571888,-40.3404336840066,3.48823028074777));
#221736=CARTESIAN_POINT('Origin',(5.52999282761009E-15,1.84898592019556E-13,
3.48823028058481));
#221737=CARTESIAN_POINT('',(45.2779489569777,-40.3404336838186,3.48823028058454));
#221738=CARTESIAN_POINT('Origin',(60.71525,1.85785428279622E-13,3.36123028058482));
#221739=CARTESIAN_POINT('',(45.4410373245177,-40.4880553924336,3.36123028058454));
#221740=CARTESIAN_POINT('',(49.0510171431408,-36.0301015792669,3.36123028058457));
#221741=CARTESIAN_POINT('Origin',(5.5478765747851E-15,1.85785428279622E-13,
3.36123028058482));
#221742=CARTESIAN_POINT('',(49.1733470784092,-36.1189794796875,3.36123028058457));
#221743=CARTESIAN_POINT('',(39.5520252162596,-29.1286799712083,3.36123028058462));
#221744=CARTESIAN_POINT('',(45.5534068532516,-40.5892333705615,3.36123028058454));
#221745=CARTESIAN_POINT('Origin',(5.5478765747851E-15,1.85785428279622E-13,
3.36123028058482));
#221746=CARTESIAN_POINT('',(45.4414312095063,-40.4884100480704,3.36123028058454));
#221747=CARTESIAN_POINT('Origin',(5.5478765747851E-15,1.85785428279622E-13,
3.36123028058482));
#221748=CARTESIAN_POINT('',(45.7165002428312,-40.736849336529,3.48823028058456));
#221749=CARTESIAN_POINT('',(49.3516463039594,-36.2478178024862,3.48823028042671));
#221750=CARTESIAN_POINT('Origin',(5.52999282761008E-15,1.84898592019556E-13,
3.48823028058484));
#221751=CARTESIAN_POINT('',(49.4832728536536,-36.3434519499939,3.77003198802682));
#221752=CARTESIAN_POINT('',(49.351646303739,-36.2478178023243,3.48823028058459));
#221753=CARTESIAN_POINT('',(49.482936761635,-36.3439095507828,3.77003198860238));
#221754=CARTESIAN_POINT('Origin',(5.49031038273072E-15,1.82930781209959E-13,
3.77003198860263));
#221755=CARTESIAN_POINT('',(45.8377889771256,-40.8452921850237,3.77003198860235));
#221756=CARTESIAN_POINT('Origin',(5.49031038273072E-15,1.82930781209959E-13,
3.77003198860263));
#221757=CARTESIAN_POINT('',(45.8374112534718,-40.845716073179,3.77003198802693));
#221758=CARTESIAN_POINT('Origin',(5.49031038273072E-15,1.82930781209959E-13,
3.77003198860263));
#221759=CARTESIAN_POINT('',(45.8374112537096,-40.8457160734115,3.77003198860235));
#221760=CARTESIAN_POINT('Origin',(62.2224557307631,1.82930781209959E-13,
3.77003198860263));
#221761=CARTESIAN_POINT('',(49.866980369603,-36.6229335645802,3.77003198860238));
#221762=CARTESIAN_POINT('',(40.5385041740537,-29.8453988870281,3.77003198860243));
#221763=CARTESIAN_POINT('',(46.190562802649,-41.1629311642473,3.77003198860235));
#221764=CARTESIAN_POINT('Origin',(5.49031038273072E-15,1.82930781209959E-13,
3.77003198860263));
#221765=CARTESIAN_POINT('',(45.8381794369742,-40.8456437566505,3.77003198860235));
#221766=CARTESIAN_POINT('Origin',(5.57972911860581E-15,1.8736496251029E-13,
3.13503198860263));
#221767=CARTESIAN_POINT('Origin',(48.3573798485719,-35.5261507575143,3.1350249154141));
#221768=CARTESIAN_POINT('Origin',(44.8038837346045,-39.9143530044111,3.13502491541405));
#221769=CARTESIAN_POINT('Origin',(5.57972911860581E-15,1.8736496251029E-13,
3.13503198860263));
#221770=CARTESIAN_POINT('Origin',(49.8978080023041,-36.6453726047983,3.20381846780044));
#221771=CARTESIAN_POINT('Origin',(46.2189206177148,-41.188419527609,3.20382022872215));
#221772=CARTESIAN_POINT('Origin',(5.51210908043506E-15,1.8401175575949E-13,
3.61523028058481));
#221773=CARTESIAN_POINT('Origin',(49.1861997321271,-36.1282716303333,3.58786945047134));
#221774=CARTESIAN_POINT('Origin',(45.5650984170293,-40.5998100962466,3.58781461834286));
#221775=CARTESIAN_POINT('Origin',(5.51210908043507E-15,1.8401175575949E-13,
3.61523028058481));
#221776=CARTESIAN_POINT('Origin',(49.0382355735229,-36.0208713038475,3.58781440266324));
#221777=CARTESIAN_POINT('Origin',(45.4292815791815,-40.4774090812908,3.58786923592671));
#221778=CARTESIAN_POINT('Origin',(60.4792282238308,1.82930781209959E-13,
3.77003198860263));
#221779=CARTESIAN_POINT('',(40.3862543050944,-44.3789831537289,3.77003198860233));
#221780=CARTESIAN_POINT('',(44.37898315373,-40.3862543050931,3.77003198860235));
#221781=CARTESIAN_POINT('Origin',(5.49031038273072E-15,1.82930781209959E-13,
3.77003198860263));
#221782=CARTESIAN_POINT('',(44.7317571974364,-40.7038934808036,3.77003198860235));
#221783=CARTESIAN_POINT('',(33.1880655373225,-30.3099068238761,3.77003198860242));
#221784=CARTESIAN_POINT('',(44.7313678842181,-40.7043213166061,3.77003198902512));
#221785=CARTESIAN_POINT('Origin',(5.49031038273072E-15,1.82930781209959E-13,
3.77003198860263));
#221786=CARTESIAN_POINT('',(40.7043213163689,-44.7313678839549,3.77003198882056));
#221787=CARTESIAN_POINT('Origin',(5.49031038273072E-15,1.82930781209959E-13,
3.77003198860263));
#221788=CARTESIAN_POINT('',(40.7038934808044,-44.7317571974348,3.77003198860232));
#221789=CARTESIAN_POINT('Origin',(5.49031038273072E-15,1.82930781209959E-13,
3.77003198860263));
#221790=CARTESIAN_POINT('',(40.386614028275,-44.3793826667952,3.77003198860233));
#221791=CARTESIAN_POINT('Origin',(5.49031038273072E-15,1.82930781209959E-13,
3.77003198860263));
#221792=CARTESIAN_POINT('',(44.8522789915946,-40.8131880745599,3.48823028058453));
#221793=CARTESIAN_POINT('',(44.7313678836765,-40.7043213161132,3.77003198860235));
#221794=CARTESIAN_POINT('',(40.8131880747515,-44.8522789918026,3.48823028074774));
#221795=CARTESIAN_POINT('Origin',(5.52999282761009E-15,1.84898592019556E-13,
3.48823028058481));
#221796=CARTESIAN_POINT('',(40.8131880745612,-44.8522789915935,3.48823028058451));
#221797=CARTESIAN_POINT('Origin',(60.71525,1.85785428279622E-13,3.36123028058482));
#221798=CARTESIAN_POINT('',(40.959952356613,-45.0161393894786,3.36123028058451));
#221799=CARTESIAN_POINT('',(45.0161393894798,-40.9599523566118,3.36123028058454));
#221800=CARTESIAN_POINT('Origin',(5.5478765747851E-15,1.85785428279622E-13,
3.36123028058482));
#221801=CARTESIAN_POINT('',(45.1285089182138,-41.0611303347397,3.36123028058454));
#221802=CARTESIAN_POINT('',(33.3184119221875,-30.4272712359681,3.3612302805846));
#221803=CARTESIAN_POINT('',(41.0611303347409,-45.1285089182126,3.36123028058451));
#221804=CARTESIAN_POINT('Origin',(5.5478765747851E-15,1.85785428279622E-13,
3.36123028058482));
#221805=CARTESIAN_POINT('',(40.9603070122498,-45.0165332744673,3.36123028058451));
#221806=CARTESIAN_POINT('Origin',(5.5478765747851E-15,1.85785428279622E-13,
3.36123028058482));
#221807=CARTESIAN_POINT('',(41.2079002115913,-45.292364129855,3.48823028058453));
#221808=CARTESIAN_POINT('',(45.2923641300585,-41.2079002117741,3.48823028042666));
#221809=CARTESIAN_POINT('Origin',(5.52999282761008E-15,1.84898592019556E-13,
3.48823028058484));
#221810=CARTESIAN_POINT('',(45.4132731252663,-41.3167691863802,3.77003198802679));
#221811=CARTESIAN_POINT('',(45.2923641298562,-41.20790021159,3.48823028058456));
#221812=CARTESIAN_POINT('',(45.4128910420877,-41.3171891492018,3.77003198860235));
#221813=CARTESIAN_POINT('Origin',(5.49031038273072E-15,1.82930781209959E-13,
3.77003198860263));
#221814=CARTESIAN_POINT('',(41.3171891492031,-45.4128910420865,3.77003198860232));
#221815=CARTESIAN_POINT('Origin',(5.49031038273072E-15,1.82930781209959E-13,
3.77003198860263));
#221816=CARTESIAN_POINT('',(41.3167691863815,-45.4132731252652,3.7700319880269));
#221817=CARTESIAN_POINT('Origin',(5.49031038273072E-15,1.82930781209959E-13,
3.77003198860263));
#221818=CARTESIAN_POINT('',(41.3167691865937,-45.4132731255213,3.77003198860232));
#221819=CARTESIAN_POINT('Origin',(62.2224557307631,1.82930781209959E-13,
3.77003198860263));
#221820=CARTESIAN_POINT('',(45.7656648676111,-41.6348281284255,3.77003198860234));
#221821=CARTESIAN_POINT('',(34.1507877370015,-31.1767457860023,3.77003198860241));
#221822=CARTESIAN_POINT('',(41.6348281284267,-45.7656648676099,3.77003198860232));
#221823=CARTESIAN_POINT('Origin',(5.49031038273072E-15,1.82930781209959E-13,
3.77003198860263));
#221824=CARTESIAN_POINT('',(41.3175407208299,-45.4132815019352,3.77003198860232));
#221825=CARTESIAN_POINT('Origin',(5.57972911860581E-15,1.8736496251029E-13,
3.13503198860263));
#221826=CARTESIAN_POINT('Origin',(44.3789791175472,-40.3862573897237,3.13502491541404));
#221827=CARTESIAN_POINT('Origin',(40.3862573897248,-44.3789791175461,3.13502491541401));
#221828=CARTESIAN_POINT('Origin',(5.57972911860581E-15,1.8736496251029E-13,
3.13503198860263));
#221829=CARTESIAN_POINT('Origin',(45.7939781049198,-41.6603666103112,3.20381846780193));
#221830=CARTESIAN_POINT('Origin',(41.6603663369564,-45.793977801883,3.20382022871952));
#221831=CARTESIAN_POINT('Origin',(5.51210908043506E-15,1.8401175575949E-13,
3.61523028058481));
#221832=CARTESIAN_POINT('Origin',(45.1403198695222,-41.0717150501539,3.58786945047173));
#221833=CARTESIAN_POINT('Origin',(41.071652282027,-45.1402498046829,3.5878146183419));
#221834=CARTESIAN_POINT('Origin',(5.51210908043507E-15,1.8401175575949E-13,
3.61523028058481));
#221835=CARTESIAN_POINT('Origin',(45.0043926651417,-40.9494366077805,3.58781440266656));
#221836=CARTESIAN_POINT('Origin',(40.9493738530224,-45.0043225899478,3.58786923592653));
#221837=CARTESIAN_POINT('Origin',(60.4792282238308,1.82930781209959E-13,
3.77003198860263));
#221838=CARTESIAN_POINT('',(35.5261472678871,-48.3573835402113,3.7700319886023));
#221839=CARTESIAN_POINT('',(39.9143573409162,-44.8038810887668,3.77003198860232));
#221840=CARTESIAN_POINT('Origin',(5.49031038273072E-15,1.82930781209959E-13,
3.77003198860263));
#221841=CARTESIAN_POINT('',(40.2319965165892,-45.1566551325069,3.77003198860231));
#221842=CARTESIAN_POINT('',(26.8427652369017,-30.2864073093061,3.77003198860242));
#221843=CARTESIAN_POINT('',(40.2315646150508,-45.157039930268,3.7700319890254));
#221844=CARTESIAN_POINT('Origin',(5.49031038273072E-15,1.82930781209959E-13,
3.77003198860263));
#221845=CARTESIAN_POINT('',(35.8056376404645,-48.7410849259192,3.77003198882053));
#221846=CARTESIAN_POINT('Origin',(5.49031038273072E-15,1.82930781209959E-13,
3.77003198860263));
#221847=CARTESIAN_POINT('',(35.8051714542882,-48.741427385705,3.77003198860229));
#221848=CARTESIAN_POINT('Origin',(5.49031038273072E-15,1.82930781209959E-13,
3.77003198860263));
#221849=CARTESIAN_POINT('',(35.5264632599797,-48.3578184660146,3.77003198860229));
#221850=CARTESIAN_POINT('Origin',(5.49031038273072E-15,1.82930781209959E-13,
3.77003198860263));
#221851=CARTESIAN_POINT('',(40.3404336838198,-45.2779489569766,3.4882302805845));
#221852=CARTESIAN_POINT('',(40.2315646145633,-45.1570399297209,3.77003198860232));
#221853=CARTESIAN_POINT('',(35.9012693630584,-48.8727133450216,3.48823028074772));
#221854=CARTESIAN_POINT('Origin',(5.52999282761009E-15,1.84898592019556E-13,
3.48823028058481));
#221855=CARTESIAN_POINT('',(35.901269362891,-48.8727133447938,3.48823028058448));
#221856=CARTESIAN_POINT('Origin',(60.71525,1.85785428279622E-13,3.36123028058482));
#221857=CARTESIAN_POINT('',(36.0301015792682,-49.0510171431398,3.36123028058448));
#221858=CARTESIAN_POINT('',(40.4880553924349,-45.4410373245165,3.36123028058451));
#221859=CARTESIAN_POINT('Origin',(5.5478765747851E-15,1.85785428279622E-13,
3.36123028058482));
#221860=CARTESIAN_POINT('',(40.5892333705628,-45.5534068532505,3.3612302805845));
#221861=CARTESIAN_POINT('',(26.948440628206,-30.4037717213981,3.3612302805846));
#221862=CARTESIAN_POINT('',(36.1189794796889,-49.1733470784082,3.36123028058448));
#221863=CARTESIAN_POINT('Origin',(5.5478765747851E-15,1.85785428279622E-13,
3.36123028058482));
#221864=CARTESIAN_POINT('',(36.0304131198717,-49.0514459419939,3.36123028058447));
#221865=CARTESIAN_POINT('Origin',(5.5478765747851E-15,1.85785428279622E-13,
3.36123028058482));
#221866=CARTESIAN_POINT('',(36.2478178023256,-49.3516463037379,3.4882302805845));
#221867=CARTESIAN_POINT('',(40.7368493367122,-45.7165002430342,3.48823028042664));
#221868=CARTESIAN_POINT('Origin',(5.52999282761008E-15,1.84898592019556E-13,
3.48823028058484));
#221869=CARTESIAN_POINT('',(40.8457160731802,-45.8374112534706,3.77003198802676));
#221870=CARTESIAN_POINT('',(40.7368493365303,-45.71650024283,3.48823028058453));
#221871=CARTESIAN_POINT('',(40.8452921850249,-45.8377889771244,3.77003198860232));
#221872=CARTESIAN_POINT('Origin',(5.49031038273072E-15,1.82930781209959E-13,
3.77003198860263));
#221873=CARTESIAN_POINT('',(36.3439095507841,-49.482936761634,3.77003198860229));
#221874=CARTESIAN_POINT('Origin',(5.49031038273072E-15,1.82930781209959E-13,
3.77003198860263));
#221875=CARTESIAN_POINT('',(36.3434519499953,-49.4832728536526,3.77003198802686));
#221876=CARTESIAN_POINT('Origin',(5.49031038273072E-15,1.82930781209959E-13,
3.77003198860263));
#221877=CARTESIAN_POINT('',(36.3434519501796,-49.4832728539295,3.77003198860229));
#221878=CARTESIAN_POINT('Origin',(62.2224557307631,1.82930781209959E-13,
3.77003198860263));
#221879=CARTESIAN_POINT('',(41.1629311642486,-46.1905628026478,3.77003198860231));
#221880=CARTESIAN_POINT('',(27.6232705441551,-31.1532462714323,3.77003198860241));
#221881=CARTESIAN_POINT('',(36.6229335645815,-49.866980369602,3.77003198860229));
#221882=CARTESIAN_POINT('Origin',(5.49031038273072E-15,1.82930781209959E-13,
3.77003198860263));
#221883=CARTESIAN_POINT('',(36.3442183822969,-49.4833618317446,3.77003198860228));
#221884=CARTESIAN_POINT('Origin',(5.57972911860581E-15,1.8736496251029E-13,
3.13503198860263));
#221885=CARTESIAN_POINT('Origin',(39.9143530044124,-44.8038837346033,3.13502491541403));
#221886=CARTESIAN_POINT('Origin',(35.5261507575157,-48.3573798485708,3.13502491541401));
#221887=CARTESIAN_POINT('Origin',(5.57972911860581E-15,1.8736496251029E-13,
3.13503198860263));
#221888=CARTESIAN_POINT('Origin',(41.1884198004194,-46.21892092124,3.20381846780197));
#221889=CARTESIAN_POINT('Origin',(36.6453723646299,-49.8978076723495,3.20382022872569));
#221890=CARTESIAN_POINT('Origin',(5.51210908043506E-15,1.8401175575949E-13,
3.61523028058481));
#221891=CARTESIAN_POINT('Origin',(40.5998732162085,-45.5651681650769,3.58786945046948));
#221892=CARTESIAN_POINT('Origin',(36.1282165298264,-49.186123490054,3.58781461834262));
#221893=CARTESIAN_POINT('Origin',(5.51210908043507E-15,1.8401175575949E-13,
3.61523028058481));
#221894=CARTESIAN_POINT('Origin',(40.47747221295,-45.4293513150133,3.58781440266855));
#221895=CARTESIAN_POINT('Origin',(36.0208162177209,-49.0381593225528,3.58786923592943));
#221896=CARTESIAN_POINT('Origin',(60.4792282238308,1.82930781209959E-13,
3.77003198860263));
#221897=CARTESIAN_POINT('',(30.2768083268887,-51.8059703131941,3.77003198860227));
#221898=CARTESIAN_POINT('',(35.012421476459,-48.7306271754171,3.77003198860229));
#221899=CARTESIAN_POINT('Origin',(5.49031038273072E-15,1.82930781209959E-13,
3.77003198860263));
#221900=CARTESIAN_POINT('',(35.2914456628196,-49.1146710209409,3.77003198860229));
#221901=CARTESIAN_POINT('',(20.6381965522797,-28.9462038689909,3.77003198860243));
#221902=CARTESIAN_POINT('',(35.2909759049639,-49.1150085647348,3.77003198902485));
#221903=CARTESIAN_POINT('Origin',(5.49031038273072E-15,1.82930781209959E-13,
3.77003198860263));
#221904=CARTESIAN_POINT('',(30.5146599057598,-52.2167844417073,3.7700319888205));
#221905=CARTESIAN_POINT('Origin',(5.49031038273072E-15,1.82930781209959E-13,
3.77003198860263));
#221906=CARTESIAN_POINT('',(30.5141604766051,-52.217076295738,3.77003198860226));
#221907=CARTESIAN_POINT('Origin',(5.49031038273072E-15,1.82930781209959E-13,
3.77003198860263));
#221908=CARTESIAN_POINT('',(30.2770771258177,-51.8064358865961,3.77003198860227));
#221909=CARTESIAN_POINT('Origin',(5.49031038273072E-15,1.82930781209959E-13,
3.77003198860263));
#221910=CARTESIAN_POINT('',(35.3866101428265,-49.2466351556007,3.48823028058447));
#221911=CARTESIAN_POINT('',(35.2909759045368,-49.1150085641405,3.77003198860229));
#221912=CARTESIAN_POINT('',(30.5960088314001,-52.3576880235598,3.48823028074769));
#221913=CARTESIAN_POINT('Origin',(5.52999282761009E-15,1.84898592019556E-13,
3.48823028058481));
#221914=CARTESIAN_POINT('',(30.5960088312575,-52.3576880233157,3.48823028058445));
#221915=CARTESIAN_POINT('Origin',(60.71525,1.85785428279622E-13,3.36123028058482));
#221916=CARTESIAN_POINT('',(30.7054974692375,-52.5484816883954,3.36123028058446));
#221917=CARTESIAN_POINT('',(35.5163757878401,-49.4242607783455,3.36123028058448));
#221918=CARTESIAN_POINT('Origin',(5.5478765747851E-15,1.85785428279622E-13,
3.36123028058482));
#221919=CARTESIAN_POINT('',(35.6052536882608,-49.5465907136139,3.36123028058448));
#221920=CARTESIAN_POINT('',(20.7197400704249,-29.0584388930976,3.36123028058461));
#221921=CARTESIAN_POINT('',(30.781101527075,-52.6794317578282,3.36123028058446));
#221922=CARTESIAN_POINT('Origin',(5.5478765747851E-15,1.85785428279622E-13,
3.36123028058482));
#221923=CARTESIAN_POINT('',(30.7057624815037,-52.5489407031051,3.36123028058445));
#221924=CARTESIAN_POINT('Origin',(5.5478765747851E-15,1.85785428279622E-13,
3.36123028058482));
#221925=CARTESIAN_POINT('',(30.8905967158742,-52.870221513221,3.48823028058447));
#221926=CARTESIAN_POINT('',(35.7350130972991,-49.724220730839,3.48823028042661));
#221927=CARTESIAN_POINT('Origin',(5.52999282761008E-15,1.84898592019556E-13,
3.48823028058484));
#221928=CARTESIAN_POINT('',(35.8306448082808,-49.855849050773,3.77003198802673));
#221929=CARTESIAN_POINT('',(35.7350130971395,-49.7242207306169,3.4882302805845));
#221930=CARTESIAN_POINT('',(35.8301837593561,-49.8561803968397,3.77003198860229));
#221931=CARTESIAN_POINT('Origin',(5.49031038273072E-15,1.82930781209959E-13,
3.77003198860263));
#221932=CARTESIAN_POINT('',(30.9724384738749,-53.0108370710507,3.77003198860226));
#221933=CARTESIAN_POINT('Origin',(5.49031038273072E-15,1.82930781209959E-13,
3.77003198860263));
#221934=CARTESIAN_POINT('',(30.9719482486888,-53.0111234896148,3.77003198802684));
#221935=CARTESIAN_POINT('Origin',(5.49031038273072E-15,1.82930781209959E-13,
3.77003198860263));
#221936=CARTESIAN_POINT('',(30.9719482488431,-53.0111234899094,3.77003198860226));
#221937=CARTESIAN_POINT('Origin',(62.2224557307631,1.82930781209959E-13,
3.77003198860263));
#221938=CARTESIAN_POINT('',(36.1092077731534,-50.2402240048077,3.77003198860228));
#221939=CARTESIAN_POINT('',(21.2404668433939,-29.7751578089174,3.77003198860242));
#221940=CARTESIAN_POINT('',(31.2097904767612,-53.4219427993281,3.77003198860226));
#221941=CARTESIAN_POINT('Origin',(5.49031038273072E-15,1.82930781209959E-13,
3.77003198860263));
#221942=CARTESIAN_POINT('',(30.9727011816508,-53.0112920942662,3.77003198860226));
#221943=CARTESIAN_POINT('Origin',(5.57972911860581E-15,1.8736496251029E-13,
3.13503198860263));
#221944=CARTESIAN_POINT('Origin',(35.0124168871459,-48.7306293534713,3.13502491541405));
#221945=CARTESIAN_POINT('Origin',(30.2768121832823,-51.8059670065423,3.13502491541396));
#221946=CARTESIAN_POINT('Origin',(5.57972911860581E-15,1.8736496251029E-13,
3.13503198860263));
#221947=CARTESIAN_POINT('Origin',(36.1315925493471,-50.2710910626317,3.20381846780222));
#221948=CARTESIAN_POINT('Origin',(31.228884024128,-53.4549467201719,3.20382022872136));
#221949=CARTESIAN_POINT('Origin',(5.51210908043506E-15,1.8401175575949E-13,
3.61523028058481));
#221950=CARTESIAN_POINT('Origin',(35.6146058558668,-49.5593997624572,3.58786945047169));
#221951=CARTESIAN_POINT('Origin',(30.7889524770101,-52.6931037136105,3.58781461834191));
#221952=CARTESIAN_POINT('Origin',(5.51210908043507E-15,1.8401175575949E-13,
3.61523028058481));
#221953=CARTESIAN_POINT('Origin',(35.5070721047329,-49.4115325425344,3.58781440266241));
#221954=CARTESIAN_POINT('Origin',(30.6976069821031,-52.5347237197183,3.58786923592823));
#221955=CARTESIAN_POINT('Origin',(60.4792282238308,1.82930781209959E-13,
3.77003198860263));
#221956=CARTESIAN_POINT('',(24.6957503380314,-54.6869600343293,3.77003198860225));
#221957=CARTESIAN_POINT('',(29.7268821954856,-52.1234703131941,3.77003198860227));
#221958=CARTESIAN_POINT('Origin',(5.49031038273072E-15,1.82930781209959E-13,
3.77003198860263));
#221959=CARTESIAN_POINT('',(29.9642343451585,-52.5345762957638,3.77003198860226));
#221960=CARTESIAN_POINT('',(14.8448439902567,-26.3470240215573,3.77003198860244));
#221961=CARTESIAN_POINT('',(29.9637318777518,-52.5348628873914,3.77003198902526));
#221962=CARTESIAN_POINT('Origin',(5.49031038273072E-15,1.82930781209959E-13,
3.77003198860263));
#221963=CARTESIAN_POINT('',(24.8893571715245,-55.1203859400875,3.77003198882048));
#221964=CARTESIAN_POINT('Origin',(5.49031038273072E-15,1.82930781209959E-13,
3.77003198860263));
#221965=CARTESIAN_POINT('',(24.8888299712416,-55.1206239907492,3.77003198860224));
#221966=CARTESIAN_POINT('Origin',(5.49031038273072E-15,1.82930781209959E-13,
3.77003198860263));
#221967=CARTESIAN_POINT('',(24.6959689987794,-54.6874511544104,3.77003198860225));
#221968=CARTESIAN_POINT('Origin',(5.49031038273072E-15,1.82930781209959E-13,
3.77003198860263));
#221969=CARTESIAN_POINT('',(30.0450834959843,-52.675764913939,3.48823028058445));
#221970=CARTESIAN_POINT('',(29.9637318773888,-52.534862886755,3.77003198860227));
#221971=CARTESIAN_POINT('',(24.9555320243585,-55.2690209155612,3.48823028074766));
#221972=CARTESIAN_POINT('Origin',(5.52999282761009E-15,1.84898592019556E-13,
3.48823028058481));
#221973=CARTESIAN_POINT('',(24.9555320242422,-55.2690209153036,3.48823028058443));
#221974=CARTESIAN_POINT('Origin',(60.71525,1.85785428279622E-13,3.36123028058482));
#221975=CARTESIAN_POINT('',(25.0444775033954,-55.4702140717962,3.36123028058443));
#221976=CARTESIAN_POINT('',(30.1555713378344,-52.8659816883954,3.36123028058445));
#221977=CARTESIAN_POINT('Origin',(5.5478765747851E-15,1.85785428279622E-13,
3.36123028058482));
#221978=CARTESIAN_POINT('',(30.2311753956719,-52.9969317578282,3.36123028058445));
#221979=CARTESIAN_POINT('',(14.9038494342991,-26.4492244485618,3.36123028058463));
#221980=CARTESIAN_POINT('',(25.1059793847708,-55.6083495590297,3.36123028058443));
#221981=CARTESIAN_POINT('Origin',(5.5478765747851E-15,1.85785428279622E-13,
3.36123028058482));
#221982=CARTESIAN_POINT('',(25.0446930837944,-55.4706982733002,3.36123028058443));
#221983=CARTESIAN_POINT('Origin',(5.5478765747851E-15,1.85785428279622E-13,
3.36123028058482));
#221984=CARTESIAN_POINT('',(25.1949317875307,-55.8095395120002,3.48823028058446));
#221985=CARTESIAN_POINT('',(30.3416565763598,-53.1871522508545,3.48823028042659));
#221986=CARTESIAN_POINT('Origin',(5.52999282761008E-15,1.84898592019556E-13,
3.48823028058484));
#221987=CARTESIAN_POINT('',(30.4230055008174,-53.328055732868,3.7700319880267));
#221988=CARTESIAN_POINT('',(30.3416565762242,-53.187152250617,3.48823028058447));
#221989=CARTESIAN_POINT('',(30.4225123424717,-53.3283370710507,3.77003198860226));
#221990=CARTESIAN_POINT('Origin',(5.49031038273072E-15,1.82930781209959E-13,
3.77003198860263));
#221991=CARTESIAN_POINT('',(25.2616268796463,-55.9579395562862,3.77003198860224));
#221992=CARTESIAN_POINT('Origin',(5.49031038273072E-15,1.82930781209959E-13,
3.77003198860263));
#221993=CARTESIAN_POINT('',(25.2611094010728,-55.9581731633341,3.77003198802682));
#221994=CARTESIAN_POINT('Origin',(5.49031038273072E-15,1.82930781209959E-13,
3.77003198860263));
#221995=CARTESIAN_POINT('',(25.2611094011954,-55.9581731636432,3.77003198860224));
#221996=CARTESIAN_POINT('Origin',(62.2224557307631,1.82930781209959E-13,
3.77003198860263));
#221997=CARTESIAN_POINT('',(30.6598643453581,-53.7394427993281,3.77003198860226));
#221998=CARTESIAN_POINT('',(15.2806508669898,-27.1018636743469,3.77003198860244));
#221999=CARTESIAN_POINT('',(25.454706393409,-56.3916032444846,3.77003198860224));
#222000=CARTESIAN_POINT('Origin',(5.49031038273072E-15,1.82930781209959E-13,
3.77003198860263));
#222001=CARTESIAN_POINT('',(25.2618405854041,-55.958419547277,3.77003198860224));
#222002=CARTESIAN_POINT('Origin',(5.57972911860581E-15,1.8736496251029E-13,
3.13503198860263));
#222003=CARTESIAN_POINT('Origin',(29.7268774036444,-52.1234719996029,3.13502491541398));
#222004=CARTESIAN_POINT('Origin',(24.6957545189385,-54.6869571488945,3.13502491541394));
#222005=CARTESIAN_POINT('Origin',(5.57972911860581E-15,1.8736496251029E-13,
3.13503198860263));
#222006=CARTESIAN_POINT('Origin',(30.6789000092848,-53.7724806104344,3.20381846779911));
#222007=CARTESIAN_POINT('Origin',(25.4702454951989,-56.4264221855612,3.20382022872151));
#222008=CARTESIAN_POINT('Origin',(5.51210908043506E-15,1.8401175575949E-13,
3.61523028058481));
#222009=CARTESIAN_POINT('Origin',(30.2391374209345,-53.0106482050714,3.58786945046866));
#222010=CARTESIAN_POINT('Origin',(25.1123582178529,-55.6227672661395,3.58781461834242));
#222011=CARTESIAN_POINT('Origin',(5.51210908043507E-15,1.8401175575949E-13,
3.61523028058481));
#222012=CARTESIAN_POINT('Origin',(30.1476490842058,-52.852350679495,3.58781440266416));
#222013=CARTESIAN_POINT('Origin',(25.0380683404964,-55.4557066902189,3.58786923593021));
#222014=CARTESIAN_POINT('Origin',(60.4792282238308,1.82930781209959E-13,
3.77003198860263));
#222015=CARTESIAN_POINT('',(18.8441205405526,-56.9687879773462,3.77003198860223));
#222016=CARTESIAN_POINT('',(24.1156489724283,-54.9452378026824,3.77003198860224));
#222017=CARTESIAN_POINT('Origin',(5.49031038273072E-15,1.82930781209959E-13,
3.77003198860263));
#222018=CARTESIAN_POINT('',(24.3087286055926,-55.3789017591234,3.77003198860224));
#222019=CARTESIAN_POINT('',(9.71531210235053,-22.6015516358799,3.77003198860247));
#222020=CARTESIAN_POINT('',(24.3081989337723,-55.3791342586257,3.77003198902492));
#222021=CARTESIAN_POINT('Origin',(5.49031038273072E-15,1.82930781209959E-13,
3.77003198860263));
#222022=CARTESIAN_POINT('',(18.9913614316851,-57.4200769554257,3.77003198882047));
#222023=CARTESIAN_POINT('Origin',(5.49031038273072E-15,1.82930781209959E-13,
3.77003198860263));
#222024=CARTESIAN_POINT('',(18.9908122363906,-57.4202585945856,3.77003198860223));
#222025=CARTESIAN_POINT('Origin',(5.49031038273072E-15,1.82930781209959E-13,
3.77003198860263));
#222026=CARTESIAN_POINT('',(18.8442866674268,-56.9692992632922,3.77003198860223));
#222027=CARTESIAN_POINT('Origin',(5.49031038273072E-15,1.82930781209959E-13,
3.77003198860263));
#222028=CARTESIAN_POINT('',(24.374376627022,-55.5277679687678,3.48823028058442));
#222029=CARTESIAN_POINT('',(24.308198933478,-55.3791342579554,3.77003198860224));
#222030=CARTESIAN_POINT('',(19.0416371861772,-57.5748148486256,3.48823028074764));
#222031=CARTESIAN_POINT('Origin',(5.52999282761009E-15,1.84898592019556E-13,
3.48823028058481));
#222032=CARTESIAN_POINT('',(19.0416371860884,-57.5748148483572,3.48823028058441));
#222033=CARTESIAN_POINT('Origin',(60.71525,1.85785428279622E-13,3.36123028058482));
#222034=CARTESIAN_POINT('',(19.1090650011322,-57.7842031819379,3.36123028058441));
#222035=CARTESIAN_POINT('',(24.4643761377923,-55.7284918401494,3.36123028058443));
#222036=CARTESIAN_POINT('Origin',(5.5478765747851E-15,1.85785428279622E-13,
3.36123028058482));
#222037=CARTESIAN_POINT('',(24.5258780191677,-55.8666273273828,3.36123028058442));
#222038=CARTESIAN_POINT('',(9.75435829333414,-22.68925081671,3.36123028058466));
#222039=CARTESIAN_POINT('',(19.1557908785631,-57.9280106456672,3.36123028058441));
#222040=CARTESIAN_POINT('Origin',(5.5478765747851E-15,1.85785428279622E-13,
3.36123028058482));
#222041=CARTESIAN_POINT('',(19.1092287877201,-57.7847072652232,3.36123028058441));
#222042=CARTESIAN_POINT('Origin',(5.5478765747851E-15,1.85785428279622E-13,
3.36123028058482));
#222043=CARTESIAN_POINT('',(19.2232259141446,-58.137396516989,3.48823028058443));
#222044=CARTESIAN_POINT('',(24.6158705165699,-56.0673542006825,3.48823028042655));
#222045=CARTESIAN_POINT('Origin',(5.52999282761008E-15,1.84898592019556E-13,
3.48823028058484));
#222046=CARTESIAN_POINT('',(24.6820453786638,-56.2159890767406,3.77003198802669));
#222047=CARTESIAN_POINT('',(24.61587051646,-56.0673542004321,3.48823028058445));
#222048=CARTESIAN_POINT('',(24.6815255140433,-56.2162173246393,3.77003198860224));
#222049=CARTESIAN_POINT('Origin',(5.49031038273072E-15,1.82930781209959E-13,
3.77003198860263));
#222050=CARTESIAN_POINT('',(19.2740436149891,-58.2919551457913,3.77003198860222));
#222051=CARTESIAN_POINT('Origin',(5.49031038273072E-15,1.82930781209959E-13,
3.77003198860263));
#222052=CARTESIAN_POINT('',(19.2735045526316,-58.2921333818753,3.7700319880268));
#222053=CARTESIAN_POINT('Origin',(5.49031038273072E-15,1.82930781209959E-13,
3.77003198860263));
#222054=CARTESIAN_POINT('',(19.2735045527213,-58.2921333821955,3.77003198860222));
#222055=CARTESIAN_POINT('Origin',(62.2224557307631,1.82930781209959E-13,
3.77003198860263));
#222056=CARTESIAN_POINT('',(24.8746050278059,-56.6498810128377,3.77003198860224));
#222057=CARTESIAN_POINT('',(10.0037024164492,-23.2492868865832,3.77003198860246));
#222058=CARTESIAN_POINT('',(19.4207352200707,-58.7434254837928,3.77003198860222));
#222059=CARTESIAN_POINT('Origin',(5.49031038273072E-15,1.82930781209959E-13,
3.77003198860263));
#222060=CARTESIAN_POINT('',(19.2742059773237,-58.2924548456757,3.77003198860222));
#222061=CARTESIAN_POINT('Origin',(5.57972911860581E-15,1.8736496251029E-13,
3.13503198860263));
#222062=CARTESIAN_POINT('Origin',(24.1156440305597,-54.9452389789691,3.13502491541393));
#222063=CARTESIAN_POINT('Origin',(18.8441250001663,-56.968785544742,3.1350249154139));
#222064=CARTESIAN_POINT('Origin',(5.57972911860581E-15,1.8736496251029E-13,
3.13503198860263));
#222065=CARTESIAN_POINT('Origin',(24.8900830207518,-56.6847276080569,3.20381846780338));
#222066=CARTESIAN_POINT('Origin',(19.4325496266317,-58.7796779614975,3.20382022872089));
#222067=CARTESIAN_POINT('Origin',(5.51210908043506E-15,1.8401175575949E-13,
3.61523028058481));
#222068=CARTESIAN_POINT('Origin',(24.5323626684716,-55.8811008927591,3.58786945046644));
#222069=CARTESIAN_POINT('Origin',(19.1606277069622,-57.9430161406885,3.58781461834223));
#222070=CARTESIAN_POINT('Origin',(5.51210908043507E-15,1.8401175575949E-13,
3.61523028058481));
#222071=CARTESIAN_POINT('Origin',(24.4579221115133,-55.7141074023456,3.5878144026674));
#222072=CARTESIAN_POINT('Origin',(19.1042073825996,-57.7691053333649,3.5878692359277));
#222073=CARTESIAN_POINT('Origin',(60.4792282238308,1.82930781209959E-13,
3.77003198860263));
#222074=CARTESIAN_POINT('',(12.7860306150458,-58.626453957798,3.77003198860222));
#222075=CARTESIAN_POINT('',(18.2401996527051,-57.1650137687743,3.77003198860223));
#222076=CARTESIAN_POINT('Origin',(5.49031038273072E-15,1.82930781209959E-13,
3.77003198860263));
#222077=CARTESIAN_POINT('',(18.3868913484954,-57.6164843860299,3.77003198860223));
#222078=CARTESIAN_POINT('',(5.47329194811204,-17.8725121057136,3.7700319886025));
#222079=CARTESIAN_POINT('',(18.386340275457,-57.6166602460943,3.770031989025));
#222080=CARTESIAN_POINT('Origin',(5.49031038273072E-15,1.82930781209959E-13,
3.77003198860263));
#222081=CARTESIAN_POINT('',(12.8852923618023,-59.0906615917168,3.77003198882045));
#222082=CARTESIAN_POINT('Origin',(5.49031038273072E-15,1.82930781209959E-13,
3.77003198860263));
#222083=CARTESIAN_POINT('',(12.8847271885949,-59.0907848292981,3.77003198860221));
#222084=CARTESIAN_POINT('Origin',(5.49031038273072E-15,1.82930781209959E-13,
3.77003198860263));
#222085=CARTESIAN_POINT('',(12.7861423879254,-58.626979807853,3.77003198860222));
#222086=CARTESIAN_POINT('Origin',(5.49031038273072E-15,1.82930781209959E-13,
3.77003198860263));
#222087=CARTESIAN_POINT('',(18.4366189870679,-57.7713971777983,3.48823028058441));
#222088=CARTESIAN_POINT('',(18.3863402752344,-57.6166602453967,3.77003198860222));
#222089=CARTESIAN_POINT('',(12.9191181862654,-59.2498070619039,3.48823028074763));
#222090=CARTESIAN_POINT('Origin',(5.52999282761009E-15,1.84898592019556E-13,
3.48823028058481));
#222091=CARTESIAN_POINT('',(12.9191181862052,-59.2498070616276,3.4882302805844));
#222092=CARTESIAN_POINT('Origin',(60.71525,1.85785428279622E-13,3.36123028058482));
#222093=CARTESIAN_POINT('',(12.9642895838877,-59.4650964698963,3.3612302805844));
#222094=CARTESIAN_POINT('',(18.5051441132848,-57.980428973366,3.36123028058441));
#222095=CARTESIAN_POINT('Origin',(5.5478765747851E-15,1.85785428279622E-13,
3.36123028058482));
#222096=CARTESIAN_POINT('',(18.5518699907157,-58.1242364370953,3.36123028058441));
#222097=CARTESIAN_POINT('',(5.49583002221492,-17.9418771653397,3.36123028058469));
#222098=CARTESIAN_POINT('',(12.995727518883,-59.6130003254552,3.3612302805844));
#222099=CARTESIAN_POINT('Origin',(5.5478765747851E-15,1.85785428279622E-13,
3.36123028058482));
#222100=CARTESIAN_POINT('',(12.9643997821844,-59.465614912121,3.3612302805844));
#222101=CARTESIAN_POINT('Origin',(5.5478765747851E-15,1.85785428279622E-13,
3.36123028058482));
#222102=CARTESIAN_POINT('',(13.0409063549245,-59.8282880397052,3.48823028058442));
#222103=CARTESIAN_POINT('',(18.6203878281985,-58.3332704850397,3.48823028042654));
#222104=CARTESIAN_POINT('Origin',(5.52999282761008E-15,1.84898592019556E-13,
3.48823028058484));
#222105=CARTESIAN_POINT('',(18.6706636022915,-58.4880082803365,3.77003198802666));
#222106=CARTESIAN_POINT('',(18.6203878281154,-58.3332704847792,3.48823028058443));
#222107=CARTESIAN_POINT('',(18.6701227271417,-58.4881809372194,3.77003198860222));
#222108=CARTESIAN_POINT('Origin',(5.49031038273072E-15,1.82930781209959E-13,
3.77003198860263));
#222109=CARTESIAN_POINT('',(13.0752898951332,-59.9873118763432,3.77003198860221));
#222110=CARTESIAN_POINT('Origin',(5.49031038273072E-15,1.82930781209959E-13,
3.77003198860263));
#222111=CARTESIAN_POINT('',(13.0747351550717,-59.9874327886715,3.77003198802678));
#222112=CARTESIAN_POINT('Origin',(5.49031038273072E-15,1.82930781209959E-13,
3.77003198860263));
#222113=CARTESIAN_POINT('',(13.0747351551274,-59.9874327889994,3.77003198860221));
#222114=CARTESIAN_POINT('Origin',(62.2224557307631,1.82930781209959E-13,
3.77003198860263));
#222115=CARTESIAN_POINT('',(18.8168143322233,-58.9396512752209,3.77003198860221));
#222116=CARTESIAN_POINT('',(5.63975536249314,-18.3848338156963,3.7700319886025));
#222117=CARTESIAN_POINT('',(13.1739864076113,-60.4516424606486,3.7700319886022));
#222118=CARTESIAN_POINT('Origin',(5.49031038273072E-15,1.82930781209959E-13,
3.77003198860263));
#222119=CARTESIAN_POINT('',(13.075399135169,-59.9878258103048,3.77003198860221));
#222120=CARTESIAN_POINT('Origin',(5.57972911860581E-15,1.8736496251029E-13,
3.13503198860263));
#222121=CARTESIAN_POINT('Origin',(18.2401946149531,-57.1650144220513,3.13502491541393));
#222122=CARTESIAN_POINT('Origin',(12.7860353045056,-58.6264520046765,3.13502491541391));
#222123=CARTESIAN_POINT('Origin',(5.57972911860581E-15,1.8736496251029E-13,
3.13503198860263));
#222124=CARTESIAN_POINT('Origin',(18.828565074056,-58.9759248679618,3.20381846780251));
#222125=CARTESIAN_POINT('Origin',(13.1819466778355,-60.4889312852477,3.20382022871903));
#222126=CARTESIAN_POINT('Origin',(5.51210908043506E-15,1.8401175575949E-13,
3.61523028058481));
#222127=CARTESIAN_POINT('Origin',(18.5568062168847,-58.1393085451904,3.58786945047095));
#222128=CARTESIAN_POINT('Origin',(12.9989693492953,-59.6284292050465,3.58781461833786));
#222129=CARTESIAN_POINT('Origin',(5.51210908043507E-15,1.8401175575949E-13,
3.61523028058481));
#222130=CARTESIAN_POINT('Origin',(18.5002290260152,-57.9654487055678,3.58781440266512));
#222131=CARTESIAN_POINT('Origin',(12.9610367308101,-59.4495735695156,3.58786923592612));
#222132=CARTESIAN_POINT('Origin',(60.4792282238308,1.82930781209959E-13,
3.77003198860263));
#222133=CARTESIAN_POINT('',(6.58785426247156,-59.641796240314,3.77003198860221));
#222134=CARTESIAN_POINT('',(12.1649068885798,-58.7584778814673,3.77003198860222));
#222135=CARTESIAN_POINT('Origin',(5.49031038273072E-15,1.82930781209959E-13,
3.77003198860263));
#222136=CARTESIAN_POINT('',(12.2636034620796,-59.2228087529785,3.77003198860221));
#222137=CARTESIAN_POINT('',(2.30379013587727,-12.3655710936231,3.77003198860254));
#222138=CARTESIAN_POINT('',(12.2630370254948,-59.2229260468454,3.77003198902505));
#222139=CARTESIAN_POINT('Origin',(5.49031038273072E-15,1.82930781209959E-13,
3.77003198860263));
#222140=CARTESIAN_POINT('',(6.63804933238279,-60.113836574093,3.77003198882045));
#222141=CARTESIAN_POINT('Origin',(5.49031038273072E-15,1.82930781209959E-13,
3.77003198860263));
#222142=CARTESIAN_POINT('',(6.63747437341838,-60.1139000598791,3.77003198860221));
#222143=CARTESIAN_POINT('Origin',(5.49031038273072E-15,1.82930781209959E-13,
3.77003198860263));
#222144=CARTESIAN_POINT('',(6.58791045674951,-59.6423308931547,3.77003198860221));
#222145=CARTESIAN_POINT('Origin',(5.49031038273072E-15,1.82930781209959E-13,
3.77003198860263));
#222146=CARTESIAN_POINT('',(12.296865891381,-59.3820708699068,3.4882302805844));
#222147=CARTESIAN_POINT('',(12.2630370253463,-59.2229260461282,3.77003198860221));
#222148=CARTESIAN_POINT('',(6.65505462400559,-60.2756459901927,3.48823028074762));
#222149=CARTESIAN_POINT('Origin',(5.52999282761009E-15,1.84898592019556E-13,
3.48823028058481));
#222150=CARTESIAN_POINT('',(6.65505462397456,-60.2756459899116,3.48823028058439));
#222151=CARTESIAN_POINT('Origin',(60.71525,1.85785428279622E-13,3.36123028058482));
#222152=CARTESIAN_POINT('',(6.67747469701007,-60.4944777170591,3.36123028058439));
#222153=CARTESIAN_POINT('',(12.3431658574217,-59.5971203935656,3.3612302805844));
#222154=CARTESIAN_POINT('Origin',(5.5478765747851E-15,1.85785428279622E-13,
3.36123028058482));
#222155=CARTESIAN_POINT('',(12.3746037924171,-59.7450242491244,3.3612302805844));
#222156=CARTESIAN_POINT('',(2.31399271319981,-12.4135704460891,3.36123028058473));
#222157=CARTESIAN_POINT('',(6.69328024897516,-60.6448574988552,3.36123028058439));
#222158=CARTESIAN_POINT('Origin',(5.5478765747851E-15,1.85785428279622E-13,
3.36123028058482));
#222159=CARTESIAN_POINT('',(6.67753009965994,-60.4950048380617,3.36123028058439));
#222160=CARTESIAN_POINT('Origin',(5.5478765747851E-15,1.85785428279622E-13,
3.36123028058482));
#222161=CARTESIAN_POINT('',(6.71570789669471,-60.8636883187842,3.48823028058441));
#222162=CARTESIAN_POINT('',(12.4208962742148,-59.9600752509412,3.48823028042653));
#222163=CARTESIAN_POINT('Origin',(5.52999282761008E-15,1.84898592019556E-13,
3.48823028058484));
#222164=CARTESIAN_POINT('',(12.454722128405,-60.1192206258103,3.77003198802665));
#222165=CARTESIAN_POINT('',(12.4208962741593,-59.9600752506734,3.48823028058442));
#222166=CARTESIAN_POINT('',(12.4541661686672,-60.1193358000125,3.77003198860221));
#222167=CARTESIAN_POINT('Origin',(5.49031038273072E-15,1.82930781209959E-13,
3.77003198860263));
#222168=CARTESIAN_POINT('',(6.7332805630058,-61.025435064826,3.7700319886022));
#222169=CARTESIAN_POINT('Origin',(5.49031038273072E-15,1.82930781209959E-13,
3.77003198860263));
#222170=CARTESIAN_POINT('',(6.73271622308859,-61.0254973286577,3.77003198802678));
#222171=CARTESIAN_POINT('Origin',(5.49031038273072E-15,1.82930781209959E-13,
3.77003198860263));
#222172=CARTESIAN_POINT('',(6.7327162231097,-61.0254973289896,3.7700319886022));
#222173=CARTESIAN_POINT('Origin',(62.2224557307631,1.82930781209959E-13,
3.77003198860263));
#222174=CARTESIAN_POINT('',(12.5528626811454,-60.5836663843179,3.7700319886022));
#222175=CARTESIAN_POINT('',(2.3791451040456,-12.7200883457667,3.77003198860254));
#222176=CARTESIAN_POINT('',(6.78290064323623,-61.497538592386,3.7700319886022));
#222177=CARTESIAN_POINT('Origin',(5.49031038273072E-15,1.82930781209959E-13,
3.77003198860263));
#222178=CARTESIAN_POINT('',(6.73333548388602,-61.0259576020966,3.7700319886022));
#222179=CARTESIAN_POINT('Origin',(5.57972911860581E-15,1.8736496251029E-13,
3.13503198860263));
#222180=CARTESIAN_POINT('Origin',(12.1649018101392,-58.7584780045771,3.13502491541395));
#222181=CARTESIAN_POINT('Origin',(6.58785913039885,-59.6417947880739,3.1350249154139));
#222182=CARTESIAN_POINT('Origin',(5.57972911860581E-15,1.8736496251029E-13,
3.13503198860263));
#222183=CARTESIAN_POINT('Origin',(12.5607574282794,-60.6209695535071,3.20381846780018));
#222184=CARTESIAN_POINT('Origin',(6.78691956273308,-61.5354552197178,3.20382022872141));
#222185=CARTESIAN_POINT('Origin',(5.51210908043506E-15,1.8401175575949E-13,
3.61523028058481));
#222186=CARTESIAN_POINT('Origin',(12.3779375131254,-59.760529766771,3.5878694504689));
#222187=CARTESIAN_POINT('Origin',(6.69489156322728,-60.6605407209774,3.58781461834439));
#222188=CARTESIAN_POINT('Origin',(5.51210908043507E-15,1.8401175575949E-13,
3.61523028058481));
#222189=CARTESIAN_POINT('Origin',(12.3398435598856,-59.5817084227214,3.58781440266202));
#222190=CARTESIAN_POINT('Origin',(6.67586224832421,-60.4786998370195,3.58786923592969));
#222191=CARTESIAN_POINT('Origin',(60.4792282238308,1.82930781209959E-13,
3.77003198860263));
#222192=CARTESIAN_POINT('',(0.317500000000634,-60.0036905223729,3.77003198860221));
#222193=CARTESIAN_POINT('',(5.95633285891271,-59.708171814489,3.77003198860221));
#222194=CARTESIAN_POINT('Origin',(5.49031038273072E-15,1.82930781209959E-13,
3.77003198860263));
#222195=CARTESIAN_POINT('',(6.00595296980932,-60.18027563406,3.77003198860221));
#222196=CARTESIAN_POINT('',(0.34504741944992,-6.32035708677281,3.77003198860258));
#222197=CARTESIAN_POINT('',(6.00537737567573,-60.1803330766331,3.77003198902507));
#222198=CARTESIAN_POINT('Origin',(5.49031038273072E-15,1.82930781209959E-13,
3.77003198860263));
#222199=CARTESIAN_POINT('',(0.31807844537663,-60.4783917833344,3.77003198882044));
#222200=CARTESIAN_POINT('Origin',(5.49031038273072E-15,1.82930781209959E-13,
3.77003198860263));
#222201=CARTESIAN_POINT('',(0.317500000025924,-60.4783948217618,3.7700319886022));
#222202=CARTESIAN_POINT('Origin',(5.49031038273072E-15,1.82930781209959E-13,
3.77003198860263));
#222203=CARTESIAN_POINT('',(0.317500000000634,-60.0042281202308,3.77003198860221));
#222204=CARTESIAN_POINT('Origin',(5.49031038273072E-15,1.82930781209959E-13,
3.77003198860263));
#222205=CARTESIAN_POINT('',(6.02238575970337,-60.3421421670673,3.48823028058439));
#222206=CARTESIAN_POINT('',(6.00537737560301,-60.1803330759043,3.77003198860221));
#222207=CARTESIAN_POINT('',(0.318076890625489,-60.6410923275231,3.48823028074762));
#222208=CARTESIAN_POINT('Origin',(5.52999282761009E-15,1.84898592019556E-13,
3.48823028058481));
#222209=CARTESIAN_POINT('',(0.318076890624007,-60.6410923272403,3.48823028058439));
#222210=CARTESIAN_POINT('Origin',(60.71525,1.85785428279622E-13,3.36123028058482));
#222211=CARTESIAN_POINT('',(0.317500000000643,-60.8610688070705,3.36123028058439));
#222212=CARTESIAN_POINT('',(6.04595329345123,-60.5608532912341,3.36123028058439));
#222213=CARTESIAN_POINT('Origin',(5.5478765747851E-15,1.85785428279622E-13,
3.36123028058482));
#222214=CARTESIAN_POINT('',(6.06175884541631,-60.7112330730301,3.36123028058439));
#222215=CARTESIAN_POINT('',(0.347626240494121,-6.34489293004938,3.36123028058477));
#222216=CARTESIAN_POINT('',(0.317500000000645,-61.0122769227454,3.36123028058439));
#222217=CARTESIAN_POINT('Origin',(5.5478765747851E-15,1.85785428279622E-13,
3.36123028058482));
#222218=CARTESIAN_POINT('',(0.317500000000643,-60.8615988316029,3.36123028058439));
#222219=CARTESIAN_POINT('Origin',(5.5478765747851E-15,1.85785428279622E-13,
3.36123028058482));
#222220=CARTESIAN_POINT('',(0.316930737396561,-61.2322532920971,3.48823028058441));
#222221=CARTESIAN_POINT('',(6.08531878141099,-60.9299448849409,3.48823028042652));
#222222=CARTESIAN_POINT('Origin',(5.52999282761008E-15,1.84898592019556E-13,
3.48823028058484));
#222223=CARTESIAN_POINT('',(6.10232411256149,-61.0917542093521,3.77003198802665));
#222224=CARTESIAN_POINT('',(6.08531878138382,-60.9299448846688,3.48823028058441));
#222225=CARTESIAN_POINT('',(6.10175915944695,-61.0918106390009,3.7700319886022));
#222226=CARTESIAN_POINT('Origin',(5.49031038273072E-15,1.82930781209959E-13,
3.77003198860263));
#222227=CARTESIAN_POINT('',(0.317500000000649,-61.3949508163452,3.7700319886022));
#222228=CARTESIAN_POINT('Origin',(5.49031038273072E-15,1.82930781209959E-13,
3.77003198860263));
#222229=CARTESIAN_POINT('',(0.316932243253905,-61.3949537495048,3.77003198802678));
#222230=CARTESIAN_POINT('Origin',(5.49031038273072E-15,1.82930781209959E-13,
3.77003198860263));
#222231=CARTESIAN_POINT('',(0.316932243240209,-61.3949537498371,3.7700319886022));
#222232=CARTESIAN_POINT('Origin',(62.2224557307631,1.82930781209959E-13,
3.77003198860263));
#222233=CARTESIAN_POINT('',(6.15137923967738,-61.5639141665609,3.7700319886022));
#222234=CARTESIAN_POINT('',(0.364094271196581,-6.50157577599598,3.77003198860258));
#222235=CARTESIAN_POINT('',(0.317500000000654,-61.8696548221179,3.77003198860219));
#222236=CARTESIAN_POINT('Origin',(5.49031038273072E-15,1.82930781209959E-13,
3.77003198860263));
#222237=CARTESIAN_POINT('',(0.317500000000649,-61.3954762318971,3.7700319886022));
#222238=CARTESIAN_POINT('Origin',(5.57972911860581E-15,1.8736496251029E-13,
3.13503198860263));
#222239=CARTESIAN_POINT('Origin',(5.95632779542376,-59.7081714060827,3.13502491541391));
#222240=CARTESIAN_POINT('Origin',(0.317504993061173,-60.0036895869252,3.13502491541391));
#222241=CARTESIAN_POINT('Origin',(5.57972911860581E-15,1.8736496251029E-13,
3.13503198860263));
#222242=CARTESIAN_POINT('Origin',(6.15533149560982,-61.601838210872,3.20381846780011));
#222243=CARTESIAN_POINT('Origin',(0.317533536649249,-61.907783829675,3.20382022871824));
#222244=CARTESIAN_POINT('Origin',(5.51210908043506E-15,1.8401175575949E-13,
3.61523028058481));
#222245=CARTESIAN_POINT('Origin',(6.06345353572214,-60.727002118532,3.58786945046753));
#222246=CARTESIAN_POINT('Origin',(0.317463144197163,-61.0280426587402,3.58781461834126));
#222247=CARTESIAN_POINT('Origin',(5.51210908043507E-15,1.8401175575949E-13,
3.61523028058481));
#222248=CARTESIAN_POINT('Origin',(6.04426018543824,-60.5451784741221,3.58781440266149));
#222249=CARTESIAN_POINT('Origin',(0.317545622031384,-60.8452088131247,3.5878692359282));
#222250=CARTESIAN_POINT('Origin',(60.4792282238308,1.82930781209959E-13,
3.77003198860263));
#222251=CARTESIAN_POINT('',(-5.9563328589115,-59.7081718144891,3.77003198860221));
#222252=CARTESIAN_POINT('',(-0.317499999999366,-60.0036905223729,3.77003198860221));
#222253=CARTESIAN_POINT('Origin',(5.49031038273072E-15,1.82930781209959E-13,
3.77003198860263));
#222254=CARTESIAN_POINT('',(-0.317500000024619,-60.4783948217624,3.7700319886022));
#222255=CARTESIAN_POINT('',(-0.317499999999991,-4.53881144958709E-13,3.77003198860263));
#222256=CARTESIAN_POINT('',(-0.318078445377219,-60.4783917836887,3.77003198902499));
#222257=CARTESIAN_POINT('Origin',(5.49031038273072E-15,1.82930781209959E-13,
3.77003198860263));
#222258=CARTESIAN_POINT('',(-6.00537737563932,-60.1803330762805,3.77003198882045));
#222259=CARTESIAN_POINT('Origin',(5.49031038273072E-15,1.82930781209959E-13,
3.77003198860263));
#222260=CARTESIAN_POINT('',(-6.00595296980802,-60.1802756340595,3.77003198860221));
#222261=CARTESIAN_POINT('Origin',(5.49031038273072E-15,1.82930781209959E-13,
3.77003198860263));
#222262=CARTESIAN_POINT('',(-5.95638905318945,-59.7087064673298,3.77003198860221));
#222263=CARTESIAN_POINT('Origin',(5.49031038273072E-15,1.82930781209959E-13,
3.77003198860263));
#222264=CARTESIAN_POINT('',(-0.318076890622726,-60.6410923272404,3.48823028058439));
#222265=CARTESIAN_POINT('',(-0.318078445373366,-60.4783917829565,3.7700319886022));
#222266=CARTESIAN_POINT('',(-6.02238575973022,-60.3421421673487,3.48823028074762));
#222267=CARTESIAN_POINT('Origin',(5.52999282761009E-15,1.84898592019556E-13,
3.48823028058481));
#222268=CARTESIAN_POINT('',(-6.02238575970214,-60.3421421670674,3.48823028058439));
#222269=CARTESIAN_POINT('Origin',(60.71525,1.85785428279622E-13,3.36123028058482));
#222270=CARTESIAN_POINT('',(-6.04595329344999,-60.5608532912342,3.36123028058439));
#222271=CARTESIAN_POINT('',(-0.317499999999354,-60.8610688070705,3.36123028058439));
#222272=CARTESIAN_POINT('Origin',(5.5478765747851E-15,1.85785428279622E-13,
3.36123028058482));
#222273=CARTESIAN_POINT('',(-0.317499999999355,-61.0122769227454,3.36123028058439));
#222274=CARTESIAN_POINT('',(-0.317499999999991,-4.53498694770213E-13,3.36123028058482));
#222275=CARTESIAN_POINT('',(-6.06175884541508,-60.7112330730303,3.36123028058439));
#222276=CARTESIAN_POINT('Origin',(5.5478765747851E-15,1.85785428279622E-13,
3.36123028058482));
#222277=CARTESIAN_POINT('',(-6.04600869609986,-60.5613804122368,3.36123028058439));
#222278=CARTESIAN_POINT('Origin',(5.5478765747851E-15,1.85785428279622E-13,
3.36123028058482));
#222279=CARTESIAN_POINT('',(-6.08531878138258,-60.9299448846689,3.48823028058441));
#222280=CARTESIAN_POINT('',(-0.316930737396683,-61.2322532923705,3.48823028042652));
#222281=CARTESIAN_POINT('Origin',(5.52999282761008E-15,1.84898592019556E-13,
3.48823028058484));
#222282=CARTESIAN_POINT('',(-0.316932243252611,-61.3949537495047,3.77003198802664));
#222283=CARTESIAN_POINT('',(-0.316930737395267,-61.2322532920971,3.48823028058441));
#222284=CARTESIAN_POINT('',(-0.317499999999355,-61.3949508163452,3.7700319886022));
#222285=CARTESIAN_POINT('Origin',(5.49031038273072E-15,1.82930781209959E-13,
3.77003198860263));
#222286=CARTESIAN_POINT('',(-6.10175915944571,-61.0918106390011,3.7700319886022));
#222287=CARTESIAN_POINT('Origin',(5.49031038273072E-15,1.82930781209959E-13,
3.77003198860263));
#222288=CARTESIAN_POINT('',(-6.10232411256026,-61.0917542093523,3.77003198802677));
#222289=CARTESIAN_POINT('Origin',(5.49031038273072E-15,1.82930781209959E-13,
3.77003198860263));
#222290=CARTESIAN_POINT('',(-6.10232411260861,-61.0917542096813,3.7700319886022));
#222291=CARTESIAN_POINT('Origin',(62.2224557307631,1.82930781209959E-13,
3.77003198860263));
#222292=CARTESIAN_POINT('',(-0.317499999999346,-61.8696548221179,3.77003198860219));
#222293=CARTESIAN_POINT('',(-0.317499999999998,-4.72140483888146E-13,3.77003198860263));
#222294=CARTESIAN_POINT('',(-6.15137923967613,-61.5639141665611,3.7700319886022));
#222295=CARTESIAN_POINT('Origin',(5.49031038273072E-15,1.82930781209959E-13,
3.77003198860263));
#222296=CARTESIAN_POINT('',(-6.10181408032593,-61.0923331762716,3.7700319886022));
#222297=CARTESIAN_POINT('Origin',(5.57972911860581E-15,1.8736496251029E-13,
3.13503198860263));
#222298=CARTESIAN_POINT('Origin',(-0.317504993060079,-60.0036895869252,
3.13502491541387));
#222299=CARTESIAN_POINT('Origin',(-5.9563277954224,-59.7081714060829,3.13502491541391));
#222300=CARTESIAN_POINT('Origin',(5.57972911860581E-15,1.8736496251029E-13,
3.13503198860263));
#222301=CARTESIAN_POINT('Origin',(-0.317533537010846,-61.9077842377865,
3.20381846780275));
#222302=CARTESIAN_POINT('Origin',(-6.15533145331086,-61.6018378049613,3.20382022872096));
#222303=CARTESIAN_POINT('Origin',(5.51210908043506E-15,1.8401175575949E-13,
3.61523028058481));
#222304=CARTESIAN_POINT('Origin',(-0.31746290747785,-61.0281367271388,3.58786945046874));
#222305=CARTESIAN_POINT('Origin',(-6.06344346747435,-60.7269085901922,3.58781461834308));
#222306=CARTESIAN_POINT('Origin',(5.51210908043507E-15,1.8401175575949E-13,
3.61523028058481));
#222307=CARTESIAN_POINT('Origin',(-0.317545368444823,-60.8453028802683,
3.58781440266191));
#222308=CARTESIAN_POINT('Origin',(-6.0442501005473,-60.5450849487949,3.58786923592771));
#222309=CARTESIAN_POINT('Origin',(60.4792282238308,1.82930781209959E-13,
3.77003198860263));
#222310=CARTESIAN_POINT('',(-12.1649068885786,-58.7584778814676,3.77003198860222));
#222311=CARTESIAN_POINT('',(-6.58785426247035,-59.6417962403142,3.77003198860221));
#222312=CARTESIAN_POINT('Origin',(5.49031038273072E-15,1.82930781209959E-13,
3.77003198860263));
#222313=CARTESIAN_POINT('',(-6.63747437341721,-60.1139000598799,3.77003198860221));
#222314=CARTESIAN_POINT('',(0.345047419449671,6.32035708677198,3.77003198860267));
#222315=CARTESIAN_POINT('',(-6.63804933242046,-60.1138365744453,3.77003198902501));
#222316=CARTESIAN_POINT('Origin',(5.49031038273072E-15,1.82930781209959E-13,
3.77003198860263));
#222317=CARTESIAN_POINT('',(-12.2630370254217,-59.2229260464986,3.77003198882045));
#222318=CARTESIAN_POINT('Origin',(5.49031038273072E-15,1.82930781209959E-13,
3.77003198860263));
#222319=CARTESIAN_POINT('',(-12.2636034620782,-59.2228087529782,3.77003198860221));
#222320=CARTESIAN_POINT('Origin',(5.49031038273072E-15,1.82930781209959E-13,
3.77003198860263));
#222321=CARTESIAN_POINT('',(-12.1650186614582,-58.7590037315225,3.77003198860222));
#222322=CARTESIAN_POINT('Origin',(5.49031038273072E-15,1.82930781209959E-13,
3.77003198860263));
#222323=CARTESIAN_POINT('',(-6.65505462397334,-60.2756459899118,3.48823028058439));
#222324=CARTESIAN_POINT('',(-6.63804933234009,-60.1138365737174,3.77003198860221));
#222325=CARTESIAN_POINT('',(-12.296865891437,-59.3820708701839,3.48823028074763));
#222326=CARTESIAN_POINT('Origin',(5.52999282761009E-15,1.84898592019556E-13,
3.48823028058481));
#222327=CARTESIAN_POINT('',(-12.2968658913797,-59.382070869907,3.4882302805844));
#222328=CARTESIAN_POINT('Origin',(60.71525,1.85785428279622E-13,3.36123028058482));
#222329=CARTESIAN_POINT('',(-12.3431658574205,-59.5971203935659,3.3612302805844));
#222330=CARTESIAN_POINT('',(-6.67747469700884,-60.4944777170593,3.36123028058439));
#222331=CARTESIAN_POINT('Origin',(5.5478765747851E-15,1.85785428279622E-13,
3.36123028058482));
#222332=CARTESIAN_POINT('',(-6.69328024897394,-60.6448574988553,3.36123028058439));
#222333=CARTESIAN_POINT('',(0.347626240493851,6.34489293004856,3.36123028058486));
#222334=CARTESIAN_POINT('',(-12.3746037924158,-59.7450242491247,3.3612302805844));
#222335=CARTESIAN_POINT('Origin',(5.5478765747851E-15,1.85785428279622E-13,
3.36123028058482));
#222336=CARTESIAN_POINT('',(-12.3432760557172,-59.5976388357906,3.3612302805844));
#222337=CARTESIAN_POINT('Origin',(5.5478765747851E-15,1.85785428279622E-13,
3.36123028058482));
#222338=CARTESIAN_POINT('',(-12.420896274158,-59.9600752506736,3.48823028058442));
#222339=CARTESIAN_POINT('',(-6.71570789672347,-60.8636883190562,3.48823028042652));
#222340=CARTESIAN_POINT('Origin',(5.52999282761008E-15,1.84898592019556E-13,
3.48823028058484));
#222341=CARTESIAN_POINT('',(-6.73271622308735,-61.0254973286578,3.77003198802665));
#222342=CARTESIAN_POINT('',(-6.71570789669348,-60.8636883187843,3.48823028058441));
#222343=CARTESIAN_POINT('',(-6.73328056300457,-61.0254350648261,3.7700319886022));
#222344=CARTESIAN_POINT('Origin',(5.49031038273072E-15,1.82930781209959E-13,
3.77003198860263));
#222345=CARTESIAN_POINT('',(-12.4541661686659,-60.1193358000128,3.77003198860221));
#222346=CARTESIAN_POINT('Origin',(5.49031038273072E-15,1.82930781209959E-13,
3.77003198860263));
#222347=CARTESIAN_POINT('',(-12.4547221284037,-60.1192206258107,3.77003198802678));
#222348=CARTESIAN_POINT('Origin',(5.49031038273072E-15,1.82930781209959E-13,
3.77003198860263));
#222349=CARTESIAN_POINT('',(-12.4547221284862,-60.1192206261329,3.77003198860221));
#222350=CARTESIAN_POINT('Origin',(62.2224557307631,1.82930781209959E-13,
3.77003198860263));
#222351=CARTESIAN_POINT('',(-6.78290064323498,-61.4975385923861,3.7700319886022));
#222352=CARTESIAN_POINT('',(0.364094271196325,6.50157577599512,3.77003198860267));
#222353=CARTESIAN_POINT('',(-12.5528626811441,-60.5836663843181,3.7700319886022));
#222354=CARTESIAN_POINT('Origin',(5.49031038273072E-15,1.82930781209959E-13,
3.77003198860263));
#222355=CARTESIAN_POINT('',(-12.4542754087017,-60.1198497339743,3.7700319886022));
#222356=CARTESIAN_POINT('Origin',(5.57972911860581E-15,1.8736496251029E-13,
3.13503198860263));
#222357=CARTESIAN_POINT('Origin',(-6.58785913039748,-59.641794788074,3.13502491541394));
#222358=CARTESIAN_POINT('Origin',(-12.1649018101377,-58.7584780045774,3.1350249154139));
#222359=CARTESIAN_POINT('Origin',(5.57972911860581E-15,1.8736496251029E-13,
3.13503198860263));
#222360=CARTESIAN_POINT('Origin',(-6.78691960575311,-61.535455625553,3.20381846780075));
#222361=CARTESIAN_POINT('Origin',(-12.5607573437809,-60.6209691542415,3.2038202287205));
#222362=CARTESIAN_POINT('Origin',(5.51210908043506E-15,1.8401175575949E-13,
3.61523028058481));
#222363=CARTESIAN_POINT('Origin',(-6.69490116062999,-60.660634298804,3.58786945047091));
#222364=CARTESIAN_POINT('Origin',(-12.3779177236593,-59.7604378032097,3.58781461834093));
#222365=CARTESIAN_POINT('Origin',(5.51210908043507E-15,1.8401175575949E-13,
3.61523028058481));
#222366=CARTESIAN_POINT('Origin',(-6.67587182882074,-60.478793415361,3.58781440266411));
#222367=CARTESIAN_POINT('Origin',(-12.3398237541835,-59.5816164638921,3.58786923592573));
#222368=CARTESIAN_POINT('Origin',(60.4792282238308,1.82930781209959E-13,
3.77003198860263));
#222369=CARTESIAN_POINT('',(-18.240199652704,-57.1650137687747,3.77003198860223));
#222370=CARTESIAN_POINT('',(-12.7860306150445,-58.6264539577983,3.77003198860222));
#222371=CARTESIAN_POINT('Origin',(5.49031038273072E-15,1.82930781209959E-13,
3.77003198860263));
#222372=CARTESIAN_POINT('',(-12.8847271885938,-59.090784829299,3.77003198860221));
#222373=CARTESIAN_POINT('',(2.30379013587678,12.3655710936223,3.77003198860271));
#222374=CARTESIAN_POINT('',(-12.8852923618765,-59.090661592063,3.77003198902489));
#222375=CARTESIAN_POINT('Origin',(5.49031038273072E-15,1.82930781209959E-13,
3.77003198860263));
#222376=CARTESIAN_POINT('',(-18.3863402753482,-57.6166602457572,3.77003198882046));
#222377=CARTESIAN_POINT('Origin',(5.49031038273072E-15,1.82930781209959E-13,
3.77003198860263));
#222378=CARTESIAN_POINT('',(-18.386891348494,-57.6164843860297,3.77003198860222));
#222379=CARTESIAN_POINT('Origin',(5.49031038273072E-15,1.82930781209959E-13,
3.77003198860263));
#222380=CARTESIAN_POINT('',(-18.2403657795782,-57.1655250547206,3.77003198860222));
#222381=CARTESIAN_POINT('Origin',(5.49031038273072E-15,1.82930781209959E-13,
3.77003198860263));
#222382=CARTESIAN_POINT('',(-12.9191181862039,-59.2498070616279,3.4882302805844));
#222383=CARTESIAN_POINT('',(-12.8852923617205,-59.0906615913477,3.77003198860221));
#222384=CARTESIAN_POINT('',(-18.4366189871527,-57.771397178068,3.48823028074764));
#222385=CARTESIAN_POINT('Origin',(5.52999282761009E-15,1.84898592019556E-13,
3.48823028058481));
#222386=CARTESIAN_POINT('',(-18.4366189870667,-57.7713971777987,3.48823028058441));
#222387=CARTESIAN_POINT('Origin',(60.71525,1.85785428279622E-13,3.36123028058482));
#222388=CARTESIAN_POINT('',(-18.5051441132836,-57.9804289733664,3.36123028058441));
#222389=CARTESIAN_POINT('',(-12.9642895838864,-59.4650964698966,3.3612302805844));
#222390=CARTESIAN_POINT('Origin',(5.5478765747851E-15,1.85785428279622E-13,
3.36123028058482));
#222391=CARTESIAN_POINT('',(-12.9957275188818,-59.6130003254554,3.3612302805844));
#222392=CARTESIAN_POINT('',(2.31399271319931,12.4135704460882,3.3612302805849));
#222393=CARTESIAN_POINT('',(-18.5518699907145,-58.1242364370956,3.36123028058441));
#222394=CARTESIAN_POINT('Origin',(5.5478765747851E-15,1.85785428279622E-13,
3.36123028058482));
#222395=CARTESIAN_POINT('',(-18.5053078998715,-57.9809330566517,3.3612302805844));
#222396=CARTESIAN_POINT('Origin',(5.5478765747851E-15,1.85785428279622E-13,
3.36123028058482));
#222397=CARTESIAN_POINT('',(-18.6203878281142,-58.3332704847796,3.48823028058443));
#222398=CARTESIAN_POINT('',(-13.0409063549815,-59.8282880399726,3.48823028042653));
#222399=CARTESIAN_POINT('Origin',(5.52999282761008E-15,1.84898592019556E-13,
3.48823028058484));
#222400=CARTESIAN_POINT('',(-13.0747351550704,-59.9874327886717,3.77003198802665));
#222401=CARTESIAN_POINT('',(-13.0409063549232,-59.8282880397054,3.48823028058442));
#222402=CARTESIAN_POINT('',(-13.0752898951319,-59.9873118763435,3.77003198860221));
#222403=CARTESIAN_POINT('Origin',(5.49031038273072E-15,1.82930781209959E-13,
3.77003198860263));
#222404=CARTESIAN_POINT('',(-18.6701227271405,-58.4881809372197,3.77003198860222));
#222405=CARTESIAN_POINT('Origin',(5.49031038273072E-15,1.82930781209959E-13,
3.77003198860263));
#222406=CARTESIAN_POINT('',(-18.6706636022903,-58.4880082803369,3.77003198802679));
#222407=CARTESIAN_POINT('Origin',(5.49031038273072E-15,1.82930781209959E-13,
3.77003198860263));
#222408=CARTESIAN_POINT('',(-18.670663602406,-58.4880082806487,3.77003198860222));
#222409=CARTESIAN_POINT('Origin',(62.2224557307631,1.82930781209959E-13,
3.77003198860263));
#222410=CARTESIAN_POINT('',(-13.1739864076101,-60.4516424606488,3.7700319886022));
#222411=CARTESIAN_POINT('',(2.3791451040451,12.7200883457658,3.77003198860271));
#222412=CARTESIAN_POINT('',(-18.8168143322221,-58.9396512752213,3.77003198860221));
#222413=CARTESIAN_POINT('Origin',(5.49031038273072E-15,1.82930781209959E-13,
3.77003198860263));
#222414=CARTESIAN_POINT('',(-18.6702850894751,-58.4886806371042,3.77003198860221));
#222415=CARTESIAN_POINT('Origin',(5.57972911860581E-15,1.8736496251029E-13,
3.13503198860263));
#222416=CARTESIAN_POINT('Origin',(-12.7860353045042,-58.6264520046768,3.13502491541392));
#222417=CARTESIAN_POINT('Origin',(-18.2401946149518,-57.1650144220517,3.13502491541393));
#222418=CARTESIAN_POINT('Origin',(5.57972911860581E-15,1.8736496251029E-13,
3.13503198860263));
#222419=CARTESIAN_POINT('Origin',(-13.1819467630409,-60.4889316843646,3.20381846780152));
#222420=CARTESIAN_POINT('Origin',(-18.8285649482867,-58.9759244797155,3.20382022872249));
#222421=CARTESIAN_POINT('Origin',(5.51210908043506E-15,1.8401175575949E-13,
3.61523028058481));
#222422=CARTESIAN_POINT('Origin',(-12.9989886756684,-59.6285212670402,3.58786945046826));
#222423=CARTESIAN_POINT('Origin',(-18.556776923018,-58.1392191539787,3.58781461834011));
#222424=CARTESIAN_POINT('Origin',(5.51210908043507E-15,1.8401175575949E-13,
3.61523028058481));
#222425=CARTESIAN_POINT('Origin',(-12.9610560404233,-59.4496656337922,3.58781440266299));
#222426=CARTESIAN_POINT('Origin',(-18.5001997164934,-57.965359320759,3.58786923592875));
#222427=CARTESIAN_POINT('Origin',(60.4792282238308,1.82930781209959E-13,
3.77003198860263));
#222428=CARTESIAN_POINT('',(-24.1156489724272,-54.9452378026829,3.77003198860224));
#222429=CARTESIAN_POINT('',(-18.8441205405514,-56.9687879773466,3.77003198860223));
#222430=CARTESIAN_POINT('Origin',(5.49031038273072E-15,1.82930781209959E-13,
3.77003198860263));
#222431=CARTESIAN_POINT('',(-18.9908122363897,-57.4202585945866,3.77003198860222));
#222432=CARTESIAN_POINT('',(5.47329194811131,17.872512105713,3.77003198860275));
#222433=CARTESIAN_POINT('',(-18.9913614317952,-57.4200769557627,3.77003198902513));
#222434=CARTESIAN_POINT('Origin',(5.49031038273072E-15,1.82930781209959E-13,
3.77003198860263));
#222435=CARTESIAN_POINT('',(-24.3081989336288,-55.379134258302,3.77003198882047));
#222436=CARTESIAN_POINT('Origin',(5.49031038273072E-15,1.82930781209959E-13,
3.77003198860263));
#222437=CARTESIAN_POINT('',(-24.3087286055912,-55.3789017591234,3.77003198860224));
#222438=CARTESIAN_POINT('Origin',(5.49031038273072E-15,1.82930781209959E-13,
3.77003198860263));
#222439=CARTESIAN_POINT('',(-24.1158676331753,-54.9457289227641,3.77003198860224));
#222440=CARTESIAN_POINT('Origin',(5.49031038273072E-15,1.82930781209959E-13,
3.77003198860263));
#222441=CARTESIAN_POINT('',(-19.0416371860872,-57.5748148483576,3.48823028058441));
#222442=CARTESIAN_POINT('',(-18.9913614315652,-57.4200769550672,3.77003198860223));
#222443=CARTESIAN_POINT('',(-24.3743766271346,-55.5277679690272,3.48823028074766));
#222444=CARTESIAN_POINT('Origin',(5.52999282761009E-15,1.84898592019556E-13,
3.48823028058481));
#222445=CARTESIAN_POINT('',(-24.3743766270209,-55.5277679687683,3.48823028058442));
#222446=CARTESIAN_POINT('Origin',(60.71525,1.85785428279622E-13,3.36123028058482));
#222447=CARTESIAN_POINT('',(-24.4643761377912,-55.7284918401498,3.36123028058443));
#222448=CARTESIAN_POINT('',(-19.109065001131,-57.7842031819383,3.36123028058441));
#222449=CARTESIAN_POINT('Origin',(5.5478765747851E-15,1.85785428279622E-13,
3.36123028058482));
#222450=CARTESIAN_POINT('',(-19.155790878562,-57.9280106456676,3.36123028058441));
#222451=CARTESIAN_POINT('',(5.4958300222142,17.9418771653391,3.36123028058494));
#222452=CARTESIAN_POINT('',(-24.5258780191666,-55.8666273273833,3.36123028058442));
#222453=CARTESIAN_POINT('Origin',(5.5478765747851E-15,1.85785428279622E-13,
3.36123028058482));
#222454=CARTESIAN_POINT('',(-24.4645917181903,-55.7289760416539,3.36123028058442));
#222455=CARTESIAN_POINT('Origin',(5.5478765747851E-15,1.85785428279622E-13,
3.36123028058482));
#222456=CARTESIAN_POINT('',(-24.6158705164589,-56.0673542004326,3.48823028058445));
#222457=CARTESIAN_POINT('',(-19.2232259142293,-58.137396517249,3.48823028042654));
#222458=CARTESIAN_POINT('Origin',(5.52999282761008E-15,1.84898592019556E-13,
3.48823028058484));
#222459=CARTESIAN_POINT('',(-19.2735045526304,-58.2921333818756,3.77003198802666));
#222460=CARTESIAN_POINT('',(-19.2232259141434,-58.1373965169893,3.48823028058443));
#222461=CARTESIAN_POINT('',(-19.2740436149879,-58.2919551457917,3.77003198860222));
#222462=CARTESIAN_POINT('Origin',(5.49031038273072E-15,1.82930781209959E-13,
3.77003198860263));
#222463=CARTESIAN_POINT('',(-24.6815255140421,-56.2162173246398,3.77003198860223));
#222464=CARTESIAN_POINT('Origin',(5.49031038273072E-15,1.82930781209959E-13,
3.77003198860263));
#222465=CARTESIAN_POINT('',(-24.6820453786627,-56.2159890767412,3.77003198802681));
#222466=CARTESIAN_POINT('Origin',(5.49031038273072E-15,1.82930781209959E-13,
3.77003198860263));
#222467=CARTESIAN_POINT('',(-24.6820453788103,-56.2159890770392,3.77003198860223));
#222468=CARTESIAN_POINT('Origin',(62.2224557307631,1.82930781209959E-13,
3.77003198860263));
#222469=CARTESIAN_POINT('',(-19.4207352200695,-58.7434254837932,3.77003198860222));
#222470=CARTESIAN_POINT('',(5.6397553624924,18.3848338156956,3.77003198860276));
#222471=CARTESIAN_POINT('',(-24.8746050278048,-56.6498810128382,3.77003198860222));
#222472=CARTESIAN_POINT('Origin',(5.49031038273072E-15,1.82930781209959E-13,
3.77003198860263));
#222473=CARTESIAN_POINT('',(-24.6817392197999,-56.2166973156306,3.77003198860223));
#222474=CARTESIAN_POINT('Origin',(5.57972911860581E-15,1.8736496251029E-13,
3.13503198860263));
#222475=CARTESIAN_POINT('Origin',(-18.8441250001649,-56.9687855447424,3.13502491541394));
#222476=CARTESIAN_POINT('Origin',(-24.1156440305584,-54.9452389789697,3.13502491541395));
#222477=CARTESIAN_POINT('Origin',(5.57972911860581E-15,1.8736496251029E-13,
3.13503198860263));
#222478=CARTESIAN_POINT('Origin',(-19.4325497530904,-58.7796783495202,3.20381846780163));
#222479=CARTESIAN_POINT('Origin',(-24.8900828550892,-56.6847272350805,3.20382022871814));
#222480=CARTESIAN_POINT('Origin',(5.51210908043506E-15,1.8401175575949E-13,
3.61523028058481));
#222481=CARTESIAN_POINT('Origin',(-19.1606565505628,-57.9431056782031,3.58786945046785));
#222482=CARTESIAN_POINT('Origin',(-24.5323241911526,-55.881015053282,3.58781461834135));
#222483=CARTESIAN_POINT('Origin',(5.51210908043507E-15,1.8401175575949E-13,
3.61523028058481));
#222484=CARTESIAN_POINT('Origin',(-19.1042362097712,-57.7691948748994,3.58781440266517));
#222485=CARTESIAN_POINT('Origin',(-24.4578836192973,-55.7140215708735,3.58786923592871));
#222486=CARTESIAN_POINT('Origin',(60.4792282238308,1.82930781209959E-13,
3.77003198860263));
#222487=CARTESIAN_POINT('',(-29.7268821954845,-52.1234703131947,3.77003198860226));
#222488=CARTESIAN_POINT('',(-24.6957503380303,-54.6869600343298,3.77003198860224));
#222489=CARTESIAN_POINT('Origin',(5.49031038273072E-15,1.82930781209959E-13,
3.77003198860263));
#222490=CARTESIAN_POINT('',(-24.8888299712407,-55.1206239907502,3.77003198860224));
#222491=CARTESIAN_POINT('',(9.71531210234964,22.6015516358795,3.77003198860278));
#222492=CARTESIAN_POINT('',(-24.8893571716689,-55.1203859404104,3.77003198902472));
#222493=CARTESIAN_POINT('Origin',(5.49031038273072E-15,1.82930781209959E-13,
3.77003198860263));
#222494=CARTESIAN_POINT('',(-29.963731877575,-52.5348628870839,3.77003198882049));
#222495=CARTESIAN_POINT('Origin',(5.49031038273072E-15,1.82930781209959E-13,
3.77003198860263));
#222496=CARTESIAN_POINT('',(-29.964234345157,-52.5345762957639,3.77003198860226));
#222497=CARTESIAN_POINT('Origin',(5.49031038273072E-15,1.82930781209959E-13,
3.77003198860263));
#222498=CARTESIAN_POINT('',(-29.7271509944135,-52.1239358865967,3.77003198860226));
#222499=CARTESIAN_POINT('Origin',(5.49031038273072E-15,1.82930781209959E-13,
3.77003198860263));
#222500=CARTESIAN_POINT('',(-24.955532024241,-55.2690209153041,3.48823028058442));
#222501=CARTESIAN_POINT('',(-24.8893571713678,-55.1203859397435,3.77003198860224));
#222502=CARTESIAN_POINT('',(-30.0450834961233,-52.6757649141853,3.48823028074767));
#222503=CARTESIAN_POINT('Origin',(5.52999282761009E-15,1.84898592019556E-13,
3.48823028058481));
#222504=CARTESIAN_POINT('',(-30.0450834959832,-52.6757649139397,3.48823028058444));
#222505=CARTESIAN_POINT('Origin',(60.71525,1.85785428279622E-13,3.36123028058482));
#222506=CARTESIAN_POINT('',(-30.1555713378333,-52.865981688396,3.36123028058444));
#222507=CARTESIAN_POINT('',(-25.0444775033943,-55.4702140717967,3.36123028058442));
#222508=CARTESIAN_POINT('Origin',(5.5478765747851E-15,1.85785428279622E-13,
3.36123028058482));
#222509=CARTESIAN_POINT('',(-25.1059793847697,-55.6083495590302,3.36123028058442));
#222510=CARTESIAN_POINT('',(9.75435829333326,22.6892508167096,3.36123028058498));
#222511=CARTESIAN_POINT('',(-30.2311753956707,-52.9969317578288,3.36123028058444));
#222512=CARTESIAN_POINT('Origin',(5.5478765747851E-15,1.85785428279622E-13,
3.36123028058482));
#222513=CARTESIAN_POINT('',(-30.1558363500995,-52.8664407031057,3.36123028058444));
#222514=CARTESIAN_POINT('Origin',(5.5478765747851E-15,1.85785428279622E-13,
3.36123028058482));
#222515=CARTESIAN_POINT('',(-30.3416565762231,-53.1871522506176,3.48823028058446));
#222516=CARTESIAN_POINT('',(-25.1949317876421,-55.80953951225,3.48823028042655));
#222517=CARTESIAN_POINT('Origin',(5.52999282761008E-15,1.84898592019556E-13,
3.48823028058484));
#222518=CARTESIAN_POINT('',(-25.2611094010716,-55.9581731633345,3.77003198802667));
#222519=CARTESIAN_POINT('',(-25.1949317875296,-55.8095395120007,3.48823028058444));
#222520=CARTESIAN_POINT('',(-25.2616268796452,-55.9579395562867,3.77003198860223));
#222521=CARTESIAN_POINT('Origin',(5.49031038273072E-15,1.82930781209959E-13,
3.77003198860263));
#222522=CARTESIAN_POINT('',(-30.4225123424706,-53.3283370710513,3.77003198860225));
#222523=CARTESIAN_POINT('Origin',(5.49031038273072E-15,1.82930781209959E-13,
3.77003198860263));
#222524=CARTESIAN_POINT('',(-30.4230055008163,-53.3280557328687,3.77003198802683));
#222525=CARTESIAN_POINT('Origin',(5.49031038273072E-15,1.82930781209959E-13,
3.77003198860263));
#222526=CARTESIAN_POINT('',(-30.4230055009943,-53.3280557331497,3.77003198860225));
#222527=CARTESIAN_POINT('Origin',(62.2224557307631,1.82930781209959E-13,
3.77003198860263));
#222528=CARTESIAN_POINT('',(-25.4547063934078,-56.3916032444851,3.77003198860223));
#222529=CARTESIAN_POINT('',(10.0037024164483,23.2492868865828,3.77003198860279));
#222530=CARTESIAN_POINT('',(-30.659864345357,-53.7394427993287,3.77003198860225));
#222531=CARTESIAN_POINT('Origin',(5.49031038273072E-15,1.82930781209959E-13,
3.77003198860263));
#222532=CARTESIAN_POINT('',(-30.4227750502466,-53.3287920942669,3.77003198860225));
#222533=CARTESIAN_POINT('Origin',(5.57972911860581E-15,1.8736496251029E-13,
3.13503198860263));
#222534=CARTESIAN_POINT('Origin',(-24.6957545189372,-54.6869571488951,3.13502491541393));
#222535=CARTESIAN_POINT('Origin',(-29.7268774036433,-52.1234719996036,3.13502491541395));
#222536=CARTESIAN_POINT('Origin',(5.57972911860581E-15,1.8736496251029E-13,
3.13503198860263));
#222537=CARTESIAN_POINT('Origin',(-25.4702456615231,-56.4264225582405,3.20381846780269));
#222538=CARTESIAN_POINT('Origin',(-30.6788998055448,-53.7724802568237,3.20382022872574));
#222539=CARTESIAN_POINT('Origin',(5.51210908043506E-15,1.8401175575949E-13,
3.61523028058481));
#222540=CARTESIAN_POINT('Origin',(-25.1123962626642,-55.622853298181,3.58786945046793));
#222541=CARTESIAN_POINT('Origin',(-30.2390901817304,-53.0105668578083,3.58781461834049));
#222542=CARTESIAN_POINT('Origin',(5.51210908043507E-15,1.8401175575949E-13,
3.61523028058481));
#222543=CARTESIAN_POINT('Origin',(-25.038106369386,-55.4557927279741,3.58781440266369));
#222544=CARTESIAN_POINT('Origin',(-30.1476018310241,-52.852269341751,3.58786923593029));
#222545=CARTESIAN_POINT('Origin',(60.4792282238308,1.82930781209959E-13,
3.77003198860263));
#222546=CARTESIAN_POINT('',(-35.0124214764581,-48.7306271754178,3.77003198860228));
#222547=CARTESIAN_POINT('',(-30.2768083268876,-51.8059703131947,3.77003198860226));
#222548=CARTESIAN_POINT('Origin',(5.49031038273072E-15,1.82930781209959E-13,
3.77003198860263));
#222549=CARTESIAN_POINT('',(-30.5141604766043,-52.2170762957392,3.77003198860226));
#222550=CARTESIAN_POINT('',(14.8448439902557,26.347024021557,3.77003198860281));
#222551=CARTESIAN_POINT('',(-30.5146599059375,-52.216784442014,3.77003198902515));
#222552=CARTESIAN_POINT('Origin',(5.49031038273072E-15,1.82930781209959E-13,
3.77003198860263));
#222553=CARTESIAN_POINT('',(-35.2909759047564,-49.1150085644481,3.77003198882052));
#222554=CARTESIAN_POINT('Origin',(5.49031038273072E-15,1.82930781209959E-13,
3.77003198860263));
#222555=CARTESIAN_POINT('',(-35.2914456628182,-49.1146710209411,3.77003198860228));
#222556=CARTESIAN_POINT('Origin',(5.49031038273072E-15,1.82930781209959E-13,
3.77003198860263));
#222557=CARTESIAN_POINT('',(-35.0127374685506,-48.731062101221,3.77003198860228));
#222558=CARTESIAN_POINT('Origin',(5.49031038273072E-15,1.82930781209959E-13,
3.77003198860263));
#222559=CARTESIAN_POINT('',(-30.5960088312564,-52.3576880233163,3.48823028058444));
#222560=CARTESIAN_POINT('',(-30.514659905568,-52.2167844413816,3.77003198860226));
#222561=CARTESIAN_POINT('',(-35.3866101429905,-49.246635155831,3.48823028074769));
#222562=CARTESIAN_POINT('Origin',(5.52999282761009E-15,1.84898592019556E-13,
3.48823028058481));
#222563=CARTESIAN_POINT('',(-35.3866101428255,-49.2466351556014,3.48823028058446));
#222564=CARTESIAN_POINT('Origin',(60.71525,1.85785428279622E-13,3.36123028058482));
#222565=CARTESIAN_POINT('',(-35.5163757878391,-49.4242607783462,3.36123028058446));
#222566=CARTESIAN_POINT('',(-30.7054974692364,-52.548481688396,3.36123028058444));
#222567=CARTESIAN_POINT('Origin',(5.5478765747851E-15,1.85785428279622E-13,
3.36123028058482));
#222568=CARTESIAN_POINT('',(-30.7811015270739,-52.6794317578288,3.36123028058444));
#222569=CARTESIAN_POINT('',(14.903849434298,26.4492244485615,3.361230280585));
#222570=CARTESIAN_POINT('',(-35.6052536882598,-49.5465907136146,3.36123028058446));
#222571=CARTESIAN_POINT('Origin',(5.5478765747851E-15,1.85785428279622E-13,
3.36123028058482));
#222572=CARTESIAN_POINT('',(-35.5166873284426,-49.4246895772004,3.36123028058446));
#222573=CARTESIAN_POINT('Origin',(5.5478765747851E-15,1.85785428279622E-13,
3.36123028058482));
#222574=CARTESIAN_POINT('',(-35.7350130971385,-49.7242207306176,3.48823028058449));
#222575=CARTESIAN_POINT('',(-30.8905967160111,-52.8702215134578,3.48823028042657));
#222576=CARTESIAN_POINT('Origin',(5.52999282761008E-15,1.84898592019556E-13,
3.48823028058484));
#222577=CARTESIAN_POINT('',(-30.9719482486877,-53.0111234896154,3.7700319880267));
#222578=CARTESIAN_POINT('',(-30.8905967158731,-52.8702215132217,3.48823028058446));
#222579=CARTESIAN_POINT('',(-30.9724384738737,-53.0108370710513,3.77003198860225));
#222580=CARTESIAN_POINT('Origin',(5.49031038273072E-15,1.82930781209959E-13,
3.77003198860263));
#222581=CARTESIAN_POINT('',(-35.830183759355,-49.8561803968404,3.77003198860227));
#222582=CARTESIAN_POINT('Origin',(5.49031038273072E-15,1.82930781209959E-13,
3.77003198860263));
#222583=CARTESIAN_POINT('',(-35.8306448082798,-49.8558490507738,3.77003198802685));
#222584=CARTESIAN_POINT('Origin',(5.49031038273072E-15,1.82930781209959E-13,
3.77003198860263));
#222585=CARTESIAN_POINT('',(-35.8306448084862,-49.8558490510346,3.77003198860227));
#222586=CARTESIAN_POINT('Origin',(62.2224557307631,1.82930781209959E-13,
3.77003198860263));
#222587=CARTESIAN_POINT('',(-31.2097904767601,-53.4219427993288,3.77003198860225));
#222588=CARTESIAN_POINT('',(15.2806508669887,27.1018636743466,3.77003198860282));
#222589=CARTESIAN_POINT('',(-36.1092077731524,-50.2402240048084,3.77003198860227));
#222590=CARTESIAN_POINT('Origin',(5.49031038273072E-15,1.82930781209959E-13,
3.77003198860263));
#222591=CARTESIAN_POINT('',(-35.8304925908678,-49.8566054669511,3.77003198860227));
#222592=CARTESIAN_POINT('Origin',(5.57972911860581E-15,1.8736496251029E-13,
3.13503198860263));
#222593=CARTESIAN_POINT('Origin',(-30.2768121832811,-51.805967006543,3.13502491541393));
#222594=CARTESIAN_POINT('Origin',(-35.0124168871447,-48.7306293534721,3.135024915414));
#222595=CARTESIAN_POINT('Origin',(5.57972911860581E-15,1.8736496251029E-13,
3.13503198860263));
#222596=CARTESIAN_POINT('Origin',(-31.228884228498,-53.4549470734241,3.20381846780309));
#222597=CARTESIAN_POINT('Origin',(-36.1315923097639,-50.2710907322494,3.20382022872386));
#222598=CARTESIAN_POINT('Origin',(5.51210908043506E-15,1.8401175575949E-13,
3.61523028058481));
#222599=CARTESIAN_POINT('Origin',(-30.788999306205,-52.693185297594,3.58786945046744));
#222600=CARTESIAN_POINT('Origin',(-35.6145503723404,-49.5593237986655,3.58781461834121));
#222601=CARTESIAN_POINT('Origin',(5.51210908043507E-15,1.8401175575949E-13,
3.61523028058481));
#222602=CARTESIAN_POINT('Origin',(-30.6976537960623,-52.5348053110496,3.5878144026648));
#222603=CARTESIAN_POINT('Origin',(-35.5070166083019,-49.4114565896691,3.58786923593059));
#222604=CARTESIAN_POINT('Origin',(60.4792282238308,1.82930781209959E-13,
3.77003198860263));
#222605=CARTESIAN_POINT('',(-39.9143573409153,-44.8038810887676,3.77003198860231));
#222606=CARTESIAN_POINT('',(-35.5261472678861,-48.357383540212,3.77003198860228));
#222607=CARTESIAN_POINT('Origin',(5.49031038273072E-15,1.82930781209959E-13,
3.77003198860263));
#222608=CARTESIAN_POINT('',(-35.8051714542876,-48.7414273857062,3.77003198860228));
#222609=CARTESIAN_POINT('',(20.6381965522785,28.9462038689909,3.77003198860283));
#222610=CARTESIAN_POINT('',(-35.8056376406732,-48.7410849262054,3.77003198902507));
#222611=CARTESIAN_POINT('Origin',(5.49031038273072E-15,1.82930781209959E-13,
3.77003198860263));
#222612=CARTESIAN_POINT('',(-40.2315646148138,-45.157039930004,3.77003198882054));
#222613=CARTESIAN_POINT('Origin',(5.49031038273072E-15,1.82930781209959E-13,
3.77003198860263));
#222614=CARTESIAN_POINT('',(-40.2319965165878,-45.1566551325073,3.7700319886023));
#222615=CARTESIAN_POINT('Origin',(5.49031038273072E-15,1.82930781209959E-13,
3.77003198860263));
#222616=CARTESIAN_POINT('',(-39.914717064096,-44.8042806018339,3.77003198860231));
#222617=CARTESIAN_POINT('Origin',(5.49031038273072E-15,1.82930781209959E-13,
3.77003198860263));
#222618=CARTESIAN_POINT('',(-35.90126936289,-48.8727133447945,3.48823028058446));
#222619=CARTESIAN_POINT('',(-35.8056376402397,-48.7410849256153,3.77003198860228));
#222620=CARTESIAN_POINT('',(-40.3404336840069,-45.2779489571885,3.48823028074772));
#222621=CARTESIAN_POINT('Origin',(5.52999282761009E-15,1.84898592019556E-13,
3.48823028058481));
#222622=CARTESIAN_POINT('',(-40.3404336838189,-45.2779489569774,3.48823028058449));
#222623=CARTESIAN_POINT('Origin',(60.71525,1.85785428279622E-13,3.36123028058482));
#222624=CARTESIAN_POINT('',(-40.4880553924339,-45.4410373245173,3.36123028058449));
#222625=CARTESIAN_POINT('',(-36.0301015792672,-49.0510171431405,3.36123028058446));
#222626=CARTESIAN_POINT('Origin',(5.5478765747851E-15,1.85785428279622E-13,
3.36123028058482));
#222627=CARTESIAN_POINT('',(-36.1189794796879,-49.1733470784089,3.36123028058446));
#222628=CARTESIAN_POINT('',(20.7197400704237,29.0584388930976,3.36123028058502));
#222629=CARTESIAN_POINT('',(-40.5892333705619,-45.5534068532513,3.36123028058449));
#222630=CARTESIAN_POINT('Origin',(5.5478765747851E-15,1.85785428279622E-13,
3.36123028058482));
#222631=CARTESIAN_POINT('',(-40.4884100480707,-45.441431209506,3.36123028058449));
#222632=CARTESIAN_POINT('Origin',(5.5478765747851E-15,1.85785428279622E-13,
3.36123028058482));
#222633=CARTESIAN_POINT('',(-40.7368493365293,-45.7165002428309,3.48823028058451));
#222634=CARTESIAN_POINT('',(-36.2478178024865,-49.351646303959,3.4882302804266));
#222635=CARTESIAN_POINT('Origin',(5.52999282761008E-15,1.84898592019556E-13,
3.48823028058484));
#222636=CARTESIAN_POINT('',(-36.3434519499943,-49.4832728536533,3.77003198802672));
#222637=CARTESIAN_POINT('',(-36.2478178023246,-49.3516463037386,3.48823028058449));
#222638=CARTESIAN_POINT('',(-36.3439095507831,-49.4829367616347,3.77003198860228));
#222639=CARTESIAN_POINT('Origin',(5.49031038273072E-15,1.82930781209959E-13,
3.77003198860263));
#222640=CARTESIAN_POINT('',(-40.845292185024,-45.8377889771253,3.7700319886023));
#222641=CARTESIAN_POINT('Origin',(5.49031038273072E-15,1.82930781209959E-13,
3.77003198860263));
#222642=CARTESIAN_POINT('',(-40.8457160731793,-45.8374112534715,3.77003198802688));
#222643=CARTESIAN_POINT('Origin',(5.49031038273072E-15,1.82930781209959E-13,
3.77003198860263));
#222644=CARTESIAN_POINT('',(-40.8457160734119,-45.8374112537092,3.7700319886023));
#222645=CARTESIAN_POINT('Origin',(62.2224557307631,1.82930781209959E-13,
3.77003198860263));
#222646=CARTESIAN_POINT('',(-36.6229335645805,-49.8669803696027,3.77003198860227));
#222647=CARTESIAN_POINT('',(21.2404668433927,29.7751578089173,3.77003198860284));
#222648=CARTESIAN_POINT('',(-41.1629311642477,-46.1905628026487,3.7700319886023));
#222649=CARTESIAN_POINT('Origin',(5.49031038273072E-15,1.82930781209959E-13,
3.77003198860263));
#222650=CARTESIAN_POINT('',(-40.8456437566508,-45.8381794369739,3.7700319886023));
#222651=CARTESIAN_POINT('Origin',(5.57972911860581E-15,1.8736496251029E-13,
3.13503198860263));
#222652=CARTESIAN_POINT('Origin',(-35.5261507575146,-48.3573798485716,3.13502491541401));
#222653=CARTESIAN_POINT('Origin',(-39.9143530044114,-44.8038837346042,3.13502491541403));
#222654=CARTESIAN_POINT('Origin',(5.57972911860581E-15,1.8736496251029E-13,
3.13503198860263));
#222655=CARTESIAN_POINT('Origin',(-36.6453726047996,-49.8978080023045,3.20381846780233));
#222656=CARTESIAN_POINT('Origin',(-41.1884195276103,-46.218920617716,3.20382022872564));
#222657=CARTESIAN_POINT('Origin',(5.51210908043506E-15,1.8401175575949E-13,
3.61523028058481));
#222658=CARTESIAN_POINT('Origin',(-36.1282716303348,-49.1861997321284,3.5878694504674));
#222659=CARTESIAN_POINT('Origin',(-40.5998100962477,-45.5650984170299,3.58781461834035));
#222660=CARTESIAN_POINT('Origin',(5.51210908043507E-15,1.8401175575949E-13,
3.61523028058481));
#222661=CARTESIAN_POINT('Origin',(-36.020871303843,-49.0382355735282,3.5878144026659));
#222662=CARTESIAN_POINT('Origin',(-40.4774090812932,-45.4292815791794,3.58786923592717));
#222663=CARTESIAN_POINT('Origin',(60.4792282238308,1.82930781209959E-13,
3.77003198860263));
#222664=CARTESIAN_POINT('',(-44.3789831537292,-40.386254305094,3.77003198860234));
#222665=CARTESIAN_POINT('',(-40.3862543050934,-44.3789831537297,3.77003198860231));
#222666=CARTESIAN_POINT('Origin',(5.49031038273072E-15,1.82930781209959E-13,
3.77003198860263));
#222667=CARTESIAN_POINT('',(-40.7038934808039,-44.7317571974361,3.77003198860231));
#222668=CARTESIAN_POINT('',(26.8427652369004,30.2864073093063,3.77003198860284));
#222669=CARTESIAN_POINT('',(-40.7043213166062,-44.7313678842175,3.77003198902489));
#222670=CARTESIAN_POINT('Origin',(5.49031038273072E-15,1.82930781209959E-13,
3.77003198860263));
#222671=CARTESIAN_POINT('',(-44.7313678839552,-40.7043213163685,3.77003198882057));
#222672=CARTESIAN_POINT('Origin',(5.49031038273072E-15,1.82930781209959E-13,
3.77003198860263));
#222673=CARTESIAN_POINT('',(-44.7317571974351,-40.7038934808041,3.77003198860234));
#222674=CARTESIAN_POINT('Origin',(5.49031038273072E-15,1.82930781209959E-13,
3.77003198860263));
#222675=CARTESIAN_POINT('',(-44.3793826667955,-40.3866140282747,3.77003198860234));
#222676=CARTESIAN_POINT('Origin',(5.49031038273072E-15,1.82930781209959E-13,
3.77003198860263));
#222677=CARTESIAN_POINT('',(-40.8131880745603,-44.8522789915943,3.48823028058449));
#222678=CARTESIAN_POINT('',(-40.7043213161135,-44.7313678836761,3.77003198860231));
#222679=CARTESIAN_POINT('',(-44.8522789918029,-40.8131880747511,3.48823028074775));
#222680=CARTESIAN_POINT('Origin',(5.52999282761009E-15,1.84898592019556E-13,
3.48823028058481));
#222681=CARTESIAN_POINT('',(-44.8522789915938,-40.8131880745608,3.48823028058452));
#222682=CARTESIAN_POINT('Origin',(60.71525,1.85785428279622E-13,3.36123028058482));
#222683=CARTESIAN_POINT('',(-45.016139389479,-40.9599523566127,3.36123028058452));
#222684=CARTESIAN_POINT('',(-40.9599523566121,-45.0161393894795,3.36123028058449));
#222685=CARTESIAN_POINT('Origin',(5.5478765747851E-15,1.85785428279622E-13,
3.36123028058482));
#222686=CARTESIAN_POINT('',(-41.06113033474,-45.1285089182134,3.36123028058449));
#222687=CARTESIAN_POINT('',(26.9484406282047,30.4037717213984,3.36123028058503));
#222688=CARTESIAN_POINT('',(-45.1285089182129,-41.0611303347406,3.36123028058452));
#222689=CARTESIAN_POINT('Origin',(5.5478765747851E-15,1.85785428279622E-13,
3.36123028058482));
#222690=CARTESIAN_POINT('',(-45.0165332744676,-40.9603070122494,3.36123028058452));
#222691=CARTESIAN_POINT('Origin',(5.5478765747851E-15,1.85785428279622E-13,
3.36123028058482));
#222692=CARTESIAN_POINT('',(-45.2923641298554,-41.2079002115909,3.48823028058454));
#222693=CARTESIAN_POINT('',(-41.2079002117744,-45.2923641300582,3.48823028042662));
#222694=CARTESIAN_POINT('Origin',(5.52999282761008E-15,1.84898592019556E-13,
3.48823028058484));
#222695=CARTESIAN_POINT('',(-41.3167691863805,-45.413273125266,3.77003198802675));
#222696=CARTESIAN_POINT('',(-41.2079002115903,-45.2923641298559,3.48823028058452));
#222697=CARTESIAN_POINT('',(-41.3171891492021,-45.4128910420874,3.7700319886023));
#222698=CARTESIAN_POINT('Origin',(5.49031038273072E-15,1.82930781209959E-13,
3.77003198860263));
#222699=CARTESIAN_POINT('',(-45.4128910420869,-41.3171891492027,3.77003198860233));
#222700=CARTESIAN_POINT('Origin',(5.49031038273072E-15,1.82930781209959E-13,
3.77003198860263));
#222701=CARTESIAN_POINT('',(-45.4132731252655,-41.3167691863811,3.77003198802691));
#222702=CARTESIAN_POINT('Origin',(5.49031038273072E-15,1.82930781209959E-13,
3.77003198860263));
#222703=CARTESIAN_POINT('',(-45.4132731255216,-41.3167691865933,3.77003198860233));
#222704=CARTESIAN_POINT('Origin',(62.2224557307631,1.82930781209959E-13,
3.77003198860263));
#222705=CARTESIAN_POINT('',(-41.6348281284258,-45.7656648676108,3.7700319886023));
#222706=CARTESIAN_POINT('',(27.6232705441538,31.1532462714326,3.77003198860285));
#222707=CARTESIAN_POINT('',(-45.7656648676103,-41.6348281284264,3.77003198860233));
#222708=CARTESIAN_POINT('Origin',(5.49031038273072E-15,1.82930781209959E-13,
3.77003198860263));
#222709=CARTESIAN_POINT('',(-45.4132815019355,-41.3175407208296,3.77003198860233));
#222710=CARTESIAN_POINT('Origin',(5.57972911860581E-15,1.8736496251029E-13,
3.13503198860263));
#222711=CARTESIAN_POINT('Origin',(-40.3862573897238,-44.378979117547,3.13502491541399));
#222712=CARTESIAN_POINT('Origin',(-44.3789791175464,-40.3862573897246,3.13502491541403));
#222713=CARTESIAN_POINT('Origin',(5.57972911860581E-15,1.8736496251029E-13,
3.13503198860263));
#222714=CARTESIAN_POINT('Origin',(-41.6603666103058,-45.7939781049253,3.20381846780306));
#222715=CARTESIAN_POINT('Origin',(-45.7939778018807,-41.6603663369627,3.20382022872453));
#222716=CARTESIAN_POINT('Origin',(5.51210908043506E-15,1.8401175575949E-13,
3.61523028058481));
#222717=CARTESIAN_POINT('Origin',(-41.0717150501544,-45.1403198695221,3.58786945047096));
#222718=CARTESIAN_POINT('Origin',(-45.1402498046847,-41.071652282028,3.58781461833824));
#222719=CARTESIAN_POINT('Origin',(5.51210908043507E-15,1.8401175575949E-13,
3.61523028058481));
#222720=CARTESIAN_POINT('Origin',(-40.9494366077766,-45.0043926651437,3.58781440266436));
#222721=CARTESIAN_POINT('Origin',(-45.0043225899492,-40.9493738530207,3.5878692359261));
#222722=CARTESIAN_POINT('Origin',(60.4792282238308,1.82930781209959E-13,
3.77003198860263));
#222723=CARTESIAN_POINT('',(-48.3573835402116,-35.5261472678868,3.77003198860237));
#222724=CARTESIAN_POINT('',(-44.8038810887671,-39.9143573409159,3.77003198860234));
#222725=CARTESIAN_POINT('Origin',(5.49031038273072E-15,1.82930781209959E-13,
3.77003198860263));
#222726=CARTESIAN_POINT('',(-45.1566551325072,-40.2319965165888,3.77003198860234));
#222727=CARTESIAN_POINT('',(33.1880655373213,30.3099068238766,3.77003198860284));
#222728=CARTESIAN_POINT('',(-45.1570399302682,-40.2315646150503,3.77003198902526));
#222729=CARTESIAN_POINT('Origin',(5.49031038273072E-15,1.82930781209959E-13,
3.77003198860263));
#222730=CARTESIAN_POINT('',(-48.7410849259195,-35.8056376404641,3.77003198882061));
#222731=CARTESIAN_POINT('Origin',(5.49031038273072E-15,1.82930781209959E-13,
3.77003198860263));
#222732=CARTESIAN_POINT('',(-48.7414273857053,-35.8051714542879,3.77003198860237));
#222733=CARTESIAN_POINT('Origin',(5.49031038273072E-15,1.82930781209959E-13,
3.77003198860263));
#222734=CARTESIAN_POINT('',(-48.3578184660148,-35.5264632599794,3.77003198860237));
#222735=CARTESIAN_POINT('Origin',(5.49031038273072E-15,1.82930781209959E-13,
3.77003198860263));
#222736=CARTESIAN_POINT('',(-45.2779489569769,-40.3404336838195,3.48823028058452));
#222737=CARTESIAN_POINT('',(-45.1570399297212,-40.231564614563,3.77003198860234));
#222738=CARTESIAN_POINT('',(-48.8727133450219,-35.9012693630581,3.48823028074779));
#222739=CARTESIAN_POINT('Origin',(5.52999282761009E-15,1.84898592019556E-13,
3.48823028058481));
#222740=CARTESIAN_POINT('',(-48.8727133447941,-35.9012693628907,3.48823028058455));
#222741=CARTESIAN_POINT('Origin',(60.71525,1.85785428279622E-13,3.36123028058482));
#222742=CARTESIAN_POINT('',(-49.05101714314,-36.0301015792679,3.36123028058456));
#222743=CARTESIAN_POINT('',(-45.4410373245168,-40.4880553924345,3.36123028058453));
#222744=CARTESIAN_POINT('Origin',(5.5478765747851E-15,1.85785428279622E-13,
3.36123028058482));
#222745=CARTESIAN_POINT('',(-45.5534068532508,-40.5892333705625,3.36123028058452));
#222746=CARTESIAN_POINT('',(33.3184119221863,30.4272712359686,3.36123028058503));
#222747=CARTESIAN_POINT('',(-49.1733470784084,-36.1189794796885,3.36123028058456));
#222748=CARTESIAN_POINT('Origin',(5.5478765747851E-15,1.85785428279622E-13,
3.36123028058482));
#222749=CARTESIAN_POINT('',(-49.0514459419942,-36.0304131198714,3.36123028058456));
#222750=CARTESIAN_POINT('Origin',(5.5478765747851E-15,1.85785428279622E-13,
3.36123028058482));
#222751=CARTESIAN_POINT('',(-49.3516463037382,-36.2478178023253,3.48823028058458));
#222752=CARTESIAN_POINT('',(-45.7165002430345,-40.7368493367118,3.48823028042666));
#222753=CARTESIAN_POINT('Origin',(5.52999282761008E-15,1.84898592019556E-13,
3.48823028058484));
#222754=CARTESIAN_POINT('',(-45.8374112534709,-40.8457160731799,3.77003198802678));
#222755=CARTESIAN_POINT('',(-45.7165002428303,-40.7368493365299,3.48823028058455));
#222756=CARTESIAN_POINT('',(-45.8377889771247,-40.8452921850246,3.77003198860234));
#222757=CARTESIAN_POINT('Origin',(5.49031038273072E-15,1.82930781209959E-13,
3.77003198860263));
#222758=CARTESIAN_POINT('',(-49.4829367616343,-36.3439095507838,3.77003198860237));
#222759=CARTESIAN_POINT('Origin',(5.49031038273072E-15,1.82930781209959E-13,
3.77003198860263));
#222760=CARTESIAN_POINT('',(-49.4832728536529,-36.343451949995,3.77003198802694));
#222761=CARTESIAN_POINT('Origin',(5.49031038273072E-15,1.82930781209959E-13,
3.77003198860263));
#222762=CARTESIAN_POINT('',(-49.4832728539298,-36.3434519501792,3.77003198860237));
#222763=CARTESIAN_POINT('Origin',(62.2224557307631,1.82930781209959E-13,
3.77003198860263));
#222764=CARTESIAN_POINT('',(-46.1905628026481,-41.1629311642483,3.77003198860233));
#222765=CARTESIAN_POINT('',(34.1507877370002,31.1767457860028,3.77003198860285));
#222766=CARTESIAN_POINT('',(-49.8669803696023,-36.6229335645812,3.77003198860236));
#222767=CARTESIAN_POINT('Origin',(5.49031038273072E-15,1.82930781209959E-13,
3.77003198860263));
#222768=CARTESIAN_POINT('',(-49.4833618317449,-36.3442183822966,3.77003198860237));
#222769=CARTESIAN_POINT('Origin',(5.57972911860581E-15,1.8736496251029E-13,
3.13503198860263));
#222770=CARTESIAN_POINT('Origin',(-44.8038837346036,-39.9143530044121,3.13502491541405));
#222771=CARTESIAN_POINT('Origin',(-48.3573798485711,-35.5261507575154,3.13502491541409));
#222772=CARTESIAN_POINT('Origin',(5.57972911860581E-15,1.8736496251029E-13,
3.13503198860263));
#222773=CARTESIAN_POINT('Origin',(-46.2189209212445,-41.188419800416,3.20381846780359));
#222774=CARTESIAN_POINT('Origin',(-49.8978076723477,-36.6453723646279,3.20382022872044));
#222775=CARTESIAN_POINT('Origin',(5.51210908043506E-15,1.8401175575949E-13,
3.61523028058481));
#222776=CARTESIAN_POINT('Origin',(-45.5651681650776,-40.5998732162087,3.58786945046834));
#222777=CARTESIAN_POINT('Origin',(-49.1861234900546,-36.1282165298262,3.58781461834196));
#222778=CARTESIAN_POINT('Origin',(5.51210908043507E-15,1.8401175575949E-13,
3.61523028058481));
#222779=CARTESIAN_POINT('Origin',(-45.4293513150143,-40.4774722129462,3.58781440266486));
#222780=CARTESIAN_POINT('Origin',(-49.0381593225501,-36.0208162177263,3.58786923593133));
#222781=CARTESIAN_POINT('Origin',(60.4792282238308,1.82930781209959E-13,
3.77003198860263));
#222782=CARTESIAN_POINT('',(-51.8059703131944,-30.2768083268883,3.77003198860241));
#222783=CARTESIAN_POINT('',(-48.7306271754173,-35.0124214764587,3.77003198860237));
#222784=CARTESIAN_POINT('Origin',(5.49031038273072E-15,1.82930781209959E-13,
3.77003198860263));
#222785=CARTESIAN_POINT('',(-49.1146710209412,-35.2914456628193,3.77003198860238));
#222786=CARTESIAN_POINT('',(39.3975469582344,29.0164449471024,3.77003198860284));
#222787=CARTESIAN_POINT('',(-49.1150085647352,-35.2909759049636,3.77003198902498));
#222788=CARTESIAN_POINT('Origin',(5.49031038273072E-15,1.82930781209959E-13,
3.77003198860263));
#222789=CARTESIAN_POINT('',(-52.2167844417076,-30.5146599057594,3.77003198882065));
#222790=CARTESIAN_POINT('Origin',(5.49031038273072E-15,1.82930781209959E-13,
3.77003198860263));
#222791=CARTESIAN_POINT('',(-52.2170762957382,-30.5141604766047,3.77003198860241));
#222792=CARTESIAN_POINT('Origin',(5.49031038273072E-15,1.82930781209959E-13,
3.77003198860263));
#222793=CARTESIAN_POINT('',(-51.8064358865964,-30.2770771258173,3.77003198860241));
#222794=CARTESIAN_POINT('Origin',(5.49031038273072E-15,1.82930781209959E-13,
3.77003198860263));
#222795=CARTESIAN_POINT('',(-49.246635155601,-35.3866101428262,3.48823028058456));
#222796=CARTESIAN_POINT('',(-49.1150085641408,-35.2909759045365,3.77003198860237));
#222797=CARTESIAN_POINT('',(-52.3576880235601,-30.5960088313997,3.48823028074783));
#222798=CARTESIAN_POINT('Origin',(5.52999282761009E-15,1.84898592019556E-13,
3.48823028058481));
#222799=CARTESIAN_POINT('',(-52.357688023316,-30.5960088312571,3.48823028058459));
#222800=CARTESIAN_POINT('Origin',(60.71525,1.85785428279622E-13,3.36123028058482));
#222801=CARTESIAN_POINT('',(-52.5484816883957,-30.7054974692372,3.36123028058459));
#222802=CARTESIAN_POINT('',(-49.4242607783458,-35.5163757878398,3.36123028058456));
#222803=CARTESIAN_POINT('Origin',(5.5478765747851E-15,1.85785428279622E-13,
3.36123028058482));
#222804=CARTESIAN_POINT('',(-49.5465907136142,-35.6052536882604,3.36123028058456));
#222805=CARTESIAN_POINT('',(39.5520252162584,29.1286799712091,3.36123028058503));
#222806=CARTESIAN_POINT('',(-52.6794317578285,-30.7811015270746,3.36123028058459));
#222807=CARTESIAN_POINT('Origin',(5.5478765747851E-15,1.85785428279622E-13,
3.36123028058482));
#222808=CARTESIAN_POINT('',(-52.5489407031054,-30.7057624815034,3.36123028058459));
#222809=CARTESIAN_POINT('Origin',(5.5478765747851E-15,1.85785428279622E-13,
3.36123028058482));
#222810=CARTESIAN_POINT('',(-52.8702215132213,-30.8905967158739,3.48823028058462));
#222811=CARTESIAN_POINT('',(-49.7242207308393,-35.7350130972987,3.48823028042669));
#222812=CARTESIAN_POINT('Origin',(5.52999282761008E-15,1.84898592019556E-13,
3.48823028058484));
#222813=CARTESIAN_POINT('',(-49.8558490507733,-35.8306448082804,3.77003198802681));
#222814=CARTESIAN_POINT('',(-49.7242207306172,-35.7350130971391,3.48823028058458));
#222815=CARTESIAN_POINT('',(-49.85618039684,-35.8301837593557,3.77003198860237));
#222816=CARTESIAN_POINT('Origin',(5.49031038273072E-15,1.82930781209959E-13,
3.77003198860263));
#222817=CARTESIAN_POINT('',(-53.010837071051,-30.9724384738745,3.7700319886024));
#222818=CARTESIAN_POINT('Origin',(5.49031038273072E-15,1.82930781209959E-13,
3.77003198860263));
#222819=CARTESIAN_POINT('',(-53.0111234896151,-30.9719482486884,3.77003198802698));
#222820=CARTESIAN_POINT('Origin',(5.49031038273072E-15,1.82930781209959E-13,
3.77003198860263));
#222821=CARTESIAN_POINT('',(-53.0111234899097,-30.9719482488427,3.7700319886024));
#222822=CARTESIAN_POINT('Origin',(62.2224557307631,1.82930781209959E-13,
3.77003198860263));
#222823=CARTESIAN_POINT('',(-50.240224004808,-36.1092077731531,3.77003198860237));
#222824=CARTESIAN_POINT('',(40.5385041740525,29.8453988870289,3.77003198860284));
#222825=CARTESIAN_POINT('',(-53.4219427993284,-31.2097904767609,3.7700319886024));
#222826=CARTESIAN_POINT('Origin',(5.49031038273072E-15,1.82930781209959E-13,
3.77003198860263));
#222827=CARTESIAN_POINT('',(-53.0112920942665,-30.9727011816505,3.7700319886024));
#222828=CARTESIAN_POINT('Origin',(5.57972911860581E-15,1.8736496251029E-13,
3.13503198860263));
#222829=CARTESIAN_POINT('Origin',(-48.7306293534716,-35.0124168871455,3.13502491541407));
#222830=CARTESIAN_POINT('Origin',(-51.8059670065426,-30.2768121832819,3.13502491541411));
#222831=CARTESIAN_POINT('Origin',(5.57972911860581E-15,1.8736496251029E-13,
3.13503198860263));
#222832=CARTESIAN_POINT('Origin',(-50.2710910626254,-36.1315925493529,3.20381846779954));
#222833=CARTESIAN_POINT('Origin',(-53.4549467201712,-31.2288840241303,3.20382022872153));
#222834=CARTESIAN_POINT('Origin',(5.51210908043506E-15,1.8401175575949E-13,
3.61523028058481));
#222835=CARTESIAN_POINT('Origin',(-49.5593997624596,-35.6146058558681,3.58786945046727));
#222836=CARTESIAN_POINT('Origin',(-52.6931037136094,-30.7889524770089,3.58781461834492));
#222837=CARTESIAN_POINT('Origin',(5.51210908043507E-15,1.8401175575949E-13,
3.61523028058481));
#222838=CARTESIAN_POINT('Origin',(-49.4115325425325,-35.5070721047359,3.58781440266261));
#222839=CARTESIAN_POINT('Origin',(-52.5347237197169,-30.6976069821036,3.58786923592639));
#222840=CARTESIAN_POINT('Origin',(60.4792282238308,1.82930781209959E-13,
3.77003198860263));
#222841=CARTESIAN_POINT('',(-54.6869600343295,-24.695750338031,3.77003198860245));
#222842=CARTESIAN_POINT('',(-52.1234703131944,-29.7268821954852,3.77003198860241));
#222843=CARTESIAN_POINT('Origin',(5.49031038273072E-15,1.82930781209959E-13,
3.77003198860263));
#222844=CARTESIAN_POINT('',(-52.5345762957641,-29.9642343451581,3.77003198860241));
#222845=CARTESIAN_POINT('',(45.2006711678726,26.4632370872591,3.77003198860282));
#222846=CARTESIAN_POINT('',(-52.5348628873911,-29.9637318777511,3.77003198902505));
#222847=CARTESIAN_POINT('Origin',(5.49031038273072E-15,1.82930781209959E-13,
3.77003198860263));
#222848=CARTESIAN_POINT('',(-55.1203859400877,-24.8893571715241,3.77003198882068));
#222849=CARTESIAN_POINT('Origin',(5.49031038273072E-15,1.82930781209959E-13,
3.77003198860263));
#222850=CARTESIAN_POINT('',(-55.1206239907494,-24.8888299712412,3.77003198860244));
#222851=CARTESIAN_POINT('Origin',(5.49031038273072E-15,1.82930781209959E-13,
3.77003198860263));
#222852=CARTESIAN_POINT('',(-54.6874511544107,-24.6959689987791,3.77003198860245));
#222853=CARTESIAN_POINT('Origin',(5.49031038273072E-15,1.82930781209959E-13,
3.77003198860263));
#222854=CARTESIAN_POINT('',(-52.6757649139393,-30.0450834959839,3.48823028058459));
#222855=CARTESIAN_POINT('',(-52.5348628867552,-29.9637318773884,3.77003198860241));
#222856=CARTESIAN_POINT('',(-55.2690209155615,-24.9555320243581,3.48823028074786));
#222857=CARTESIAN_POINT('Origin',(5.52999282761009E-15,1.84898592019556E-13,
3.48823028058481));
#222858=CARTESIAN_POINT('',(-55.2690209153038,-24.9555320242418,3.48823028058463));
#222859=CARTESIAN_POINT('Origin',(60.71525,1.85785428279622E-13,3.36123028058482));
#222860=CARTESIAN_POINT('',(-55.4702140717965,-25.044477503395,3.36123028058463));
#222861=CARTESIAN_POINT('',(-52.8659816883957,-30.155571337834,3.3612302805846));
#222862=CARTESIAN_POINT('Origin',(5.5478765747851E-15,1.85785428279622E-13,
3.36123028058482));
#222863=CARTESIAN_POINT('',(-52.9969317578285,-30.2311753956715,3.3612302805846));
#222864=CARTESIAN_POINT('',(45.3776874999996,26.5654375142636,3.36123028058501));
#222865=CARTESIAN_POINT('',(-55.6083495590299,-25.1059793847704,3.36123028058463));
#222866=CARTESIAN_POINT('Origin',(5.5478765747851E-15,1.85785428279622E-13,
3.36123028058482));
#222867=CARTESIAN_POINT('',(-55.4706982733005,-25.0446930837941,3.36123028058463));
#222868=CARTESIAN_POINT('Origin',(5.5478765747851E-15,1.85785428279622E-13,
3.36123028058482));
#222869=CARTESIAN_POINT('',(-55.8095395120005,-25.1949317875303,3.48823028058465));
#222870=CARTESIAN_POINT('',(-53.1871522508548,-30.3416565763594,3.48823028042673));
#222871=CARTESIAN_POINT('Origin',(5.52999282761008E-15,1.84898592019556E-13,
3.48823028058484));
#222872=CARTESIAN_POINT('',(-53.3280557328683,-30.423005500817,3.77003198802685));
#222873=CARTESIAN_POINT('',(-53.1871522506172,-30.3416565762239,3.48823028058462));
#222874=CARTESIAN_POINT('',(-53.328337071051,-30.4225123424714,3.77003198860241));
#222875=CARTESIAN_POINT('Origin',(5.49031038273072E-15,1.82930781209959E-13,
3.77003198860263));
#222876=CARTESIAN_POINT('',(-55.9579395562864,-25.2616268796459,3.77003198860244));
#222877=CARTESIAN_POINT('Origin',(5.49031038273072E-15,1.82930781209959E-13,
3.77003198860263));
#222878=CARTESIAN_POINT('',(-55.9581731633343,-25.2611094010724,3.77003198802702));
#222879=CARTESIAN_POINT('Origin',(5.49031038273072E-15,1.82930781209959E-13,
3.77003198860263));
#222880=CARTESIAN_POINT('',(-55.9581731636435,-25.261109401195,3.77003198860244));
#222881=CARTESIAN_POINT('Origin',(62.2224557307631,1.82930781209959E-13,
3.77003198860263));
#222882=CARTESIAN_POINT('',(-53.7394427993284,-30.6598643453577,3.7700319886024));
#222883=CARTESIAN_POINT('',(46.5080917980719,27.2180767400487,3.77003198860282));
#222884=CARTESIAN_POINT('',(-56.3916032444849,-25.4547063934086,3.77003198860244));
#222885=CARTESIAN_POINT('Origin',(5.49031038273072E-15,1.82930781209959E-13,
3.77003198860263));
#222886=CARTESIAN_POINT('',(-55.9584195472773,-25.2618405854037,3.77003198860244));
#222887=CARTESIAN_POINT('Origin',(5.57972911860581E-15,1.8736496251029E-13,
3.13503198860263));
#222888=CARTESIAN_POINT('Origin',(-52.1234719996032,-29.726877403644,3.13502491541413));
#222889=CARTESIAN_POINT('Origin',(-54.6869571488948,-24.6957545189381,3.13502491541414));
#222890=CARTESIAN_POINT('Origin',(5.57972911860581E-15,1.8736496251029E-13,
3.13503198860263));
#222891=CARTESIAN_POINT('Origin',(-53.7724806104365,-30.6789000092851,3.20381846780326));
#222892=CARTESIAN_POINT('Origin',(-56.4264221855626,-25.4702454951955,3.20382022872092));
#222893=CARTESIAN_POINT('Origin',(5.51210908043506E-15,1.8401175575949E-13,
3.61523028058481));
#222894=CARTESIAN_POINT('Origin',(-53.0106482050715,-30.2391374209341,3.58786945046879));
#222895=CARTESIAN_POINT('Origin',(-55.6227672661396,-25.1123582178524,3.58781461834275));
#222896=CARTESIAN_POINT('Origin',(5.51210908043507E-15,1.8401175575949E-13,
3.61523028058481));
#222897=CARTESIAN_POINT('Origin',(-52.8523506794952,-30.1476490842058,3.58781440266405));
#222898=CARTESIAN_POINT('Origin',(-55.4557066902171,-25.0380683404975,3.58786923592836));
#222899=CARTESIAN_POINT('Origin',(60.4792282238308,1.82930781209959E-13,
3.77003198860263));
#222900=CARTESIAN_POINT('',(-56.9687879773465,-18.8441205405522,3.77003198860249));
#222901=CARTESIAN_POINT('',(-54.9452378026827,-24.1156489724279,3.77003198860245));
#222902=CARTESIAN_POINT('Origin',(5.49031038273072E-15,1.82930781209959E-13,
3.77003198860263));
#222903=CARTESIAN_POINT('',(-55.3789017591237,-24.3087286055922,3.77003198860245));
#222904=CARTESIAN_POINT('',(50.3447265545023,22.7624634345051,3.77003198860279));
#222905=CARTESIAN_POINT('',(-55.3791342586262,-24.308198933772,3.77003198902528));
#222906=CARTESIAN_POINT('Origin',(5.49031038273072E-15,1.82930781209959E-13,
3.77003198860263));
#222907=CARTESIAN_POINT('',(-57.420076955426,-18.9913614316847,3.77003198882073));
#222908=CARTESIAN_POINT('Origin',(5.49031038273072E-15,1.82930781209959E-13,
3.77003198860263));
#222909=CARTESIAN_POINT('',(-57.4202585945858,-18.9908122363903,3.77003198860249));
#222910=CARTESIAN_POINT('Origin',(5.49031038273072E-15,1.82930781209959E-13,
3.77003198860263));
#222911=CARTESIAN_POINT('',(-56.9692992632924,-18.8442866674264,3.77003198860249));
#222912=CARTESIAN_POINT('Origin',(5.49031038273072E-15,1.82930781209959E-13,
3.77003198860263));
#222913=CARTESIAN_POINT('',(-55.5277679687681,-24.3743766270217,3.48823028058463));
#222914=CARTESIAN_POINT('',(-55.3791342579556,-24.3081989334776,3.77003198860245));
#222915=CARTESIAN_POINT('',(-57.5748148486259,-19.0416371861768,3.4882302807479));
#222916=CARTESIAN_POINT('Origin',(5.52999282761009E-15,1.84898592019556E-13,
3.48823028058481));
#222917=CARTESIAN_POINT('',(-57.5748148483574,-19.041637186088,3.48823028058467));
#222918=CARTESIAN_POINT('Origin',(60.71525,1.85785428279622E-13,3.36123028058482));
#222919=CARTESIAN_POINT('',(-57.7842031819381,-19.1090650011318,3.36123028058467));
#222920=CARTESIAN_POINT('',(-55.7284918401496,-24.4643761377919,3.36123028058464));
#222921=CARTESIAN_POINT('Origin',(5.5478765747851E-15,1.85785428279622E-13,
3.36123028058482));
#222922=CARTESIAN_POINT('',(-55.8666273273831,-24.5258780191674,3.36123028058464));
#222923=CARTESIAN_POINT('',(50.541702139688,22.8501626153352,3.36123028058498));
#222924=CARTESIAN_POINT('',(-57.9280106456674,-19.1557908785628,3.36123028058467));
#222925=CARTESIAN_POINT('Origin',(5.5478765747851E-15,1.85785428279622E-13,
3.36123028058482));
#222926=CARTESIAN_POINT('',(-57.7847072652235,-19.1092287877198,3.36123028058467));
#222927=CARTESIAN_POINT('Origin',(5.5478765747851E-15,1.85785428279622E-13,
3.36123028058482));
#222928=CARTESIAN_POINT('',(-58.1373965169892,-19.2232259141442,3.4882302805847));
#222929=CARTESIAN_POINT('',(-56.0673542006828,-24.6158705165696,3.48823028042677));
#222930=CARTESIAN_POINT('Origin',(5.52999282761008E-15,1.84898592019556E-13,
3.48823028058484));
#222931=CARTESIAN_POINT('',(-56.2159890767409,-24.6820453786634,3.77003198802689));
#222932=CARTESIAN_POINT('',(-56.0673542004324,-24.6158705164596,3.48823028058466));
#222933=CARTESIAN_POINT('',(-56.2162173246396,-24.6815255140429,3.77003198860245));
#222934=CARTESIAN_POINT('Origin',(5.49031038273072E-15,1.82930781209959E-13,
3.77003198860263));
#222935=CARTESIAN_POINT('',(-58.2919551457915,-19.2740436149887,3.77003198860248));
#222936=CARTESIAN_POINT('Origin',(5.49031038273072E-15,1.82930781209959E-13,
3.77003198860263));
#222937=CARTESIAN_POINT('',(-58.2921333818755,-19.2735045526312,3.77003198802706));
#222938=CARTESIAN_POINT('Origin',(5.49031038273072E-15,1.82930781209959E-13,
3.77003198860263));
#222939=CARTESIAN_POINT('',(-58.2921333821958,-19.2735045527209,3.77003198860248));
#222940=CARTESIAN_POINT('Origin',(62.2224557307631,1.82930781209959E-13,
3.77003198860263));
#222941=CARTESIAN_POINT('',(-56.649881012838,-24.8746050278055,3.77003198860245));
#222942=CARTESIAN_POINT('',(51.799563747336,23.4101986852084,3.7700319886028));
#222943=CARTESIAN_POINT('',(-58.7434254837931,-19.4207352200704,3.77003198860248));
#222944=CARTESIAN_POINT('Origin',(5.49031038273072E-15,1.82930781209959E-13,
3.77003198860263));
#222945=CARTESIAN_POINT('',(-58.2924548456759,-19.2742059773234,3.77003198860248));
#222946=CARTESIAN_POINT('Origin',(5.57972911860581E-15,1.8736496251029E-13,
3.13503198860263));
#222947=CARTESIAN_POINT('Origin',(-54.9452389789694,-24.1156440305593,3.13502491541412));
#222948=CARTESIAN_POINT('Origin',(-56.9687855447422,-18.8441250001659,3.13502491541418));
#222949=CARTESIAN_POINT('Origin',(5.57972911860581E-15,1.8736496251029E-13,
3.13503198860263));
#222950=CARTESIAN_POINT('Origin',(-56.684727608054,-24.8900830207542,3.20381846780062));
#222951=CARTESIAN_POINT('Origin',(-58.7796779614966,-19.4325496266337,3.20382022872046));
#222952=CARTESIAN_POINT('Origin',(5.51210908043506E-15,1.8401175575949E-13,
3.61523028058481));
#222953=CARTESIAN_POINT('Origin',(-55.8811008927584,-24.5323626684708,3.58786945046843));
#222954=CARTESIAN_POINT('Origin',(-57.9430161406882,-19.1606277069616,3.58781461834337));
#222955=CARTESIAN_POINT('Origin',(5.51210908043507E-15,1.8401175575949E-13,
3.61523028058481));
#222956=CARTESIAN_POINT('Origin',(-55.7141074023436,-24.457922111514,3.58781440266405));
#222957=CARTESIAN_POINT('Origin',(-57.7691053333672,-19.1042073825995,3.58786923593191));
#222958=CARTESIAN_POINT('Origin',(60.4792282238308,1.82930781209959E-13,
3.77003198860263));
#222959=CARTESIAN_POINT('',(-58.6264539577983,-12.7860306150454,3.77003198860253));
#222960=CARTESIAN_POINT('',(-57.1650137687745,-18.2401996527048,3.77003198860249));
#222961=CARTESIAN_POINT('Origin',(5.49031038273072E-15,1.82930781209959E-13,
3.77003198860263));
#222962=CARTESIAN_POINT('',(-57.6164843860301,-18.386891348495,3.77003198860249));
#222963=CARTESIAN_POINT('',(54.6058629360811,18.0763596539235,3.77003198860276));
#222964=CARTESIAN_POINT('',(-57.6166602460947,-18.3863402754567,3.77003198902533));
#222965=CARTESIAN_POINT('Origin',(5.49031038273072E-15,1.82930781209959E-13,
3.77003198860263));
#222966=CARTESIAN_POINT('',(-59.090661591717,-12.8852923618019,3.77003198882077));
#222967=CARTESIAN_POINT('Origin',(5.49031038273072E-15,1.82930781209959E-13,
3.77003198860263));
#222968=CARTESIAN_POINT('',(-59.0907848292983,-12.8847271885945,3.77003198860253));
#222969=CARTESIAN_POINT('Origin',(5.49031038273072E-15,1.82930781209959E-13,
3.77003198860263));
#222970=CARTESIAN_POINT('',(-58.6269798078532,-12.786142387925,3.77003198860253));
#222971=CARTESIAN_POINT('Origin',(5.49031038273072E-15,1.82930781209959E-13,
3.77003198860263));
#222972=CARTESIAN_POINT('',(-57.7713971777986,-18.4366189870675,3.48823028058468));
#222973=CARTESIAN_POINT('',(-57.616660245397,-18.386340275234,3.77003198860249));
#222974=CARTESIAN_POINT('',(-59.2498070619041,-12.919118186265,3.48823028074795));
#222975=CARTESIAN_POINT('Origin',(5.52999282761009E-15,1.84898592019556E-13,
3.48823028058481));
#222976=CARTESIAN_POINT('',(-59.2498070616278,-12.9191181862048,3.48823028058471));
#222977=CARTESIAN_POINT('Origin',(60.71525,1.85785428279622E-13,3.36123028058482));
#222978=CARTESIAN_POINT('',(-59.4650964698965,-12.9642895838873,3.36123028058472));
#222979=CARTESIAN_POINT('',(-57.9804289733662,-18.5051441132844,3.36123028058468));
#222980=CARTESIAN_POINT('Origin',(5.5478765747851E-15,1.85785428279622E-13,
3.36123028058482));
#222981=CARTESIAN_POINT('',(-58.1242364370955,-18.5518699907153,3.36123028058468));
#222982=CARTESIAN_POINT('',(54.8193466381475,18.1457247135496,3.36123028058495));
#222983=CARTESIAN_POINT('',(-59.6130003254554,-12.9957275188826,3.36123028058472));
#222984=CARTESIAN_POINT('Origin',(5.5478765747851E-15,1.85785428279622E-13,
3.36123028058482));
#222985=CARTESIAN_POINT('',(-59.4656149121213,-12.964399782184,3.36123028058472));
#222986=CARTESIAN_POINT('Origin',(5.5478765747851E-15,1.85785428279622E-13,
3.36123028058482));
#222987=CARTESIAN_POINT('',(-59.8282880397054,-13.0409063549241,3.48823028058474));
#222988=CARTESIAN_POINT('',(-58.33327048504,-18.6203878281982,3.48823028042681));
#222989=CARTESIAN_POINT('Origin',(5.52999282761008E-15,1.84898592019556E-13,
3.48823028058484));
#222990=CARTESIAN_POINT('',(-58.4880082803367,-18.6706636022911,3.77003198802693));
#222991=CARTESIAN_POINT('',(-58.3332704847794,-18.620387828115,3.4882302805847));
#222992=CARTESIAN_POINT('',(-58.4881809372196,-18.6701227271413,3.77003198860249));
#222993=CARTESIAN_POINT('Origin',(5.49031038273072E-15,1.82930781209959E-13,
3.77003198860263));
#222994=CARTESIAN_POINT('',(-59.9873118763435,-13.0752898951328,3.77003198860253));
#222995=CARTESIAN_POINT('Origin',(5.49031038273072E-15,1.82930781209959E-13,
3.77003198860263));
#222996=CARTESIAN_POINT('',(-59.9874327886717,-13.0747351550713,3.7700319880271));
#222997=CARTESIAN_POINT('Origin',(5.49031038273072E-15,1.82930781209959E-13,
3.77003198860263));
#222998=CARTESIAN_POINT('',(-59.9874327889996,-13.074735155127,3.77003198860253));
#222999=CARTESIAN_POINT('Origin',(62.2224557307631,1.82930781209959E-13,
3.77003198860263));
#223000=CARTESIAN_POINT('',(-58.9396512752212,-18.8168143322229,3.77003198860249));
#223001=CARTESIAN_POINT('',(56.1826270286323,18.5886813639062,3.77003198860276));
#223002=CARTESIAN_POINT('',(-60.4516424606488,-13.1739864076109,3.77003198860253));
#223003=CARTESIAN_POINT('Origin',(5.49031038273072E-15,1.82930781209959E-13,
3.77003198860263));
#223004=CARTESIAN_POINT('',(-59.987825810305,-13.0753991351686,3.77003198860253));
#223005=CARTESIAN_POINT('Origin',(5.57972911860581E-15,1.8736496251029E-13,
3.13503198860263));
#223006=CARTESIAN_POINT('Origin',(-57.1650144220515,-18.2401946149528,3.13502491541416));
#223007=CARTESIAN_POINT('Origin',(-58.6264520046767,-12.7860353045052,3.13502491541418));
#223008=CARTESIAN_POINT('Origin',(5.57972911860581E-15,1.8736496251029E-13,
3.13503198860263));
#223009=CARTESIAN_POINT('Origin',(-58.9759248679613,-18.8285650740585,3.20381846780257));
#223010=CARTESIAN_POINT('Origin',(-60.4889312852508,-13.1819466778333,3.20382022872411));
#223011=CARTESIAN_POINT('Origin',(5.51210908043506E-15,1.8401175575949E-13,
3.61523028058481));
#223012=CARTESIAN_POINT('Origin',(-58.1393085451926,-18.556806216885,3.58786945046721));
#223013=CARTESIAN_POINT('Origin',(-59.6284292050451,-12.9989693492946,3.58781461834119));
#223014=CARTESIAN_POINT('Origin',(5.51210908043507E-15,1.8401175575949E-13,
3.61523028058481));
#223015=CARTESIAN_POINT('Origin',(-57.9654487055678,-18.5002290260137,3.58781440266419));
#223016=CARTESIAN_POINT('Origin',(-59.4495735695182,-12.9610367308095,3.58786923593005));
#223017=CARTESIAN_POINT('Origin',(60.4792282238308,1.82930781209959E-13,
3.77003198860263));
#223018=CARTESIAN_POINT('',(-59.6417962403142,-6.58785426247119,3.77003198860258));
#223019=CARTESIAN_POINT('',(-58.7584778814675,-12.1649068885794,3.77003198860253));
#223020=CARTESIAN_POINT('Origin',(5.49031038273072E-15,1.82930781209959E-13,
3.77003198860263));
#223021=CARTESIAN_POINT('',(-59.2228087529787,-12.2636034620792,3.77003198860253));
#223022=CARTESIAN_POINT('',(57.7988642628859,12.6101209950216,3.77003198860272));
#223023=CARTESIAN_POINT('',(-59.2229260468455,-12.2630370254944,3.7700319890253));
#223024=CARTESIAN_POINT('Origin',(5.49031038273072E-15,1.82930781209959E-13,
3.77003198860263));
#223025=CARTESIAN_POINT('',(-60.1138365740932,-6.63804933238242,3.77003198882081));
#223026=CARTESIAN_POINT('Origin',(5.49031038273072E-15,1.82930781209959E-13,
3.77003198860263));
#223027=CARTESIAN_POINT('',(-60.1139000598793,-6.63747437341801,3.77003198860257));
#223028=CARTESIAN_POINT('Origin',(5.49031038273072E-15,1.82930781209959E-13,
3.77003198860263));
#223029=CARTESIAN_POINT('',(-59.6423308931549,-6.58791045674914,3.77003198860258));
#223030=CARTESIAN_POINT('Origin',(5.49031038273072E-15,1.82930781209959E-13,
3.77003198860263));
#223031=CARTESIAN_POINT('',(-59.382070869907,-12.2968658913806,3.48823028058472));
#223032=CARTESIAN_POINT('',(-59.2229260461284,-12.2630370253459,3.77003198860253));
#223033=CARTESIAN_POINT('',(-60.2756459901929,-6.65505462400522,3.48823028074799));
#223034=CARTESIAN_POINT('Origin',(5.52999282761009E-15,1.84898592019556E-13,
3.48823028058481));
#223035=CARTESIAN_POINT('',(-60.2756459899118,-6.65505462397419,3.48823028058476));
#223036=CARTESIAN_POINT('Origin',(60.71525,1.85785428279622E-13,3.36123028058482));
#223037=CARTESIAN_POINT('',(-60.4944777170593,-6.67747469700969,3.36123028058476));
#223038=CARTESIAN_POINT('',(-59.5971203935658,-12.3431658574213,3.36123028058472));
#223039=CARTESIAN_POINT('Origin',(5.5478765747851E-15,1.85785428279622E-13,
3.36123028058482));
#223040=CARTESIAN_POINT('',(-59.7450242491247,-12.3746037924167,3.36123028058472));
#223041=CARTESIAN_POINT('',(58.0246834617327,12.6581203474876,3.36123028058491));
#223042=CARTESIAN_POINT('',(-60.6448574988554,-6.69328024897478,3.36123028058476));
#223043=CARTESIAN_POINT('Origin',(5.5478765747851E-15,1.85785428279622E-13,
3.36123028058482));
#223044=CARTESIAN_POINT('',(-60.4950048380619,-6.67753009965956,3.36123028058476));
#223045=CARTESIAN_POINT('Origin',(5.5478765747851E-15,1.85785428279622E-13,
3.36123028058482));
#223046=CARTESIAN_POINT('',(-60.8636883187844,-6.71570789669434,3.48823028058479));
#223047=CARTESIAN_POINT('',(-59.9600752509414,-12.4208962742144,3.48823028042685));
#223048=CARTESIAN_POINT('Origin',(5.52999282761008E-15,1.84898592019556E-13,
3.48823028058484));
#223049=CARTESIAN_POINT('',(-60.1192206258106,-12.4547221284046,3.77003198802697));
#223050=CARTESIAN_POINT('',(-59.9600752506736,-12.4208962741589,3.48823028058475));
#223051=CARTESIAN_POINT('',(-60.1193358000127,-12.4541661686668,3.77003198860253));
#223052=CARTESIAN_POINT('Origin',(5.49031038273072E-15,1.82930781209959E-13,
3.77003198860263));
#223053=CARTESIAN_POINT('',(-61.0254350648262,-6.73328056300543,3.77003198860258));
#223054=CARTESIAN_POINT('Origin',(5.49031038273072E-15,1.82930781209959E-13,
3.77003198860263));
#223055=CARTESIAN_POINT('',(-61.0254973286579,-6.73271622308821,3.77003198802715));
#223056=CARTESIAN_POINT('Origin',(5.49031038273072E-15,1.82930781209959E-13,
3.77003198860263));
#223057=CARTESIAN_POINT('',(-61.0254973289898,-6.73271622310933,3.77003198860258));
#223058=CARTESIAN_POINT('Origin',(62.2224557307631,1.82930781209959E-13,
3.77003198860263));
#223059=CARTESIAN_POINT('',(-60.5836663843181,-12.552862681145,3.77003198860253));
#223060=CARTESIAN_POINT('',(59.4667368016499,12.9646382471652,3.77003198860272));
#223061=CARTESIAN_POINT('',(-61.4975385923862,-6.78290064323585,3.77003198860257));
#223062=CARTESIAN_POINT('Origin',(5.49031038273072E-15,1.82930781209959E-13,
3.77003198860263));
#223063=CARTESIAN_POINT('',(-61.0259576020967,-6.73333548388565,3.77003198860257));
#223064=CARTESIAN_POINT('Origin',(5.57972911860581E-15,1.8736496251029E-13,
3.13503198860263));
#223065=CARTESIAN_POINT('Origin',(-58.7584780045773,-12.1649018101387,3.13502491541424));
#223066=CARTESIAN_POINT('Origin',(-59.6417947880741,-6.58785913039848,3.13502491541428));
#223067=CARTESIAN_POINT('Origin',(5.57972911860581E-15,1.8736496251029E-13,
3.13503198860263));
#223068=CARTESIAN_POINT('Origin',(-60.620969553509,-12.5607574282782,3.20381846780322));
#223069=CARTESIAN_POINT('Origin',(-61.5354552197175,-6.78691956273327,3.20382022872119));
#223070=CARTESIAN_POINT('Origin',(5.51210908043506E-15,1.8401175575949E-13,
3.61523028058481));
#223071=CARTESIAN_POINT('Origin',(-59.7605297667716,-12.3779375131251,3.58786945046874));
#223072=CARTESIAN_POINT('Origin',(-60.6605407209804,-6.69489156322718,3.58781461833949));
#223073=CARTESIAN_POINT('Origin',(5.51210908043507E-15,1.8401175575949E-13,
3.61523028058481));
#223074=CARTESIAN_POINT('Origin',(-59.5817084227228,-12.3398435598866,3.58781440266546));
#223075=CARTESIAN_POINT('Origin',(-60.4786998370192,-6.67586224832366,3.58786923592885));
#223076=CARTESIAN_POINT('Origin',(60.4792282238308,1.82930781209959E-13,
3.77003198860263));
#223077=CARTESIAN_POINT('',(-60.003690522373,-0.317499999999817,3.77003198860262));
#223078=CARTESIAN_POINT('',(-59.7081718144892,-5.95633285891234,3.77003198860258));
#223079=CARTESIAN_POINT('Origin',(5.49031038273072E-15,1.82930781209959E-13,
3.77003198860263));
#223080=CARTESIAN_POINT('',(-60.1802756340603,-6.00595296980896,3.77003198860258));
#223081=CARTESIAN_POINT('',(59.785232315514,6.60293000146494,3.77003198860268));
#223082=CARTESIAN_POINT('',(-60.1803330766332,-6.00537737567535,3.77003198902537));
#223083=CARTESIAN_POINT('Origin',(5.49031038273072E-15,1.82930781209959E-13,
3.77003198860263));
#223084=CARTESIAN_POINT('',(-60.4783917833346,-0.318078445375805,3.77003198882085));
#223085=CARTESIAN_POINT('Origin',(5.49031038273072E-15,1.82930781209959E-13,
3.77003198860263));
#223086=CARTESIAN_POINT('',(-60.478394821762,-0.317500000025102,3.77003198860262));
#223087=CARTESIAN_POINT('Origin',(5.49031038273072E-15,1.82930781209959E-13,
3.77003198860263));
#223088=CARTESIAN_POINT('',(-60.004228120231,-0.317499999999817,3.77003198860262));
#223089=CARTESIAN_POINT('Origin',(5.49031038273072E-15,1.82930781209959E-13,
3.77003198860263));
#223090=CARTESIAN_POINT('',(-60.3421421670675,-6.02238575970299,3.48823028058476));
#223091=CARTESIAN_POINT('',(-60.1803330759045,-6.00537737560264,3.77003198860258));
#223092=CARTESIAN_POINT('',(-60.6410923275232,-0.318076890624665,3.48823028074803));
#223093=CARTESIAN_POINT('Origin',(5.52999282761009E-15,1.84898592019556E-13,
3.48823028058481));
#223094=CARTESIAN_POINT('',(-60.6410923272405,-0.318076890623182,3.4882302805848));
#223095=CARTESIAN_POINT('Origin',(60.71525,1.85785428279622E-13,3.36123028058482));
#223096=CARTESIAN_POINT('',(-60.8610688070707,-0.317499999999814,3.36123028058481));
#223097=CARTESIAN_POINT('',(-60.5608532912343,-6.04595329345084,3.36123028058477));
#223098=CARTESIAN_POINT('Origin',(5.5478765747851E-15,1.85785428279622E-13,
3.36123028058482));
#223099=CARTESIAN_POINT('',(-60.7112330730303,-6.06175884541593,3.36123028058477));
#223100=CARTESIAN_POINT('',(60.0186752706391,6.62746584474152,3.36123028058487));
#223101=CARTESIAN_POINT('',(-61.0122769227456,-0.317499999999814,3.36123028058481));
#223102=CARTESIAN_POINT('Origin',(5.5478765747851E-15,1.85785428279622E-13,
3.36123028058482));
#223103=CARTESIAN_POINT('',(-60.8615988316031,-0.317499999999814,3.36123028058481));
#223104=CARTESIAN_POINT('Origin',(5.5478765747851E-15,1.85785428279622E-13,
3.36123028058482));
#223105=CARTESIAN_POINT('',(-61.2322532920972,-0.316930737395729,3.48823028058483));
#223106=CARTESIAN_POINT('',(-60.9299448849411,-6.08531878141062,3.4882302804269));
#223107=CARTESIAN_POINT('Origin',(5.52999282761008E-15,1.84898592019556E-13,
3.48823028058484));
#223108=CARTESIAN_POINT('',(-61.0917542093523,-6.10232411256111,3.77003198802702));
#223109=CARTESIAN_POINT('',(-60.929944884669,-6.08531878138344,3.48823028058479));
#223110=CARTESIAN_POINT('',(-61.0918106390011,-6.10175915944657,3.77003198860258));
#223111=CARTESIAN_POINT('Origin',(5.49031038273072E-15,1.82930781209959E-13,
3.77003198860263));
#223112=CARTESIAN_POINT('',(-61.3949508163453,-0.317499999999817,3.77003198860262));
#223113=CARTESIAN_POINT('Origin',(5.49031038273072E-15,1.82930781209959E-13,
3.77003198860263));
#223114=CARTESIAN_POINT('',(-61.394953749505,-0.316932243253074,3.77003198802719));
#223115=CARTESIAN_POINT('Origin',(5.49031038273072E-15,1.82930781209959E-13,
3.77003198860263));
#223116=CARTESIAN_POINT('',(-61.3949537498373,-0.316932243239378,3.77003198860262));
#223117=CARTESIAN_POINT('Origin',(62.2224557307631,1.82930781209959E-13,
3.77003198860263));
#223118=CARTESIAN_POINT('',(-61.5639141665611,-6.151379239677,3.77003198860258));
#223119=CARTESIAN_POINT('',(61.5094129706996,6.78414869068811,3.77003198860268));
#223120=CARTESIAN_POINT('',(-61.8696548221181,-0.317499999999817,3.77003198860262));
#223121=CARTESIAN_POINT('Origin',(5.49031038273072E-15,1.82930781209959E-13,
3.77003198860263));
#223122=CARTESIAN_POINT('',(-61.3954762318973,-0.317499999999817,3.77003198860261));
#223123=CARTESIAN_POINT('Origin',(5.57972911860581E-15,1.8736496251029E-13,
3.13503198860263));
#223124=CARTESIAN_POINT('Origin',(-59.7081714060829,-5.95632779542337,3.1350249154143));
#223125=CARTESIAN_POINT('Origin',(-60.0036895869254,-0.317504993060535,
3.13502491541431));
#223126=CARTESIAN_POINT('Origin',(5.57972911860581E-15,1.8736496251029E-13,
3.13503198860263));
#223127=CARTESIAN_POINT('Origin',(-61.6018382108717,-6.1553314956104,3.20381846779944));
#223128=CARTESIAN_POINT('Origin',(-61.9077838296769,-0.317533536648401,
3.20382022872143));
#223129=CARTESIAN_POINT('Origin',(5.51210908043506E-15,1.8401175575949E-13,
3.61523028058481));
#223130=CARTESIAN_POINT('Origin',(-60.7270021185311,-6.06345353572164,3.58786945047009));
#223131=CARTESIAN_POINT('Origin',(-61.0280426587404,-0.317463144196334,
3.58781461834189));
#223132=CARTESIAN_POINT('Origin',(5.51210908043507E-15,1.8401175575949E-13,
3.61523028058481));
#223133=CARTESIAN_POINT('Origin',(-60.5451784741226,-6.04426018543762,3.5878144026621));
#223134=CARTESIAN_POINT('Origin',(-60.845208813124,-0.317545622030571,3.5878692359272));
#223135=CARTESIAN_POINT('Origin',(60.4792282238308,1.82930781209959E-13,
3.77003198860263));
#223136=CARTESIAN_POINT('',(-59.7081718144893,5.95633285891189,3.77003198860266));
#223137=CARTESIAN_POINT('',(-60.003690522373,0.317500000000183,3.77003198860262));
#223138=CARTESIAN_POINT('Origin',(5.49031038273072E-15,1.82930781209959E-13,
3.77003198860263));
#223139=CARTESIAN_POINT('',(-60.4783948217626,0.317500000025444,3.77003198860262));
#223140=CARTESIAN_POINT('',(60.4792282238308,0.317500000000183,3.77003198860264));
#223141=CARTESIAN_POINT('',(-60.4783917836893,0.318078445378037,3.77003198902564));
#223142=CARTESIAN_POINT('Origin',(5.49031038273072E-15,1.82930781209959E-13,
3.77003198860263));
#223143=CARTESIAN_POINT('',(-60.1803330762807,6.00537737563972,3.7700319888209));
#223144=CARTESIAN_POINT('Origin',(5.49031038273072E-15,1.82930781209959E-13,
3.77003198860263));
#223145=CARTESIAN_POINT('',(-60.1802756340597,6.00595296980842,3.77003198860266));
#223146=CARTESIAN_POINT('Origin',(5.49031038273072E-15,1.82930781209959E-13,
3.77003198860263));
#223147=CARTESIAN_POINT('',(-59.7087064673299,5.95638905318984,3.77003198860266));
#223148=CARTESIAN_POINT('Origin',(5.49031038273072E-15,1.82930781209959E-13,
3.77003198860263));
#223149=CARTESIAN_POINT('',(-60.6410923272405,0.318076890623551,3.48823028058481));
#223150=CARTESIAN_POINT('',(-60.4783917829566,0.318078445374188,3.77003198860262));
#223151=CARTESIAN_POINT('',(-60.3421421673489,6.02238575973063,3.48823028074808));
#223152=CARTESIAN_POINT('Origin',(5.52999282761009E-15,1.84898592019556E-13,
3.48823028058481));
#223153=CARTESIAN_POINT('',(-60.3421421670675,6.02238575970255,3.48823028058485));
#223154=CARTESIAN_POINT('Origin',(60.71525,1.85785428279622E-13,3.36123028058482));
#223155=CARTESIAN_POINT('',(-60.5608532912344,6.04595329345039,3.36123028058485));
#223156=CARTESIAN_POINT('',(-60.8610688070707,0.317500000000186,3.36123028058481));
#223157=CARTESIAN_POINT('Origin',(5.5478765747851E-15,1.85785428279622E-13,
3.36123028058482));
#223158=CARTESIAN_POINT('',(-61.0122769227456,0.317500000000186,3.36123028058481));
#223159=CARTESIAN_POINT('',(60.71525,0.317500000000186,3.36123028058483));
#223160=CARTESIAN_POINT('',(-60.7112330730304,6.06175884541548,3.36123028058485));
#223161=CARTESIAN_POINT('Origin',(5.5478765747851E-15,1.85785428279622E-13,
3.36123028058482));
#223162=CARTESIAN_POINT('',(-60.5613804122369,6.04600869610026,3.36123028058485));
#223163=CARTESIAN_POINT('Origin',(5.5478765747851E-15,1.85785428279622E-13,
3.36123028058482));
#223164=CARTESIAN_POINT('',(-60.9299448846691,6.08531878138299,3.48823028058487));
#223165=CARTESIAN_POINT('',(-61.2322532923707,0.316930737397515,3.48823028042694));
#223166=CARTESIAN_POINT('Origin',(5.52999282761008E-15,1.84898592019556E-13,
3.48823028058484));
#223167=CARTESIAN_POINT('',(-61.3949537495049,0.316932243253443,3.77003198802707));
#223168=CARTESIAN_POINT('',(-61.2322532920972,0.316930737396099,3.48823028058484));
#223169=CARTESIAN_POINT('',(-61.3949508163453,0.317500000000183,3.77003198860262));
#223170=CARTESIAN_POINT('Origin',(5.49031038273072E-15,1.82930781209959E-13,
3.77003198860263));
#223171=CARTESIAN_POINT('',(-61.0918106390012,6.10175915944611,3.77003198860266));
#223172=CARTESIAN_POINT('Origin',(5.49031038273072E-15,1.82930781209959E-13,
3.77003198860263));
#223173=CARTESIAN_POINT('',(-61.0917542093524,6.10232411256066,3.77003198802724));
#223174=CARTESIAN_POINT('Origin',(5.49031038273072E-15,1.82930781209959E-13,
3.77003198860263));
#223175=CARTESIAN_POINT('',(-61.0917542096815,6.10232411260902,3.77003198860266));
#223176=CARTESIAN_POINT('Origin',(62.2224557307631,1.82930781209959E-13,
3.77003198860263));
#223177=CARTESIAN_POINT('',(-61.8696548221181,0.317500000000183,3.77003198860262));
#223178=CARTESIAN_POINT('',(62.2224557307631,0.317500000000183,3.77003198860264));
#223179=CARTESIAN_POINT('',(-61.5639141665612,6.15137923967653,3.77003198860266));
#223180=CARTESIAN_POINT('Origin',(5.49031038273072E-15,1.82930781209959E-13,
3.77003198860263));
#223181=CARTESIAN_POINT('',(-61.0923331762718,6.10181408032633,3.77003198860266));
#223182=CARTESIAN_POINT('Origin',(5.57972911860581E-15,1.8736496251029E-13,
3.13503198860263));
#223183=CARTESIAN_POINT('Origin',(-60.0036895869254,0.317504993060735,3.13502491541433));
#223184=CARTESIAN_POINT('Origin',(-59.708171406083,5.95632779542278,3.13502491541439));
#223185=CARTESIAN_POINT('Origin',(5.57972911860581E-15,1.8736496251029E-13,
3.13503198860263));
#223186=CARTESIAN_POINT('Origin',(-61.9077842377855,0.317533537011735,3.20381846780048));
#223187=CARTESIAN_POINT('Origin',(-61.6018378049612,6.15533145331065,3.2038202287209));
#223188=CARTESIAN_POINT('Origin',(5.51210908043506E-15,1.8401175575949E-13,
3.61523028058481));
#223189=CARTESIAN_POINT('Origin',(-61.0281367271391,0.317462907478675,3.58786945046904));
#223190=CARTESIAN_POINT('Origin',(-60.7269085901933,6.06344346747484,3.58781461834164));
#223191=CARTESIAN_POINT('Origin',(5.51210908043507E-15,1.8401175575949E-13,
3.61523028058481));
#223192=CARTESIAN_POINT('Origin',(-60.8453028802703,0.317545368445655,3.58781440266595));
#223193=CARTESIAN_POINT('Origin',(-60.5450849487958,6.0442501005477,3.587869235929));
#223194=CARTESIAN_POINT('Origin',(60.4792282238308,1.82930781209959E-13,
3.77003198860263));
#223195=CARTESIAN_POINT('',(-58.7584778814677,12.164906888579,3.77003198860271));
#223196=CARTESIAN_POINT('',(-59.6417962403143,6.58785426247075,3.77003198860266));
#223197=CARTESIAN_POINT('Origin',(5.49031038273072E-15,1.82930781209959E-13,
3.77003198860263));
#223198=CARTESIAN_POINT('',(-60.1139000598801,6.63747437341761,3.77003198860266));
#223199=CARTESIAN_POINT('',(59.8516078896891,-5.97140859790491,3.77003198860259));
#223200=CARTESIAN_POINT('',(-60.1138365744456,6.63804933242088,3.77003198902554));
#223201=CARTESIAN_POINT('Origin',(5.49031038273072E-15,1.82930781209959E-13,
3.77003198860263));
#223202=CARTESIAN_POINT('',(-59.2229260464987,12.2630370254221,3.77003198882094));
#223203=CARTESIAN_POINT('Origin',(5.49031038273072E-15,1.82930781209959E-13,
3.77003198860263));
#223204=CARTESIAN_POINT('',(-59.2228087529783,12.2636034620787,3.7700319886027));
#223205=CARTESIAN_POINT('Origin',(5.49031038273072E-15,1.82930781209959E-13,
3.77003198860263));
#223206=CARTESIAN_POINT('',(-58.7590037315226,12.1650186614586,3.77003198860271));
#223207=CARTESIAN_POINT('Origin',(5.49031038273072E-15,1.82930781209959E-13,
3.77003198860263));
#223208=CARTESIAN_POINT('',(-60.2756459899119,6.65505462397374,3.48823028058485));
#223209=CARTESIAN_POINT('',(-60.1138365737176,6.63804933234049,3.77003198860266));
#223210=CARTESIAN_POINT('',(-59.382070870184,12.2968658914375,3.48823028074812));
#223211=CARTESIAN_POINT('Origin',(5.52999282761009E-15,1.84898592019556E-13,
3.48823028058481));
#223212=CARTESIAN_POINT('',(-59.3820708699071,12.2968658913801,3.48823028058489));
#223213=CARTESIAN_POINT('Origin',(60.71525,1.85785428279622E-13,3.36123028058482));
#223214=CARTESIAN_POINT('',(-59.597120393566,12.3431658574209,3.3612302805849));
#223215=CARTESIAN_POINT('',(-60.4944777170594,6.67747469700925,3.36123028058485));
#223216=CARTESIAN_POINT('Origin',(5.5478765747851E-15,1.85785428279622E-13,
3.36123028058482));
#223217=CARTESIAN_POINT('',(-60.6448574988555,6.69328024897434,3.36123028058485));
#223218=CARTESIAN_POINT('',(60.0850508448142,-5.99594444118149,3.36123028058478));
#223219=CARTESIAN_POINT('',(-59.7450242491248,12.3746037924162,3.3612302805849));
#223220=CARTESIAN_POINT('Origin',(5.5478765747851E-15,1.85785428279622E-13,
3.36123028058482));
#223221=CARTESIAN_POINT('',(-59.5976388357907,12.3432760557176,3.3612302805849));
#223222=CARTESIAN_POINT('Origin',(5.5478765747851E-15,1.85785428279622E-13,
3.36123028058482));
#223223=CARTESIAN_POINT('',(-59.9600752506738,12.4208962741584,3.48823028058492));
#223224=CARTESIAN_POINT('',(-60.8636883190563,6.71570789672388,3.48823028042699));
#223225=CARTESIAN_POINT('Origin',(5.52999282761008E-15,1.84898592019556E-13,
3.48823028058484));
#223226=CARTESIAN_POINT('',(-61.0254973286579,6.73271622308775,3.77003198802711));
#223227=CARTESIAN_POINT('',(-60.8636883187845,6.71570789669389,3.48823028058488));
#223228=CARTESIAN_POINT('',(-61.0254350648263,6.73328056300497,3.77003198860266));
#223229=CARTESIAN_POINT('Origin',(5.49031038273072E-15,1.82930781209959E-13,
3.77003198860263));
#223230=CARTESIAN_POINT('',(-60.1193358000129,12.4541661686664,3.77003198860271));
#223231=CARTESIAN_POINT('Origin',(5.49031038273072E-15,1.82930781209959E-13,
3.77003198860263));
#223232=CARTESIAN_POINT('',(-60.1192206258108,12.4547221284042,3.77003198802728));
#223233=CARTESIAN_POINT('Origin',(5.49031038273072E-15,1.82930781209959E-13,
3.77003198860263));
#223234=CARTESIAN_POINT('',(-60.119220626133,12.4547221284867,3.77003198860271));
#223235=CARTESIAN_POINT('Origin',(62.2224557307631,1.82930781209959E-13,
3.77003198860263));
#223236=CARTESIAN_POINT('',(-61.4975385923863,6.78290064323539,3.77003198860267));
#223237=CARTESIAN_POINT('',(61.5757885448748,-6.15262728712807,3.77003198860259));
#223238=CARTESIAN_POINT('',(-60.5836663843182,12.5528626811445,3.77003198860271));
#223239=CARTESIAN_POINT('Origin',(5.49031038273072E-15,1.82930781209959E-13,
3.77003198860263));
#223240=CARTESIAN_POINT('',(-60.1198497339744,12.4542754087021,3.77003198860271));
#223241=CARTESIAN_POINT('Origin',(5.57972911860581E-15,1.8736496251029E-13,
3.13503198860263));
#223242=CARTESIAN_POINT('Origin',(-59.6417947880742,6.58785913039789,3.13502491541435));
#223243=CARTESIAN_POINT('Origin',(-58.7584780045775,12.1649018101381,3.1350249154144));
#223244=CARTESIAN_POINT('Origin',(5.57972911860581E-15,1.8736496251029E-13,
3.13503198860263));
#223245=CARTESIAN_POINT('Origin',(-61.5354556255549,6.78691960575353,3.20381846780464));
#223246=CARTESIAN_POINT('Origin',(-60.620969154241,12.5607573437829,3.20382022872046));
#223247=CARTESIAN_POINT('Origin',(5.51210908043506E-15,1.8401175575949E-13,
3.61523028058481));
#223248=CARTESIAN_POINT('Origin',(-60.6606342988042,6.69490116063041,3.5878694504714));
#223249=CARTESIAN_POINT('Origin',(-59.760437803209,12.3779177236595,3.58781461834269));
#223250=CARTESIAN_POINT('Origin',(5.51210908043507E-15,1.8401175575949E-13,
3.61523028058481));
#223251=CARTESIAN_POINT('Origin',(-60.4787934153616,6.67587182882183,3.58781440266543));
#223252=CARTESIAN_POINT('Origin',(-59.5816164638928,12.3398237541834,3.58786923592735));
#223253=CARTESIAN_POINT('Origin',(60.4792282238308,1.82930781209959E-13,
3.77003198860263));
#223254=CARTESIAN_POINT('',(-57.1650137687748,18.2401996527044,3.77003198860275));
#223255=CARTESIAN_POINT('',(-58.6264539577984,12.7860306150449,3.77003198860271));
#223256=CARTESIAN_POINT('Origin',(5.49031038273072E-15,1.82930781209959E-13,
3.77003198860263));
#223257=CARTESIAN_POINT('',(-59.0907848292991,12.8847271885942,3.77003198860271));
#223258=CARTESIAN_POINT('',(57.9308881865556,-11.9889972685545,3.77003198860255));
#223259=CARTESIAN_POINT('',(-59.090661592063,12.8852923618769,3.77003198902532));
#223260=CARTESIAN_POINT('Origin',(5.49031038273072E-15,1.82930781209959E-13,
3.77003198860263));
#223261=CARTESIAN_POINT('',(-57.6166602457573,18.3863402753485,3.77003198882099));
#223262=CARTESIAN_POINT('Origin',(5.49031038273072E-15,1.82930781209959E-13,
3.77003198860263));
#223263=CARTESIAN_POINT('',(-57.6164843860298,18.3868913484944,3.77003198860275));
#223264=CARTESIAN_POINT('Origin',(5.49031038273072E-15,1.82930781209959E-13,
3.77003198860263));
#223265=CARTESIAN_POINT('',(-57.1655250547207,18.2403657795786,3.77003198860275));
#223266=CARTESIAN_POINT('Origin',(5.49031038273072E-15,1.82930781209959E-13,
3.77003198860263));
#223267=CARTESIAN_POINT('',(-59.249807061628,12.9191181862044,3.48823028058489));
#223268=CARTESIAN_POINT('',(-59.0906615913478,12.8852923617209,3.77003198860271));
#223269=CARTESIAN_POINT('',(-57.7713971780681,18.4366189871531,3.48823028074816));
#223270=CARTESIAN_POINT('Origin',(5.52999282761009E-15,1.84898592019556E-13,
3.48823028058481));
#223271=CARTESIAN_POINT('',(-57.7713971777988,18.4366189870671,3.48823028058493));
#223272=CARTESIAN_POINT('Origin',(60.71525,1.85785428279622E-13,3.36123028058482));
#223273=CARTESIAN_POINT('',(-57.9804289733665,18.505144113284,3.36123028058494));
#223274=CARTESIAN_POINT('',(-59.4650964698967,12.9642895838869,3.3612302805849));
#223275=CARTESIAN_POINT('Origin',(5.5478765747851E-15,1.85785428279622E-13,
3.36123028058482));
#223276=CARTESIAN_POINT('',(-59.6130003254556,12.9957275188822,3.3612302805849));
#223277=CARTESIAN_POINT('',(58.1567073854023,-12.0369966210205,3.36123028058474));
#223278=CARTESIAN_POINT('',(-58.1242364370958,18.5518699907149,3.36123028058494));
#223279=CARTESIAN_POINT('Origin',(5.5478765747851E-15,1.85785428279622E-13,
3.36123028058482));
#223280=CARTESIAN_POINT('',(-57.9809330566518,18.5053078998719,3.36123028058494));
#223281=CARTESIAN_POINT('Origin',(5.5478765747851E-15,1.85785428279622E-13,
3.36123028058482));
#223282=CARTESIAN_POINT('',(-58.3332704847797,18.6203878281146,3.48823028058496));
#223283=CARTESIAN_POINT('',(-59.8282880399728,13.0409063549819,3.48823028042702));
#223284=CARTESIAN_POINT('Origin',(5.52999282761008E-15,1.84898592019556E-13,
3.48823028058484));
#223285=CARTESIAN_POINT('',(-59.9874327886718,13.0747351550709,3.77003198802716));
#223286=CARTESIAN_POINT('',(-59.8282880397056,13.0409063549237,3.48823028058492));
#223287=CARTESIAN_POINT('',(-59.9873118763436,13.0752898951323,3.77003198860271));
#223288=CARTESIAN_POINT('Origin',(5.49031038273072E-15,1.82930781209959E-13,
3.77003198860263));
#223289=CARTESIAN_POINT('',(-58.4881809372199,18.6701227271409,3.77003198860275));
#223290=CARTESIAN_POINT('Origin',(5.49031038273072E-15,1.82930781209959E-13,
3.77003198860263));
#223291=CARTESIAN_POINT('',(-58.488008280337,18.6706636022907,3.77003198802732));
#223292=CARTESIAN_POINT('Origin',(5.49031038273072E-15,1.82930781209959E-13,
3.77003198860263));
#223293=CARTESIAN_POINT('',(-58.4880082806488,18.6706636024064,3.77003198860275));
#223294=CARTESIAN_POINT('Origin',(62.2224557307631,1.82930781209959E-13,
3.77003198860263));
#223295=CARTESIAN_POINT('',(-60.451642460649,13.1739864076105,3.77003198860271));
#223296=CARTESIAN_POINT('',(59.5987607253196,-12.3435145206981,3.77003198860255));
#223297=CARTESIAN_POINT('',(-58.9396512752214,18.8168143322225,3.77003198860275));
#223298=CARTESIAN_POINT('Origin',(5.49031038273072E-15,1.82930781209959E-13,
3.77003198860263));
#223299=CARTESIAN_POINT('',(-58.4886806371043,18.6702850894755,3.77003198860275));
#223300=CARTESIAN_POINT('Origin',(5.57972911860581E-15,1.8736496251029E-13,
3.13503198860263));
#223301=CARTESIAN_POINT('Origin',(-58.6264520046769,12.7860353045046,3.13502491541439));
#223302=CARTESIAN_POINT('Origin',(-57.1650144220518,18.2401946149522,3.13502491541442));
#223303=CARTESIAN_POINT('Origin',(5.57972911860581E-15,1.8736496251029E-13,
3.13503198860263));
#223304=CARTESIAN_POINT('Origin',(-60.4889316843638,13.1819467630405,3.20381846779971));
#223305=CARTESIAN_POINT('Origin',(-58.9759244797154,18.8285649482883,3.20382022872347));
#223306=CARTESIAN_POINT('Origin',(5.51210908043506E-15,1.8401175575949E-13,
3.61523028058481));
#223307=CARTESIAN_POINT('Origin',(-59.6285212670405,12.9989886756689,3.58786945046839));
#223308=CARTESIAN_POINT('Origin',(-58.13921915398,18.5567769230188,3.5878146183382));
#223309=CARTESIAN_POINT('Origin',(5.51210908043507E-15,1.8401175575949E-13,
3.61523028058481));
#223310=CARTESIAN_POINT('Origin',(-59.4496656337924,12.9610560404238,3.58781440266355));
#223311=CARTESIAN_POINT('Origin',(-57.9653593207587,18.5001997164983,3.58786923593086));
#223312=CARTESIAN_POINT('Origin',(60.4792282238308,1.82930781209959E-13,
3.77003198860263));
#223313=CARTESIAN_POINT('',(-54.945237802683,24.1156489724276,3.77003198860279));
#223314=CARTESIAN_POINT('',(-56.9687879773467,18.8441205405518,3.77003198860275));
#223315=CARTESIAN_POINT('Origin',(5.49031038273072E-15,1.82930781209959E-13,
3.77003198860263));
#223316=CARTESIAN_POINT('',(-57.4202585945867,18.99081223639,3.77003198860275));
#223317=CARTESIAN_POINT('',(54.8020887275097,-17.472438766075,3.77003198860251));
#223318=CARTESIAN_POINT('',(-57.4200769557625,18.9913614317955,3.77003198902548));
#223319=CARTESIAN_POINT('Origin',(5.49031038273072E-15,1.82930781209959E-13,
3.77003198860263));
#223320=CARTESIAN_POINT('',(-55.3791342583021,24.3081989336292,3.77003198882103));
#223321=CARTESIAN_POINT('Origin',(5.49031038273072E-15,1.82930781209959E-13,
3.77003198860263));
#223322=CARTESIAN_POINT('',(-55.3789017591235,24.3087286055916,3.77003198860279));
#223323=CARTESIAN_POINT('Origin',(5.49031038273072E-15,1.82930781209959E-13,
3.77003198860263));
#223324=CARTESIAN_POINT('',(-54.9457289227642,24.1158676331756,3.77003198860279));
#223325=CARTESIAN_POINT('Origin',(5.49031038273072E-15,1.82930781209959E-13,
3.77003198860263));
#223326=CARTESIAN_POINT('',(-57.5748148483577,19.0416371860876,3.48823028058494));
#223327=CARTESIAN_POINT('',(-57.4200769550674,18.9913614315656,3.77003198860275));
#223328=CARTESIAN_POINT('',(-55.5277679690273,24.3743766271349,3.4882302807482));
#223329=CARTESIAN_POINT('Origin',(5.52999282761009E-15,1.84898592019556E-13,
3.48823028058481));
#223330=CARTESIAN_POINT('',(-55.5277679687684,24.3743766270213,3.48823028058497));
#223331=CARTESIAN_POINT('Origin',(60.71525,1.85785428279622E-13,3.36123028058482));
#223332=CARTESIAN_POINT('',(-55.7284918401499,24.4643761377916,3.36123028058498));
#223333=CARTESIAN_POINT('',(-57.7842031819384,19.1090650011314,3.36123028058494));
#223334=CARTESIAN_POINT('Origin',(5.5478765747851E-15,1.85785428279622E-13,
3.36123028058482));
#223335=CARTESIAN_POINT('',(-57.9280106456677,19.1557908785624,3.36123028058494));
#223336=CARTESIAN_POINT('',(55.0155724295761,-17.5418038257011,3.3612302805847));
#223337=CARTESIAN_POINT('',(-55.8666273273834,24.525878019167,3.36123028058498));
#223338=CARTESIAN_POINT('Origin',(5.5478765747851E-15,1.85785428279622E-13,
3.36123028058482));
#223339=CARTESIAN_POINT('',(-55.728976041654,24.4645917181906,3.36123028058498));
#223340=CARTESIAN_POINT('Origin',(5.5478765747851E-15,1.85785428279622E-13,
3.36123028058482));
#223341=CARTESIAN_POINT('',(-56.0673542004327,24.6158705164592,3.488230280585));
#223342=CARTESIAN_POINT('',(-58.1373965172491,19.2232259142297,3.48823028042707));
#223343=CARTESIAN_POINT('Origin',(5.52999282761008E-15,1.84898592019556E-13,
3.48823028058484));
#223344=CARTESIAN_POINT('',(-58.2921333818757,19.2735045526308,3.7700319880272));
#223345=CARTESIAN_POINT('',(-58.1373965169894,19.2232259141438,3.48823028058497));
#223346=CARTESIAN_POINT('',(-58.2919551457918,19.2740436149883,3.77003198860276));
#223347=CARTESIAN_POINT('Origin',(5.49031038273072E-15,1.82930781209959E-13,
3.77003198860263));
#223348=CARTESIAN_POINT('',(-56.2162173246399,24.6815255140425,3.77003198860279));
#223349=CARTESIAN_POINT('Origin',(5.49031038273072E-15,1.82930781209959E-13,
3.77003198860263));
#223350=CARTESIAN_POINT('',(-56.2159890767413,24.682045378663,3.77003198802737));
#223351=CARTESIAN_POINT('Origin',(5.49031038273072E-15,1.82930781209959E-13,
3.77003198860263));
#223352=CARTESIAN_POINT('',(-56.2159890770393,24.6820453788107,3.77003198860279));
#223353=CARTESIAN_POINT('Origin',(62.2224557307631,1.82930781209959E-13,
3.77003198860263));
#223354=CARTESIAN_POINT('',(-58.7434254837933,19.4207352200699,3.77003198860276));
#223355=CARTESIAN_POINT('',(56.3788528200609,-17.9847604760577,3.77003198860251));
#223356=CARTESIAN_POINT('',(-56.6498810128383,24.8746050278051,3.77003198860279));
#223357=CARTESIAN_POINT('Origin',(5.49031038273072E-15,1.82930781209959E-13,
3.77003198860263));
#223358=CARTESIAN_POINT('',(-56.2166973156307,24.6817392198003,3.77003198860279));
#223359=CARTESIAN_POINT('Origin',(5.57972911860581E-15,1.8736496251029E-13,
3.13503198860263));
#223360=CARTESIAN_POINT('Origin',(-56.9687855447426,18.8441250001653,3.13502491541443));
#223361=CARTESIAN_POINT('Origin',(-54.9452389789698,24.1156440305588,3.13502491541451));
#223362=CARTESIAN_POINT('Origin',(5.57972911860581E-15,1.8736496251029E-13,
3.13503198860263));
#223363=CARTESIAN_POINT('Origin',(-58.7796783495213,19.4325497530908,3.20381846780393));
#223364=CARTESIAN_POINT('Origin',(-56.6847272350798,24.8900828550892,3.2038202287169));
#223365=CARTESIAN_POINT('Origin',(5.51210908043506E-15,1.8401175575949E-13,
3.61523028058481));
#223366=CARTESIAN_POINT('Origin',(-57.9431056782028,19.1606565505631,3.58786945046924));
#223367=CARTESIAN_POINT('Origin',(-55.8810150532822,24.532324191153,3.58781461834167));
#223368=CARTESIAN_POINT('Origin',(5.51210908043507E-15,1.8401175575949E-13,
3.61523028058481));
#223369=CARTESIAN_POINT('Origin',(-57.7691948748981,19.1042362097749,3.58781440266532));
#223370=CARTESIAN_POINT('Origin',(-55.7140215708733,24.4578836192983,3.58786923592957));
#223371=CARTESIAN_POINT('Origin',(60.4792282238308,1.82930781209959E-13,
3.77003198860263));
#223372=CARTESIAN_POINT('',(-52.1234703131948,29.7268821954849,3.77003198860283));
#223373=CARTESIAN_POINT('',(-54.6869600343299,24.6957503380306,3.77003198860279));
#223374=CARTESIAN_POINT('Origin',(5.49031038273072E-15,1.82930781209959E-13,
3.77003198860263));
#223375=CARTESIAN_POINT('',(-55.1206239907504,24.888829971241,3.77003198860279));
#223376=CARTESIAN_POINT('',(50.603004322856,-22.1823620689011,3.77003198860248));
#223377=CARTESIAN_POINT('',(-55.1203859404111,24.8893571716696,3.77003198902569));
#223378=CARTESIAN_POINT('Origin',(5.49031038273072E-15,1.82930781209959E-13,
3.77003198860263));
#223379=CARTESIAN_POINT('',(-52.534862887084,29.9637318775753,3.77003198882107));
#223380=CARTESIAN_POINT('Origin',(5.49031038273072E-15,1.82930781209959E-13,
3.77003198860263));
#223381=CARTESIAN_POINT('',(-52.5345762957639,29.9642343451574,3.77003198860283));
#223382=CARTESIAN_POINT('Origin',(5.49031038273072E-15,1.82930781209959E-13,
3.77003198860263));
#223383=CARTESIAN_POINT('',(-52.1239358865968,29.7271509944138,3.77003198860283));
#223384=CARTESIAN_POINT('Origin',(5.49031038273072E-15,1.82930781209959E-13,
3.77003198860263));
#223385=CARTESIAN_POINT('',(-55.2690209153042,24.9555320242414,3.48823028058498));
#223386=CARTESIAN_POINT('',(-55.1203859397436,24.8893571713681,3.77003198860279));
#223387=CARTESIAN_POINT('',(-52.6757649141853,30.0450834961236,3.48823028074825));
#223388=CARTESIAN_POINT('Origin',(5.52999282761009E-15,1.84898592019556E-13,
3.48823028058481));
#223389=CARTESIAN_POINT('',(-52.6757649139398,30.0450834959835,3.48823028058502));
#223390=CARTESIAN_POINT('Origin',(60.71525,1.85785428279622E-13,3.36123028058482));
#223391=CARTESIAN_POINT('',(-52.8659816883961,30.1555713378337,3.36123028058502));
#223392=CARTESIAN_POINT('',(-55.4702140717968,25.0444775033946,3.36123028058499));
#223393=CARTESIAN_POINT('Origin',(5.5478765747851E-15,1.85785428279622E-13,
3.36123028058482));
#223394=CARTESIAN_POINT('',(-55.6083495590303,25.10597938477,3.36123028058499));
#223395=CARTESIAN_POINT('',(50.7999799080417,-22.2700612497312,3.36123028058467));
#223396=CARTESIAN_POINT('',(-52.9969317578289,30.2311753956711,3.36123028058502));
#223397=CARTESIAN_POINT('Origin',(5.5478765747851E-15,1.85785428279622E-13,
3.36123028058482));
#223398=CARTESIAN_POINT('',(-52.8664407031058,30.1558363500999,3.36123028058502));
#223399=CARTESIAN_POINT('Origin',(5.5478765747851E-15,1.85785428279622E-13,
3.36123028058482));
#223400=CARTESIAN_POINT('',(-53.1871522506177,30.3416565762235,3.48823028058504));
#223401=CARTESIAN_POINT('',(-55.8095395122501,25.1949317876425,3.48823028042712));
#223402=CARTESIAN_POINT('Origin',(5.52999282761008E-15,1.84898592019556E-13,
3.48823028058484));
#223403=CARTESIAN_POINT('',(-55.9581731633346,25.261109401072,3.77003198802724));
#223404=CARTESIAN_POINT('',(-55.8095395120008,25.19493178753,3.48823028058501));
#223405=CARTESIAN_POINT('',(-55.9579395562868,25.2616268796456,3.7700319886028));
#223406=CARTESIAN_POINT('Origin',(5.49031038273072E-15,1.82930781209959E-13,
3.77003198860263));
#223407=CARTESIAN_POINT('',(-53.3283370710514,30.422512342471,3.77003198860283));
#223408=CARTESIAN_POINT('Origin',(5.49031038273072E-15,1.82930781209959E-13,
3.77003198860263));
#223409=CARTESIAN_POINT('',(-53.3280557328688,30.4230055008167,3.77003198802741));
#223410=CARTESIAN_POINT('Origin',(5.49031038273072E-15,1.82930781209959E-13,
3.77003198860263));
#223411=CARTESIAN_POINT('',(-53.3280557331497,30.4230055009947,3.77003198860283));
#223412=CARTESIAN_POINT('Origin',(62.2224557307631,1.82930781209959E-13,
3.77003198860263));
#223413=CARTESIAN_POINT('',(-56.3916032444852,25.4547063934082,3.7700319886028));
#223414=CARTESIAN_POINT('',(52.0578415156897,-22.8300973196044,3.77003198860247));
#223415=CARTESIAN_POINT('',(-53.7394427993288,30.6598643453573,3.77003198860284));
#223416=CARTESIAN_POINT('Origin',(5.49031038273072E-15,1.82930781209959E-13,
3.77003198860263));
#223417=CARTESIAN_POINT('',(-53.3287920942669,30.422775050247,3.77003198860283));
#223418=CARTESIAN_POINT('Origin',(5.57972911860581E-15,1.8736496251029E-13,
3.13503198860263));
#223419=CARTESIAN_POINT('Origin',(-54.6869571488952,24.6957545189375,3.13502491541449));
#223420=CARTESIAN_POINT('Origin',(-52.1234719996037,29.7268774036436,3.13502491541452));
#223421=CARTESIAN_POINT('Origin',(5.57972911860581E-15,1.8736496251029E-13,
3.13503198860263));
#223422=CARTESIAN_POINT('Origin',(-56.4264225582392,25.4702456615255,3.20381846780165));
#223423=CARTESIAN_POINT('Origin',(-53.7724802568194,30.6788998055474,3.20382022872094));
#223424=CARTESIAN_POINT('Origin',(5.51210908043506E-15,1.8401175575949E-13,
3.61523028058481));
#223425=CARTESIAN_POINT('Origin',(-55.62285329818,25.112396262664,3.58786945047063));
#223426=CARTESIAN_POINT('Origin',(-53.0105668578065,30.2390901817298,3.58781461834535));
#223427=CARTESIAN_POINT('Origin',(5.51210908043507E-15,1.8401175575949E-13,
3.61523028058481));
#223428=CARTESIAN_POINT('Origin',(-55.4557927279724,25.0381063693915,3.58781440266499));
#223429=CARTESIAN_POINT('Origin',(-52.8522693417508,30.147601831022,3.58786923592841));
#223430=CARTESIAN_POINT('Origin',(60.4792282238308,1.82930781209959E-13,
3.77003198860263));
#223431=CARTESIAN_POINT('',(-48.7306271754178,35.0124214764584,3.77003198860287));
#223432=CARTESIAN_POINT('',(-51.8059703131948,30.276808326888,3.77003198860283));
#223433=CARTESIAN_POINT('Origin',(5.49031038273072E-15,1.82930781209959E-13,
3.77003198860263));
#223434=CARTESIAN_POINT('',(-52.2170762957392,30.5141604766046,3.77003198860283));
#223435=CARTESIAN_POINT('',(45.5181711678734,-25.9133109558552,3.77003198860245));
#223436=CARTESIAN_POINT('',(-52.2167844420139,30.5146599059378,3.77003198902559));
#223437=CARTESIAN_POINT('Origin',(5.49031038273072E-15,1.82930781209959E-13,
3.77003198860263));
#223438=CARTESIAN_POINT('',(-49.1150085644482,35.2909759047568,3.77003198882111));
#223439=CARTESIAN_POINT('Origin',(5.49031038273072E-15,1.82930781209959E-13,
3.77003198860263));
#223440=CARTESIAN_POINT('',(-49.1146710209412,35.2914456628186,3.77003198860286));
#223441=CARTESIAN_POINT('Origin',(5.49031038273072E-15,1.82930781209959E-13,
3.77003198860263));
#223442=CARTESIAN_POINT('',(-48.731062101221,35.012737468551,3.77003198860287));
#223443=CARTESIAN_POINT('Origin',(5.49031038273072E-15,1.82930781209959E-13,
3.77003198860263));
#223444=CARTESIAN_POINT('',(-52.3576880233164,30.5960088312567,3.48823028058502));
#223445=CARTESIAN_POINT('',(-52.2167844413817,30.5146599055683,3.77003198860283));
#223446=CARTESIAN_POINT('',(-49.2466351558311,35.3866101429909,3.48823028074828));
#223447=CARTESIAN_POINT('Origin',(5.52999282761009E-15,1.84898592019556E-13,
3.48823028058481));
#223448=CARTESIAN_POINT('',(-49.2466351556015,35.3866101428259,3.48823028058505));
#223449=CARTESIAN_POINT('Origin',(60.71525,1.85785428279622E-13,3.36123028058482));
#223450=CARTESIAN_POINT('',(-49.4242607783462,35.5163757878395,3.36123028058506));
#223451=CARTESIAN_POINT('',(-52.5484816883961,30.7054974692368,3.36123028058502));
#223452=CARTESIAN_POINT('Origin',(5.5478765747851E-15,1.85785428279622E-13,
3.36123028058482));
#223453=CARTESIAN_POINT('',(-52.6794317578289,30.7811015270742,3.36123028058502));
#223454=CARTESIAN_POINT('',(45.6951875000003,-26.0155113828597,3.36123028058464));
#223455=CARTESIAN_POINT('',(-49.5465907136146,35.6052536882601,3.36123028058506));
#223456=CARTESIAN_POINT('Origin',(5.5478765747851E-15,1.85785428279622E-13,
3.36123028058482));
#223457=CARTESIAN_POINT('',(-49.4246895772004,35.516687328443,3.36123028058506));
#223458=CARTESIAN_POINT('Origin',(5.5478765747851E-15,1.85785428279622E-13,
3.36123028058482));
#223459=CARTESIAN_POINT('',(-49.7242207306177,35.7350130971388,3.48823028058508));
#223460=CARTESIAN_POINT('',(-52.8702215134579,30.8905967160115,3.48823028042716));
#223461=CARTESIAN_POINT('Origin',(5.52999282761008E-15,1.84898592019556E-13,
3.48823028058484));
#223462=CARTESIAN_POINT('',(-53.0111234896155,30.971948248688,3.77003198802728));
#223463=CARTESIAN_POINT('',(-52.8702215132218,30.8905967158735,3.48823028058505));
#223464=CARTESIAN_POINT('',(-53.0108370710514,30.9724384738741,3.77003198860284));
#223465=CARTESIAN_POINT('Origin',(5.49031038273072E-15,1.82930781209959E-13,
3.77003198860263));
#223466=CARTESIAN_POINT('',(-49.8561803968405,35.8301837593554,3.77003198860287));
#223467=CARTESIAN_POINT('Origin',(5.49031038273072E-15,1.82930781209959E-13,
3.77003198860263));
#223468=CARTESIAN_POINT('',(-49.8558490507739,35.8306448082802,3.77003198802745));
#223469=CARTESIAN_POINT('Origin',(5.49031038273072E-15,1.82930781209959E-13,
3.77003198860263));
#223470=CARTESIAN_POINT('',(-49.8558490510346,35.8306448084866,3.77003198860287));
#223471=CARTESIAN_POINT('Origin',(62.2224557307631,1.82930781209959E-13,
3.77003198860263));
#223472=CARTESIAN_POINT('',(-53.4219427993288,31.2097904767605,3.77003198860284));
#223473=CARTESIAN_POINT('',(46.8255917980726,-26.6681506086448,3.77003198860245));
#223474=CARTESIAN_POINT('',(-50.2402240048085,36.1092077731528,3.77003198860287));
#223475=CARTESIAN_POINT('Origin',(5.49031038273072E-15,1.82930781209959E-13,
3.77003198860263));
#223476=CARTESIAN_POINT('',(-49.8566054669511,35.8304925908682,3.77003198860287));
#223477=CARTESIAN_POINT('Origin',(5.57972911860581E-15,1.8736496251029E-13,
3.13503198860263));
#223478=CARTESIAN_POINT('Origin',(-51.8059670065431,30.2768121832814,3.13502491541452));
#223479=CARTESIAN_POINT('Origin',(-48.7306293534722,35.012416887145,3.13502491541459));
#223480=CARTESIAN_POINT('Origin',(5.57972911860581E-15,1.8736496251029E-13,
3.13503198860263));
#223481=CARTESIAN_POINT('Origin',(-53.4549470734237,31.2288842284977,3.20381846780235));
#223482=CARTESIAN_POINT('Origin',(-50.2710907322488,36.131592309763,3.20382022872186));
#223483=CARTESIAN_POINT('Origin',(5.51210908043506E-15,1.8401175575949E-13,
3.61523028058481));
#223484=CARTESIAN_POINT('Origin',(-52.6931852975926,30.7889993062046,3.58786945047073));
#223485=CARTESIAN_POINT('Origin',(-49.5593237986663,35.6145503723413,3.58781461834041));
#223486=CARTESIAN_POINT('Origin',(5.51210908043507E-15,1.8401175575949E-13,
3.61523028058481));
#223487=CARTESIAN_POINT('Origin',(-52.5348053110472,30.6976537960624,3.58781440266096));
#223488=CARTESIAN_POINT('Origin',(-49.4114565896721,35.5070166082958,3.58786923592867));
#223489=CARTESIAN_POINT('Origin',(60.4792282238308,1.82930781209959E-13,
3.77003198860263));
#223490=CARTESIAN_POINT('',(-44.8038810887676,39.9143573409156,3.7700319886029));
#223491=CARTESIAN_POINT('',(-48.3573835402121,35.5261472678865,3.77003198860287));
#223492=CARTESIAN_POINT('Origin',(5.49031038273072E-15,1.82930781209959E-13,
3.77003198860263));
#223493=CARTESIAN_POINT('',(-48.7414273857063,35.805171454288,3.77003198860287));
#223494=CARTESIAN_POINT('',(39.7707905934409,-28.5027191556737,3.77003198860244));
#223495=CARTESIAN_POINT('',(-48.7410849262055,35.8056376406736,3.77003198902568));
#223496=CARTESIAN_POINT('Origin',(5.49031038273072E-15,1.82930781209959E-13,
3.77003198860263));
#223497=CARTESIAN_POINT('',(-45.157039930004,40.2315646148142,3.77003198882114));
#223498=CARTESIAN_POINT('Origin',(5.49031038273072E-15,1.82930781209959E-13,
3.77003198860263));
#223499=CARTESIAN_POINT('',(-45.1566551325073,40.2319965165881,3.7700319886029));
#223500=CARTESIAN_POINT('Origin',(5.49031038273072E-15,1.82930781209959E-13,
3.77003198860263));
#223501=CARTESIAN_POINT('',(-44.804280601834,39.9147170640963,3.7700319886029));
#223502=CARTESIAN_POINT('Origin',(5.49031038273072E-15,1.82930781209959E-13,
3.77003198860263));
#223503=CARTESIAN_POINT('',(-48.8727133447945,35.9012693628904,3.48823028058505));
#223504=CARTESIAN_POINT('',(-48.7410849256153,35.8056376402401,3.77003198860287));
#223505=CARTESIAN_POINT('',(-45.2779489571886,40.3404336840073,3.48823028074832));
#223506=CARTESIAN_POINT('Origin',(5.52999282761009E-15,1.84898592019556E-13,
3.48823028058481));
#223507=CARTESIAN_POINT('',(-45.2779489569775,40.3404336838192,3.48823028058509));
#223508=CARTESIAN_POINT('Origin',(60.71525,1.85785428279622E-13,3.36123028058482));
#223509=CARTESIAN_POINT('',(-45.4410373245174,40.4880553924343,3.36123028058509));
#223510=CARTESIAN_POINT('',(-49.0510171431405,36.0301015792676,3.36123028058506));
#223511=CARTESIAN_POINT('Origin',(5.5478765747851E-15,1.85785428279622E-13,
3.36123028058482));
#223512=CARTESIAN_POINT('',(-49.1733470784089,36.1189794796882,3.36123028058506));
#223513=CARTESIAN_POINT('',(39.9252688514649,-28.6149541797803,3.36123028058462));
#223514=CARTESIAN_POINT('',(-45.5534068532513,40.5892333705622,3.36123028058509));
#223515=CARTESIAN_POINT('Origin',(5.5478765747851E-15,1.85785428279622E-13,
3.36123028058482));
#223516=CARTESIAN_POINT('',(-45.441431209506,40.4884100480711,3.36123028058509));
#223517=CARTESIAN_POINT('Origin',(5.5478765747851E-15,1.85785428279622E-13,
3.36123028058482));
#223518=CARTESIAN_POINT('',(-45.7165002428309,40.7368493365297,3.48823028058512));
#223519=CARTESIAN_POINT('',(-49.3516463039591,36.2478178024869,3.48823028042719));
#223520=CARTESIAN_POINT('Origin',(5.52999282761008E-15,1.84898592019556E-13,
3.48823028058484));
#223521=CARTESIAN_POINT('',(-49.4832728536533,36.3434519499946,3.77003198802732));
#223522=CARTESIAN_POINT('',(-49.3516463037387,36.247817802325,3.48823028058509));
#223523=CARTESIAN_POINT('',(-49.4829367616348,36.3439095507835,3.77003198860287));
#223524=CARTESIAN_POINT('Origin',(5.49031038273072E-15,1.82930781209959E-13,
3.77003198860263));
#223525=CARTESIAN_POINT('',(-45.8377889771253,40.8452921850243,3.7700319886029));
#223526=CARTESIAN_POINT('Origin',(5.49031038273072E-15,1.82930781209959E-13,
3.77003198860263));
#223527=CARTESIAN_POINT('',(-45.8374112534715,40.8457160731797,3.77003198802748));
#223528=CARTESIAN_POINT('Origin',(5.49031038273072E-15,1.82930781209959E-13,
3.77003198860263));
#223529=CARTESIAN_POINT('',(-45.8374112537093,40.8457160734122,3.7700319886029));
#223530=CARTESIAN_POINT('Origin',(62.2224557307631,1.82930781209959E-13,
3.77003198860263));
#223531=CARTESIAN_POINT('',(-49.8669803696028,36.6229335645809,3.77003198860288));
#223532=CARTESIAN_POINT('',(40.911747809259,-29.3316730956001,3.77003198860243));
#223533=CARTESIAN_POINT('',(-46.1905628026487,41.162931164248,3.77003198860291));
#223534=CARTESIAN_POINT('Origin',(5.49031038273072E-15,1.82930781209959E-13,
3.77003198860263));
#223535=CARTESIAN_POINT('',(-45.838179436974,40.8456437566512,3.7700319886029));
#223536=CARTESIAN_POINT('Origin',(5.57972911860581E-15,1.8736496251029E-13,
3.13503198860263));
#223537=CARTESIAN_POINT('Origin',(-48.3573798485717,35.526150757515,3.13502491541459));
#223538=CARTESIAN_POINT('Origin',(-44.8038837346043,39.9143530044117,3.13502491541463));
#223539=CARTESIAN_POINT('Origin',(5.57972911860581E-15,1.8736496251029E-13,
3.13503198860263));
#223540=CARTESIAN_POINT('Origin',(-49.8978080023019,36.6453726048011,3.20381846780002));
#223541=CARTESIAN_POINT('Origin',(-46.2189206177177,41.1884195276069,3.20382022872409));
#223542=CARTESIAN_POINT('Origin',(5.51210908043506E-15,1.8401175575949E-13,
3.61523028058481));
#223543=CARTESIAN_POINT('Origin',(-49.1861997321276,36.1282716303346,3.58786945046978));
#223544=CARTESIAN_POINT('Origin',(-45.5650984170303,40.5998100962484,3.58781461834004));
#223545=CARTESIAN_POINT('Origin',(5.51210908043507E-15,1.8401175575949E-13,
3.61523028058481));
#223546=CARTESIAN_POINT('Origin',(-49.038235573526,36.0208713038445,3.58781440266443));
#223547=CARTESIAN_POINT('Origin',(-45.4292815791818,40.4774090812934,3.58786923593075));
#223548=CARTESIAN_POINT('Origin',(60.4792282238308,1.82930781209959E-13,
3.77003198860263));
#223549=CARTESIAN_POINT('',(-40.386254305094,44.3789831537295,3.77003198860293));
#223550=CARTESIAN_POINT('',(-44.3789831537298,40.3862543050938,3.7700319886029));
#223551=CARTESIAN_POINT('Origin',(5.49031038273072E-15,1.82930781209959E-13,
3.77003198860263));
#223552=CARTESIAN_POINT('',(-44.7317571974361,40.7038934808043,3.7700319886029));
#223553=CARTESIAN_POINT('',(33.61296347236,-29.838009859698,3.77003198860242));
#223554=CARTESIAN_POINT('',(-44.7313678842178,40.7043213166068,3.7700319890257));
#223555=CARTESIAN_POINT('Origin',(5.49031038273072E-15,1.82930781209959E-13,
3.77003198860263));
#223556=CARTESIAN_POINT('',(-40.7043213163686,44.7313678839555,3.77003198882117));
#223557=CARTESIAN_POINT('Origin',(5.49031038273072E-15,1.82930781209959E-13,
3.77003198860263));
#223558=CARTESIAN_POINT('',(-40.7038934808041,44.7317571974354,3.77003198860293));
#223559=CARTESIAN_POINT('Origin',(5.49031038273072E-15,1.82930781209959E-13,
3.77003198860263));
#223560=CARTESIAN_POINT('',(-40.3866140282747,44.3793826667959,3.77003198860293));
#223561=CARTESIAN_POINT('Origin',(5.49031038273072E-15,1.82930781209959E-13,
3.77003198860263));
#223562=CARTESIAN_POINT('',(-44.8522789915944,40.8131880745606,3.48823028058509));
#223563=CARTESIAN_POINT('',(-44.7313678836762,40.7043213161139,3.7700319886029));
#223564=CARTESIAN_POINT('',(-40.8131880747512,44.8522789918032,3.48823028074835));
#223565=CARTESIAN_POINT('Origin',(5.52999282761009E-15,1.84898592019556E-13,
3.48823028058481));
#223566=CARTESIAN_POINT('',(-40.8131880745609,44.8522789915941,3.48823028058512));
#223567=CARTESIAN_POINT('Origin',(60.71525,1.85785428279622E-13,3.36123028058482));
#223568=CARTESIAN_POINT('',(-40.9599523566127,45.0161393894793,3.36123028058512));
#223569=CARTESIAN_POINT('',(-45.0161393894795,40.9599523566124,3.3612302805851));
#223570=CARTESIAN_POINT('Origin',(5.5478765747851E-15,1.85785428279622E-13,
3.36123028058482));
#223571=CARTESIAN_POINT('',(-45.1285089182135,41.0611303347403,3.3612302805851));
#223572=CARTESIAN_POINT('',(33.743309857225,-29.95537427179,3.36123028058461));
#223573=CARTESIAN_POINT('',(-41.0611303347406,45.1285089182133,3.36123028058512));
#223574=CARTESIAN_POINT('Origin',(5.5478765747851E-15,1.85785428279622E-13,
3.36123028058482));
#223575=CARTESIAN_POINT('',(-40.9603070122495,45.0165332744679,3.36123028058512));
#223576=CARTESIAN_POINT('Origin',(5.5478765747851E-15,1.85785428279622E-13,
3.36123028058482));
#223577=CARTESIAN_POINT('',(-41.2079002115909,45.2923641298557,3.48823028058515));
#223578=CARTESIAN_POINT('',(-45.2923641300582,41.2079002117747,3.48823028042723));
#223579=CARTESIAN_POINT('Origin',(5.52999282761008E-15,1.84898592019556E-13,
3.48823028058484));
#223580=CARTESIAN_POINT('',(-45.413273125266,41.3167691863808,3.77003198802735));
#223581=CARTESIAN_POINT('',(-45.2923641298559,41.2079002115907,3.48823028058512));
#223582=CARTESIAN_POINT('',(-45.4128910420874,41.3171891492025,3.77003198860291));
#223583=CARTESIAN_POINT('Origin',(5.49031038273072E-15,1.82930781209959E-13,
3.77003198860263));
#223584=CARTESIAN_POINT('',(-41.3171891492027,45.4128910420872,3.77003198860294));
#223585=CARTESIAN_POINT('Origin',(5.49031038273072E-15,1.82930781209959E-13,
3.77003198860263));
#223586=CARTESIAN_POINT('',(-41.3167691863812,45.4132731252658,3.77003198802751));
#223587=CARTESIAN_POINT('Origin',(5.49031038273072E-15,1.82930781209959E-13,
3.77003198860263));
#223588=CARTESIAN_POINT('',(-41.3167691865933,45.4132731255219,3.77003198860294));
#223589=CARTESIAN_POINT('Origin',(62.2224557307631,1.82930781209959E-13,
3.77003198860263));
#223590=CARTESIAN_POINT('',(-45.7656648676108,41.6348281284261,3.77003198860291));
#223591=CARTESIAN_POINT('',(34.5756856720389,-30.7048488218242,3.77003198860241));
#223592=CARTESIAN_POINT('',(-41.6348281284264,45.7656648676106,3.77003198860294));
#223593=CARTESIAN_POINT('Origin',(5.49031038273072E-15,1.82930781209959E-13,
3.77003198860263));
#223594=CARTESIAN_POINT('',(-41.3175407208296,45.4132815019359,3.77003198860294));
#223595=CARTESIAN_POINT('Origin',(5.57972911860581E-15,1.8736496251029E-13,
3.13503198860263));
#223596=CARTESIAN_POINT('Origin',(-44.378979117547,40.3862573897242,3.1350249154146));
#223597=CARTESIAN_POINT('Origin',(-40.3862573897246,44.3789791175467,3.13502491541465));
#223598=CARTESIAN_POINT('Origin',(5.57972911860581E-15,1.8736496251029E-13,
3.13503198860263));
#223599=CARTESIAN_POINT('Origin',(-45.7939781049206,41.6603666103108,3.20381846780257));
#223600=CARTESIAN_POINT('Origin',(-41.6603663369642,45.7939778018766,3.20382022872076));
#223601=CARTESIAN_POINT('Origin',(5.51210908043506E-15,1.8401175575949E-13,
3.61523028058481));
#223602=CARTESIAN_POINT('Origin',(-45.1403198695224,41.0717150501549,3.58786945047098));
#223603=CARTESIAN_POINT('Origin',(-41.0716522820265,45.1402498046834,3.58781461834337));
#223604=CARTESIAN_POINT('Origin',(5.51210908043507E-15,1.8401175575949E-13,
3.61523028058481));
#223605=CARTESIAN_POINT('Origin',(-45.0043926651443,40.9494366077763,3.5878144026647));
#223606=CARTESIAN_POINT('Origin',(-40.9493738530234,45.0043225899479,3.58786923592787));
#223607=CARTESIAN_POINT('Origin',(60.4792282238308,1.82930781209959E-13,
3.77003198860263));
#223608=CARTESIAN_POINT('',(-35.5261472678868,48.3573835402119,3.77003198860296));
#223609=CARTESIAN_POINT('',(-39.9143573409159,44.8038810887674,3.77003198860293));
#223610=CARTESIAN_POINT('Origin',(5.49031038273072E-15,1.82930781209959E-13,
3.77003198860263));
#223611=CARTESIAN_POINT('',(-40.2319965165888,45.1566551325076,3.77003198860293));
#223612=CARTESIAN_POINT('',(27.3146622010794,-29.8615093742682,3.77003198860242));
#223613=CARTESIAN_POINT('',(-40.23156461505,45.1570399302682,3.77003198902564));
#223614=CARTESIAN_POINT('Origin',(5.49031038273072E-15,1.82930781209959E-13,
3.77003198860263));
#223615=CARTESIAN_POINT('',(-35.8056376404641,48.7410849259198,3.7700319888212));
#223616=CARTESIAN_POINT('Origin',(5.49031038273072E-15,1.82930781209959E-13,
3.77003198860263));
#223617=CARTESIAN_POINT('',(-35.8051714542879,48.7414273857056,3.77003198860296));
#223618=CARTESIAN_POINT('Origin',(5.49031038273072E-15,1.82930781209959E-13,
3.77003198860263));
#223619=CARTESIAN_POINT('',(-35.5264632599794,48.3578184660151,3.77003198860296));
#223620=CARTESIAN_POINT('Origin',(5.49031038273072E-15,1.82930781209959E-13,
3.77003198860263));
#223621=CARTESIAN_POINT('',(-40.3404336838195,45.2779489569772,3.48823028058512));
#223622=CARTESIAN_POINT('',(-40.231564614563,45.1570399297216,3.77003198860294));
#223623=CARTESIAN_POINT('',(-35.9012693630581,48.8727133450222,3.48823028074838));
#223624=CARTESIAN_POINT('Origin',(5.52999282761009E-15,1.84898592019556E-13,
3.48823028058481));
#223625=CARTESIAN_POINT('',(-35.9012693628907,48.8727133447944,3.48823028058514));
#223626=CARTESIAN_POINT('Origin',(60.71525,1.85785428279622E-13,3.36123028058482));
#223627=CARTESIAN_POINT('',(-36.0301015792679,49.0510171431404,3.36123028058515));
#223628=CARTESIAN_POINT('',(-40.4880553924345,45.4410373245172,3.36123028058512));
#223629=CARTESIAN_POINT('Origin',(5.5478765747851E-15,1.85785428279622E-13,
3.36123028058482));
#223630=CARTESIAN_POINT('',(-40.5892333705625,45.5534068532511,3.36123028058513));
#223631=CARTESIAN_POINT('',(27.4203375923837,-29.9788737863602,3.36123028058461));
#223632=CARTESIAN_POINT('',(-36.1189794796885,49.1733470784087,3.36123028058515));
#223633=CARTESIAN_POINT('Origin',(5.5478765747851E-15,1.85785428279622E-13,
3.36123028058482));
#223634=CARTESIAN_POINT('',(-36.0304131198714,49.0514459419945,3.36123028058515));
#223635=CARTESIAN_POINT('Origin',(5.5478765747851E-15,1.85785428279622E-13,
3.36123028058482));
#223636=CARTESIAN_POINT('',(-36.2478178023253,49.3516463037385,3.48823028058518));
#223637=CARTESIAN_POINT('',(-40.7368493367119,45.7165002430348,3.48823028042726));
#223638=CARTESIAN_POINT('Origin',(5.52999282761008E-15,1.84898592019556E-13,
3.48823028058484));
#223639=CARTESIAN_POINT('',(-40.8457160731799,45.8374112534712,3.77003198802738));
#223640=CARTESIAN_POINT('',(-40.7368493365299,45.7165002428307,3.48823028058515));
#223641=CARTESIAN_POINT('',(-40.8452921850246,45.8377889771251,3.77003198860294));
#223642=CARTESIAN_POINT('Origin',(5.49031038273072E-15,1.82930781209959E-13,
3.77003198860263));
#223643=CARTESIAN_POINT('',(-36.3439095507838,49.4829367616346,3.77003198860296));
#223644=CARTESIAN_POINT('Origin',(5.49031038273072E-15,1.82930781209959E-13,
3.77003198860263));
#223645=CARTESIAN_POINT('',(-36.343451949995,49.4832728536532,3.77003198802754));
#223646=CARTESIAN_POINT('Origin',(5.49031038273072E-15,1.82930781209959E-13,
3.77003198860263));
#223647=CARTESIAN_POINT('',(-36.3434519501792,49.4832728539301,3.77003198860296));
#223648=CARTESIAN_POINT('Origin',(62.2224557307631,1.82930781209959E-13,
3.77003198860263));
#223649=CARTESIAN_POINT('',(-41.1629311642483,46.1905628026485,3.77003198860294));
#223650=CARTESIAN_POINT('',(28.0951675083328,-30.7283483363944,3.77003198860241));
#223651=CARTESIAN_POINT('',(-36.6229335645812,49.8669803696026,3.77003198860297));
#223652=CARTESIAN_POINT('Origin',(5.49031038273072E-15,1.82930781209959E-13,
3.77003198860263));
#223653=CARTESIAN_POINT('',(-36.3442183822966,49.4833618317452,3.77003198860296));
#223654=CARTESIAN_POINT('Origin',(5.57972911860581E-15,1.8736496251029E-13,
3.13503198860263));
#223655=CARTESIAN_POINT('Origin',(-39.9143530044121,44.803883734604,3.13502491541464));
#223656=CARTESIAN_POINT('Origin',(-35.5261507575155,48.3573798485714,3.13502491541468));
#223657=CARTESIAN_POINT('Origin',(5.57972911860581E-15,1.8736496251029E-13,
3.13503198860263));
#223658=CARTESIAN_POINT('Origin',(-41.1884198004166,46.218920921244,3.2038184678044));
#223659=CARTESIAN_POINT('Origin',(-36.6453723646293,49.8978076723462,3.20382022872021));
#223660=CARTESIAN_POINT('Origin',(5.51210908043506E-15,1.8401175575949E-13,
3.61523028058481));
#223661=CARTESIAN_POINT('Origin',(-40.5998732162083,45.5651681650775,3.58786945047012));
#223662=CARTESIAN_POINT('Origin',(-36.1282165298269,49.1861234900557,3.58781461834067));
#223663=CARTESIAN_POINT('Origin',(5.51210908043507E-15,1.8401175575949E-13,
3.61523028058481));
#223664=CARTESIAN_POINT('Origin',(-40.4774722129442,45.4293513150162,3.58781440266541));
#223665=CARTESIAN_POINT('Origin',(-36.0208162177245,49.0381593225492,3.58786923592834));
#223666=CARTESIAN_POINT('Origin',(60.4792282238308,1.82930781209959E-13,
3.77003198860263));
#223667=CARTESIAN_POINT('',(-30.2768083268883,51.8059703131947,3.77003198860298));
#223668=CARTESIAN_POINT('',(-35.0124214764587,48.7306271754176,3.77003198860296));
#223669=CARTESIAN_POINT('Origin',(5.49031038273072E-15,1.82930781209959E-13,
3.77003198860263));
#223670=CARTESIAN_POINT('',(-35.2914456628193,49.1146710209415,3.77003198860296));
#223671=CARTESIAN_POINT('',(21.1519223437074,-28.572960233785,3.77003198860243));
#223672=CARTESIAN_POINT('',(-35.2909759049636,49.1150085647355,3.77003198902554));
#223673=CARTESIAN_POINT('Origin',(5.49031038273072E-15,1.82930781209959E-13,
3.77003198860263));
#223674=CARTESIAN_POINT('',(-30.5146599057594,52.2167844417079,3.77003198882123));
#223675=CARTESIAN_POINT('Origin',(5.49031038273072E-15,1.82930781209959E-13,
3.77003198860263));
#223676=CARTESIAN_POINT('',(-30.5141604766047,52.2170762957385,3.77003198860299));
#223677=CARTESIAN_POINT('Origin',(5.49031038273072E-15,1.82930781209959E-13,
3.77003198860263));
#223678=CARTESIAN_POINT('',(-30.2770771258173,51.8064358865967,3.77003198860298));
#223679=CARTESIAN_POINT('Origin',(5.49031038273072E-15,1.82930781209959E-13,
3.77003198860263));
#223680=CARTESIAN_POINT('',(-35.3866101428262,49.2466351556013,3.48823028058515));
#223681=CARTESIAN_POINT('',(-35.2909759045365,49.1150085641411,3.77003198860296));
#223682=CARTESIAN_POINT('',(-30.5960088313997,52.3576880235604,3.4882302807484));
#223683=CARTESIAN_POINT('Origin',(5.52999282761009E-15,1.84898592019556E-13,
3.48823028058481));
#223684=CARTESIAN_POINT('',(-30.5960088312571,52.3576880233163,3.48823028058517));
#223685=CARTESIAN_POINT('Origin',(60.71525,1.85785428279622E-13,3.36123028058482));
#223686=CARTESIAN_POINT('',(-30.7054974692372,52.5484816883959,3.36123028058518));
#223687=CARTESIAN_POINT('',(-35.5163757878398,49.4242607783461,3.36123028058515));
#223688=CARTESIAN_POINT('Origin',(5.5478765747851E-15,1.85785428279622E-13,
3.36123028058482));
#223689=CARTESIAN_POINT('',(-35.6052536882604,49.5465907136145,3.36123028058516));
#223690=CARTESIAN_POINT('',(21.2334658618526,-28.6851952578917,3.36123028058461));
#223691=CARTESIAN_POINT('',(-30.7811015270746,52.6794317578288,3.36123028058518));
#223692=CARTESIAN_POINT('Origin',(5.5478765747851E-15,1.85785428279622E-13,
3.36123028058482));
#223693=CARTESIAN_POINT('',(-30.7057624815034,52.5489407031057,3.36123028058518));
#223694=CARTESIAN_POINT('Origin',(5.5478765747851E-15,1.85785428279622E-13,
3.36123028058482));
#223695=CARTESIAN_POINT('',(-30.8905967158739,52.8702215132216,3.4882302805852));
#223696=CARTESIAN_POINT('',(-35.7350130972987,49.7242207308396,3.48823028042729));
#223697=CARTESIAN_POINT('Origin',(5.52999282761008E-15,1.84898592019556E-13,
3.48823028058484));
#223698=CARTESIAN_POINT('',(-35.8306448082804,49.8558490507736,3.77003198802741));
#223699=CARTESIAN_POINT('',(-35.7350130971392,49.7242207306175,3.48823028058518));
#223700=CARTESIAN_POINT('',(-35.8301837593557,49.8561803968403,3.77003198860297));
#223701=CARTESIAN_POINT('Origin',(5.49031038273072E-15,1.82930781209959E-13,
3.77003198860263));
#223702=CARTESIAN_POINT('',(-30.9724384738745,53.0108370710513,3.77003198860299));
#223703=CARTESIAN_POINT('Origin',(5.49031038273072E-15,1.82930781209959E-13,
3.77003198860263));
#223704=CARTESIAN_POINT('',(-30.9719482486884,53.0111234896154,3.77003198802757));
#223705=CARTESIAN_POINT('Origin',(5.49031038273072E-15,1.82930781209959E-13,
3.77003198860263));
#223706=CARTESIAN_POINT('',(-30.9719482488427,53.01112348991,3.77003198860299));
#223707=CARTESIAN_POINT('Origin',(62.2224557307631,1.82930781209959E-13,
3.77003198860263));
#223708=CARTESIAN_POINT('',(-36.1092077731531,50.2402240048083,3.77003198860297));
#223709=CARTESIAN_POINT('',(21.7541926348216,-29.4019141737115,3.77003198860242));
#223710=CARTESIAN_POINT('',(-31.2097904767608,53.4219427993287,3.77003198860299));
#223711=CARTESIAN_POINT('Origin',(5.49031038273072E-15,1.82930781209959E-13,
3.77003198860263));
#223712=CARTESIAN_POINT('',(-30.9727011816504,53.0112920942668,3.77003198860299));
#223713=CARTESIAN_POINT('Origin',(5.57972911860581E-15,1.8736496251029E-13,
3.13503198860263));
#223714=CARTESIAN_POINT('Origin',(-35.0124168871455,48.7306293534719,3.13502491541467));
#223715=CARTESIAN_POINT('Origin',(-30.2768121832819,51.8059670065428,3.13502491541469));
#223716=CARTESIAN_POINT('Origin',(5.57972911860581E-15,1.8736496251029E-13,
3.13503198860263));
#223717=CARTESIAN_POINT('Origin',(-36.1315925493535,50.2710910626265,3.20381846780134));
#223718=CARTESIAN_POINT('Origin',(-31.2288840241293,53.4549467201713,3.20382022872142));
#223719=CARTESIAN_POINT('Origin',(5.51210908043506E-15,1.8401175575949E-13,
3.61523028058481));
#223720=CARTESIAN_POINT('Origin',(-35.6146058558677,49.5593997624595,3.58786945046899));
#223721=CARTESIAN_POINT('Origin',(-30.7889524770103,52.6931037136122,3.58781461834046));
#223722=CARTESIAN_POINT('Origin',(5.51210908043507E-15,1.8401175575949E-13,
3.61523028058481));
#223723=CARTESIAN_POINT('Origin',(-35.5070721047356,49.411532542534,3.58781440266494));
#223724=CARTESIAN_POINT('Origin',(-30.6976069821026,52.5347237197209,3.58786923593167));
#223725=CARTESIAN_POINT('Origin',(60.4792282238308,1.82930781209959E-13,
3.77003198860263));
#223726=CARTESIAN_POINT('',(-24.695750338031,54.6869600343298,3.770031988603));
#223727=CARTESIAN_POINT('',(-29.7268821954852,52.1234703131947,3.77003198860298));
#223728=CARTESIAN_POINT('Origin',(5.49031038273072E-15,1.82930781209959E-13,
3.77003198860263));
#223729=CARTESIAN_POINT('',(-29.9642343451581,52.5345762957644,3.77003198860299));
#223730=CARTESIAN_POINT('',(15.3947701216595,-26.0295240215571,3.77003198860244));
#223731=CARTESIAN_POINT('',(-29.9637318777512,52.5348628873916,3.77003198902577));
#223732=CARTESIAN_POINT('Origin',(5.49031038273072E-15,1.82930781209959E-13,
3.77003198860263));
#223733=CARTESIAN_POINT('',(-24.8893571715241,55.120385940088,3.77003198882125));
#223734=CARTESIAN_POINT('Origin',(5.49031038273072E-15,1.82930781209959E-13,
3.77003198860263));
#223735=CARTESIAN_POINT('',(-24.8888299712412,55.1206239907497,3.77003198860301));
#223736=CARTESIAN_POINT('Origin',(5.49031038273072E-15,1.82930781209959E-13,
3.77003198860263));
#223737=CARTESIAN_POINT('',(-24.6959689987791,54.687451154411,3.770031988603));
#223738=CARTESIAN_POINT('Origin',(5.49031038273072E-15,1.82930781209959E-13,
3.77003198860263));
#223739=CARTESIAN_POINT('',(-30.0450834959839,52.6757649139396,3.48823028058517));
#223740=CARTESIAN_POINT('',(-29.9637318773884,52.5348628867555,3.77003198860299));
#223741=CARTESIAN_POINT('',(-24.9555320243581,55.2690209155618,3.48823028074843));
#223742=CARTESIAN_POINT('Origin',(5.52999282761009E-15,1.84898592019556E-13,
3.48823028058481));
#223743=CARTESIAN_POINT('',(-24.9555320242418,55.2690209153041,3.48823028058519));
#223744=CARTESIAN_POINT('Origin',(60.71525,1.85785428279622E-13,3.36123028058482));
#223745=CARTESIAN_POINT('',(-25.044477503395,55.4702140717967,3.3612302805852));
#223746=CARTESIAN_POINT('',(-30.155571337834,52.865981688396,3.36123028058518));
#223747=CARTESIAN_POINT('Origin',(5.5478765747851E-15,1.85785428279622E-13,
3.36123028058482));
#223748=CARTESIAN_POINT('',(-30.2311753956715,52.9969317578288,3.36123028058518));
#223749=CARTESIAN_POINT('',(15.4537755657018,-26.1317244485615,3.36123028058463));
#223750=CARTESIAN_POINT('',(-25.1059793847704,55.6083495590302,3.3612302805852));
#223751=CARTESIAN_POINT('Origin',(5.5478765747851E-15,1.85785428279622E-13,
3.36123028058482));
#223752=CARTESIAN_POINT('',(-25.0446930837941,55.4706982733008,3.3612302805852));
#223753=CARTESIAN_POINT('Origin',(5.5478765747851E-15,1.85785428279622E-13,
3.36123028058482));
#223754=CARTESIAN_POINT('',(-25.1949317875303,55.8095395120008,3.48823028058522));
#223755=CARTESIAN_POINT('',(-30.3416565763594,53.1871522508551,3.48823028042731));
#223756=CARTESIAN_POINT('Origin',(5.52999282761008E-15,1.84898592019556E-13,
3.48823028058484));
#223757=CARTESIAN_POINT('',(-30.423005500817,53.3280557328686,3.77003198802744));
#223758=CARTESIAN_POINT('',(-30.3416565762239,53.1871522506175,3.4882302805852));
#223759=CARTESIAN_POINT('',(-30.4225123424714,53.3283370710513,3.77003198860299));
#223760=CARTESIAN_POINT('Origin',(5.49031038273072E-15,1.82930781209959E-13,
3.77003198860263));
#223761=CARTESIAN_POINT('',(-25.2616268796459,55.9579395562867,3.77003198860301));
#223762=CARTESIAN_POINT('Origin',(5.49031038273072E-15,1.82930781209959E-13,
3.77003198860263));
#223763=CARTESIAN_POINT('',(-25.2611094010724,55.9581731633346,3.77003198802759));
#223764=CARTESIAN_POINT('Origin',(5.49031038273072E-15,1.82930781209959E-13,
3.77003198860263));
#223765=CARTESIAN_POINT('',(-25.261109401195,55.9581731636437,3.77003198860301));
#223766=CARTESIAN_POINT('Origin',(62.2224557307631,1.82930781209959E-13,
3.77003198860263));
#223767=CARTESIAN_POINT('',(-30.6598643453577,53.7394427993287,3.77003198860299));
#223768=CARTESIAN_POINT('',(15.8305769983926,-26.7843636743467,3.77003198860244));
#223769=CARTESIAN_POINT('',(-25.4547063934086,56.3916032444851,3.77003198860301));
#223770=CARTESIAN_POINT('Origin',(5.49031038273072E-15,1.82930781209959E-13,
3.77003198860263));
#223771=CARTESIAN_POINT('',(-25.2618405854037,55.9584195472775,3.77003198860301));
#223772=CARTESIAN_POINT('Origin',(5.57972911860581E-15,1.8736496251029E-13,
3.13503198860263));
#223773=CARTESIAN_POINT('Origin',(-29.7268774036442,52.1234719996035,3.13502491541469));
#223774=CARTESIAN_POINT('Origin',(-24.6957545189381,54.6869571488951,3.13502491541473));
#223775=CARTESIAN_POINT('Origin',(5.57972911860581E-15,1.8736496251029E-13,
3.13503198860263));
#223776=CARTESIAN_POINT('Origin',(-30.6789000092897,53.7724806104335,3.20381846780308));
#223777=CARTESIAN_POINT('Origin',(-25.4702454952008,56.4264221855609,3.2038202287226));
#223778=CARTESIAN_POINT('Origin',(5.51210908043506E-15,1.8401175575949E-13,
3.61523028058481));
#223779=CARTESIAN_POINT('Origin',(-30.2391374209354,53.010648205074,3.5878694504651));
#223780=CARTESIAN_POINT('Origin',(-25.1123582178531,55.6227672661415,3.58781461834012));
#223781=CARTESIAN_POINT('Origin',(5.51210908043507E-15,1.8401175575949E-13,
3.61523028058481));
#223782=CARTESIAN_POINT('Origin',(-30.1476490842064,52.8523506794932,3.58781440266171));
#223783=CARTESIAN_POINT('Origin',(-25.0380683404989,55.4557066902178,3.58786923593092));
#223784=CARTESIAN_POINT('Origin',(60.4792282238308,1.82930781209959E-13,
3.77003198860263));
#223785=CARTESIAN_POINT('',(-18.8441205405522,56.9687879773467,3.77003198860303));
#223786=CARTESIAN_POINT('',(-24.1156489724279,54.9452378026829,3.77003198860301));
#223787=CARTESIAN_POINT('Origin',(5.49031038273072E-15,1.82930781209959E-13,
3.77003198860263));
#223788=CARTESIAN_POINT('',(-24.3087286055922,55.378901759124,3.77003198860301));
#223789=CARTESIAN_POINT('',(10.2954134679533,-22.3432738675265,3.77003198860247));
#223790=CARTESIAN_POINT('',(-24.3081989337718,55.3791342586262,3.77003198902562));
#223791=CARTESIAN_POINT('Origin',(5.49031038273072E-15,1.82930781209959E-13,
3.77003198860263));
#223792=CARTESIAN_POINT('',(-18.9913614316847,57.4200769554262,3.77003198882127));
#223793=CARTESIAN_POINT('Origin',(5.49031038273072E-15,1.82930781209959E-13,
3.77003198860263));
#223794=CARTESIAN_POINT('',(-18.9908122363903,57.4202585945861,3.77003198860302));
#223795=CARTESIAN_POINT('Origin',(5.49031038273072E-15,1.82930781209959E-13,
3.77003198860263));
#223796=CARTESIAN_POINT('',(-18.8442866674264,56.9692992632927,3.77003198860302));
#223797=CARTESIAN_POINT('Origin',(5.49031038273072E-15,1.82930781209959E-13,
3.77003198860263));
#223798=CARTESIAN_POINT('',(-24.3743766270217,55.5277679687684,3.4882302805852));
#223799=CARTESIAN_POINT('',(-24.3081989334776,55.3791342579559,3.77003198860301));
#223800=CARTESIAN_POINT('',(-19.0416371861768,57.5748148486261,3.48823028074845));
#223801=CARTESIAN_POINT('Origin',(5.52999282761009E-15,1.84898592019556E-13,
3.48823028058481));
#223802=CARTESIAN_POINT('',(-19.041637186088,57.5748148483577,3.48823028058521));
#223803=CARTESIAN_POINT('Origin',(60.71525,1.85785428279622E-13,3.36123028058482));
#223804=CARTESIAN_POINT('',(-19.1090650011318,57.7842031819384,3.36123028058522));
#223805=CARTESIAN_POINT('',(-24.464376137792,55.7284918401499,3.3612302805852));
#223806=CARTESIAN_POINT('Origin',(5.5478765747851E-15,1.85785428279622E-13,
3.36123028058482));
#223807=CARTESIAN_POINT('',(-24.5258780191674,55.8666273273834,3.36123028058521));
#223808=CARTESIAN_POINT('',(10.3344596589369,-22.4309730483566,3.36123028058466));
#223809=CARTESIAN_POINT('',(-19.1557908785628,57.9280106456677,3.36123028058522));
#223810=CARTESIAN_POINT('Origin',(5.5478765747851E-15,1.85785428279622E-13,
3.36123028058482));
#223811=CARTESIAN_POINT('',(-19.1092287877198,57.7847072652237,3.36123028058521));
#223812=CARTESIAN_POINT('Origin',(5.5478765747851E-15,1.85785428279622E-13,
3.36123028058482));
#223813=CARTESIAN_POINT('',(-19.2232259141442,58.1373965169894,3.48823028058524));
#223814=CARTESIAN_POINT('',(-24.6158705165696,56.0673542006831,3.48823028042733));
#223815=CARTESIAN_POINT('Origin',(5.52999282761008E-15,1.84898592019556E-13,
3.48823028058484));
#223816=CARTESIAN_POINT('',(-24.6820453786634,56.2159890767412,3.77003198802746));
#223817=CARTESIAN_POINT('',(-24.6158705164596,56.0673542004326,3.48823028058523));
#223818=CARTESIAN_POINT('',(-24.6815255140429,56.2162173246398,3.77003198860301));
#223819=CARTESIAN_POINT('Origin',(5.49031038273072E-15,1.82930781209959E-13,
3.77003198860263));
#223820=CARTESIAN_POINT('',(-19.2740436149887,58.2919551457918,3.77003198860303));
#223821=CARTESIAN_POINT('Origin',(5.49031038273072E-15,1.82930781209959E-13,
3.77003198860263));
#223822=CARTESIAN_POINT('',(-19.2735045526312,58.2921333818758,3.77003198802761));
#223823=CARTESIAN_POINT('Origin',(5.49031038273072E-15,1.82930781209959E-13,
3.77003198860263));
#223824=CARTESIAN_POINT('',(-19.2735045527209,58.292133382196,3.77003198860303));
#223825=CARTESIAN_POINT('Origin',(62.2224557307631,1.82930781209959E-13,
3.77003198860263));
#223826=CARTESIAN_POINT('',(-24.8746050278055,56.6498810128383,3.77003198860302));
#223827=CARTESIAN_POINT('',(10.5838037820519,-22.9910091182298,3.77003198860247));
#223828=CARTESIAN_POINT('',(-19.4207352200703,58.7434254837933,3.77003198860304));
#223829=CARTESIAN_POINT('Origin',(5.49031038273072E-15,1.82930781209959E-13,
3.77003198860263));
#223830=CARTESIAN_POINT('',(-19.2742059773234,58.2924548456762,3.77003198860303));
#223831=CARTESIAN_POINT('Origin',(5.57972911860581E-15,1.8736496251029E-13,
3.13503198860263));
#223832=CARTESIAN_POINT('Origin',(-24.1156440305593,54.9452389789697,3.1350249154147));
#223833=CARTESIAN_POINT('Origin',(-18.844125000166,56.9687855447425,3.13502491541473));
#223834=CARTESIAN_POINT('Origin',(5.57972911860581E-15,1.8736496251029E-13,
3.13503198860263));
#223835=CARTESIAN_POINT('Origin',(-24.890083020755,56.6847276080529,3.20381846779927));
#223836=CARTESIAN_POINT('Origin',(-19.4325496266324,58.7796779614993,3.20382022872482));
#223837=CARTESIAN_POINT('Origin',(5.51210908043506E-15,1.8401175575949E-13,
3.61523028058481));
#223838=CARTESIAN_POINT('Origin',(-24.5323626684706,55.8811008927581,3.58786945047008));
#223839=CARTESIAN_POINT('Origin',(-19.160627706962,57.9430161406896,3.58781461834175));
#223840=CARTESIAN_POINT('Origin',(5.51210908043507E-15,1.8401175575949E-13,
3.61523028058481));
#223841=CARTESIAN_POINT('Origin',(-24.4579221115101,55.7141074023466,3.5878144026663));
#223842=CARTESIAN_POINT('Origin',(-19.1042073826016,57.769105333365,3.58786923592921));
#223843=CARTESIAN_POINT('Origin',(60.4792282238308,1.82930781209959E-13,
3.77003198860263));
#223844=CARTESIAN_POINT('',(-12.7860306150453,58.6264539577985,3.77003198860304));
#223845=CARTESIAN_POINT('',(-18.2401996527048,57.1650137687748,3.77003198860303));
#223846=CARTESIAN_POINT('Origin',(5.49031038273072E-15,1.82930781209959E-13,
3.77003198860263));
#223847=CARTESIAN_POINT('',(-18.386891348495,57.6164843860304,3.77003198860303));
#223848=CARTESIAN_POINT('',(6.07721283595923,-17.6762863142852,3.77003198860251));
#223849=CARTESIAN_POINT('',(-18.3863402754567,57.616660246095,3.77003198902593));
#223850=CARTESIAN_POINT('Origin',(5.49031038273072E-15,1.82930781209959E-13,
3.77003198860263));
#223851=CARTESIAN_POINT('',(-12.8852923618019,59.0906615917172,3.77003198882128));
#223852=CARTESIAN_POINT('Origin',(5.49031038273072E-15,1.82930781209959E-13,
3.77003198860263));
#223853=CARTESIAN_POINT('',(-12.8847271885945,59.0907848292986,3.77003198860304));
#223854=CARTESIAN_POINT('Origin',(5.49031038273072E-15,1.82930781209959E-13,
3.77003198860263));
#223855=CARTESIAN_POINT('',(-12.786142387925,58.6269798078534,3.77003198860304));
#223856=CARTESIAN_POINT('Origin',(5.49031038273072E-15,1.82930781209959E-13,
3.77003198860263));
#223857=CARTESIAN_POINT('',(-18.4366189870675,57.7713971777988,3.48823028058521));
#223858=CARTESIAN_POINT('',(-18.386340275234,57.6166602453972,3.77003198860303));
#223859=CARTESIAN_POINT('',(-12.919118186265,59.2498070619043,3.48823028074846));
#223860=CARTESIAN_POINT('Origin',(5.52999282761009E-15,1.84898592019556E-13,
3.48823028058481));
#223861=CARTESIAN_POINT('',(-12.9191181862048,59.2498070616281,3.48823028058522));
#223862=CARTESIAN_POINT('Origin',(60.71525,1.85785428279622E-13,3.36123028058482));
#223863=CARTESIAN_POINT('',(-12.9642895838873,59.4650964698968,3.36123028058523));
#223864=CARTESIAN_POINT('',(-18.5051441132844,57.9804289733665,3.36123028058522));
#223865=CARTESIAN_POINT('Origin',(5.5478765747851E-15,1.85785428279622E-13,
3.36123028058482));
#223866=CARTESIAN_POINT('',(-18.5518699907153,58.1242364370958,3.36123028058522));
#223867=CARTESIAN_POINT('',(6.0997509100621,-17.7456513739113,3.36123028058469));
#223868=CARTESIAN_POINT('',(-12.9957275188826,59.6130003254556,3.36123028058523));
#223869=CARTESIAN_POINT('Origin',(5.5478765747851E-15,1.85785428279622E-13,
3.36123028058482));
#223870=CARTESIAN_POINT('',(-12.964399782184,59.4656149121215,3.36123028058523));
#223871=CARTESIAN_POINT('Origin',(5.5478765747851E-15,1.85785428279622E-13,
3.36123028058482));
#223872=CARTESIAN_POINT('',(-13.0409063549241,59.8282880397056,3.48823028058526));
#223873=CARTESIAN_POINT('',(-18.6203878281982,58.3332704850402,3.48823028042735));
#223874=CARTESIAN_POINT('Origin',(5.52999282761008E-15,1.84898592019556E-13,
3.48823028058484));
#223875=CARTESIAN_POINT('',(-18.6706636022911,58.488008280337,3.77003198802748));
#223876=CARTESIAN_POINT('',(-18.620387828115,58.3332704847797,3.48823028058524));
#223877=CARTESIAN_POINT('',(-18.6701227271413,58.4881809372198,3.77003198860304));
#223878=CARTESIAN_POINT('Origin',(5.49031038273072E-15,1.82930781209959E-13,
3.77003198860263));
#223879=CARTESIAN_POINT('',(-13.0752898951327,59.9873118763437,3.77003198860305));
#223880=CARTESIAN_POINT('Origin',(5.49031038273072E-15,1.82930781209959E-13,
3.77003198860263));
#223881=CARTESIAN_POINT('',(-13.0747351550713,59.987432788672,3.77003198802762));
#223882=CARTESIAN_POINT('Origin',(5.49031038273072E-15,1.82930781209959E-13,
3.77003198860263));
#223883=CARTESIAN_POINT('',(-13.074735155127,59.9874327889998,3.77003198860305));
#223884=CARTESIAN_POINT('Origin',(62.2224557307631,1.82930781209959E-13,
3.77003198860263));
#223885=CARTESIAN_POINT('',(-18.8168143322229,58.9396512752214,3.77003198860304));
#223886=CARTESIAN_POINT('',(6.24367625034032,-18.1886080242679,3.7700319886025));
#223887=CARTESIAN_POINT('',(-13.1739864076109,60.451642460649,3.77003198860305));
#223888=CARTESIAN_POINT('Origin',(5.49031038273072E-15,1.82930781209959E-13,
3.77003198860263));
#223889=CARTESIAN_POINT('',(-13.0753991351685,59.9878258103052,3.77003198860304));
#223890=CARTESIAN_POINT('Origin',(5.57972911860581E-15,1.8736496251029E-13,
3.13503198860263));
#223891=CARTESIAN_POINT('Origin',(-18.2401946149527,57.1650144220518,3.13502491541473));
#223892=CARTESIAN_POINT('Origin',(-12.7860353045051,58.6264520046769,3.13502491541478));
#223893=CARTESIAN_POINT('Origin',(5.57972911860581E-15,1.8736496251029E-13,
3.13503198860263));
#223894=CARTESIAN_POINT('Origin',(-18.8285650740578,58.9759248679607,3.20381846780158));
#223895=CARTESIAN_POINT('Origin',(-13.1819466778329,60.48893128525,3.20382022872197));
#223896=CARTESIAN_POINT('Origin',(5.51210908043506E-15,1.8401175575949E-13,
3.61523028058481));
#223897=CARTESIAN_POINT('Origin',(-18.5568062168843,58.1393085451906,3.58786945047204));
#223898=CARTESIAN_POINT('Origin',(-12.9989693492947,59.6284292050461,3.58781461834054));
#223899=CARTESIAN_POINT('Origin',(5.51210908043507E-15,1.8401175575949E-13,
3.61523028058481));
#223900=CARTESIAN_POINT('Origin',(-18.5002290260139,57.9654487055657,3.58781440266093));
#223901=CARTESIAN_POINT('Origin',(-12.961036730812,59.4495735695173,3.58786923592967));
#223902=CARTESIAN_POINT('Origin',(60.4792282238308,1.82930781209959E-13,
3.77003198860263));
#223903=CARTESIAN_POINT('',(-6.58785426247116,59.6417962403144,3.77003198860304));
#223904=CARTESIAN_POINT('',(-12.1649068885794,58.7584778814678,3.77003198860304));
#223905=CARTESIAN_POINT('Origin',(5.49031038273072E-15,1.82930781209959E-13,
3.77003198860263));
#223906=CARTESIAN_POINT('',(-12.2636034620792,59.222808752979,3.77003198860304));
#223907=CARTESIAN_POINT('',(2.92491386234308,-12.2335471699534,3.77003198860254));
#223908=CARTESIAN_POINT('',(-12.2630370254944,59.222926046846,3.77003198902597));
#223909=CARTESIAN_POINT('Origin',(5.49031038273072E-15,1.82930781209959E-13,
3.77003198860263));
#223910=CARTESIAN_POINT('',(-6.63804933238239,60.1138365740934,3.77003198882129));
#223911=CARTESIAN_POINT('Origin',(5.49031038273072E-15,1.82930781209959E-13,
3.77003198860263));
#223912=CARTESIAN_POINT('',(-6.63747437341798,60.1139000598795,3.77003198860305));
#223913=CARTESIAN_POINT('Origin',(5.49031038273072E-15,1.82930781209959E-13,
3.77003198860263));
#223914=CARTESIAN_POINT('',(-6.58791045674911,59.6423308931551,3.77003198860304));
#223915=CARTESIAN_POINT('Origin',(5.49031038273072E-15,1.82930781209959E-13,
3.77003198860263));
#223916=CARTESIAN_POINT('',(-12.2968658913805,59.3820708699072,3.48823028058522));
#223917=CARTESIAN_POINT('',(-12.2630370253459,59.2229260461286,3.77003198860304));
#223918=CARTESIAN_POINT('',(-6.65505462400518,60.2756459901931,3.48823028074846));
#223919=CARTESIAN_POINT('Origin',(5.52999282761009E-15,1.84898592019556E-13,
3.48823028058481));
#223920=CARTESIAN_POINT('',(-6.65505462397415,60.2756459899121,3.48823028058523));
#223921=CARTESIAN_POINT('Origin',(60.71525,1.85785428279622E-13,3.36123028058482));
#223922=CARTESIAN_POINT('',(-6.67747469700966,60.4944777170595,3.36123028058524));
#223923=CARTESIAN_POINT('',(-12.3431658574213,59.5971203935661,3.36123028058523));
#223924=CARTESIAN_POINT('Origin',(5.5478765747851E-15,1.85785428279622E-13,
3.36123028058482));
#223925=CARTESIAN_POINT('',(-12.3746037924166,59.7450242491249,3.36123028058523));
#223926=CARTESIAN_POINT('',(2.93511643966565,-12.2815465224194,3.36123028058473));
#223927=CARTESIAN_POINT('',(-6.69328024897475,60.6448574988556,3.36123028058524));
#223928=CARTESIAN_POINT('Origin',(5.5478765747851E-15,1.85785428279622E-13,
3.36123028058482));
#223929=CARTESIAN_POINT('',(-6.67753009965953,60.4950048380621,3.36123028058524));
#223930=CARTESIAN_POINT('Origin',(5.5478765747851E-15,1.85785428279622E-13,
3.36123028058482));
#223931=CARTESIAN_POINT('',(-6.7157078966943,60.8636883187846,3.48823028058527));
#223932=CARTESIAN_POINT('',(-12.4208962742143,59.9600752509416,3.48823028042737));
#223933=CARTESIAN_POINT('Origin',(5.52999282761008E-15,1.84898592019556E-13,
3.48823028058484));
#223934=CARTESIAN_POINT('',(-12.4547221284046,60.1192206258108,3.77003198802749));
#223935=CARTESIAN_POINT('',(-12.4208962741589,59.9600752506738,3.48823028058526));
#223936=CARTESIAN_POINT('',(-12.4541661686668,60.119335800013,3.77003198860305));
#223937=CARTESIAN_POINT('Origin',(5.49031038273072E-15,1.82930781209959E-13,
3.77003198860263));
#223938=CARTESIAN_POINT('',(-6.73328056300539,61.0254350648264,3.77003198860305));
#223939=CARTESIAN_POINT('Origin',(5.49031038273072E-15,1.82930781209959E-13,
3.77003198860263));
#223940=CARTESIAN_POINT('',(-6.73271622308818,61.0254973286581,3.77003198802763));
#223941=CARTESIAN_POINT('Origin',(5.49031038273072E-15,1.82930781209959E-13,
3.77003198860263));
#223942=CARTESIAN_POINT('',(-6.73271622310929,61.02549732899,3.77003198860305));
#223943=CARTESIAN_POINT('Origin',(62.2224557307631,1.82930781209959E-13,
3.77003198860263));
#223944=CARTESIAN_POINT('',(-12.5528626811449,60.5836663843183,3.77003198860305));
#223945=CARTESIAN_POINT('',(3.00026883051142,-12.588064422097,3.77003198860254));
#223946=CARTESIAN_POINT('',(-6.78290064323581,61.4975385923864,3.77003198860306));
#223947=CARTESIAN_POINT('Origin',(5.49031038273072E-15,1.82930781209959E-13,
3.77003198860263));
#223948=CARTESIAN_POINT('',(-6.73333548388561,61.025957602097,3.77003198860305));
#223949=CARTESIAN_POINT('Origin',(5.57972911860581E-15,1.8736496251029E-13,
3.13503198860263));
#223950=CARTESIAN_POINT('Origin',(-12.1649018101387,58.7584780045775,3.13502491541476));
#223951=CARTESIAN_POINT('Origin',(-6.58785913039843,59.6417947880743,3.13502491541476));
#223952=CARTESIAN_POINT('Origin',(5.57972911860581E-15,1.8736496251029E-13,
3.13503198860263));
#223953=CARTESIAN_POINT('Origin',(-12.5607574282781,60.6209695535074,3.20381846780062));
#223954=CARTESIAN_POINT('Origin',(-6.78691956273312,61.5354552197182,3.20382022872275));
#223955=CARTESIAN_POINT('Origin',(5.51210908043506E-15,1.8401175575949E-13,
3.61523028058481));
#223956=CARTESIAN_POINT('Origin',(-12.3779375131253,59.7605297667728,3.58786945046749));
#223957=CARTESIAN_POINT('Origin',(-6.6948915632271,60.6605407209801,3.58781461834101));
#223958=CARTESIAN_POINT('Origin',(5.51210908043507E-15,1.8401175575949E-13,
3.61523028058481));
#223959=CARTESIAN_POINT('Origin',(-12.3398435598879,59.5817084227243,3.58781440266877));
#223960=CARTESIAN_POINT('Origin',(-6.67586224832368,60.4786998370192,3.58786923592871));
#223961=CARTESIAN_POINT('Origin',(60.4792282238308,1.82930781209959E-13,
3.77003198860263));
#223962=CARTESIAN_POINT('',(-0.317500000000204,60.0036905223732,3.77003198860305));
#223963=CARTESIAN_POINT('',(-5.9563328589123,59.7081718144894,3.77003198860304));
#223964=CARTESIAN_POINT('Origin',(5.49031038273072E-15,1.82930781209959E-13,
3.77003198860263));
#223965=CARTESIAN_POINT('',(-6.00595296980892,60.1802756340604,3.77003198860304));
#223966=CARTESIAN_POINT('',(0.9765688230087,-6.25398151259745,3.77003198860258));
#223967=CARTESIAN_POINT('',(-6.00537737567533,60.1803330766335,3.77003198902593));
#223968=CARTESIAN_POINT('Origin',(5.49031038273072E-15,1.82930781209959E-13,
3.77003198860263));
#223969=CARTESIAN_POINT('',(-0.3180784453762,60.4783917833348,3.77003198882129));
#223970=CARTESIAN_POINT('Origin',(5.49031038273072E-15,1.82930781209959E-13,
3.77003198860263));
#223971=CARTESIAN_POINT('',(-0.31750000002549,60.4783948217622,3.77003198860305));
#223972=CARTESIAN_POINT('Origin',(5.49031038273072E-15,1.82930781209959E-13,
3.77003198860263));
#223973=CARTESIAN_POINT('',(-0.317500000000204,60.0042281202312,3.77003198860305));
#223974=CARTESIAN_POINT('Origin',(5.49031038273072E-15,1.82930781209959E-13,
3.77003198860263));
#223975=CARTESIAN_POINT('',(-6.02238575970296,60.3421421670677,3.48823028058523));
#223976=CARTESIAN_POINT('',(-6.0053773756026,60.1803330759047,3.77003198860305));
#223977=CARTESIAN_POINT('',(-0.318076890625054,60.6410923275234,3.48823028074847));
#223978=CARTESIAN_POINT('Origin',(5.52999282761009E-15,1.84898592019556E-13,
3.48823028058481));
#223979=CARTESIAN_POINT('',(-0.318076890623573,60.6410923272407,3.48823028058523));
#223980=CARTESIAN_POINT('Origin',(60.71525,1.85785428279622E-13,3.36123028058482));
#223981=CARTESIAN_POINT('',(-0.317500000000207,60.8610688070709,3.36123028058524));
#223982=CARTESIAN_POINT('',(-6.04595329345081,60.5608532912345,3.36123028058524));
#223983=CARTESIAN_POINT('Origin',(5.5478765747851E-15,1.85785428279622E-13,
3.36123028058482));
#223984=CARTESIAN_POINT('',(-6.0617588454159,60.7112330730305,3.36123028058524));
#223985=CARTESIAN_POINT('',(0.97914764405288,-6.27851735587403,3.36123028058477));
#223986=CARTESIAN_POINT('',(-0.317500000000208,61.0122769227458,3.36123028058524));
#223987=CARTESIAN_POINT('Origin',(5.5478765747851E-15,1.85785428279622E-13,
3.36123028058482));
#223988=CARTESIAN_POINT('',(-0.317500000000207,60.8615988316033,3.36123028058524));
#223989=CARTESIAN_POINT('Origin',(5.5478765747851E-15,1.85785428279622E-13,
3.36123028058482));
#223990=CARTESIAN_POINT('',(-0.316930737396123,61.2322532920974,3.48823028058527));
#223991=CARTESIAN_POINT('',(-6.08531878141059,60.9299448849413,3.48823028042737));
#223992=CARTESIAN_POINT('Origin',(5.52999282761008E-15,1.84898592019556E-13,
3.48823028058484));
#223993=CARTESIAN_POINT('',(-6.10232411256108,61.0917542093525,3.7700319880275));
#223994=CARTESIAN_POINT('',(-6.08531878138341,60.9299448846692,3.48823028058527));
#223995=CARTESIAN_POINT('',(-6.10175915944654,61.0918106390013,3.77003198860305));
#223996=CARTESIAN_POINT('Origin',(5.49031038273072E-15,1.82930781209959E-13,
3.77003198860263));
#223997=CARTESIAN_POINT('',(-0.317500000000209,61.3949508163455,3.77003198860305));
#223998=CARTESIAN_POINT('Origin',(5.49031038273072E-15,1.82930781209959E-13,
3.77003198860263));
#223999=CARTESIAN_POINT('',(-0.316932243253465,61.3949537495052,3.77003198802764));
#224000=CARTESIAN_POINT('Origin',(5.49031038273072E-15,1.82930781209959E-13,
3.77003198860263));
#224001=CARTESIAN_POINT('',(-0.316932243239769,61.3949537498375,3.77003198860305));
#224002=CARTESIAN_POINT('Origin',(62.2224557307631,1.82930781209959E-13,
3.77003198860263));
#224003=CARTESIAN_POINT('',(-6.15137923967696,61.5639141665613,3.77003198860306));
#224004=CARTESIAN_POINT('',(0.995615674755347,-6.43520020182062,3.77003198860258));
#224005=CARTESIAN_POINT('',(-0.317500000000211,61.8696548221182,3.77003198860306));
#224006=CARTESIAN_POINT('Origin',(5.49031038273072E-15,1.82930781209959E-13,
3.77003198860263));
#224007=CARTESIAN_POINT('',(-0.317500000000209,61.3954762318975,3.77003198860305));
#224008=CARTESIAN_POINT('Origin',(5.57972911860581E-15,1.8736496251029E-13,
3.13503198860263));
#224009=CARTESIAN_POINT('Origin',(-5.95632779542334,59.7081714060832,3.13502491541474));
#224010=CARTESIAN_POINT('Origin',(-0.317504993060902,60.0036895869256,3.13502491541474));
#224011=CARTESIAN_POINT('Origin',(5.57972911860581E-15,1.8736496251029E-13,
3.13503198860263));
#224012=CARTESIAN_POINT('Origin',(-6.15533149561,61.6018382108726,3.20381846780166));
#224013=CARTESIAN_POINT('Origin',(-0.317533536648822,61.9077838296764,3.20382022872102));
#224014=CARTESIAN_POINT('Origin',(5.51210908043506E-15,1.8401175575949E-13,
3.61523028058481));
#224015=CARTESIAN_POINT('Origin',(-6.06345353572148,60.72700211853,3.58786945047319));
#224016=CARTESIAN_POINT('Origin',(-0.317463144196723,61.0280426587414,3.58781461834048));
#224017=CARTESIAN_POINT('Origin',(5.51210908043507E-15,1.8401175575949E-13,
3.61523028058481));
#224018=CARTESIAN_POINT('Origin',(-6.04426018543877,60.5451784741234,3.58781440266375));
#224019=CARTESIAN_POINT('Origin',(-0.317545622030984,60.8452088131242,3.58786923592738));
#224020=CARTESIAN_POINT('Origin',(60.4792282238308,1.82930781209959E-13,
3.77003198860263));
#224021=CARTESIAN_POINT('',(5.95633285891191,59.7081718144894,3.77003198860304));
#224022=CARTESIAN_POINT('',(0.317499999999796,60.0036905223732,3.77003198860305));
#224023=CARTESIAN_POINT('Origin',(5.49031038273072E-15,1.82930781209959E-13,
3.77003198860263));
#224024=CARTESIAN_POINT('',(0.317500000025055,60.4783948217628,3.77003198860305));
#224025=CARTESIAN_POINT('',(0.317500000000005,-2.71227701960981E-14,3.77003198860263));
#224026=CARTESIAN_POINT('',(0.318078445377653,60.4783917836891,3.77003198902584));
#224027=CARTESIAN_POINT('Origin',(5.49031038273072E-15,1.82930781209959E-13,
3.77003198860263));
#224028=CARTESIAN_POINT('',(6.00537737563974,60.1803330762809,3.77003198882129));
#224029=CARTESIAN_POINT('Origin',(5.49031038273072E-15,1.82930781209959E-13,
3.77003198860263));
#224030=CARTESIAN_POINT('',(6.00595296980844,60.1802756340599,3.77003198860305));
#224031=CARTESIAN_POINT('Origin',(5.49031038273072E-15,1.82930781209959E-13,
3.77003198860263));
#224032=CARTESIAN_POINT('',(5.95638905318986,59.7087064673301,3.77003198860304));
#224033=CARTESIAN_POINT('Origin',(5.49031038273072E-15,1.82930781209959E-13,
3.77003198860263));
#224034=CARTESIAN_POINT('',(0.31807689062316,60.6410923272407,3.48823028058523));
#224035=CARTESIAN_POINT('',(0.318078445373799,60.4783917829568,3.77003198860305));
#224036=CARTESIAN_POINT('',(6.02238575973065,60.3421421673491,3.48823028074847));
#224037=CARTESIAN_POINT('Origin',(5.52999282761009E-15,1.84898592019556E-13,
3.48823028058481));
#224038=CARTESIAN_POINT('',(6.02238575970257,60.3421421670677,3.48823028058523));
#224039=CARTESIAN_POINT('Origin',(60.71525,1.85785428279622E-13,3.36123028058482));
#224040=CARTESIAN_POINT('',(6.04595329345041,60.5608532912345,3.36123028058524));
#224041=CARTESIAN_POINT('',(0.317499999999793,60.8610688070709,3.36123028058524));
#224042=CARTESIAN_POINT('Origin',(5.5478765747851E-15,1.85785428279622E-13,
3.36123028058482));
#224043=CARTESIAN_POINT('',(0.317499999999792,61.0122769227458,3.36123028058524));
#224044=CARTESIAN_POINT('',(0.317500000000005,-2.50921887534909E-14,3.36123028058482));
#224045=CARTESIAN_POINT('',(6.0617588454155,60.7112330730306,3.36123028058524));
#224046=CARTESIAN_POINT('Origin',(5.5478765747851E-15,1.85785428279622E-13,
3.36123028058482));
#224047=CARTESIAN_POINT('',(6.04600869610028,60.5613804122371,3.36123028058524));
#224048=CARTESIAN_POINT('Origin',(5.5478765747851E-15,1.85785428279622E-13,
3.36123028058482));
#224049=CARTESIAN_POINT('',(6.08531878138301,60.9299448846692,3.48823028058527));
#224050=CARTESIAN_POINT('',(0.316930737397122,61.2322532923709,3.48823028042737));
#224051=CARTESIAN_POINT('Origin',(5.52999282761008E-15,1.84898592019556E-13,
3.48823028058484));
#224052=CARTESIAN_POINT('',(0.316932243253051,61.3949537495051,3.7700319880275));
#224053=CARTESIAN_POINT('',(0.316930737395706,61.2322532920974,3.48823028058527));
#224054=CARTESIAN_POINT('',(0.317499999999791,61.3949508163455,3.77003198860305));
#224055=CARTESIAN_POINT('Origin',(5.49031038273072E-15,1.82930781209959E-13,
3.77003198860263));
#224056=CARTESIAN_POINT('',(6.10175915944613,61.0918106390014,3.77003198860305));
#224057=CARTESIAN_POINT('Origin',(5.49031038273072E-15,1.82930781209959E-13,
3.77003198860263));
#224058=CARTESIAN_POINT('',(6.10232411256069,61.0917542093526,3.77003198802763));
#224059=CARTESIAN_POINT('Origin',(5.49031038273072E-15,1.82930781209959E-13,
3.77003198860263));
#224060=CARTESIAN_POINT('',(6.10232411260904,61.0917542096817,3.77003198860305));
#224061=CARTESIAN_POINT('Origin',(62.2224557307631,1.82930781209959E-13,
3.77003198860263));
#224062=CARTESIAN_POINT('',(0.31749999999979,61.8696548221183,3.77003198860306));
#224063=CARTESIAN_POINT('',(0.317500000000005,-3.32092165059103E-14,3.77003198860263));
#224064=CARTESIAN_POINT('',(6.15137923967656,61.5639141665614,3.77003198860306));
#224065=CARTESIAN_POINT('Origin',(5.49031038273072E-15,1.82930781209959E-13,
3.77003198860263));
#224066=CARTESIAN_POINT('',(6.10181408032636,61.0923331762719,3.77003198860305));
#224067=CARTESIAN_POINT('Origin',(5.57972911860581E-15,1.8736496251029E-13,
3.13503198860263));
#224068=CARTESIAN_POINT('Origin',(0.317504993060349,60.0036895869256,3.13502491541474));
#224069=CARTESIAN_POINT('Origin',(5.95632779542282,59.7081714060832,3.13502491541477));
#224070=CARTESIAN_POINT('Origin',(5.57972911860581E-15,1.8736496251029E-13,
3.13503198860263));
#224071=CARTESIAN_POINT('Origin',(0.317533537011351,61.9077842377866,3.20381846780236));
#224072=CARTESIAN_POINT('Origin',(6.15533145331141,61.6018378049635,3.20382022872551));
#224073=CARTESIAN_POINT('Origin',(5.51210908043506E-15,1.8401175575949E-13,
3.61523028058481));
#224074=CARTESIAN_POINT('Origin',(0.317462907478283,61.0281367271393,3.5878694504696));
#224075=CARTESIAN_POINT('Origin',(6.06344346747481,60.7269085901928,3.58781461834324));
#224076=CARTESIAN_POINT('Origin',(5.51210908043507E-15,1.8401175575949E-13,
3.61523028058481));
#224077=CARTESIAN_POINT('Origin',(0.31754536844525,60.84530288027,3.58781440266518));
#224078=CARTESIAN_POINT('Origin',(6.04425010054761,60.5450849487963,3.58786923593018));
#224079=CARTESIAN_POINT('Origin',(60.4792282238308,1.82930781209959E-13,
3.77003198860263));
#224080=CARTESIAN_POINT('',(12.164906888579,58.7584778814679,3.77003198860304));
#224081=CARTESIAN_POINT('',(6.58785426247077,59.6417962403145,3.77003198860304));
#224082=CARTESIAN_POINT('Origin',(5.49031038273072E-15,1.82930781209959E-13,
3.77003198860263));
#224083=CARTESIAN_POINT('',(6.63747437341763,60.1139000598802,3.77003198860305));
#224084=CARTESIAN_POINT('',(0.976568823008617,6.25398151259742,3.77003198860267));
#224085=CARTESIAN_POINT('',(6.63804933242087,60.1138365744455,3.77003198902578));
#224086=CARTESIAN_POINT('Origin',(5.49031038273072E-15,1.82930781209959E-13,
3.77003198860263));
#224087=CARTESIAN_POINT('',(12.2630370254222,59.2229260464989,3.77003198882128));
#224088=CARTESIAN_POINT('Origin',(5.49031038273072E-15,1.82930781209959E-13,
3.77003198860263));
#224089=CARTESIAN_POINT('',(12.2636034620787,59.2228087529784,3.77003198860304));
#224090=CARTESIAN_POINT('Origin',(5.49031038273072E-15,1.82930781209959E-13,
3.77003198860263));
#224091=CARTESIAN_POINT('',(12.1650186614586,58.7590037315228,3.77003198860304));
#224092=CARTESIAN_POINT('Origin',(5.49031038273072E-15,1.82930781209959E-13,
3.77003198860263));
#224093=CARTESIAN_POINT('',(6.65505462397376,60.2756459899121,3.48823028058523));
#224094=CARTESIAN_POINT('',(6.6380493323405,60.1138365737177,3.77003198860305));
#224095=CARTESIAN_POINT('',(12.2968658914375,59.3820708701842,3.48823028074845));
#224096=CARTESIAN_POINT('Origin',(5.52999282761009E-15,1.84898592019556E-13,
3.48823028058481));
#224097=CARTESIAN_POINT('',(12.2968658913801,59.3820708699073,3.48823028058522));
#224098=CARTESIAN_POINT('Origin',(60.71525,1.85785428279622E-13,3.36123028058482));
#224099=CARTESIAN_POINT('',(12.3431658574209,59.5971203935661,3.36123028058523));
#224100=CARTESIAN_POINT('',(6.67747469700926,60.4944777170596,3.36123028058524));
#224101=CARTESIAN_POINT('Origin',(5.5478765747851E-15,1.85785428279622E-13,
3.36123028058482));
#224102=CARTESIAN_POINT('',(6.69328024897435,60.6448574988556,3.36123028058524));
#224103=CARTESIAN_POINT('',(0.979147644052797,6.27851735587401,3.36123028058486));
#224104=CARTESIAN_POINT('',(12.3746037924162,59.745024249125,3.36123028058523));
#224105=CARTESIAN_POINT('Origin',(5.5478765747851E-15,1.85785428279622E-13,
3.36123028058482));
#224106=CARTESIAN_POINT('',(12.3432760557176,59.5976388357908,3.36123028058523));
#224107=CARTESIAN_POINT('Origin',(5.5478765747851E-15,1.85785428279622E-13,
3.36123028058482));
#224108=CARTESIAN_POINT('',(12.4208962741585,59.9600752506739,3.48823028058526));
#224109=CARTESIAN_POINT('',(6.7157078967239,60.8636883190565,3.48823028042737));
#224110=CARTESIAN_POINT('Origin',(5.52999282761008E-15,1.84898592019556E-13,
3.48823028058484));
#224111=CARTESIAN_POINT('',(6.73271622308777,61.0254973286581,3.7700319880275));
#224112=CARTESIAN_POINT('',(6.7157078966939,60.8636883187847,3.48823028058527));
#224113=CARTESIAN_POINT('',(6.73328056300499,61.0254350648264,3.77003198860305));
#224114=CARTESIAN_POINT('Origin',(5.49031038273072E-15,1.82930781209959E-13,
3.77003198860263));
#224115=CARTESIAN_POINT('',(12.4541661686664,60.1193358000131,3.77003198860305));
#224116=CARTESIAN_POINT('Origin',(5.49031038273072E-15,1.82930781209959E-13,
3.77003198860263));
#224117=CARTESIAN_POINT('',(12.4547221284042,60.119220625811,3.77003198802762));
#224118=CARTESIAN_POINT('Origin',(5.49031038273072E-15,1.82930781209959E-13,
3.77003198860263));
#224119=CARTESIAN_POINT('',(12.4547221284867,60.1192206261331,3.77003198860305));
#224120=CARTESIAN_POINT('Origin',(62.2224557307631,1.82930781209959E-13,
3.77003198860263));
#224121=CARTESIAN_POINT('',(6.78290064323541,61.4975385923864,3.77003198860306));
#224122=CARTESIAN_POINT('',(0.995615674755264,6.43520020182058,3.77003198860267));
#224123=CARTESIAN_POINT('',(12.5528626811445,60.5836663843184,3.77003198860305));
#224124=CARTESIAN_POINT('Origin',(5.49031038273072E-15,1.82930781209959E-13,
3.77003198860263));
#224125=CARTESIAN_POINT('',(12.4542754087022,60.1198497339746,3.77003198860305));
#224126=CARTESIAN_POINT('Origin',(5.57972911860581E-15,1.8736496251029E-13,
3.13503198860263));
#224127=CARTESIAN_POINT('Origin',(6.5878591303979,59.6417947880743,3.13502491541472));
#224128=CARTESIAN_POINT('Origin',(12.1649018101382,58.7584780045777,3.13502491541471));
#224129=CARTESIAN_POINT('Origin',(5.57972911860581E-15,1.8736496251029E-13,
3.13503198860263));
#224130=CARTESIAN_POINT('Origin',(6.7869196057536,61.5354556255538,3.20381846780299));
#224131=CARTESIAN_POINT('Origin',(12.5607573437845,60.6209691542431,3.20382022872538));
#224132=CARTESIAN_POINT('Origin',(5.51210908043506E-15,1.8401175575949E-13,
3.61523028058481));
#224133=CARTESIAN_POINT('Origin',(6.6949011606306,60.6606342988062,3.58786945046787));
#224134=CARTESIAN_POINT('Origin',(12.3779177236597,59.7604378032101,3.58781461834168));
#224135=CARTESIAN_POINT('Origin',(5.51210908043507E-15,1.8401175575949E-13,
3.61523028058481));
#224136=CARTESIAN_POINT('Origin',(6.67587182882186,60.4787934153623,3.58781440266664));
#224137=CARTESIAN_POINT('Origin',(12.3398237541835,59.5816164638945,3.5878692359302));
#224138=CARTESIAN_POINT('Origin',(60.4792282238308,1.82930781209959E-13,
3.77003198860263));
#224139=CARTESIAN_POINT('',(18.2401996527044,57.1650137687749,3.77003198860303));
#224140=CARTESIAN_POINT('',(12.786030615045,58.6264539577986,3.77003198860304));
#224141=CARTESIAN_POINT('Origin',(5.49031038273072E-15,1.82930781209959E-13,
3.77003198860263));
#224142=CARTESIAN_POINT('',(12.8847271885942,59.0907848292993,3.77003198860304));
#224143=CARTESIAN_POINT('',(2.92491386234291,12.2335471699534,3.77003198860271));
#224144=CARTESIAN_POINT('',(12.8852923618769,59.090661592063,3.77003198902557));
#224145=CARTESIAN_POINT('Origin',(5.49031038273072E-15,1.82930781209959E-13,
3.77003198860263));
#224146=CARTESIAN_POINT('',(18.3863402753486,57.6166602457575,3.77003198882127));
#224147=CARTESIAN_POINT('Origin',(5.49031038273072E-15,1.82930781209959E-13,
3.77003198860263));
#224148=CARTESIAN_POINT('',(18.3868913484944,57.6164843860299,3.77003198860303));
#224149=CARTESIAN_POINT('Origin',(5.49031038273072E-15,1.82930781209959E-13,
3.77003198860263));
#224150=CARTESIAN_POINT('',(18.2403657795786,57.1655250547209,3.77003198860303));
#224151=CARTESIAN_POINT('Origin',(5.49031038273072E-15,1.82930781209959E-13,
3.77003198860263));
#224152=CARTESIAN_POINT('',(12.9191181862044,59.2498070616282,3.48823028058522));
#224153=CARTESIAN_POINT('',(12.8852923617209,59.090661591348,3.77003198860304));
#224154=CARTESIAN_POINT('',(18.4366189871531,57.7713971780683,3.48823028074845));
#224155=CARTESIAN_POINT('Origin',(5.52999282761009E-15,1.84898592019556E-13,
3.48823028058481));
#224156=CARTESIAN_POINT('',(18.4366189870671,57.7713971777989,3.48823028058521));
#224157=CARTESIAN_POINT('Origin',(60.71525,1.85785428279622E-13,3.36123028058482));
#224158=CARTESIAN_POINT('',(18.505144113284,57.9804289733666,3.36123028058522));
#224159=CARTESIAN_POINT('',(12.9642895838869,59.4650964698968,3.36123028058523));
#224160=CARTESIAN_POINT('Origin',(5.5478765747851E-15,1.85785428279622E-13,
3.36123028058482));
#224161=CARTESIAN_POINT('',(12.9957275188822,59.6130003254557,3.36123028058523));
#224162=CARTESIAN_POINT('',(2.93511643966547,12.2815465224194,3.3612302805849));
#224163=CARTESIAN_POINT('',(18.5518699907149,58.1242364370959,3.36123028058522));
#224164=CARTESIAN_POINT('Origin',(5.5478765747851E-15,1.85785428279622E-13,
3.36123028058482));
#224165=CARTESIAN_POINT('',(18.505307899872,57.9809330566519,3.36123028058522));
#224166=CARTESIAN_POINT('Origin',(5.5478765747851E-15,1.85785428279622E-13,
3.36123028058482));
#224167=CARTESIAN_POINT('',(18.6203878281146,58.3332704847798,3.48823028058524));
#224168=CARTESIAN_POINT('',(13.0409063549819,59.8282880399729,3.48823028042736));
#224169=CARTESIAN_POINT('Origin',(5.52999282761008E-15,1.84898592019556E-13,
3.48823028058484));
#224170=CARTESIAN_POINT('',(13.0747351550709,59.987432788672,3.77003198802749));
#224171=CARTESIAN_POINT('',(13.0409063549237,59.8282880397057,3.48823028058526));
#224172=CARTESIAN_POINT('',(13.0752898951324,59.9873118763438,3.77003198860305));
#224173=CARTESIAN_POINT('Origin',(5.49031038273072E-15,1.82930781209959E-13,
3.77003198860263));
#224174=CARTESIAN_POINT('',(18.6701227271409,58.48818093722,3.77003198860304));
#224175=CARTESIAN_POINT('Origin',(5.49031038273072E-15,1.82930781209959E-13,
3.77003198860263));
#224176=CARTESIAN_POINT('',(18.6706636022907,58.4880082803372,3.77003198802761));
#224177=CARTESIAN_POINT('Origin',(5.49031038273072E-15,1.82930781209959E-13,
3.77003198860263));
#224178=CARTESIAN_POINT('',(18.6706636024065,58.488008280649,3.77003198860304));
#224179=CARTESIAN_POINT('Origin',(62.2224557307631,1.82930781209959E-13,
3.77003198860263));
#224180=CARTESIAN_POINT('',(13.1739864076105,60.4516424606491,3.77003198860305));
#224181=CARTESIAN_POINT('',(3.00026883051124,12.588064422097,3.77003198860271));
#224182=CARTESIAN_POINT('',(18.8168143322225,58.9396512752216,3.77003198860304));
#224183=CARTESIAN_POINT('Origin',(5.49031038273072E-15,1.82930781209959E-13,
3.77003198860263));
#224184=CARTESIAN_POINT('',(18.6702850894756,58.4886806371044,3.77003198860304));
#224185=CARTESIAN_POINT('Origin',(5.57972911860581E-15,1.8736496251029E-13,
3.13503198860263));
#224186=CARTESIAN_POINT('Origin',(12.7860353045046,58.626452004677,3.13502491541474));
#224187=CARTESIAN_POINT('Origin',(18.2401946149522,57.165014422052,3.13502491541474));
#224188=CARTESIAN_POINT('Origin',(5.57972911860581E-15,1.8736496251029E-13,
3.13503198860263));
#224189=CARTESIAN_POINT('Origin',(13.1819467630385,60.4889316843659,3.20381846780306));
#224190=CARTESIAN_POINT('Origin',(18.8285649482899,58.9759244797141,3.20382022872186));
#224191=CARTESIAN_POINT('Origin',(5.51210908043506E-15,1.8401175575949E-13,
3.61523028058481));
#224192=CARTESIAN_POINT('Origin',(12.9989886756684,59.6285212670385,3.5878694504728));
#224193=CARTESIAN_POINT('Origin',(18.5567769230182,58.1392191539783,3.58781461834213));
#224194=CARTESIAN_POINT('Origin',(5.51210908043507E-15,1.8401175575949E-13,
3.61523028058481));
#224195=CARTESIAN_POINT('Origin',(12.9610560404269,59.4496656337922,3.58781440266432));
#224196=CARTESIAN_POINT('Origin',(18.5001997164952,57.9653593207579,3.58786923592793));
#224197=CARTESIAN_POINT('Origin',(60.4792282238308,1.82930781209959E-13,
3.77003198860263));
#224198=CARTESIAN_POINT('',(24.1156489724276,54.9452378026831,3.77003198860301));
#224199=CARTESIAN_POINT('',(18.8441205405518,56.9687879773468,3.77003198860303));
#224200=CARTESIAN_POINT('Origin',(5.49031038273072E-15,1.82930781209959E-13,
3.77003198860263));
#224201=CARTESIAN_POINT('',(18.9908122363901,57.4202585945868,3.77003198860303));
#224202=CARTESIAN_POINT('',(6.07721283595898,17.6762863142852,3.77003198860275));
#224203=CARTESIAN_POINT('',(18.9913614317957,57.4200769557631,3.77003198902602));
#224204=CARTESIAN_POINT('Origin',(5.49031038273072E-15,1.82930781209959E-13,
3.77003198860263));
#224205=CARTESIAN_POINT('',(24.3081989336292,55.3791342583022,3.77003198882125));
#224206=CARTESIAN_POINT('Origin',(5.49031038273072E-15,1.82930781209959E-13,
3.77003198860263));
#224207=CARTESIAN_POINT('',(24.3087286055916,55.3789017591236,3.77003198860302));
#224208=CARTESIAN_POINT('Origin',(5.49031038273072E-15,1.82930781209959E-13,
3.77003198860263));
#224209=CARTESIAN_POINT('',(24.1158676331756,54.9457289227643,3.77003198860301));
#224210=CARTESIAN_POINT('Origin',(5.49031038273072E-15,1.82930781209959E-13,
3.77003198860263));
#224211=CARTESIAN_POINT('',(19.0416371860877,57.5748148483578,3.48823028058521));
#224212=CARTESIAN_POINT('',(18.9913614315656,57.4200769550675,3.77003198860303));
#224213=CARTESIAN_POINT('',(24.3743766271349,55.5277679690274,3.48823028074843));
#224214=CARTESIAN_POINT('Origin',(5.52999282761009E-15,1.84898592019556E-13,
3.48823028058481));
#224215=CARTESIAN_POINT('',(24.3743766270213,55.5277679687685,3.4882302805852));
#224216=CARTESIAN_POINT('Origin',(60.71525,1.85785428279622E-13,3.36123028058482));
#224217=CARTESIAN_POINT('',(24.4643761377916,55.72849184015,3.3612302805852));
#224218=CARTESIAN_POINT('',(19.1090650011314,57.7842031819385,3.36123028058522));
#224219=CARTESIAN_POINT('Origin',(5.5478765747851E-15,1.85785428279622E-13,
3.36123028058482));
#224220=CARTESIAN_POINT('',(19.1557908785624,57.9280106456678,3.36123028058522));
#224221=CARTESIAN_POINT('',(6.09975091006187,17.7456513739113,3.36123028058494));
#224222=CARTESIAN_POINT('',(24.525878019167,55.8666273273835,3.36123028058521));
#224223=CARTESIAN_POINT('Origin',(5.5478765747851E-15,1.85785428279622E-13,
3.36123028058482));
#224224=CARTESIAN_POINT('',(24.4645917181906,55.7289760416541,3.3612302805852));
#224225=CARTESIAN_POINT('Origin',(5.5478765747851E-15,1.85785428279622E-13,
3.36123028058482));
#224226=CARTESIAN_POINT('',(24.6158705164593,56.0673542004328,3.48823028058523));
#224227=CARTESIAN_POINT('',(19.2232259142297,58.1373965172492,3.48823028042735));
#224228=CARTESIAN_POINT('Origin',(5.52999282761008E-15,1.84898592019556E-13,
3.48823028058484));
#224229=CARTESIAN_POINT('',(19.2735045526308,58.2921333818758,3.77003198802748));
#224230=CARTESIAN_POINT('',(19.2232259141438,58.1373965169896,3.48823028058524));
#224231=CARTESIAN_POINT('',(19.2740436149883,58.2919551457919,3.77003198860303));
#224232=CARTESIAN_POINT('Origin',(5.49031038273072E-15,1.82930781209959E-13,
3.77003198860263));
#224233=CARTESIAN_POINT('',(24.6815255140425,56.21621732464,3.77003198860303));
#224234=CARTESIAN_POINT('Origin',(5.49031038273072E-15,1.82930781209959E-13,
3.77003198860263));
#224235=CARTESIAN_POINT('',(24.6820453786631,56.2159890767414,3.7700319880276));
#224236=CARTESIAN_POINT('Origin',(5.49031038273072E-15,1.82930781209959E-13,
3.77003198860263));
#224237=CARTESIAN_POINT('',(24.6820453788107,56.2159890770394,3.77003198860303));
#224238=CARTESIAN_POINT('Origin',(62.2224557307631,1.82930781209959E-13,
3.77003198860263));
#224239=CARTESIAN_POINT('',(19.42073522007,58.7434254837935,3.77003198860304));
#224240=CARTESIAN_POINT('',(6.24367625034007,18.1886080242679,3.77003198860276));
#224241=CARTESIAN_POINT('',(24.8746050278051,56.6498810128384,3.77003198860303));
#224242=CARTESIAN_POINT('Origin',(5.49031038273072E-15,1.82930781209959E-13,
3.77003198860263));
#224243=CARTESIAN_POINT('',(24.6817392198003,56.2166973156308,3.77003198860302));
#224244=CARTESIAN_POINT('Origin',(5.57972911860581E-15,1.8736496251029E-13,
3.13503198860263));
#224245=CARTESIAN_POINT('Origin',(18.8441250001652,56.9687855447427,3.13502491541475));
#224246=CARTESIAN_POINT('Origin',(24.1156440305588,54.9452389789699,3.13502491541474));
#224247=CARTESIAN_POINT('Origin',(5.57972911860581E-15,1.8736496251029E-13,
3.13503198860263));
#224248=CARTESIAN_POINT('Origin',(19.4325497530937,58.77967834952,3.20381846780313));
#224249=CARTESIAN_POINT('Origin',(24.8900828550905,56.6847272350808,3.20382022871978));
#224250=CARTESIAN_POINT('Origin',(5.51210908043506E-15,1.8401175575949E-13,
3.61523028058481));
#224251=CARTESIAN_POINT('Origin',(19.1606565505629,57.9431056782021,3.58786945047102));
#224252=CARTESIAN_POINT('Origin',(24.5323241911531,55.8810150532823,3.58781461834224));
#224253=CARTESIAN_POINT('Origin',(5.51210908043507E-15,1.8401175575949E-13,
3.61523028058481));
#224254=CARTESIAN_POINT('Origin',(19.1042362097724,57.7691948748974,3.58781440266281));
#224255=CARTESIAN_POINT('Origin',(24.4578836192999,55.7140215708719,3.58786923592786));
#224256=CARTESIAN_POINT('Origin',(60.4792282238308,1.82930781209959E-13,
3.77003198860263));
#224257=CARTESIAN_POINT('',(29.7268821954849,52.1234703131949,3.770031988603));
#224258=CARTESIAN_POINT('',(24.6957503380306,54.68696003433,3.77003198860302));
#224259=CARTESIAN_POINT('Origin',(5.49031038273072E-15,1.82930781209959E-13,
3.77003198860263));
#224260=CARTESIAN_POINT('',(24.8888299712411,55.1206239907505,3.77003198860301));
#224261=CARTESIAN_POINT('',(10.295413467953,22.3432738675266,3.77003198860278));
#224262=CARTESIAN_POINT('',(24.8893571716697,55.1203859404114,3.77003198902604));
#224263=CARTESIAN_POINT('Origin',(5.49031038273072E-15,1.82930781209959E-13,
3.77003198860263));
#224264=CARTESIAN_POINT('',(29.9637318775753,52.5348628870841,3.77003198882124));
#224265=CARTESIAN_POINT('Origin',(5.49031038273072E-15,1.82930781209959E-13,
3.77003198860263));
#224266=CARTESIAN_POINT('',(29.9642343451574,52.534576295764,3.770031988603));
#224267=CARTESIAN_POINT('Origin',(5.49031038273072E-15,1.82930781209959E-13,
3.77003198860263));
#224268=CARTESIAN_POINT('',(29.7271509944138,52.1239358865969,3.77003198860299));
#224269=CARTESIAN_POINT('Origin',(5.49031038273072E-15,1.82930781209959E-13,
3.77003198860263));
#224270=CARTESIAN_POINT('',(24.9555320242414,55.2690209153043,3.4882302805852));
#224271=CARTESIAN_POINT('',(24.8893571713682,55.1203859397437,3.77003198860302));
#224272=CARTESIAN_POINT('',(30.0450834961236,52.6757649141854,3.48823028074842));
#224273=CARTESIAN_POINT('Origin',(5.52999282761009E-15,1.84898592019556E-13,
3.48823028058481));
#224274=CARTESIAN_POINT('',(30.0450834959836,52.6757649139398,3.48823028058519));
#224275=CARTESIAN_POINT('Origin',(60.71525,1.85785428279622E-13,3.36123028058482));
#224276=CARTESIAN_POINT('',(30.1555713378337,52.8659816883962,3.36123028058519));
#224277=CARTESIAN_POINT('',(25.0444775033946,55.4702140717969,3.36123028058521));
#224278=CARTESIAN_POINT('Origin',(5.5478765747851E-15,1.85785428279622E-13,
3.36123028058482));
#224279=CARTESIAN_POINT('',(25.1059793847701,55.6083495590304,3.36123028058521));
#224280=CARTESIAN_POINT('',(10.3344596589366,22.4309730483567,3.36123028058497));
#224281=CARTESIAN_POINT('',(30.2311753956711,52.996931757829,3.36123028058519));
#224282=CARTESIAN_POINT('Origin',(5.5478765747851E-15,1.85785428279622E-13,
3.36123028058482));
#224283=CARTESIAN_POINT('',(30.1558363500999,52.8664407031059,3.36123028058519));
#224284=CARTESIAN_POINT('Origin',(5.5478765747851E-15,1.85785428279622E-13,
3.36123028058482));
#224285=CARTESIAN_POINT('',(30.3416565762235,53.1871522506177,3.48823028058522));
#224286=CARTESIAN_POINT('',(25.1949317876425,55.8095395122502,3.48823028042734));
#224287=CARTESIAN_POINT('Origin',(5.52999282761008E-15,1.84898592019556E-13,
3.48823028058484));
#224288=CARTESIAN_POINT('',(25.261109401072,55.9581731633347,3.77003198802746));
#224289=CARTESIAN_POINT('',(25.19493178753,55.8095395120009,3.48823028058523));
#224290=CARTESIAN_POINT('',(25.2616268796456,55.9579395562869,3.77003198860303));
#224291=CARTESIAN_POINT('Origin',(5.49031038273072E-15,1.82930781209959E-13,
3.77003198860263));
#224292=CARTESIAN_POINT('',(30.422512342471,53.3283370710515,3.77003198860301));
#224293=CARTESIAN_POINT('Origin',(5.49031038273072E-15,1.82930781209959E-13,
3.77003198860263));
#224294=CARTESIAN_POINT('',(30.4230055008167,53.3280557328689,3.77003198802758));
#224295=CARTESIAN_POINT('Origin',(5.49031038273072E-15,1.82930781209959E-13,
3.77003198860263));
#224296=CARTESIAN_POINT('',(30.4230055009947,53.3280557331498,3.77003198860301));
#224297=CARTESIAN_POINT('Origin',(62.2224557307631,1.82930781209959E-13,
3.77003198860263));
#224298=CARTESIAN_POINT('',(25.4547063934082,56.3916032444853,3.77003198860303));
#224299=CARTESIAN_POINT('',(10.5838037820516,22.9910091182299,3.77003198860279));
#224300=CARTESIAN_POINT('',(30.6598643453574,53.7394427993289,3.77003198860301));
#224301=CARTESIAN_POINT('Origin',(5.49031038273072E-15,1.82930781209959E-13,
3.77003198860263));
#224302=CARTESIAN_POINT('',(30.422775050247,53.328792094267,3.770031988603));
#224303=CARTESIAN_POINT('Origin',(5.57972911860581E-15,1.8736496251029E-13,
3.13503198860263));
#224304=CARTESIAN_POINT('Origin',(24.6957545189376,54.6869571488953,3.13502491541468));
#224305=CARTESIAN_POINT('Origin',(29.7268774036436,52.1234719996038,3.13502491541472));
#224306=CARTESIAN_POINT('Origin',(5.57972911860581E-15,1.8736496251029E-13,
3.13503198860263));
#224307=CARTESIAN_POINT('Origin',(25.4702456615188,56.4264225582421,3.20381846780199));
#224308=CARTESIAN_POINT('Origin',(30.678899805548,53.7724802568186,3.20382022872022));
#224309=CARTESIAN_POINT('Origin',(5.51210908043506E-15,1.8401175575949E-13,
3.61523028058481));
#224310=CARTESIAN_POINT('Origin',(25.112396262664,55.6228532981801,3.587869450471));
#224311=CARTESIAN_POINT('Origin',(30.2390901817309,53.0105668578086,3.5878146183411));
#224312=CARTESIAN_POINT('Origin',(5.51210908043507E-15,1.8401175575949E-13,
3.61523028058481));
#224313=CARTESIAN_POINT('Origin',(25.0381063693916,55.4557927279711,3.58781440266272));
#224314=CARTESIAN_POINT('Origin',(30.1476018310216,52.8522693417523,3.58786923593059));
#224315=CARTESIAN_POINT('Origin',(60.4792282238308,1.82930781209959E-13,
3.77003198860263));
#224316=CARTESIAN_POINT('',(35.0124214764584,48.7306271754179,3.77003198860297));
#224317=CARTESIAN_POINT('',(30.276808326888,51.8059703131949,3.77003198860299));
#224318=CARTESIAN_POINT('Origin',(5.49031038273072E-15,1.82930781209959E-13,
3.77003198860263));
#224319=CARTESIAN_POINT('',(30.5141604766046,52.2170762957393,3.770031988603));
#224320=CARTESIAN_POINT('',(15.3947701216591,26.0295240215572,3.77003198860281));
#224321=CARTESIAN_POINT('',(30.5146599059377,52.2167844420138,3.77003198902568));
#224322=CARTESIAN_POINT('Origin',(5.49031038273072E-15,1.82930781209959E-13,
3.77003198860263));
#224323=CARTESIAN_POINT('',(35.2909759047567,49.1150085644483,3.77003198882122));
#224324=CARTESIAN_POINT('Origin',(5.49031038273072E-15,1.82930781209959E-13,
3.77003198860263));
#224325=CARTESIAN_POINT('',(35.2914456628186,49.1146710209413,3.77003198860297));
#224326=CARTESIAN_POINT('Origin',(5.49031038273072E-15,1.82930781209959E-13,
3.77003198860263));
#224327=CARTESIAN_POINT('',(35.012737468551,48.7310621012211,3.77003198860297));
#224328=CARTESIAN_POINT('Origin',(5.49031038273072E-15,1.82930781209959E-13,
3.77003198860263));
#224329=CARTESIAN_POINT('',(30.5960088312567,52.3576880233165,3.48823028058518));
#224330=CARTESIAN_POINT('',(30.5146599055683,52.2167844413817,3.770031988603));
#224331=CARTESIAN_POINT('',(35.3866101429909,49.2466351558311,3.48823028074839));
#224332=CARTESIAN_POINT('Origin',(5.52999282761009E-15,1.84898592019556E-13,
3.48823028058481));
#224333=CARTESIAN_POINT('',(35.3866101428259,49.2466351556015,3.48823028058516));
#224334=CARTESIAN_POINT('Origin',(60.71525,1.85785428279622E-13,3.36123028058482));
#224335=CARTESIAN_POINT('',(35.5163757878395,49.4242607783463,3.36123028058517));
#224336=CARTESIAN_POINT('',(30.7054974692368,52.5484816883962,3.36123028058519));
#224337=CARTESIAN_POINT('Origin',(5.5478765747851E-15,1.85785428279622E-13,
3.36123028058482));
#224338=CARTESIAN_POINT('',(30.7811015270742,52.679431757829,3.36123028058519));
#224339=CARTESIAN_POINT('',(15.4537755657014,26.1317244485617,3.361230280585));
#224340=CARTESIAN_POINT('',(35.6052536882601,49.5465907136147,3.36123028058517));
#224341=CARTESIAN_POINT('Origin',(5.5478765747851E-15,1.85785428279622E-13,
3.36123028058482));
#224342=CARTESIAN_POINT('',(35.516687328443,49.4246895772005,3.36123028058516));
#224343=CARTESIAN_POINT('Origin',(5.5478765747851E-15,1.85785428279622E-13,
3.36123028058482));
#224344=CARTESIAN_POINT('',(35.7350130971388,49.7242207306177,3.48823028058519));
#224345=CARTESIAN_POINT('',(30.8905967160115,52.870221513458,3.48823028042732));
#224346=CARTESIAN_POINT('Origin',(5.52999282761008E-15,1.84898592019556E-13,
3.48823028058484));
#224347=CARTESIAN_POINT('',(30.971948248688,53.0111234896156,3.77003198802745));
#224348=CARTESIAN_POINT('',(30.8905967158735,52.8702215132218,3.48823028058522));
#224349=CARTESIAN_POINT('',(30.9724384738741,53.0108370710515,3.77003198860301));
#224350=CARTESIAN_POINT('Origin',(5.49031038273072E-15,1.82930781209959E-13,
3.77003198860263));
#224351=CARTESIAN_POINT('',(35.8301837593554,49.8561803968406,3.77003198860298));
#224352=CARTESIAN_POINT('Origin',(5.49031038273072E-15,1.82930781209959E-13,
3.77003198860263));
#224353=CARTESIAN_POINT('',(35.8306448082802,49.8558490507739,3.77003198802756));
#224354=CARTESIAN_POINT('Origin',(5.49031038273072E-15,1.82930781209959E-13,
3.77003198860263));
#224355=CARTESIAN_POINT('',(35.8306448084866,49.8558490510347,3.77003198860298));
#224356=CARTESIAN_POINT('Origin',(62.2224557307631,1.82930781209959E-13,
3.77003198860263));
#224357=CARTESIAN_POINT('',(31.2097904767605,53.4219427993289,3.77003198860301));
#224358=CARTESIAN_POINT('',(15.8305769983922,26.7843636743468,3.77003198860281));
#224359=CARTESIAN_POINT('',(36.1092077731528,50.2402240048086,3.77003198860298));
#224360=CARTESIAN_POINT('Origin',(5.49031038273072E-15,1.82930781209959E-13,
3.77003198860263));
#224361=CARTESIAN_POINT('',(35.8304925908681,49.8566054669512,3.77003198860297));
#224362=CARTESIAN_POINT('Origin',(5.57972911860581E-15,1.8736496251029E-13,
3.13503198860263));
#224363=CARTESIAN_POINT('Origin',(30.2768121832815,51.8059670065431,3.1350249154147));
#224364=CARTESIAN_POINT('Origin',(35.012416887145,48.7306293534723,3.13502491541466));
#224365=CARTESIAN_POINT('Origin',(5.57972911860581E-15,1.8736496251029E-13,
3.13503198860263));
#224366=CARTESIAN_POINT('Origin',(31.2288842284977,53.4549470734237,3.20381846780249));
#224367=CARTESIAN_POINT('Origin',(36.131592309765,50.2710907322454,3.20382022871924));
#224368=CARTESIAN_POINT('Origin',(5.51210908043506E-15,1.8401175575949E-13,
3.61523028058481));
#224369=CARTESIAN_POINT('Origin',(30.7889993062046,52.6931852975928,3.58786945047126));
#224370=CARTESIAN_POINT('Origin',(35.6145503723404,49.5593237986651,3.5878146183433));
#224371=CARTESIAN_POINT('Origin',(5.51210908043507E-15,1.8401175575949E-13,
3.61523028058481));
#224372=CARTESIAN_POINT('Origin',(30.6976537960638,52.5348053110502,3.58781440266714));
#224373=CARTESIAN_POINT('Origin',(35.5070166083019,49.4114565896684,3.58786923592972));
#224374=CARTESIAN_POINT('Origin',(60.4792282238308,1.82930781209959E-13,
3.77003198860263));
#224375=CARTESIAN_POINT('',(39.9143573409156,44.8038810887677,3.77003198860295));
#224376=CARTESIAN_POINT('',(35.5261472678865,48.3573835402122,3.77003198860297));
#224377=CARTESIAN_POINT('Origin',(5.49031038273072E-15,1.82930781209959E-13,
3.77003198860263));
#224378=CARTESIAN_POINT('',(35.8051714542879,48.7414273857063,3.77003198860297));
#224379=CARTESIAN_POINT('',(21.151922343707,28.5729602337853,3.77003198860282));
#224380=CARTESIAN_POINT('',(35.8056376406733,48.7410849262052,3.77003198902553));
#224381=CARTESIAN_POINT('Origin',(5.49031038273072E-15,1.82930781209959E-13,
3.77003198860263));
#224382=CARTESIAN_POINT('',(40.2315646148141,45.157039930004,3.77003198882119));
#224383=CARTESIAN_POINT('Origin',(5.49031038273072E-15,1.82930781209959E-13,
3.77003198860263));
#224384=CARTESIAN_POINT('',(40.2319965165881,45.1566551325074,3.77003198860295));
#224385=CARTESIAN_POINT('Origin',(5.49031038273072E-15,1.82930781209959E-13,
3.77003198860263));
#224386=CARTESIAN_POINT('',(39.9147170640963,44.804280601834,3.77003198860295));
#224387=CARTESIAN_POINT('Origin',(5.49031038273072E-15,1.82930781209959E-13,
3.77003198860263));
#224388=CARTESIAN_POINT('',(35.9012693628904,48.8727133447946,3.48823028058516));
#224389=CARTESIAN_POINT('',(35.80563764024,48.7410849256154,3.77003198860297));
#224390=CARTESIAN_POINT('',(40.3404336840073,45.2779489571886,3.48823028074837));
#224391=CARTESIAN_POINT('Origin',(5.52999282761009E-15,1.84898592019556E-13,
3.48823028058481));
#224392=CARTESIAN_POINT('',(40.3404336838192,45.2779489569775,3.48823028058513));
#224393=CARTESIAN_POINT('Origin',(60.71525,1.85785428279622E-13,3.36123028058482));
#224394=CARTESIAN_POINT('',(40.4880553924343,45.4410373245174,3.36123028058514));
#224395=CARTESIAN_POINT('',(36.0301015792676,49.0510171431406,3.36123028058517));
#224396=CARTESIAN_POINT('Origin',(5.5478765747851E-15,1.85785428279622E-13,
3.36123028058482));
#224397=CARTESIAN_POINT('',(36.1189794796882,49.173347078409,3.36123028058517));
#224398=CARTESIAN_POINT('',(21.2334658618522,28.685195257892,3.36123028058502));
#224399=CARTESIAN_POINT('',(40.5892333705622,45.5534068532514,3.36123028058514));
#224400=CARTESIAN_POINT('Origin',(5.5478765747851E-15,1.85785428279622E-13,
3.36123028058482));
#224401=CARTESIAN_POINT('',(40.488410048071,45.4414312095061,3.36123028058514));
#224402=CARTESIAN_POINT('Origin',(5.5478765747851E-15,1.85785428279622E-13,
3.36123028058482));
#224403=CARTESIAN_POINT('',(40.7368493365296,45.7165002428309,3.48823028058517));
#224404=CARTESIAN_POINT('',(36.2478178024869,49.3516463039592,3.4882302804273));
#224405=CARTESIAN_POINT('Origin',(5.52999282761008E-15,1.84898592019556E-13,
3.48823028058484));
#224406=CARTESIAN_POINT('',(36.3434519499946,49.4832728536534,3.77003198802742));
#224407=CARTESIAN_POINT('',(36.247817802325,49.3516463037387,3.48823028058519));
#224408=CARTESIAN_POINT('',(36.3439095507835,49.4829367616348,3.77003198860298));
#224409=CARTESIAN_POINT('Origin',(5.49031038273072E-15,1.82930781209959E-13,
3.77003198860263));
#224410=CARTESIAN_POINT('',(40.8452921850243,45.8377889771254,3.77003198860295));
#224411=CARTESIAN_POINT('Origin',(5.49031038273072E-15,1.82930781209959E-13,
3.77003198860263));
#224412=CARTESIAN_POINT('',(40.8457160731797,45.8374112534716,3.77003198802753));
#224413=CARTESIAN_POINT('Origin',(5.49031038273072E-15,1.82930781209959E-13,
3.77003198860263));
#224414=CARTESIAN_POINT('',(40.8457160734122,45.8374112537093,3.77003198860295));
#224415=CARTESIAN_POINT('Origin',(62.2224557307631,1.82930781209959E-13,
3.77003198860263));
#224416=CARTESIAN_POINT('',(36.6229335645808,49.8669803696028,3.77003198860298));
#224417=CARTESIAN_POINT('',(21.7541926348211,29.4019141737118,3.77003198860283));
#224418=CARTESIAN_POINT('',(41.162931164248,46.1905628026487,3.77003198860296));
#224419=CARTESIAN_POINT('Origin',(5.49031038273072E-15,1.82930781209959E-13,
3.77003198860263));
#224420=CARTESIAN_POINT('',(40.8456437566512,45.838179436974,3.77003198860295));
#224421=CARTESIAN_POINT('Origin',(5.57972911860581E-15,1.8736496251029E-13,
3.13503198860263));
#224422=CARTESIAN_POINT('Origin',(35.5261507575148,48.3573798485718,3.13502491541469));
#224423=CARTESIAN_POINT('Origin',(39.9143530044117,44.8038837346043,3.13502491541463));
#224424=CARTESIAN_POINT('Origin',(5.57972911860581E-15,1.8736496251029E-13,
3.13503198860263));
#224425=CARTESIAN_POINT('Origin',(36.6453726047997,49.8978080023046,3.20381846780288));
#224426=CARTESIAN_POINT('Origin',(41.188419527607,46.2189206177163,3.20382022872233));
#224427=CARTESIAN_POINT('Origin',(5.51210908043506E-15,1.8401175575949E-13,
3.61523028058481));
#224428=CARTESIAN_POINT('Origin',(36.1282716303338,49.1861997321267,3.58786945047242));
#224429=CARTESIAN_POINT('Origin',(40.5998100962474,45.5650984170292,3.58781461834315));
#224430=CARTESIAN_POINT('Origin',(5.51210908043507E-15,1.8401175575949E-13,
3.61523028058481));
#224431=CARTESIAN_POINT('Origin',(36.0208713038508,49.0382355735231,3.5878144026671));
#224432=CARTESIAN_POINT('Origin',(40.4774090812936,45.4292815791797,3.58786923592817));
#224433=CARTESIAN_POINT('Origin',(60.4792282238308,1.82930781209959E-13,
3.77003198860263));
#224434=CARTESIAN_POINT('',(44.3789831537295,40.3862543050941,3.77003198860292));
#224435=CARTESIAN_POINT('',(40.3862543050938,44.3789831537298,3.77003198860294));
#224436=CARTESIAN_POINT('Origin',(5.49031038273072E-15,1.82930781209959E-13,
3.77003198860263));
#224437=CARTESIAN_POINT('',(40.7038934808042,44.7317571974362,3.77003198860294));
#224438=CARTESIAN_POINT('',(27.314662201079,29.8615093742685,3.77003198860284));
#224439=CARTESIAN_POINT('',(40.7043213166065,44.7313678842176,3.77003198902556));
#224440=CARTESIAN_POINT('Origin',(5.49031038273072E-15,1.82930781209959E-13,
3.77003198860263));
#224441=CARTESIAN_POINT('',(44.7313678839555,40.7043213163686,3.77003198882116));
#224442=CARTESIAN_POINT('Origin',(5.49031038273072E-15,1.82930781209959E-13,
3.77003198860263));
#224443=CARTESIAN_POINT('',(44.7317571974354,40.7038934808041,3.77003198860292));
#224444=CARTESIAN_POINT('Origin',(5.49031038273072E-15,1.82930781209959E-13,
3.77003198860263));
#224445=CARTESIAN_POINT('',(44.3793826667958,40.3866140282747,3.77003198860292));
#224446=CARTESIAN_POINT('Origin',(5.49031038273072E-15,1.82930781209959E-13,
3.77003198860263));
#224447=CARTESIAN_POINT('',(40.8131880745606,44.8522789915944,3.48823028058513));
#224448=CARTESIAN_POINT('',(40.7043213161139,44.7313678836762,3.77003198860295));
#224449=CARTESIAN_POINT('',(44.8522789918032,40.8131880747512,3.48823028074834));
#224450=CARTESIAN_POINT('Origin',(5.52999282761009E-15,1.84898592019556E-13,
3.48823028058481));
#224451=CARTESIAN_POINT('',(44.8522789915941,40.8131880745609,3.4882302805851));
#224452=CARTESIAN_POINT('Origin',(60.71525,1.85785428279622E-13,3.36123028058482));
#224453=CARTESIAN_POINT('',(45.0161393894793,40.9599523566127,3.36123028058511));
#224454=CARTESIAN_POINT('',(40.9599523566124,45.0161393894796,3.36123028058514));
#224455=CARTESIAN_POINT('Origin',(5.5478765747851E-15,1.85785428279622E-13,
3.36123028058482));
#224456=CARTESIAN_POINT('',(41.0611303347403,45.1285089182135,3.36123028058514));
#224457=CARTESIAN_POINT('',(27.4203375923833,29.9788737863605,3.36123028058502));
#224458=CARTESIAN_POINT('',(45.1285089182132,41.0611303347406,3.36123028058511));
#224459=CARTESIAN_POINT('Origin',(5.5478765747851E-15,1.85785428279622E-13,
3.36123028058482));
#224460=CARTESIAN_POINT('',(45.0165332744679,40.9603070122495,3.36123028058511));
#224461=CARTESIAN_POINT('Origin',(5.5478765747851E-15,1.85785428279622E-13,
3.36123028058482));
#224462=CARTESIAN_POINT('',(45.2923641298556,41.207900211591,3.48823028058513));
#224463=CARTESIAN_POINT('',(41.2079002117747,45.2923641300583,3.48823028042727));
#224464=CARTESIAN_POINT('Origin',(5.52999282761008E-15,1.84898592019556E-13,
3.48823028058484));
#224465=CARTESIAN_POINT('',(41.3167691863808,45.4132731252661,3.77003198802739));
#224466=CARTESIAN_POINT('',(41.2079002115907,45.292364129856,3.48823028058516));
#224467=CARTESIAN_POINT('',(41.3171891492024,45.4128910420875,3.77003198860295));
#224468=CARTESIAN_POINT('Origin',(5.49031038273072E-15,1.82930781209959E-13,
3.77003198860263));
#224469=CARTESIAN_POINT('',(45.4128910420872,41.3171891492028,3.77003198860292));
#224470=CARTESIAN_POINT('Origin',(5.49031038273072E-15,1.82930781209959E-13,
3.77003198860263));
#224471=CARTESIAN_POINT('',(45.4132731252658,41.3167691863812,3.7700319880275));
#224472=CARTESIAN_POINT('Origin',(5.49031038273072E-15,1.82930781209959E-13,
3.77003198860263));
#224473=CARTESIAN_POINT('',(45.4132731255219,41.3167691865933,3.77003198860292));
#224474=CARTESIAN_POINT('Origin',(62.2224557307631,1.82930781209959E-13,
3.77003198860263));
#224475=CARTESIAN_POINT('',(41.6348281284261,45.7656648676109,3.77003198860295));
#224476=CARTESIAN_POINT('',(28.0951675083324,30.7283483363947,3.77003198860284));
#224477=CARTESIAN_POINT('',(45.7656648676106,41.6348281284264,3.77003198860293));
#224478=CARTESIAN_POINT('Origin',(5.49031038273072E-15,1.82930781209959E-13,
3.77003198860263));
#224479=CARTESIAN_POINT('',(45.4132815019358,41.3175407208296,3.77003198860292));
#224480=CARTESIAN_POINT('Origin',(5.57972911860581E-15,1.8736496251029E-13,
3.13503198860263));
#224481=CARTESIAN_POINT('Origin',(40.3862573897244,44.378979117547,3.13502491541459));
#224482=CARTESIAN_POINT('Origin',(44.3789791175466,40.3862573897247,3.13502491541461));
#224483=CARTESIAN_POINT('Origin',(5.57972911860581E-15,1.8736496251029E-13,
3.13503198860263));
#224484=CARTESIAN_POINT('Origin',(41.6603666103045,45.793978104926,3.20381846780249));
#224485=CARTESIAN_POINT('Origin',(45.7939778018837,41.6603663369562,3.20382022872035));
#224486=CARTESIAN_POINT('Origin',(5.51210908043506E-15,1.8401175575949E-13,
3.61523028058481));
#224487=CARTESIAN_POINT('Origin',(41.0717150501554,45.140319869523,3.58786945046952));
#224488=CARTESIAN_POINT('Origin',(45.1402498046841,41.0716522820273,3.58781461834098));
#224489=CARTESIAN_POINT('Origin',(5.51210908043507E-15,1.8401175575949E-13,
3.61523028058481));
#224490=CARTESIAN_POINT('Origin',(40.9494366077803,45.0043926651426,3.58781440266742));
#224491=CARTESIAN_POINT('Origin',(45.0043225899514,40.9493738530214,3.58786923593014));
#224492=CARTESIAN_POINT('Origin',(60.4792282238308,1.82930781209959E-13,
3.77003198860263));
#224493=CARTESIAN_POINT('',(48.3573835402119,35.5261472678868,3.77003198860288));
#224494=CARTESIAN_POINT('',(44.8038810887674,39.9143573409159,3.77003198860291));
#224495=CARTESIAN_POINT('Origin',(5.49031038273072E-15,1.82930781209959E-13,
3.77003198860263));
#224496=CARTESIAN_POINT('',(45.1566551325075,40.2319965165889,3.77003198860291));
#224497=CARTESIAN_POINT('',(33.6129634723596,29.8380098596984,3.77003198860284));
#224498=CARTESIAN_POINT('',(45.1570399302682,40.2315646150501,3.77003198902562));
#224499=CARTESIAN_POINT('Origin',(5.49031038273072E-15,1.82930781209959E-13,
3.77003198860263));
#224500=CARTESIAN_POINT('',(48.7410849259197,35.8056376404642,3.77003198882112));
#224501=CARTESIAN_POINT('Origin',(5.49031038273072E-15,1.82930781209959E-13,
3.77003198860263));
#224502=CARTESIAN_POINT('',(48.7414273857055,35.8051714542879,3.77003198860288));
#224503=CARTESIAN_POINT('Origin',(5.49031038273072E-15,1.82930781209959E-13,
3.77003198860263));
#224504=CARTESIAN_POINT('',(48.3578184660151,35.5264632599794,3.77003198860288));
#224505=CARTESIAN_POINT('Origin',(5.49031038273072E-15,1.82930781209959E-13,
3.77003198860263));
#224506=CARTESIAN_POINT('',(45.2779489569772,40.3404336838195,3.4882302805851));
#224507=CARTESIAN_POINT('',(45.1570399297215,40.231564614563,3.77003198860292));
#224508=CARTESIAN_POINT('',(48.8727133450222,35.9012693630581,3.4882302807483));
#224509=CARTESIAN_POINT('Origin',(5.52999282761009E-15,1.84898592019556E-13,
3.48823028058481));
#224510=CARTESIAN_POINT('',(48.8727133447943,35.9012693628907,3.48823028058507));
#224511=CARTESIAN_POINT('Origin',(60.71525,1.85785428279622E-13,3.36123028058482));
#224512=CARTESIAN_POINT('',(49.0510171431403,36.0301015792679,3.36123028058508));
#224513=CARTESIAN_POINT('',(45.4410373245171,40.4880553924346,3.3612302805851));
#224514=CARTESIAN_POINT('Origin',(5.5478765747851E-15,1.85785428279622E-13,
3.36123028058482));
#224515=CARTESIAN_POINT('',(45.5534068532511,40.5892333705625,3.36123028058511));
#224516=CARTESIAN_POINT('',(33.7433098572246,29.9553742717904,3.36123028058502));
#224517=CARTESIAN_POINT('',(49.1733470784087,36.1189794796885,3.36123028058508));
#224518=CARTESIAN_POINT('Origin',(5.5478765747851E-15,1.85785428279622E-13,
3.36123028058482));
#224519=CARTESIAN_POINT('',(49.0514459419945,36.0304131198714,3.36123028058508));
#224520=CARTESIAN_POINT('Origin',(5.5478765747851E-15,1.85785428279622E-13,
3.36123028058482));
#224521=CARTESIAN_POINT('',(49.3516463037384,36.2478178023253,3.4882302805851));
#224522=CARTESIAN_POINT('',(45.7165002430348,40.7368493367119,3.48823028042724));
#224523=CARTESIAN_POINT('Origin',(5.52999282761008E-15,1.84898592019556E-13,
3.48823028058484));
#224524=CARTESIAN_POINT('',(45.8374112534712,40.8457160731799,3.77003198802736));
#224525=CARTESIAN_POINT('',(45.7165002428306,40.73684933653,3.48823028058513));
#224526=CARTESIAN_POINT('',(45.8377889771251,40.8452921850246,3.77003198860292));
#224527=CARTESIAN_POINT('Origin',(5.49031038273072E-15,1.82930781209959E-13,
3.77003198860263));
#224528=CARTESIAN_POINT('',(49.4829367616345,36.3439095507838,3.77003198860289));
#224529=CARTESIAN_POINT('Origin',(5.49031038273072E-15,1.82930781209959E-13,
3.77003198860263));
#224530=CARTESIAN_POINT('',(49.4832728536532,36.343451949995,3.77003198802746));
#224531=CARTESIAN_POINT('Origin',(5.49031038273072E-15,1.82930781209959E-13,
3.77003198860263));
#224532=CARTESIAN_POINT('',(49.48327285393,36.3434519501792,3.77003198860289));
#224533=CARTESIAN_POINT('Origin',(62.2224557307631,1.82930781209959E-13,
3.77003198860263));
#224534=CARTESIAN_POINT('',(46.1905628026484,41.1629311642483,3.77003198860292));
#224535=CARTESIAN_POINT('',(34.5756856720385,30.7048488218246,3.77003198860284));
#224536=CARTESIAN_POINT('',(49.8669803696025,36.6229335645812,3.77003198860289));
#224537=CARTESIAN_POINT('Origin',(5.49031038273072E-15,1.82930781209959E-13,
3.77003198860263));
#224538=CARTESIAN_POINT('',(49.4833618317452,36.3442183822966,3.77003198860289));
#224539=CARTESIAN_POINT('Origin',(5.57972911860581E-15,1.8736496251029E-13,
3.13503198860263));
#224540=CARTESIAN_POINT('Origin',(44.8038837346038,39.9143530044123,3.13502491541461));
#224541=CARTESIAN_POINT('Origin',(48.3573798485713,35.5261507575156,3.13502491541455));
#224542=CARTESIAN_POINT('Origin',(5.57972911860581E-15,1.8736496251029E-13,
3.13503198860263));
#224543=CARTESIAN_POINT('Origin',(46.2189209212384,41.1884198004221,3.20381846780305));
#224544=CARTESIAN_POINT('Origin',(49.8978076723488,36.6453723646243,3.20382022871834));
#224545=CARTESIAN_POINT('Origin',(5.51210908043506E-15,1.8401175575949E-13,
3.61523028058481));
#224546=CARTESIAN_POINT('Origin',(45.5651681650784,40.5998732162089,3.58786945046786));
#224547=CARTESIAN_POINT('Origin',(49.1861234900541,36.1282165298258,3.58781461834413));
#224548=CARTESIAN_POINT('Origin',(5.51210908043507E-15,1.8401175575949E-13,
3.61523028058481));
#224549=CARTESIAN_POINT('Origin',(45.4293513150117,40.4774722129473,3.58781440266322));
#224550=CARTESIAN_POINT('Origin',(49.0381593225504,36.0208162177234,3.58786923592905));
#224551=CARTESIAN_POINT('Origin',(60.4792282238308,1.82930781209959E-13,
3.77003198860263));
#224552=CARTESIAN_POINT('',(51.8059703131946,30.2768083268883,3.77003198860285));
#224553=CARTESIAN_POINT('',(48.7306271754176,35.0124214764587,3.77003198860288));
#224554=CARTESIAN_POINT('Origin',(5.49031038273072E-15,1.82930781209959E-13,
3.77003198860263));
#224555=CARTESIAN_POINT('',(49.1146710209415,35.2914456628193,3.77003198860288));
#224556=CARTESIAN_POINT('',(39.7707905934405,28.5027191556742,3.77003198860283));
#224557=CARTESIAN_POINT('',(49.1150085647359,35.290975904964,3.77003198902583));
#224558=CARTESIAN_POINT('Origin',(5.49031038273072E-15,1.82930781209959E-13,
3.77003198860263));
#224559=CARTESIAN_POINT('',(52.2167844417078,30.5146599057594,3.77003198882108));
#224560=CARTESIAN_POINT('Origin',(5.49031038273072E-15,1.82930781209959E-13,
3.77003198860263));
#224561=CARTESIAN_POINT('',(52.2170762957385,30.5141604766047,3.77003198860285));
#224562=CARTESIAN_POINT('Origin',(5.49031038273072E-15,1.82930781209959E-13,
3.77003198860263));
#224563=CARTESIAN_POINT('',(51.8064358865966,30.2770771258173,3.77003198860285));
#224564=CARTESIAN_POINT('Origin',(5.49031038273072E-15,1.82930781209959E-13,
3.77003198860263));
#224565=CARTESIAN_POINT('',(49.2466351556012,35.3866101428262,3.48823028058506));
#224566=CARTESIAN_POINT('',(49.115008564141,35.2909759045365,3.77003198860288));
#224567=CARTESIAN_POINT('',(52.3576880235603,30.5960088313998,3.48823028074826));
#224568=CARTESIAN_POINT('Origin',(5.52999282761009E-15,1.84898592019556E-13,
3.48823028058481));
#224569=CARTESIAN_POINT('',(52.3576880233162,30.5960088312571,3.48823028058503));
#224570=CARTESIAN_POINT('Origin',(60.71525,1.85785428279622E-13,3.36123028058482));
#224571=CARTESIAN_POINT('',(52.5484816883959,30.7054974692372,3.36123028058504));
#224572=CARTESIAN_POINT('',(49.424260778346,35.5163757878398,3.36123028058507));
#224573=CARTESIAN_POINT('Origin',(5.5478765747851E-15,1.85785428279622E-13,
3.36123028058482));
#224574=CARTESIAN_POINT('',(49.5465907136144,35.6052536882604,3.36123028058507));
#224575=CARTESIAN_POINT('',(39.9252688514646,28.6149541797808,3.36123028058502));
#224576=CARTESIAN_POINT('',(52.6794317578287,30.7811015270746,3.36123028058504));
#224577=CARTESIAN_POINT('Origin',(5.5478765747851E-15,1.85785428279622E-13,
3.36123028058482));
#224578=CARTESIAN_POINT('',(52.5489407031056,30.7057624815034,3.36123028058504));
#224579=CARTESIAN_POINT('Origin',(5.5478765747851E-15,1.85785428279622E-13,
3.36123028058482));
#224580=CARTESIAN_POINT('',(52.8702215132216,30.8905967158739,3.48823028058506));
#224581=CARTESIAN_POINT('',(49.7242207308395,35.7350130972988,3.4882302804272));
#224582=CARTESIAN_POINT('Origin',(5.52999282761008E-15,1.84898592019556E-13,
3.48823028058484));
#224583=CARTESIAN_POINT('',(49.8558490507736,35.8306448082805,3.77003198802733));
#224584=CARTESIAN_POINT('',(49.7242207306174,35.7350130971392,3.4882302805851));
#224585=CARTESIAN_POINT('',(49.8561803968403,35.8301837593557,3.77003198860288));
#224586=CARTESIAN_POINT('Origin',(5.49031038273072E-15,1.82930781209959E-13,
3.77003198860263));
#224587=CARTESIAN_POINT('',(53.0108370710512,30.9724384738745,3.77003198860285));
#224588=CARTESIAN_POINT('Origin',(5.49031038273072E-15,1.82930781209959E-13,
3.77003198860263));
#224589=CARTESIAN_POINT('',(53.0111234896153,30.9719482486884,3.77003198802743));
#224590=CARTESIAN_POINT('Origin',(5.49031038273072E-15,1.82930781209959E-13,
3.77003198860263));
#224591=CARTESIAN_POINT('',(53.01112348991,30.9719482488427,3.77003198860285));
#224592=CARTESIAN_POINT('Origin',(62.2224557307631,1.82930781209959E-13,
3.77003198860263));
#224593=CARTESIAN_POINT('',(50.2402240048083,36.1092077731531,3.77003198860289));
#224594=CARTESIAN_POINT('',(40.9117478092586,29.3316730956006,3.77003198860284));
#224595=CARTESIAN_POINT('',(53.4219427993286,31.2097904767608,3.77003198860285));
#224596=CARTESIAN_POINT('Origin',(5.49031038273072E-15,1.82930781209959E-13,
3.77003198860263));
#224597=CARTESIAN_POINT('',(53.0112920942667,30.9727011816505,3.77003198860285));
#224598=CARTESIAN_POINT('Origin',(5.57972911860581E-15,1.8736496251029E-13,
3.13503198860263));
#224599=CARTESIAN_POINT('Origin',(48.7306293534718,35.0124168871457,3.13502491541459));
#224600=CARTESIAN_POINT('Origin',(51.8059670065428,30.276812183282,3.13502491541455));
#224601=CARTESIAN_POINT('Origin',(5.57972911860581E-15,1.8736496251029E-13,
3.13503198860263));
#224602=CARTESIAN_POINT('Origin',(50.2710910626284,36.1315925493517,3.20381846780242));
#224603=CARTESIAN_POINT('Origin',(53.4549467201727,31.2288840241313,3.20382022872574));
#224604=CARTESIAN_POINT('Origin',(5.51210908043506E-15,1.8401175575949E-13,
3.61523028058481));
#224605=CARTESIAN_POINT('Origin',(49.5593997624585,35.614605855867,3.58786945047113));
#224606=CARTESIAN_POINT('Origin',(52.6931037136114,30.78895247701,3.58781461834159));
#224607=CARTESIAN_POINT('Origin',(5.51210908043507E-15,1.8401175575949E-13,
3.61523028058481));
#224608=CARTESIAN_POINT('Origin',(49.4115325425393,35.5070721047293,3.5878144026661));
#224609=CARTESIAN_POINT('Origin',(52.5347237197189,30.6976069821031,3.58786923592938));
#224610=CARTESIAN_POINT('Origin',(60.4792282238308,1.82930781209959E-13,
3.77003198860263));
#224611=CARTESIAN_POINT('',(54.6869600343297,24.695750338031,3.77003198860281));
#224612=CARTESIAN_POINT('',(52.1234703131946,29.7268821954852,3.77003198860284));
#224613=CARTESIAN_POINT('Origin',(5.49031038273072E-15,1.82930781209959E-13,
3.77003198860263));
#224614=CARTESIAN_POINT('',(52.5345762957643,29.9642343451581,3.77003198860284));
#224615=CARTESIAN_POINT('',(45.518171167873,25.9133109558558,3.77003198860281));
#224616=CARTESIAN_POINT('',(52.5348628873916,29.9637318777512,3.77003198902563));
#224617=CARTESIAN_POINT('Origin',(5.49031038273072E-15,1.82930781209959E-13,
3.77003198860263));
#224618=CARTESIAN_POINT('',(55.1203859400879,24.8893571715241,3.77003198882105));
#224619=CARTESIAN_POINT('Origin',(5.49031038273072E-15,1.82930781209959E-13,
3.77003198860263));
#224620=CARTESIAN_POINT('',(55.1206239907496,24.8888299712412,3.77003198860281));
#224621=CARTESIAN_POINT('Origin',(5.49031038273072E-15,1.82930781209959E-13,
3.77003198860263));
#224622=CARTESIAN_POINT('',(54.6874511544109,24.6959689987791,3.77003198860281));
#224623=CARTESIAN_POINT('Origin',(5.49031038273072E-15,1.82930781209959E-13,
3.77003198860263));
#224624=CARTESIAN_POINT('',(52.6757649139395,30.0450834959839,3.48823028058503));
#224625=CARTESIAN_POINT('',(52.5348628867555,29.9637318773884,3.77003198860284));
#224626=CARTESIAN_POINT('',(55.2690209155617,24.9555320243581,3.48823028074822));
#224627=CARTESIAN_POINT('Origin',(5.52999282761009E-15,1.84898592019556E-13,
3.48823028058481));
#224628=CARTESIAN_POINT('',(55.269020915304,24.9555320242418,3.48823028058499));
#224629=CARTESIAN_POINT('Origin',(60.71525,1.85785428279622E-13,3.36123028058482));
#224630=CARTESIAN_POINT('',(55.4702140717966,25.044477503395,3.361230280585));
#224631=CARTESIAN_POINT('',(52.8659816883959,30.155571337834,3.36123028058503));
#224632=CARTESIAN_POINT('Origin',(5.5478765747851E-15,1.85785428279622E-13,
3.36123028058482));
#224633=CARTESIAN_POINT('',(52.9969317578287,30.2311753956715,3.36123028058503));
#224634=CARTESIAN_POINT('',(45.6951875,26.0155113828602,3.361230280585));
#224635=CARTESIAN_POINT('',(55.6083495590301,25.1059793847704,3.361230280585));
#224636=CARTESIAN_POINT('Origin',(5.5478765747851E-15,1.85785428279622E-13,
3.36123028058482));
#224637=CARTESIAN_POINT('',(55.4706982733007,25.0446930837941,3.361230280585));
#224638=CARTESIAN_POINT('Origin',(5.5478765747851E-15,1.85785428279622E-13,
3.36123028058482));
#224639=CARTESIAN_POINT('',(55.8095395120007,25.1949317875303,3.48823028058502));
#224640=CARTESIAN_POINT('',(53.187152250855,30.3416565763594,3.48823028042716));
#224641=CARTESIAN_POINT('Origin',(5.52999282761008E-15,1.84898592019556E-13,
3.48823028058484));
#224642=CARTESIAN_POINT('',(53.3280557328685,30.423005500817,3.77003198802729));
#224643=CARTESIAN_POINT('',(53.1871522506175,30.3416565762239,3.48823028058506));
#224644=CARTESIAN_POINT('',(53.3283370710512,30.4225123424714,3.77003198860285));
#224645=CARTESIAN_POINT('Origin',(5.49031038273072E-15,1.82930781209959E-13,
3.77003198860263));
#224646=CARTESIAN_POINT('',(55.9579395562866,25.2616268796459,3.77003198860281));
#224647=CARTESIAN_POINT('Origin',(5.49031038273072E-15,1.82930781209959E-13,
3.77003198860263));
#224648=CARTESIAN_POINT('',(55.9581731633345,25.2611094010724,3.77003198802739));
#224649=CARTESIAN_POINT('Origin',(5.49031038273072E-15,1.82930781209959E-13,
3.77003198860263));
#224650=CARTESIAN_POINT('',(55.9581731636437,25.261109401195,3.77003198860281));
#224651=CARTESIAN_POINT('Origin',(62.2224557307631,1.82930781209959E-13,
3.77003198860263));
#224652=CARTESIAN_POINT('',(53.7394427993286,30.6598643453577,3.77003198860285));
#224653=CARTESIAN_POINT('',(46.8255917980722,26.6681506086454,3.77003198860282));
#224654=CARTESIAN_POINT('',(56.391603244485,25.4547063934086,3.77003198860281));
#224655=CARTESIAN_POINT('Origin',(5.49031038273072E-15,1.82930781209959E-13,
3.77003198860263));
#224656=CARTESIAN_POINT('',(55.9584195472775,25.2618405854037,3.77003198860281));
#224657=CARTESIAN_POINT('Origin',(5.57972911860581E-15,1.8736496251029E-13,
3.13503198860263));
#224658=CARTESIAN_POINT('Origin',(52.1234719996034,29.7268774036441,3.13502491541453));
#224659=CARTESIAN_POINT('Origin',(54.6869571488949,24.6957545189382,3.13502491541452));
#224660=CARTESIAN_POINT('Origin',(5.57972911860581E-15,1.8736496251029E-13,
3.13503198860263));
#224661=CARTESIAN_POINT('Origin',(53.7724806104344,30.6789000092885,3.20381846780295));
#224662=CARTESIAN_POINT('Origin',(56.4264221855617,25.4702454951996,3.20382022872323));
#224663=CARTESIAN_POINT('Origin',(5.51210908043506E-15,1.8401175575949E-13,
3.61523028058481));
#224664=CARTESIAN_POINT('Origin',(53.0106482050721,30.2391374209343,3.58786945046861));
#224665=CARTESIAN_POINT('Origin',(55.62276726614,25.1123582178526,3.58781461834227));
#224666=CARTESIAN_POINT('Origin',(5.51210908043507E-15,1.8401175575949E-13,
3.61523028058481));
#224667=CARTESIAN_POINT('Origin',(52.8523506794959,30.1476490842084,3.58781440266723));
#224668=CARTESIAN_POINT('Origin',(55.4557066902163,25.0380683404988,3.58786923592829));
#224669=CARTESIAN_POINT('Origin',(60.4792282238308,1.82930781209959E-13,
3.77003198860263));
#224670=CARTESIAN_POINT('',(56.9687879773466,18.8441205405522,3.77003198860277));
#224671=CARTESIAN_POINT('',(54.9452378026828,24.1156489724279,3.7700319886028));
#224672=CARTESIAN_POINT('Origin',(5.49031038273072E-15,1.82930781209959E-13,
3.77003198860263));
#224673=CARTESIAN_POINT('',(55.3789017591239,24.3087286055922,3.7700319886028));
#224674=CARTESIAN_POINT('',(50.6030043228557,22.1823620689018,3.77003198860279));
#224675=CARTESIAN_POINT('',(55.3791342586263,24.3081989337719,3.77003198902557));
#224676=CARTESIAN_POINT('Origin',(5.49031038273072E-15,1.82930781209959E-13,
3.77003198860263));
#224677=CARTESIAN_POINT('',(57.4200769554261,18.9913614316847,3.770031988821));
#224678=CARTESIAN_POINT('Origin',(5.49031038273072E-15,1.82930781209959E-13,
3.77003198860263));
#224679=CARTESIAN_POINT('',(57.420258594586,18.9908122363903,3.77003198860277));
#224680=CARTESIAN_POINT('Origin',(5.49031038273072E-15,1.82930781209959E-13,
3.77003198860263));
#224681=CARTESIAN_POINT('',(56.9692992632926,18.8442866674264,3.77003198860277));
#224682=CARTESIAN_POINT('Origin',(5.49031038273072E-15,1.82930781209959E-13,
3.77003198860263));
#224683=CARTESIAN_POINT('',(55.5277679687683,24.3743766270217,3.48823028058499));
#224684=CARTESIAN_POINT('',(55.3791342579558,24.3081989334776,3.7700319886028));
#224685=CARTESIAN_POINT('',(57.574814848626,19.0416371861768,3.48823028074819));
#224686=CARTESIAN_POINT('Origin',(5.52999282761009E-15,1.84898592019556E-13,
3.48823028058481));
#224687=CARTESIAN_POINT('',(57.5748148483576,19.041637186088,3.48823028058495));
#224688=CARTESIAN_POINT('Origin',(60.71525,1.85785428279622E-13,3.36123028058482));
#224689=CARTESIAN_POINT('',(57.7842031819382,19.1090650011318,3.36123028058496));
#224690=CARTESIAN_POINT('',(55.7284918401498,24.464376137792,3.36123028058499));
#224691=CARTESIAN_POINT('Origin',(5.5478765747851E-15,1.85785428279622E-13,
3.36123028058482));
#224692=CARTESIAN_POINT('',(55.8666273273833,24.5258780191674,3.36123028058499));
#224693=CARTESIAN_POINT('',(50.7999799080414,22.2700612497319,3.36123028058498));
#224694=CARTESIAN_POINT('',(57.9280106456676,19.1557908785627,3.36123028058496));
#224695=CARTESIAN_POINT('Origin',(5.5478765747851E-15,1.85785428279622E-13,
3.36123028058482));
#224696=CARTESIAN_POINT('',(57.7847072652236,19.1092287877198,3.36123028058496));
#224697=CARTESIAN_POINT('Origin',(5.5478765747851E-15,1.85785428279622E-13,
3.36123028058482));
#224698=CARTESIAN_POINT('',(58.1373965169893,19.2232259141442,3.48823028058498));
#224699=CARTESIAN_POINT('',(56.067354200683,24.6158705165696,3.48823028042713));
#224700=CARTESIAN_POINT('Origin',(5.52999282761008E-15,1.84898592019556E-13,
3.48823028058484));
#224701=CARTESIAN_POINT('',(56.2159890767411,24.6820453786634,3.77003198802725));
#224702=CARTESIAN_POINT('',(56.0673542004326,24.6158705164596,3.48823028058502));
#224703=CARTESIAN_POINT('',(56.2162173246397,24.6815255140429,3.77003198860281));
#224704=CARTESIAN_POINT('Origin',(5.49031038273072E-15,1.82930781209959E-13,
3.77003198860263));
#224705=CARTESIAN_POINT('',(58.2919551457916,19.2740436149887,3.77003198860277));
#224706=CARTESIAN_POINT('Origin',(5.49031038273072E-15,1.82930781209959E-13,
3.77003198860263));
#224707=CARTESIAN_POINT('',(58.2921333818757,19.2735045526312,3.77003198802735));
#224708=CARTESIAN_POINT('Origin',(5.49031038273072E-15,1.82930781209959E-13,
3.77003198860263));
#224709=CARTESIAN_POINT('',(58.2921333821959,19.2735045527209,3.77003198860277));
#224710=CARTESIAN_POINT('Origin',(62.2224557307631,1.82930781209959E-13,
3.77003198860263));
#224711=CARTESIAN_POINT('',(56.6498810128382,24.8746050278055,3.77003198860281));
#224712=CARTESIAN_POINT('',(52.0578415156894,22.8300973196051,3.77003198860279));
#224713=CARTESIAN_POINT('',(58.7434254837932,19.4207352200703,3.77003198860277));
#224714=CARTESIAN_POINT('Origin',(5.49031038273072E-15,1.82930781209959E-13,
3.77003198860263));
#224715=CARTESIAN_POINT('',(58.2924548456761,19.2742059773234,3.77003198860277));
#224716=CARTESIAN_POINT('Origin',(5.57972911860581E-15,1.8736496251029E-13,
3.13503198860263));
#224717=CARTESIAN_POINT('Origin',(54.9452389789695,24.1156440305594,3.1350249154145));
#224718=CARTESIAN_POINT('Origin',(56.9687855447424,18.8441250001659,3.13502491541445));
#224719=CARTESIAN_POINT('Origin',(5.57972911860581E-15,1.8736496251029E-13,
3.13503198860263));
#224720=CARTESIAN_POINT('Origin',(56.6847276080577,24.8900830207505,3.20381846780404));
#224721=CARTESIAN_POINT('Origin',(58.7796779614983,19.4325496266339,3.20382022872385));
#224722=CARTESIAN_POINT('Origin',(5.51210908043506E-15,1.8401175575949E-13,
3.61523028058481));
#224723=CARTESIAN_POINT('Origin',(55.8811008927585,24.5323626684708,3.58786945046915));
#224724=CARTESIAN_POINT('Origin',(57.943016140689,19.1606277069619,3.58781461834233));
#224725=CARTESIAN_POINT('Origin',(5.51210908043507E-15,1.8401175575949E-13,
3.61523028058481));
#224726=CARTESIAN_POINT('Origin',(55.7141074023463,24.4579221115114,3.58781440266683));
#224727=CARTESIAN_POINT('Origin',(57.7691053333667,19.1042073826001,3.58786923593115));
#224728=CARTESIAN_POINT('Origin',(60.4792282238308,1.82930781209959E-13,
3.77003198860263));
#224729=CARTESIAN_POINT('',(58.6264539577984,12.7860306150453,3.77003198860272));
#224730=CARTESIAN_POINT('',(57.1650137687747,18.2401996527048,3.77003198860276));
#224731=CARTESIAN_POINT('Origin',(5.49031038273072E-15,1.82930781209959E-13,
3.77003198860263));
#224732=CARTESIAN_POINT('',(57.6164843860303,18.386891348495,3.77003198860276));
#224733=CARTESIAN_POINT('',(54.8020887275094,17.4724387660757,3.77003198860276));
#224734=CARTESIAN_POINT('',(57.6166602460946,18.3863402754566,3.77003198902546));
#224735=CARTESIAN_POINT('Origin',(5.49031038273072E-15,1.82930781209959E-13,
3.77003198860263));
#224736=CARTESIAN_POINT('',(59.0906615917171,12.8852923618019,3.77003198882096));
#224737=CARTESIAN_POINT('Origin',(5.49031038273072E-15,1.82930781209959E-13,
3.77003198860263));
#224738=CARTESIAN_POINT('',(59.0907848292984,12.8847271885945,3.77003198860272));
#224739=CARTESIAN_POINT('Origin',(5.49031038273072E-15,1.82930781209959E-13,
3.77003198860263));
#224740=CARTESIAN_POINT('',(58.6269798078533,12.786142387925,3.77003198860272));
#224741=CARTESIAN_POINT('Origin',(5.49031038273072E-15,1.82930781209959E-13,
3.77003198860263));
#224742=CARTESIAN_POINT('',(57.7713971777987,18.4366189870675,3.48823028058495));
#224743=CARTESIAN_POINT('',(57.6166602453971,18.386340275234,3.77003198860276));
#224744=CARTESIAN_POINT('',(59.2498070619042,12.919118186265,3.48823028074814));
#224745=CARTESIAN_POINT('Origin',(5.52999282761009E-15,1.84898592019556E-13,
3.48823028058481));
#224746=CARTESIAN_POINT('',(59.249807061628,12.9191181862048,3.48823028058491));
#224747=CARTESIAN_POINT('Origin',(60.71525,1.85785428279622E-13,3.36123028058482));
#224748=CARTESIAN_POINT('',(59.4650964698966,12.9642895838873,3.36123028058491));
#224749=CARTESIAN_POINT('',(57.9804289733663,18.5051441132844,3.36123028058495));
#224750=CARTESIAN_POINT('Origin',(5.5478765747851E-15,1.85785428279622E-13,
3.36123028058482));
#224751=CARTESIAN_POINT('',(58.1242364370956,18.5518699907153,3.36123028058495));
#224752=CARTESIAN_POINT('',(55.0155724295758,17.5418038257018,3.36123028058494));
#224753=CARTESIAN_POINT('',(59.6130003254555,12.9957275188826,3.36123028058491));
#224754=CARTESIAN_POINT('Origin',(5.5478765747851E-15,1.85785428279622E-13,
3.36123028058482));
#224755=CARTESIAN_POINT('',(59.4656149121214,12.964399782184,3.36123028058491));
#224756=CARTESIAN_POINT('Origin',(5.5478765747851E-15,1.85785428279622E-13,
3.36123028058482));
#224757=CARTESIAN_POINT('',(59.8282880397055,13.0409063549241,3.48823028058494));
#224758=CARTESIAN_POINT('',(58.3332704850401,18.6203878281981,3.48823028042708));
#224759=CARTESIAN_POINT('Origin',(5.52999282761008E-15,1.84898592019556E-13,
3.48823028058484));
#224760=CARTESIAN_POINT('',(58.4880082803368,18.6706636022911,3.77003198802721));
#224761=CARTESIAN_POINT('',(58.3332704847796,18.620387828115,3.48823028058497));
#224762=CARTESIAN_POINT('',(58.4881809372197,18.6701227271413,3.77003198860276));
#224763=CARTESIAN_POINT('Origin',(5.49031038273072E-15,1.82930781209959E-13,
3.77003198860263));
#224764=CARTESIAN_POINT('',(59.9873118763436,13.0752898951327,3.77003198860272));
#224765=CARTESIAN_POINT('Origin',(5.49031038273072E-15,1.82930781209959E-13,
3.77003198860263));
#224766=CARTESIAN_POINT('',(59.9874327886718,13.0747351550713,3.7700319880273));
#224767=CARTESIAN_POINT('Origin',(5.49031038273072E-15,1.82930781209959E-13,
3.77003198860263));
#224768=CARTESIAN_POINT('',(59.9874327889997,13.074735155127,3.77003198860272));
#224769=CARTESIAN_POINT('Origin',(62.2224557307631,1.82930781209959E-13,
3.77003198860263));
#224770=CARTESIAN_POINT('',(58.9396512752213,18.8168143322229,3.77003198860277));
#224771=CARTESIAN_POINT('',(56.3788528200606,17.9847604760584,3.77003198860276));
#224772=CARTESIAN_POINT('',(60.4516424606489,13.1739864076109,3.77003198860273));
#224773=CARTESIAN_POINT('Origin',(5.49031038273072E-15,1.82930781209959E-13,
3.77003198860263));
#224774=CARTESIAN_POINT('',(59.9878258103051,13.0753991351685,3.77003198860272));
#224775=CARTESIAN_POINT('Origin',(5.57972911860581E-15,1.8736496251029E-13,
3.13503198860263));
#224776=CARTESIAN_POINT('Origin',(57.1650144220517,18.2401946149527,3.13502491541448));
#224777=CARTESIAN_POINT('Origin',(58.6264520046768,12.7860353045052,3.13502491541442));
#224778=CARTESIAN_POINT('Origin',(5.57972911860581E-15,1.8736496251029E-13,
3.13503198860263));
#224779=CARTESIAN_POINT('Origin',(58.9759248679598,18.8285650740607,3.20381846780176));
#224780=CARTESIAN_POINT('Origin',(60.48893128525,13.1819466778333,3.20382022872223));
#224781=CARTESIAN_POINT('Origin',(5.51210908043506E-15,1.8401175575949E-13,
3.61523028058481));
#224782=CARTESIAN_POINT('Origin',(58.1393085451921,18.5568062168848,3.58786945046851));
#224783=CARTESIAN_POINT('Origin',(59.6284292050456,12.9989693492946,3.58781461834058));
#224784=CARTESIAN_POINT('Origin',(5.51210908043507E-15,1.8401175575949E-13,
3.61523028058481));
#224785=CARTESIAN_POINT('Origin',(57.9654487055676,18.5002290260159,3.58781440266516));
#224786=CARTESIAN_POINT('Origin',(59.4495735695174,12.9610367308101,3.58786923592919));
#224787=CARTESIAN_POINT('Origin',(60.4792282238308,1.82930781209959E-13,
3.77003198860263));
#224788=CARTESIAN_POINT('',(59.6417962403143,6.58785426247114,3.77003198860268));
#224789=CARTESIAN_POINT('',(58.7584778814676,12.1649068885794,3.77003198860272));
#224790=CARTESIAN_POINT('Origin',(5.49031038273072E-15,1.82930781209959E-13,
3.77003198860263));
#224791=CARTESIAN_POINT('',(59.2228087529788,12.2636034620792,3.77003198860272));
#224792=CARTESIAN_POINT('',(57.9308881865554,11.9889972685553,3.77003198860272));
#224793=CARTESIAN_POINT('',(59.2229260468459,12.2630370254944,3.77003198902565));
#224794=CARTESIAN_POINT('Origin',(5.49031038273072E-15,1.82930781209959E-13,
3.77003198860263));
#224795=CARTESIAN_POINT('',(60.1138365740932,6.63804933238237,3.77003198882092));
#224796=CARTESIAN_POINT('Origin',(5.49031038273072E-15,1.82930781209959E-13,
3.77003198860263));
#224797=CARTESIAN_POINT('',(60.1139000598794,6.63747437341796,3.77003198860268));
#224798=CARTESIAN_POINT('Origin',(5.49031038273072E-15,1.82930781209959E-13,
3.77003198860263));
#224799=CARTESIAN_POINT('',(59.6423308931549,6.58791045674909,3.77003198860268));
#224800=CARTESIAN_POINT('Origin',(5.49031038273072E-15,1.82930781209959E-13,
3.77003198860263));
#224801=CARTESIAN_POINT('',(59.3820708699071,12.2968658913805,3.4882302805849));
#224802=CARTESIAN_POINT('',(59.2229260461285,12.2630370253459,3.77003198860272));
#224803=CARTESIAN_POINT('',(60.2756459901929,6.65505462400517,3.48823028074809));
#224804=CARTESIAN_POINT('Origin',(5.52999282761009E-15,1.84898592019556E-13,
3.48823028058481));
#224805=CARTESIAN_POINT('',(60.2756459899119,6.65505462397414,3.48823028058486));
#224806=CARTESIAN_POINT('Origin',(60.71525,1.85785428279622E-13,3.36123028058482));
#224807=CARTESIAN_POINT('',(60.4944777170594,6.67747469700965,3.36123028058487));
#224808=CARTESIAN_POINT('',(59.5971203935659,12.3431658574213,3.36123028058491));
#224809=CARTESIAN_POINT('Origin',(5.5478765747851E-15,1.85785428279622E-13,
3.36123028058482));
#224810=CARTESIAN_POINT('',(59.7450242491248,12.3746037924166,3.36123028058491));
#224811=CARTESIAN_POINT('',(58.1567073854021,12.0369966210212,3.36123028058491));
#224812=CARTESIAN_POINT('',(60.6448574988554,6.69328024897474,3.36123028058487));
#224813=CARTESIAN_POINT('Origin',(5.5478765747851E-15,1.85785428279622E-13,
3.36123028058482));
#224814=CARTESIAN_POINT('',(60.495004838062,6.67753009965952,3.36123028058487));
#224815=CARTESIAN_POINT('Origin',(5.5478765747851E-15,1.85785428279622E-13,
3.36123028058482));
#224816=CARTESIAN_POINT('',(60.8636883187845,6.71570789669429,3.48823028058489));
#224817=CARTESIAN_POINT('',(59.9600752509415,12.4208962742143,3.48823028042704));
#224818=CARTESIAN_POINT('Origin',(5.52999282761008E-15,1.84898592019556E-13,
3.48823028058484));
#224819=CARTESIAN_POINT('',(60.1192206258106,12.4547221284046,3.77003198802716));
#224820=CARTESIAN_POINT('',(59.9600752506737,12.4208962741588,3.48823028058493));
#224821=CARTESIAN_POINT('',(60.1193358000128,12.4541661686668,3.77003198860272));
#224822=CARTESIAN_POINT('Origin',(5.49031038273072E-15,1.82930781209959E-13,
3.77003198860263));
#224823=CARTESIAN_POINT('',(61.0254350648262,6.73328056300537,3.77003198860268));
#224824=CARTESIAN_POINT('Origin',(5.49031038273072E-15,1.82930781209959E-13,
3.77003198860263));
#224825=CARTESIAN_POINT('',(61.025497328658,6.73271622308816,3.77003198802725));
#224826=CARTESIAN_POINT('Origin',(5.49031038273072E-15,1.82930781209959E-13,
3.77003198860263));
#224827=CARTESIAN_POINT('',(61.0254973289899,6.73271622310927,3.77003198860268));
#224828=CARTESIAN_POINT('Origin',(62.2224557307631,1.82930781209959E-13,
3.77003198860263));
#224829=CARTESIAN_POINT('',(60.5836663843182,12.5528626811449,3.77003198860272));
#224830=CARTESIAN_POINT('',(59.5987607253194,12.3435145206988,3.77003198860272));
#224831=CARTESIAN_POINT('',(61.4975385923862,6.78290064323579,3.77003198860268));
#224832=CARTESIAN_POINT('Origin',(5.49031038273072E-15,1.82930781209959E-13,
3.77003198860263));
#224833=CARTESIAN_POINT('',(61.0259576020968,6.73333548388559,3.77003198860268));
#224834=CARTESIAN_POINT('Origin',(5.57972911860581E-15,1.8736496251029E-13,
3.13503198860263));
#224835=CARTESIAN_POINT('Origin',(58.7584780045774,12.1649018101387,3.13502491541444));
#224836=CARTESIAN_POINT('Origin',(59.6417947880741,6.58785913039846,3.13502491541438));
#224837=CARTESIAN_POINT('Origin',(5.57972911860581E-15,1.8736496251029E-13,
3.13503198860263));
#224838=CARTESIAN_POINT('Origin',(60.6209695535092,12.560757428278,3.20381846780363));
#224839=CARTESIAN_POINT('Origin',(61.5354552197175,6.78691956273252,3.203820228721));
#224840=CARTESIAN_POINT('Origin',(5.51210908043506E-15,1.8401175575949E-13,
3.61523028058481));
#224841=CARTESIAN_POINT('Origin',(59.7605297667717,12.3779375131251,3.58786945046858));
#224842=CARTESIAN_POINT('Origin',(60.6605407209801,6.69489156322711,3.58781461834032));
#224843=CARTESIAN_POINT('Origin',(5.51210908043507E-15,1.8401175575949E-13,
3.61523028058481));
#224844=CARTESIAN_POINT('Origin',(59.5817084227231,12.3398435598876,3.58781440266648));
#224845=CARTESIAN_POINT('Origin',(60.478699837019,6.67586224832342,3.58786923592837));
#224846=CARTESIAN_POINT('Origin',(57.8669800961561,1.94016234460786E-13,
2.18253198860263));
#224847=CARTESIAN_POINT('Origin',(60.4792282238308,1.82930781209959E-13,
3.77003198860263));
#224848=CARTESIAN_POINT('',(60.0036905223731,0.317500000000183,3.77003198860264));
#224849=CARTESIAN_POINT('',(59.7081718144892,5.95633285891229,3.77003198860268));
#224850=CARTESIAN_POINT('Origin',(5.49031038273072E-15,1.82930781209959E-13,
3.77003198860263));
#224851=CARTESIAN_POINT('',(60.1802756340603,6.00595296980891,3.77003198860268));
#224852=CARTESIAN_POINT('',(59.851607889689,5.97140859790567,3.77003198860268));
#224853=CARTESIAN_POINT('',(60.1803330766335,6.00537737567532,3.77003198902561));
#224854=CARTESIAN_POINT('Origin',(5.49031038273072E-15,1.82930781209959E-13,
3.77003198860263));
#224855=CARTESIAN_POINT('',(60.4783917833346,0.318078445376176,3.77003198882088));
#224856=CARTESIAN_POINT('Origin',(5.49031038273072E-15,1.82930781209959E-13,
3.77003198860263));
#224857=CARTESIAN_POINT('',(60.478394821762,0.317500000025467,3.77003198860264));
#224858=CARTESIAN_POINT('Origin',(5.49031038273072E-15,1.82930781209959E-13,
3.77003198860263));
#224859=CARTESIAN_POINT('',(60.004228120231,0.317500000000183,3.77003198860264));
#224860=CARTESIAN_POINT('Origin',(5.49031038273072E-15,1.82930781209959E-13,
3.77003198860263));
#224861=CARTESIAN_POINT('',(60.3421421670675,6.02238575970295,3.48823028058486));
#224862=CARTESIAN_POINT('',(60.1803330759045,6.00537737560258,3.77003198860268));
#224863=CARTESIAN_POINT('',(60.6410923275233,0.318076890625034,3.48823028074806));
#224864=CARTESIAN_POINT('Origin',(5.52999282761009E-15,1.84898592019556E-13,
3.48823028058481));
#224865=CARTESIAN_POINT('',(60.6410923272405,0.318076890623551,3.48823028058482));
#224866=CARTESIAN_POINT('Origin',(60.71525,1.85785428279622E-13,3.36123028058482));
#224867=CARTESIAN_POINT('',(60.8610688070707,0.317500000000186,3.36123028058483));
#224868=CARTESIAN_POINT('',(60.5608532912343,6.04595329345079,3.36123028058486));
#224869=CARTESIAN_POINT('Origin',(5.5478765747851E-15,1.85785428279622E-13,
3.36123028058482));
#224870=CARTESIAN_POINT('',(60.7112330730304,6.06175884541589,3.36123028058486));
#224871=CARTESIAN_POINT('',(60.0850508448141,5.99594444118226,3.36123028058486));
#224872=CARTESIAN_POINT('',(61.0122769227456,0.317500000000186,3.36123028058483));
#224873=CARTESIAN_POINT('Origin',(5.5478765747851E-15,1.85785428279622E-13,
3.36123028058482));
#224874=CARTESIAN_POINT('',(60.8615988316031,0.317500000000186,3.36123028058483));
#224875=CARTESIAN_POINT('Origin',(5.5478765747851E-15,1.85785428279622E-13,
3.36123028058482));
#224876=CARTESIAN_POINT('',(61.2322532920972,0.316930737396099,3.48823028058485));
#224877=CARTESIAN_POINT('',(60.9299448849412,6.08531878141057,3.488230280427));
#224878=CARTESIAN_POINT('Origin',(5.52999282761008E-15,1.84898592019556E-13,
3.48823028058484));
#224879=CARTESIAN_POINT('',(61.0917542093523,6.10232411256106,3.77003198802712));
#224880=CARTESIAN_POINT('',(60.929944884669,6.08531878138339,3.48823028058489));
#224881=CARTESIAN_POINT('',(61.0918106390012,6.10175915944652,3.77003198860268));
#224882=CARTESIAN_POINT('Origin',(5.49031038273072E-15,1.82930781209959E-13,
3.77003198860263));
#224883=CARTESIAN_POINT('',(61.3949508163454,0.317500000000183,3.77003198860264));
#224884=CARTESIAN_POINT('Origin',(5.49031038273072E-15,1.82930781209959E-13,
3.77003198860263));
#224885=CARTESIAN_POINT('',(61.394953749505,0.316932243253439,3.77003198802722));
#224886=CARTESIAN_POINT('Origin',(5.49031038273072E-15,1.82930781209959E-13,
3.77003198860263));
#224887=CARTESIAN_POINT('',(61.3949537498373,0.316932243239743,3.77003198860264));
#224888=CARTESIAN_POINT('Origin',(62.2224557307631,1.82930781209959E-13,
3.77003198860263));
#224889=CARTESIAN_POINT('',(61.5639141665612,6.15137923967694,3.77003198860268));
#224890=CARTESIAN_POINT('',(61.5757885448747,6.15262728712883,3.77003198860268));
#224891=CARTESIAN_POINT('',(61.8696548221181,0.317500000000183,3.77003198860264));
#224892=CARTESIAN_POINT('Origin',(5.49031038273072E-15,1.82930781209959E-13,
3.77003198860263));
#224893=CARTESIAN_POINT('',(61.3954762318973,0.317500000000183,3.77003198860264));
#224894=CARTESIAN_POINT('Origin',(63.2144358269191,1.94016234460786E-13,
2.18253198860263));
#224895=CARTESIAN_POINT('Origin',(65.,1.80713690559794E-13,4.08753198860263));
#224896=CARTESIAN_POINT('Origin',(5.57972911860581E-15,1.8736496251029E-13,
3.13503198860263));
#224897=CARTESIAN_POINT('Origin',(59.708171406083,5.95632779542321,3.13502491541438));
#224898=CARTESIAN_POINT('Origin',(60.0036895869254,0.317504993060939,3.13502491541434));
#224899=CARTESIAN_POINT('Origin',(5.57972911860581E-15,1.8736496251029E-13,
3.13503198860263));
#224900=CARTESIAN_POINT('Origin',(61.6018382108745,6.15533149560987,3.20381846780522));
#224901=CARTESIAN_POINT('Origin',(61.9077838296783,0.317533536648817,3.20382022872431));
#224902=CARTESIAN_POINT('Origin',(5.51210908043506E-15,1.8401175575949E-13,
3.61523028058481));
#224903=CARTESIAN_POINT('Origin',(60.7270021185312,6.06345353572159,3.58786945047074));
#224904=CARTESIAN_POINT('Origin',(61.0280426587405,0.3174631441967,3.58781461834159));
#224905=CARTESIAN_POINT('Origin',(5.51210908043507E-15,1.8401175575949E-13,
3.61523028058481));
#224906=CARTESIAN_POINT('Origin',(60.5451784741228,6.04426018543852,3.58781440266261));
#224907=CARTESIAN_POINT('Origin',(60.8452088131258,0.317545622030932,3.58786923593057));
#224908=CARTESIAN_POINT('Origin',(58.2637721346185,-0.190499999999809,2.65878198860262));
#224909=CARTESIAN_POINT('',(59.0285534841296,0.0152400000001907,2.65878198860263));
#224910=CARTESIAN_POINT('',(62.8464427007196,0.0152400000001907,2.65878198860263));
#224911=CARTESIAN_POINT('',(58.2637721346185,0.0152400000001907,2.65878198860263));
#224912=CARTESIAN_POINT('',(62.8464427007196,-0.0152399999998093,2.65878198860263));
#224913=CARTESIAN_POINT('Origin',(-1.95097259456047E-16,1.90690598485538E-13,
2.65878198860263));
#224914=CARTESIAN_POINT('',(59.0285534841296,-0.0152399999998093,2.65878198860263));
#224915=CARTESIAN_POINT('',(58.9578504383728,-0.0152399999998093,2.65878198860263));
#224916=CARTESIAN_POINT('Origin',(4.7062627014205E-16,1.90690598485538E-13,
2.65878198860263));
#224917=CARTESIAN_POINT('Origin',(0.,-0.190500000000089,42.7590319886026));
#224918=CARTESIAN_POINT('',(60.0036905223731,-0.190499999999816,3.64303198860263));
#224919=CARTESIAN_POINT('',(59.5728760150042,-0.190499999999814,3.40423097483311));
#224920=CARTESIAN_POINT('Origin',(59.9654595002504,-0.190499999999813,3.20400220531706));
#224921=CARTESIAN_POINT('',(59.2165773020941,-0.19049999946855,2.83404198860262));
#224922=CARTESIAN_POINT('',(59.5728760150042,-0.190499999999814,3.4042309748331));
#224923=CARTESIAN_POINT('',(62.6567671111299,-0.190499999999809,2.83404198860262));
#224924=CARTESIAN_POINT('',(62.9165533988763,-0.190499999999811,2.83404198860262));
#224925=CARTESIAN_POINT('',(62.3004688883555,-0.190500000605564,3.4042309748331));
#224926=CARTESIAN_POINT('',(62.6567671111299,-0.190499999999811,2.83404198860262));
#224927=CARTESIAN_POINT('',(61.8696548221181,-0.190499999999816,3.64303198860263));
#224928=CARTESIAN_POINT('Origin',(61.9078859673766,-0.190499999999813,3.20400259788328));
#224929=CARTESIAN_POINT('',(61.4682752798284,-0.190500000711747,3.64303198860263));
#224930=CARTESIAN_POINT('',(5.50819412990574E-15,-0.190499999999816,3.64303198860262));
#224931=CARTESIAN_POINT('',(61.3422370451705,-0.190499999999815,3.42473028058486));
#224932=CARTESIAN_POINT('',(61.4682752798284,-0.190499999999816,3.64303198860263));
#224933=CARTESIAN_POINT('',(61.0122769227456,-0.190499999999813,3.23423028058482));
#224934=CARTESIAN_POINT('Origin',(61.0417043405089,-0.190499486622215,3.56425722717113));
#224935=CARTESIAN_POINT('',(60.8610688070707,-0.190499999999813,3.23423028058482));
#224936=CARTESIAN_POINT('',(5.56576032196012E-15,-0.190499999999813,3.23423028058481));
#224937=CARTESIAN_POINT('',(60.5311086139135,-0.190499999999815,3.42473028058481));
#224938=CARTESIAN_POINT('Origin',(60.83163848074,-0.190499486573319,3.56425909741097));
#224939=CARTESIAN_POINT('',(60.4050703266283,-0.190499999999816,3.64303198860263));
#224940=CARTESIAN_POINT('',(60.5311086139135,-0.190499999999815,3.42473028058481));
#224941=CARTESIAN_POINT('',(5.50819412990574E-15,-0.190499999999816,3.64303198860262));
#224942=CARTESIAN_POINT('Origin',(0.,0.190499999999911,42.7590319886026));
#224943=CARTESIAN_POINT('',(61.8696548221181,0.190500000000184,3.64303198860263));
#224944=CARTESIAN_POINT('',(62.3004688883555,0.190500000000186,3.4042309748331));
#224945=CARTESIAN_POINT('Origin',(61.9078859670888,0.190500000000187,3.20400259735841));
#224946=CARTESIAN_POINT('',(62.6567671111299,0.190500000452956,2.83404198860263));
#224947=CARTESIAN_POINT('',(62.3004688883555,0.190500000000186,3.4042309748331));
#224948=CARTESIAN_POINT('',(59.2165773020941,0.19050000000019,2.83404198860263));
#224949=CARTESIAN_POINT('',(0.,0.19050000000019,2.83404198860263));
#224950=CARTESIAN_POINT('',(59.5728760150042,0.190499999293458,3.40423097483312));
#224951=CARTESIAN_POINT('',(59.2165773020941,0.19050000000019,2.83404198860263));
#224952=CARTESIAN_POINT('',(60.0036905223731,0.190500000000184,3.64303198860263));
#224953=CARTESIAN_POINT('Origin',(59.9654594999465,0.190500000000187,3.20400220587196));
#224954=CARTESIAN_POINT('',(60.4050703266283,0.190499999258583,3.64303198860264));
#224955=CARTESIAN_POINT('',(60.4789282006569,0.190500000000184,3.64303198860263));
#224956=CARTESIAN_POINT('',(60.5311086139135,0.190500000000185,3.42473028058481));
#224957=CARTESIAN_POINT('',(60.4050703266283,0.190500000000184,3.64303198860263));
#224958=CARTESIAN_POINT('',(60.8610688070707,0.190500000000187,3.23423028058482));
#224959=CARTESIAN_POINT('Origin',(60.8316414495914,0.190499486502742,3.5642574300434));
#224960=CARTESIAN_POINT('',(61.0122769227456,0.190500000000187,3.23423028058482));
#224961=CARTESIAN_POINT('',(61.0128056337175,0.190500000000187,3.23423028058482));
#224962=CARTESIAN_POINT('',(61.3422370451705,0.190500000000185,3.42473028058486));
#224963=CARTESIAN_POINT('Origin',(61.04170717438,0.190499486688283,3.56425912918013));
#224964=CARTESIAN_POINT('',(61.4682752798284,0.190500000000184,3.64303198860263));
#224965=CARTESIAN_POINT('',(61.3422370451705,0.190500000000185,3.42473028058486));
#224966=CARTESIAN_POINT('',(61.8701762063762,0.190500000000184,3.64303198860263));
#224967=CARTESIAN_POINT('Origin',(58.2637721346185,0.0152400000001895,2.83404198860262));
#224968=CARTESIAN_POINT('Ctrl Pts',(62.6567671111299,0.19050000000019,2.83404198860263));
#224969=CARTESIAN_POINT('Ctrl Pts',(62.6673774406538,0.19050000000019,2.82419652440072));
#224970=CARTESIAN_POINT('Ctrl Pts',(62.6779562874464,0.18966280967327,2.81438790575662));
#224971=CARTESIAN_POINT('Ctrl Pts',(62.6884465439473,0.188003604115333,
2.80466781256922));
#224972=CARTESIAN_POINT('Ctrl Pts',(62.6985959295774,0.186398312858107,
2.79526356453104));
#224973=CARTESIAN_POINT('Ctrl Pts',(62.7086636500148,0.184023290311467,
2.78594102496265));
#224974=CARTESIAN_POINT('Ctrl Pts',(62.7185939622165,0.180846261210796,
2.77675109088818));
#224975=CARTESIAN_POINT('Ctrl Pts',(62.727987426086,0.177840987311745,2.76805797913727));
#224976=CARTESIAN_POINT('Ctrl Pts',(62.7372588214081,0.174117798731289,
2.75948271210212));
#224977=CARTESIAN_POINT('Ctrl Pts',(62.7463424082311,0.169611579426594,
2.7510857557328));
#224978=CARTESIAN_POINT('Ctrl Pts',(62.7547090486368,0.165461025548891,
2.74335155163331));
#224979=CARTESIAN_POINT('Ctrl Pts',(62.7629168328854,0.160645870588248,
2.73576818686008));
#224980=CARTESIAN_POINT('Ctrl Pts',(62.770889261081,0.155086395962765,2.72840626160565));
#224981=CARTESIAN_POINT('Ctrl Pts',(62.7732017594456,0.153473803705493,
2.72627084693725));
#224982=CARTESIAN_POINT('Ctrl Pts',(62.7754942590276,0.151798403770733,
2.72415424587544));
#224983=CARTESIAN_POINT('Ctrl Pts',(62.7777643638146,0.150057792857846,
2.72205867173257));
#224984=CARTESIAN_POINT('Ctrl Pts',(62.780225303358,0.148170858717228,2.71978693462861));
#224985=CARTESIAN_POINT('Ctrl Pts',(62.7826571567199,0.146210769553957,
2.71754411340762));
#224986=CARTESIAN_POINT('Ctrl Pts',(62.7850565204095,0.14417542182634,2.71533341844259));
#224987=CARTESIAN_POINT('Ctrl Pts',(62.791641592883,0.138589394016812,2.70926614876406));
#224988=CARTESIAN_POINT('Ctrl Pts',(62.7979456687654,0.132410786669233,
2.70347381860423));
#224989=CARTESIAN_POINT('Ctrl Pts',(62.8038680995982,0.125664597436926,
2.69804914171409));
#224990=CARTESIAN_POINT('Ctrl Pts',(62.8092868022739,0.119492200548509,
2.69308585687218));
#224991=CARTESIAN_POINT('Ctrl Pts',(62.8143744518939,0.11284434746039,2.68842799053199));
#224992=CARTESIAN_POINT('Ctrl Pts',(62.8190433630434,0.105708043833423,
2.6841476705423));
#224993=CARTESIAN_POINT('Ctrl Pts',(62.8213367169483,0.102202714803628,
2.68204519134565));
#224994=CARTESIAN_POINT('Ctrl Pts',(62.8235285419788,0.0985794274534579,
2.68003431778517));
#224995=CARTESIAN_POINT('Ctrl Pts',(62.8256051102647,0.0948363533474084,
2.67812693945267));
#224996=CARTESIAN_POINT('Ctrl Pts',(62.8259991188709,0.0941261414938091,
2.67776503299219));
#224997=CARTESIAN_POINT('Ctrl Pts',(62.8263888407139,0.0934111032314617,
2.6774065963994));
#224998=CARTESIAN_POINT('Ctrl Pts',(62.826774159152,0.0926913160162657,
2.67705178968871));
#224999=CARTESIAN_POINT('Ctrl Pts',(62.8271474363889,0.0919940221515445,
2.67670807068773));
#225000=CARTESIAN_POINT('Ctrl Pts',(62.8275165811343,0.0912922715312271,
2.67636775825281));
#225001=CARTESIAN_POINT('Ctrl Pts',(62.8278814873655,0.0905861384171377,
2.67603099699271));
#225002=CARTESIAN_POINT('Ctrl Pts',(62.8318581602824,0.0828908452420619,
2.67236104217145));
#225003=CARTESIAN_POINT('Ctrl Pts',(62.8353337180912,0.074669831663276,
2.66911440541491));
#225004=CARTESIAN_POINT('Ctrl Pts',(62.8381654210186,0.0660491922299371,
2.66646778189648));
#225005=CARTESIAN_POINT('Ctrl Pts',(62.8393612667489,0.0624086426656371,
2.66535009634991));
#225006=CARTESIAN_POINT('Ctrl Pts',(62.8404425512865,0.0586971697059423,
2.6643389791236));
#225007=CARTESIAN_POINT('Ctrl Pts',(62.8414000604479,0.0549254519866671,
2.66344564884808));
#225008=CARTESIAN_POINT('Ctrl Pts',(62.8430124819501,0.048573973592406,
2.661941302986));
#225009=CARTESIAN_POINT('Ctrl Pts',(62.8442717146911,0.042052924695462,
2.66077206705434));
#225010=CARTESIAN_POINT('Ctrl Pts',(62.8451307298764,0.0354197192408986,
2.65998225155728));
#225011=CARTESIAN_POINT('Ctrl Pts',(62.8453454836727,0.0337614178772578,
2.65978479768302));
#225012=CARTESIAN_POINT('Ctrl Pts',(62.8455349903695,0.0320960919387808,
2.65961098966636));
#225013=CARTESIAN_POINT('Ctrl Pts',(62.8456982067485,0.0304246312367792,
2.65946139030515));
#225014=CARTESIAN_POINT('Ctrl Pts',(62.845943031317,0.0279174401837767,
2.65923699126334));
#225015=CARTESIAN_POINT('Ctrl Pts',(62.8461286892223,0.0253964615341582,
2.65906707562455));
#225016=CARTESIAN_POINT('Ctrl Pts',(62.846253337618,0.0228647168033014,
2.65895332562933));
#225017=CARTESIAN_POINT('Ctrl Pts',(62.8463779860137,0.0203329720724447,
2.65883957563411));
#225018=CARTESIAN_POINT('Ctrl Pts',(62.8464416340693,0.0177904683743446,
2.65878198860262));
#225019=CARTESIAN_POINT('Ctrl Pts',(62.8464427007196,0.0152400000001907,
2.65878198860262));
#225020=CARTESIAN_POINT('Ctrl Pts',(59.0285534841296,0.015240000000191,
2.65878198860262));
#225021=CARTESIAN_POINT('Ctrl Pts',(59.0285496414744,0.0238699985094254,
2.65878198860262));
#225022=CARTESIAN_POINT('Ctrl Pts',(59.0292582026622,0.0324255116355521,
2.65945335517854));
#225023=CARTESIAN_POINT('Ctrl Pts',(59.0305954788489,0.0407807192227339,
2.66072561226598));
#225024=CARTESIAN_POINT('Ctrl Pts',(59.0314592220531,0.0461773260303339,
2.66154735980336));
#225025=CARTESIAN_POINT('Ctrl Pts',(59.0325843328198,0.0514905268410215,
2.66261895766881));
#225026=CARTESIAN_POINT('Ctrl Pts',(59.0339399880044,0.0566895722963242,
2.66391429251026));
#225027=CARTESIAN_POINT('Ctrl Pts',(59.0357368312948,0.063580609227557,
2.66563118464122));
#225028=CARTESIAN_POINT('Ctrl Pts',(59.0379438906768,0.0702685278902536,
2.66774105138698));
#225029=CARTESIAN_POINT('Ctrl Pts',(59.0405007795597,0.0766865040606001,
2.67016894181749));
#225030=CARTESIAN_POINT('Ctrl Pts',(59.0417792240012,0.0798954921457732,
2.67138288703274));
#225031=CARTESIAN_POINT('Ctrl Pts',(59.0431451240705,0.0830371938950924,
2.67267613167551));
#225032=CARTESIAN_POINT('Ctrl Pts',(59.0445909239228,0.0861046703639672,
2.67403835432553));
#225033=CARTESIAN_POINT('Ctrl Pts',(59.0453138238489,0.0876384085984046,
2.67471946565054));
#225034=CARTESIAN_POINT('Ctrl Pts',(59.0460566986719,0.089153606943806,
2.67541781389523));
#225035=CARTESIAN_POINT('Ctrl Pts',(59.0468186034775,0.0906495011922447,
2.67613207244169));
#225036=CARTESIAN_POINT('Ctrl Pts',(59.047009079679,0.0910234747543544,
2.67631063707831));
#225037=CARTESIAN_POINT('Ctrl Pts',(59.0472007452523,0.0913962421598847,
2.67649019601846));
#225038=CARTESIAN_POINT('Ctrl Pts',(59.0473935854286,0.0917677921728875,
2.67667072836657));
#225039=CARTESIAN_POINT('Ctrl Pts',(59.0479721059574,0.092882442211896,
2.67721232541091));
#225040=CARTESIAN_POINT('Ctrl Pts',(59.048561197931,0.0939861339739832,
2.67776268340048));
#225041=CARTESIAN_POINT('Ctrl Pts',(59.0491604624443,0.0950785796751064,
2.67832123541517));
#225042=CARTESIAN_POINT('Ctrl Pts',(59.0533816042975,0.102773626133288,
2.68225560368441));
#225043=CARTESIAN_POINT('Ctrl Pts',(59.0580834293365,0.10995882346637,2.68661792998879));
#225044=CARTESIAN_POINT('Ctrl Pts',(59.0631465696369,0.116642428646637,
2.69130986622563));
#225045=CARTESIAN_POINT('Ctrl Pts',(59.0656021872114,0.119883969936843,
2.69358545023044));
#225046=CARTESIAN_POINT('Ctrl Pts',(59.0681433715118,0.123007567718211,
2.69593918853465));
#225047=CARTESIAN_POINT('Ctrl Pts',(59.0707593633743,0.126014035556604,
2.69836306235476));
#225048=CARTESIAN_POINT('Ctrl Pts',(59.0747642641417,0.13061672776123,2.70207384382209));
#225049=CARTESIAN_POINT('Ctrl Pts',(59.0789414743143,0.134943070277463,
2.70594760814209));
#225050=CARTESIAN_POINT('Ctrl Pts',(59.0832455674828,0.138985142830926,
2.70995196345689));
#225051=CARTESIAN_POINT('Ctrl Pts',(59.0852444106167,0.140862302235665,
2.71181160678087));
#225052=CARTESIAN_POINT('Ctrl Pts',(59.0872703932641,0.142678271527306,
2.7136996277208));
#225053=CARTESIAN_POINT('Ctrl Pts',(59.0893195943183,0.144431197308928,
2.71561183138642));
#225054=CARTESIAN_POINT('Ctrl Pts',(59.0894766575049,0.144565552163213,
2.71575839426293));
#225055=CARTESIAN_POINT('Ctrl Pts',(59.0896338466133,0.14469956892598,2.7159050890319));
#225056=CARTESIAN_POINT('Ctrl Pts',(59.0897911602042,0.144833247843271,
2.71605191409893));
#225057=CARTESIAN_POINT('Ctrl Pts',(59.0920009418701,0.146711033602277,
2.71811436362734));
#225058=CARTESIAN_POINT('Ctrl Pts',(59.0942367399983,0.148520654545085,
2.7202009102694));
#225059=CARTESIAN_POINT('Ctrl Pts',(59.0964928714566,0.150262619641469,
2.72230624862163));
#225060=CARTESIAN_POINT('Ctrl Pts',(59.1045829576265,0.156508996679146,
2.72985561753101));
#225061=CARTESIAN_POINT('Ctrl Pts',(59.1129958342953,0.161935290146134,
2.73770089914346));
#225062=CARTESIAN_POINT('Ctrl Pts',(59.1216309196491,0.166622470788088,
2.74574823347109));
#225063=CARTESIAN_POINT('Ctrl Pts',(59.1311200109819,0.17177321144469,2.75459144547098));
#225064=CARTESIAN_POINT('Ctrl Pts',(59.1408779306752,0.17603186436329,2.76367911754385));
#225065=CARTESIAN_POINT('Ctrl Pts',(59.1508087658119,0.179468536018209,
2.77292162564885));
#225066=CARTESIAN_POINT('Ctrl Pts',(59.1615315754607,0.183179278918869,
2.78290121484987));
#225067=CARTESIAN_POINT('Ctrl Pts',(59.1724570142889,0.185932239425938,
2.79306229500547));
#225068=CARTESIAN_POINT('Ctrl Pts',(59.1834936683191,0.18776628610095,2.80331916685715));
#225069=CARTESIAN_POINT('Ctrl Pts',(59.1944377361589,0.189584947008325,
2.81348999409005));
#225070=CARTESIAN_POINT('Ctrl Pts',(59.2054925958133,0.19050000000019,2.82375635967032));
#225071=CARTESIAN_POINT('Ctrl Pts',(59.2165773020941,0.19050000000019,2.83404198860263));
#225072=CARTESIAN_POINT('Origin',(0.,-0.0152399999998105,2.83404198860262));
#225073=CARTESIAN_POINT('Ctrl Pts',(62.8464427007196,-0.0152399999998093,
2.65878198860262));
#225074=CARTESIAN_POINT('Ctrl Pts',(62.8464391086779,-0.0238289333902187,
2.65878198860262));
#225075=CARTESIAN_POINT('Ctrl Pts',(62.8457180711405,-0.0323412407622019,
2.65944603041843));
#225076=CARTESIAN_POINT('Ctrl Pts',(62.8443658068291,-0.040653113049866,
2.66070439264048));
#225077=CARTESIAN_POINT('Ctrl Pts',(62.843501774309,-0.0459640037531338,
2.66150842619576));
#225078=CARTESIAN_POINT('Ctrl Pts',(62.8423809556999,-0.0511932363888254,
2.66255428265356));
#225079=CARTESIAN_POINT('Ctrl Pts',(62.841033859251,-0.0563116129572788,
2.66381699700655));
#225080=CARTESIAN_POINT('Ctrl Pts',(62.8391953428955,-0.0632971699620584,
2.66554034873254));
#225081=CARTESIAN_POINT('Ctrl Pts',(62.8369299537504,-0.0700734120982055,
2.66766759643958));
#225082=CARTESIAN_POINT('Ctrl Pts',(62.8343031482014,-0.0765705776093055,
2.67012012783133));
#225083=CARTESIAN_POINT('Ctrl Pts',(62.8329897454269,-0.0798191603648555,
2.67134639352721));
#225084=CARTESIAN_POINT('Ctrl Pts',(62.8315859904681,-0.0829981827951411,
2.67265375584997));
#225085=CARTESIAN_POINT('Ctrl Pts',(62.8301000734874,-0.0861004173276881,
2.67403135126924));
#225086=CARTESIAN_POINT('Ctrl Pts',(62.8293571149971,-0.0876515345939617,
2.67472014897888));
#225087=CARTESIAN_POINT('Ctrl Pts',(62.8285936160519,-0.0891834722995234,
2.67542649668616));
#225088=CARTESIAN_POINT('Ctrl Pts',(62.82781060087,-0.0906954364276871,
2.67614899656085));
#225089=CARTESIAN_POINT('Ctrl Pts',(62.8276148470746,-0.091073427459728,
2.67632962152953));
#225090=CARTESIAN_POINT('Ctrl Pts',(62.8274178735164,-0.0914501705141547,
2.67651125590934));
#225091=CARTESIAN_POINT('Ctrl Pts',(62.8272196962038,-0.0918256539326625,
2.67669387767507));
#225092=CARTESIAN_POINT('Ctrl Pts',(62.8266251642659,-0.0929521041881856,
2.67724174297227));
#225093=CARTESIAN_POINT('Ctrl Pts',(62.826019798519,-0.0940672158684688,
2.67779849504731));
#225094=CARTESIAN_POINT('Ctrl Pts',(62.8254040313373,-0.095170690748659,
2.67836353617992));
#225095=CARTESIAN_POINT('Ctrl Pts',(62.8211486980557,-0.102796386827314,
2.68226832098888));
#225096=CARTESIAN_POINT('Ctrl Pts',(62.8164204928785,-0.109916699411195,
2.68659153751368));
#225097=CARTESIAN_POINT('Ctrl Pts',(62.8113377077397,-0.116542502759485,
2.69123699486152));
#225098=CARTESIAN_POINT('Ctrl Pts',(62.8088115774776,-0.119835508836209,
2.69354577441193));
#225099=CARTESIAN_POINT('Ctrl Pts',(62.8061972539433,-0.123006400629109,
2.69593478828097));
#225100=CARTESIAN_POINT('Ctrl Pts',(62.8035061084565,-0.126056303769779,
2.69839565261203));
#225101=CARTESIAN_POINT('Ctrl Pts',(62.7975690395531,-0.132784845643092,
2.70382468689029));
#225102=CARTESIAN_POINT('Ctrl Pts',(62.7912680187378,-0.138932019324493,
2.7096115581507));
#225103=CARTESIAN_POINT('Ctrl Pts',(62.7847385034067,-0.14444511341298,
2.71562701361751));
#225104=CARTESIAN_POINT('Ctrl Pts',(62.7823531891148,-0.146459116207277,
2.71782453535842));
#225105=CARTESIAN_POINT('Ctrl Pts',(62.7799396422115,-0.148396130390791,
2.72005051502386));
#225106=CARTESIAN_POINT('Ctrl Pts',(62.7775029828616,-0.150257579786298,
2.72229986760101));
#225107=CARTESIAN_POINT('Ctrl Pts',(62.7693185019449,-0.156509991333256,
2.72985520488842));
#225108=CARTESIAN_POINT('Ctrl Pts',(62.7608162581027,-0.161942805717608,
2.73770845534472));
#225109=CARTESIAN_POINT('Ctrl Pts',(62.7520965944504,-0.166635979460947,
2.74576706701628));
#225110=CARTESIAN_POINT('Ctrl Pts',(62.7425126511844,-0.171794333347877,
2.75462443584869));
#225111=CARTESIAN_POINT('Ctrl Pts',(62.7326655363513,-0.176059615357052,
2.76373036322983));
#225112=CARTESIAN_POINT('Ctrl Pts',(62.7226511116316,-0.179500292056274,
2.7729966463658));
#225113=CARTESIAN_POINT('Ctrl Pts',(62.7118651471245,-0.183206048282619,
2.78297683033192));
#225114=CARTESIAN_POINT('Ctrl Pts',(62.7008840239674,-0.185955767118741,
2.79314401478563));
#225115=CARTESIAN_POINT('Ctrl Pts',(62.6897991274287,-0.187785458034744,
2.80341452427555));
#225116=CARTESIAN_POINT('Ctrl Pts',(62.6788639144191,-0.189590441945804,
2.81354634721108));
#225117=CARTESIAN_POINT('Ctrl Pts',(62.6678262782739,-0.19049999999981,
2.82378004209077));
#225118=CARTESIAN_POINT('Ctrl Pts',(62.6567671111299,-0.190499999999811,
2.83404198860262));
#225119=CARTESIAN_POINT('Ctrl Pts',(59.2165773020941,-0.190499999999811,
2.83404198860262));
#225120=CARTESIAN_POINT('Ctrl Pts',(59.2059936184297,-0.19049999999981,
2.8242212644308));
#225121=CARTESIAN_POINT('Ctrl Pts',(59.1954479901471,-0.189665225488525,
2.81442815028649));
#225122=CARTESIAN_POINT('Ctrl Pts',(59.1849969778475,-0.188008762314082,
2.80471618166538));
#225123=CARTESIAN_POINT('Ctrl Pts',(59.1749056059515,-0.186409301377087,
2.79533842146494));
#225124=CARTESIAN_POINT('Ctrl Pts',(59.1649012152168,-0.184043455438379,
2.78603515650548));
#225125=CARTESIAN_POINT('Ctrl Pts',(59.1550396955556,-0.180877423727034,
2.77685887347105));
#225126=CARTESIAN_POINT('Ctrl Pts',(59.1457174710389,-0.177884532220033,
2.7681844121695));
#225127=CARTESIAN_POINT('Ctrl Pts',(59.1365220583474,-0.174176304387683,
2.75962261522018));
#225128=CARTESIAN_POINT('Ctrl Pts',(59.1275197082979,-0.169686797573322,
2.75123537702072));
#225129=CARTESIAN_POINT('Ctrl Pts',(59.1192286949278,-0.165552037114362,
2.74351087134539));
#225130=CARTESIAN_POINT('Ctrl Pts',(59.1111009786111,-0.160754293904838,
2.73593399450272));
#225131=CARTESIAN_POINT('Ctrl Pts',(59.1032135992748,-0.15521351501467,
2.72857657813005));
#225132=CARTESIAN_POINT('Ctrl Pts',(59.1008617419729,-0.15356136659691,
2.72638274508602));
#225133=CARTESIAN_POINT('Ctrl Pts',(59.0985314603587,-0.151842962928119,
2.72420861709732));
#225134=CARTESIAN_POINT('Ctrl Pts',(59.096225375957,-0.15005568617995,2.72205663736708));
#225135=CARTESIAN_POINT('Ctrl Pts',(59.0939428540559,-0.148286670996516,
2.71992664556747));
#225136=CARTESIAN_POINT('Ctrl Pts',(59.0916862380348,-0.146452235168713,
2.71782089927866));
#225137=CARTESIAN_POINT('Ctrl Pts',(59.0894604907299,-0.144552116609777,
2.71574387311227));
#225138=CARTESIAN_POINT('Ctrl Pts',(59.0893057166152,-0.144419986081231,
2.71559944077468));
#225139=CARTESIAN_POINT('Ctrl Pts',(59.0891510807051,-0.144287542501913,
2.7154551521605));
#225140=CARTESIAN_POINT('Ctrl Pts',(59.0889965840074,-0.14415478504376,
2.71531100781712));
#225141=CARTESIAN_POINT('Ctrl Pts',(59.0822228828154,-0.138334211749356,
2.70899119176068));
#225142=CARTESIAN_POINT('Ctrl Pts',(59.0757535782846,-0.131883990153991,
2.70298296066826));
#225143=CARTESIAN_POINT('Ctrl Pts',(59.0697047694308,-0.124808417215229,
2.69736727774127));
#225144=CARTESIAN_POINT('Ctrl Pts',(59.0640662283032,-0.118212753510043,
2.69213248525422));
#225145=CARTESIAN_POINT('Ctrl Pts',(59.0587927761314,-0.111072931137408,
2.68723866185464));
#225146=CARTESIAN_POINT('Ctrl Pts',(59.0540076654699,-0.10338954476835,
2.68278595829559));
#225147=CARTESIAN_POINT('Ctrl Pts',(59.0522572100838,-0.100578862632676,
2.68115710172796));
#225148=CARTESIAN_POINT('Ctrl Pts',(59.0505724231957,-0.0976954648437236,
2.67958763637796));
#225149=CARTESIAN_POINT('Ctrl Pts',(59.048960544286,-0.0947395585251538,
2.67808378645346));
#225150=CARTESIAN_POINT('Ctrl Pts',(59.0485729412563,-0.0940287618036577,
2.67772216078581));
#225151=CARTESIAN_POINT('Ctrl Pts',(59.0481896206934,-0.0933131922165624,
2.67736403603544));
#225152=CARTESIAN_POINT('Ctrl Pts',(59.0478106940136,-0.0925929271969761,
2.6770095693446));
#225153=CARTESIAN_POINT('Ctrl Pts',(59.0474436087926,-0.0918951704592519,
2.67666617973785));
#225154=CARTESIAN_POINT('Ctrl Pts',(59.0470806471271,-0.0911930071932342,
2.676326223141));
#225155=CARTESIAN_POINT('Ctrl Pts',(59.0467219102889,-0.0904865115876359,
2.67598984158754));
#225156=CARTESIAN_POINT('Ctrl Pts',(59.0427915336441,-0.0827460357496678,
2.672304392922));
#225157=CARTESIAN_POINT('Ctrl Pts',(59.039366072413,-0.0744802459940899,
2.66904964539953));
#225158=CARTESIAN_POINT('Ctrl Pts',(59.0365841602689,-0.0658168714606044,
2.66640203566702));
#225159=CARTESIAN_POINT('Ctrl Pts',(59.0354304183829,-0.0622239118141111,
2.66530399299418));
#225160=CARTESIAN_POINT('Ctrl Pts',(59.0343871039217,-0.0585629032862787,
2.66430995142239));
#225161=CARTESIAN_POINT('Ctrl Pts',(59.0334626554262,-0.054844071499784,
2.6634305347334));
#225162=CARTESIAN_POINT('Ctrl Pts',(59.0318859121827,-0.0485012163582169,
2.66193059792864));
#225163=CARTESIAN_POINT('Ctrl Pts',(59.0306571138137,-0.0419914004942296,
2.66076519817106));
#225164=CARTESIAN_POINT('Ctrl Pts',(59.0298212958157,-0.0353717968086348,
2.65997805604439));
#225165=CARTESIAN_POINT('Ctrl Pts',(59.0294033868167,-0.0320619949658374,
2.65958448498105));
#225166=CARTESIAN_POINT('Ctrl Pts',(59.0290851681639,-0.0287246785544886,
2.65928526260741));
#225167=CARTESIAN_POINT('Ctrl Pts',(59.0288723192866,-0.0253670368746793,
2.65908463971303));
#225168=CARTESIAN_POINT('Ctrl Pts',(59.0286594704093,-0.0220093951948699,
2.65888401681865));
#225169=CARTESIAN_POINT('Ctrl Pts',(59.0285519740191,-0.0186314705078166,
2.65878198860262));
#225170=CARTESIAN_POINT('Ctrl Pts',(59.0285534841296,-0.0152399999998093,
2.65878198860262));
#225171=CARTESIAN_POINT('Origin',(61.4240753804089,0.31749999970617,3.56647653909435));
#225172=CARTESIAN_POINT('Origin',(61.4683012396074,0.317551690013559,3.64299466007648));
#225173=CARTESIAN_POINT('Origin',(61.3422370451705,0.317500000000185,3.42473028058485));
#225174=CARTESIAN_POINT('Ctrl Pts',(61.2322532920972,0.316930737396099,
3.48823028058485));
#225175=CARTESIAN_POINT('Ctrl Pts',(61.2327440814646,0.190500000000179,
3.48794691941601));
#225176=CARTESIAN_POINT('Ctrl Pts',(61.3422370451705,0.190500000000185,
3.42473028058486));
#225177=CARTESIAN_POINT('Ctrl Pts',(61.1872475084174,0.317046579199821,
3.41028005925091));
#225178=CARTESIAN_POINT('Ctrl Pts',(61.1875064541755,0.1905000000014,3.40982512230973));
#225179=CARTESIAN_POINT('Ctrl Pts',(61.2747290395309,0.190500000000186,
3.30780486372821));
#225180=CARTESIAN_POINT('Ctrl Pts',(61.1019842137032,0.317266596913676,
3.36123028058482));
#225181=CARTESIAN_POINT('Ctrl Pts',(61.1018997758111,0.190500000000209,
3.36099721048472));
#225182=CARTESIAN_POINT('Ctrl Pts',(61.1468362071712,0.190500000000187,
3.23423045308393));
#225183=CARTESIAN_POINT('Ctrl Pts',(61.0122769227456,0.317500000000186,
3.36123028058482));
#225184=CARTESIAN_POINT('Ctrl Pts',(61.0122769227456,0.190500000000186,
3.36123028058482));
#225185=CARTESIAN_POINT('Ctrl Pts',(61.0122769227456,0.190500000000187,
3.23423028058482));
#225186=CARTESIAN_POINT('Origin',(61.0122769227456,0.317500000000187,3.23423028058482));
#225187=CARTESIAN_POINT('Origin',(5.50819412990574E-15,0.317500000000184,
3.64303198860263));
#225188=CARTESIAN_POINT('Origin',(61.8696548221181,0.317500000000184,3.64303198860263));
#225189=CARTESIAN_POINT('Origin',(5.56576032196012E-15,0.317500000000187,
3.23423028058482));
#225190=CARTESIAN_POINT('Origin',(60.8610688070707,0.317500000000187,3.23423028058482));
#225191=CARTESIAN_POINT('Ctrl Pts',(62.4081695979768,0.318048871877314,
3.47153072139072));
#225192=CARTESIAN_POINT('Ctrl Pts',(62.4086377819835,0.190309034175474,
3.47182327902663));
#225193=CARTESIAN_POINT('Ctrl Pts',(62.3003077603771,0.19050014212524,3.40413028959023));
#225194=CARTESIAN_POINT('Ctrl Pts',(62.2931881445372,0.317932489890133,
3.65553807120956));
#225195=CARTESIAN_POINT('Ctrl Pts',(62.2934975005737,0.190309294367812,
3.6558627549695));
#225196=CARTESIAN_POINT('Ctrl Pts',(62.2083564003272,0.190500141995652,
3.5512812683729));
#225197=CARTESIAN_POINT('Ctrl Pts',(62.0866281564673,0.317722686167576,
3.77003198860264));
#225198=CARTESIAN_POINT('Ctrl Pts',(62.0868143053088,0.190309769569989,
3.77025505748508));
#225199=CARTESIAN_POINT('Ctrl Pts',(62.0431695205372,0.19050014176205,3.64284211731158));
#225200=CARTESIAN_POINT('Ctrl Pts',(61.8696548221181,0.317500000000183,
3.77003198860264));
#225201=CARTESIAN_POINT('Ctrl Pts',(61.8696548221181,0.190310267889111,
3.77003198860264));
#225202=CARTESIAN_POINT('Ctrl Pts',(61.8696548221181,0.190500141514099,
3.6428423982169));
#225203=CARTESIAN_POINT('Origin',(62.3004688883555,0.317500000000185,3.4042309748331));
#225204=CARTESIAN_POINT('Ctrl Pts',(60.8610688070707,0.317500000000186,
3.36123028058482));
#225205=CARTESIAN_POINT('Ctrl Pts',(60.8610688070707,0.190500000000186,
3.36123028058482));
#225206=CARTESIAN_POINT('Ctrl Pts',(60.8610688070707,0.190500000000187,
3.23423028058482));
#225207=CARTESIAN_POINT('Ctrl Pts',(60.7710583184321,0.31773477376044,3.36123028058482));
#225208=CARTESIAN_POINT('Ctrl Pts',(60.7709717342409,0.190500000000059,
3.36146538610129));
#225209=CARTESIAN_POINT('Ctrl Pts',(60.7260547307357,0.190500000000187,
3.23423043688415));
#225210=CARTESIAN_POINT('Ctrl Pts',(60.6859465754578,0.317958617919221,
3.41054258693101));
#225211=CARTESIAN_POINT('Ctrl Pts',(60.6862105562578,0.190500000001745,
3.41100608859818));
#225212=CARTESIAN_POINT('Ctrl Pts',(60.598389295541,0.190500000000186,3.30819866970851));
#225213=CARTESIAN_POINT('Ctrl Pts',(60.6410923272405,0.318076890623551,
3.48823028058482));
#225214=CARTESIAN_POINT('Ctrl Pts',(60.6415942020421,0.190500000000185,
3.48852004212259));
#225215=CARTESIAN_POINT('Ctrl Pts',(60.5311086139135,0.190500000000185,
3.42473028058481));
#225216=CARTESIAN_POINT('Origin',(60.5311086139135,0.317500000000185,3.42473028058481));
#225217=CARTESIAN_POINT('Origin',(62.4786179998493,0.3174999999779,3.11913648178449));
#225218=CARTESIAN_POINT('Origin',(62.6567671111299,0.317500000000189,2.83404198860263));
#225219=CARTESIAN_POINT('Origin',(60.4497583458784,0.317499999994999,3.56563113460752));
#225220=CARTESIAN_POINT('Origin',(60.4050521322804,0.317550804320461,3.64299171721808));
#225221=CARTESIAN_POINT('Ctrl Pts',(62.9541448057648,0.0152661173110579,
2.59908173516024));
#225222=CARTESIAN_POINT('Ctrl Pts',(62.9168399481843,0.0152570710388248,
2.65878198860262));
#225223=CARTESIAN_POINT('Ctrl Pts',(62.8464427007196,0.0152400000001907,
2.65878198860262));
#225224=CARTESIAN_POINT('Ctrl Pts',(62.9541233134297,0.103381504925395,
2.59908193475635));
#225225=CARTESIAN_POINT('Ctrl Pts',(62.9168211560341,0.0794415635237661,
2.65878715325387));
#225226=CARTESIAN_POINT('Ctrl Pts',(62.8464212442881,0.0662446030561332,
2.65878198860262));
#225227=CARTESIAN_POINT('Ctrl Pts',(62.9290872705826,0.184683583687983,
2.63878778849892));
#225228=CARTESIAN_POINT('Ctrl Pts',(62.8936771137448,0.138547994784479,
2.69564460180121));
#225229=CARTESIAN_POINT('Ctrl Pts',(62.8213855864655,0.113305567451748,
2.6818048162489));
#225230=CARTESIAN_POINT('Ctrl Pts',(62.8564203507742,0.291340992631895,
2.75443238878626));
#225231=CARTESIAN_POINT('Ctrl Pts',(62.8329175802742,0.20191035119155,2.79268340777087));
#225232=CARTESIAN_POINT('Ctrl Pts',(62.7487193609389,0.175042741958035,
2.74885926835605));
#225233=CARTESIAN_POINT('Ctrl Pts',(62.8099434033762,0.318045276842822,
2.82856655361685));
#225234=CARTESIAN_POINT('Ctrl Pts',(62.7947175425004,0.205831635643201,
2.85384197230834));
#225235=CARTESIAN_POINT('Ctrl Pts',(62.7022409210441,0.190500000000191,
2.79184624278459));
#225236=CARTESIAN_POINT('Ctrl Pts',(62.7644678366119,0.318045750793234,
2.90134173516025));
#225237=CARTESIAN_POINT('Ctrl Pts',(62.7649326510149,0.190500000000187,
2.90163218716392));
#225238=CARTESIAN_POINT('Ctrl Pts',(62.6567671111299,0.19050000000019,2.83404198860263));
#225239=CARTESIAN_POINT('Origin',(62.8464427007196,0.0152400000001916,2.53178198860262));
#225240=CARTESIAN_POINT('Origin',(5.50819412990574E-15,0.317500000000184,
3.64303198860263));
#225241=CARTESIAN_POINT('Origin',(60.0036905223731,0.317500000000184,3.64303198860263));
#225242=CARTESIAN_POINT('Origin',(-1.95097259456047E-16,1.91577434745604E-13,
2.53178198860262));
#225243=CARTESIAN_POINT('Origin',(62.8464427007196,-0.0152399999998084,
2.53178198860262));
#225244=CARTESIAN_POINT('Ctrl Pts',(60.0036905223731,0.317500000000183,
3.77003198860264));
#225245=CARTESIAN_POINT('Ctrl Pts',(60.0036905223731,0.190309748265493,
3.77003198860264));
#225246=CARTESIAN_POINT('Ctrl Pts',(60.0036905223731,0.190500142289713,
3.64284187937064));
#225247=CARTESIAN_POINT('Ctrl Pts',(59.7867137603524,0.317270385524599,
3.77003198860264));
#225248=CARTESIAN_POINT('Ctrl Pts',(59.7869045527984,0.190310262476557,
3.76980208962932));
#225249=CARTESIAN_POINT('Ctrl Pts',(59.8301727552497,0.190500142032646,
3.6428419392832));
#225250=CARTESIAN_POINT('Ctrl Pts',(59.5801552670728,0.317049440713801,
3.65553535416585));
#225251=CARTESIAN_POINT('Ctrl Pts',(59.5804765271851,0.19031076108255,3.65520057834439));
#225252=CARTESIAN_POINT('Ctrl Pts',(59.6649871046547,0.19050014178529,3.55127910964224));
#225253=CARTESIAN_POINT('Ctrl Pts',(59.4651754363832,0.316925998273232,
3.47153072139074));
#225254=CARTESIAN_POINT('Ctrl Pts',(59.4656607446594,0.190311035335236,
3.47122746281584));
#225255=CARTESIAN_POINT('Ctrl Pts',(59.5730368716576,0.190500141647087,
3.40413045901283));
#225256=CARTESIAN_POINT('Origin',(59.5728760150042,0.317500000000185,3.40423097483311));
#225257=CARTESIAN_POINT('Ctrl Pts',(62.7644678366119,-0.318045750792856,
2.90134173516023));
#225258=CARTESIAN_POINT('Ctrl Pts',(62.7649326510148,-0.190499999999811,
2.90163218716391));
#225259=CARTESIAN_POINT('Ctrl Pts',(62.6567671111299,-0.190499999999811,
2.83404198860262));
#225260=CARTESIAN_POINT('Ctrl Pts',(62.8099640589334,-0.318045262794995,
2.82853349835363));
#225261=CARTESIAN_POINT('Ctrl Pts',(62.7947344577641,-0.205840330722858,
2.85381483162469));
#225262=CARTESIAN_POINT('Ctrl Pts',(62.7022616416345,-0.19049999999981,
2.79182701594314));
#225263=CARTESIAN_POINT('Ctrl Pts',(62.8562601188215,-0.291334117855231,
2.75468822073634));
#225264=CARTESIAN_POINT('Ctrl Pts',(62.8328016940824,-0.201836550627568,
2.79286913083857));
#225265=CARTESIAN_POINT('Ctrl Pts',(62.7485591297232,-0.175038734051986,
2.74900763297918));
#225266=CARTESIAN_POINT('Ctrl Pts',(62.928611257107,-0.185622189560187,
2.63954450640402));
#225267=CARTESIAN_POINT('Ctrl Pts',(62.8932808767899,-0.139140155999895,
2.69627684028843));
#225268=CARTESIAN_POINT('Ctrl Pts',(62.8209095783125,-0.113848895265506,
2.68224356036487));
#225269=CARTESIAN_POINT('Ctrl Pts',(62.9541233349674,-0.103673266462647,
2.59908178706356));
#225270=CARTESIAN_POINT('Ctrl Pts',(62.9168211653022,-0.0796882264535046,
2.65878704321517));
#225271=CARTESIAN_POINT('Ctrl Pts',(62.8464212664863,-0.0664134143649492,
2.65878198860262));
#225272=CARTESIAN_POINT('Ctrl Pts',(62.9541448057648,-0.0152661173106757,
2.59908173516024));
#225273=CARTESIAN_POINT('Ctrl Pts',(62.9168399481843,-0.0152570710384434,
2.65878198860262));
#225274=CARTESIAN_POINT('Ctrl Pts',(62.8464427007196,-0.0152399999998093,
2.65878198860262));
#225275=CARTESIAN_POINT('Origin',(62.6567671111299,-0.31749999999981,2.83404198860262));
#225276=CARTESIAN_POINT('Origin',(59.3947266586253,0.31749999997129,3.11913648167031));
#225277=CARTESIAN_POINT('Origin',(59.2165773020941,0.317500000000189,2.83404198860263));
#225278=CARTESIAN_POINT('Origin',(62.4786179998359,-0.317499999976169,3.1191364817761));
#225279=CARTESIAN_POINT('Origin',(62.3004688883555,-0.317499999999815,3.4042309748331));
#225280=CARTESIAN_POINT('Ctrl Pts',(59.1088767419348,0.316922544675878,
2.90134173516024));
#225281=CARTESIAN_POINT('Ctrl Pts',(59.1093642282367,0.190500000000189,
2.9010371155323));
#225282=CARTESIAN_POINT('Ctrl Pts',(59.2165773020941,0.19050000000019,2.83404198860262));
#225283=CARTESIAN_POINT('Ctrl Pts',(59.0634407053229,0.316922012809351,
2.82862991747967));
#225284=CARTESIAN_POINT('Ctrl Pts',(59.0793536643051,0.20569497374123,2.85314045886384));
#225285=CARTESIAN_POINT('Ctrl Pts',(59.1711393827298,0.19050000000019,2.79187960999874));
#225286=CARTESIAN_POINT('Ctrl Pts',(59.0174076205275,0.290332993455118,
2.7547062579332));
#225287=CARTESIAN_POINT('Ctrl Pts',(59.0412846811395,0.201480151666008,
2.79224250381903));
#225288=CARTESIAN_POINT('Ctrl Pts',(59.1251084688121,0.175054909459896,
2.7490180910826));
#225289=CARTESIAN_POINT('Ctrl Pts',(58.9458296250063,0.184894967401825,
2.63947868311706));
#225290=CARTESIAN_POINT('Ctrl Pts',(58.9812445774292,0.138672156931444,
2.69595066767909));
#225291=CARTESIAN_POINT('Ctrl Pts',(59.0535312451933,0.113807322597966,
2.68220539436061));
#225292=CARTESIAN_POINT('Ctrl Pts',(58.9208287018089,0.103171606455877,
2.59908178585054));
#225293=CARTESIAN_POINT('Ctrl Pts',(58.9581363848276,0.0793367652459778,
2.65877670944829));
#225294=CARTESIAN_POINT('Ctrl Pts',(59.0285307646513,0.0663350652345533,
2.65878198860262));
#225295=CARTESIAN_POINT('Ctrl Pts',(58.9208513795073,0.0152121934561115,
2.59908173516024));
#225296=CARTESIAN_POINT('Ctrl Pts',(58.9581562369413,0.0152218248292979,
2.65878198860262));
#225297=CARTESIAN_POINT('Ctrl Pts',(59.0285534841296,0.015240000000191,
2.65878198860262));
#225298=CARTESIAN_POINT('Origin',(59.0285534841296,0.0152400000001916,2.53178198860262));
#225299=CARTESIAN_POINT('Ctrl Pts',(61.8696548221181,-0.317499999999817,
3.77003198860264));
#225300=CARTESIAN_POINT('Ctrl Pts',(61.8696548221181,-0.19031025693103,
3.77003198860264));
#225301=CARTESIAN_POINT('Ctrl Pts',(61.8696548221181,-0.190500141530065,
3.64284238727555));
#225302=CARTESIAN_POINT('Ctrl Pts',(62.0866315324121,-0.317722689632047,
3.77003198860264));
#225303=CARTESIAN_POINT('Ctrl Pts',(62.0868176889517,-0.190309758575249,
3.77025506105891));
#225304=CARTESIAN_POINT('Ctrl Pts',(62.0431722165643,-0.190500141778049,
3.64284210641918));
#225305=CARTESIAN_POINT('Ctrl Pts',(62.2931898887681,-0.317932491655493,
3.65553527987835));
#225306=CARTESIAN_POINT('Ctrl Pts',(62.293499245807,-0.190309283352059,
3.65585996533076));
#225307=CARTESIAN_POINT('Ctrl Pts',(62.2083577878532,-0.190500142011671,
3.55127902710177));
#225308=CARTESIAN_POINT('Ctrl Pts',(62.4081695979768,-0.318048871876944,
3.47153072139071));
#225309=CARTESIAN_POINT('Ctrl Pts',(62.4086377820239,-0.190309023146102,
3.47182327905188));
#225310=CARTESIAN_POINT('Ctrl Pts',(62.3003077510784,-0.190500142141273,
3.40413028377964));
#225311=CARTESIAN_POINT('Origin',(61.8696548221181,-0.317499999999816,3.64303198860263));
#225312=CARTESIAN_POINT('Origin',(4.7062627014205E-16,1.91577434745604E-13,
2.53178198860262));
#225313=CARTESIAN_POINT('Origin',(59.0285534841296,-0.0152399999998084,
2.53178198860262));
#225314=CARTESIAN_POINT('Origin',(62.2224557307631,-0.317499999999816,3.64303198860263));
#225315=CARTESIAN_POINT('Origin',(61.4683012396074,-0.317551690013422,3.64299466007613));
#225316=CARTESIAN_POINT('Ctrl Pts',(58.9208513795073,-0.0152121934557287,
2.59908173516024));
#225317=CARTESIAN_POINT('Ctrl Pts',(58.9581562369414,-0.0152218248289162,
2.65878198860262));
#225318=CARTESIAN_POINT('Ctrl Pts',(59.0285534841296,-0.0152399999998093,
2.65878198860262));
#225319=CARTESIAN_POINT('Ctrl Pts',(58.9208288705618,-0.102871702177174,
2.59908193199893));
#225320=CARTESIAN_POINT('Ctrl Pts',(58.9581365422946,-0.0790852439331895,
2.65877685806655));
#225321=CARTESIAN_POINT('Ctrl Pts',(59.0285309330218,-0.0661608181923042,
2.65878198860262));
#225322=CARTESIAN_POINT('Ctrl Pts',(58.9453619764183,-0.183955833237358,
2.63872492669802));
#225323=CARTESIAN_POINT('Ctrl Pts',(58.9808530699761,-0.138075936735796,
2.69532212015275));
#225324=CARTESIAN_POINT('Ctrl Pts',(59.0530636028226,-0.113261762367989,
2.68176836726639));
#225325=CARTESIAN_POINT('Ctrl Pts',(59.0172303255293,-0.290319860890428,
2.75442176402246));
#225326=CARTESIAN_POINT('Ctrl Pts',(59.0411528690721,-0.201541405841727,
2.79203179920136));
#225327=CARTESIAN_POINT('Ctrl Pts',(59.1249311745757,-0.175047309550979,
2.74885310748172));
#225328=CARTESIAN_POINT('Ctrl Pts',(59.0634600627912,-0.316922027357153,
2.82866089558405));
#225329=CARTESIAN_POINT('Ctrl Pts',(59.0793694364684,-0.205687000367097,
2.85316563119185));
#225330=CARTESIAN_POINT('Ctrl Pts',(59.1711586818656,-0.19049999999981,
2.79189751796654));
#225331=CARTESIAN_POINT('Ctrl Pts',(59.1088767419348,-0.3169225446755,2.90134173516024));
#225332=CARTESIAN_POINT('Ctrl Pts',(59.1093642282367,-0.190499999999811,
2.9010371155323));
#225333=CARTESIAN_POINT('Ctrl Pts',(59.2165773020941,-0.190499999999811,
2.83404198860262));
#225334=CARTESIAN_POINT('Origin',(59.2165773020941,-0.31749999999981,2.83404198860262));
#225335=CARTESIAN_POINT('Origin',(61.4240753793285,-0.317499999994572,3.56647653971808));
#225336=CARTESIAN_POINT('Origin',(61.3422370451705,-0.317499999999815,3.42473028058486));
#225337=CARTESIAN_POINT('Origin',(59.3947266586072,-0.317499999969147,3.1191364816816));
#225338=CARTESIAN_POINT('Origin',(59.5728760150042,-0.317499999999815,3.4042309748331));
#225339=CARTESIAN_POINT('Ctrl Pts',(61.0122769227456,-0.317499999999814,
3.36123028058482));
#225340=CARTESIAN_POINT('Ctrl Pts',(61.0122769227456,-0.190499999999814,
3.36123028058482));
#225341=CARTESIAN_POINT('Ctrl Pts',(61.0122769227456,-0.190499999999813,
3.23423028058482));
#225342=CARTESIAN_POINT('Ctrl Pts',(61.1022873990971,-0.317265808076204,
3.36123028058482));
#225343=CARTESIAN_POINT('Ctrl Pts',(61.1022028716704,-0.190499999999688,
3.36099641108529));
#225344=CARTESIAN_POINT('Ctrl Pts',(61.1472909869838,-0.190499999999813,
3.23423043688437));
#225345=CARTESIAN_POINT('Ctrl Pts',(61.1873990841185,-0.317046189128919,
3.41054258905285));
#225346=CARTESIAN_POINT('Ctrl Pts',(61.1876587562326,-0.190500000001028,
3.41008815825968));
#225347=CARTESIAN_POINT('Ctrl Pts',(61.2749563897835,-0.190499999999814,
3.30819867304271));
#225348=CARTESIAN_POINT('Ctrl Pts',(61.2322532920972,-0.316930737395729,
3.48823028058483));
#225349=CARTESIAN_POINT('Ctrl Pts',(61.2327440814646,-0.190499999999809,
3.487946919416));
#225350=CARTESIAN_POINT('Ctrl Pts',(61.3422370451705,-0.190499999999815,
3.42473028058484));
#225351=CARTESIAN_POINT('Origin',(61.0122769227456,-0.317499999999813,3.23423028058482));
#225352=CARTESIAN_POINT('Ctrl Pts',(59.4651754363832,-0.316925998272862,
3.47153072139073));
#225353=CARTESIAN_POINT('Ctrl Pts',(59.4656607446034,-0.190311049924885,
3.47122746285078));
#225354=CARTESIAN_POINT('Ctrl Pts',(59.573036859247,-0.190500141624861,
3.4041304667679));
#225355=CARTESIAN_POINT('Ctrl Pts',(59.5801570044831,-0.317049442578994,
3.65553813457986));
#225356=CARTESIAN_POINT('Ctrl Pts',(59.5804782634893,-0.190310775687599,
3.65520336072057));
#225357=CARTESIAN_POINT('Ctrl Pts',(59.6649884842709,-0.190500141763048,
3.55128134519903));
#225358=CARTESIAN_POINT('Ctrl Pts',(59.7867171285936,-0.317270389088646,
3.77003198860264));
#225359=CARTESIAN_POINT('Ctrl Pts',(59.7869079131804,-0.190310277117966,
3.76980209314202));
#225360=CARTESIAN_POINT('Ctrl Pts',(59.8301754438931,-0.190500142010366,
3.6428419538746));
#225361=CARTESIAN_POINT('Ctrl Pts',(60.0036905223731,-0.317499999999817,
3.77003198860264));
#225362=CARTESIAN_POINT('Ctrl Pts',(60.0036905223731,-0.190309762954565,
3.77003198860264));
#225363=CARTESIAN_POINT('Ctrl Pts',(60.0036905223731,-0.19050014226739,
3.64284189403806));
#225364=CARTESIAN_POINT('Origin',(60.0036905223731,-0.317499999999816,3.64303198860263));
#225365=CARTESIAN_POINT('Origin',(60.71525,-0.317499999999813,3.23423028058482));
#225366=CARTESIAN_POINT('Origin',(60.8610688070707,-0.317499999999813,3.23423028058482));
#225367=CARTESIAN_POINT('Origin',(60.4792282238308,-0.317499999999816,3.64303198860263));
#225368=CARTESIAN_POINT('Origin',(60.4050521322803,-0.317550804320321,3.64299171721791));
#225369=CARTESIAN_POINT('Ctrl Pts',(60.6410923272405,-0.318076890623181,
3.48823028058482));
#225370=CARTESIAN_POINT('Ctrl Pts',(60.6415942020421,-0.190499999999815,
3.48852004212259));
#225371=CARTESIAN_POINT('Ctrl Pts',(60.5311086139135,-0.190499999999815,
3.42473028058481));
#225372=CARTESIAN_POINT('Ctrl Pts',(60.6860981505083,-0.317958218318571,
3.41028005848409));
#225373=CARTESIAN_POINT('Ctrl Pts',(60.6863613750299,-0.190499999999808,
3.41074404220335));
#225374=CARTESIAN_POINT('Ctrl Pts',(60.5986166446971,-0.190499999999814,
3.307804862439));
#225375=CARTESIAN_POINT('Ctrl Pts',(60.771361502534,-0.317733982967355,
3.36123028058482));
#225376=CARTESIAN_POINT('Ctrl Pts',(60.7712750141982,-0.190499999999842,
3.36146460586441));
#225377=CARTESIAN_POINT('Ctrl Pts',(60.7265095085039,-0.190499999999813,
3.23423045308464));
#225378=CARTESIAN_POINT('Ctrl Pts',(60.8610688070707,-0.317499999999814,
3.36123028058482));
#225379=CARTESIAN_POINT('Ctrl Pts',(60.8610688070707,-0.190499999999814,
3.36123028058482));
#225380=CARTESIAN_POINT('Ctrl Pts',(60.8610688070707,-0.190499999999813,
3.23423028058482));
#225381=CARTESIAN_POINT('Origin',(60.5311086139135,-0.317499999999815,3.42473028058481));
#225382=CARTESIAN_POINT('Origin',(60.4497583469872,-0.317500000300251,3.5656311352477));
#225383=CARTESIAN_POINT('Origin',(57.9645097668785,5.90076614434095,2.65878198860267));
#225384=CARTESIAN_POINT('',(58.7035958781039,6.18532049829418,2.65878198860267));
#225385=CARTESIAN_POINT('',(62.5005702980931,6.58439859103048,2.65878198860267));
#225386=CARTESIAN_POINT('',(57.9430040808458,6.10537907909402,2.65878198860267));
#225387=CARTESIAN_POINT('',(62.5037563256535,6.55408556365965,2.65878198860267));
#225388=CARTESIAN_POINT('Origin',(5.50059263827931E-15,1.84980347606071E-13,
2.65878198860263));
#225389=CARTESIAN_POINT('',(58.7067819056643,6.15500747092335,2.65878198860267));
#225390=CARTESIAN_POINT('',(58.63646617859,6.14761699020205,2.65878198860267));
#225391=CARTESIAN_POINT('Origin',(5.72291486498914E-15,1.85445891303602E-13,
2.65878198860263));
#225392=CARTESIAN_POINT('Origin',(0.019912672252488,-0.189456421067745,
42.7590319886026));
#225393=CARTESIAN_POINT('',(59.6948966996543,6.08263713962406,3.64303198860267));
#225394=CARTESIAN_POINT('',(59.2664422392336,6.03760476121538,3.40423097483316));
#225395=CARTESIAN_POINT('Origin',(59.6568751110701,6.07864090963233,3.20400220531864));
#225396=CARTESIAN_POINT('',(58.9120953678975,6.00036140481925,2.83404198860266));
#225397=CARTESIAN_POINT('',(59.2664422392336,6.03760476121538,3.40423097483316));
#225398=CARTESIAN_POINT('',(62.3334394572619,6.35995915837821,2.83404198860267));
#225399=CARTESIAN_POINT('',(62.5918026085422,6.38711421981435,2.83404198860267));
#225400=CARTESIAN_POINT('',(61.9790930734951,6.32271585208523,3.40423097483316));
#225401=CARTESIAN_POINT('',(62.3334394572619,6.35995915837821,2.83404198860267));
#225402=CARTESIAN_POINT('',(61.5506390517262,6.27768352038871,3.64303198860268));
#225403=CARTESIAN_POINT('Origin',(61.5886607627696,6.28167976325143,3.20400259788071));
#225404=CARTESIAN_POINT('',(61.1514583086406,6.23572793293823,3.64303198860268));
#225405=CARTESIAN_POINT('',(0.0199126722524935,-0.189456421067472,3.64303198860262));
#225406=CARTESIAN_POINT('',(61.0261105245454,6.22255335066435,3.4247302805849));
#225407=CARTESIAN_POINT('',(61.1514583085662,6.2357279336461,3.64303198860268));
#225408=CARTESIAN_POINT('',(60.6979579581954,6.18806312612766,3.23423028058487));
#225409=CARTESIAN_POINT('Origin',(60.7272241158227,6.19113963944967,3.56425722717094));
#225410=CARTESIAN_POINT('',(60.5475781763993,6.17225757416257,3.23423028058487));
#225411=CARTESIAN_POINT('',(0.0199126722524936,-0.189456421067469,3.23423028058481));
#225412=CARTESIAN_POINT('',(60.2194255397045,6.13776734223234,3.42473028058486));
#225413=CARTESIAN_POINT('Origin',(60.5183090188079,6.16918177799164,3.56425909741038));
#225414=CARTESIAN_POINT('',(60.0940777033447,6.12459275374953,3.64303198860267));
#225415=CARTESIAN_POINT('',(60.2194255397045,6.13776734223234,3.42473028058486));
#225416=CARTESIAN_POINT('',(0.0199126722524935,-0.189456421067472,3.64303198860262));
#225417=CARTESIAN_POINT('Origin',(-0.019912672252488,0.189456421067567,
42.7590319886026));
#225418=CARTESIAN_POINT('',(61.5108137072212,6.65659636252402,3.64303198860268));
#225419=CARTESIAN_POINT('',(61.9392677289269,6.70162869482191,3.40423097483315));
#225420=CARTESIAN_POINT('Origin',(61.5488354179799,6.66059260535681,3.20400259735912));
#225421=CARTESIAN_POINT('',(62.2936141127097,6.73887200096321,2.83404198860267));
#225422=CARTESIAN_POINT('',(61.9392677289269,6.70162869482191,3.40423097483315));
#225423=CARTESIAN_POINT('',(58.872270023448,6.37927424642597,2.83404198860267));
#225424=CARTESIAN_POINT('',(-0.019912672252488,0.189456421067845,2.83404198860263));
#225425=CARTESIAN_POINT('',(59.2266168948024,6.41651760264857,3.40423097483316));
#225426=CARTESIAN_POINT('',(58.872270023448,6.37927424642597,2.83404198860267));
#225427=CARTESIAN_POINT('',(59.6550713551493,6.46154998175937,3.64303198860268));
#225428=CARTESIAN_POINT('Origin',(59.6170497662628,6.45755375173588,3.20400220587344));
#225429=CARTESIAN_POINT('',(60.0542523589172,6.50350559514725,3.64303198860268));
#225430=CARTESIAN_POINT('',(60.1277056317065,6.51122584595726,3.64303198860268));
#225431=CARTESIAN_POINT('',(60.1796001951995,6.51668018436765,3.42473028058486));
#225432=CARTESIAN_POINT('',(60.0542523588397,6.50350559588484,3.64303198860268));
#225433=CARTESIAN_POINT('',(60.5077528318944,6.55117041629788,3.23423028058487));
#225434=CARTESIAN_POINT('Origin',(60.4784867342337,6.54809390915812,3.56425743004413));
#225435=CARTESIAN_POINT('',(60.6581326136904,6.56697596826297,3.23423028058487));
#225436=CARTESIAN_POINT('',(60.6586584283283,6.56703123360838,3.23423028058487));
#225437=CARTESIAN_POINT('',(60.9862851800404,6.60146619279966,3.42473028058489));
#225438=CARTESIAN_POINT('Origin',(60.6874016969832,6.57005175674002,3.56425912917906));
#225439=CARTESIAN_POINT('',(61.1116329640613,6.61464077578141,3.64303198860268));
#225440=CARTESIAN_POINT('',(60.9862851800404,6.60146619279966,3.42473028058489));
#225441=CARTESIAN_POINT('',(61.5113322352818,6.65665086201929,3.64303198860268));
#225442=CARTESIAN_POINT('Origin',(57.030176100279,11.9273822599896,2.65878198860271));
#225443=CARTESIAN_POINT('',(57.7354693911204,12.2876333308473,2.65878198860271));
#225444=CARTESIAN_POINT('',(61.4699285681954,13.0814171332235,2.65878198860272));
#225445=CARTESIAN_POINT('',(56.9874003490102,12.1286263473646,2.65878198860271));
#225446=CARTESIAN_POINT('',(61.4762657165316,13.0516031943531,2.65878198860272));
#225447=CARTESIAN_POINT('Origin',(5.50299975530876E-15,1.8496514966728E-13,
2.65878198860263));
#225448=CARTESIAN_POINT('',(57.7418065394566,12.257819391977,2.65878198860271));
#225449=CARTESIAN_POINT('',(57.672648524885,12.2431194021877,2.65878198860271));
#225450=CARTESIAN_POINT('Origin',(5.72166156020094E-15,1.85453804358607E-13,
2.65878198860263));
#225451=CARTESIAN_POINT('Origin',(0.0396071771007832,-0.186337117939879,
42.7590319886026));
#225452=CARTESIAN_POINT('',(58.7320730967338,12.2891316338726,3.64303198860272));
#225453=CARTESIAN_POINT('',(58.3106729199896,12.1995602612167,3.4042309748332));
#225454=CARTESIAN_POINT('Origin',(58.6946775141712,12.2811829574214,3.20400220531691));
#225455=CARTESIAN_POINT('',(57.9621601887016,12.1254815938992,2.83404198860271));
#225456=CARTESIAN_POINT('',(58.3106729199896,12.1995602612167,3.4042309748332));
#225457=CARTESIAN_POINT('',(61.3271735965893,12.84073727331,2.83404198860271));
#225458=CARTESIAN_POINT('',(61.581282930652,12.8947498796466,2.83404198860271));
#225459=CARTESIAN_POINT('',(60.9786613449626,12.7666587067856,3.4042309748332));
#225460=CARTESIAN_POINT('',(61.3271735965893,12.84073727331,2.83404198860271));
#225461=CARTESIAN_POINT('',(60.5572615995843,12.6770874264381,3.64303198860273));
#225462=CARTESIAN_POINT('Origin',(60.5946573025915,12.6850361284906,3.20400259788215));
#225463=CARTESIAN_POINT('',(60.164653163458,12.5936359264448,3.64303198860272));
#225464=CARTESIAN_POINT('',(0.0396071771007887,-0.186337117939606,3.64303198860262));
#225465=CARTESIAN_POINT('',(60.0413691664787,12.5674311046656,3.42473028058494));
#225466=CARTESIAN_POINT('',(60.16465316331,12.593635927141,3.64303198860272));
#225467=CARTESIAN_POINT('',(59.7186194643909,12.4988285377098,3.23423028058491));
#225468=CARTESIAN_POINT('Origin',(59.747403715734,12.5049473440523,3.56425722717254));
#225469=CARTESIAN_POINT('',(59.5707156088321,12.4673906027145,3.23423028058491));
#225470=CARTESIAN_POINT('',(0.0396071771007888,-0.186337117939603,3.23423028058481));
#225471=CARTESIAN_POINT('',(59.2479658375576,12.3987880210526,3.4247302805849));
#225472=CARTESIAN_POINT('Origin',(59.5419282989951,12.4612721960125,3.56425909740992));
#225473=CARTESIAN_POINT('',(59.124681789249,12.3725831876354,3.64303198860272));
#225474=CARTESIAN_POINT('',(59.2479658375576,12.3987880210526,3.4247302805849));
#225475=CARTESIAN_POINT('',(0.0396071771007887,-0.186337117939606,3.64303198860262));
#225476=CARTESIAN_POINT('Origin',(-0.0396071771007832,0.186337117939701,
42.7590319886026));
#225477=CARTESIAN_POINT('',(60.4780472453827,13.0497616623177,3.64303198860272));
#225478=CARTESIAN_POINT('',(60.8994469906352,13.1393329432572,3.4042309748332));
#225479=CARTESIAN_POINT('Origin',(60.5154429481088,13.0577103643104,3.20400259735752));
#225480=CARTESIAN_POINT('',(61.2479592422937,13.2134115096321,2.83404198860272));
#225481=CARTESIAN_POINT('',(60.8994469906352,13.1393329432572,3.4042309748332));
#225482=CARTESIAN_POINT('',(57.8829458346105,12.4981558292589,2.83404198860271));
#225483=CARTESIAN_POINT('',(-0.0396071771007831,0.186337117939978,2.83404198860263));
#225484=CARTESIAN_POINT('',(58.2314585659348,12.5722344964055,3.40423097483319));
#225485=CARTESIAN_POINT('',(57.8829458346105,12.4981558292589,2.83404198860271));
#225486=CARTESIAN_POINT('',(58.6528587425322,12.6618058697521,3.64303198860272));
#225487=CARTESIAN_POINT('Origin',(58.6154631596726,12.6538571932379,3.20400220587084));
#225488=CARTESIAN_POINT('',(59.0454674352017,12.7452574227893,3.64303198860272));
#225489=CARTESIAN_POINT('',(59.1177113373238,12.7606133389844,3.64303198860272));
#225490=CARTESIAN_POINT('',(59.1687514833561,12.7714622569322,3.4247302805849));
#225491=CARTESIAN_POINT('',(59.0454674350475,12.7452574235149,3.64303198860272));
#225492=CARTESIAN_POINT('',(59.4915012546305,12.8400648385941,3.23423028058491));
#225493=CARTESIAN_POINT('Origin',(59.4627170622781,12.8339460446679,3.5642574300432));
#225494=CARTESIAN_POINT('',(59.6394051101893,12.8715027735894,3.23423028058491));
#225495=CARTESIAN_POINT('',(59.639922267558,12.8716126987815,3.23423028058491));
#225496=CARTESIAN_POINT('',(59.9621548122771,12.9401053405452,3.42473028058493));
#225497=CARTESIAN_POINT('Origin',(59.6681923469394,12.8776211648734,3.5642591291771));
#225498=CARTESIAN_POINT('',(60.0854388091085,12.9663101630206,3.64303198860272));
#225499=CARTESIAN_POINT('',(59.9621548122771,12.9401053405452,3.42473028058493));
#225500=CARTESIAN_POINT('',(60.4785572361439,13.0498700642004,3.64303198860272));
#225501=CARTESIAN_POINT('Origin',(55.4710078899933,17.8233194796326,2.65878198860275));
#225502=CARTESIAN_POINT('',(56.1347810195642,18.2553202812751,2.65878198860275));
#225503=CARTESIAN_POINT('',(59.7658094374951,19.4351129318423,2.65878198860276));
#225504=CARTESIAN_POINT('',(55.4074307335706,18.0189898472952,2.65878198860275));
#225505=CARTESIAN_POINT('',(59.7752282754837,19.4061247292256,2.65878198860276));
#225506=CARTESIAN_POINT('Origin',(5.50698230308588E-15,1.84950286596632E-13,
2.65878198860263));
#225507=CARTESIAN_POINT('',(56.1441998575527,18.2263320786585,2.65878198860275));
#225508=CARTESIAN_POINT('',(56.0769572651639,18.2044836359655,2.65878198860275));
#225509=CARTESIAN_POINT('Origin',(5.71958798166808E-15,1.85461543059045E-13,
2.65878198860263));
#225510=CARTESIAN_POINT('Origin',(0.0588677374284276,-0.181176266354316,
42.7590319886026));
#225511=CARTESIAN_POINT('',(57.1257686104891,18.3609838302742,3.64303198860276));
#225512=CARTESIAN_POINT('',(56.7160396659414,18.227854826074,3.40423097483324));
#225513=CARTESIAN_POINT('Origin',(57.089408747774,18.3491697947258,3.20400220531851));
#225514=CARTESIAN_POINT('',(56.3771794531164,18.1177524692166,2.83404198860275));
#225515=CARTESIAN_POINT('',(56.7160396659414,18.227854826074,3.40423097483324));
#225516=CARTESIAN_POINT('',(59.6489943884564,19.1808295835784,2.83404198860276));
#225517=CARTESIAN_POINT('',(59.8960658302617,19.2611079613976,2.83404198860276));
#225518=CARTESIAN_POINT('',(59.3101346421294,19.0707273770999,3.40423097483324));
#225519=CARTESIAN_POINT('',(59.6489943884564,19.1808295835784,2.83404198860276));
#225520=CARTESIAN_POINT('',(58.9004061169357,18.9375985097924,3.64303198860277));
#225521=CARTESIAN_POINT('Origin',(58.9367660967588,18.9494125833916,3.20400259788259));
#225522=CARTESIAN_POINT('',(58.5186714879535,18.8135654093534,3.64303198860276));
#225523=CARTESIAN_POINT('',(0.0588677374284331,-0.181176266354043,3.64303198860263));
#225524=CARTESIAN_POINT('',(58.3988020033598,18.7746174535802,3.424730280585));
#225525=CARTESIAN_POINT('',(58.5186714877335,18.8135654100305,3.64303198860276));
#225526=CARTESIAN_POINT('',(58.08499127881,18.6726541682848,3.23423028058495));
#225527=CARTESIAN_POINT('Origin',(58.1129782575896,18.6817482287255,3.56425722717045));
#225528=CARTESIAN_POINT('',(57.9411838150807,18.6259282908539,3.23423028058495));
#225529=CARTESIAN_POINT('',(0.0588677374284332,-0.18117626635404,3.23423028058481));
#225530=CARTESIAN_POINT('',(57.6273730232605,18.523964983701,3.42473028058494));
#225531=CARTESIAN_POINT('Origin',(57.9131937527917,18.6168343081659,3.56425909741474));
#225532=CARTESIAN_POINT('',(57.5075034888353,18.485017010988,3.64303198860276));
#225533=CARTESIAN_POINT('',(57.6273730232605,18.523964983701,3.42473028058494));
#225534=CARTESIAN_POINT('',(0.0588677374284331,-0.181176266354043,3.64303198860263));
#225535=CARTESIAN_POINT('Origin',(-0.0588677374284276,0.181176266354137,
42.7590319886026));
#225536=CARTESIAN_POINT('',(58.7826706420788,19.2999510425009,3.64303198860277));
#225537=CARTESIAN_POINT('',(59.1923991670855,19.433079910384,3.40423097483324));
#225538=CARTESIAN_POINT('Origin',(58.8190306216281,19.311765116011,3.20400259735763));
#225539=CARTESIAN_POINT('',(59.5312589134598,19.5431821167169,2.83404198860276));
#225540=CARTESIAN_POINT('',(59.1923991670855,19.433079910384,3.40423097483324));
#225541=CARTESIAN_POINT('',(56.2594439784239,18.4801050014193,2.83404198860275));
#225542=CARTESIAN_POINT('',(-0.0588677374284273,0.181176266354414,2.83404198860262));
#225543=CARTESIAN_POINT('',(56.5983041913029,18.5902073581105,3.40423097483324));
#225544=CARTESIAN_POINT('',(56.2594439784239,18.4801050014193,2.83404198860275));
#225545=CARTESIAN_POINT('',(57.0080331356322,18.7233363629827,3.64303198860276));
#225546=CARTESIAN_POINT('Origin',(56.9716732726285,18.7115223273404,3.20400220587256));
#225547=CARTESIAN_POINT('',(57.3897680142076,18.8473695429911,3.64303198860276));
#225548=CARTESIAN_POINT('',(57.460011026353,18.8701928819397,3.64303198860276));
#225549=CARTESIAN_POINT('',(57.5096375484037,18.8863175164095,3.42473028058494));
#225550=CARTESIAN_POINT('',(57.3897680139784,18.8473695436964,3.64303198860276));
#225551=CARTESIAN_POINT('',(57.8234483402239,18.9882808235623,3.23423028058495));
#225552=CARTESIAN_POINT('Origin',(57.7954614188164,18.9791867816369,3.56425743004576));
#225553=CARTESIAN_POINT('',(57.9672558039532,19.0350067009933,3.23423028058495));
#225554=CARTESIAN_POINT('',(57.9677586379683,19.0351700816687,3.23423028058495));
#225555=CARTESIAN_POINT('',(58.281066528503,19.1369699862886,3.42473028058497));
#225556=CARTESIAN_POINT('Origin',(57.9952457951704,19.044100660709,3.564259129176));
#225557=CARTESIAN_POINT('',(58.4009360128767,19.1759179427389,3.64303198860277));
#225558=CARTESIAN_POINT('',(58.281066528503,19.1369699862886,3.42473028058497));
#225559=CARTESIAN_POINT('',(58.783166507975,19.3001121590972,3.64303198860277));
#225560=CARTESIAN_POINT('Origin',(53.3040877092102,23.5239806812874,2.65878198860279));
#225561=CARTESIAN_POINT('',(53.9190682401995,24.0229981225299,2.65878198860279));
#225562=CARTESIAN_POINT('',(57.4068835917979,25.575873566121,2.6587819886028));
#225563=CARTESIAN_POINT('',(53.2204057122638,23.7119335237428,2.65878198860279));
#225564=CARTESIAN_POINT('',(57.4192809246789,25.5480287005721,2.6587819886028));
#225565=CARTESIAN_POINT('Origin',(5.51249664798382E-15,1.8493592123704E-13,
2.65878198860263));
#225566=CARTESIAN_POINT('',(53.9314655730804,23.995153256981,2.65878198860279));
#225567=CARTESIAN_POINT('',(53.8668751267878,23.9663957374946,2.65878198860279));
#225568=CARTESIAN_POINT('Origin',(5.71671684795091E-15,1.85469022618095E-13,
2.65878198860263));
#225569=CARTESIAN_POINT('Origin',(0.0774833305059401,-0.174030409681005,
42.7590319886026));
#225570=CARTESIAN_POINT('',(54.8935822490122,24.2316692455485,3.6430319886028));
#225571=CARTESIAN_POINT('',(54.5000136127188,24.056441199033,3.40423097483328));
#225572=CARTESIAN_POINT('Origin',(54.8586564724108,24.2161192879489,3.20400220531754));
#225573=CARTESIAN_POINT('',(54.1745185417598,23.9115214570972,2.83404198860279));
#225574=CARTESIAN_POINT('',(54.5000136127188,24.056441199033,3.40423097483328));
#225575=CARTESIAN_POINT('',(57.317288315449,25.3107727110825,2.8340419886028));
#225576=CARTESIAN_POINT('',(57.5546148985775,25.4164373136776,2.8340419886028));
#225577=CARTESIAN_POINT('',(56.9917936927131,25.1658531674651,3.40423097483328));
#225578=CARTESIAN_POINT('',(57.317288315449,25.3107727110825,2.8340419886028));
#225579=CARTESIAN_POINT('',(56.5982254591675,24.9906253009261,3.64303198860281));
#225580=CARTESIAN_POINT('Origin',(56.6331513482583,25.0061753086093,3.20400259788195));
#225581=CARTESIAN_POINT('',(56.2315470018077,24.8273695326456,3.64303198860281));
#225582=CARTESIAN_POINT('',(0.0774833305059456,-0.174030409680732,3.64303198860263));
#225583=CARTESIAN_POINT('',(56.1164053447571,24.776105164832,3.42473028058504));
#225584=CARTESIAN_POINT('',(56.2315470015181,24.8273695332959,3.64303198860281));
#225585=CARTESIAN_POINT('',(55.8149717737126,24.641898292288,3.23423028058499));
#225586=CARTESIAN_POINT('Origin',(55.8418548487321,24.6538679703977,3.56425722716871));
#225587=CARTESIAN_POINT('',(55.6768362864792,24.5803964109126,3.23423028058499));
#225588=CARTESIAN_POINT('',(0.0774833305059457,-0.174030409680729,3.23423028058481));
#225589=CARTESIAN_POINT('',(55.3754026508175,24.4461895095991,3.42473028058498));
#225590=CARTESIAN_POINT('Origin',(55.6499501367166,24.568426487816,3.56425909741775));
#225591=CARTESIAN_POINT('',(55.260260945979,24.3949251197297,3.6430319886028));
#225592=CARTESIAN_POINT('',(55.3754026508175,24.4461895095991,3.42473028058498));
#225593=CARTESIAN_POINT('',(0.0774833305059456,-0.174030409680732,3.64303198860263));
#225594=CARTESIAN_POINT('Origin',(-0.0774833305059401,0.174030409680826,
42.7590319886026));
#225595=CARTESIAN_POINT('',(56.4432587981556,25.338686120288,3.64303198860281));
#225596=CARTESIAN_POINT('',(56.8368270314553,25.5139139873792,3.40423097483328));
#225597=CARTESIAN_POINT('Origin',(56.4781846869834,25.354236127854,3.20400259735723));
#225598=CARTESIAN_POINT('',(57.1623216542531,25.6588335308577,2.8340419886028));
#225599=CARTESIAN_POINT('',(56.8368270314553,25.5139139873792,3.40423097483328));
#225600=CARTESIAN_POINT('',(54.0195518809641,24.2595822759735,2.83404198860279));
#225601=CARTESIAN_POINT('',(-0.0774833305059396,0.174030409681103,2.83404198860262));
#225602=CARTESIAN_POINT('',(54.3450469519943,24.4045020177494,3.40423097483328));
#225603=CARTESIAN_POINT('',(54.0195518809641,24.2595822759735,2.83404198860279));
#225604=CARTESIAN_POINT('',(54.7386155880003,24.5797300649104,3.6430319886028));
#225605=CARTESIAN_POINT('Origin',(54.7036898111205,24.5641801071868,3.20400220587398));
#225606=CARTESIAN_POINT('',(55.1052942852688,24.7429859384141,3.64303198860281));
#225607=CARTESIAN_POINT('',(55.1727668102971,24.7730266428387,3.64303198860281));
#225608=CARTESIAN_POINT('',(55.2204359898056,24.794250328961,3.42473028058499));
#225609=CARTESIAN_POINT('',(55.1052942849672,24.7429859390916,3.64303198860281));
#225610=CARTESIAN_POINT('',(55.5218696254673,24.9284572302744,3.23423028058499));
#225611=CARTESIAN_POINT('Origin',(55.494986605568,24.9164875765746,3.56425743003997));
#225612=CARTESIAN_POINT('',(55.6600051127008,24.9899591116498,3.23423028058499));
#225613=CARTESIAN_POINT('',(55.6604881142076,24.9901741577757,3.23423028058499));
#225614=CARTESIAN_POINT('',(55.9614386837453,25.1241659841938,3.42473028058501));
#225615=CARTESIAN_POINT('Origin',(55.6868911941839,25.0019290044718,3.56425912917526));
#225616=CARTESIAN_POINT('',(56.0765803405063,25.1754303526578,3.64303198860281));
#225617=CARTESIAN_POINT('',(55.9614386837453,25.1241659841938,3.42473028058501));
#225618=CARTESIAN_POINT('',(56.4437351063763,25.3388981863709,3.64303198860281));
#225619=CARTESIAN_POINT('Origin',(50.5531567888875,28.9669082278886,2.65878198860283));
#225620=CARTESIAN_POINT('',(51.1126068659047,29.5274749692187,2.65878198860283));
#225621=CARTESIAN_POINT('',(54.4189959163063,31.4364195775137,2.65878198860284));
#225622=CARTESIAN_POINT('',(50.4502867888875,29.1450842944632,2.65878198860283));
#225623=CARTESIAN_POINT('',(54.4342359163063,31.4100231232064,2.65878198860284));
#225624=CARTESIAN_POINT('Origin',(5.51948237368594E-15,1.84922210978388E-13,
2.65878198860263));
#225625=CARTESIAN_POINT('',(51.1278468659047,29.5010785149114,2.65878198860283));
#225626=CARTESIAN_POINT('',(51.0666162321543,29.465726992033,2.65878198860283));
#225627=CARTESIAN_POINT('Origin',(5.71307961579125E-15,1.85476161088142E-13,
2.65878198860263));
#225628=CARTESIAN_POINT('Origin',(0.0952500000000002,-0.164977839421025,
42.7590319886026));
#225629=CARTESIAN_POINT('',(52.0599703131946,29.8368674217658,3.64303198860284));
#225630=CARTESIAN_POINT('',(51.6868740054943,29.6214601680814,3.40423097483331));
#225631=CARTESIAN_POINT('Origin',(52.0268612768246,29.8177519107051,3.20400220531536));
#225632=CARTESIAN_POINT('',(51.3783102685129,29.4433108120864,2.83404198860283));
#225633=CARTESIAN_POINT('',(51.6868740054943,29.6214601680814,3.40423097483331));
#225634=CARTESIAN_POINT('',(54.3576020372438,31.1634057161443,2.83404198860284));
#225635=CARTESIAN_POINT('',(54.582583561987,31.2932988600175,2.83404198860284));
#225636=CARTESIAN_POINT('',(54.0490387253004,30.985256604233,3.40423097483332));
#225637=CARTESIAN_POINT('',(54.3576020372438,31.1634057161443,2.83404198860284));
#225638=CARTESIAN_POINT('',(53.6759427993286,30.7698495716383,3.64303198860285));
#225639=CARTESIAN_POINT('Origin',(53.7090519423386,30.7889651442678,3.20400259788415));
#225640=CARTESIAN_POINT('',(53.3283379195024,30.5691597998769,3.64303198860284));
#225641=CARTESIAN_POINT('',(0.0952500000000057,-0.164977839420752,3.64303198860263));
#225642=CARTESIAN_POINT('',(53.2191856060845,30.5061406831646,3.42473028058507));
#225643=CARTESIAN_POINT('',(53.3283379191464,30.5691598004935,3.64303198860284));
#225644=CARTESIAN_POINT('',(52.9334317578287,30.3411606219521,3.23423028058503));
#225645=CARTESIAN_POINT('Origin',(52.9589163924918,30.3558747754324,3.56425722716898));
#225646=CARTESIAN_POINT('',(52.8024816883959,30.2655565641147,3.23423028058503));
#225647=CARTESIAN_POINT('',(0.0952500000000058,-0.164977839420749,3.23423028058481));
#225648=CARTESIAN_POINT('',(52.5167277788841,30.100576467536,3.42473028058502));
#225649=CARTESIAN_POINT('Origin',(52.7769940214379,30.2508418455893,3.5642590974096));
#225650=CARTESIAN_POINT('',(52.4075754202456,30.0375573238934,3.64303198860284));
#225651=CARTESIAN_POINT('',(52.5167277788841,30.100576467536,3.42473028058502));
#225652=CARTESIAN_POINT('',(0.0952500000000057,-0.164977839420752,3.64303198860263));
#225653=CARTESIAN_POINT('Origin',(-0.0952500000000002,0.164977839420846,
42.7590319886026));
#225654=CARTESIAN_POINT('',(53.4854427993286,31.0998052504802,3.64303198860285));
#225655=CARTESIAN_POINT('',(53.8585387249978,31.3152122835989,3.40423097483333));
#225656=CARTESIAN_POINT('Origin',(53.5185519420887,31.1189208229654,3.20400259735773));
#225657=CARTESIAN_POINT('',(54.1671020370177,31.4933613953778,2.83404198860284));
#225658=CARTESIAN_POINT('',(53.8585387249979,31.3152122835989,3.40423097483333));
#225659=CARTESIAN_POINT('',(51.1878102687785,29.7732664904683,2.83404198860283));
#225660=CARTESIAN_POINT('',(-0.0952499999999994,0.164977839421122,2.83404198860262));
#225661=CARTESIAN_POINT('',(51.4963740058474,29.9514158463116,3.40423097483332));
#225662=CARTESIAN_POINT('',(51.1878102687785,29.7732664904682,2.83404198860283));
#225663=CARTESIAN_POINT('',(51.8694703131946,30.1668231006077,3.64303198860284));
#225664=CARTESIAN_POINT('Origin',(51.8363612765612,30.1477075893948,3.20400220587076));
#225665=CARTESIAN_POINT('',(52.2170754206163,30.3675130020933,3.64303198860284));
#225666=CARTESIAN_POINT('',(52.2810382154239,30.4044419397496,3.64303198860284));
#225667=CARTESIAN_POINT('',(52.3262277788841,30.4305321463779,3.42473028058504));
#225668=CARTESIAN_POINT('',(52.2170754202456,30.3675130027353,3.64303198860284));
#225669=CARTESIAN_POINT('',(52.6119816883959,30.5955122429565,3.23423028058503));
#225670=CARTESIAN_POINT('Origin',(52.5864971060028,30.580798119516,3.56425743004708));
#225671=CARTESIAN_POINT('',(52.7429317578287,30.671116300794,3.23423028058504));
#225672=CARTESIAN_POINT('',(52.7433896349617,30.67138065628,3.23423028058504));
#225673=CARTESIAN_POINT('',(53.0286856060845,30.8360963620065,3.42473028058505));
#225674=CARTESIAN_POINT('Origin',(52.768419360041,30.6858309820707,3.5642591291773));
#225675=CARTESIAN_POINT('',(53.1378379191464,30.8991154793354,3.64303198860285));
#225676=CARTESIAN_POINT('',(53.0286856060845,30.8360963620065,3.42473028058505));
#225677=CARTESIAN_POINT('',(53.4858943313413,31.1000659426093,3.64303198860285));
#225678=CARTESIAN_POINT('Origin',(47.2483549038575,34.0924682662297,2.65878198860287));
#225679=CARTESIAN_POINT('',(47.7461450747864,34.7084426211234,2.65878198860287));
#225680=CARTESIAN_POINT('',(50.8348823336486,36.9525415975215,2.65878198860288));
#225681=CARTESIAN_POINT('',(47.1274239660509,34.2589154226524,2.65878198860287));
#225682=CARTESIAN_POINT('',(50.8527980281384,36.9278827595329,2.65878198860288));
#225683=CARTESIAN_POINT('Origin',(5.52786294311959E-15,1.84909306033141E-13,
2.65878198860263));
#225684=CARTESIAN_POINT('',(47.7640607692763,34.6837837831348,2.65878198860287));
#225685=CARTESIAN_POINT('',(47.706860803705,34.6422255755468,2.65878198860287));
#225686=CARTESIAN_POINT('Origin',(5.70871613546578E-15,1.85482880258616E-13,
2.65878198860263));
#225687=CARTESIAN_POINT('Origin',(0.111973090561716,-0.154117737428517,
42.7590319886026));
#225688=CARTESIAN_POINT('',(48.6559784483765,35.1151666347443,3.64303198860288));
#225689=CARTESIAN_POINT('',(48.3074421904918,34.8619402208393,3.40423097483335));
#225690=CARTESIAN_POINT('Origin',(48.6250489017664,35.0926950037602,3.2040022053186));
#225691=CARTESIAN_POINT('',(48.0191904763612,34.65251309241,2.83404198860287));
#225692=CARTESIAN_POINT('',(48.3074421904918,34.8619402208393,3.40423097483335));
#225693=CARTESIAN_POINT('',(50.8023624960591,36.6746059268181,2.83404198860288));
#225694=CARTESIAN_POINT('',(51.0125340177515,36.8273044755032,2.83404198860288));
#225695=CARTESIAN_POINT('',(50.5141111791245,36.4651790855638,3.40423097483335));
#225696=CARTESIAN_POINT('',(50.8023624960591,36.6746059268181,2.83404198860288));
#225697=CARTESIAN_POINT('',(50.1655752777671,36.2119529314387,3.64303198860289));
#225698=CARTESIAN_POINT('Origin',(50.1965049239958,36.2344246348,3.2040025978838));
#225699=CARTESIAN_POINT('',(49.8408524072786,35.9760279553333,3.64303198860289));
#225700=CARTESIAN_POINT('',(0.111973090561722,-0.154117737428244,3.64303198860263));
#225701=CARTESIAN_POINT('',(49.7388853330811,35.9019445403521,3.42473028058511));
#225702=CARTESIAN_POINT('',(49.8408524068603,35.9760279559089,3.64303198860289));
#225703=CARTESIAN_POINT('',(49.4719419865733,35.7079988465461,3.23423028058507));
#225704=CARTESIAN_POINT('Origin',(49.4957489658887,35.7252962640517,3.56425722717078));
#225705=CARTESIAN_POINT('',(49.3496120513049,35.6191209461254,3.23423028058507));
#225706=CARTESIAN_POINT('',(0.111973090561722,-0.154117737428241,3.23423028058481));
#225707=CARTESIAN_POINT('',(49.0826686475734,35.425175210744,3.42473028058506));
#225708=CARTESIAN_POINT('Origin',(49.3258021153704,35.60182264971,3.56425909741427));
#225709=CARTESIAN_POINT('',(48.9807015312178,35.3510917642536,3.64303198860288));
#225710=CARTESIAN_POINT('',(49.0826686475734,35.425175210744,3.42473028058506));
#225711=CARTESIAN_POINT('',(0.111973090561722,-0.154117737428244,3.64303198860263));
#225712=CARTESIAN_POINT('Origin',(-0.111973090561716,0.154117737428338,
42.7590319886026));
#225713=CARTESIAN_POINT('',(49.9416290966437,36.5201884062956,3.64303198860289));
#225714=CARTESIAN_POINT('',(50.2901649976455,36.7734145609101,3.40423097483336));
#225715=CARTESIAN_POINT('Origin',(49.9725587426394,36.5426601094876,3.20400259735887));
#225716=CARTESIAN_POINT('',(50.5784163146694,36.9828414020413,2.83404198860288));
#225717=CARTESIAN_POINT('',(50.2901649976455,36.7734145609101,3.40423097483336));
#225718=CARTESIAN_POINT('',(47.7952442955502,34.9607485668368,2.83404198860286));
#225719=CARTESIAN_POINT('',(-0.111973090561715,0.154117737428614,2.83404198860262));
#225720=CARTESIAN_POINT('',(48.0834960097835,35.1701756951247,3.40423097483336));
#225721=CARTESIAN_POINT('',(47.7952442955502,34.9607485668368,2.83404198860287));
#225722=CARTESIAN_POINT('',(48.432032267253,35.4234021096012,3.64303198860288));
#225723=CARTESIAN_POINT('Origin',(48.4011027203975,35.4009304784387,3.20400220587243));
#225724=CARTESIAN_POINT('',(48.7567553505302,35.6593272385106,3.64303198860288));
#225725=CARTESIAN_POINT('',(48.8165076253519,35.7027398082301,3.64303198860288));
#225726=CARTESIAN_POINT('',(48.85872246645,35.7334106856009,3.42473028058506));
#225727=CARTESIAN_POINT('',(48.7567553500944,35.6593272391105,3.64303198860288));
#225728=CARTESIAN_POINT('',(49.1256658701815,35.9273564209823,3.23423028058507));
#225729=CARTESIAN_POINT('Origin',(49.1018589397087,35.9100590388148,3.56425743004647));
#225730=CARTESIAN_POINT('',(49.2479958054498,36.0162343214029,3.23423028058507));
#225731=CARTESIAN_POINT('',(49.2484235416113,36.0165450899149,3.23423028058507));
#225732=CARTESIAN_POINT('',(49.5149391519577,36.2101800152089,3.4247302805851));
#225733=CARTESIAN_POINT('Origin',(49.2718056808886,36.0335325740073,3.56425912917859));
#225734=CARTESIAN_POINT('',(49.6169062257369,36.2842634307658,3.64303198860289));
#225735=CARTESIAN_POINT('',(49.5149391519577,36.2101800152089,3.4247302805851));
#225736=CARTESIAN_POINT('',(49.9420509053691,36.5204948682733,3.64303198860289));
#225737=CARTESIAN_POINT('Origin',(43.425890155147,38.8445040879384,2.6587819886029));
#225738=CARTESIAN_POINT('',(43.8565665267056,39.5091373124625,2.6587819886029));
#225739=CARTESIAN_POINT('',(46.6938111422604,42.0638038389703,2.65878198860292));
#225740=CARTESIAN_POINT('',(43.2882232241948,38.9973987043321,2.6587819886029));
#225741=CARTESIAN_POINT('',(46.7142062431422,42.0411527846897,2.65878198860292));
#225742=CARTESIAN_POINT('Origin',(5.5375465370123E-15,1.84897347790577E-13,
2.65878198860263));
#225743=CARTESIAN_POINT('',(43.8769616275874,39.4864862581819,2.6587819886029));
#225744=CARTESIAN_POINT('',(43.8244190249878,39.4391766863033,2.6587819886029));
#225745=CARTESIAN_POINT('Origin',(5.70367421417806E-15,1.85489106512878E-13,
2.65878198860263));
#225746=CARTESIAN_POINT('Origin',(0.127469380511363,-0.141569089253533,
42.7590319886026));
#225747=CARTESIAN_POINT('',(44.7189015017598,40.0087367337516,3.64303198860291));
#225748=CARTESIAN_POINT('',(44.398743929868,39.7204655612076,3.40423097483339));
#225749=CARTESIAN_POINT('Origin',(44.6904903154964,39.9831551867367,3.20400220531785));
#225750=CARTESIAN_POINT('',(44.1339623846891,39.4820551877881,2.8340419886029));
#225751=CARTESIAN_POINT('',(44.398743929868,39.7204655612076,3.40423097483339));
#225752=CARTESIAN_POINT('',(46.6905216402897,41.7839914803029,2.83404198860292));
#225753=CARTESIAN_POINT('',(46.8835804757584,41.9578224365464,2.83404198860292));
#225754=CARTESIAN_POINT('',(46.4257404601128,41.5455814340038,3.40423097483339));
#225755=CARTESIAN_POINT('',(46.6905216402897,41.7839914803029,2.83404198860291));
#225756=CARTESIAN_POINT('',(46.1055832156409,41.2573105570839,3.64303198860293));
#225757=CARTESIAN_POINT('Origin',(46.133994493411,41.2828921864918,3.20400259788132));
#225758=CARTESIAN_POINT('',(45.8073000862124,40.9887352200424,3.64303198860291));
#225759=CARTESIAN_POINT('',(0.127469380511368,-0.14156908925326,3.64303198860262));
#225760=CARTESIAN_POINT('',(45.7136354238375,40.9043991801906,3.42473028058514));
#225761=CARTESIAN_POINT('',(45.8073000857358,40.9887352205716,3.64303198860291));
#225762=CARTESIAN_POINT('',(45.4684272662435,40.6836127633981,3.23423028058511));
#225763=CARTESIAN_POINT('Origin',(45.4902957559646,40.7033039308034,3.56425722717177));
#225764=CARTESIAN_POINT('',(45.3560577375095,40.5824347852702,3.2342302805851));
#225765=CARTESIAN_POINT('',(0.127469380511368,-0.141569089253257,3.23423028058481));
#225766=CARTESIAN_POINT('',(45.1108495273512,40.3616483211486,3.4247302805851));
#225767=CARTESIAN_POINT('Origin',(45.3341863992351,40.5627424347172,3.56425909741047));
#225768=CARTESIAN_POINT('',(45.0171848263432,40.277312245553,3.64303198860291));
#225769=CARTESIAN_POINT('',(45.1108495273512,40.3616483211486,3.4247302805851));
#225770=CARTESIAN_POINT('',(0.127469380511368,-0.14156908925326,3.64303198860262));
#225771=CARTESIAN_POINT('Origin',(-0.127469380511363,0.141569089253354,
42.7590319886026));
#225772=CARTESIAN_POINT('',(45.8506444546181,41.5404487355908,3.64303198860292));
#225773=CARTESIAN_POINT('',(46.1708016986853,41.8287196129602,3.40423097483339));
#225774=CARTESIAN_POINT('Origin',(45.879055732176,41.5660303648075,3.20400259736081));
#225775=CARTESIAN_POINT('',(46.4355828789643,42.0671296591459,2.83404198860292));
#225776=CARTESIAN_POINT('',(46.1708016986853,41.8287196129602,3.40423097483339));
#225777=CARTESIAN_POINT('',(43.8790236240219,39.7651933659001,2.8340419886029));
#225778=CARTESIAN_POINT('',(-0.127469380511361,0.141569089253629,2.83404198860262));
#225779=CARTESIAN_POINT('',(44.1438051693184,40.0036037391891,3.4042309748334));
#225780=CARTESIAN_POINT('',(43.8790236240219,39.7651933659001,2.8340419886029));
#225781=CARTESIAN_POINT('',(44.4639627407371,40.2918749122585,3.64303198860291));
#225782=CARTESIAN_POINT('Origin',(44.435551554248,40.2662933650404,3.20400220587245));
#225783=CARTESIAN_POINT('',(44.7622460658166,40.5604504235089,3.64303198860292));
#225784=CARTESIAN_POINT('',(44.8171331622256,40.6098709880931,3.64303198860292));
#225785=CARTESIAN_POINT('',(44.8559107663285,40.6447864996555,3.4247302805851));
#225786=CARTESIAN_POINT('',(44.7622460653205,40.5604504240599,3.64303198860292));
#225787=CARTESIAN_POINT('',(45.1011189764868,40.8655729637771,3.23423028058511));
#225788=CARTESIAN_POINT('Origin',(45.0792505316455,40.8458818366205,3.56425743004429));
#225789=CARTESIAN_POINT('',(45.2134885052208,40.966750941905,3.23423028058511));
#225790=CARTESIAN_POINT('',(45.2138814140438,40.9671047185983,3.23423028058511));
#225791=CARTESIAN_POINT('',(45.4586966628148,41.1875373586975,3.42473028058513));
#225792=CARTESIAN_POINT('Origin',(45.2353597879082,40.9864432425615,3.56425912917935));
#225793=CARTESIAN_POINT('',(45.5523613247131,41.2718733990785,3.64303198860292));
#225794=CARTESIAN_POINT('',(45.4586966628148,41.1875373586975,3.42473028058513));
#225795=CARTESIAN_POINT('',(45.8510319186316,41.5407976097556,3.64303198860292));
#225796=CARTESIAN_POINT('Origin',(39.127642266445,43.1709513941246,2.65878198860293));
#225797=CARTESIAN_POINT('',(39.4864862581816,43.8769616275877,2.65878198860293));
#225798=CARTESIAN_POINT('',(42.0411527846894,46.7142062431425,2.65878198860295));
#225799=CARTESIAN_POINT('',(38.9747476500513,43.3086183250769,2.65878198860293));
#225800=CARTESIAN_POINT('',(42.06380383897,46.6938111422607,2.65878198860295));
#225801=CARTESIAN_POINT('Origin',(5.54842705988296E-15,1.84886467267707E-13,
2.65878198860263));
#225802=CARTESIAN_POINT('',(39.5091373124621,43.8565665267059,2.65878198860293));
#225803=CARTESIAN_POINT('',(39.4618277405835,43.8040239241062,2.65878198860293));
#225804=CARTESIAN_POINT('Origin',(5.69800909227282E-15,1.85494771634783E-13,
2.65878198860263));
#225805=CARTESIAN_POINT('Origin',(0.141569089253444,-0.127469380511452,
42.7590319886026));
#225806=CARTESIAN_POINT('',(40.2918749122581,44.4639627407374,3.64303198860293));
#225807=CARTESIAN_POINT('',(40.0036037397142,44.1438051688456,3.40423097483342));
#225808=CARTESIAN_POINT('Origin',(40.2662933652436,44.4355515544743,3.20400220531713));
#225809=CARTESIAN_POINT('',(39.7651933655048,43.8790236243779,2.83404198860293));
#225810=CARTESIAN_POINT('',(40.0036037397142,44.1438051688456,3.40423097483342));
#225811=CARTESIAN_POINT('',(42.0671296588095,46.4355828792673,2.83404198860295));
#225812=CARTESIAN_POINT('',(42.240960615053,46.628641714736,2.83404198860295));
#225813=CARTESIAN_POINT('',(41.8287196134096,46.1708016982807,3.40423097483344));
#225814=CARTESIAN_POINT('',(42.0671296588095,46.4355828792673,2.83404198860294));
#225815=CARTESIAN_POINT('',(41.5404487355905,45.8506444546185,3.64303198860296));
#225816=CARTESIAN_POINT('Origin',(41.566030364998,45.8790557323883,3.20400259788057));
#225817=CARTESIAN_POINT('',(41.2718733996072,45.5523613242371,3.64303198860294));
#225818=CARTESIAN_POINT('',(0.141569089253449,-0.127469380511178,3.64303198860262));
#225819=CARTESIAN_POINT('',(41.1875373586971,45.4586966628151,3.42473028058517));
#225820=CARTESIAN_POINT('',(41.2718733990782,45.5523613247134,3.64303198860294));
#225821=CARTESIAN_POINT('',(40.9667509419047,45.2134885052211,3.23423028058514));
#225822=CARTESIAN_POINT('Origin',(40.9864413462824,45.2353576819759,3.56425722717126));
#225823=CARTESIAN_POINT('',(40.8655729637768,45.1011189764871,3.23423028058513));
#225824=CARTESIAN_POINT('',(0.141569089253449,-0.127469380511176,3.23423028058481));
#225825=CARTESIAN_POINT('',(40.6447864996552,44.8559107663288,3.42473028058512));
#225826=CARTESIAN_POINT('Origin',(40.8458798501231,45.0792483253113,3.56425909741017));
#225827=CARTESIAN_POINT('',(40.5604504240596,44.7622460653208,3.64303198860294));
#225828=CARTESIAN_POINT('',(40.6447864996552,44.8559107663288,3.42473028058512));
#225829=CARTESIAN_POINT('',(0.141569089253449,-0.127469380511178,3.64303198860262));
#225830=CARTESIAN_POINT('Origin',(-0.141569089253444,0.127469380511273,
42.7590319886026));
#225831=CARTESIAN_POINT('',(41.2573105570836,46.1055832156412,3.64303198860295));
#225832=CARTESIAN_POINT('',(41.5455814344529,46.4257404597084,3.40423097483342));
#225833=CARTESIAN_POINT('Origin',(41.2828921862997,46.1339944931982,3.20400259735886));
#225834=CARTESIAN_POINT('',(41.7839914799664,46.6905216405928,2.83404198860295));
#225835=CARTESIAN_POINT('',(41.5455814344529,46.4257404597084,3.40423097483342));
#225836=CARTESIAN_POINT('',(39.4820551873929,44.133962385045,2.83404198860293));
#225837=CARTESIAN_POINT('',(-0.141569089253442,0.127469380511548,2.83404198860262));
#225838=CARTESIAN_POINT('',(39.7204655617325,44.3987439293954,3.40423097483342));
#225839=CARTESIAN_POINT('',(39.4820551873929,44.133962385045,2.83404198860293));
#225840=CARTESIAN_POINT('',(40.0087367337512,44.7189015017601,3.64303198860294));
#225841=CARTESIAN_POINT('Origin',(39.9831551865319,44.6904903152697,3.2040022058757));
#225842=CARTESIAN_POINT('',(40.2773122461039,45.0171848258472,3.64303198860295));
#225843=CARTESIAN_POINT('',(40.3267328095859,45.0720719232486,3.64303198860295));
#225844=CARTESIAN_POINT('',(40.3616483211483,45.1108495273515,3.42473028058513));
#225845=CARTESIAN_POINT('',(40.2773122455527,45.0171848263435,3.64303198860295));
#225846=CARTESIAN_POINT('',(40.5824347852699,45.3560577375099,3.23423028058514));
#225847=CARTESIAN_POINT('Origin',(40.5627444213189,45.3341886054746,3.56425743004301));
#225848=CARTESIAN_POINT('',(40.6836127633978,45.4684272662438,3.23423028058514));
#225849=CARTESIAN_POINT('',(40.6839665400911,45.4688201750668,3.23423028058514));
#225850=CARTESIAN_POINT('',(40.9043991801903,45.7136354238378,3.42473028058516));
#225851=CARTESIAN_POINT('Origin',(40.7033058269857,45.4902978619874,3.56425912917592));
#225852=CARTESIAN_POINT('',(40.9887352205713,45.8073000857361,3.64303198860295));
#225853=CARTESIAN_POINT('',(40.9043991801903,45.7136354238378,3.42473028058516));
#225854=CARTESIAN_POINT('',(41.2576594312484,46.1059706796547,3.64303198860295));
#225855=CARTESIAN_POINT('Origin',(34.4007037410862,47.0244087227344,2.65878198860296));
#225856=CARTESIAN_POINT('',(34.6837837831345,47.7640607692766,2.65878198860296));
#225857=CARTESIAN_POINT('',(36.9278827595326,50.8527980281387,2.65878198860298));
#225858=CARTESIAN_POINT('',(34.2342565846635,47.1453396605411,2.65878198860296));
#225859=CARTESIAN_POINT('',(36.9525415975211,50.8348823336489,2.65878198860298));
#225860=CARTESIAN_POINT('Origin',(5.5603853024461E-15,1.84876783673814E-13,
2.65878198860263));
#225861=CARTESIAN_POINT('',(34.7084426211231,47.7461450747867,2.65878198860296));
#225862=CARTESIAN_POINT('',(34.6668844135351,47.6889451092154,2.65878198860296));
#225863=CARTESIAN_POINT('Origin',(5.69178283801114E-15,1.85499813556071E-13,
2.65878198860263));
#225864=CARTESIAN_POINT('Origin',(0.154117737428428,-0.111973090561805,
42.7590319886026));
#225865=CARTESIAN_POINT('',(35.4234021096009,48.4320322672533,3.64303198860296));
#225866=CARTESIAN_POINT('',(35.1701756956958,48.0834960093686,3.40423097483345));
#225867=CARTESIAN_POINT('Origin',(35.4009304786174,48.4011027206441,3.20400220531654));
#225868=CARTESIAN_POINT('',(34.9607485664065,47.7952442958629,2.83404198860295));
#225869=CARTESIAN_POINT('',(35.1701756956958,48.0834960093686,3.40423097483344));
#225870=CARTESIAN_POINT('',(36.9828414016746,50.578416314936,2.83404198860297));
#225871=CARTESIAN_POINT('',(37.1355399503597,50.7885878366283,2.83404198860297));
#225872=CARTESIAN_POINT('',(36.7734145613994,50.29016499729,3.40423097483345));
#225873=CARTESIAN_POINT('',(36.9828414016746,50.5784163149359,2.83404198860297));
#225874=CARTESIAN_POINT('',(36.5201884062952,49.941629096644,3.64303198860299));
#225875=CARTESIAN_POINT('Origin',(36.542660109656,49.9725587428719,3.2040025978818));
#225876=CARTESIAN_POINT('',(36.2842634313411,49.616906225319,3.64303198860297));
#225877=CARTESIAN_POINT('',(0.154117737428433,-0.111973090561532,3.64303198860262));
#225878=CARTESIAN_POINT('',(36.2101800152086,49.514939151958,3.42473028058521));
#225879=CARTESIAN_POINT('',(36.2842634307655,49.6169062257372,3.64303198860297));
#225880=CARTESIAN_POINT('',(36.0162343214026,49.2479958054501,3.23423028058516));
#225881=CARTESIAN_POINT('Origin',(36.0335309082456,49.2718033882769,3.56425722717131));
#225882=CARTESIAN_POINT('',(35.927356420982,49.1256658701818,3.23423028058516));
#225883=CARTESIAN_POINT('',(0.154117737428433,-0.111973090561529,3.23423028058481));
#225884=CARTESIAN_POINT('',(35.7334106856005,48.8587224664503,3.42473028058515));
#225885=CARTESIAN_POINT('Origin',(35.9100572938233,49.1018565378139,3.5642590974097));
#225886=CARTESIAN_POINT('',(35.6593272391101,48.7567553500947,3.64303198860296));
#225887=CARTESIAN_POINT('',(35.7334106856005,48.8587224664503,3.42473028058515));
#225888=CARTESIAN_POINT('',(0.154117737428433,-0.111973090561532,3.64303198860262));
#225889=CARTESIAN_POINT('Origin',(-0.154117737428428,0.111973090561626,
42.7590319886026));
#225890=CARTESIAN_POINT('',(36.2119529314384,50.1655752777674,3.64303198860298));
#225891=CARTESIAN_POINT('',(36.4651790860528,50.5141111787692,3.40423097483345));
#225892=CARTESIAN_POINT('Origin',(36.2344246346307,50.1965049237635,3.2040025973597));
#225893=CARTESIAN_POINT('',(36.6746059264518,50.8023624963252,2.83404198860297));
#225894=CARTESIAN_POINT('',(36.4651790860528,50.5141111787692,3.40423097483345));
#225895=CARTESIAN_POINT('',(34.6525130919796,48.0191904766739,2.83404198860296));
#225896=CARTESIAN_POINT('',(-0.154117737428425,0.111973090561901,2.83404198860262));
#225897=CARTESIAN_POINT('',(34.8619402214104,48.3074421900769,3.40423097483345));
#225898=CARTESIAN_POINT('',(34.6525130919796,48.0191904766739,2.83404198860296));
#225899=CARTESIAN_POINT('',(35.115166634744,48.6559784483767,3.64303198860297));
#225900=CARTESIAN_POINT('Origin',(35.0926950035816,48.6250489015213,3.2040022058722));
#225901=CARTESIAN_POINT('',(35.3510917648536,48.9807015307819,3.64303198860298));
#225902=CARTESIAN_POINT('',(35.3945043333729,49.0404538064756,3.64303198860298));
#225903=CARTESIAN_POINT('',(35.4251752107437,49.0826686475737,3.42473028058515));
#225904=CARTESIAN_POINT('',(35.3510917642532,48.9807015312181,3.64303198860298));
#225905=CARTESIAN_POINT('',(35.6191209461251,49.3496120513052,3.23423028058516));
#225906=CARTESIAN_POINT('Origin',(35.6018243948128,49.3258045171784,3.56425743004293));
#225907=CARTESIAN_POINT('',(35.7079988465457,49.4719419865736,3.23423028058516));
#225908=CARTESIAN_POINT('',(35.7083096150578,49.472369722735,3.23423028058516));
#225909=CARTESIAN_POINT('',(35.9019445403517,49.7388853330814,3.42473028058518));
#225910=CARTESIAN_POINT('Origin',(35.7252979297061,49.4957512585779,3.56425912917861));
#225911=CARTESIAN_POINT('',(35.9760279559086,49.8408524068606,3.64303198860298));
#225912=CARTESIAN_POINT('',(35.9019445403517,49.7388853330814,3.42473028058518));
#225913=CARTESIAN_POINT('',(36.2122593934161,50.1659970864928,3.64303198860298));
#225914=CARTESIAN_POINT('Origin',(29.2968639067301,50.3626567888878,2.65878198860297));
#225915=CARTESIAN_POINT('',(29.501078514911,51.1278468659049,2.65878198860298));
#225916=CARTESIAN_POINT('',(31.410023123206,54.4342359163065,2.658781988603));
#225917=CARTESIAN_POINT('',(29.1186878401555,50.4655267888878,2.65878198860297));
#225918=CARTESIAN_POINT('',(31.4364195775134,54.4189959163065,2.658781988603));
#225919=CARTESIAN_POINT('Origin',(5.57329024769379E-15,1.8486840310438E-13,
2.65878198860263));
#225920=CARTESIAN_POINT('',(29.5274749692184,51.1126068659049,2.65878198860298));
#225921=CARTESIAN_POINT('',(29.49212344634,51.0513762321546,2.65878198860298));
#225922=CARTESIAN_POINT('Origin',(5.68506366753766E-15,1.85504177036396E-13,
2.65878198860263));
#225923=CARTESIAN_POINT('Origin',(0.164977839420936,-0.0952500000000889,
42.7590319886026));
#225924=CARTESIAN_POINT('',(30.1668231006074,51.8694703131949,3.64303198860299));
#225925=CARTESIAN_POINT('',(29.9514158469229,51.4963740054945,3.40423097483346));
#225926=CARTESIAN_POINT('Origin',(30.1477075895462,51.8363612768243,3.20400220531662));
#225927=CARTESIAN_POINT('',(29.7732664900075,51.1878102690446,2.83404198860297));
#225928=CARTESIAN_POINT('',(29.9514158469229,51.4963740054945,3.40423097483346));
#225929=CARTESIAN_POINT('',(31.4933613949858,54.1671020372441,2.834041988603));
#225930=CARTESIAN_POINT('',(31.623254538859,54.3920835619873,2.83404198860299));
#225931=CARTESIAN_POINT('',(31.3152122841225,53.8585387246956,3.40423097483348));
#225932=CARTESIAN_POINT('',(31.4933613949858,54.1671020372441,2.83404198860299));
#225933=CARTESIAN_POINT('',(31.0998052504799,53.4854427993289,3.64303198860301));
#225934=CARTESIAN_POINT('Origin',(31.1189208231087,53.5185519423378,3.2040025978818));
#225935=CARTESIAN_POINT('',(30.8991154799516,53.1378379187907,3.643031988603));
#225936=CARTESIAN_POINT('',(0.164977839420941,-0.0952499999998158,3.64303198860262));
#225937=CARTESIAN_POINT('',(30.8360963620061,53.0286856060848,3.42473028058523));
#225938=CARTESIAN_POINT('',(30.899115479335,53.1378379191467,3.643031988603));
#225939=CARTESIAN_POINT('',(30.6711163007936,52.742931757829,3.23423028058519));
#225940=CARTESIAN_POINT('Origin',(30.6858295650771,52.7684169058685,3.56425722717158));
#225941=CARTESIAN_POINT('',(30.5955122429562,52.6119816883962,3.23423028058518));
#225942=CARTESIAN_POINT('',(0.164977839420941,-0.095249999999813,3.23423028058481));
#225943=CARTESIAN_POINT('',(30.4305321463776,52.3262277788844,3.42473028058517));
#225944=CARTESIAN_POINT('Origin',(30.5807966351508,52.586494534866,3.56425909741312));
#225945=CARTESIAN_POINT('',(30.367513002735,52.2170754202459,3.64303198860299));
#225946=CARTESIAN_POINT('',(30.4305321463776,52.3262277788844,3.42473028058517));
#225947=CARTESIAN_POINT('',(0.164977839420941,-0.0952499999998158,3.64303198860262));
#225948=CARTESIAN_POINT('Origin',(-0.164977839420936,0.0952499999999103,
42.7590319886026));
#225949=CARTESIAN_POINT('',(30.769849571638,53.6759427993289,3.64303198860301));
#225950=CARTESIAN_POINT('',(30.9852566047567,54.0490387249981,3.40423097483348));
#225951=CARTESIAN_POINT('Origin',(30.7889651441231,53.709051942089,3.20400259735764));
#225952=CARTESIAN_POINT('',(31.1634057157522,54.3576020374702,2.83404198860299));
#225953=CARTESIAN_POINT('',(30.9852566047567,54.0490387249981,3.40423097483348));
#225954=CARTESIAN_POINT('',(29.443310811626,51.3783102687787,2.83404198860297));
#225955=CARTESIAN_POINT('',(-0.164977839420933,0.0952500000001842,2.83404198860262));
#225956=CARTESIAN_POINT('',(29.6214601686927,51.6868740051414,3.40423097483347));
#225957=CARTESIAN_POINT('',(29.443310811626,51.3783102687787,2.83404198860297));
#225958=CARTESIAN_POINT('',(29.8368674217655,52.0599703131949,3.643031988603));
#225959=CARTESIAN_POINT('Origin',(29.8177519105523,52.026861276561,3.20400220587187));
#225960=CARTESIAN_POINT('',(30.0375573245353,52.4075754198751,3.643031988603));
#225961=CARTESIAN_POINT('',(30.0744862609074,52.4715382154242,3.643031988603));
#225962=CARTESIAN_POINT('',(30.1005764675357,52.5167277788844,3.42473028058518));
#225963=CARTESIAN_POINT('',(30.0375573238931,52.4075754202459,3.643031988603));
#225964=CARTESIAN_POINT('',(30.2655565641143,52.8024816883962,3.23423028058519));
#225965=CARTESIAN_POINT('Origin',(30.2508433300764,52.776996592504,3.56425743004371));
#225966=CARTESIAN_POINT('',(30.3411606219517,52.933431757829,3.23423028058519));
#225967=CARTESIAN_POINT('',(30.3414249774377,52.933889634962,3.23423028058519));
#225968=CARTESIAN_POINT('',(30.5061406831642,53.2191856060848,3.42473028058522));
#225969=CARTESIAN_POINT('Origin',(30.355876192312,52.9589188467315,3.56425912917328));
#225970=CARTESIAN_POINT('',(30.5691598004931,53.3283379191467,3.643031988603));
#225971=CARTESIAN_POINT('',(30.5061406831642,53.2191856060848,3.42473028058522));
#225972=CARTESIAN_POINT('',(30.770110263767,53.6763943313416,3.64303198860301));
#225973=CARTESIAN_POINT('Origin',(23.8720415006489,53.1491210481986,2.65878198860299));
#225974=CARTESIAN_POINT('',(23.9951532569806,53.9314655730807,2.658781988603));
#225975=CARTESIAN_POINT('',(25.5480287005717,57.4192809246791,2.65878198860302));
#225976=CARTESIAN_POINT('',(23.6840886581935,53.232803045145,2.65878198860299));
#225977=CARTESIAN_POINT('',(25.5758735661207,57.4068835917982,2.65878198860302));
#225978=CARTESIAN_POINT('Origin',(5.58700050634535E-15,1.84861417378678E-13,
2.65878198860263));
#225979=CARTESIAN_POINT('',(24.0229981225296,53.9190682401997,2.658781988603));
#225980=CARTESIAN_POINT('',(23.9942406030432,53.8544777939071,2.658781988603));
#225981=CARTESIAN_POINT('Origin',(5.67792519749014E-15,1.85507814268556E-13,
2.65878198860263));
#225982=CARTESIAN_POINT('Origin',(0.174030409680916,-0.0774833305060288,
42.7590319886026));
#225983=CARTESIAN_POINT('',(24.57973006491,54.7386155880006,3.64303198860301));
#225984=CARTESIAN_POINT('',(24.4045020183944,54.3450469517072,3.40423097483348));
#225985=CARTESIAN_POINT('Origin',(24.5641801073106,54.7036898113997,3.20400220531693));
#225986=CARTESIAN_POINT('',(24.259582275487,54.0195518811808,2.834041988603));
#225987=CARTESIAN_POINT('',(24.4045020183944,54.3450469517072,3.40423097483348));
#225988=CARTESIAN_POINT('',(25.658833530444,57.1623216544373,2.83404198860302));
#225989=CARTESIAN_POINT('',(25.764498133039,57.3996482375659,2.83404198860302));
#225990=CARTESIAN_POINT('',(25.5139139879315,56.8368270312095,3.4042309748335));
#225991=CARTESIAN_POINT('',(25.658833530444,57.1623216544373,2.83404198860302));
#225992=CARTESIAN_POINT('',(25.3386861202876,56.4432587981559,3.64303198860302));
#225993=CARTESIAN_POINT('Origin',(25.3542361279708,56.478184687247,3.20400259788312));
#225994=CARTESIAN_POINT('',(25.1754303533072,56.0765803402172,3.64303198860302));
#225995=CARTESIAN_POINT('',(0.174030409680921,-0.0774833305057557,3.64303198860262));
#225996=CARTESIAN_POINT('',(25.1241659841934,55.9614386837455,3.42473028058525));
#225997=CARTESIAN_POINT('',(25.1754303526574,56.0765803405065,3.64303198860302));
#225998=CARTESIAN_POINT('',(24.9899591116494,55.660005112701,3.2342302805852));
#225999=CARTESIAN_POINT('Origin',(25.0019278517708,55.6868886053377,3.56425722717229));
#226000=CARTESIAN_POINT('',(24.928457230274,55.5218696254675,3.2342302805852));
#226001=CARTESIAN_POINT('',(0.174030409680921,-0.0774833305057528,3.23423028058481));
#226002=CARTESIAN_POINT('',(24.7942503289606,55.2204359898058,3.4247302805852));
#226003=CARTESIAN_POINT('Origin',(24.9164863691,55.4949838933624,3.564259097415));
#226004=CARTESIAN_POINT('',(24.7429859390912,55.1052942849674,3.64303198860301));
#226005=CARTESIAN_POINT('',(24.7942503289606,55.2204359898058,3.4247302805852));
#226006=CARTESIAN_POINT('',(0.174030409680921,-0.0774833305057557,3.64303198860263));
#226007=CARTESIAN_POINT('Origin',(-0.174030409680916,0.0774833305058502,
42.7590319886026));
#226008=CARTESIAN_POINT('',(24.9906253009257,56.5982254591678,3.64303198860303));
#226009=CARTESIAN_POINT('',(25.165853168017,56.9917936924675,3.4042309748335));
#226010=CARTESIAN_POINT('Origin',(25.0061753084924,56.633151347997,3.20400259736051));
#226011=CARTESIAN_POINT('',(25.3107727106687,57.3172883156333,2.83404198860302));
#226012=CARTESIAN_POINT('',(25.165853168017,56.9917936924675,3.4042309748335));
#226013=CARTESIAN_POINT('',(23.9115214566113,54.1745185419762,2.834041988603));
#226014=CARTESIAN_POINT('',(-0.174030409680912,0.0774833305061238,2.83404198860263));
#226015=CARTESIAN_POINT('',(24.0564411996779,54.5000136124318,3.40423097483349));
#226016=CARTESIAN_POINT('',(23.9115214566113,54.1745185419762,2.834041988603));
#226017=CARTESIAN_POINT('',(24.2316692455482,54.8935822490125,3.64303198860301));
#226018=CARTESIAN_POINT('Origin',(24.216119287825,54.8586564721335,3.20400220587276));
#226019=CARTESIAN_POINT('',(24.3949251204068,55.2602609456777,3.64303198860301));
#226020=CARTESIAN_POINT('',(24.4249658234765,55.3277334713092,3.64303198860301));
#226021=CARTESIAN_POINT('',(24.4461895095988,55.3754026508177,3.42473028058519));
#226022=CARTESIAN_POINT('',(24.3949251197294,55.2602609459793,3.64303198860301));
#226023=CARTESIAN_POINT('',(24.5803964109122,55.6768362864794,3.2342302805852));
#226024=CARTESIAN_POINT('Origin',(24.5684276954198,55.6499528488657,3.56425743004438));
#226025=CARTESIAN_POINT('',(24.6418982922876,55.8149717737129,3.23423028058521));
#226026=CARTESIAN_POINT('',(24.6421133384135,55.8154547752197,3.23423028058521));
#226027=CARTESIAN_POINT('',(24.7761051648316,56.1164053447574,3.42473028058522));
#226028=CARTESIAN_POINT('Origin',(24.6538691229768,55.8418574376299,3.56425912917584));
#226029=CARTESIAN_POINT('',(24.8273695332956,56.2315470015184,3.64303198860302));
#226030=CARTESIAN_POINT('',(24.7761051648316,56.1164053447574,3.42473028058522));
#226031=CARTESIAN_POINT('',(24.9908373670086,56.5987017673885,3.64303198860303));
#226032=CARTESIAN_POINT('Origin',(18.1856720123407,55.3532724151367,2.658781988603));
#226033=CARTESIAN_POINT('',(18.2263320786581,56.144199857553,2.65878198860301));
#226034=CARTESIAN_POINT('',(19.4061247292252,59.7752282754839,2.65878198860304));
#226035=CARTESIAN_POINT('',(17.9900016446781,55.4168495715594,2.658781988603));
#226036=CARTESIAN_POINT('',(19.4351129318419,59.7658094374954,2.65878198860304));
#226037=CARTESIAN_POINT('Origin',(5.60136586593794E-15,1.8485590303378E-13,
2.65878198860263));
#226038=CARTESIAN_POINT('',(18.2553202812748,56.1347810195644,2.65878198860301));
#226039=CARTESIAN_POINT('',(18.2334718385819,56.0675384271755,2.65878198860301));
#226040=CARTESIAN_POINT('Origin',(5.67044563844026E-15,1.85510685402273E-13,
2.65878198860263));
#226041=CARTESIAN_POINT('Origin',(0.181176266354227,-0.0588677374285163,
42.7590319886026));
#226042=CARTESIAN_POINT('',(18.7233363629823,57.0080331356325,3.64303198860302));
#226043=CARTESIAN_POINT('',(18.5902073587821,56.5983041910848,3.4042309748335));
#226044=CARTESIAN_POINT('Origin',(18.7115223274336,56.9716732729167,3.2040022053203));
#226045=CARTESIAN_POINT('',(18.4801050009137,56.2594439785883,2.83404198860301));
#226046=CARTESIAN_POINT('',(18.5902073587821,56.5983041910848,3.4042309748335));
#226047=CARTESIAN_POINT('',(19.5431821162865,59.5312589135998,2.83404198860303));
#226048=CARTESIAN_POINT('',(19.6234604941057,59.7783303554051,2.83404198860303));
#226049=CARTESIAN_POINT('',(19.4330799109591,59.1923991668988,3.40423097483352));
#226050=CARTESIAN_POINT('',(19.5431821162865,59.5312589135998,2.83404198860303));
#226051=CARTESIAN_POINT('',(19.2999510425005,58.7826706420791,3.64303198860304));
#226052=CARTESIAN_POINT('Origin',(19.3117651160994,58.8190306219014,3.20400259788138));
#226053=CARTESIAN_POINT('',(19.1759179434157,58.4009360126569,3.64303198860303));
#226054=CARTESIAN_POINT('',(0.181176266354232,-0.0588677374282432,3.64303198860263));
#226055=CARTESIAN_POINT('',(19.1369699862882,58.2810665285032,3.42473028058526));
#226056=CARTESIAN_POINT('',(19.1759179427385,58.4009360128769,3.64303198860303));
#226057=CARTESIAN_POINT('',(19.0350067009929,57.9672558039534,3.23423028058522));
#226058=CARTESIAN_POINT('Origin',(19.0440997849306,57.9952431000156,3.56425722717456));
#226059=CARTESIAN_POINT('',(18.9882808235619,57.8234483402241,3.23423028058522));
#226060=CARTESIAN_POINT('',(0.181176266354233,-0.0588677374282403,3.23423028058481));
#226061=CARTESIAN_POINT('',(18.8863175164091,57.5096375484039,3.42473028058521));
#226062=CARTESIAN_POINT('Origin',(18.9791858642781,57.7954585952479,3.56425909741103));
#226063=CARTESIAN_POINT('',(18.8473695436961,57.3897680139786,3.64303198860302));
#226064=CARTESIAN_POINT('',(18.8863175164091,57.5096375484039,3.42473028058521));
#226065=CARTESIAN_POINT('',(0.181176266354232,-0.0588677374282432,3.64303198860263));
#226066=CARTESIAN_POINT('Origin',(-0.181176266354227,0.0588677374283377,
42.7590319886026));
#226067=CARTESIAN_POINT('',(18.937598509792,58.9004061169359,3.64303198860304));
#226068=CARTESIAN_POINT('',(19.0707273776751,59.3101346419426,3.40423097483351));
#226069=CARTESIAN_POINT('Origin',(18.9494125833028,58.9367660964869,3.20400259736099));
#226070=CARTESIAN_POINT('',(19.1808295831469,59.6489943885967,2.83404198860303));
#226071=CARTESIAN_POINT('',(19.0707273776751,59.3101346419426,3.40423097483351));
#226072=CARTESIAN_POINT('',(18.1177524687105,56.377179453281,2.83404198860301));
#226073=CARTESIAN_POINT('',(-0.181176266354223,0.0588677374286111,2.83404198860262));
#226074=CARTESIAN_POINT('',(18.2278548267456,56.7160396657233,3.4042309748335));
#226075=CARTESIAN_POINT('',(18.1177524687105,56.377179453281,2.83404198860301));
#226076=CARTESIAN_POINT('',(18.3609838302739,57.1257686104893,3.64303198860302));
#226077=CARTESIAN_POINT('Origin',(18.3491697946318,57.0894087474861,3.20400220587187));
#226078=CARTESIAN_POINT('',(18.4850170116929,57.5075034886063,3.64303198860303));
#226079=CARTESIAN_POINT('',(18.5078403492309,57.5777465012101,3.64303198860303));
#226080=CARTESIAN_POINT('',(18.5239649837007,57.6273730232608,3.42473028058521));
#226081=CARTESIAN_POINT('',(18.4850170109876,57.5075034888355,3.64303198860303));
#226082=CARTESIAN_POINT('',(18.6259282908535,57.941183815081,3.23423028058522));
#226083=CARTESIAN_POINT('Origin',(18.6168352256576,57.9131965763127,3.56425743004216));
#226084=CARTESIAN_POINT('',(18.6726541682844,58.0849912788103,3.23423028058522));
#226085=CARTESIAN_POINT('',(18.6728175489599,58.0854941128254,3.23423028058522));
#226086=CARTESIAN_POINT('',(18.7746174535798,58.3988020033601,3.42473028058524));
#226087=CARTESIAN_POINT('Origin',(18.6817491043768,58.1129809527812,3.56425912918029));
#226088=CARTESIAN_POINT('',(18.8135654100301,58.5186714877338,3.64303198860303));
#226089=CARTESIAN_POINT('',(18.7746174535798,58.3988020033601,3.42473028058524));
#226090=CARTESIAN_POINT('',(18.9377596263884,58.9009019828321,3.64303198860304));
#226091=CARTESIAN_POINT('Origin',(12.3000564958688,56.9509617460777,2.65878198860302));
#226092=CARTESIAN_POINT('',(12.2578193919766,57.7418065394568,2.65878198860302));
#226093=CARTESIAN_POINT('',(13.0516031943527,61.4762657165318,2.65878198860305));
#226094=CARTESIAN_POINT('',(12.0988124084938,56.9937374973465,2.65878198860302));
#226095=CARTESIAN_POINT('',(13.0814171332231,61.4699285681957,2.65878198860305));
#226096=CARTESIAN_POINT('Origin',(5.61622893658571E-15,1.84851920486003E-13,
2.65878198860263));
#226097=CARTESIAN_POINT('',(12.2876333308469,57.7354693911207,2.65878198860302));
#226098=CARTESIAN_POINT('',(12.2729333410577,57.6663113765491,2.65878198860302));
#226099=CARTESIAN_POINT('Origin',(5.66270693800216E-15,1.85512758980806E-13,
2.65878198860263));
#226100=CARTESIAN_POINT('Origin',(0.18633711793979,-0.0396071771008719,
42.7590319886026));
#226101=CARTESIAN_POINT('',(12.6618058697518,58.6528587425324,3.64303198860303));
#226102=CARTESIAN_POINT('',(12.5722344970959,58.2314585657882,3.40423097483351));
#226103=CARTESIAN_POINT('Origin',(12.6538571933006,58.6154631599698,3.20400220531712));
#226104=CARTESIAN_POINT('',(12.4981558287383,57.8829458347213,2.83404198860302));
#226105=CARTESIAN_POINT('',(12.5722344970959,58.2314585657882,3.40423097483351));
#226106=CARTESIAN_POINT('',(13.2134115091892,61.247959242388,2.83404198860304));
#226107=CARTESIAN_POINT('',(13.2674241155258,61.5020685764507,2.83404198860305));
#226108=CARTESIAN_POINT('',(13.1393329438492,60.8994469905095,3.40423097483353));
#226109=CARTESIAN_POINT('',(13.2134115091892,61.247959242388,2.83404198860304));
#226110=CARTESIAN_POINT('',(13.0497616623173,60.478047245383,3.64303198860306));
#226111=CARTESIAN_POINT('Origin',(13.0577103643695,60.515442948389,3.20400259788024));
#226112=CARTESIAN_POINT('',(12.9663101637165,60.0854388089607,3.64303198860304));
#226113=CARTESIAN_POINT('',(0.186337117939796,-0.0396071771005988,3.64303198860263));
#226114=CARTESIAN_POINT('',(12.9401053405448,59.9621548122774,3.42473028058526));
#226115=CARTESIAN_POINT('',(12.9663101630202,60.0854388091087,3.64303198860304));
#226116=CARTESIAN_POINT('',(12.871502773589,59.6394051101896,3.23423028058523));
#226117=CARTESIAN_POINT('Origin',(12.8776205756132,59.6681895750061,3.56425722717471));
#226118=CARTESIAN_POINT('',(12.8400648385937,59.4915012546307,3.23423028058523));
#226119=CARTESIAN_POINT('',(0.186337117939796,-0.0396071771005959,3.23423028058481));
#226120=CARTESIAN_POINT('',(12.7714622569318,59.1687514833563,3.42473028058522));
#226121=CARTESIAN_POINT('Origin',(12.8339454274779,59.4627141582879,3.56425909740963));
#226122=CARTESIAN_POINT('',(12.7452574235146,59.0454674350477,3.64303198860304));
#226123=CARTESIAN_POINT('',(12.7714622569318,59.1687514833563,3.42473028058522));
#226124=CARTESIAN_POINT('',(0.186337117939796,-0.0396071771005988,3.64303198860263));
#226125=CARTESIAN_POINT('Origin',(-0.18633711793979,0.0396071771006933,
42.7590319886026));
#226126=CARTESIAN_POINT('',(12.6770874264377,60.5572615995845,3.64303198860305));
#226127=CARTESIAN_POINT('',(12.7666587073772,60.978661344837,3.40423097483353));
#226128=CARTESIAN_POINT('Origin',(12.6850361284308,60.5946573023123,3.20400259736161));
#226129=CARTESIAN_POINT('',(12.8407372728672,61.3271735966836,2.83404198860304));
#226130=CARTESIAN_POINT('',(12.7666587073772,60.978661344837,3.40423097483353));
#226131=CARTESIAN_POINT('',(12.125481593379,57.9621601888123,2.83404198860302));
#226132=CARTESIAN_POINT('',(-0.186337117939786,0.0396071771009666,2.83404198860262));
#226133=CARTESIAN_POINT('',(12.1995602619078,58.3106729198428,3.40423097483351));
#226134=CARTESIAN_POINT('',(12.125481593379,57.9621601888123,2.83404198860302));
#226135=CARTESIAN_POINT('',(12.2891316338722,58.732073096734,3.64303198860303));
#226136=CARTESIAN_POINT('Origin',(12.2811829573577,58.6946775138734,3.20400220587296));
#226137=CARTESIAN_POINT('',(12.3725831883598,59.1246817890952,3.64303198860304));
#226138=CARTESIAN_POINT('',(12.3879391031045,59.1969256915256,3.64303198860304));
#226139=CARTESIAN_POINT('',(12.3987880210522,59.2479658375578,3.42473028058521));
#226140=CARTESIAN_POINT('',(12.372583187635,59.1246817892492,3.64303198860304));
#226141=CARTESIAN_POINT('',(12.4673906027141,59.5707156088323,3.23423028058523));
#226142=CARTESIAN_POINT('Origin',(12.461272813341,59.5419312029578,3.56425743004745));
#226143=CARTESIAN_POINT('',(12.4988285377094,59.7186194643911,3.23423028058523));
#226144=CARTESIAN_POINT('',(12.4989384629016,59.7191366217598,3.23423028058523));
#226145=CARTESIAN_POINT('',(12.5674311046652,60.0413691664789,3.42473028058526));
#226146=CARTESIAN_POINT('Origin',(12.504947933183,59.7474064876941,3.56425912917753));
#226147=CARTESIAN_POINT('',(12.5936359271406,60.1646531633103,3.64303198860304));
#226148=CARTESIAN_POINT('',(12.5674311046652,60.0413691664789,3.42473028058526));
#226149=CARTESIAN_POINT('',(12.6771958283204,60.5577715903457,3.64303198860305));
#226150=CARTESIAN_POINT('Origin',(6.27967898647588,57.9246844223737,2.65878198860302));
#226151=CARTESIAN_POINT('',(6.15500747092297,58.7067819056645,2.65878198860303));
#226152=CARTESIAN_POINT('',(6.55408556365926,62.5037563256537,2.65878198860306));
#226153=CARTESIAN_POINT('',(6.07506605172282,57.9461901084064,2.65878198860302));
#226154=CARTESIAN_POINT('',(6.58439859103008,62.5005702980933,2.65878198860306));
#226155=CARTESIAN_POINT('Origin',(5.63142687537637E-15,1.84849513368974E-13,
2.65878198860263));
#226156=CARTESIAN_POINT('',(6.1853204982938,58.7035958781041,2.65878198860303));
#226157=CARTESIAN_POINT('',(6.1779300175725,58.6332801510297,2.65878198860303));
#226158=CARTESIAN_POINT('Origin',(5.65479388299727E-15,1.85514012285594E-13,
2.65878198860263));
#226159=CARTESIAN_POINT('Origin',(0.189456421067656,-0.0199126722525767,
42.7590319886026));
#226160=CARTESIAN_POINT('',(6.46154998175899,59.6550713551495,3.64303198860304));
#226161=CARTESIAN_POINT('',(6.41651760335031,59.2266168947288,3.40423097483351));
#226162=CARTESIAN_POINT('Origin',(6.45755375176729,59.6170497665656,3.20400220531847));
#226163=CARTESIAN_POINT('',(6.37927424589664,58.8722700235038,2.83404198860304));
#226164=CARTESIAN_POINT('',(6.41651760335031,59.2266168947288,3.40423097483351));
#226165=CARTESIAN_POINT('',(6.73887200051313,62.2936141127571,2.83404198860306));
#226166=CARTESIAN_POINT('',(6.76602706194927,62.5519772640374,2.83404198860306));
#226167=CARTESIAN_POINT('',(6.70162869542398,61.9392677288638,3.40423097483354));
#226168=CARTESIAN_POINT('',(6.73887200051313,62.2936141127571,2.83404198860306));
#226169=CARTESIAN_POINT('',(6.65659636252364,61.5108137072214,3.64303198860306));
#226170=CARTESIAN_POINT('Origin',(6.66059260538633,61.5488354182647,3.20400259788118));
#226171=CARTESIAN_POINT('',(6.61464077648901,61.111632963987,3.64303198860305));
#226172=CARTESIAN_POINT('',(0.189456421067662,-0.0199126722523036,3.64303198860263));
#226173=CARTESIAN_POINT('',(6.60146619279927,60.9862851800406,3.42473028058528));
#226174=CARTESIAN_POINT('',(6.61464077578103,61.1116329640614,3.64303198860305));
#226175=CARTESIAN_POINT('',(6.56697596826259,60.6581326136906,3.23423028058524));
#226176=CARTESIAN_POINT('Origin',(6.57005146045409,60.6873988786433,3.5642572271707));
#226177=CARTESIAN_POINT('',(6.55117041629749,60.5077528318946,3.23423028058524));
#226178=CARTESIAN_POINT('',(0.189456421067662,-0.0199126722523007,3.23423028058481));
#226179=CARTESIAN_POINT('',(6.51668018436727,60.1796001951997,3.42473028058523));
#226180=CARTESIAN_POINT('Origin',(6.54809359889897,60.4784837816403,3.56425909741505));
#226181=CARTESIAN_POINT('',(6.50350559588446,60.0542523588399,3.64303198860304));
#226182=CARTESIAN_POINT('',(6.51668018436727,60.1796001951997,3.42473028058523));
#226183=CARTESIAN_POINT('',(0.189456421067662,-0.0199126722523036,3.64303198860263));
#226184=CARTESIAN_POINT('Origin',(-0.189456421067656,0.0199126722523981,
42.7590319886026));
#226185=CARTESIAN_POINT('',(6.27768352038833,61.5506390517264,3.64303198860306));
#226186=CARTESIAN_POINT('',(6.32271585268621,61.9790930734321,3.40423097483353));
#226187=CARTESIAN_POINT('Origin',(6.28167976322103,61.5886607624844,3.20400259735781));
#226188=CARTESIAN_POINT('',(6.35995915792791,62.3334394573094,2.83404198860306));
#226189=CARTESIAN_POINT('',(6.32271585268621,61.9790930734321,3.40423097483353));
#226190=CARTESIAN_POINT('',(6.00036140429027,58.9120953679532,2.83404198860304));
#226191=CARTESIAN_POINT('',(-0.189456421067651,0.0199126722526713,2.83404198860263));
#226192=CARTESIAN_POINT('',(6.03760476191735,59.26644223916,3.40423097483352));
#226193=CARTESIAN_POINT('',(6.00036140429027,58.9120953679532,2.83404198860304));
#226194=CARTESIAN_POINT('',(6.08263713962368,59.6948966996544,3.64303198860304));
#226195=CARTESIAN_POINT('Origin',(6.07864090960019,59.656875110768,3.20400220587394));
#226196=CARTESIAN_POINT('',(6.12459275448634,60.0940777032674,3.64303198860305));
#226197=CARTESIAN_POINT('',(6.13231300382157,60.1675309762117,3.64303198860304));
#226198=CARTESIAN_POINT('',(6.13776734223196,60.2194255397047,3.42473028058523));
#226199=CARTESIAN_POINT('',(6.12459275374915,60.0940777033449,3.64303198860304));
#226200=CARTESIAN_POINT('',(6.17225757416218,60.5475781763996,3.23423028058524));
#226201=CARTESIAN_POINT('Origin',(6.16918208839113,60.518311971387,3.56425743004107));
#226202=CARTESIAN_POINT('',(6.18806312612727,60.6979579581956,3.23423028058524));
#226203=CARTESIAN_POINT('',(6.18811839147268,60.6984837728335,3.23423028058524));
#226204=CARTESIAN_POINT('',(6.22255335066396,61.0261105245456,3.42473028058526));
#226205=CARTESIAN_POINT('Origin',(6.19113993560424,60.7272269341776,3.56425912917774));
#226206=CARTESIAN_POINT('',(6.23572793364572,61.1514583085664,3.64303198860305));
#226207=CARTESIAN_POINT('',(6.22255335066396,61.0261105245456,3.42473028058526));
#226208=CARTESIAN_POINT('',(6.2777380198836,61.551157579787,3.64303198860306));
#226209=CARTESIAN_POINT('Origin',(0.190499999999802,58.2637721346187,2.65878198860302));
#226210=CARTESIAN_POINT('',(-0.0152400000002005,59.0285534841298,2.65878198860303));
#226211=CARTESIAN_POINT('',(-0.0152400000002138,62.8464427007198,2.65878198860306));
#226212=CARTESIAN_POINT('',(-0.0152400000001978,58.2637721346187,2.65878198860302));
#226213=CARTESIAN_POINT('',(0.0152399999997862,62.8464427007198,2.65878198860306));
#226214=CARTESIAN_POINT('Origin',(-4.80914138193527E-17,1.90543592639901E-13,
2.65878198860263));
#226215=CARTESIAN_POINT('',(0.0152399999997995,59.0285534841298,2.65878198860303));
#226216=CARTESIAN_POINT('',(0.0152399999997998,58.957850438373,2.65878198860303));
#226217=CARTESIAN_POINT('Origin',(3.94085276091011E-16,1.90767139479589E-13,
2.65878198860263));
#226218=CARTESIAN_POINT('Origin',(0.1905,-8.8662823435301E-14,42.7590319886026));
#226219=CARTESIAN_POINT('',(0.190499999999796,60.0036905223732,3.64303198860304));
#226220=CARTESIAN_POINT('',(0.190499999999798,59.5728760150044,3.40423097483352));
#226221=CARTESIAN_POINT('Origin',(0.190499999999796,59.9654595002493,3.20400220532009));
#226222=CARTESIAN_POINT('',(0.190499999468327,59.2165773020943,2.83404198860303));
#226223=CARTESIAN_POINT('',(0.190499999999798,59.5728760150044,3.40423097483352));
#226224=CARTESIAN_POINT('',(0.190499999999787,62.6567671111301,2.83404198860305));
#226225=CARTESIAN_POINT('',(0.190499999999786,62.9165533988765,2.83404198860306));
#226226=CARTESIAN_POINT('',(0.190500000604986,62.3004688883556,3.40423097483354));
#226227=CARTESIAN_POINT('',(0.190499999999787,62.6567671111301,2.83404198860305));
#226228=CARTESIAN_POINT('',(0.19049999999979,61.8696548221183,3.64303198860307));
#226229=CARTESIAN_POINT('Origin',(0.190499999999789,61.9078859673757,3.20400259788174));
#226230=CARTESIAN_POINT('',(0.190500000711646,61.4682752798286,3.64303198860306));
#226231=CARTESIAN_POINT('',(0.190500000000006,1.84482744665075E-13,3.64303198860263));
#226232=CARTESIAN_POINT('',(0.190499999999791,61.3422370451707,3.42473028058527));
#226233=CARTESIAN_POINT('',(0.190499999999791,61.4682752798286,3.64303198860306));
#226234=CARTESIAN_POINT('',(0.190499999999793,61.0122769227458,3.23423028058524));
#226235=CARTESIAN_POINT('Origin',(0.190499486622193,61.0417043405088,3.56425722717157));
#226236=CARTESIAN_POINT('',(0.190499999999793,60.8610688070709,3.23423028058524));
#226237=CARTESIAN_POINT('',(0.190500000000006,1.87337391734738E-13,3.23423028058481));
#226238=CARTESIAN_POINT('',(0.190499999999794,60.5311086139136,3.42473028058523));
#226239=CARTESIAN_POINT('Origin',(0.19049948657329,60.8316384807389,3.56425909740902));
#226240=CARTESIAN_POINT('',(0.190499999999795,60.4050703266284,3.64303198860304));
#226241=CARTESIAN_POINT('',(0.190499999999794,60.5311086139136,3.42473028058523));
#226242=CARTESIAN_POINT('',(0.190500000000006,1.84482744665075E-13,3.64303198860263));
#226243=CARTESIAN_POINT('Origin',(-0.1905,-8.99930778254002E-14,42.7590319886026));
#226244=CARTESIAN_POINT('',(-0.190500000000211,61.8696548221182,3.64303198860306));
#226245=CARTESIAN_POINT('',(-0.190500000000212,62.3004688883556,3.40423097483353));
#226246=CARTESIAN_POINT('Origin',(-0.190500000000211,61.9078859670883,3.20400259735724));
#226247=CARTESIAN_POINT('',(-0.190500000452774,62.6567671111301,2.83404198860305));
#226248=CARTESIAN_POINT('',(-0.190500000000212,62.3004688883556,3.40423097483353));
#226249=CARTESIAN_POINT('',(-0.190500000000202,59.2165773020943,2.83404198860303));
#226250=CARTESIAN_POINT('',(-0.190499999999994,1.83179523652187E-13,2.83404198860262));
#226251=CARTESIAN_POINT('',(-0.190499999294346,59.5728760150044,3.40423097483352));
#226252=CARTESIAN_POINT('',(-0.190500000000201,59.2165773020943,2.83404198860303));
#226253=CARTESIAN_POINT('',(-0.190500000000204,60.0036905223732,3.64303198860304));
#226254=CARTESIAN_POINT('Origin',(-0.190500000000204,59.9654594999458,3.20400220587403));
#226255=CARTESIAN_POINT('',(-0.190499999258359,60.4050703266284,3.64303198860304));
#226256=CARTESIAN_POINT('',(-0.190500000000206,60.478928200657,3.64303198860305));
#226257=CARTESIAN_POINT('',(-0.190500000000206,60.5311086139136,3.42473028058523));
#226258=CARTESIAN_POINT('',(-0.190500000000205,60.4050703266284,3.64303198860304));
#226259=CARTESIAN_POINT('',(-0.190500000000207,60.8610688070709,3.23423028058524));
#226260=CARTESIAN_POINT('Origin',(-0.190499486502772,60.8316414495897,3.56425743004083));
#226261=CARTESIAN_POINT('',(-0.190500000000207,61.0122769227458,3.23423028058524));
#226262=CARTESIAN_POINT('',(-0.190500000000207,61.0128056337177,3.23423028058524));
#226263=CARTESIAN_POINT('',(-0.190500000000209,61.3422370451707,3.42473028058527));
#226264=CARTESIAN_POINT('Origin',(-0.190499486688304,61.0417071743814,3.56425912917754));
#226265=CARTESIAN_POINT('',(-0.190500000000209,61.4682752798286,3.64303198860306));
#226266=CARTESIAN_POINT('',(-0.190500000000209,61.3422370451707,3.42473028058527));
#226267=CARTESIAN_POINT('',(-0.190500000000211,61.8701762063764,3.64303198860306));
#226268=CARTESIAN_POINT('Origin',(-5.90076614434095,57.9645097668786,2.65878198860302));
#226269=CARTESIAN_POINT('',(-6.18532049829418,58.7035958781041,2.65878198860303));
#226270=CARTESIAN_POINT('',(-6.58439859103049,62.5005702980932,2.65878198860306));
#226271=CARTESIAN_POINT('',(-6.10537907909402,57.943004080846,2.65878198860302));
#226272=CARTESIAN_POINT('',(-6.55408556365967,62.5037563256536,2.65878198860306));
#226273=CARTESIAN_POINT('Origin',(-3.27251186835855E-17,1.90544397953305E-13,
2.65878198860263));
#226274=CARTESIAN_POINT('',(-6.15500747092336,58.7067819056644,2.65878198860303));
#226275=CARTESIAN_POINT('',(-6.14761699020206,58.6364661785901,2.65878198860303));
#226276=CARTESIAN_POINT('Origin',(3.86084563605877E-16,1.90766720180015E-13,
2.65878198860263));
#226277=CARTESIAN_POINT('Origin',(0.189456421067656,0.0199126722523994,
42.7590319886026));
#226278=CARTESIAN_POINT('',(-6.08263713962407,59.6948966996544,3.64303198860304));
#226279=CARTESIAN_POINT('',(-6.03760476121539,59.2664422392338,3.40423097483352));
#226280=CARTESIAN_POINT('Origin',(-6.07864090963231,59.6568751110698,3.20400220532002));
#226281=CARTESIAN_POINT('',(-6.00036140481931,58.9120953678976,2.83404198860304));
#226282=CARTESIAN_POINT('',(-6.03760476121539,59.2664422392338,3.40423097483352));
#226283=CARTESIAN_POINT('',(-6.35995915837823,62.333439457262,2.83404198860306));
#226284=CARTESIAN_POINT('',(-6.38711421981437,62.5918026085423,2.83404198860306));
#226285=CARTESIAN_POINT('',(-6.32271585208448,61.9790930734953,3.40423097483354));
#226286=CARTESIAN_POINT('',(-6.35995915837823,62.3334394572621,2.83404198860306));
#226287=CARTESIAN_POINT('',(-6.27768352038873,61.5506390517263,3.64303198860306));
#226288=CARTESIAN_POINT('Origin',(-6.28167976325153,61.5886607627708,3.20400259788305));
#226289=CARTESIAN_POINT('',(-6.23572793293792,61.1514583086408,3.64303198860305));
#226290=CARTESIAN_POINT('',(0.189456421067662,0.0199126722526725,3.64303198860263));
#226291=CARTESIAN_POINT('',(-6.22255335066436,61.0261105245456,3.42473028058528));
#226292=CARTESIAN_POINT('',(-6.23572793364612,61.1514583085664,3.64303198860305));
#226293=CARTESIAN_POINT('',(-6.18806312612767,60.6979579581955,3.23423028058524));
#226294=CARTESIAN_POINT('Origin',(-6.19113963944983,60.7272241158243,3.56425722716837));
#226295=CARTESIAN_POINT('',(-6.17225757416258,60.5475781763995,3.23423028058524));
#226296=CARTESIAN_POINT('',(0.189456421067662,0.0199126722526753,3.23423028058481));
#226297=CARTESIAN_POINT('',(-6.13776734223235,60.2194255397047,3.42473028058522));
#226298=CARTESIAN_POINT('Origin',(-6.16918177799174,60.518309018809,3.5642590974125));
#226299=CARTESIAN_POINT('',(-6.12459275374954,60.0940777033448,3.64303198860304));
#226300=CARTESIAN_POINT('',(-6.13776734223235,60.2194255397047,3.42473028058522));
#226301=CARTESIAN_POINT('',(0.189456421067662,0.0199126722526725,3.64303198860263));
#226302=CARTESIAN_POINT('Origin',(-0.189456421067656,-0.019912672252578,
42.7590319886026));
#226303=CARTESIAN_POINT('',(-6.65659636252404,61.5108137072214,3.64303198860306));
#226304=CARTESIAN_POINT('',(-6.70162869482193,61.9392677289271,3.40423097483353));
#226305=CARTESIAN_POINT('Origin',(-6.66059260535667,61.5488354179786,3.20400259735651));
#226306=CARTESIAN_POINT('',(-6.73887200096381,62.2936141127098,2.83404198860306));
#226307=CARTESIAN_POINT('',(-6.70162869482193,61.9392677289271,3.40423097483353));
#226308=CARTESIAN_POINT('',(-6.37927424642597,58.8722700234482,2.83404198860303));
#226309=CARTESIAN_POINT('',(-0.18945642106765,-0.0199126722523048,2.83404198860263));
#226310=CARTESIAN_POINT('',(-6.41651760264873,59.2266168948026,3.40423097483352));
#226311=CARTESIAN_POINT('',(-6.37927424642597,58.8722700234482,2.83404198860304));
#226312=CARTESIAN_POINT('',(-6.46154998175939,59.6550713551494,3.64303198860304));
#226313=CARTESIAN_POINT('Origin',(-6.45755375173598,59.6170497662638,3.20400220587227));
#226314=CARTESIAN_POINT('',(-6.50350559514721,60.0542523589174,3.64303198860304));
#226315=CARTESIAN_POINT('',(-6.51122584595728,60.1277056317067,3.64303198860304));
#226316=CARTESIAN_POINT('',(-6.51668018436767,60.1796001951997,3.42473028058524));
#226317=CARTESIAN_POINT('',(-6.50350559588486,60.0542523588399,3.64303198860304));
#226318=CARTESIAN_POINT('',(-6.55117041629789,60.5077528318945,3.23423028058524));
#226319=CARTESIAN_POINT('Origin',(-6.54809390915841,60.4784867342365,3.56425743004926));
#226320=CARTESIAN_POINT('',(-6.56697596826298,60.6581326136906,3.23423028058524));
#226321=CARTESIAN_POINT('',(-6.5670312336084,60.6586584283285,3.23423028058524));
#226322=CARTESIAN_POINT('',(-6.60146619279967,60.9862851800406,3.42473028058526));
#226323=CARTESIAN_POINT('Origin',(-6.57005175674006,60.6874016969835,3.56425912917843));
#226324=CARTESIAN_POINT('',(-6.61464077578143,61.1116329640614,3.64303198860305));
#226325=CARTESIAN_POINT('',(-6.60146619279967,60.9862851800406,3.42473028058526));
#226326=CARTESIAN_POINT('',(-6.65665086201932,61.511332235282,3.64303198860306));
#226327=CARTESIAN_POINT('Origin',(-11.9273822599896,57.0301761002792,2.65878198860302));
#226328=CARTESIAN_POINT('',(-12.2876333308473,57.7354693911206,2.65878198860302));
#226329=CARTESIAN_POINT('',(-13.0814171332235,61.4699285681956,2.65878198860305));
#226330=CARTESIAN_POINT('',(-12.1286263473646,56.9874003490103,2.65878198860302));
#226331=CARTESIAN_POINT('',(-13.0516031943531,61.4762657165317,2.65878198860305));
#226332=CARTESIAN_POINT('Origin',(-1.75271798929331E-17,1.90546805070335E-13,
2.65878198860263));
#226333=CARTESIAN_POINT('',(-12.257819391977,57.7418065394567,2.65878198860302));
#226334=CARTESIAN_POINT('',(-12.2431194021877,57.6726485248851,2.65878198860302));
#226335=CARTESIAN_POINT('Origin',(3.78171508600985E-16,1.90765466875227E-13,
2.65878198860263));
#226336=CARTESIAN_POINT('Origin',(0.18633711793979,0.0396071771006945,42.7590319886026));
#226337=CARTESIAN_POINT('',(-12.2891316338726,58.7320730967339,3.64303198860303));
#226338=CARTESIAN_POINT('',(-12.1995602612167,58.3106729199897,3.4042309748335));
#226339=CARTESIAN_POINT('Origin',(-12.2811829574212,58.6946775141702,3.20400220531898));
#226340=CARTESIAN_POINT('',(-12.1254815938993,57.9621601887017,2.83404198860302));
#226341=CARTESIAN_POINT('',(-12.1995602612167,58.3106729199897,3.40423097483351));
#226342=CARTESIAN_POINT('',(-12.84073727331,61.3271735965895,2.83404198860304));
#226343=CARTESIAN_POINT('',(-12.8947498796467,61.5812829306521,2.83404198860305));
#226344=CARTESIAN_POINT('',(-12.766658706785,60.9786613449629,3.40423097483352));
#226345=CARTESIAN_POINT('',(-12.84073727331,61.3271735965895,2.83404198860304));
#226346=CARTESIAN_POINT('',(-12.6770874264381,60.5572615995845,3.64303198860306));
#226347=CARTESIAN_POINT('Origin',(-12.6850361284905,60.5946573025913,3.20400259788163));
#226348=CARTESIAN_POINT('',(-12.5936359264448,60.1646531634582,3.64303198860305));
#226349=CARTESIAN_POINT('',(0.186337117939795,0.0396071771009677,3.64303198860263));
#226350=CARTESIAN_POINT('',(-12.5674311046656,60.0413691664789,3.42473028058527));
#226351=CARTESIAN_POINT('',(-12.593635927141,60.1646531633102,3.64303198860304));
#226352=CARTESIAN_POINT('',(-12.4988285377098,59.7186194643911,3.23423028058523));
#226353=CARTESIAN_POINT('Origin',(-12.5049473440522,59.7474037157336,3.56425722717387));
#226354=CARTESIAN_POINT('',(-12.4673906027145,59.5707156088322,3.23423028058523));
#226355=CARTESIAN_POINT('',(0.186337117939795,0.0396071771009705,3.23423028058481));
#226356=CARTESIAN_POINT('',(-12.3987880210526,59.2479658375578,3.42473028058522));
#226357=CARTESIAN_POINT('Origin',(-12.4612721960129,59.5419282989965,3.56425909741342));
#226358=CARTESIAN_POINT('',(-12.3725831876354,59.1246817892492,3.64303198860304));
#226359=CARTESIAN_POINT('',(-12.3987880210526,59.2479658375578,3.42473028058522));
#226360=CARTESIAN_POINT('',(0.186337117939795,0.0396071771009677,3.64303198860263));
#226361=CARTESIAN_POINT('Origin',(-0.18633711793979,-0.0396071771008732,
42.7590319886026));
#226362=CARTESIAN_POINT('',(-13.0497616623177,60.4780472453829,3.64303198860305));
#226363=CARTESIAN_POINT('',(-13.1393329432572,60.8994469906353,3.40423097483352));
#226364=CARTESIAN_POINT('Origin',(-13.0577103643104,60.5154429481089,3.20400259735817));
#226365=CARTESIAN_POINT('',(-13.2134115096321,61.2479592422938,2.83404198860304));
#226366=CARTESIAN_POINT('',(-13.1393329432572,60.8994469906353,3.40423097483352));
#226367=CARTESIAN_POINT('',(-12.4981558292589,57.8829458346107,2.83404198860303));
#226368=CARTESIAN_POINT('',(-0.186337117939783,-0.0396071771005999,2.83404198860263));
#226369=CARTESIAN_POINT('',(-12.5722344964054,58.231458565935,3.40423097483351));
#226370=CARTESIAN_POINT('',(-12.4981558292589,57.8829458346107,2.83404198860303));
#226371=CARTESIAN_POINT('',(-12.6618058697522,58.6528587425324,3.64303198860303));
#226372=CARTESIAN_POINT('Origin',(-12.6538571932377,58.615463159672,3.20400220587252));
#226373=CARTESIAN_POINT('',(-12.7452574227899,59.0454674352017,3.64303198860304));
#226374=CARTESIAN_POINT('',(-12.7606133389844,59.1177113373239,3.64303198860304));
#226375=CARTESIAN_POINT('',(-12.7714622569322,59.1687514833562,3.42473028058522));
#226376=CARTESIAN_POINT('',(-12.745257423515,59.0454674350476,3.64303198860304));
#226377=CARTESIAN_POINT('',(-12.8400648385941,59.4915012546306,3.23423028058523));
#226378=CARTESIAN_POINT('Origin',(-12.8339460446679,59.4627170622779,3.56425743004263));
#226379=CARTESIAN_POINT('',(-12.8715027735894,59.6394051101895,3.23423028058523));
#226380=CARTESIAN_POINT('',(-12.8716126987815,59.6399222675582,3.23423028058523));
#226381=CARTESIAN_POINT('',(-12.9401053405452,59.9621548122773,3.42473028058525));
#226382=CARTESIAN_POINT('Origin',(-12.8776211648735,59.6681923469398,3.56425912917723));
#226383=CARTESIAN_POINT('',(-12.9663101630206,60.0854388091086,3.64303198860304));
#226384=CARTESIAN_POINT('',(-12.9401053405452,59.9621548122773,3.42473028058525));
#226385=CARTESIAN_POINT('',(-13.0498700642004,60.478557236144,3.64303198860305));
#226386=CARTESIAN_POINT('Origin',(-17.8233194796326,55.4710078899935,2.658781988603));
#226387=CARTESIAN_POINT('',(-18.2553202812751,56.1347810195643,2.658781988603));
#226388=CARTESIAN_POINT('',(-19.4351129318423,59.7658094374952,2.65878198860303));
#226389=CARTESIAN_POINT('',(-18.0189898472952,55.4074307335707,2.658781988603));
#226390=CARTESIAN_POINT('',(-19.4061247292256,59.7752282754838,2.65878198860303));
#226391=CARTESIAN_POINT('Origin',(-2.66410924515271E-18,1.90550787618112E-13,
2.65878198860263));
#226392=CARTESIAN_POINT('',(-18.2263320786585,56.1441998575529,2.658781988603));
#226393=CARTESIAN_POINT('',(-18.2044836359655,56.076957265164,2.658781988603));
#226394=CARTESIAN_POINT('Origin',(3.70432808162889E-16,1.90763393296694E-13,
2.65878198860263));
#226395=CARTESIAN_POINT('Origin',(0.181176266354227,0.0588677374283389,
42.7590319886026));
#226396=CARTESIAN_POINT('',(-18.3609838302743,57.1257686104892,3.64303198860302));
#226397=CARTESIAN_POINT('',(-18.227854826074,56.7160396659415,3.40423097483349));
#226398=CARTESIAN_POINT('Origin',(-18.3491697947259,57.0894087477744,3.20400220531829));
#226399=CARTESIAN_POINT('',(-18.1177524692165,56.3771794531165,2.834041988603));
#226400=CARTESIAN_POINT('',(-18.227854826074,56.7160396659415,3.4042309748335));
#226401=CARTESIAN_POINT('',(-19.1808295835784,59.6489943884565,2.83404198860303));
#226402=CARTESIAN_POINT('',(-19.2611079613977,59.8960658302619,2.83404198860303));
#226403=CARTESIAN_POINT('',(-19.0707273770998,59.3101346421295,3.40423097483351));
#226404=CARTESIAN_POINT('',(-19.1808295835784,59.6489943884565,2.83404198860302));
#226405=CARTESIAN_POINT('',(-18.9375985097924,58.9004061169358,3.64303198860304));
#226406=CARTESIAN_POINT('Origin',(-18.9494125833917,58.9367660967595,3.20400259788406));
#226407=CARTESIAN_POINT('',(-18.8135654093537,58.5186714879535,3.64303198860303));
#226408=CARTESIAN_POINT('',(0.181176266354232,0.0588677374286121,3.64303198860262));
#226409=CARTESIAN_POINT('',(-18.7746174535802,58.3988020033599,3.42473028058526));
#226410=CARTESIAN_POINT('',(-18.8135654100305,58.5186714877336,3.64303198860303));
#226411=CARTESIAN_POINT('',(-18.6726541682848,58.0849912788101,3.23423028058522));
#226412=CARTESIAN_POINT('Origin',(-18.6817482287253,58.1129782575892,3.56425722717134));
#226413=CARTESIAN_POINT('',(-18.6259282908539,57.9411838150808,3.23423028058522));
#226414=CARTESIAN_POINT('',(0.181176266354232,0.0588677374286149,3.23423028058481));
#226415=CARTESIAN_POINT('',(-18.523964983701,57.6273730232606,3.42473028058521));
#226416=CARTESIAN_POINT('Origin',(-18.6168343081645,57.9131937527875,3.56425909740641));
#226417=CARTESIAN_POINT('',(-18.485017010988,57.5075034888354,3.64303198860303));
#226418=CARTESIAN_POINT('',(-18.523964983701,57.6273730232606,3.42473028058521));
#226419=CARTESIAN_POINT('',(0.181176266354232,0.0588677374286121,3.64303198860263));
#226420=CARTESIAN_POINT('Origin',(-0.181176266354227,-0.0588677374285176,
42.7590319886026));
#226421=CARTESIAN_POINT('',(-19.2999510425009,58.7826706420789,3.64303198860303));
#226422=CARTESIAN_POINT('',(-19.433079910384,59.1923991670856,3.40423097483351));
#226423=CARTESIAN_POINT('Origin',(-19.3117651160115,58.8190306216296,3.20400259736054));
#226424=CARTESIAN_POINT('',(-19.5431821167169,59.5312589134599,2.83404198860303));
#226425=CARTESIAN_POINT('',(-19.433079910384,59.1923991670856,3.40423097483351));
#226426=CARTESIAN_POINT('',(-18.4801050014193,56.259443978424,2.834041988603));
#226427=CARTESIAN_POINT('',(-0.181176266354219,-0.0588677374282441,2.83404198860262));
#226428=CARTESIAN_POINT('',(-18.5902073581108,56.5983041913029,3.40423097483349));
#226429=CARTESIAN_POINT('',(-18.4801050014193,56.259443978424,2.834041988603));
#226430=CARTESIAN_POINT('',(-18.7233363629827,57.0080331356323,3.64303198860302));
#226431=CARTESIAN_POINT('Origin',(-18.7115223273403,56.9716732726283,3.20400220587359));
#226432=CARTESIAN_POINT('',(-18.8473695429914,57.3897680142076,3.64303198860302));
#226433=CARTESIAN_POINT('',(-18.8701928819397,57.4600110263531,3.64303198860303));
#226434=CARTESIAN_POINT('',(-18.8863175164095,57.5096375484038,3.42473028058521));
#226435=CARTESIAN_POINT('',(-18.8473695436964,57.3897680139785,3.64303198860302));
#226436=CARTESIAN_POINT('',(-18.9882808235623,57.823448340224,3.23423028058522));
#226437=CARTESIAN_POINT('Origin',(-18.9791867816366,57.7954614188155,3.56425743004422));
#226438=CARTESIAN_POINT('',(-19.0350067009933,57.9672558039533,3.23423028058522));
#226439=CARTESIAN_POINT('',(-19.0351700816687,57.9677586379684,3.23423028058522));
#226440=CARTESIAN_POINT('',(-19.1369699862886,58.2810665285031,3.42473028058524));
#226441=CARTESIAN_POINT('Origin',(-19.0441006607083,57.9952457951683,3.56425912918035));
#226442=CARTESIAN_POINT('',(-19.1759179427389,58.4009360128768,3.64303198860304));
#226443=CARTESIAN_POINT('',(-19.1369699862886,58.2810665285031,3.42473028058524));
#226444=CARTESIAN_POINT('',(-19.3001121590972,58.7831665079751,3.64303198860303));
#226445=CARTESIAN_POINT('Origin',(-23.5239806812874,53.3040877092103,2.65878198860298));
#226446=CARTESIAN_POINT('',(-24.0229981225299,53.9190682401996,2.65878198860299));
#226447=CARTESIAN_POINT('',(-25.5758735661211,57.406883591798,2.65878198860301));
#226448=CARTESIAN_POINT('',(-23.7119335237428,53.2204057122639,2.65878198860298));
#226449=CARTESIAN_POINT('',(-25.5480287005721,57.419280924679,2.65878198860301));
#226450=CARTESIAN_POINT('Origin',(1.17012503474363E-17,1.9055630196301E-13,
2.65878198860263));
#226451=CARTESIAN_POINT('',(-23.995153256981,53.9314655730805,2.65878198860299));
#226452=CARTESIAN_POINT('',(-23.9663957374946,53.8668751267879,2.65878198860299));
#226453=CARTESIAN_POINT('Origin',(3.62953249113008E-16,1.90760522162977E-13,
2.65878198860263));
#226454=CARTESIAN_POINT('Origin',(0.174030409680915,0.0774833305058514,
42.7590319886026));
#226455=CARTESIAN_POINT('',(-24.2316692455485,54.8935822490123,3.643031988603));
#226456=CARTESIAN_POINT('',(-24.056441199033,54.5000136127189,3.40423097483348));
#226457=CARTESIAN_POINT('Origin',(-24.2161192879492,54.8586564724116,3.20400220531659));
#226458=CARTESIAN_POINT('',(-23.9115214570978,54.1745185417596,2.83404198860299));
#226459=CARTESIAN_POINT('',(-24.056441199033,54.5000136127189,3.40423097483348));
#226460=CARTESIAN_POINT('',(-25.3107727110825,57.3172883154491,2.83404198860301));
#226461=CARTESIAN_POINT('',(-25.4164373136776,57.5546148985776,2.83404198860301));
#226462=CARTESIAN_POINT('',(-25.1658531674641,56.9917936927136,3.4042309748335));
#226463=CARTESIAN_POINT('',(-25.3107727110825,57.3172883154491,2.83404198860301));
#226464=CARTESIAN_POINT('',(-24.9906253009261,56.5982254591676,3.64303198860302));
#226465=CARTESIAN_POINT('Origin',(-25.0061753086091,56.6331513482581,3.20400259788199));
#226466=CARTESIAN_POINT('',(-24.8273695326455,56.2315470018078,3.64303198860301));
#226467=CARTESIAN_POINT('',(0.174030409680921,0.0774833305061245,3.64303198860263));
#226468=CARTESIAN_POINT('',(-24.776105164832,56.1164053447572,3.42473028058524));
#226469=CARTESIAN_POINT('',(-24.8273695332959,56.2315470015182,3.64303198860301));
#226470=CARTESIAN_POINT('',(-24.641898292288,55.8149717737127,3.2342302805852));
#226471=CARTESIAN_POINT('Origin',(-24.6538679703971,55.841854848731,3.56425722717164));
#226472=CARTESIAN_POINT('',(-24.5803964109126,55.6768362864792,3.2342302805852));
#226473=CARTESIAN_POINT('',(0.174030409680921,0.0774833305061274,3.23423028058481));
#226474=CARTESIAN_POINT('',(-24.4461895095991,55.3754026508176,3.42473028058519));
#226475=CARTESIAN_POINT('Origin',(-24.5684264878145,55.6499501367131,3.56425909741001));
#226476=CARTESIAN_POINT('',(-24.3949251197297,55.2602609459791,3.643031988603));
#226477=CARTESIAN_POINT('',(-24.4461895095991,55.3754026508176,3.42473028058519));
#226478=CARTESIAN_POINT('',(0.174030409680921,0.0774833305061245,3.64303198860262));
#226479=CARTESIAN_POINT('Origin',(-0.174030409680915,-0.07748333050603,
42.7590319886026));
#226480=CARTESIAN_POINT('',(-25.338686120288,56.4432587981557,3.64303198860301));
#226481=CARTESIAN_POINT('',(-25.5139139873792,56.8368270314554,3.40423097483349));
#226482=CARTESIAN_POINT('Origin',(-25.3542361278549,56.4781846869857,3.20400259736215));
#226483=CARTESIAN_POINT('',(-25.6588335308575,57.1623216542532,2.83404198860301));
#226484=CARTESIAN_POINT('',(-25.5139139873792,56.8368270314554,3.40423097483349));
#226485=CARTESIAN_POINT('',(-24.2595822759735,54.0195518809642,2.83404198860299));
#226486=CARTESIAN_POINT('',(-0.174030409680907,-0.0774833305057564,2.83404198860262));
#226487=CARTESIAN_POINT('',(-24.4045020177488,54.3450469519947,3.40423097483348));
#226488=CARTESIAN_POINT('',(-24.2595822759735,54.0195518809642,2.83404198860299));
#226489=CARTESIAN_POINT('',(-24.5797300649104,54.7386155880004,3.64303198860301));
#226490=CARTESIAN_POINT('Origin',(-24.5641801071872,54.7036898111215,3.20400220587239));
#226491=CARTESIAN_POINT('',(-24.7429859384138,55.105294285269,3.64303198860301));
#226492=CARTESIAN_POINT('',(-24.7730266428387,55.1727668102972,3.64303198860301));
#226493=CARTESIAN_POINT('',(-24.794250328961,55.2204359898057,3.42473028058518));
#226494=CARTESIAN_POINT('',(-24.7429859390916,55.1052942849672,3.64303198860301));
#226495=CARTESIAN_POINT('',(-24.9284572302744,55.5218696254674,3.2342302805852));
#226496=CARTESIAN_POINT('Origin',(-24.9164875765749,55.4949866055689,3.56425743004152));
#226497=CARTESIAN_POINT('',(-24.9899591116498,55.6600051127008,3.2342302805852));
#226498=CARTESIAN_POINT('',(-24.9901741577757,55.6604881142077,3.2342302805852));
#226499=CARTESIAN_POINT('',(-25.1241659841938,55.9614386837454,3.42473028058522));
#226500=CARTESIAN_POINT('Origin',(-25.0019290044706,55.6868911941813,3.56425912918012));
#226501=CARTESIAN_POINT('',(-25.1754303526578,56.0765803405064,3.64303198860301));
#226502=CARTESIAN_POINT('',(-25.1241659841938,55.9614386837454,3.42473028058522));
#226503=CARTESIAN_POINT('',(-25.3388981863709,56.4437351063764,3.64303198860301));
#226504=CARTESIAN_POINT('Origin',(-28.9669082278886,50.5531567888876,2.65878198860297));
#226505=CARTESIAN_POINT('',(-29.5274749692187,51.1126068659047,2.65878198860297));
#226506=CARTESIAN_POINT('',(-31.4364195775137,54.4189959163063,2.65878198860299));
#226507=CARTESIAN_POINT('',(-29.1450842944632,50.4502867888876,2.65878198860296));
#226508=CARTESIAN_POINT('',(-31.4100231232064,54.4342359163063,2.65878198860299));
#226509=CARTESIAN_POINT('Origin',(2.54115089989956E-17,1.90563287688712E-13,
2.65878198860263));
#226510=CARTESIAN_POINT('',(-29.5010785149114,51.1278468659047,2.65878198860297));
#226511=CARTESIAN_POINT('',(-29.465726992033,51.0666162321544,2.65878198860297));
#226512=CARTESIAN_POINT('Origin',(3.55814779065492E-16,1.90756884930817E-13,
2.65878198860263));
#226513=CARTESIAN_POINT('Origin',(0.164977839420935,0.0952499999999114,
42.7590319886026));
#226514=CARTESIAN_POINT('',(-29.8368674217658,52.0599703131947,3.64303198860298));
#226515=CARTESIAN_POINT('',(-29.6214601680814,51.6868740054943,3.40423097483346));
#226516=CARTESIAN_POINT('Origin',(-29.8177519107044,52.0268612768235,3.20400220531785));
#226517=CARTESIAN_POINT('',(-29.4433108120869,51.3783102685126,2.83404198860297));
#226518=CARTESIAN_POINT('',(-29.6214601680814,51.6868740054943,3.40423097483346));
#226519=CARTESIAN_POINT('',(-31.1634057161443,54.3576020372439,2.83404198860299));
#226520=CARTESIAN_POINT('',(-31.2932988600175,54.5825835619871,2.83404198860299));
#226521=CARTESIAN_POINT('',(-30.9852566042332,54.0490387253004,3.40423097483347));
#226522=CARTESIAN_POINT('',(-31.1634057161443,54.3576020372439,2.83404198860299));
#226523=CARTESIAN_POINT('',(-30.7698495716383,53.6759427993287,3.643031988603));
#226524=CARTESIAN_POINT('Origin',(-30.7889651442679,53.7090519423389,3.20400259788483));
#226525=CARTESIAN_POINT('',(-30.569159799877,53.3283379195024,3.64303198860299));
#226526=CARTESIAN_POINT('',(0.164977839420941,0.0952500000001846,3.64303198860263));
#226527=CARTESIAN_POINT('',(-30.5061406831646,53.2191856060846,3.42473028058522));
#226528=CARTESIAN_POINT('',(-30.5691598004935,53.3283379191465,3.64303198860299));
#226529=CARTESIAN_POINT('',(-30.3411606219521,52.9334317578288,3.23423028058518));
#226530=CARTESIAN_POINT('Origin',(-30.3558747754313,52.95891639249,3.56425722717323));
#226531=CARTESIAN_POINT('',(-30.2655565641147,52.802481688396,3.23423028058517));
#226532=CARTESIAN_POINT('',(0.164977839420941,0.0952500000001874,3.23423028058481));
#226533=CARTESIAN_POINT('',(-30.100576467536,52.5167277788842,3.42473028058516));
#226534=CARTESIAN_POINT('Origin',(-30.250841845591,52.7769940214409,3.56425909741636));
#226535=CARTESIAN_POINT('',(-30.0375573238934,52.4075754202457,3.64303198860298));
#226536=CARTESIAN_POINT('',(-30.100576467536,52.5167277788842,3.42473028058516));
#226537=CARTESIAN_POINT('',(0.164977839420941,0.0952500000001846,3.64303198860263));
#226538=CARTESIAN_POINT('Origin',(-0.164977839420935,-0.0952500000000901,
42.7590319886026));
#226539=CARTESIAN_POINT('',(-31.0998052504802,53.4854427993287,3.64303198860299));
#226540=CARTESIAN_POINT('',(-31.3152122835989,53.8585387249979,3.40423097483347));
#226541=CARTESIAN_POINT('Origin',(-31.1189208229661,53.5185519420901,3.20400259736088));
#226542=CARTESIAN_POINT('',(-31.4933613953777,54.1671020370178,2.83404198860299));
#226543=CARTESIAN_POINT('',(-31.3152122835989,53.8585387249979,3.40423097483347));
#226544=CARTESIAN_POINT('',(-29.7732664904682,51.1878102687785,2.83404198860297));
#226545=CARTESIAN_POINT('',(-0.164977839420927,-0.0952499999998162,2.83404198860262));
#226546=CARTESIAN_POINT('',(-29.9514158463113,51.4963740058476,3.40423097483345));
#226547=CARTESIAN_POINT('',(-29.7732664904682,51.1878102687785,2.83404198860297));
#226548=CARTESIAN_POINT('',(-30.1668231006077,51.8694703131947,3.64303198860298));
#226549=CARTESIAN_POINT('Origin',(-30.1477075893944,51.8363612765605,3.20400220587241));
#226550=CARTESIAN_POINT('',(-30.3675130020929,52.2170754206166,3.64303198860298));
#226551=CARTESIAN_POINT('',(-30.4044419397496,52.281038215424,3.64303198860298));
#226552=CARTESIAN_POINT('',(-30.4305321463779,52.3262277788842,3.42473028058517));
#226553=CARTESIAN_POINT('',(-30.3675130027353,52.2170754202457,3.64303198860298));
#226554=CARTESIAN_POINT('',(-30.5955122429565,52.611981688396,3.23423028058517));
#226555=CARTESIAN_POINT('Origin',(-30.580798119513,52.5864971059978,3.5642574300363));
#226556=CARTESIAN_POINT('',(-30.671116300794,52.7429317578288,3.23423028058517));
#226557=CARTESIAN_POINT('',(-30.6713806562799,52.7433896349617,3.23423028058517));
#226558=CARTESIAN_POINT('',(-30.8360963620065,53.0286856060846,3.4247302805852));
#226559=CARTESIAN_POINT('Origin',(-30.6858309820704,52.7684193600405,3.56425912917864));
#226560=CARTESIAN_POINT('',(-30.8991154793354,53.1378379191465,3.64303198860299));
#226561=CARTESIAN_POINT('',(-30.8360963620065,53.0286856060846,3.4247302805852));
#226562=CARTESIAN_POINT('',(-31.1000659426093,53.4858943313413,3.64303198860299));
#226563=CARTESIAN_POINT('Origin',(-34.0924682662297,47.2483549038576,2.65878198860294));
#226564=CARTESIAN_POINT('',(-34.7084426211234,47.7461450747865,2.65878198860295));
#226565=CARTESIAN_POINT('',(-36.9525415975215,50.8348823336486,2.65878198860297));
#226566=CARTESIAN_POINT('',(-34.2589154226524,47.1274239660509,2.65878198860294));
#226567=CARTESIAN_POINT('',(-36.9278827595329,50.8527980281385,2.65878198860297));
#226568=CARTESIAN_POINT('Origin',(3.83164542466812E-17,1.90571668258146E-13,
2.65878198860263));
#226569=CARTESIAN_POINT('',(-34.6837837831348,47.7640607692763,2.65878198860295));
#226570=CARTESIAN_POINT('',(-34.6422255755468,47.706860803705,2.65878198860295));
#226571=CARTESIAN_POINT('Origin',(3.49095608592005E-16,1.90752521450492E-13,
2.65878198860263));
#226572=CARTESIAN_POINT('Origin',(0.154117737428427,0.111973090561628,42.7590319886026));
#226573=CARTESIAN_POINT('',(-35.1151666347443,48.6559784483765,3.64303198860296));
#226574=CARTESIAN_POINT('',(-34.8619402208392,48.3074421904918,3.40423097483344));
#226575=CARTESIAN_POINT('Origin',(-35.0926950037607,48.6250489017672,3.20400220531682));
#226576=CARTESIAN_POINT('',(-34.6525130924105,48.0191904763608,2.83404198860294));
#226577=CARTESIAN_POINT('',(-34.8619402208392,48.3074421904918,3.40423097483344));
#226578=CARTESIAN_POINT('',(-36.674605926818,50.8023624960591,2.83404198860297));
#226579=CARTESIAN_POINT('',(-36.8273044755032,51.0125340177515,2.83404198860297));
#226580=CARTESIAN_POINT('',(-36.4651790855639,50.5141111791244,3.40423097483344));
#226581=CARTESIAN_POINT('',(-36.674605926818,50.8023624960591,2.83404198860296));
#226582=CARTESIAN_POINT('',(-36.2119529314387,50.1655752777672,3.64303198860298));
#226583=CARTESIAN_POINT('Origin',(-36.2344246347996,50.1965049239953,3.20400259788265));
#226584=CARTESIAN_POINT('',(-35.9760279553333,49.8408524072786,3.64303198860296));
#226585=CARTESIAN_POINT('',(0.154117737428432,0.111973090561901,3.64303198860263));
#226586=CARTESIAN_POINT('',(-35.9019445403521,49.7388853330811,3.42473028058518));
#226587=CARTESIAN_POINT('',(-35.9760279559089,49.8408524068604,3.64303198860296));
#226588=CARTESIAN_POINT('',(-35.7079988465461,49.4719419865733,3.23423028058515));
#226589=CARTESIAN_POINT('Origin',(-35.7252962640516,49.4957489658886,3.56425722717188));
#226590=CARTESIAN_POINT('',(-35.6191209461254,49.3496120513049,3.23423028058515));
#226591=CARTESIAN_POINT('',(0.154117737428432,0.111973090561904,3.23423028058481));
#226592=CARTESIAN_POINT('',(-35.425175210744,49.0826686475735,3.42473028058514));
#226593=CARTESIAN_POINT('Origin',(-35.6018226497097,49.3258021153701,3.56425909741368));
#226594=CARTESIAN_POINT('',(-35.3510917642536,48.9807015312178,3.64303198860296));
#226595=CARTESIAN_POINT('',(-35.425175210744,49.0826686475735,3.42473028058514));
#226596=CARTESIAN_POINT('',(0.154117737428432,0.111973090561901,3.64303198860263));
#226597=CARTESIAN_POINT('Origin',(-0.154117737428427,-0.111973090561806,
42.7590319886026));
#226598=CARTESIAN_POINT('',(-36.5201884062956,49.9416290966437,3.64303198860297));
#226599=CARTESIAN_POINT('',(-36.7734145609101,50.2901649976455,3.40423097483344));
#226600=CARTESIAN_POINT('Origin',(-36.5426601094868,49.9725587426385,3.20400259735612));
#226601=CARTESIAN_POINT('',(-36.9828414020409,50.5784163146698,2.83404198860296));
#226602=CARTESIAN_POINT('',(-36.7734145609101,50.2901649976455,3.40423097483344));
#226603=CARTESIAN_POINT('',(-34.9607485668368,47.7952442955502,2.83404198860294));
#226604=CARTESIAN_POINT('',(-0.154117737428418,-0.111973090561532,2.83404198860262));
#226605=CARTESIAN_POINT('',(-35.1701756951248,48.0834960097834,3.40423097483343));
#226606=CARTESIAN_POINT('',(-34.9607485668368,47.7952442955502,2.83404198860294));
#226607=CARTESIAN_POINT('',(-35.4234021096012,48.4320322672531,3.64303198860295));
#226608=CARTESIAN_POINT('Origin',(-35.4009304784384,48.4011027203971,3.20400220587326));
#226609=CARTESIAN_POINT('',(-35.6593272385106,48.7567553505302,3.64303198860296));
#226610=CARTESIAN_POINT('',(-35.7027398082301,48.8165076253519,3.64303198860296));
#226611=CARTESIAN_POINT('',(-35.7334106856009,48.85872246645,3.42473028058515));
#226612=CARTESIAN_POINT('',(-35.6593272391104,48.7567553500944,3.64303198860296));
#226613=CARTESIAN_POINT('',(-35.9273564209823,49.1256658701815,3.23423028058515));
#226614=CARTESIAN_POINT('Origin',(-35.9100590388141,49.1018589397078,3.56425743004463));
#226615=CARTESIAN_POINT('',(-36.0162343214029,49.2479958054499,3.23423028058515));
#226616=CARTESIAN_POINT('',(-36.0165450899149,49.2484235416113,3.23423028058515));
#226617=CARTESIAN_POINT('',(-36.2101800152089,49.5149391519577,3.42473028058518));
#226618=CARTESIAN_POINT('Origin',(-36.0335325740083,49.27180568089,3.56425912917508));
#226619=CARTESIAN_POINT('',(-36.2842634307658,49.616906225737,3.64303198860296));
#226620=CARTESIAN_POINT('',(-36.2101800152089,49.5149391519577,3.42473028058518));
#226621=CARTESIAN_POINT('',(-36.5204948682733,49.9420509053691,3.64303198860297));
#226622=CARTESIAN_POINT('Origin',(-38.8445040879384,43.4258901551471,2.65878198860291));
#226623=CARTESIAN_POINT('',(-39.5091373124624,43.8565665267056,2.65878198860292));
#226624=CARTESIAN_POINT('',(-42.0638038389703,46.6938111422604,2.65878198860294));
#226625=CARTESIAN_POINT('',(-38.9973987043321,43.2882232241948,2.65878198860291));
#226626=CARTESIAN_POINT('',(-42.0411527846897,46.7142062431422,2.65878198860294));
#226627=CARTESIAN_POINT('Origin',(5.02746968098277E-17,1.90581351852038E-13,
2.65878198860263));
#226628=CARTESIAN_POINT('',(-39.4864862581819,43.8769616275874,2.65878198860292));
#226629=CARTESIAN_POINT('',(-39.4391766863032,43.8244190249878,2.65878198860292));
#226630=CARTESIAN_POINT('Origin',(3.42869354330331E-16,1.90747479529204E-13,
2.65878198860263));
#226631=CARTESIAN_POINT('Origin',(0.141569089253443,0.127469380511274,42.7590319886026));
#226632=CARTESIAN_POINT('',(-40.0087367337515,44.7189015017598,3.64303198860293));
#226633=CARTESIAN_POINT('',(-39.7204655612076,44.3987439298681,3.4042309748334));
#226634=CARTESIAN_POINT('Origin',(-39.9831551867368,44.6904903154967,3.20400220531776));
#226635=CARTESIAN_POINT('',(-39.4820551877884,44.1339623846889,2.83404198860292));
#226636=CARTESIAN_POINT('',(-39.7204655612076,44.3987439298681,3.4042309748334));
#226637=CARTESIAN_POINT('',(-41.7839914803029,46.6905216402897,2.83404198860294));
#226638=CARTESIAN_POINT('',(-41.9578224365464,46.8835804757584,2.83404198860294));
#226639=CARTESIAN_POINT('',(-41.5455814340025,46.4257404601139,3.40423097483342));
#226640=CARTESIAN_POINT('',(-41.7839914803029,46.6905216402897,2.83404198860294));
#226641=CARTESIAN_POINT('',(-41.2573105570839,46.1055832156409,3.64303198860295));
#226642=CARTESIAN_POINT('Origin',(-41.2828921864922,46.1339944934115,3.20400259788282));
#226643=CARTESIAN_POINT('',(-40.9887352200424,45.8073000862123,3.64303198860294));
#226644=CARTESIAN_POINT('',(0.141569089253448,0.127469380511547,3.64303198860263));
#226645=CARTESIAN_POINT('',(-40.9043991801906,45.7136354238375,3.42473028058516));
#226646=CARTESIAN_POINT('',(-40.9887352205716,45.8073000857359,3.64303198860294));
#226647=CARTESIAN_POINT('',(-40.6836127633981,45.4684272662436,3.23423028058512));
#226648=CARTESIAN_POINT('Origin',(-40.7033039308037,45.490295755965,3.56425722717074));
#226649=CARTESIAN_POINT('',(-40.5824347852702,45.3560577375096,3.23423028058512));
#226650=CARTESIAN_POINT('',(0.141569089253449,0.12746938051155,3.23423028058481));
#226651=CARTESIAN_POINT('',(-40.3616483211486,45.1108495273513,3.42473028058512));
#226652=CARTESIAN_POINT('Origin',(-40.5627424347179,45.334186399236,3.56425909741268));
#226653=CARTESIAN_POINT('',(-40.277312245553,45.0171848263432,3.64303198860293));
#226654=CARTESIAN_POINT('',(-40.3616483211486,45.1108495273513,3.42473028058512));
#226655=CARTESIAN_POINT('',(0.141569089253448,0.127469380511547,3.64303198860263));
#226656=CARTESIAN_POINT('Origin',(-0.141569089253443,-0.127469380511452,
42.7590319886026));
#226657=CARTESIAN_POINT('',(-41.5404487355908,45.8506444546182,3.64303198860294));
#226658=CARTESIAN_POINT('',(-41.8287196129601,46.1708016986854,3.40423097483341));
#226659=CARTESIAN_POINT('Origin',(-41.5660303648069,45.8790557321753,3.20400259735887));
#226660=CARTESIAN_POINT('',(-42.0671296591458,46.4355828789644,2.83404198860293));
#226661=CARTESIAN_POINT('',(-41.8287196129601,46.1708016986854,3.40423097483341));
#226662=CARTESIAN_POINT('',(-39.7651933659001,43.879023624022,2.83404198860291));
#226663=CARTESIAN_POINT('',(-0.141569089253434,-0.127469380511178,2.83404198860262));
#226664=CARTESIAN_POINT('',(-40.00360373919,44.1438051693176,3.40423097483341));
#226665=CARTESIAN_POINT('',(-39.7651933659001,43.879023624022,2.83404198860291));
#226666=CARTESIAN_POINT('',(-40.2918749122584,44.4639627407371,3.64303198860293));
#226667=CARTESIAN_POINT('Origin',(-40.2662933650409,44.4355515542486,3.20400220587102));
#226668=CARTESIAN_POINT('',(-40.5604504235087,44.7622460658168,3.64303198860293));
#226669=CARTESIAN_POINT('',(-40.609870988093,44.8171331622256,3.64303198860293));
#226670=CARTESIAN_POINT('',(-40.6447864996555,44.8559107663285,3.42473028058512));
#226671=CARTESIAN_POINT('',(-40.5604504240599,44.7622460653205,3.64303198860293));
#226672=CARTESIAN_POINT('',(-40.8655729637771,45.1011189764869,3.23423028058512));
#226673=CARTESIAN_POINT('Origin',(-40.8458818366199,45.0792505316449,3.56425743004204));
#226674=CARTESIAN_POINT('',(-40.966750941905,45.2134885052208,3.23423028058512));
#226675=CARTESIAN_POINT('',(-40.9671047185982,45.2138814140438,3.23423028058512));
#226676=CARTESIAN_POINT('',(-41.1875373586974,45.4586966628148,3.42473028058515));
#226677=CARTESIAN_POINT('Origin',(-40.9864432425629,45.23535978791,3.56425912917542));
#226678=CARTESIAN_POINT('',(-41.2718733990785,45.5523613247131,3.64303198860294));
#226679=CARTESIAN_POINT('',(-41.1875373586974,45.4586966628148,3.42473028058515));
#226680=CARTESIAN_POINT('',(-41.5407976097556,45.8510319186317,3.64303198860294));
#226681=CARTESIAN_POINT('Origin',(-43.1709513941246,39.127642266445,2.65878198860289));
#226682=CARTESIAN_POINT('',(-43.8769616275876,39.4864862581816,2.65878198860289));
#226683=CARTESIAN_POINT('',(-46.7142062431425,42.0411527846894,2.65878198860291));
#226684=CARTESIAN_POINT('',(-43.3086183250768,38.9747476500513,2.65878198860289));
#226685=CARTESIAN_POINT('',(-46.6938111422606,42.06380383897,2.65878198860291));
#226686=CARTESIAN_POINT('Origin',(6.11552196804858E-17,1.90592232374909E-13,
2.65878198860263));
#226687=CARTESIAN_POINT('',(-43.8565665267058,39.5091373124622,2.65878198860289));
#226688=CARTESIAN_POINT('',(-43.8040239241062,39.4618277405835,2.65878198860289));
#226689=CARTESIAN_POINT('Origin',(3.37204232425085E-16,1.90741814407299E-13,
2.65878198860263));
#226690=CARTESIAN_POINT('Origin',(0.127469380511362,0.141569089253355,42.7590319886026));
#226691=CARTESIAN_POINT('',(-44.4639627407373,40.2918749122582,3.64303198860289));
#226692=CARTESIAN_POINT('',(-44.1438051688456,40.0036037397142,3.40423097483338));
#226693=CARTESIAN_POINT('Origin',(-44.4355515544742,40.2662933652435,3.20400220531717));
#226694=CARTESIAN_POINT('',(-43.8790236243777,39.7651933655051,2.83404198860289));
#226695=CARTESIAN_POINT('',(-44.1438051688456,40.0036037397142,3.40423097483338));
#226696=CARTESIAN_POINT('',(-46.4355828792672,42.0671296588095,2.8340419886029));
#226697=CARTESIAN_POINT('',(-46.6286417147359,42.240960615053,2.8340419886029));
#226698=CARTESIAN_POINT('',(-46.1708016982804,41.8287196134099,3.40423097483339));
#226699=CARTESIAN_POINT('',(-46.4355828792672,42.0671296588095,2.8340419886029));
#226700=CARTESIAN_POINT('',(-45.8506444546184,41.5404487355905,3.64303198860291));
#226701=CARTESIAN_POINT('Origin',(-45.879055732388,41.5660303649979,3.20400259787986));
#226702=CARTESIAN_POINT('',(-45.5523613242372,41.2718733996071,3.6430319886029));
#226703=CARTESIAN_POINT('',(0.127469380511367,0.141569089253628,3.64303198860262));
#226704=CARTESIAN_POINT('',(-45.458696662815,41.1875373586972,3.42473028058513));
#226705=CARTESIAN_POINT('',(-45.5523613247134,41.2718733990782,3.6430319886029));
#226706=CARTESIAN_POINT('',(-45.2134885052211,40.9667509419047,3.23423028058509));
#226707=CARTESIAN_POINT('Origin',(-45.2353576819753,40.986441346282,3.56425722717232));
#226708=CARTESIAN_POINT('',(-45.1011189764871,40.8655729637768,3.23423028058508));
#226709=CARTESIAN_POINT('',(0.127469380511367,0.141569089253631,3.23423028058481));
#226710=CARTESIAN_POINT('',(-44.8559107663287,40.6447864996552,3.42473028058509));
#226711=CARTESIAN_POINT('Origin',(-45.0792483253111,40.8458798501231,3.56425909740998));
#226712=CARTESIAN_POINT('',(-44.7622460653207,40.5604504240596,3.6430319886029));
#226713=CARTESIAN_POINT('',(-44.8559107663287,40.6447864996552,3.42473028058509));
#226714=CARTESIAN_POINT('',(0.127469380511367,0.141569089253628,3.64303198860262));
#226715=CARTESIAN_POINT('Origin',(-0.127469380511362,-0.141569089253534,
42.7590319886026));
#226716=CARTESIAN_POINT('',(-46.1055832156411,41.2573105570836,3.64303198860291));
#226717=CARTESIAN_POINT('',(-46.4257404597083,41.545581434453,3.40423097483338));
#226718=CARTESIAN_POINT('Origin',(-46.1339944931981,41.2828921862996,3.20400259735835));
#226719=CARTESIAN_POINT('',(-46.6905216405927,41.7839914799664,2.8340419886029));
#226720=CARTESIAN_POINT('',(-46.4257404597083,41.545581434453,3.40423097483338));
#226721=CARTESIAN_POINT('',(-44.1339623850449,39.482055187393,2.83404198860288));
#226722=CARTESIAN_POINT('',(-0.127469380511352,-0.141569089253259,2.83404198860262));
#226723=CARTESIAN_POINT('',(-44.3987439293959,39.720465561732,3.40423097483337));
#226724=CARTESIAN_POINT('',(-44.1339623850449,39.482055187393,2.83404198860288));
#226725=CARTESIAN_POINT('',(-44.7189015017601,40.0087367337513,3.6430319886029));
#226726=CARTESIAN_POINT('Origin',(-44.6904903152701,39.9831551865324,3.20400220587441));
#226727=CARTESIAN_POINT('',(-45.0171848258471,40.277312246104,3.6430319886029));
#226728=CARTESIAN_POINT('',(-45.0720719232486,40.3267328095859,3.6430319886029));
#226729=CARTESIAN_POINT('',(-45.1108495273515,40.3616483211483,3.42473028058508));
#226730=CARTESIAN_POINT('',(-45.0171848263434,40.2773122455527,3.6430319886029));
#226731=CARTESIAN_POINT('',(-45.3560577375098,40.5824347852699,3.23423028058509));
#226732=CARTESIAN_POINT('Origin',(-45.3341886054739,40.5627444213184,3.56425743004201));
#226733=CARTESIAN_POINT('',(-45.4684272662438,40.6836127633978,3.23423028058509));
#226734=CARTESIAN_POINT('',(-45.4688201750668,40.6839665400911,3.23423028058509));
#226735=CARTESIAN_POINT('',(-45.7136354238378,40.9043991801903,3.42473028058511));
#226736=CARTESIAN_POINT('Origin',(-45.4902978619855,40.7033058269841,3.56425912918036));
#226737=CARTESIAN_POINT('',(-45.8073000857361,40.9887352205713,3.64303198860291));
#226738=CARTESIAN_POINT('',(-45.7136354238378,40.9043991801903,3.42473028058511));
#226739=CARTESIAN_POINT('',(-46.1059706796546,41.2576594312484,3.64303198860291));
#226740=CARTESIAN_POINT('Origin',(-47.0244087227343,34.4007037410863,2.65878198860285));
#226741=CARTESIAN_POINT('',(-47.7640607692765,34.6837837831345,2.65878198860285));
#226742=CARTESIAN_POINT('',(-50.8527980281387,36.9278827595326,2.65878198860287));
#226743=CARTESIAN_POINT('',(-47.145339660541,34.2342565846636,2.65878198860285));
#226744=CARTESIAN_POINT('',(-50.8348823336488,36.9525415975211,2.65878198860287));
#226745=CARTESIAN_POINT('Origin',(7.08388135731919E-17,1.90604190617472E-13,
2.65878198860263));
#226746=CARTESIAN_POINT('',(-47.7461450747866,34.7084426211231,2.65878198860285));
#226747=CARTESIAN_POINT('',(-47.6889451092153,34.6668844135351,2.65878198860285));
#226748=CARTESIAN_POINT('Origin',(3.32162311137368E-16,1.90735588153037E-13,
2.65878198860263));
#226749=CARTESIAN_POINT('Origin',(0.111973090561715,0.154117737428339,42.7590319886026));
#226750=CARTESIAN_POINT('',(-48.4320322672532,35.4234021096009,3.64303198860286));
#226751=CARTESIAN_POINT('',(-48.0834960093685,35.1701756956958,3.40423097483334));
#226752=CARTESIAN_POINT('Origin',(-48.4011027206437,35.4009304786171,3.20400220531728));
#226753=CARTESIAN_POINT('',(-47.7952442958629,34.9607485664063,2.83404198860285));
#226754=CARTESIAN_POINT('',(-48.0834960093685,35.1701756956958,3.40423097483334));
#226755=CARTESIAN_POINT('',(-50.5784163149358,36.9828414016746,2.83404198860287));
#226756=CARTESIAN_POINT('',(-50.7885878366283,37.1355399503597,2.83404198860287));
#226757=CARTESIAN_POINT('',(-50.29016499729,36.7734145613993,3.40423097483335));
#226758=CARTESIAN_POINT('',(-50.5784163149359,36.9828414016746,2.83404198860287));
#226759=CARTESIAN_POINT('',(-49.9416290966439,36.5201884062952,3.64303198860288));
#226760=CARTESIAN_POINT('Origin',(-49.9725587428718,36.5426601096559,3.20400259788167));
#226761=CARTESIAN_POINT('',(-49.6169062253184,36.2842634313418,3.64303198860287));
#226762=CARTESIAN_POINT('',(0.111973090561721,0.154117737428612,3.64303198860263));
#226763=CARTESIAN_POINT('',(-49.5149391519579,36.2101800152086,3.42473028058509));
#226764=CARTESIAN_POINT('',(-49.6169062257371,36.2842634307655,3.64303198860287));
#226765=CARTESIAN_POINT('',(-49.2479958054501,36.0162343214026,3.23423028058506));
#226766=CARTESIAN_POINT('Origin',(-49.271803388277,36.0335309082457,3.56425722717104));
#226767=CARTESIAN_POINT('',(-49.1256658701817,35.927356420982,3.23423028058506));
#226768=CARTESIAN_POINT('',(0.111973090561721,0.154117737428615,3.23423028058481));
#226769=CARTESIAN_POINT('',(-48.8587224664502,35.7334106856006,3.42473028058505));
#226770=CARTESIAN_POINT('Origin',(-49.1018565378153,35.9100572938243,3.56425909741256));
#226771=CARTESIAN_POINT('',(-48.7567553500946,35.6593272391101,3.64303198860287));
#226772=CARTESIAN_POINT('',(-48.8587224664502,35.7334106856006,3.42473028058505));
#226773=CARTESIAN_POINT('',(0.111973090561721,0.154117737428612,3.64303198860263));
#226774=CARTESIAN_POINT('Origin',(-0.111973090561715,-0.154117737428517,
42.7590319886026));
#226775=CARTESIAN_POINT('',(-50.1655752777673,36.2119529314384,3.64303198860287));
#226776=CARTESIAN_POINT('',(-50.5141111787691,36.4651790860529,3.40423097483334));
#226777=CARTESIAN_POINT('Origin',(-50.1965049237621,36.2344246346297,3.20400259735654));
#226778=CARTESIAN_POINT('',(-50.8023624963254,36.6746059264515,2.83404198860287));
#226779=CARTESIAN_POINT('',(-50.5141111787691,36.4651790860529,3.40423097483334));
#226780=CARTESIAN_POINT('',(-48.0191904766738,34.6525130919796,2.83404198860285));
#226781=CARTESIAN_POINT('',(-0.111973090561705,-0.154117737428242,2.83404198860262));
#226782=CARTESIAN_POINT('',(-48.3074421900768,34.8619402214103,3.40423097483334));
#226783=CARTESIAN_POINT('',(-48.0191904766738,34.6525130919796,2.83404198860285));
#226784=CARTESIAN_POINT('',(-48.6559784483767,35.115166634744,3.64303198860286));
#226785=CARTESIAN_POINT('Origin',(-48.6250489015209,35.0926950035814,3.20400220587282));
#226786=CARTESIAN_POINT('',(-48.9807015307821,35.3510917648532,3.64303198860287));
#226787=CARTESIAN_POINT('',(-49.0404538064756,35.394504333373,3.64303198860286));
#226788=CARTESIAN_POINT('',(-49.0826686475736,35.4251752107437,3.42473028058505));
#226789=CARTESIAN_POINT('',(-48.980701531218,35.3510917642533,3.64303198860286));
#226790=CARTESIAN_POINT('',(-49.3496120513051,35.6191209461251,3.23423028058506));
#226791=CARTESIAN_POINT('Origin',(-49.3258045171776,35.6018243948123,3.56425743004168));
#226792=CARTESIAN_POINT('',(-49.4719419865735,35.7079988465457,3.23423028058506));
#226793=CARTESIAN_POINT('',(-49.4723697227349,35.7083096150578,3.23423028058506));
#226794=CARTESIAN_POINT('',(-49.7388853330813,35.9019445403517,3.42473028058508));
#226795=CARTESIAN_POINT('Origin',(-49.4957512585782,35.7252979297064,3.56425912917766));
#226796=CARTESIAN_POINT('',(-49.8408524068606,35.9760279559086,3.64303198860287));
#226797=CARTESIAN_POINT('',(-49.7388853330813,35.9019445403517,3.42473028058508));
#226798=CARTESIAN_POINT('',(-50.1659970864927,36.2122593934161,3.64303198860287));
#226799=CARTESIAN_POINT('Origin',(-50.3626567888877,29.2968639067301,2.65878198860282));
#226800=CARTESIAN_POINT('',(-51.1278468659049,29.501078514911,2.65878198860282));
#226801=CARTESIAN_POINT('',(-54.4342359163065,31.410023123206,2.65878198860283));
#226802=CARTESIAN_POINT('',(-50.4655267888877,29.1186878401555,2.65878198860282));
#226803=CARTESIAN_POINT('',(-54.4189959163065,31.4364195775134,2.65878198860283));
#226804=CARTESIAN_POINT('Origin',(7.92193830068373E-17,1.9061709556272E-13,
2.65878198860263));
#226805=CARTESIAN_POINT('',(-51.1126068659049,29.5274749692184,2.65878198860282));
#226806=CARTESIAN_POINT('',(-51.0513762321546,29.49212344634,2.65878198860282));
#226807=CARTESIAN_POINT('Origin',(3.27798830811897E-16,1.90728868982564E-13,
2.65878198860263));
#226808=CARTESIAN_POINT('Origin',(0.095249999999999,0.164977839420847,42.7590319886026));
#226809=CARTESIAN_POINT('',(-51.8694703131948,30.1668231006073,3.64303198860283));
#226810=CARTESIAN_POINT('',(-51.4963740054945,29.9514158469229,3.4042309748333));
#226811=CARTESIAN_POINT('Origin',(-51.8363612768229,30.1477075895454,3.20400220531979));
#226812=CARTESIAN_POINT('',(-51.1878102690446,29.7732664900073,2.83404198860282));
#226813=CARTESIAN_POINT('',(-51.4963740054945,29.9514158469229,3.4042309748333));
#226814=CARTESIAN_POINT('',(-54.167102037244,31.4933613949858,2.83404198860283));
#226815=CARTESIAN_POINT('',(-54.3920835619873,31.623254538859,2.83404198860283));
#226816=CARTESIAN_POINT('',(-53.8585387246954,31.3152122841228,3.40423097483331));
#226817=CARTESIAN_POINT('',(-54.167102037244,31.4933613949858,2.83404198860283));
#226818=CARTESIAN_POINT('',(-53.4854427993288,31.0998052504798,3.64303198860284));
#226819=CARTESIAN_POINT('Origin',(-53.5185519423381,31.1189208231089,3.20400259788301));
#226820=CARTESIAN_POINT('',(-53.1378379187908,30.8991154799513,3.64303198860283));
#226821=CARTESIAN_POINT('',(0.0952500000000046,0.16497783942112,3.64303198860263));
#226822=CARTESIAN_POINT('',(-53.0286856060847,30.8360963620061,3.42473028058505));
#226823=CARTESIAN_POINT('',(-53.1378379191466,30.899115479335,3.64303198860283));
#226824=CARTESIAN_POINT('',(-52.7429317578289,30.6711163007936,3.23423028058502));
#226825=CARTESIAN_POINT('Origin',(-52.7684169058678,30.6858295650768,3.56425722717264));
#226826=CARTESIAN_POINT('',(-52.6119816883961,30.5955122429562,3.23423028058502));
#226827=CARTESIAN_POINT('',(0.0952500000000046,0.164977839421123,3.23423028058481));
#226828=CARTESIAN_POINT('',(-52.3262277788843,30.4305321463775,3.42473028058501));
#226829=CARTESIAN_POINT('Origin',(-52.5864945348658,30.5807966351507,3.56425909741258));
#226830=CARTESIAN_POINT('',(-52.2170754202458,30.3675130027349,3.64303198860282));
#226831=CARTESIAN_POINT('',(-52.3262277788843,30.4305321463775,3.42473028058501));
#226832=CARTESIAN_POINT('',(0.0952500000000046,0.16497783942112,3.64303198860263));
#226833=CARTESIAN_POINT('Origin',(-0.095249999999999,-0.164977839421025,
42.7590319886026));
#226834=CARTESIAN_POINT('',(-53.6759427993288,30.769849571638,3.64303198860283));
#226835=CARTESIAN_POINT('',(-54.0490387249981,30.9852566047567,3.40423097483331));
#226836=CARTESIAN_POINT('Origin',(-53.7090519420892,30.7889651441233,3.20400259735861));
#226837=CARTESIAN_POINT('',(-54.3576020374704,31.1634057157518,2.83404198860283));
#226838=CARTESIAN_POINT('',(-54.0490387249981,30.9852566047567,3.40423097483331));
#226839=CARTESIAN_POINT('',(-51.3783102687787,29.443310811626,2.83404198860281));
#226840=CARTESIAN_POINT('',(-0.0952499999999886,-0.164977839420749,2.83404198860262));
#226841=CARTESIAN_POINT('',(-51.6868740051411,29.621460168693,3.4042309748333));
#226842=CARTESIAN_POINT('',(-51.3783102687787,29.443310811626,2.83404198860281));
#226843=CARTESIAN_POINT('',(-52.0599703131948,29.8368674217655,3.64303198860283));
#226844=CARTESIAN_POINT('Origin',(-52.0268612765603,29.817751910552,3.20400220587313));
#226845=CARTESIAN_POINT('',(-52.407575419875,30.0375573245353,3.64303198860283));
#226846=CARTESIAN_POINT('',(-52.4715382154241,30.0744862609074,3.64303198860283));
#226847=CARTESIAN_POINT('',(-52.5167277788843,30.1005764675357,3.42473028058501));
#226848=CARTESIAN_POINT('',(-52.4075754202458,30.0375573238931,3.64303198860283));
#226849=CARTESIAN_POINT('',(-52.8024816883961,30.2655565641143,3.23423028058502));
#226850=CARTESIAN_POINT('Origin',(-52.776996592507,30.2508433300782,3.56425743005036));
#226851=CARTESIAN_POINT('',(-52.9334317578289,30.3411606219517,3.23423028058502));
#226852=CARTESIAN_POINT('',(-52.9338896349619,30.3414249774377,3.23423028058502));
#226853=CARTESIAN_POINT('',(-53.2191856060847,30.5061406831642,3.42473028058504));
#226854=CARTESIAN_POINT('Origin',(-52.9589188467298,30.3558761923111,3.56425912917622));
#226855=CARTESIAN_POINT('',(-53.3283379191466,30.5691598004931,3.64303198860283));
#226856=CARTESIAN_POINT('',(-53.2191856060847,30.5061406831642,3.42473028058504));
#226857=CARTESIAN_POINT('',(-53.6763943313415,30.770110263767,3.64303198860283));
#226858=CARTESIAN_POINT('Origin',(-53.1491210481985,23.8720415006489,2.65878198860278));
#226859=CARTESIAN_POINT('',(-53.9314655730806,23.9951532569806,2.65878198860278));
#226860=CARTESIAN_POINT('',(-57.419280924679,25.5480287005717,2.65878198860279));
#226861=CARTESIAN_POINT('',(-53.2328030451449,23.6840886581935,2.65878198860278));
#226862=CARTESIAN_POINT('',(-57.4068835917981,25.5758735661207,2.65878198860279));
#226863=CARTESIAN_POINT('Origin',(8.62051087089598E-17,1.90630805821371E-13,
2.65878198860263));
#226864=CARTESIAN_POINT('',(-53.9190682401996,24.0229981225296,2.65878198860278));
#226865=CARTESIAN_POINT('',(-53.854477793907,23.9942406030432,2.65878198860278));
#226866=CARTESIAN_POINT('Origin',(3.24161598652235E-16,1.90721730512516E-13,
2.65878198860263));
#226867=CARTESIAN_POINT('Origin',(0.0774833305059389,0.174030409680827,
42.7590319886026));
#226868=CARTESIAN_POINT('',(-54.7386155880005,24.57973006491,3.64303198860279));
#226869=CARTESIAN_POINT('',(-54.3450469517071,24.4045020183944,3.40423097483326));
#226870=CARTESIAN_POINT('Origin',(-54.7036898113995,24.5641801073105,3.20400220531701));
#226871=CARTESIAN_POINT('',(-54.0195518811806,24.2595822754873,2.83404198860278));
#226872=CARTESIAN_POINT('',(-54.3450469517071,24.4045020183944,3.40423097483326));
#226873=CARTESIAN_POINT('',(-57.1623216544373,25.658833530444,2.83404198860279));
#226874=CARTESIAN_POINT('',(-57.3996482375658,25.7644981330391,2.83404198860279));
#226875=CARTESIAN_POINT('',(-56.8368270312095,25.5139139879314,3.40423097483327));
#226876=CARTESIAN_POINT('',(-57.1623216544372,25.658833530444,2.83404198860279));
#226877=CARTESIAN_POINT('',(-56.4432587981558,25.3386861202876,3.6430319886028));
#226878=CARTESIAN_POINT('Origin',(-56.4781846872464,25.3542361279706,3.20400259788151));
#226879=CARTESIAN_POINT('',(-56.076580340217,25.1754303533075,3.6430319886028));
#226880=CARTESIAN_POINT('',(0.0774833305059444,0.1740304096811,3.64303198860263));
#226881=CARTESIAN_POINT('',(-55.9614386837454,25.1241659841934,3.42473028058502));
#226882=CARTESIAN_POINT('',(-56.0765803405064,25.1754303526574,3.64303198860279));
#226883=CARTESIAN_POINT('',(-55.6600051127009,24.9899591116494,3.23423028058498));
#226884=CARTESIAN_POINT('Origin',(-55.6868886053398,25.0019278517718,3.56425722716828));
#226885=CARTESIAN_POINT('',(-55.5218696254674,24.928457230274,3.23423028058498));
#226886=CARTESIAN_POINT('',(0.0774833305059445,0.174030409681103,3.23423028058481));
#226887=CARTESIAN_POINT('',(-55.2204359898058,24.7942503289606,3.42473028058497));
#226888=CARTESIAN_POINT('Origin',(-55.49498389336,24.916486369099,3.56425909741029));
#226889=CARTESIAN_POINT('',(-55.1052942849673,24.7429859390912,3.64303198860279));
#226890=CARTESIAN_POINT('',(-55.2204359898058,24.7942503289606,3.42473028058497));
#226891=CARTESIAN_POINT('',(0.0774833305059444,0.1740304096811,3.64303198860263));
#226892=CARTESIAN_POINT('Origin',(-0.0774833305059389,-0.174030409681005,
42.7590319886026));
#226893=CARTESIAN_POINT('',(-56.5982254591677,24.9906253009257,3.64303198860279));
#226894=CARTESIAN_POINT('',(-56.9917936924674,25.165853168017,3.40423097483327));
#226895=CARTESIAN_POINT('Origin',(-56.6331513479964,25.0061753084922,3.20400259735894));
#226896=CARTESIAN_POINT('',(-57.317288315633,25.3107727106691,2.83404198860279));
#226897=CARTESIAN_POINT('',(-56.9917936924674,25.165853168017,3.40423097483326));
#226898=CARTESIAN_POINT('',(-54.1745185419761,23.9115214566113,2.83404198860277));
#226899=CARTESIAN_POINT('',(-0.0774833305059281,-0.174030409680729,2.83404198860262));
#226900=CARTESIAN_POINT('',(-54.5000136124314,24.0564411996785,3.40423097483327));
#226901=CARTESIAN_POINT('',(-54.1745185419761,23.9115214566113,2.83404198860278));
#226902=CARTESIAN_POINT('',(-54.8935822490124,24.2316692455482,3.64303198860279));
#226903=CARTESIAN_POINT('Origin',(-54.8586564721335,24.216119287825,3.2040022058723));
#226904=CARTESIAN_POINT('',(-55.2602609456777,24.3949251204066,3.64303198860279));
#226905=CARTESIAN_POINT('',(-55.3277334713091,24.4249658234765,3.64303198860279));
#226906=CARTESIAN_POINT('',(-55.3754026508176,24.4461895095988,3.42473028058497));
#226907=CARTESIAN_POINT('',(-55.2602609459792,24.3949251197294,3.64303198860279));
#226908=CARTESIAN_POINT('',(-55.6768362864793,24.5803964109122,3.23423028058498));
#226909=CARTESIAN_POINT('Origin',(-55.6499528488641,24.5684276954192,3.56425743004096));
#226910=CARTESIAN_POINT('',(-55.8149717737128,24.6418982922876,3.23423028058498));
#226911=CARTESIAN_POINT('',(-55.8154547752196,24.6421133384135,3.23423028058498));
#226912=CARTESIAN_POINT('',(-56.1164053447573,24.7761051648316,3.424730280585));
#226913=CARTESIAN_POINT('Origin',(-55.8418574376303,24.6538691229771,3.56425912917466));
#226914=CARTESIAN_POINT('',(-56.2315470015183,24.8273695332955,3.64303198860279));
#226915=CARTESIAN_POINT('',(-56.1164053447573,24.7761051648316,3.424730280585));
#226916=CARTESIAN_POINT('',(-56.5987017673884,24.9908373670086,3.64303198860279));
#226917=CARTESIAN_POINT('Origin',(-55.3532724151366,18.1856720123407,2.65878198860274));
#226918=CARTESIAN_POINT('',(-56.1441998575528,18.2263320786581,2.65878198860274));
#226919=CARTESIAN_POINT('',(-59.7752282754838,19.4061247292252,2.65878198860275));
#226920=CARTESIAN_POINT('',(-55.4168495715593,17.9900016446781,2.65878198860274));
#226921=CARTESIAN_POINT('',(-59.7658094374952,19.4351129318419,2.65878198860275));
#226922=CARTESIAN_POINT('Origin',(9.17194536069053E-17,1.90645171180964E-13,
2.65878198860263));
#226923=CARTESIAN_POINT('',(-56.1347810195643,18.2553202812748,2.65878198860274));
#226924=CARTESIAN_POINT('',(-56.0675384271754,18.2334718385818,2.65878198860274));
#226925=CARTESIAN_POINT('Origin',(3.21290464935061E-16,1.90714250953466E-13,
2.65878198860263));
#226926=CARTESIAN_POINT('Origin',(0.0588677374284264,0.181176266354138,
42.7590319886026));
#226927=CARTESIAN_POINT('',(-57.0080331356323,18.7233363629823,3.64303198860275));
#226928=CARTESIAN_POINT('',(-56.5983041910847,18.5902073587821,3.40423097483322));
#226929=CARTESIAN_POINT('Origin',(-56.9716732729175,18.7115223274339,3.204002205318));
#226930=CARTESIAN_POINT('',(-56.2594439785882,18.4801050009135,2.83404198860274));
#226931=CARTESIAN_POINT('',(-56.5983041910847,18.5902073587821,3.40423097483322));
#226932=CARTESIAN_POINT('',(-59.5312589135997,19.5431821162865,2.83404198860274));
#226933=CARTESIAN_POINT('',(-59.778330355405,19.6234604941057,2.83404198860274));
#226934=CARTESIAN_POINT('',(-59.1923991668985,19.4330799109595,3.40423097483322));
#226935=CARTESIAN_POINT('',(-59.5312589135997,19.5431821162865,2.83404198860274));
#226936=CARTESIAN_POINT('',(-58.7826706420789,19.2999510425005,3.64303198860276));
#226937=CARTESIAN_POINT('Origin',(-58.8190306219021,19.3117651160996,3.20400259788237));
#226938=CARTESIAN_POINT('',(-58.4009360126568,19.1759179434156,3.64303198860275));
#226939=CARTESIAN_POINT('',(0.0588677374284319,0.181176266354411,3.64303198860263));
#226940=CARTESIAN_POINT('',(-58.2810665285031,19.1369699862882,3.42473028058497));
#226941=CARTESIAN_POINT('',(-58.4009360128768,19.1759179427385,3.64303198860275));
#226942=CARTESIAN_POINT('',(-57.9672558039533,19.0350067009929,3.23423028058494));
#226943=CARTESIAN_POINT('Origin',(-57.9952431000166,19.044099784931,3.56425722717267));
#226944=CARTESIAN_POINT('',(-57.823448340224,18.9882808235619,3.23423028058494));
#226945=CARTESIAN_POINT('',(0.0588677374284319,0.181176266354414,3.23423028058481));
#226946=CARTESIAN_POINT('',(-57.5096375484038,18.8863175164091,3.42473028058494));
#226947=CARTESIAN_POINT('Origin',(-57.7954585952457,18.9791858642774,3.56425909740675));
#226948=CARTESIAN_POINT('',(-57.3897680139785,18.8473695436961,3.64303198860275));
#226949=CARTESIAN_POINT('',(-57.5096375484038,18.8863175164091,3.42473028058494));
#226950=CARTESIAN_POINT('',(0.0588677374284319,0.181176266354411,3.64303198860263));
#226951=CARTESIAN_POINT('Origin',(-0.0588677374284264,-0.181176266354316,
42.7590319886026));
#226952=CARTESIAN_POINT('',(-58.9004061169358,18.937598509792,3.64303198860275));
#226953=CARTESIAN_POINT('',(-59.3101346419425,19.0707273776751,3.40423097483323));
#226954=CARTESIAN_POINT('Origin',(-58.9367660964859,18.9494125833024,3.20400259735869));
#226955=CARTESIAN_POINT('',(-59.6489943885963,19.1808295831477,2.83404198860274));
#226956=CARTESIAN_POINT('',(-59.3101346419425,19.0707273776751,3.40423097483323));
#226957=CARTESIAN_POINT('',(-56.3771794532808,18.1177524687105,2.83404198860273));
#226958=CARTESIAN_POINT('',(-0.0588677374284154,-0.181176266354039,2.83404198860262));
#226959=CARTESIAN_POINT('',(-56.7160396657233,18.2278548267451,3.40423097483323));
#226960=CARTESIAN_POINT('',(-56.3771794532808,18.1177524687105,2.83404198860274));
#226961=CARTESIAN_POINT('',(-57.1257686104892,18.3609838302738,3.64303198860275));
#226962=CARTESIAN_POINT('Origin',(-57.0894087474844,18.3491697946313,3.20400220587492));
#226963=CARTESIAN_POINT('',(-57.5075034886063,18.4850170116926,3.64303198860275));
#226964=CARTESIAN_POINT('',(-57.57774650121,18.5078403492308,3.64303198860275));
#226965=CARTESIAN_POINT('',(-57.6273730232606,18.5239649837006,3.42473028058492));
#226966=CARTESIAN_POINT('',(-57.5075034888354,18.4850170109876,3.64303198860275));
#226967=CARTESIAN_POINT('',(-57.9411838150808,18.6259282908535,3.23423028058494));
#226968=CARTESIAN_POINT('Origin',(-57.913196576314,18.6168352256581,3.56425743004465));
#226969=CARTESIAN_POINT('',(-58.0849912788101,18.6726541682844,3.23423028058494));
#226970=CARTESIAN_POINT('',(-58.0854941128252,18.6728175489599,3.23423028058494));
#226971=CARTESIAN_POINT('',(-58.3988020033599,18.7746174535798,3.42473028058496));
#226972=CARTESIAN_POINT('Origin',(-58.1129809527837,18.6817491043776,3.56425912917502));
#226973=CARTESIAN_POINT('',(-58.5186714877337,18.8135654100301,3.64303198860275));
#226974=CARTESIAN_POINT('',(-58.3988020033599,18.7746174535798,3.42473028058496));
#226975=CARTESIAN_POINT('',(-58.900901982832,18.9377596263884,3.64303198860275));
#226976=CARTESIAN_POINT('Origin',(-56.9509617460775,12.3000564958688,2.6587819886027));
#226977=CARTESIAN_POINT('',(-57.7418065394567,12.2578193919766,2.6587819886027));
#226978=CARTESIAN_POINT('',(-61.4762657165316,13.0516031943527,2.6587819886027));
#226979=CARTESIAN_POINT('',(-56.9937374973464,12.0988124084938,2.6587819886027));
#226980=CARTESIAN_POINT('',(-61.4699285681955,13.081417133223,2.6587819886027));
#226981=CARTESIAN_POINT('Origin',(9.57020013840216E-17,1.90660034251612E-13,
2.65878198860263));
#226982=CARTESIAN_POINT('',(-57.7354693911205,12.2876333308469,2.6587819886027));
#226983=CARTESIAN_POINT('',(-57.6663113765489,12.2729333410577,2.6587819886027));
#226984=CARTESIAN_POINT('Origin',(3.19216886402203E-16,1.90706512253028E-13,
2.65878198860263));
#226985=CARTESIAN_POINT('Origin',(0.039607177100782,0.186337117939701,42.7590319886026));
#226986=CARTESIAN_POINT('',(-58.6528587425323,12.6618058697518,3.64303198860271));
#226987=CARTESIAN_POINT('',(-58.2314585657881,12.5722344970959,3.40423097483318));
#226988=CARTESIAN_POINT('Origin',(-58.6154631599687,12.6538571933004,3.20400220531852));
#226989=CARTESIAN_POINT('',(-57.882945834721,12.4981558287389,2.83404198860269));
#226990=CARTESIAN_POINT('',(-58.2314585657881,12.5722344970959,3.40423097483318));
#226991=CARTESIAN_POINT('',(-61.2479592423879,13.2134115091892,2.8340419886027));
#226992=CARTESIAN_POINT('',(-61.5020685764505,13.2674241155258,2.8340419886027));
#226993=CARTESIAN_POINT('',(-60.8994469905094,13.139332943849,3.40423097483318));
#226994=CARTESIAN_POINT('',(-61.2479592423878,13.2134115091892,2.8340419886027));
#226995=CARTESIAN_POINT('',(-60.4780472453828,13.0497616623173,3.64303198860271));
#226996=CARTESIAN_POINT('Origin',(-60.5154429483887,13.0577103643695,3.2040025978796));
#226997=CARTESIAN_POINT('',(-60.0854388089606,12.9663101637162,3.64303198860271));
#226998=CARTESIAN_POINT('',(0.0396071771007875,0.186337117939974,3.64303198860263));
#226999=CARTESIAN_POINT('',(-59.9621548122772,12.9401053405448,3.42473028058494));
#227000=CARTESIAN_POINT('',(-60.0854388091086,12.9663101630202,3.64303198860271));
#227001=CARTESIAN_POINT('',(-59.6394051101894,12.871502773589,3.2342302805849));
#227002=CARTESIAN_POINT('Origin',(-59.6681895750092,12.8776205756138,3.56425722716818));
#227003=CARTESIAN_POINT('',(-59.4915012546306,12.8400648385937,3.2342302805849));
#227004=CARTESIAN_POINT('',(0.0396071771007876,0.186337117939977,3.23423028058482));
#227005=CARTESIAN_POINT('',(-59.1687514833561,12.7714622569318,3.42473028058489));
#227006=CARTESIAN_POINT('Origin',(-59.46271415829,12.8339454274783,3.56425909741383));
#227007=CARTESIAN_POINT('',(-59.0454674350475,12.7452574235145,3.64303198860271));
#227008=CARTESIAN_POINT('',(-59.1687514833561,12.7714622569318,3.42473028058489));
#227009=CARTESIAN_POINT('',(0.0396071771007875,0.186337117939974,3.64303198860263));
#227010=CARTESIAN_POINT('Origin',(-0.039607177100782,-0.18633711793988,
42.7590319886026));
#227011=CARTESIAN_POINT('',(-60.5572615995844,12.6770874264377,3.64303198860271));
#227012=CARTESIAN_POINT('',(-60.9786613448368,12.7666587073772,3.40423097483318));
#227013=CARTESIAN_POINT('Origin',(-60.5946573023108,12.6850361284305,3.20400259735845));
#227014=CARTESIAN_POINT('',(-61.3271735966834,12.8407372728673,2.83404198860269));
#227015=CARTESIAN_POINT('',(-60.9786613448368,12.7666587073772,3.40423097483318));
#227016=CARTESIAN_POINT('',(-57.9621601888121,12.125481593379,2.83404198860269));
#227017=CARTESIAN_POINT('',(-0.0396071771007709,-0.186337117939602,2.83404198860262));
#227018=CARTESIAN_POINT('',(-58.3106729198428,12.1995602619073,3.40423097483318));
#227019=CARTESIAN_POINT('',(-57.9621601888121,12.125481593379,2.8340419886027));
#227020=CARTESIAN_POINT('',(-58.7320730967339,12.2891316338722,3.64303198860271));
#227021=CARTESIAN_POINT('Origin',(-58.6946775138721,12.2811829573574,3.2040022058751));
#227022=CARTESIAN_POINT('',(-59.1246817890948,12.3725831883607,3.6430319886027));
#227023=CARTESIAN_POINT('',(-59.1969256915255,12.3879391031045,3.64303198860271));
#227024=CARTESIAN_POINT('',(-59.2479658375577,12.3987880210522,3.42473028058489));
#227025=CARTESIAN_POINT('',(-59.1246817892491,12.372583187635,3.6430319886027));
#227026=CARTESIAN_POINT('',(-59.5707156088321,12.4673906027141,3.23423028058489));
#227027=CARTESIAN_POINT('Origin',(-59.5419312029586,12.4612728133412,3.5642574300495));
#227028=CARTESIAN_POINT('',(-59.718619464391,12.4988285377094,3.23423028058489));
#227029=CARTESIAN_POINT('',(-59.7191366217597,12.4989384629015,3.23423028058489));
#227030=CARTESIAN_POINT('',(-60.0413691664788,12.5674311046652,3.42473028058491));
#227031=CARTESIAN_POINT('Origin',(-59.7474064876925,12.5049479331827,3.56425912918016));
#227032=CARTESIAN_POINT('',(-60.1646531633101,12.5936359271406,3.64303198860271));
#227033=CARTESIAN_POINT('',(-60.0413691664788,12.5674311046652,3.42473028058491));
#227034=CARTESIAN_POINT('',(-60.5577715903455,12.6771958283204,3.64303198860271));
#227035=CARTESIAN_POINT('Origin',(-57.9246844223735,6.27967898647588,2.65878198860266));
#227036=CARTESIAN_POINT('',(-58.7067819056643,6.15500747092296,2.65878198860266));
#227037=CARTESIAN_POINT('',(-62.5037563256535,6.55408556365924,2.65878198860266));
#227038=CARTESIAN_POINT('',(-57.9461901084062,6.07506605172281,2.65878198860265));
#227039=CARTESIAN_POINT('',(-62.5005702980931,6.58439859103007,2.65878198860266));
#227040=CARTESIAN_POINT('Origin',(9.81091184134694E-17,1.90675232190402E-13,
2.65878198860263));
#227041=CARTESIAN_POINT('',(-58.7035958781039,6.18532049829379,2.65878198860266));
#227042=CARTESIAN_POINT('',(-58.6332801510296,6.17793001757249,2.65878198860266));
#227043=CARTESIAN_POINT('Origin',(3.17963581613999E-16,1.90698599198023E-13,
2.65878198860263));
#227044=CARTESIAN_POINT('Origin',(0.0199126722524868,0.189456421067567,
42.7590319886026));
#227045=CARTESIAN_POINT('',(-59.6550713551493,6.46154998175898,3.64303198860266));
#227046=CARTESIAN_POINT('',(-59.2266168947286,6.4165176033503,3.40423097483314));
#227047=CARTESIAN_POINT('Origin',(-59.6170497665662,6.45755375176737,3.20400220531682));
#227048=CARTESIAN_POINT('',(-58.8722700235037,6.37927424589668,2.83404198860265));
#227049=CARTESIAN_POINT('',(-59.2266168947286,6.4165176033503,3.40423097483314));
#227050=CARTESIAN_POINT('',(-62.293614112757,6.73887200051311,2.83404198860265));
#227051=CARTESIAN_POINT('',(-62.5519772640372,6.76602706194925,2.83404198860265));
#227052=CARTESIAN_POINT('',(-61.9392677288637,6.70162869542366,3.40423097483313));
#227053=CARTESIAN_POINT('',(-62.293614112757,6.73887200051311,2.83404198860265));
#227054=CARTESIAN_POINT('',(-61.5108137072212,6.65659636252362,3.64303198860267));
#227055=CARTESIAN_POINT('Origin',(-61.548835418265,6.66059260538636,3.20400259788154));
#227056=CARTESIAN_POINT('',(-61.1116329639869,6.61464077648907,3.64303198860266));
#227057=CARTESIAN_POINT('',(0.0199126722524923,0.18945642106784,3.64303198860263));
#227058=CARTESIAN_POINT('',(-60.9862851800405,6.60146619279925,3.42473028058489));
#227059=CARTESIAN_POINT('',(-61.1116329640613,6.61464077578101,3.64303198860266));
#227060=CARTESIAN_POINT('',(-60.6581326136904,6.56697596826257,3.23423028058485));
#227061=CARTESIAN_POINT('Origin',(-60.687398878641,6.57005146045385,3.56425722717401));
#227062=CARTESIAN_POINT('',(-60.5077528318944,6.55117041629748,3.23423028058485));
#227063=CARTESIAN_POINT('',(0.0199126722524923,0.189456421067843,3.23423028058482));
#227064=CARTESIAN_POINT('',(-60.1796001951996,6.51668018436725,3.42473028058484));
#227065=CARTESIAN_POINT('Origin',(-60.4784837816376,6.5480935988987,3.56425909740982));
#227066=CARTESIAN_POINT('',(-60.0542523588397,6.50350559588444,3.64303198860266));
#227067=CARTESIAN_POINT('',(-60.1796001951996,6.51668018436725,3.42473028058484));
#227068=CARTESIAN_POINT('',(0.0199126722524923,0.18945642106784,3.64303198860263));
#227069=CARTESIAN_POINT('Origin',(-0.0199126722524868,-0.189456421067745,
42.7590319886026));
#227070=CARTESIAN_POINT('',(-61.5506390517262,6.27768352038831,3.64303198860266));
#227071=CARTESIAN_POINT('',(-61.9790930734319,6.32271585268618,3.40423097483313));
#227072=CARTESIAN_POINT('Origin',(-61.5886607624842,6.28167976322102,3.20400259735761));
#227073=CARTESIAN_POINT('',(-62.3334394573092,6.35995915792815,2.83404198860265));
#227074=CARTESIAN_POINT('',(-61.9790930734319,6.32271585268619,3.40423097483313));
#227075=CARTESIAN_POINT('',(-58.9120953679531,6.00036140429027,2.83404198860265));
#227076=CARTESIAN_POINT('',(-0.0199126722524756,-0.189456421067467,2.83404198860262));
#227077=CARTESIAN_POINT('',(-59.2664422391598,6.03760476191725,3.40423097483313));
#227078=CARTESIAN_POINT('',(-58.912095367953,6.00036140429027,2.83404198860265));
#227079=CARTESIAN_POINT('',(-59.6948966996543,6.08263713962367,3.64303198860266));
#227080=CARTESIAN_POINT('Origin',(-59.6568751107688,6.07864090960027,3.20400220587169));
#227081=CARTESIAN_POINT('',(-60.0940777032672,6.12459275448651,3.64303198860266));
#227082=CARTESIAN_POINT('',(-60.1675309762115,6.13231300382155,3.64303198860266));
#227083=CARTESIAN_POINT('',(-60.2194255397045,6.13776734223194,3.42473028058484));
#227084=CARTESIAN_POINT('',(-60.0940777033447,6.12459275374913,3.64303198860266));
#227085=CARTESIAN_POINT('',(-60.5475781763994,6.17225757416217,3.23423028058485));
#227086=CARTESIAN_POINT('Origin',(-60.518311971389,6.16918208839134,3.56425743004515));
#227087=CARTESIAN_POINT('',(-60.6979579581954,6.18806312612726,3.23423028058485));
#227088=CARTESIAN_POINT('',(-60.6984837728333,6.18811839147267,3.23423028058485));
#227089=CARTESIAN_POINT('',(-61.0261105245454,6.22255335066394,3.42473028058488));
#227090=CARTESIAN_POINT('Origin',(-60.7272269341761,6.19113993560407,3.56425912918035));
#227091=CARTESIAN_POINT('',(-61.1514583085663,6.2357279336457,3.64303198860266));
#227092=CARTESIAN_POINT('',(-61.0261105245454,6.22255335066394,3.42473028058488));
#227093=CARTESIAN_POINT('',(-61.5511575797868,6.27773801988358,3.64303198860266));
#227094=CARTESIAN_POINT('Origin',(-58.2637721346185,0.190500000000191,2.65878198860262));
#227095=CARTESIAN_POINT('',(-58.2637721346185,-0.0152399999998093,2.65878198860261));
#227096=CARTESIAN_POINT('',(-58.9578504383728,0.0152400000001907,2.65878198860261));
#227097=CARTESIAN_POINT('Origin',(0.,0.190499999999911,42.7590319886026));
#227098=CARTESIAN_POINT('',(-60.0036905223731,0.190500000000184,3.64303198860262));
#227099=CARTESIAN_POINT('',(-59.5728760150042,0.190500000000185,3.4042309748331));
#227100=CARTESIAN_POINT('Origin',(-59.9654595002501,0.190500000000187,3.20400220531729));
#227101=CARTESIAN_POINT('',(-59.2165773020941,0.190499999468791,2.8340419886026));
#227102=CARTESIAN_POINT('',(-59.5728760150042,0.190500000000186,3.4042309748331));
#227103=CARTESIAN_POINT('',(-62.6567671111299,0.190500000000188,2.8340419886026));
#227104=CARTESIAN_POINT('',(-62.9165533988763,0.19050000000019,2.83404198860261));
#227105=CARTESIAN_POINT('',(-62.3004688883554,0.190500000605476,3.40423097483309));
#227106=CARTESIAN_POINT('',(-62.6567671111299,0.19050000000019,2.83404198860261));
#227107=CARTESIAN_POINT('',(-61.8696548221181,0.190500000000184,3.64303198860263));
#227108=CARTESIAN_POINT('Origin',(-61.9078859673764,0.190500000000187,3.20400259788294));
#227109=CARTESIAN_POINT('',(-61.4682752798284,0.190500000712183,3.64303198860261));
#227110=CARTESIAN_POINT('',(5.50819412990574E-15,0.190500000000184,3.64303198860262));
#227111=CARTESIAN_POINT('',(-61.3422370451705,0.190500000000185,3.42473028058485));
#227112=CARTESIAN_POINT('',(-61.4682752798284,0.190500000000184,3.64303198860261));
#227113=CARTESIAN_POINT('',(-61.0122769227456,0.190500000000187,3.23423028058481));
#227114=CARTESIAN_POINT('Origin',(-61.0417043405097,0.190499486622583,3.56425722716956));
#227115=CARTESIAN_POINT('',(-60.8610688070707,0.190500000000187,3.23423028058481));
#227116=CARTESIAN_POINT('',(5.56576032196012E-15,0.190500000000187,3.23423028058482));
#227117=CARTESIAN_POINT('',(-60.5311086139135,0.190500000000185,3.4247302805848));
#227118=CARTESIAN_POINT('Origin',(-60.8316384807435,0.190499486573693,3.56425909741752));
#227119=CARTESIAN_POINT('',(-60.4050703266282,0.190500000000184,3.64303198860261));
#227120=CARTESIAN_POINT('',(-60.5311086139135,0.190500000000185,3.4247302805848));
#227121=CARTESIAN_POINT('',(5.50819412990574E-15,0.190500000000184,3.64303198860263));
#227122=CARTESIAN_POINT('Origin',(0.,-0.190500000000089,42.7590319886026));
#227123=CARTESIAN_POINT('',(-61.8696548221181,-0.190499999999816,3.64303198860261));
#227124=CARTESIAN_POINT('',(-62.3004688883554,-0.190499999999815,3.40423097483308));
#227125=CARTESIAN_POINT('Origin',(-61.9078859670883,-0.190499999999813,
3.20400259735739));
#227126=CARTESIAN_POINT('',(-62.6567671111299,-0.190500000452382,2.8340419886026));
#227127=CARTESIAN_POINT('',(-62.3004688883554,-0.190499999999814,3.40423097483308));
#227128=CARTESIAN_POINT('',(-59.2165773020941,-0.190499999999811,2.83404198860261));
#227129=CARTESIAN_POINT('',(1.12442271988212E-14,-0.190499999999811,2.83404198860262));
#227130=CARTESIAN_POINT('',(-59.5728760150042,-0.190499999293226,3.4042309748331));
#227131=CARTESIAN_POINT('',(-59.2165773020941,-0.190499999999811,2.83404198860261));
#227132=CARTESIAN_POINT('',(-60.003690522373,-0.190499999999816,3.64303198860261));
#227133=CARTESIAN_POINT('Origin',(-59.9654594999467,-0.190499999999813,
3.20400220587133));
#227134=CARTESIAN_POINT('',(-60.4050703266283,-0.190499999257704,3.64303198860261));
#227135=CARTESIAN_POINT('',(-60.4789282006568,-0.190499999999816,3.64303198860261));
#227136=CARTESIAN_POINT('',(-60.5311086139135,-0.190499999999815,3.42473028058479));
#227137=CARTESIAN_POINT('',(-60.4050703266282,-0.190499999999816,3.64303198860261));
#227138=CARTESIAN_POINT('',(-60.8610688070707,-0.190499999999813,3.2342302805848));
#227139=CARTESIAN_POINT('Origin',(-60.8316414495926,-0.190499486502376,
3.56425743004576));
#227140=CARTESIAN_POINT('',(-61.0122769227456,-0.190499999999813,3.2342302805848));
#227141=CARTESIAN_POINT('',(-61.0128056337175,-0.190499999999813,3.2342302805848));
#227142=CARTESIAN_POINT('',(-61.3422370451705,-0.190499999999815,3.42473028058483));
#227143=CARTESIAN_POINT('Origin',(-61.0417071743823,-0.190499486687921,
3.56425912917566));
#227144=CARTESIAN_POINT('',(-61.4682752798284,-0.190499999999816,3.64303198860261));
#227145=CARTESIAN_POINT('',(-61.3422370451705,-0.190499999999815,3.42473028058483));
#227146=CARTESIAN_POINT('',(-61.8701762063762,-0.190499999999816,3.64303198860261));
#227147=CARTESIAN_POINT('Origin',(-57.9645097668784,-5.90076614434097,2.65878198860257));
#227148=CARTESIAN_POINT('',(-58.7035958781038,-6.1853204982942,2.65878198860257));
#227149=CARTESIAN_POINT('',(-62.500570298093,-6.58439859103053,2.65878198860257));
#227150=CARTESIAN_POINT('',(-57.9430040808457,-6.10537907909404,2.65878198860257));
#227151=CARTESIAN_POINT('',(-62.5037563256534,-6.5540855636597,2.65878198860257));
#227152=CARTESIAN_POINT('Origin',(9.81091184134687E-17,1.90705964780674E-13,
2.65878198860263));
#227153=CARTESIAN_POINT('',(-58.7067819056642,-6.15500747092338,2.65878198860257));
#227154=CARTESIAN_POINT('',(-58.6364661785899,-6.14761699020208,2.65878198860257));
#227155=CARTESIAN_POINT('Origin',(3.17963581613999E-16,1.90682597773053E-13,
2.65878198860263));
#227156=CARTESIAN_POINT('Origin',(-0.0199126722524893,0.189456421067567,
42.7590319886026));
#227157=CARTESIAN_POINT('',(-59.6948966996542,-6.08263713962411,3.64303198860258));
#227158=CARTESIAN_POINT('',(-59.2664422392335,-6.03760476121542,3.40423097483305));
#227159=CARTESIAN_POINT('Origin',(-59.656875111071,-6.07864090963248,3.20400220531675));
#227160=CARTESIAN_POINT('',(-58.9120953678974,-6.0003614048193,2.83404198860256));
#227161=CARTESIAN_POINT('',(-59.2664422392335,-6.03760476121542,3.40423097483305));
#227162=CARTESIAN_POINT('',(-62.3334394572618,-6.35995915837826,2.83404198860256));
#227163=CARTESIAN_POINT('',(-62.5918026085421,-6.3871142198144,2.83404198860256));
#227164=CARTESIAN_POINT('',(-61.9790930734951,-6.32271585208499,3.40423097483306));
#227165=CARTESIAN_POINT('',(-62.3334394572618,-6.35995915837826,2.83404198860256));
#227166=CARTESIAN_POINT('',(-61.5506390517261,-6.27768352038877,3.64303198860258));
#227167=CARTESIAN_POINT('Origin',(-61.5886607627703,-6.28167976325155,3.2040025978822));
#227168=CARTESIAN_POINT('',(-61.1514583086406,-6.23572793293815,3.64303198860257));
#227169=CARTESIAN_POINT('',(-0.0199126722524838,0.18945642106784,3.64303198860263));
#227170=CARTESIAN_POINT('',(-61.0261105245453,-6.22255335066439,3.4247302805848));
#227171=CARTESIAN_POINT('',(-61.1514583085662,-6.23572793364615,3.64303198860257));
#227172=CARTESIAN_POINT('',(-60.6979579581953,-6.1880631261277,3.23423028058476));
#227173=CARTESIAN_POINT('Origin',(-60.7272241158216,-6.19113963944962,3.56425722717282));
#227174=CARTESIAN_POINT('',(-60.5475781763993,-6.17225757416261,3.23423028058476));
#227175=CARTESIAN_POINT('',(-0.0199126722524838,0.189456421067843,3.23423028058482));
#227176=CARTESIAN_POINT('',(-60.2194255397045,-6.13776734223238,3.42473028058475));
#227177=CARTESIAN_POINT('Origin',(-60.5183090188083,-6.16918177799173,3.56425909741148));
#227178=CARTESIAN_POINT('',(-60.0940777033446,-6.12459275374958,3.64303198860258));
#227179=CARTESIAN_POINT('',(-60.2194255397045,-6.13776734223238,3.42473028058475));
#227180=CARTESIAN_POINT('',(-0.0199126722524838,0.18945642106784,3.64303198860263));
#227181=CARTESIAN_POINT('Origin',(0.0199126722524893,-0.189456421067745,
42.7590319886026));
#227182=CARTESIAN_POINT('',(-61.5108137072212,-6.65659636252408,3.64303198860257));
#227183=CARTESIAN_POINT('',(-61.9392677289269,-6.70162869482196,3.40423097483304));
#227184=CARTESIAN_POINT('Origin',(-61.548835417979,-6.66059260535676,3.20400259735693));
#227185=CARTESIAN_POINT('',(-62.2936141127096,-6.73887200096389,2.83404198860256));
#227186=CARTESIAN_POINT('',(-61.9392677289269,-6.70162869482196,3.40423097483304));
#227187=CARTESIAN_POINT('',(-58.872270023448,-6.37927424642599,2.83404198860256));
#227188=CARTESIAN_POINT('',(0.0199126722525006,-0.189456421067466,2.83404198860262));
#227189=CARTESIAN_POINT('',(-59.2266168948024,-6.41651760264851,3.40423097483305));
#227190=CARTESIAN_POINT('',(-58.872270023448,-6.379274246426,2.83404198860256));
#227191=CARTESIAN_POINT('',(-59.6550713551492,-6.46154998175942,3.64303198860257));
#227192=CARTESIAN_POINT('Origin',(-59.6170497662624,-6.45755375173588,3.20400220587399));
#227193=CARTESIAN_POINT('',(-60.0542523589172,-6.50350559514724,3.64303198860257));
#227194=CARTESIAN_POINT('',(-60.1277056317064,-6.51122584595731,3.64303198860257));
#227195=CARTESIAN_POINT('',(-60.1796001951995,-6.51668018436769,3.42473028058476));
#227196=CARTESIAN_POINT('',(-60.0542523588397,-6.50350559588489,3.64303198860257));
#227197=CARTESIAN_POINT('',(-60.5077528318943,-6.55117041629792,3.23423028058476));
#227198=CARTESIAN_POINT('Origin',(-60.4784867342349,-6.54809390915829,3.56425743004616));
#227199=CARTESIAN_POINT('',(-60.6581326136904,-6.56697596826301,3.23423028058476));
#227200=CARTESIAN_POINT('',(-60.6586584283283,-6.56703123360843,3.23423028058476));
#227201=CARTESIAN_POINT('',(-60.9862851800404,-6.60146619279971,3.42473028058479));
#227202=CARTESIAN_POINT('Origin',(-60.6874016969837,-6.57005175674012,3.56425912917731));
#227203=CARTESIAN_POINT('',(-61.1116329640612,-6.61464077578146,3.64303198860257));
#227204=CARTESIAN_POINT('',(-60.9862851800404,-6.60146619279971,3.42473028058479));
#227205=CARTESIAN_POINT('',(-61.5113322352818,-6.65665086201935,3.64303198860257));
#227206=CARTESIAN_POINT('Origin',(-57.0301761002789,-11.9273822599896,2.65878198860253));
#227207=CARTESIAN_POINT('',(-57.7354693911204,-12.2876333308473,2.65878198860253));
#227208=CARTESIAN_POINT('',(-61.4699285681953,-13.0814171332235,2.65878198860252));
#227209=CARTESIAN_POINT('',(-56.9874003490101,-12.1286263473646,2.65878198860253));
#227210=CARTESIAN_POINT('',(-61.4762657165315,-13.0516031943531,2.65878198860252));
#227211=CARTESIAN_POINT('Origin',(9.5702001384024E-17,1.90721162719465E-13,
2.65878198860263));
#227212=CARTESIAN_POINT('',(-57.7418065394565,-12.257819391977,2.65878198860253));
#227213=CARTESIAN_POINT('',(-57.6726485248849,-12.2431194021877,2.65878198860253));
#227214=CARTESIAN_POINT('Origin',(3.19216886402205E-16,1.90674684718048E-13,
2.65878198860263));
#227215=CARTESIAN_POINT('Origin',(-0.0396071771007845,0.1863371179397,42.7590319886026));
#227216=CARTESIAN_POINT('',(-58.7320730967337,-12.2891316338726,3.64303198860253));
#227217=CARTESIAN_POINT('',(-58.3106729199895,-12.1995602612167,3.40423097483302));
#227218=CARTESIAN_POINT('Origin',(-58.694677514171,-12.2811829574214,3.20400220531634));
#227219=CARTESIAN_POINT('',(-57.9621601887015,-12.1254815938993,2.83404198860251));
#227220=CARTESIAN_POINT('',(-58.3106729199895,-12.1995602612167,3.40423097483301));
#227221=CARTESIAN_POINT('',(-61.3271735965892,-12.8407372733101,2.83404198860251));
#227222=CARTESIAN_POINT('',(-61.5812829306519,-12.8947498796467,2.83404198860251));
#227223=CARTESIAN_POINT('',(-60.9786613449625,-12.7666587067857,3.404230974833));
#227224=CARTESIAN_POINT('',(-61.3271735965892,-12.8407372733101,2.83404198860251));
#227225=CARTESIAN_POINT('',(-60.5572615995842,-12.6770874264382,3.64303198860254));
#227226=CARTESIAN_POINT('Origin',(-60.594657302592,-12.6850361284908,3.20400259788303));
#227227=CARTESIAN_POINT('',(-60.1646531634579,-12.5936359264448,3.64303198860253));
#227228=CARTESIAN_POINT('',(-0.039607177100779,0.186337117939974,3.64303198860263));
#227229=CARTESIAN_POINT('',(-60.0413691664786,-12.5674311046657,3.42473028058475));
#227230=CARTESIAN_POINT('',(-60.1646531633099,-12.5936359271411,3.64303198860253));
#227231=CARTESIAN_POINT('',(-59.7186194643908,-12.4988285377098,3.23423028058472));
#227232=CARTESIAN_POINT('Origin',(-59.7474037157348,-12.5049473440525,3.56425722717003));
#227233=CARTESIAN_POINT('',(-59.570715608832,-12.4673906027145,3.23423028058472));
#227234=CARTESIAN_POINT('',(-0.0396071771007789,0.186337117939976,3.23423028058482));
#227235=CARTESIAN_POINT('',(-59.2479658375575,-12.3987880210526,3.42473028058471));
#227236=CARTESIAN_POINT('Origin',(-59.5419282989973,-12.4612721960131,3.56425909741388));
#227237=CARTESIAN_POINT('',(-59.1246817892489,-12.3725831876354,3.64303198860253));
#227238=CARTESIAN_POINT('',(-59.2479658375575,-12.3987880210526,3.42473028058471));
#227239=CARTESIAN_POINT('',(-0.039607177100779,0.186337117939974,3.64303198860263));
#227240=CARTESIAN_POINT('Origin',(0.0396071771007845,-0.186337117939879,
42.7590319886026));
#227241=CARTESIAN_POINT('',(-60.4780472453826,-13.0497616623178,3.64303198860253));
#227242=CARTESIAN_POINT('',(-60.8994469906351,-13.1393329432572,3.404230974833));
#227243=CARTESIAN_POINT('Origin',(-60.5154429481095,-13.0577103643106,3.20400259735919));
#227244=CARTESIAN_POINT('',(-61.2479592422936,-13.213411509632,2.83404198860251));
#227245=CARTESIAN_POINT('',(-60.8994469906351,-13.1393329432572,3.404230974833));
#227246=CARTESIAN_POINT('',(-57.8829458346104,-12.498155829259,2.83404198860252));
#227247=CARTESIAN_POINT('',(0.0396071771007956,-0.186337117939599,2.83404198860262));
#227248=CARTESIAN_POINT('',(-58.2314585659347,-12.5722344964057,3.404230974833));
#227249=CARTESIAN_POINT('',(-57.8829458346104,-12.498155829259,2.83404198860252));
#227250=CARTESIAN_POINT('',(-58.6528587425321,-12.6618058697522,3.64303198860253));
#227251=CARTESIAN_POINT('Origin',(-58.6154631596709,-12.6538571932375,3.20400220587388));
#227252=CARTESIAN_POINT('',(-59.0454674352016,-12.7452574227894,3.64303198860253));
#227253=CARTESIAN_POINT('',(-59.1177113373237,-12.7606133389845,3.64303198860253));
#227254=CARTESIAN_POINT('',(-59.168751483356,-12.7714622569322,3.42473028058471));
#227255=CARTESIAN_POINT('',(-59.0454674350473,-12.745257423515,3.64303198860253));
#227256=CARTESIAN_POINT('',(-59.4915012546304,-12.8400648385941,3.23423028058472));
#227257=CARTESIAN_POINT('Origin',(-59.4627170622801,-12.8339460446684,3.56425743004694));
#227258=CARTESIAN_POINT('',(-59.6394051101892,-12.8715027735894,3.23423028058472));
#227259=CARTESIAN_POINT('',(-59.6399222675579,-12.8716126987816,3.23423028058472));
#227260=CARTESIAN_POINT('',(-59.962154812277,-12.9401053405452,3.42473028058473));
#227261=CARTESIAN_POINT('Origin',(-59.6681923469391,-12.8776211648734,3.56425912917748));
#227262=CARTESIAN_POINT('',(-60.0854388091084,-12.9663101630206,3.64303198860253));
#227263=CARTESIAN_POINT('',(-59.962154812277,-12.9401053405452,3.42473028058473));
#227264=CARTESIAN_POINT('',(-60.4785572361438,-13.0498700642004,3.64303198860253));
#227265=CARTESIAN_POINT('Origin',(-55.4710078899932,-17.8233194796326,2.65878198860249));
#227266=CARTESIAN_POINT('',(-56.1347810195641,-18.2553202812751,2.65878198860248));
#227267=CARTESIAN_POINT('',(-59.765809437495,-19.4351129318423,2.65878198860248));
#227268=CARTESIAN_POINT('',(-55.4074307335705,-18.0189898472952,2.65878198860249));
#227269=CARTESIAN_POINT('',(-59.7752282754835,-19.4061247292256,2.65878198860248));
#227270=CARTESIAN_POINT('Origin',(9.1719453606903E-17,1.90736025790112E-13,
2.65878198860263));
#227271=CARTESIAN_POINT('',(-56.1441998575526,-18.2263320786585,2.65878198860248));
#227272=CARTESIAN_POINT('',(-56.0769572651637,-18.2044836359655,2.65878198860248));
#227273=CARTESIAN_POINT('Origin',(3.2129046493506E-16,1.9066694601761E-13,
2.65878198860263));
#227274=CARTESIAN_POINT('Origin',(-0.0588677374284288,0.181176266354137,
42.7590319886026));
#227275=CARTESIAN_POINT('',(-57.1257686104889,-18.3609838302743,3.64303198860249));
#227276=CARTESIAN_POINT('',(-56.7160396659413,-18.227854826074,3.40423097483297));
#227277=CARTESIAN_POINT('Origin',(-57.0894087477751,-18.3491697947262,3.2040022053157));
#227278=CARTESIAN_POINT('',(-56.3771794531163,-18.1177524692166,2.83404198860248));
#227279=CARTESIAN_POINT('',(-56.7160396659413,-18.227854826074,3.40423097483297));
#227280=CARTESIAN_POINT('',(-59.6489943884562,-19.1808295835785,2.83404198860248));
#227281=CARTESIAN_POINT('',(-59.8960658302616,-19.2611079613977,2.83404198860247));
#227282=CARTESIAN_POINT('',(-59.3101346421293,-19.0707273770996,3.40423097483296));
#227283=CARTESIAN_POINT('',(-59.6489943884562,-19.1808295835785,2.83404198860247));
#227284=CARTESIAN_POINT('',(-58.9004061169356,-18.9375985097924,3.64303198860249));
#227285=CARTESIAN_POINT('Origin',(-58.9367660967578,-18.9494125833913,3.20400259788049));
#227286=CARTESIAN_POINT('',(-58.5186714879534,-18.8135654093535,3.64303198860249));
#227287=CARTESIAN_POINT('',(-0.0588677374284233,0.18117626635441,3.64303198860263));
#227288=CARTESIAN_POINT('',(-58.3988020033597,-18.7746174535802,3.42473028058471));
#227289=CARTESIAN_POINT('',(-58.5186714877334,-18.8135654100305,3.64303198860249));
#227290=CARTESIAN_POINT('',(-58.0849912788099,-18.6726541682848,3.23423028058468));
#227291=CARTESIAN_POINT('Origin',(-58.1129782575883,-18.6817482287252,3.56425722717167));
#227292=CARTESIAN_POINT('',(-57.9411838150806,-18.6259282908539,3.23423028058468));
#227293=CARTESIAN_POINT('',(-0.0588677374284233,0.181176266354413,3.23423028058481));
#227294=CARTESIAN_POINT('',(-57.6273730232604,-18.523964983701,3.42473028058467));
#227295=CARTESIAN_POINT('Origin',(-57.9131937527887,-18.616834308165,3.56425909740917));
#227296=CARTESIAN_POINT('',(-57.5075034888351,-18.485017010988,3.64303198860249));
#227297=CARTESIAN_POINT('',(-57.6273730232604,-18.523964983701,3.42473028058467));
#227298=CARTESIAN_POINT('',(-0.0588677374284233,0.18117626635441,3.64303198860263));
#227299=CARTESIAN_POINT('Origin',(0.0588677374284288,-0.181176266354316,
42.7590319886026));
#227300=CARTESIAN_POINT('',(-58.7826706420787,-19.2999510425009,3.64303198860248));
#227301=CARTESIAN_POINT('',(-59.1923991670854,-19.433079910384,3.40423097483296));
#227302=CARTESIAN_POINT('Origin',(-58.8190306216284,-19.3117651160112,3.2040025973581));
#227303=CARTESIAN_POINT('',(-59.5312589134597,-19.5431821167168,2.83404198860247));
#227304=CARTESIAN_POINT('',(-59.1923991670854,-19.433079910384,3.40423097483296));
#227305=CARTESIAN_POINT('',(-56.2594439784237,-18.4801050014193,2.83404198860248));
#227306=CARTESIAN_POINT('',(0.0588677374284398,-0.181176266354035,2.83404198860262));
#227307=CARTESIAN_POINT('',(-56.5983041913028,-18.5902073581105,3.40423097483297));
#227308=CARTESIAN_POINT('',(-56.2594439784237,-18.4801050014193,2.83404198860248));
#227309=CARTESIAN_POINT('',(-57.0080331356321,-18.7233363629827,3.64303198860249));
#227310=CARTESIAN_POINT('Origin',(-56.9716732726287,-18.7115223273405,3.20400220587185));
#227311=CARTESIAN_POINT('',(-57.3897680142074,-18.8473695429911,3.64303198860249));
#227312=CARTESIAN_POINT('',(-57.4600110263529,-18.8701928819397,3.64303198860249));
#227313=CARTESIAN_POINT('',(-57.5096375484035,-18.8863175164095,3.42473028058467));
#227314=CARTESIAN_POINT('',(-57.3897680139783,-18.8473695436965,3.64303198860249));
#227315=CARTESIAN_POINT('',(-57.8234483402237,-18.9882808235623,3.23423028058468));
#227316=CARTESIAN_POINT('Origin',(-57.7954614188151,-18.9791867816366,3.56425743004336));
#227317=CARTESIAN_POINT('',(-57.967255803953,-19.0350067009933,3.23423028058468));
#227318=CARTESIAN_POINT('',(-57.9677586379681,-19.0351700816687,3.23423028058468));
#227319=CARTESIAN_POINT('',(-58.2810665285028,-19.1369699862886,3.4247302805847));
#227320=CARTESIAN_POINT('Origin',(-57.9952457951659,-19.0441006607077,3.56425912918371));
#227321=CARTESIAN_POINT('',(-58.4009360128765,-19.1759179427389,3.64303198860248));
#227322=CARTESIAN_POINT('',(-58.2810665285028,-19.1369699862886,3.4247302805847));
#227323=CARTESIAN_POINT('',(-58.7831665079749,-19.3001121590972,3.64303198860248));
#227324=CARTESIAN_POINT('Origin',(-53.30408770921,-23.5239806812874,2.65878198860245));
#227325=CARTESIAN_POINT('',(-53.9190682401993,-24.0229981225299,2.65878198860245));
#227326=CARTESIAN_POINT('',(-57.4068835917977,-25.575873566121,2.65878198860243));
#227327=CARTESIAN_POINT('',(-53.2204057122636,-23.7119335237428,2.65878198860245));
#227328=CARTESIAN_POINT('',(-57.4192809246787,-25.5480287005721,2.65878198860243));
#227329=CARTESIAN_POINT('Origin',(8.62051087089599E-17,1.90750391149705E-13,
2.65878198860263));
#227330=CARTESIAN_POINT('',(-53.9314655730802,-23.995153256981,2.65878198860245));
#227331=CARTESIAN_POINT('',(-53.8668751267876,-23.9663957374946,2.65878198860245));
#227332=CARTESIAN_POINT('Origin',(3.24161598652236E-16,1.9065946645856E-13,
2.65878198860263));
#227333=CARTESIAN_POINT('Origin',(-0.0774833305059413,0.174030409680826,
42.7590319886026));
#227334=CARTESIAN_POINT('',(-54.893582249012,-24.2316692455485,3.64303198860245));
#227335=CARTESIAN_POINT('',(-54.5000136127187,-24.056441199033,3.40423097483293));
#227336=CARTESIAN_POINT('Origin',(-54.858656472411,-24.2161192879491,3.20400220531633));
#227337=CARTESIAN_POINT('',(-54.1745185417597,-23.9115214570971,2.83404198860244));
#227338=CARTESIAN_POINT('',(-54.5000136127187,-24.056441199033,3.40423097483292));
#227339=CARTESIAN_POINT('',(-57.3172883154488,-25.3107727110825,2.83404198860243));
#227340=CARTESIAN_POINT('',(-57.5546148985774,-25.4164373136776,2.83404198860243));
#227341=CARTESIAN_POINT('',(-56.9917936927132,-25.1658531674645,3.40423097483292));
#227342=CARTESIAN_POINT('',(-57.3172883154488,-25.3107727110825,2.83404198860243));
#227343=CARTESIAN_POINT('',(-56.5982254591674,-24.9906253009261,3.64303198860245));
#227344=CARTESIAN_POINT('Origin',(-56.6331513482578,-25.0061753086091,3.204002597881));
#227345=CARTESIAN_POINT('',(-56.2315470018073,-24.827369532646,3.64303198860244));
#227346=CARTESIAN_POINT('',(-0.0774833305059357,0.174030409681099,3.64303198860263));
#227347=CARTESIAN_POINT('',(-56.116405344757,-24.776105164832,3.42473028058466));
#227348=CARTESIAN_POINT('',(-56.231547001518,-24.8273695332959,3.64303198860244));
#227349=CARTESIAN_POINT('',(-55.8149717737125,-24.641898292288,3.23423028058464));
#227350=CARTESIAN_POINT('Origin',(-55.8418548487312,-24.6538679703973,3.5642572271703));
#227351=CARTESIAN_POINT('',(-55.676836286479,-24.5803964109126,3.23423028058464));
#227352=CARTESIAN_POINT('',(-0.0774833305059357,0.174030409681102,3.23423028058481));
#227353=CARTESIAN_POINT('',(-55.3754026508173,-24.4461895095991,3.42473028058463));
#227354=CARTESIAN_POINT('Origin',(-55.6499501367103,-24.5684264878134,3.56425909740456));
#227355=CARTESIAN_POINT('',(-55.2602609459789,-24.3949251197297,3.64303198860245));
#227356=CARTESIAN_POINT('',(-55.3754026508173,-24.4461895095991,3.42473028058463));
#227357=CARTESIAN_POINT('',(-0.0774833305059357,0.174030409681099,3.64303198860263));
#227358=CARTESIAN_POINT('Origin',(0.0774833305059413,-0.174030409681004,
42.7590319886026));
#227359=CARTESIAN_POINT('',(-56.4432587981555,-25.338686120288,3.64303198860244));
#227360=CARTESIAN_POINT('',(-56.8368270314552,-25.5139139873792,3.40423097483292));
#227361=CARTESIAN_POINT('Origin',(-56.4781846869838,-25.3542361278542,3.20400259735806));
#227362=CARTESIAN_POINT('',(-57.1623216542527,-25.658833530858,2.83404198860243));
#227363=CARTESIAN_POINT('',(-56.8368270314552,-25.5139139873792,3.40423097483292));
#227364=CARTESIAN_POINT('',(-54.0195518809639,-24.2595822759735,2.83404198860244));
#227365=CARTESIAN_POINT('',(0.077483330505952,-0.174030409680723,2.83404198860262));
#227366=CARTESIAN_POINT('',(-54.3450469519943,-24.4045020177489,3.40423097483293));
#227367=CARTESIAN_POINT('',(-54.0195518809639,-24.2595822759735,2.83404198860244));
#227368=CARTESIAN_POINT('',(-54.7386155880002,-24.5797300649104,3.64303198860245));
#227369=CARTESIAN_POINT('Origin',(-54.7036898111213,-24.5641801071872,3.20400220587176));
#227370=CARTESIAN_POINT('',(-55.1052942852685,-24.7429859384143,3.64303198860244));
#227371=CARTESIAN_POINT('',(-55.1727668102969,-24.7730266428387,3.64303198860244));
#227372=CARTESIAN_POINT('',(-55.2204359898054,-24.794250328961,3.42473028058462));
#227373=CARTESIAN_POINT('',(-55.105294284967,-24.7429859390916,3.64303198860244));
#227374=CARTESIAN_POINT('',(-55.5218696254671,-24.9284572302744,3.23423028058463));
#227375=CARTESIAN_POINT('Origin',(-55.4949866055708,-24.9164875765759,3.56425743004543));
#227376=CARTESIAN_POINT('',(-55.6600051127006,-24.9899591116498,3.23423028058463));
#227377=CARTESIAN_POINT('',(-55.6604881142074,-24.9901741577757,3.23423028058463));
#227378=CARTESIAN_POINT('',(-55.9614386837451,-25.1241659841938,3.42473028058465));
#227379=CARTESIAN_POINT('Origin',(-55.6868911941847,-25.0019290044722,3.56425912917205));
#227380=CARTESIAN_POINT('',(-56.0765803405061,-25.1754303526578,3.64303198860244));
#227381=CARTESIAN_POINT('',(-55.9614386837451,-25.1241659841938,3.42473028058465));
#227382=CARTESIAN_POINT('',(-56.4437351063762,-25.3388981863709,3.64303198860244));
#227383=CARTESIAN_POINT('Origin',(-50.5531567888873,-28.9669082278885,2.65878198860241));
#227384=CARTESIAN_POINT('',(-51.1126068659045,-29.5274749692187,2.65878198860241));
#227385=CARTESIAN_POINT('',(-54.4189959163061,-31.4364195775137,2.65878198860239));
#227386=CARTESIAN_POINT('',(-50.4502867888873,-29.1450842944631,2.65878198860241));
#227387=CARTESIAN_POINT('',(-54.434235916306,-31.4100231232064,2.65878198860239));
#227388=CARTESIAN_POINT('Origin',(7.92193830068374E-17,1.90764101408356E-13,
2.65878198860263));
#227389=CARTESIAN_POINT('',(-51.1278468659044,-29.5010785149114,2.65878198860241));
#227390=CARTESIAN_POINT('',(-51.0666162321541,-29.465726992033,2.65878198860241));
#227391=CARTESIAN_POINT('Origin',(3.27798830811898E-16,1.90652327988513E-13,
2.65878198860263));
#227392=CARTESIAN_POINT('Origin',(-0.0952500000000014,0.164977839420845,
42.7590319886026));
#227393=CARTESIAN_POINT('',(-52.0599703131944,-29.8368674217658,3.64303198860241));
#227394=CARTESIAN_POINT('',(-51.686874005494,-29.6214601680814,3.40423097483289));
#227395=CARTESIAN_POINT('Origin',(-52.0268612768234,-29.8177519107044,3.20400220531693));
#227396=CARTESIAN_POINT('',(-51.3783102685124,-29.4433108120867,2.8340419886024));
#227397=CARTESIAN_POINT('',(-51.686874005494,-29.6214601680814,3.40423097483289));
#227398=CARTESIAN_POINT('',(-54.3576020372436,-31.1634057161443,2.83404198860239));
#227399=CARTESIAN_POINT('',(-54.5825835619868,-31.2932988600175,2.83404198860239));
#227400=CARTESIAN_POINT('',(-54.0490387253004,-30.9852566042326,3.40423097483288));
#227401=CARTESIAN_POINT('',(-54.3576020372436,-31.1634057161443,2.83404198860239));
#227402=CARTESIAN_POINT('',(-53.6759427993284,-30.7698495716384,3.64303198860241));
#227403=CARTESIAN_POINT('Origin',(-53.709051942338,-30.7889651442676,3.20400259788283));
#227404=CARTESIAN_POINT('',(-53.3283379195021,-30.5691597998771,3.64303198860241));
#227405=CARTESIAN_POINT('',(-0.0952499999999959,0.164977839421119,3.64303198860263));
#227406=CARTESIAN_POINT('',(-53.2191856060843,-30.5061406831646,3.42473028058463));
#227407=CARTESIAN_POINT('',(-53.3283379191462,-30.5691598004935,3.64303198860241));
#227408=CARTESIAN_POINT('',(-52.9334317578285,-30.3411606219521,3.2342302805846));
#227409=CARTESIAN_POINT('Origin',(-52.9589163924907,-30.3558747754319,3.56425722717026));
#227410=CARTESIAN_POINT('',(-52.8024816883957,-30.2655565641147,3.2342302805846));
#227411=CARTESIAN_POINT('',(-0.0952499999999958,0.164977839421121,3.23423028058481));
#227412=CARTESIAN_POINT('',(-52.5167277788839,-30.100576467536,3.42473028058458));
#227413=CARTESIAN_POINT('Origin',(-52.7769940214367,-30.2508418455888,3.56425909740749));
#227414=CARTESIAN_POINT('',(-52.4075754202454,-30.0375573238934,3.64303198860241));
#227415=CARTESIAN_POINT('',(-52.5167277788839,-30.100576467536,3.42473028058458));
#227416=CARTESIAN_POINT('',(-0.0952499999999959,0.164977839421119,3.64303198860263));
#227417=CARTESIAN_POINT('Origin',(0.0952500000000014,-0.164977839421024,
42.7590319886026));
#227418=CARTESIAN_POINT('',(-53.4854427993284,-31.0998052504802,3.6430319886024));
#227419=CARTESIAN_POINT('',(-53.8585387249976,-31.3152122835989,3.40423097483288));
#227420=CARTESIAN_POINT('Origin',(-53.5185519420882,-31.1189208229652,3.20400259735687));
#227421=CARTESIAN_POINT('',(-54.1671020370175,-31.4933613953778,2.83404198860239));
#227422=CARTESIAN_POINT('',(-53.8585387249976,-31.3152122835989,3.40423097483288));
#227423=CARTESIAN_POINT('',(-51.1878102687783,-29.7732664904682,2.8340419886024));
#227424=CARTESIAN_POINT('',(0.0952500000000119,-0.164977839420743,2.83404198860262));
#227425=CARTESIAN_POINT('',(-51.4963740058472,-29.9514158463116,3.40423097483288));
#227426=CARTESIAN_POINT('',(-51.1878102687783,-29.7732664904682,2.8340419886024));
#227427=CARTESIAN_POINT('',(-51.8694703131944,-30.1668231006077,3.64303198860241));
#227428=CARTESIAN_POINT('Origin',(-51.83636127656,-30.1477075893942,3.20400220587218));
#227429=CARTESIAN_POINT('',(-52.2170754206163,-30.3675130020929,3.64303198860241));
#227430=CARTESIAN_POINT('',(-52.2810382154237,-30.4044419397496,3.64303198860241));
#227431=CARTESIAN_POINT('',(-52.3262277788839,-30.4305321463779,3.42473028058459));
#227432=CARTESIAN_POINT('',(-52.2170754202454,-30.3675130027353,3.64303198860241));
#227433=CARTESIAN_POINT('',(-52.6119816883956,-30.5955122429565,3.2342302805846));
#227434=CARTESIAN_POINT('Origin',(-52.5864971059999,-30.5807981195144,3.56425743004055));
#227435=CARTESIAN_POINT('',(-52.7429317578285,-30.671116300794,3.23423028058459));
#227436=CARTESIAN_POINT('',(-52.7433896349615,-30.6713806562799,3.23423028058459));
#227437=CARTESIAN_POINT('',(-53.0286856060843,-30.8360963620065,3.42473028058461));
#227438=CARTESIAN_POINT('Origin',(-52.7684193600396,-30.68583098207,3.56425912917953));
#227439=CARTESIAN_POINT('',(-53.1378379191462,-30.8991154793354,3.6430319886024));
#227440=CARTESIAN_POINT('',(-53.0286856060843,-30.8360963620065,3.42473028058461));
#227441=CARTESIAN_POINT('',(-53.4858943313411,-31.1000659426093,3.6430319886024));
#227442=CARTESIAN_POINT('Origin',(-47.2483549038573,-34.0924682662297,2.65878198860237));
#227443=CARTESIAN_POINT('',(-47.7461450747862,-34.7084426211234,2.65878198860237));
#227444=CARTESIAN_POINT('',(-50.8348823336483,-36.9525415975214,2.65878198860236));
#227445=CARTESIAN_POINT('',(-47.1274239660506,-34.2589154226524,2.65878198860237));
#227446=CARTESIAN_POINT('',(-50.8527980281382,-36.9278827595329,2.65878198860236));
#227447=CARTESIAN_POINT('Origin',(7.08388135731921E-17,1.90777006353604E-13,
2.65878198860263));
#227448=CARTESIAN_POINT('',(-47.764060769276,-34.6837837831348,2.65878198860237));
#227449=CARTESIAN_POINT('',(-47.7068608037047,-34.6422255755468,2.65878198860237));
#227450=CARTESIAN_POINT('Origin',(3.32162311137369E-16,1.90645608818039E-13,
2.65878198860263));
#227451=CARTESIAN_POINT('Origin',(-0.111973090561717,0.154117737428337,
42.7590319886026));
#227452=CARTESIAN_POINT('',(-48.6559784483762,-35.1151666347443,3.64303198860237));
#227453=CARTESIAN_POINT('',(-48.3074421904915,-34.8619402208392,3.40423097483286));
#227454=CARTESIAN_POINT('Origin',(-48.6250489017663,-35.0926950037603,3.20400220531748));
#227455=CARTESIAN_POINT('',(-48.0191904763611,-34.6525130924096,2.83404198860237));
#227456=CARTESIAN_POINT('',(-48.3074421904915,-34.8619402208392,3.40423097483286));
#227457=CARTESIAN_POINT('',(-50.8023624960588,-36.674605926818,2.83404198860235));
#227458=CARTESIAN_POINT('',(-51.0125340177512,-36.8273044755032,2.83404198860235));
#227459=CARTESIAN_POINT('',(-50.514111179124,-36.4651790855641,3.40423097483284));
#227460=CARTESIAN_POINT('',(-50.8023624960588,-36.674605926818,2.83404198860235));
#227461=CARTESIAN_POINT('',(-50.1655752777668,-36.2119529314387,3.64303198860237));
#227462=CARTESIAN_POINT('Origin',(-50.1965049239947,-36.2344246347994,3.20400259788159));
#227463=CARTESIAN_POINT('',(-49.8408524072781,-35.9760279553335,3.64303198860237));
#227464=CARTESIAN_POINT('',(-0.111973090561712,0.15411773742861,3.64303198860263));
#227465=CARTESIAN_POINT('',(-49.7388853330808,-35.9019445403521,3.4247302805846));
#227466=CARTESIAN_POINT('',(-49.8408524068601,-35.9760279559089,3.64303198860236));
#227467=CARTESIAN_POINT('',(-49.471941986573,-35.707998846546,3.23423028058456));
#227468=CARTESIAN_POINT('Origin',(-49.495748965888,-35.7252962640513,3.5642572271713));
#227469=CARTESIAN_POINT('',(-49.3496120513046,-35.6191209461254,3.23423028058456));
#227470=CARTESIAN_POINT('',(-0.111973090561712,0.154117737428613,3.23423028058481));
#227471=CARTESIAN_POINT('',(-49.0826686475732,-35.425175210744,3.42473028058456));
#227472=CARTESIAN_POINT('Origin',(-49.3258021153687,-35.601822649709,3.56425909741072));
#227473=CARTESIAN_POINT('',(-48.9807015312175,-35.3510917642536,3.64303198860237));
#227474=CARTESIAN_POINT('',(-49.0826686475732,-35.425175210744,3.42473028058456));
#227475=CARTESIAN_POINT('',(-0.111973090561712,0.15411773742861,3.64303198860263));
#227476=CARTESIAN_POINT('Origin',(0.111973090561717,-0.154117737428516,
42.7590319886026));
#227477=CARTESIAN_POINT('',(-49.9416290966434,-36.5201884062956,3.64303198860236));
#227478=CARTESIAN_POINT('',(-50.2901649976452,-36.7734145609101,3.40423097483284));
#227479=CARTESIAN_POINT('Origin',(-49.9725587426394,-36.5426601094878,3.20400259735863));
#227480=CARTESIAN_POINT('',(-50.5784163146694,-36.982841402041,2.83404198860235));
#227481=CARTESIAN_POINT('',(-50.2901649976452,-36.7734145609101,3.40423097483284));
#227482=CARTESIAN_POINT('',(-47.7952442955499,-34.9607485668368,2.83404198860236));
#227483=CARTESIAN_POINT('',(0.111973090561728,-0.154117737428234,2.83404198860262));
#227484=CARTESIAN_POINT('',(-48.0834960097833,-35.1701756951246,3.40423097483285));
#227485=CARTESIAN_POINT('',(-47.7952442955499,-34.9607485668368,2.83404198860237));
#227486=CARTESIAN_POINT('',(-48.4320322672528,-35.4234021096012,3.64303198860237));
#227487=CARTESIAN_POINT('Origin',(-48.4011027203962,-35.400930478438,3.20400220587424));
#227488=CARTESIAN_POINT('',(-48.75675535053,-35.6593272385105,3.64303198860237));
#227489=CARTESIAN_POINT('',(-48.8165076253516,-35.7027398082301,3.64303198860237));
#227490=CARTESIAN_POINT('',(-48.8587224664497,-35.7334106856009,3.42473028058455));
#227491=CARTESIAN_POINT('',(-48.7567553500941,-35.6593272391104,3.64303198860237));
#227492=CARTESIAN_POINT('',(-49.1256658701812,-35.9273564209823,3.23423028058456));
#227493=CARTESIAN_POINT('Origin',(-49.1018589397083,-35.9100590388147,3.56425743004586));
#227494=CARTESIAN_POINT('',(-49.2479958054496,-36.0162343214029,3.23423028058455));
#227495=CARTESIAN_POINT('',(-49.248423541611,-36.0165450899149,3.23423028058455));
#227496=CARTESIAN_POINT('',(-49.5149391519574,-36.2101800152089,3.42473028058458));
#227497=CARTESIAN_POINT('Origin',(-49.2718056808885,-36.0335325740075,3.56425912917758));
#227498=CARTESIAN_POINT('',(-49.6169062257367,-36.2842634307658,3.64303198860236));
#227499=CARTESIAN_POINT('',(-49.5149391519574,-36.2101800152089,3.42473028058458));
#227500=CARTESIAN_POINT('',(-49.9420509053688,-36.5204948682733,3.64303198860236));
#227501=CARTESIAN_POINT('Origin',(-43.4258901551468,-38.8445040879383,2.65878198860234));
#227502=CARTESIAN_POINT('',(-43.8565665267053,-39.5091373124624,2.65878198860234));
#227503=CARTESIAN_POINT('',(-46.6938111422601,-42.0638038389702,2.65878198860232));
#227504=CARTESIAN_POINT('',(-43.2882232241945,-38.9973987043321,2.65878198860234));
#227505=CARTESIAN_POINT('',(-46.7142062431419,-42.0411527846897,2.65878198860232));
#227506=CARTESIAN_POINT('Origin',(6.11552196804844E-17,1.90788964596167E-13,
2.65878198860263));
#227507=CARTESIAN_POINT('',(-43.8769616275871,-39.4864862581819,2.65878198860234));
#227508=CARTESIAN_POINT('',(-43.8244190249875,-39.4391766863032,2.65878198860234));
#227509=CARTESIAN_POINT('Origin',(3.37204232425086E-16,1.90639382563777E-13,
2.65878198860263));
#227510=CARTESIAN_POINT('Origin',(-0.127469380511364,0.141569089253353,
42.7590319886026));
#227511=CARTESIAN_POINT('',(-44.7189015017595,-40.0087367337515,3.64303198860233));
#227512=CARTESIAN_POINT('',(-44.3987439298677,-39.7204655612076,3.40423097483282));
#227513=CARTESIAN_POINT('Origin',(-44.6904903154948,-39.9831551867354,3.20400220532103));
#227514=CARTESIAN_POINT('',(-44.1339623846888,-39.4820551877881,2.83404198860233));
#227515=CARTESIAN_POINT('',(-44.3987439298677,-39.7204655612076,3.40423097483282));
#227516=CARTESIAN_POINT('',(-46.6905216402894,-41.7839914803029,2.83404198860232));
#227517=CARTESIAN_POINT('',(-46.8835804757581,-41.9578224365464,2.83404198860231));
#227518=CARTESIAN_POINT('',(-46.4257404601132,-41.545581434003,3.40423097483281));
#227519=CARTESIAN_POINT('',(-46.6905216402894,-41.7839914803029,2.83404198860232));
#227520=CARTESIAN_POINT('',(-46.1055832156406,-41.2573105570839,3.64303198860234));
#227521=CARTESIAN_POINT('Origin',(-46.1339944934111,-41.2828921864921,3.20400259788175));
#227522=CARTESIAN_POINT('',(-45.8073000862121,-40.9887352200423,3.64303198860232));
#227523=CARTESIAN_POINT('',(-0.127469380511358,0.141569089253626,3.64303198860262));
#227524=CARTESIAN_POINT('',(-45.7136354238372,-40.9043991801905,3.42473028058455));
#227525=CARTESIAN_POINT('',(-45.8073000857355,-40.9887352205716,3.64303198860232));
#227526=CARTESIAN_POINT('',(-45.4684272662432,-40.6836127633981,3.23423028058452));
#227527=CARTESIAN_POINT('Origin',(-45.4902957559651,-40.703303930804,3.56425722716923));
#227528=CARTESIAN_POINT('',(-45.3560577375092,-40.5824347852702,3.23423028058452));
#227529=CARTESIAN_POINT('',(-0.127469380511358,0.141569089253629,3.23423028058481));
#227530=CARTESIAN_POINT('',(-45.1108495273509,-40.3616483211486,3.42473028058452));
#227531=CARTESIAN_POINT('Origin',(-45.3341863992363,-40.5627424347186,3.56425909741396));
#227532=CARTESIAN_POINT('',(-45.0171848263429,-40.277312245553,3.64303198860233));
#227533=CARTESIAN_POINT('',(-45.1108495273509,-40.3616483211486,3.42473028058452));
#227534=CARTESIAN_POINT('',(-0.127469380511358,0.141569089253626,3.64303198860262));
#227535=CARTESIAN_POINT('Origin',(0.127469380511364,-0.141569089253532,
42.7590319886026));
#227536=CARTESIAN_POINT('',(-45.8506444546178,-41.5404487355908,3.64303198860233));
#227537=CARTESIAN_POINT('',(-46.170801698685,-41.8287196129601,3.4042309748328));
#227538=CARTESIAN_POINT('Origin',(-45.8790557321755,-41.5660303648073,3.2040025973597));
#227539=CARTESIAN_POINT('',(-46.4355828789644,-42.0671296591455,2.83404198860231));
#227540=CARTESIAN_POINT('',(-46.170801698685,-41.8287196129601,3.4042309748328));
#227541=CARTESIAN_POINT('',(-43.8790236240217,-39.7651933659001,2.83404198860233));
#227542=CARTESIAN_POINT('',(0.127469380511373,-0.141569089253249,2.83404198860262));
#227543=CARTESIAN_POINT('',(-44.1438051693175,-40.0036037391897,3.40423097483282));
#227544=CARTESIAN_POINT('',(-43.8790236240217,-39.7651933659001,2.83404198860233));
#227545=CARTESIAN_POINT('',(-44.4639627407368,-40.2918749122584,3.64303198860234));
#227546=CARTESIAN_POINT('Origin',(-44.435551554248,-40.2662933650406,3.20400220587063));
#227547=CARTESIAN_POINT('',(-44.7622460658166,-40.5604504235085,3.64303198860233));
#227548=CARTESIAN_POINT('',(-44.8171331622253,-40.609870988093,3.64303198860233));
#227549=CARTESIAN_POINT('',(-44.8559107663282,-40.6447864996555,3.42473028058451));
#227550=CARTESIAN_POINT('',(-44.7622460653202,-40.5604504240599,3.64303198860233));
#227551=CARTESIAN_POINT('',(-45.1011189764865,-40.8655729637771,3.23423028058452));
#227552=CARTESIAN_POINT('Origin',(-45.0792505316448,-40.8458818366201,3.56425743004167));
#227553=CARTESIAN_POINT('',(-45.2134885052205,-40.966750941905,3.23423028058452));
#227554=CARTESIAN_POINT('',(-45.2138814140435,-40.9671047185982,3.23423028058452));
#227555=CARTESIAN_POINT('',(-45.4586966628145,-41.1875373586974,3.42473028058454));
#227556=CARTESIAN_POINT('Origin',(-45.2353597879101,-40.9864432425634,3.56425912917358));
#227557=CARTESIAN_POINT('',(-45.5523613247128,-41.2718733990784,3.64303198860233));
#227558=CARTESIAN_POINT('',(-45.4586966628145,-41.1875373586974,3.42473028058454));
#227559=CARTESIAN_POINT('',(-45.8510319186313,-41.5407976097556,3.64303198860233));
#227560=CARTESIAN_POINT('Origin',(-39.1276422664447,-43.1709513941245,2.65878198860231));
#227561=CARTESIAN_POINT('',(-39.4864862581813,-43.8769616275876,2.65878198860231));
#227562=CARTESIAN_POINT('',(-42.0411527846891,-46.7142062431424,2.65878198860229));
#227563=CARTESIAN_POINT('',(-38.974747650051,-43.3086183250768,2.65878198860231));
#227564=CARTESIAN_POINT('',(-42.0638038389696,-46.6938111422606,2.65878198860229));
#227565=CARTESIAN_POINT('Origin',(5.02746968098233E-17,1.90799845119038E-13,
2.65878198860263));
#227566=CARTESIAN_POINT('',(-39.5091373124618,-43.8565665267058,2.65878198860231));
#227567=CARTESIAN_POINT('',(-39.4618277405832,-43.8040239241061,2.65878198860231));
#227568=CARTESIAN_POINT('Origin',(3.4286935433033E-16,1.90633717441872E-13,
2.65878198860263));
#227569=CARTESIAN_POINT('Origin',(-0.141569089253445,0.127469380511272,
42.7590319886026));
#227570=CARTESIAN_POINT('',(-40.2918749122578,-44.4639627407373,3.64303198860231));
#227571=CARTESIAN_POINT('',(-40.0036037397139,-44.1438051688455,3.40423097483279));
#227572=CARTESIAN_POINT('Origin',(-40.2662933652432,-44.4355515544741,3.20400220531654));
#227573=CARTESIAN_POINT('',(-39.7651933655044,-43.8790236243779,2.8340419886023));
#227574=CARTESIAN_POINT('',(-40.0036037397139,-44.1438051688455,3.40423097483279));
#227575=CARTESIAN_POINT('',(-42.0671296588092,-46.4355828792672,2.83404198860229));
#227576=CARTESIAN_POINT('',(-42.2409606150526,-46.6286417147359,2.83404198860228));
#227577=CARTESIAN_POINT('',(-41.8287196134086,-46.1708016982812,3.40423097483278));
#227578=CARTESIAN_POINT('',(-42.0671296588092,-46.4355828792672,2.83404198860229));
#227579=CARTESIAN_POINT('',(-41.5404487355902,-45.8506444546184,3.64303198860231));
#227580=CARTESIAN_POINT('Origin',(-41.5660303649981,-45.8790557323884,3.20400259788069));
#227581=CARTESIAN_POINT('',(-41.2718733996069,-45.552361324237,3.6430319886023));
#227582=CARTESIAN_POINT('',(-0.141569089253439,0.127469380511545,3.64303198860263));
#227583=CARTESIAN_POINT('',(-41.1875373586968,-45.458696662815,3.42473028058453));
#227584=CARTESIAN_POINT('',(-41.2718733990778,-45.5523613247133,3.6430319886023));
#227585=CARTESIAN_POINT('',(-40.9667509419044,-45.213488505221,3.23423028058449));
#227586=CARTESIAN_POINT('Origin',(-40.9864413462824,-45.2353576819761,3.5642572271696));
#227587=CARTESIAN_POINT('',(-40.8655729637765,-45.1011189764871,3.23423028058449));
#227588=CARTESIAN_POINT('',(-0.141569089253439,0.127469380511548,3.23423028058481));
#227589=CARTESIAN_POINT('',(-40.6447864996549,-44.8559107663287,3.42473028058448));
#227590=CARTESIAN_POINT('Origin',(-40.8458798501217,-45.0792483253099,3.5642590974058));
#227591=CARTESIAN_POINT('',(-40.5604504240593,-44.7622460653207,3.64303198860231));
#227592=CARTESIAN_POINT('',(-40.6447864996549,-44.8559107663287,3.42473028058448));
#227593=CARTESIAN_POINT('',(-0.141569089253439,0.127469380511545,3.64303198860263));
#227594=CARTESIAN_POINT('Origin',(0.141569089253445,-0.127469380511451,
42.7590319886026));
#227595=CARTESIAN_POINT('',(-41.2573105570833,-46.1055832156411,3.6430319886023));
#227596=CARTESIAN_POINT('',(-41.5455814344526,-46.4257404597083,3.40423097483277));
#227597=CARTESIAN_POINT('Origin',(-41.282892186299,-46.1339944931978,3.20400259735698));
#227598=CARTESIAN_POINT('',(-41.7839914799663,-46.6905216405925,2.83404198860228));
#227599=CARTESIAN_POINT('',(-41.5455814344526,-46.4257404597083,3.40423097483277));
#227600=CARTESIAN_POINT('',(-39.4820551873926,-44.1339623850449,2.8340419886023));
#227601=CARTESIAN_POINT('',(0.141569089253454,-0.127469380511168,2.83404198860262));
#227602=CARTESIAN_POINT('',(-39.7204655617324,-44.3987439293951,3.40423097483279));
#227603=CARTESIAN_POINT('',(-39.4820551873926,-44.1339623850449,2.8340419886023));
#227604=CARTESIAN_POINT('',(-40.0087367337509,-44.71890150176,3.64303198860231));
#227605=CARTESIAN_POINT('Origin',(-39.9831551865321,-44.6904903152701,3.20400220587386));
#227606=CARTESIAN_POINT('',(-40.2773122461035,-45.0171848258472,3.6430319886023));
#227607=CARTESIAN_POINT('',(-40.3267328095855,-45.0720719232485,3.6430319886023));
#227608=CARTESIAN_POINT('',(-40.361648321148,-45.1108495273514,3.42473028058448));
#227609=CARTESIAN_POINT('',(-40.2773122455524,-45.0171848263434,3.6430319886023));
#227610=CARTESIAN_POINT('',(-40.5824347852696,-45.3560577375098,3.23423028058449));
#227611=CARTESIAN_POINT('Origin',(-40.5627444213187,-45.3341886054745,3.56425743004244));
#227612=CARTESIAN_POINT('',(-40.6836127633975,-45.4684272662438,3.23423028058449));
#227613=CARTESIAN_POINT('',(-40.6839665400907,-45.4688201750667,3.23423028058449));
#227614=CARTESIAN_POINT('',(-40.9043991801899,-45.7136354238377,3.4247302805845));
#227615=CARTESIAN_POINT('Origin',(-40.7033058269853,-45.4902978619871,3.56425912917549));
#227616=CARTESIAN_POINT('',(-40.988735220571,-45.807300085736,3.6430319886023));
#227617=CARTESIAN_POINT('',(-40.9043991801899,-45.7136354238377,3.4247302805845));
#227618=CARTESIAN_POINT('',(-41.2576594312481,-46.1059706796546,3.6430319886023));
#227619=CARTESIAN_POINT('Origin',(-34.4007037410859,-47.0244087227343,2.65878198860228));
#227620=CARTESIAN_POINT('',(-34.6837837831342,-47.7640607692764,2.65878198860228));
#227621=CARTESIAN_POINT('',(-36.9278827595322,-50.8527980281386,2.65878198860226));
#227622=CARTESIAN_POINT('',(-34.2342565846632,-47.1453396605409,2.65878198860228));
#227623=CARTESIAN_POINT('',(-36.9525415975208,-50.8348823336487,2.65878198860226));
#227624=CARTESIAN_POINT('Origin',(3.83164542466798E-17,1.90809528712931E-13,
2.65878198860263));
#227625=CARTESIAN_POINT('',(-34.7084426211227,-47.7461450747866,2.65878198860228));
#227626=CARTESIAN_POINT('',(-34.6668844135347,-47.6889451092152,2.65878198860228));
#227627=CARTESIAN_POINT('Origin',(3.49095608592005E-16,1.90628675520584E-13,
2.65878198860263));
#227628=CARTESIAN_POINT('Origin',(-0.154117737428428,0.111973090561625,
42.7590319886026));
#227629=CARTESIAN_POINT('',(-35.4234021096005,-48.4320322672532,3.64303198860228));
#227630=CARTESIAN_POINT('',(-35.1701756956954,-48.0834960093685,3.40423097483276));
#227631=CARTESIAN_POINT('Origin',(-35.400930478616,-48.4011027206425,3.20400220531938));
#227632=CARTESIAN_POINT('',(-34.9607485664058,-47.795244295863,2.83404198860228));
#227633=CARTESIAN_POINT('',(-35.1701756956954,-48.0834960093685,3.40423097483276));
#227634=CARTESIAN_POINT('',(-36.9828414016742,-50.5784163149358,2.83404198860225));
#227635=CARTESIAN_POINT('',(-37.1355399503593,-50.7885878366282,2.83404198860226));
#227636=CARTESIAN_POINT('',(-36.7734145613991,-50.2901649972899,3.40423097483274));
#227637=CARTESIAN_POINT('',(-36.9828414016742,-50.5784163149358,2.83404198860226));
#227638=CARTESIAN_POINT('',(-36.5201884062949,-49.9416290966439,3.64303198860227));
#227639=CARTESIAN_POINT('Origin',(-36.5426601096556,-49.9725587428718,3.20400259788141));
#227640=CARTESIAN_POINT('',(-36.2842634313412,-49.6169062253185,3.64303198860227));
#227641=CARTESIAN_POINT('',(-0.154117737428423,0.111973090561899,3.64303198860263));
#227642=CARTESIAN_POINT('',(-36.2101800152082,-49.5149391519578,3.42473028058449));
#227643=CARTESIAN_POINT('',(-36.2842634307651,-49.6169062257371,3.64303198860227));
#227644=CARTESIAN_POINT('',(-36.0162343214022,-49.24799580545,3.23423028058446));
#227645=CARTESIAN_POINT('Origin',(-36.0335309082464,-49.2718033882784,3.56425722716715));
#227646=CARTESIAN_POINT('',(-35.9273564209816,-49.1256658701816,3.23423028058446));
#227647=CARTESIAN_POINT('',(-0.154117737428423,0.111973090561901,3.23423028058481));
#227648=CARTESIAN_POINT('',(-35.7334106856002,-48.8587224664502,3.42473028058446));
#227649=CARTESIAN_POINT('Origin',(-35.9100572938239,-49.1018565378152,3.56425909741215));
#227650=CARTESIAN_POINT('',(-35.6593272391098,-48.7567553500946,3.64303198860228));
#227651=CARTESIAN_POINT('',(-35.7334106856002,-48.8587224664502,3.42473028058446));
#227652=CARTESIAN_POINT('',(-0.154117737428423,0.111973090561899,3.64303198860263));
#227653=CARTESIAN_POINT('Origin',(0.154117737428428,-0.111973090561804,
42.7590319886026));
#227654=CARTESIAN_POINT('',(-36.211952931438,-50.1655752777673,3.64303198860227));
#227655=CARTESIAN_POINT('',(-36.4651790860525,-50.5141111787691,3.40423097483274));
#227656=CARTESIAN_POINT('Origin',(-36.2344246346306,-50.1965049237636,3.20400259735939));
#227657=CARTESIAN_POINT('',(-36.6746059264515,-50.8023624963251,2.83404198860226));
#227658=CARTESIAN_POINT('',(-36.4651790860525,-50.5141111787691,3.40423097483274));
#227659=CARTESIAN_POINT('',(-34.6525130919793,-48.0191904766737,2.83404198860227));
#227660=CARTESIAN_POINT('',(0.154117737428437,-0.111973090561521,2.83404198860262));
#227661=CARTESIAN_POINT('',(-34.8619402214099,-48.3074421900768,3.40423097483277));
#227662=CARTESIAN_POINT('',(-34.6525130919793,-48.0191904766737,2.83404198860227));
#227663=CARTESIAN_POINT('',(-35.1151666347437,-48.6559784483766,3.64303198860228));
#227664=CARTESIAN_POINT('Origin',(-35.0926950035815,-48.6250489015215,3.20400220587083));
#227665=CARTESIAN_POINT('',(-35.3510917648527,-48.9807015307822,3.64303198860227));
#227666=CARTESIAN_POINT('',(-35.3945043333726,-49.0404538064755,3.64303198860227));
#227667=CARTESIAN_POINT('',(-35.4251752107434,-49.0826686475736,3.42473028058445));
#227668=CARTESIAN_POINT('',(-35.3510917642529,-48.980701531218,3.64303198860227));
#227669=CARTESIAN_POINT('',(-35.6191209461248,-49.3496120513051,3.23423028058446));
#227670=CARTESIAN_POINT('Origin',(-35.6018243948111,-49.3258045171764,3.56425743003822));
#227671=CARTESIAN_POINT('',(-35.7079988465454,-49.4719419865734,3.23423028058446));
#227672=CARTESIAN_POINT('',(-35.7083096150574,-49.4723697227349,3.23423028058446));
#227673=CARTESIAN_POINT('',(-35.9019445403514,-49.7388853330813,3.42473028058448));
#227674=CARTESIAN_POINT('Origin',(-35.7252979297054,-49.4957512585773,3.56425912917917));
#227675=CARTESIAN_POINT('',(-35.9760279559083,-49.8408524068605,3.64303198860227));
#227676=CARTESIAN_POINT('',(-35.9019445403514,-49.7388853330813,3.42473028058448));
#227677=CARTESIAN_POINT('',(-36.2122593934157,-50.1659970864927,3.64303198860227));
#227678=CARTESIAN_POINT('Origin',(-29.2968639067297,-50.3626567888876,2.65878198860226));
#227679=CARTESIAN_POINT('',(-29.5010785149107,-51.1278468659048,2.65878198860225));
#227680=CARTESIAN_POINT('',(-31.4100231232056,-54.4342359163064,2.65878198860223));
#227681=CARTESIAN_POINT('',(-29.1186878401551,-50.4655267888876,2.65878198860226));
#227682=CARTESIAN_POINT('',(-31.436419577513,-54.4189959163064,2.65878198860223));
#227683=CARTESIAN_POINT('Origin',(2.54115089989943E-17,1.90817909282364E-13,
2.65878198860263));
#227684=CARTESIAN_POINT('',(-29.527474969218,-51.1126068659048,2.65878198860225));
#227685=CARTESIAN_POINT('',(-29.4921234463396,-51.0513762321545,2.65878198860225));
#227686=CARTESIAN_POINT('Origin',(3.55814779065493E-16,1.90624312040259E-13,
2.65878198860263));
#227687=CARTESIAN_POINT('Origin',(-0.164977839420936,0.0952499999999092,
42.7590319886026));
#227688=CARTESIAN_POINT('',(-30.166823100607,-51.8694703131947,3.64303198860225));
#227689=CARTESIAN_POINT('',(-29.9514158469225,-51.4963740054944,3.40423097483274));
#227690=CARTESIAN_POINT('Origin',(-30.1477075895448,-51.8363612768224,3.20400220532004));
#227691=CARTESIAN_POINT('',(-29.7732664900078,-51.187810269044,2.83404198860225));
#227692=CARTESIAN_POINT('',(-29.9514158469225,-51.4963740054944,3.40423097483274));
#227693=CARTESIAN_POINT('',(-31.4933613949854,-54.1671020372439,2.83404198860223));
#227694=CARTESIAN_POINT('',(-31.6232545388586,-54.3920835619872,2.83404198860223));
#227695=CARTESIAN_POINT('',(-31.3152122841225,-53.8585387246953,3.40423097483272));
#227696=CARTESIAN_POINT('',(-31.4933613949854,-54.1671020372439,2.83404198860223));
#227697=CARTESIAN_POINT('',(-31.0998052504795,-53.4854427993288,3.64303198860225));
#227698=CARTESIAN_POINT('Origin',(-31.1189208231087,-53.5185519423383,3.20400259788257));
#227699=CARTESIAN_POINT('',(-30.899115479951,-53.1378379187907,3.64303198860225));
#227700=CARTESIAN_POINT('',(-0.164977839420931,0.0952500000001823,3.64303198860263));
#227701=CARTESIAN_POINT('',(-30.8360963620057,-53.0286856060847,3.42473028058447));
#227702=CARTESIAN_POINT('',(-30.8991154793346,-53.1378379191465,3.64303198860225));
#227703=CARTESIAN_POINT('',(-30.6711163007932,-52.7429317578288,3.23423028058444));
#227704=CARTESIAN_POINT('Origin',(-30.6858295650779,-52.7684169058702,3.56425722716709));
#227705=CARTESIAN_POINT('',(-30.5955122429558,-52.611981688396,3.23423028058444));
#227706=CARTESIAN_POINT('',(-0.164977839420931,0.0952500000001852,3.23423028058481));
#227707=CARTESIAN_POINT('',(-30.4305321463772,-52.3262277788842,3.42473028058445));
#227708=CARTESIAN_POINT('Origin',(-30.5807966351508,-52.5864945348665,3.56425909741311));
#227709=CARTESIAN_POINT('',(-30.3675130027346,-52.2170754202458,3.64303198860225));
#227710=CARTESIAN_POINT('',(-30.4305321463772,-52.3262277788842,3.42473028058445));
#227711=CARTESIAN_POINT('',(-0.164977839420931,0.0952500000001823,3.64303198860263));
#227712=CARTESIAN_POINT('Origin',(0.164977839420936,-0.0952500000000878,
42.7590319886026));
#227713=CARTESIAN_POINT('',(-30.7698495716376,-53.6759427993287,3.64303198860224));
#227714=CARTESIAN_POINT('',(-30.9852566047563,-54.049038724998,3.40423097483272));
#227715=CARTESIAN_POINT('Origin',(-30.7889651441224,-53.7090519420883,3.20400259735578));
#227716=CARTESIAN_POINT('',(-31.1634057157514,-54.3576020374703,2.83404198860223));
#227717=CARTESIAN_POINT('',(-30.9852566047563,-54.049038724998,3.40423097483272));
#227718=CARTESIAN_POINT('',(-29.4433108116256,-51.3783102687786,2.83404198860225));
#227719=CARTESIAN_POINT('',(0.164977839420945,-0.0952499999998041,2.83404198860262));
#227720=CARTESIAN_POINT('',(-29.6214601686928,-51.686874005141,3.40423097483274));
#227721=CARTESIAN_POINT('',(-29.4433108116256,-51.3783102687786,2.83404198860225));
#227722=CARTESIAN_POINT('',(-29.8368674217651,-52.0599703131947,3.64303198860225));
#227723=CARTESIAN_POINT('Origin',(-29.8177519105515,-52.0268612765601,3.20400220587275));
#227724=CARTESIAN_POINT('',(-30.0375573245347,-52.4075754198751,3.64303198860225));
#227725=CARTESIAN_POINT('',(-30.074486260907,-52.471538215424,3.64303198860225));
#227726=CARTESIAN_POINT('',(-30.1005764675353,-52.5167277788842,3.42473028058443));
#227727=CARTESIAN_POINT('',(-30.0375573238927,-52.4075754202458,3.64303198860225));
#227728=CARTESIAN_POINT('',(-30.2655565641139,-52.802481688396,3.23423028058444));
#227729=CARTESIAN_POINT('Origin',(-30.2508433300764,-52.7769965925045,3.56425743004421));
#227730=CARTESIAN_POINT('',(-30.3411606219514,-52.9334317578288,3.23423028058444));
#227731=CARTESIAN_POINT('',(-30.3414249774373,-52.9338896349618,3.23423028058444));
#227732=CARTESIAN_POINT('',(-30.5061406831638,-53.2191856060847,3.42473028058446));
#227733=CARTESIAN_POINT('Origin',(-30.3558761923104,-52.9589188467293,3.56425912917629));
#227734=CARTESIAN_POINT('',(-30.5691598004928,-53.3283379191465,3.64303198860225));
#227735=CARTESIAN_POINT('',(-30.5061406831638,-53.2191856060847,3.42473028058446));
#227736=CARTESIAN_POINT('',(-30.7701102637667,-53.6763943313414,3.64303198860224));
#227737=CARTESIAN_POINT('Origin',(-23.8720415006485,-53.1491210481984,2.65878198860224));
#227738=CARTESIAN_POINT('',(-23.9951532569802,-53.9314655730804,2.65878198860223));
#227739=CARTESIAN_POINT('',(-25.5480287005713,-57.4192809246789,2.65878198860221));
#227740=CARTESIAN_POINT('',(-23.6840886581931,-53.2328030451448,2.65878198860224));
#227741=CARTESIAN_POINT('',(-25.5758735661203,-57.406883591798,2.65878198860221));
#227742=CARTESIAN_POINT('Origin',(1.17012503474357E-17,1.90824895008066E-13,
2.65878198860263));
#227743=CARTESIAN_POINT('',(-24.0229981225292,-53.9190682401995,2.65878198860223));
#227744=CARTESIAN_POINT('',(-23.9942406030429,-53.8544777939069,2.65878198860223));
#227745=CARTESIAN_POINT('Origin',(3.6295324911301E-16,1.90620674808099E-13,
2.65878198860263));
#227746=CARTESIAN_POINT('Origin',(-0.174030409680916,0.077483330505849,
42.7590319886026));
#227747=CARTESIAN_POINT('',(-24.5797300649096,-54.7386155880004,3.64303198860224));
#227748=CARTESIAN_POINT('',(-24.4045020183941,-54.345046951707,3.40423097483272));
#227749=CARTESIAN_POINT('Origin',(-24.5641801073095,-54.7036898113979,3.20400220531965));
#227750=CARTESIAN_POINT('',(-24.259582275487,-54.0195518811804,2.83404198860223));
#227751=CARTESIAN_POINT('',(-24.4045020183941,-54.345046951707,3.40423097483272));
#227752=CARTESIAN_POINT('',(-25.6588335304436,-57.1623216544372,2.83404198860221));
#227753=CARTESIAN_POINT('',(-25.7644981330387,-57.3996482375657,2.83404198860221));
#227754=CARTESIAN_POINT('',(-25.5139139879318,-56.8368270312091,3.40423097483269));
#227755=CARTESIAN_POINT('',(-25.6588335304436,-57.1623216544371,2.83404198860221));
#227756=CARTESIAN_POINT('',(-25.3386861202872,-56.4432587981557,3.64303198860223));
#227757=CARTESIAN_POINT('Origin',(-25.3542361279701,-56.478184687246,3.20400259788053));
#227758=CARTESIAN_POINT('',(-25.1754303533071,-56.0765803402169,3.64303198860223));
#227759=CARTESIAN_POINT('',(-0.174030409680911,0.0774833305061222,3.64303198860263));
#227760=CARTESIAN_POINT('',(-25.1241659841931,-55.9614386837453,3.42473028058445));
#227761=CARTESIAN_POINT('',(-25.175430352657,-56.0765803405063,3.64303198860223));
#227762=CARTESIAN_POINT('',(-24.9899591116491,-55.6600051127008,3.23423028058442));
#227763=CARTESIAN_POINT('Origin',(-25.0019278517711,-55.6868886053389,3.56425722716884));
#227764=CARTESIAN_POINT('',(-24.9284572302736,-55.5218696254673,3.23423028058442));
#227765=CARTESIAN_POINT('',(-0.174030409680911,0.077483330506125,3.23423028058481));
#227766=CARTESIAN_POINT('',(-24.7942503289602,-55.2204359898057,3.42473028058442));
#227767=CARTESIAN_POINT('Origin',(-24.9164863690992,-55.4949838933612,3.56425909741228));
#227768=CARTESIAN_POINT('',(-24.7429859390908,-55.1052942849672,3.64303198860223));
#227769=CARTESIAN_POINT('',(-24.7942503289602,-55.2204359898057,3.42473028058442));
#227770=CARTESIAN_POINT('',(-0.174030409680911,0.0774833305061222,3.64303198860262));
#227771=CARTESIAN_POINT('Origin',(0.174030409680916,-0.0774833305060277,
42.7590319886026));
#227772=CARTESIAN_POINT('',(-24.9906253009254,-56.5982254591676,3.64303198860222));
#227773=CARTESIAN_POINT('',(-25.1658531680166,-56.9917936924673,3.40423097483269));
#227774=CARTESIAN_POINT('Origin',(-25.0061753084918,-56.6331513479964,3.20400259735859));
#227775=CARTESIAN_POINT('',(-25.3107727106681,-57.3172883156332,2.83404198860221));
#227776=CARTESIAN_POINT('',(-25.1658531680166,-56.9917936924673,3.40423097483269));
#227777=CARTESIAN_POINT('',(-23.911521456611,-54.174518541976,2.83404198860223));
#227778=CARTESIAN_POINT('',(0.174030409680924,-0.0774833305057438,2.83404198860262));
#227779=CARTESIAN_POINT('',(-24.0564411996779,-54.5000136124314,3.40423097483272));
#227780=CARTESIAN_POINT('',(-23.911521456611,-54.174518541976,2.83404198860223));
#227781=CARTESIAN_POINT('',(-24.2316692455478,-54.8935822490123,3.64303198860224));
#227782=CARTESIAN_POINT('Origin',(-24.2161192878243,-54.8586564721327,3.20400220587297));
#227783=CARTESIAN_POINT('',(-24.3949251204065,-55.2602609456775,3.64303198860224));
#227784=CARTESIAN_POINT('',(-24.4249658234761,-55.327733471309,3.64303198860224));
#227785=CARTESIAN_POINT('',(-24.4461895095984,-55.3754026508175,3.42473028058442));
#227786=CARTESIAN_POINT('',(-24.394925119729,-55.2602609459791,3.64303198860224));
#227787=CARTESIAN_POINT('',(-24.5803964109118,-55.6768362864792,3.23423028058442));
#227788=CARTESIAN_POINT('Origin',(-24.5684276954193,-55.6499528488651,3.56425743004285));
#227789=CARTESIAN_POINT('',(-24.6418982922872,-55.8149717737127,3.23423028058442));
#227790=CARTESIAN_POINT('',(-24.6421133384131,-55.8154547752195,3.23423028058442));
#227791=CARTESIAN_POINT('',(-24.7761051648312,-56.1164053447572,3.42473028058444));
#227792=CARTESIAN_POINT('Origin',(-24.6538691229758,-55.8418574376282,3.5642591291781));
#227793=CARTESIAN_POINT('',(-24.8273695332952,-56.2315470015182,3.64303198860223));
#227794=CARTESIAN_POINT('',(-24.7761051648312,-56.1164053447572,3.42473028058444));
#227795=CARTESIAN_POINT('',(-24.9908373670083,-56.5987017673883,3.64303198860222));
#227796=CARTESIAN_POINT('Origin',(-18.1856720123403,-55.3532724151365,2.65878198860223));
#227797=CARTESIAN_POINT('',(-18.2263320786577,-56.1441998575527,2.65878198860222));
#227798=CARTESIAN_POINT('',(-19.4061247292248,-59.7752282754837,2.6587819886022));
#227799=CARTESIAN_POINT('',(-17.9900016446778,-55.4168495715592,2.65878198860223));
#227800=CARTESIAN_POINT('',(-19.4351129318415,-59.7658094374951,2.6587819886022));
#227801=CARTESIAN_POINT('Origin',(-2.66410924515479E-18,1.90830409352964E-13,
2.65878198860263));
#227802=CARTESIAN_POINT('',(-18.2553202812744,-56.1347810195642,2.65878198860222));
#227803=CARTESIAN_POINT('',(-18.2334718385814,-56.0675384271753,2.65878198860222));
#227804=CARTESIAN_POINT('Origin',(3.7043280816289E-16,1.90617803674382E-13,
2.65878198860263));
#227805=CARTESIAN_POINT('Origin',(-0.181176266354227,0.0588677374283364,
42.7590319886026));
#227806=CARTESIAN_POINT('',(-18.7233363629819,-57.0080331356322,3.64303198860223));
#227807=CARTESIAN_POINT('',(-18.5902073587817,-56.5983041910846,3.4042309748327));
#227808=CARTESIAN_POINT('Origin',(-18.7115223274335,-56.9716732729172,3.2040022053177));
#227809=CARTESIAN_POINT('',(-18.4801050009129,-56.2594439785881,2.83404198860222));
#227810=CARTESIAN_POINT('',(-18.5902073587817,-56.5983041910846,3.4042309748327));
#227811=CARTESIAN_POINT('',(-19.5431821162861,-59.5312589135995,2.83404198860219));
#227812=CARTESIAN_POINT('',(-19.6234604941053,-59.7783303554049,2.83404198860219));
#227813=CARTESIAN_POINT('',(-19.4330799109586,-59.1923991668985,3.40423097483268));
#227814=CARTESIAN_POINT('',(-19.5431821162861,-59.5312589135995,2.83404198860219));
#227815=CARTESIAN_POINT('',(-19.2999510425001,-58.7826706420788,3.64303198860222));
#227816=CARTESIAN_POINT('Origin',(-19.3117651160993,-58.8190306219023,3.20400259788282));
#227817=CARTESIAN_POINT('',(-19.1759179434148,-58.4009360126568,3.64303198860221));
#227818=CARTESIAN_POINT('',(-0.181176266354222,0.0588677374286096,3.64303198860262));
#227819=CARTESIAN_POINT('',(-19.1369699862878,-58.281066528503,3.42473028058445));
#227820=CARTESIAN_POINT('',(-19.1759179427381,-58.4009360128767,3.64303198860221));
#227821=CARTESIAN_POINT('',(-19.0350067009925,-57.9672558039532,3.23423028058441));
#227822=CARTESIAN_POINT('Origin',(-19.0440997849304,-57.9952431000158,3.56425722717295));
#227823=CARTESIAN_POINT('',(-18.9882808235615,-57.8234483402239,3.23423028058441));
#227824=CARTESIAN_POINT('',(-0.181176266354222,0.0588677374286124,3.23423028058481));
#227825=CARTESIAN_POINT('',(-18.8863175164087,-57.5096375484037,3.4247302805844));
#227826=CARTESIAN_POINT('Origin',(-18.9791858642775,-57.7954585952473,3.56425909740992));
#227827=CARTESIAN_POINT('',(-18.8473695436957,-57.3897680139784,3.64303198860222));
#227828=CARTESIAN_POINT('',(-18.8863175164087,-57.5096375484037,3.4247302805844));
#227829=CARTESIAN_POINT('',(-0.181176266354222,0.0588677374286096,3.64303198860263));
#227830=CARTESIAN_POINT('Origin',(0.181176266354227,-0.0588677374285151,
42.7590319886026));
#227831=CARTESIAN_POINT('',(-18.9375985097916,-58.9004061169357,3.64303198860221));
#227832=CARTESIAN_POINT('',(-19.0707273776747,-59.3101346419424,3.40423097483268));
#227833=CARTESIAN_POINT('Origin',(-18.9494125833018,-58.9367660964848,3.20400259735645));
#227834=CARTESIAN_POINT('',(-19.1808295831472,-59.6489943885963,2.83404198860219));
#227835=CARTESIAN_POINT('',(-19.0707273776747,-59.3101346419424,3.40423097483268));
#227836=CARTESIAN_POINT('',(-18.1177524687101,-56.3771794532807,2.83404198860222));
#227837=CARTESIAN_POINT('',(0.181176266354235,-0.0588677374282309,2.83404198860262));
#227838=CARTESIAN_POINT('',(-18.2278548267447,-56.7160396657232,3.40423097483271));
#227839=CARTESIAN_POINT('',(-18.1177524687101,-56.3771794532807,2.83404198860222));
#227840=CARTESIAN_POINT('',(-18.3609838302735,-57.1257686104891,3.64303198860223));
#227841=CARTESIAN_POINT('Origin',(-18.3491697946312,-57.0894087474853,3.20400220587216));
#227842=CARTESIAN_POINT('',(-18.4850170116921,-57.5075034886062,3.64303198860222));
#227843=CARTESIAN_POINT('',(-18.5078403492304,-57.5777465012099,3.64303198860222));
#227844=CARTESIAN_POINT('',(-18.5239649837002,-57.6273730232605,3.4247302805844));
#227845=CARTESIAN_POINT('',(-18.4850170109872,-57.5075034888353,3.64303198860222));
#227846=CARTESIAN_POINT('',(-18.6259282908531,-57.9411838150807,3.23423028058441));
#227847=CARTESIAN_POINT('Origin',(-18.6168352256576,-57.9131965763137,3.56425743004373));
#227848=CARTESIAN_POINT('',(-18.672654168284,-58.08499127881,3.23423028058441));
#227849=CARTESIAN_POINT('',(-18.6728175489595,-58.0854941128251,3.23423028058441));
#227850=CARTESIAN_POINT('',(-18.7746174535794,-58.3988020033598,3.42473028058443));
#227851=CARTESIAN_POINT('Origin',(-18.6817491043762,-58.1129809527804,3.56425912918054));
#227852=CARTESIAN_POINT('',(-18.8135654100297,-58.5186714877335,3.64303198860222));
#227853=CARTESIAN_POINT('',(-18.7746174535794,-58.3988020033598,3.42473028058443));
#227854=CARTESIAN_POINT('',(-18.937759626388,-58.9009019828319,3.64303198860221));
#227855=CARTESIAN_POINT('Origin',(-12.3000564958684,-56.9509617460774,2.65878198860222));
#227856=CARTESIAN_POINT('',(-12.2578193919762,-57.7418065394565,2.65878198860222));
#227857=CARTESIAN_POINT('',(-13.0516031943522,-61.4762657165315,2.65878198860219));
#227858=CARTESIAN_POINT('',(-12.0988124084934,-56.9937374973463,2.65878198860222));
#227859=CARTESIAN_POINT('',(-13.0814171332226,-61.4699285681954,2.65878198860219));
#227860=CARTESIAN_POINT('Origin',(-1.75271798929367E-17,1.90834391900741E-13,
2.65878198860263));
#227861=CARTESIAN_POINT('',(-12.2876333308465,-57.7354693911204,2.65878198860222));
#227862=CARTESIAN_POINT('',(-12.2729333410573,-57.6663113765488,2.65878198860222));
#227863=CARTESIAN_POINT('Origin',(3.78171508600986E-16,1.90615730095849E-13,
2.65878198860263));
#227864=CARTESIAN_POINT('Origin',(-0.18633711793979,0.0396071771006919,
42.7590319886026));
#227865=CARTESIAN_POINT('',(-12.6618058697513,-58.6528587425322,3.64303198860222));
#227866=CARTESIAN_POINT('',(-12.5722344970954,-58.231458565788,3.40423097483269));
#227867=CARTESIAN_POINT('Origin',(-12.6538571933001,-58.6154631599695,3.20400220531593));
#227868=CARTESIAN_POINT('',(-12.4981558287385,-57.8829458347209,2.83404198860221));
#227869=CARTESIAN_POINT('',(-12.5722344970954,-58.231458565788,3.40423097483269));
#227870=CARTESIAN_POINT('',(-13.2134115091888,-61.2479592423877,2.83404198860219));
#227871=CARTESIAN_POINT('',(-13.2674241155254,-61.5020685764504,2.83404198860219));
#227872=CARTESIAN_POINT('',(-13.1393329438489,-60.8994469905092,3.40423097483268));
#227873=CARTESIAN_POINT('',(-13.2134115091888,-61.2479592423877,2.83404198860219));
#227874=CARTESIAN_POINT('',(-13.0497616623169,-60.4780472453827,3.64303198860221));
#227875=CARTESIAN_POINT('Origin',(-13.0577103643692,-60.5154429483892,3.20400259788019));
#227876=CARTESIAN_POINT('',(-12.966310163716,-60.0854388089605,3.64303198860221));
#227877=CARTESIAN_POINT('',(-0.186337117939785,0.0396071771009651,3.64303198860263));
#227878=CARTESIAN_POINT('',(-12.9401053405444,-59.9621548122771,3.42473028058443));
#227879=CARTESIAN_POINT('',(-12.9663101630198,-60.0854388091084,3.64303198860221));
#227880=CARTESIAN_POINT('',(-12.8715027735886,-59.6394051101893,3.2342302805844));
#227881=CARTESIAN_POINT('Origin',(-12.8776205756134,-59.6681895750089,3.5642572271675));
#227882=CARTESIAN_POINT('',(-12.8400648385932,-59.4915012546304,3.2342302805844));
#227883=CARTESIAN_POINT('',(-0.186337117939785,0.0396071771009679,3.23423028058481));
#227884=CARTESIAN_POINT('',(-12.7714622569314,-59.168751483356,3.42473028058439));
#227885=CARTESIAN_POINT('Origin',(-12.8339454274777,-59.4627141582888,3.56425909741086));
#227886=CARTESIAN_POINT('',(-12.7452574235141,-59.0454674350474,3.64303198860221));
#227887=CARTESIAN_POINT('',(-12.7714622569314,-59.168751483356,3.42473028058439));
#227888=CARTESIAN_POINT('',(-0.186337117939785,0.0396071771009651,3.64303198860263));
#227889=CARTESIAN_POINT('Origin',(0.18633711793979,-0.0396071771008706,
42.7590319886026));
#227890=CARTESIAN_POINT('',(-12.6770874264373,-60.5572615995843,3.6430319886022));
#227891=CARTESIAN_POINT('',(-12.7666587073768,-60.9786613448367,3.40423097483268));
#227892=CARTESIAN_POINT('Origin',(-12.6850361284299,-60.5946573023098,3.20400259735624));
#227893=CARTESIAN_POINT('',(-12.8407372728666,-61.3271735966833,2.83404198860219));
#227894=CARTESIAN_POINT('',(-12.7666587073768,-60.9786613448367,3.40423097483267));
#227895=CARTESIAN_POINT('',(-12.1254815933786,-57.962160188812,2.83404198860222));
#227896=CARTESIAN_POINT('',(0.186337117939797,-0.0396071771005863,2.83404198860263));
#227897=CARTESIAN_POINT('',(-12.1995602619071,-58.3106729198426,3.4042309748327));
#227898=CARTESIAN_POINT('',(-12.1254815933786,-57.962160188812,2.83404198860222));
#227899=CARTESIAN_POINT('',(-12.2891316338718,-58.7320730967337,3.64303198860222));
#227900=CARTESIAN_POINT('Origin',(-12.2811829573572,-58.6946775138729,3.20400220587262));
#227901=CARTESIAN_POINT('',(-12.37258318836,-59.1246817890948,3.64303198860221));
#227902=CARTESIAN_POINT('',(-12.387939103104,-59.1969256915253,3.64303198860221));
#227903=CARTESIAN_POINT('',(-12.3987880210518,-59.2479658375576,3.42473028058439));
#227904=CARTESIAN_POINT('',(-12.3725831876346,-59.124681789249,3.64303198860221));
#227905=CARTESIAN_POINT('',(-12.4673906027137,-59.570715608832,3.2342302805844));
#227906=CARTESIAN_POINT('Origin',(-12.4612728133404,-59.5419312029567,3.5642574300453));
#227907=CARTESIAN_POINT('',(-12.498828537709,-59.7186194643909,3.2342302805844));
#227908=CARTESIAN_POINT('',(-12.4989384629011,-59.7191366217596,3.2342302805844));
#227909=CARTESIAN_POINT('',(-12.5674311046648,-60.0413691664787,3.42473028058441));
#227910=CARTESIAN_POINT('Origin',(-12.5049479331826,-59.7474064876939,3.56425912917678));
#227911=CARTESIAN_POINT('',(-12.5936359271402,-60.16465316331,3.64303198860221));
#227912=CARTESIAN_POINT('',(-12.5674311046648,-60.0413691664787,3.42473028058441));
#227913=CARTESIAN_POINT('',(-12.67719582832,-60.5577715903454,3.6430319886022));
#227914=CARTESIAN_POINT('Origin',(-6.27967898647548,-57.9246844223734,2.65878198860221));
#227915=CARTESIAN_POINT('',(-6.15500747092256,-58.7067819056642,2.65878198860221));
#227916=CARTESIAN_POINT('',(-6.55408556365883,-62.5037563256533,2.65878198860218));
#227917=CARTESIAN_POINT('',(-6.07506605172241,-57.9461901084061,2.65878198860221));
#227918=CARTESIAN_POINT('',(-6.58439859102965,-62.500570298093,2.65878198860218));
#227919=CARTESIAN_POINT('Origin',(-3.27251186835868E-17,1.90836799017771E-13,
2.65878198860263));
#227920=CARTESIAN_POINT('',(-6.18532049829339,-58.7035958781038,2.65878198860221));
#227921=CARTESIAN_POINT('',(-6.17793001757209,-58.6332801510294,2.65878198860221));
#227922=CARTESIAN_POINT('Origin',(3.86084563605879E-16,1.90614476791061E-13,
2.65878198860263));
#227923=CARTESIAN_POINT('Origin',(-0.189456421067656,0.0199126722523968,
42.7590319886026));
#227924=CARTESIAN_POINT('',(-6.46154998175858,-59.6550713551491,3.64303198860221));
#227925=CARTESIAN_POINT('',(-6.4165176033499,-59.2266168947285,3.40423097483269));
#227926=CARTESIAN_POINT('Origin',(-6.45755375176689,-59.6170497665652,3.20400220531789));
#227927=CARTESIAN_POINT('',(-6.37927424589655,-58.8722700235035,2.8340419886022));
#227928=CARTESIAN_POINT('',(-6.4165176033499,-59.2266168947285,3.40423097483269));
#227929=CARTESIAN_POINT('',(-6.7388720005127,-62.2936141127568,2.83404198860218));
#227930=CARTESIAN_POINT('',(-6.76602706194884,-62.5519772640371,2.83404198860218));
#227931=CARTESIAN_POINT('',(-6.70162869542285,-61.9392677288636,3.40423097483267));
#227932=CARTESIAN_POINT('',(-6.7388720005127,-62.2936141127568,2.83404198860218));
#227933=CARTESIAN_POINT('',(-6.65659636252321,-61.5108137072211,3.6430319886022));
#227934=CARTESIAN_POINT('Origin',(-6.66059260538586,-61.5488354182639,3.20400259787953));
#227935=CARTESIAN_POINT('',(-6.61464077648837,-61.1116329639868,3.6430319886022));
#227936=CARTESIAN_POINT('',(-0.189456421067651,0.0199126722526699,3.64303198860263));
#227937=CARTESIAN_POINT('',(-6.60146619279885,-60.9862851800403,3.42473028058442));
#227938=CARTESIAN_POINT('',(-6.6146407757806,-61.1116329640611,3.6430319886022));
#227939=CARTESIAN_POINT('',(-6.56697596826216,-60.6581326136903,3.23423028058439));
#227940=CARTESIAN_POINT('Origin',(-6.5700514604535,-60.6873988786413,3.56425722717276));
#227941=CARTESIAN_POINT('',(-6.55117041629707,-60.5077528318942,3.23423028058439));
#227942=CARTESIAN_POINT('',(-0.189456421067651,0.0199126722526728,3.23423028058481));
#227943=CARTESIAN_POINT('',(-6.51668018436685,-60.1796001951994,3.42473028058439));
#227944=CARTESIAN_POINT('Origin',(-6.54809359889834,-60.478483781638,3.56425909741048));
#227945=CARTESIAN_POINT('',(-6.50350559588404,-60.0542523588396,3.64303198860221));
#227946=CARTESIAN_POINT('',(-6.51668018436685,-60.1796001951994,3.42473028058439));
#227947=CARTESIAN_POINT('',(-0.189456421067651,0.0199126722526699,3.64303198860263));
#227948=CARTESIAN_POINT('Origin',(0.189456421067656,-0.0199126722525754,
42.7590319886026));
#227949=CARTESIAN_POINT('',(-6.2776835203879,-61.5506390517261,3.64303198860219));
#227950=CARTESIAN_POINT('',(-6.32271585268578,-61.9790930734318,3.40423097483266));
#227951=CARTESIAN_POINT('Origin',(-6.28167976322058,-61.5886607624838,3.20400259735653));
#227952=CARTESIAN_POINT('',(-6.35995915792703,-62.3334394573091,2.83404198860218));
#227953=CARTESIAN_POINT('',(-6.32271585268577,-61.9790930734318,3.40423097483266));
#227954=CARTESIAN_POINT('',(-6.00036140428986,-58.9120953679529,2.8340419886022));
#227955=CARTESIAN_POINT('',(0.189456421067662,-0.0199126722522911,2.83404198860262));
#227956=CARTESIAN_POINT('',(-6.03760476191717,-59.2664422391596,3.40423097483269));
#227957=CARTESIAN_POINT('',(-6.00036140428986,-58.9120953679529,2.8340419886022));
#227958=CARTESIAN_POINT('',(-6.08263713962327,-59.6948966996541,3.64303198860221));
#227959=CARTESIAN_POINT('Origin',(-6.07864090959983,-59.6568751107683,3.20400220587196));
#227960=CARTESIAN_POINT('',(-6.12459275448642,-60.094077703267,3.6430319886022));
#227961=CARTESIAN_POINT('',(-6.13231300382116,-60.1675309762114,3.64303198860221));
#227962=CARTESIAN_POINT('',(-6.13776734223154,-60.2194255397044,3.42473028058439));
#227963=CARTESIAN_POINT('',(-6.12459275374873,-60.0940777033446,3.6430319886022));
#227964=CARTESIAN_POINT('',(-6.17225757416176,-60.5475781763992,3.23423028058439));
#227965=CARTESIAN_POINT('Origin',(-6.1691820883912,-60.5183119713912,3.56425743004905));
#227966=CARTESIAN_POINT('',(-6.18806312612685,-60.6979579581953,3.23423028058439));
#227967=CARTESIAN_POINT('',(-6.18811839147226,-60.6984837728332,3.23423028058439));
#227968=CARTESIAN_POINT('',(-6.22255335066353,-61.0261105245453,3.42473028058442));
#227969=CARTESIAN_POINT('Origin',(-6.19113993560378,-60.727226934177,3.56425912917781));
#227970=CARTESIAN_POINT('',(-6.23572793364529,-61.1514583085661,3.6430319886022));
#227971=CARTESIAN_POINT('',(-6.22255335066353,-61.0261105245453,3.42473028058442));
#227972=CARTESIAN_POINT('',(-6.27773801988317,-61.5511575797867,3.64303198860219));
#227973=CARTESIAN_POINT('Origin',(-0.190499999999384,-58.2637721346183,
2.65878198860221));
#227974=CARTESIAN_POINT('',(0.0152400000006159,-58.2637721346183,2.65878198860221));
#227975=CARTESIAN_POINT('',(-0.0152399999993768,-58.9578504383726,2.65878198860221));
#227976=CARTESIAN_POINT('Origin',(-0.1905,-9.13233322154995E-14,42.7590319886026));
#227977=CARTESIAN_POINT('',(-0.190499999999366,-60.0036905223729,3.64303198860221));
#227978=CARTESIAN_POINT('',(-0.19049999999937,-59.572876015004,3.40423097483269));
#227979=CARTESIAN_POINT('Origin',(-0.190499999999367,-59.9654595002501,
3.20400220531674));
#227980=CARTESIAN_POINT('',(-0.190499999467556,-59.2165773020939,2.8340419886022));
#227981=CARTESIAN_POINT('',(-0.19049999999937,-59.572876015004,3.40423097483268));
#227982=CARTESIAN_POINT('',(-0.190499999999337,-62.6567671111297,2.83404198860218));
#227983=CARTESIAN_POINT('',(-0.190499999999335,-62.9165533988761,2.83404198860218));
#227984=CARTESIAN_POINT('',(-0.19050000060547,-62.3004688883553,3.40423097483267));
#227985=CARTESIAN_POINT('',(-0.190499999999338,-62.6567671111297,2.83404198860218));
#227986=CARTESIAN_POINT('',(-0.190499999999346,-61.8696548221179,3.6430319886022));
#227987=CARTESIAN_POINT('Origin',(-0.190499999999346,-61.9078859673753,
3.20400259788085));
#227988=CARTESIAN_POINT('',(-0.190500000710895,-61.4682752798282,3.64303198860219));
#227989=CARTESIAN_POINT('',(-0.190499999999995,1.81822235884877E-13,3.64303198860263));
#227990=CARTESIAN_POINT('',(-0.190499999999352,-61.3422370451704,3.42473028058442));
#227991=CARTESIAN_POINT('',(-0.190499999999351,-61.4682752798282,3.64303198860219));
#227992=CARTESIAN_POINT('',(-0.190499999999355,-61.0122769227454,3.23423028058439));
#227993=CARTESIAN_POINT('Origin',(-0.190499486621758,-61.0417043405091,
3.56425722716995));
#227994=CARTESIAN_POINT('',(-0.190499999999357,-60.8610688070705,3.23423028058439));
#227995=CARTESIAN_POINT('',(-0.190499999999994,1.84676882954539E-13,3.23423028058481));
#227996=CARTESIAN_POINT('',(-0.19049999999936,-60.5311086139133,3.42473028058439));
#227997=CARTESIAN_POINT('Origin',(-0.190499486572858,-60.8316384807424,
3.5642590974155));
#227998=CARTESIAN_POINT('',(-0.190499999999362,-60.4050703266281,3.64303198860221));
#227999=CARTESIAN_POINT('',(-0.19049999999936,-60.5311086139133,3.42473028058439));
#228000=CARTESIAN_POINT('',(-0.190499999999995,1.81822235884877E-13,3.64303198860263));
#228001=CARTESIAN_POINT('Origin',(0.1905,-8.73325690452018E-14,42.7590319886026));
#228002=CARTESIAN_POINT('',(0.190500000000654,-61.8696548221179,3.64303198860219));
#228003=CARTESIAN_POINT('',(0.190500000000659,-62.3004688883553,3.40423097483266));
#228004=CARTESIAN_POINT('Origin',(0.190500000000654,-61.9078859670877,3.20400259735625));
#228005=CARTESIAN_POINT('',(0.190500000452861,-62.6567671111297,2.83404198860218));
#228006=CARTESIAN_POINT('',(0.190500000000658,-62.3004688883553,3.40423097483266));
#228007=CARTESIAN_POINT('',(0.190500000000626,-59.2165773020939,2.8340419886022));
#228008=CARTESIAN_POINT('',(0.190500000000006,1.97084259631206E-13,2.83404198860262));
#228009=CARTESIAN_POINT('',(0.190499999294164,-59.572876015004,3.40423097483268));
#228010=CARTESIAN_POINT('',(0.190500000000626,-59.2165773020939,2.8340419886022));
#228011=CARTESIAN_POINT('',(0.190500000000634,-60.0036905223729,3.64303198860221));
#228012=CARTESIAN_POINT('Origin',(0.190500000000634,-59.9654594999461,3.20400220587172));
#228013=CARTESIAN_POINT('',(0.190499999259116,-60.4050703266281,3.6430319886022));
#228014=CARTESIAN_POINT('',(0.190500000000639,-60.4789282006567,3.6430319886022));
#228015=CARTESIAN_POINT('',(0.19050000000064,-60.5311086139133,3.42473028058439));
#228016=CARTESIAN_POINT('',(0.190500000000638,-60.4050703266281,3.6430319886022));
#228017=CARTESIAN_POINT('',(0.190500000000643,-60.8610688070705,3.23423028058439));
#228018=CARTESIAN_POINT('Origin',(0.190499486503203,-60.8316414495922,3.5642574300447));
#228019=CARTESIAN_POINT('',(0.190500000000645,-61.0122769227454,3.23423028058439));
#228020=CARTESIAN_POINT('',(0.190500000000645,-61.0128056337173,3.23423028058439));
#228021=CARTESIAN_POINT('',(0.190500000000648,-61.3422370451704,3.42473028058441));
#228022=CARTESIAN_POINT('Origin',(0.190499486688746,-61.0417071743789,3.56425912918094));
#228023=CARTESIAN_POINT('',(0.190500000000649,-61.4682752798282,3.64303198860219));
#228024=CARTESIAN_POINT('',(0.190500000000648,-61.3422370451704,3.42473028058441));
#228025=CARTESIAN_POINT('',(0.190500000000654,-61.870176206376,3.64303198860219));
#228026=CARTESIAN_POINT('Origin',(5.90076614434134,-57.9645097668782,2.65878198860221));
#228027=CARTESIAN_POINT('',(6.18532049829458,-58.7035958781036,2.65878198860221));
#228028=CARTESIAN_POINT('',(6.58439859103091,-62.5005702980928,2.65878198860218));
#228029=CARTESIAN_POINT('',(6.10537907909441,-57.9430040808455,2.65878198860221));
#228030=CARTESIAN_POINT('',(6.55408556366009,-62.5037563256532,2.65878198860218));
#228031=CARTESIAN_POINT('Origin',(5.63142687537637E-15,1.85141914433439E-13,
2.65878198860263));
#228032=CARTESIAN_POINT('',(6.15500747092375,-58.706781905664,2.65878198860221));
#228033=CARTESIAN_POINT('',(6.14761699020245,-58.6364661785897,2.65878198860221));
#228034=CARTESIAN_POINT('Origin',(5.65479388299727E-15,1.8536176889664E-13,
2.65878198860263));
#228035=CARTESIAN_POINT('Origin',(-0.189456421067656,-0.0199126722525792,
42.7590319886026));
#228036=CARTESIAN_POINT('',(6.08263713962448,-59.694896699654,3.64303198860221));
#228037=CARTESIAN_POINT('',(6.03760476121579,-59.2664422392334,3.40423097483269));
#228038=CARTESIAN_POINT('Origin',(6.07864090963303,-59.6568751110724,3.20400220531323));
#228039=CARTESIAN_POINT('',(6.00036140481974,-58.9120953678972,2.83404198860221));
#228040=CARTESIAN_POINT('',(6.03760476121579,-59.2664422392333,3.40423097483269));
#228041=CARTESIAN_POINT('',(6.35995915837864,-62.3334394572616,2.83404198860219));
#228042=CARTESIAN_POINT('',(6.38711421981479,-62.5918026085419,2.83404198860219));
#228043=CARTESIAN_POINT('',(6.32271585208535,-61.9790930734949,3.40423097483267));
#228044=CARTESIAN_POINT('',(6.35995915837864,-62.3334394572616,2.83404198860219));
#228045=CARTESIAN_POINT('',(6.27768352038914,-61.5506390517259,3.6430319886022));
#228046=CARTESIAN_POINT('Origin',(6.28167976325193,-61.58866076277,3.20400259788151));
#228047=CARTESIAN_POINT('',(6.23572793293846,-61.1514583086404,3.6430319886022));
#228048=CARTESIAN_POINT('',(-0.18945642106765,-0.0199126722523061,3.64303198860263));
#228049=CARTESIAN_POINT('',(6.22255335066477,-61.0261105245452,3.42473028058442));
#228050=CARTESIAN_POINT('',(6.23572793364653,-61.151458308566,3.6430319886022));
#228051=CARTESIAN_POINT('',(6.18806312612808,-60.6979579581952,3.23423028058439));
#228052=CARTESIAN_POINT('Origin',(6.19113963945025,-60.727224115824,3.56425722716726));
#228053=CARTESIAN_POINT('',(6.17225757416298,-60.5475781763991,3.23423028058439));
#228054=CARTESIAN_POINT('',(-0.18945642106765,-0.0199126722523032,3.23423028058481));
#228055=CARTESIAN_POINT('',(6.13776734223276,-60.2194255397043,3.42473028058439));
#228056=CARTESIAN_POINT('Origin',(6.1691817779921,-60.518309018808,3.56425909741116));
#228057=CARTESIAN_POINT('',(6.12459275374995,-60.0940777033444,3.64303198860221));
#228058=CARTESIAN_POINT('',(6.13776734223276,-60.2194255397043,3.42473028058439));
#228059=CARTESIAN_POINT('',(-0.18945642106765,-0.0199126722523061,3.64303198860263));
#228060=CARTESIAN_POINT('Origin',(0.189456421067656,0.0199126722524006,
42.7590319886026));
#228061=CARTESIAN_POINT('',(6.65659636252446,-61.510813707221,3.64303198860219));
#228062=CARTESIAN_POINT('',(6.70162869482234,-61.9392677289267,3.40423097483266));
#228063=CARTESIAN_POINT('Origin',(6.66059260535715,-61.5488354179788,3.20400259735661));
#228064=CARTESIAN_POINT('',(6.73887200096456,-62.2936141127093,2.83404198860219));
#228065=CARTESIAN_POINT('',(6.70162869482234,-61.9392677289267,3.40423097483266));
#228066=CARTESIAN_POINT('',(6.37927424642637,-58.8722700234478,2.83404198860221));
#228067=CARTESIAN_POINT('',(0.189456421067661,0.019912672252685,2.83404198860263));
#228068=CARTESIAN_POINT('',(6.41651760264875,-59.2266168948022,3.40423097483269));
#228069=CARTESIAN_POINT('',(6.37927424642637,-58.8722700234478,2.83404198860221));
#228070=CARTESIAN_POINT('',(6.46154998175979,-59.655071355149,3.64303198860221));
#228071=CARTESIAN_POINT('Origin',(6.45755375173623,-59.617049766262,3.20400220587411));
#228072=CARTESIAN_POINT('',(6.50350559514774,-60.054252358917,3.64303198860221));
#228073=CARTESIAN_POINT('',(6.51122584595768,-60.1277056317062,3.64303198860221));
#228074=CARTESIAN_POINT('',(6.51668018436807,-60.1796001951993,3.42473028058439));
#228075=CARTESIAN_POINT('',(6.50350559588526,-60.0542523588395,3.64303198860221));
#228076=CARTESIAN_POINT('',(6.5511704162983,-60.5077528318941,3.23423028058439));
#228077=CARTESIAN_POINT('Origin',(6.54809390915869,-60.4784867342349,3.56425743004622));
#228078=CARTESIAN_POINT('',(6.56697596826339,-60.6581326136902,3.23423028058439));
#228079=CARTESIAN_POINT('',(6.5670312336088,-60.6586584283281,3.23423028058439));
#228080=CARTESIAN_POINT('',(6.60146619280008,-60.9862851800402,3.42473028058441));
#228081=CARTESIAN_POINT('Origin',(6.57005175674045,-60.687401696983,3.56425912917834));
#228082=CARTESIAN_POINT('',(6.61464077578184,-61.111632964061,3.6430319886022));
#228083=CARTESIAN_POINT('',(6.60146619280008,-60.9862851800402,3.42473028058441));
#228084=CARTESIAN_POINT('',(6.65665086201973,-61.5113322352816,3.64303198860219));
#228085=CARTESIAN_POINT('Origin',(11.92738225999,-57.0301761002787,2.65878198860222));
#228086=CARTESIAN_POINT('',(12.2876333308477,-57.7354693911201,2.65878198860222));
#228087=CARTESIAN_POINT('',(13.0814171332239,-61.4699285681951,2.65878198860219));
#228088=CARTESIAN_POINT('',(12.128626347365,-56.9874003490099,2.65878198860222));
#228089=CARTESIAN_POINT('',(13.0516031943535,-61.4762657165312,2.65878198860219));
#228090=CARTESIAN_POINT('Origin',(5.61622893658571E-15,1.8513950731641E-13,
2.65878198860263));
#228091=CARTESIAN_POINT('',(12.2578193919774,-57.7418065394563,2.65878198860222));
#228092=CARTESIAN_POINT('',(12.2431194021881,-57.6726485248847,2.65878198860222));
#228093=CARTESIAN_POINT('Origin',(5.66270693800216E-15,1.85363022201428E-13,
2.65878198860263));
#228094=CARTESIAN_POINT('Origin',(-0.18633711793979,-0.0396071771008745,
42.7590319886026));
#228095=CARTESIAN_POINT('',(12.289131633873,-58.7320730967335,3.64303198860222));
#228096=CARTESIAN_POINT('',(12.1995602612171,-58.3106729199893,3.4042309748327));
#228097=CARTESIAN_POINT('Origin',(12.2811829574217,-58.6946775141705,3.20400220531643));
#228098=CARTESIAN_POINT('',(12.1254815938998,-57.9621601887012,2.83404198860222));
#228099=CARTESIAN_POINT('',(12.1995602612171,-58.3106729199893,3.4042309748327));
#228100=CARTESIAN_POINT('',(12.8407372733105,-61.327173596589,2.83404198860219));
#228101=CARTESIAN_POINT('',(12.8947498796471,-61.5812829306517,2.83404198860219));
#228102=CARTESIAN_POINT('',(12.7666587067861,-60.9786613449623,3.40423097483267));
#228103=CARTESIAN_POINT('',(12.8407372733105,-61.327173596589,2.8340419886022));
#228104=CARTESIAN_POINT('',(12.6770874264386,-60.557261599584,3.64303198860221));
#228105=CARTESIAN_POINT('Origin',(12.6850361284912,-60.5946573025921,3.20400259788329));
#228106=CARTESIAN_POINT('',(12.5936359264454,-60.1646531634577,3.64303198860221));
#228107=CARTESIAN_POINT('',(-0.186337117939784,-0.0396071771006013,3.64303198860263));
#228108=CARTESIAN_POINT('',(12.5674311046661,-60.0413691664784,3.42473028058443));
#228109=CARTESIAN_POINT('',(12.5936359271415,-60.1646531633097,3.64303198860221));
#228110=CARTESIAN_POINT('',(12.4988285377103,-59.7186194643906,3.2342302805844));
#228111=CARTESIAN_POINT('Origin',(12.5049473440529,-59.7474037157344,3.56425722716985));
#228112=CARTESIAN_POINT('',(12.4673906027149,-59.5707156088318,3.2342302805844));
#228113=CARTESIAN_POINT('',(-0.186337117939784,-0.0396071771005985,3.23423028058481));
#228114=CARTESIAN_POINT('',(12.398788021053,-59.2479658375573,3.4247302805844));
#228115=CARTESIAN_POINT('Origin',(12.461272196013,-59.5419282989947,3.56425909740943));
#228116=CARTESIAN_POINT('',(12.3725831876358,-59.1246817892487,3.64303198860221));
#228117=CARTESIAN_POINT('',(12.398788021053,-59.2479658375573,3.4247302805844));
#228118=CARTESIAN_POINT('',(-0.186337117939784,-0.0396071771006013,3.64303198860263));
#228119=CARTESIAN_POINT('Origin',(0.18633711793979,0.0396071771006958,42.7590319886026));
#228120=CARTESIAN_POINT('',(13.0497616623182,-60.4780472453824,3.6430319886022));
#228121=CARTESIAN_POINT('',(13.1393329432576,-60.8994469906349,3.40423097483267));
#228122=CARTESIAN_POINT('Origin',(13.0577103643107,-60.5154429481078,3.20400259735575));
#228123=CARTESIAN_POINT('',(13.2134115096327,-61.2479592422933,2.8340419886022));
#228124=CARTESIAN_POINT('',(13.1393329432576,-60.8994469906349,3.40423097483267));
#228125=CARTESIAN_POINT('',(12.4981558292594,-57.8829458346102,2.83404198860222));
#228126=CARTESIAN_POINT('',(0.186337117939794,0.0396071771009801,2.83404198860263));
#228127=CARTESIAN_POINT('',(12.5722344964055,-58.2314585659346,3.4042309748327));
#228128=CARTESIAN_POINT('',(12.4981558292594,-57.8829458346102,2.83404198860222));
#228129=CARTESIAN_POINT('',(12.6618058697526,-58.6528587425319,3.64303198860222));
#228130=CARTESIAN_POINT('Origin',(12.653857193238,-58.6154631596709,3.20400220587288));
#228131=CARTESIAN_POINT('',(12.7452574227896,-59.0454674352014,3.64303198860221));
#228132=CARTESIAN_POINT('',(12.7606133389849,-59.1177113373235,3.64303198860221));
#228133=CARTESIAN_POINT('',(12.7714622569326,-59.1687514833557,3.4247302805844));
#228134=CARTESIAN_POINT('',(12.7452574235154,-59.0454674350471,3.64303198860221));
#228135=CARTESIAN_POINT('',(12.8400648385945,-59.4915012546302,3.2342302805844));
#228136=CARTESIAN_POINT('Origin',(12.8339460446681,-59.4627170622764,3.56425743004005));
#228137=CARTESIAN_POINT('',(12.8715027735898,-59.639405110189,3.2342302805844));
#228138=CARTESIAN_POINT('',(12.871612698782,-59.6399222675577,3.2342302805844));
#228139=CARTESIAN_POINT('',(12.9401053405456,-59.9621548122768,3.42473028058442));
#228140=CARTESIAN_POINT('Origin',(12.8776211648735,-59.6681923469374,3.56425912918013));
#228141=CARTESIAN_POINT('',(12.966310163021,-60.0854388091081,3.64303198860221));
#228142=CARTESIAN_POINT('',(12.9401053405456,-59.9621548122768,3.42473028058442));
#228143=CARTESIAN_POINT('',(13.0498700642008,-60.4785572361435,3.6430319886022));
#228144=CARTESIAN_POINT('Origin',(17.823319479633,-55.471007889993,2.65878198860223));
#228145=CARTESIAN_POINT('',(18.2553202812755,-56.1347810195638,2.65878198860223));
#228146=CARTESIAN_POINT('',(19.4351129318427,-59.7658094374947,2.6587819886022));
#228147=CARTESIAN_POINT('',(18.0189898472955,-55.4074307335703,2.65878198860223));
#228148=CARTESIAN_POINT('',(19.406124729226,-59.7752282754833,2.6587819886022));
#228149=CARTESIAN_POINT('Origin',(5.60136586593793E-15,1.85135524768633E-13,
2.65878198860263));
#228150=CARTESIAN_POINT('',(18.2263320786588,-56.1441998575524,2.65878198860223));
#228151=CARTESIAN_POINT('',(18.2044836359659,-56.0769572651635,2.65878198860223));
#228152=CARTESIAN_POINT('Origin',(5.67044563844026E-15,1.85365095779961E-13,
2.65878198860263));
#228153=CARTESIAN_POINT('Origin',(-0.181176266354226,-0.0588677374285187,
42.7590319886026));
#228154=CARTESIAN_POINT('',(18.3609838302746,-57.1257686104887,3.64303198860223));
#228155=CARTESIAN_POINT('',(18.2278548260744,-56.716039665941,3.40423097483271));
#228156=CARTESIAN_POINT('Origin',(18.3491697947263,-57.089408747774,3.20400220531739));
#228157=CARTESIAN_POINT('',(18.1177524692163,-56.3771794531162,2.83404198860223));
#228158=CARTESIAN_POINT('',(18.2278548260744,-56.716039665941,3.40423097483271));
#228159=CARTESIAN_POINT('',(19.1808295835788,-59.648994388456,2.83404198860221));
#228160=CARTESIAN_POINT('',(19.261107961398,-59.8960658302613,2.8340419886022));
#228161=CARTESIAN_POINT('',(19.0707273770999,-59.3101346421291,3.40423097483269));
#228162=CARTESIAN_POINT('',(19.1808295835788,-59.648994388456,2.83404198860221));
#228163=CARTESIAN_POINT('',(18.9375985097928,-58.9004061169353,3.64303198860222));
#228164=CARTESIAN_POINT('Origin',(18.9494125833922,-58.9367660967591,3.2040025978833));
#228165=CARTESIAN_POINT('',(18.8135654093539,-58.5186714879531,3.64303198860221));
#228166=CARTESIAN_POINT('',(-0.181176266354221,-0.0588677374282456,3.64303198860263));
#228167=CARTESIAN_POINT('',(18.7746174535806,-58.3988020033594,3.42473028058444));
#228168=CARTESIAN_POINT('',(18.8135654100308,-58.5186714877332,3.64303198860222));
#228169=CARTESIAN_POINT('',(18.6726541682852,-58.0849912788097,3.23423028058441));
#228170=CARTESIAN_POINT('Origin',(18.6817482287255,-58.1129782575881,3.56425722717241));
#228171=CARTESIAN_POINT('',(18.6259282908542,-57.9411838150804,3.23423028058441));
#228172=CARTESIAN_POINT('',(-0.181176266354221,-0.0588677374282427,3.23423028058481));
#228173=CARTESIAN_POINT('',(18.5239649837014,-57.6273730232602,3.4247302805844));
#228174=CARTESIAN_POINT('Origin',(18.6168343081654,-57.9131937527885,3.56425909740864));
#228175=CARTESIAN_POINT('',(18.4850170109884,-57.5075034888349,3.64303198860222));
#228176=CARTESIAN_POINT('',(18.5239649837014,-57.6273730232602,3.4247302805844));
#228177=CARTESIAN_POINT('',(-0.181176266354221,-0.0588677374282456,3.64303198860263));
#228178=CARTESIAN_POINT('Origin',(0.181176266354226,0.0588677374283401,
42.7590319886026));
#228179=CARTESIAN_POINT('',(19.2999510425012,-58.7826706420785,3.64303198860222));
#228180=CARTESIAN_POINT('',(19.4330799103844,-59.1923991670851,3.40423097483269));
#228181=CARTESIAN_POINT('Origin',(19.3117651160117,-58.8190306216285,3.20400259735858));
#228182=CARTESIAN_POINT('',(19.5431821167169,-59.5312589134596,2.83404198860221));
#228183=CARTESIAN_POINT('',(19.4330799103844,-59.1923991670851,3.40423097483269));
#228184=CARTESIAN_POINT('',(18.4801050014197,-56.2594439784235,2.83404198860223));
#228185=CARTESIAN_POINT('',(0.18117626635423,0.0588677374286242,2.83404198860263));
#228186=CARTESIAN_POINT('',(18.5902073581109,-56.5983041913025,3.40423097483271));
#228187=CARTESIAN_POINT('',(18.4801050014197,-56.2594439784235,2.83404198860223));
#228188=CARTESIAN_POINT('',(18.7233363629831,-57.0080331356318,3.64303198860223));
#228189=CARTESIAN_POINT('Origin',(18.7115223273407,-56.9716732726276,3.20400220587314));
#228190=CARTESIAN_POINT('',(18.8473695429913,-57.3897680142073,3.64303198860223));
#228191=CARTESIAN_POINT('',(18.8701928819401,-57.4600110263526,3.64303198860222));
#228192=CARTESIAN_POINT('',(18.8863175164099,-57.5096375484033,3.42473028058439));
#228193=CARTESIAN_POINT('',(18.8473695436968,-57.389768013978,3.64303198860223));
#228194=CARTESIAN_POINT('',(18.9882808235627,-57.8234483402235,3.23423028058441));
#228195=CARTESIAN_POINT('Origin',(18.979186781637,-57.7954614188149,3.5642574300438));
#228196=CARTESIAN_POINT('',(19.0350067009936,-57.9672558039528,3.23423028058441));
#228197=CARTESIAN_POINT('',(19.0351700816691,-57.9677586379679,3.23423028058441));
#228198=CARTESIAN_POINT('',(19.136969986289,-58.2810665285026,3.42473028058442));
#228199=CARTESIAN_POINT('Origin',(19.0441006607087,-57.9952457951678,3.56425912917952));
#228200=CARTESIAN_POINT('',(19.1759179427393,-58.4009360128763,3.64303198860222));
#228201=CARTESIAN_POINT('',(19.136969986289,-58.2810665285026,3.42473028058442));
#228202=CARTESIAN_POINT('',(19.3001121590976,-58.7831665079746,3.64303198860222));
#228203=CARTESIAN_POINT('Origin',(23.5239806812878,-53.3040877092098,2.65878198860225));
#228204=CARTESIAN_POINT('',(24.0229981225303,-53.919068240199,2.65878198860224));
#228205=CARTESIAN_POINT('',(25.5758735661215,-57.4068835917975,2.65878198860222));
#228206=CARTESIAN_POINT('',(23.7119335237431,-53.2204057122634,2.65878198860225));
#228207=CARTESIAN_POINT('',(25.5480287005725,-57.4192809246784,2.65878198860222));
#228208=CARTESIAN_POINT('Origin',(5.58700050634534E-15,1.85130010423735E-13,
2.65878198860263));
#228209=CARTESIAN_POINT('',(23.9951532569813,-53.93146557308,2.65878198860224));
#228210=CARTESIAN_POINT('',(23.966395737495,-53.8668751267874,2.65878198860224));
#228211=CARTESIAN_POINT('Origin',(5.67792519749014E-15,1.85367966913678E-13,
2.65878198860263));
#228212=CARTESIAN_POINT('Origin',(-0.174030409680915,-0.0774833305060312,
42.7590319886026));
#228213=CARTESIAN_POINT('',(24.2316692455489,-54.8935822490118,3.64303198860224));
#228214=CARTESIAN_POINT('',(24.0564411990333,-54.5000136127184,3.40423097483272));
#228215=CARTESIAN_POINT('Origin',(24.2161192879494,-54.8586564724106,3.20400220531692));
#228216=CARTESIAN_POINT('',(23.9115214570976,-54.1745185417594,2.83404198860224));
#228217=CARTESIAN_POINT('',(24.0564411990333,-54.5000136127184,3.40423097483272));
#228218=CARTESIAN_POINT('',(25.3107727110829,-57.3172883154485,2.83404198860222));
#228219=CARTESIAN_POINT('',(25.416437313678,-57.5546148985771,2.83404198860222));
#228220=CARTESIAN_POINT('',(25.1658531674655,-56.9917936927127,3.4042309748327));
#228221=CARTESIAN_POINT('',(25.3107727110829,-57.3172883154485,2.83404198860222));
#228222=CARTESIAN_POINT('',(24.9906253009265,-56.5982254591671,3.64303198860224));
#228223=CARTESIAN_POINT('Origin',(25.0061753086093,-56.6331513482572,3.2040025978802));
#228224=CARTESIAN_POINT('',(24.8273695326461,-56.2315470018072,3.64303198860223));
#228225=CARTESIAN_POINT('',(-0.174030409680909,-0.077483330505758,3.64303198860262));
#228226=CARTESIAN_POINT('',(24.7761051648324,-56.1164053447567,3.42473028058445));
#228227=CARTESIAN_POINT('',(24.8273695332963,-56.2315470015177,3.64303198860223));
#228228=CARTESIAN_POINT('',(24.6418982922884,-55.8149717737122,3.23423028058442));
#228229=CARTESIAN_POINT('Origin',(24.653867970398,-55.8418548487315,3.56425722716896));
#228230=CARTESIAN_POINT('',(24.5803964109129,-55.6768362864787,3.23423028058442));
#228231=CARTESIAN_POINT('',(-0.174030409680909,-0.0774833305057552,3.23423028058481));
#228232=CARTESIAN_POINT('',(24.4461895095995,-55.375402650817,3.42473028058442));
#228233=CARTESIAN_POINT('Origin',(24.5684264878159,-55.649950136715,3.56425909741445));
#228234=CARTESIAN_POINT('',(24.3949251197301,-55.2602609459786,3.64303198860224));
#228235=CARTESIAN_POINT('',(24.4461895095995,-55.375402650817,3.42473028058442));
#228236=CARTESIAN_POINT('',(-0.174030409680909,-0.077483330505758,3.64303198860263));
#228237=CARTESIAN_POINT('Origin',(0.174030409680915,0.0774833305058525,
42.7590319886026));
#228238=CARTESIAN_POINT('',(25.3386861202883,-56.4432587981552,3.64303198860224));
#228239=CARTESIAN_POINT('',(25.5139139873796,-56.8368270314549,3.4042309748327));
#228240=CARTESIAN_POINT('Origin',(25.3542361278552,-56.4781846869849,3.20400259736081));
#228241=CARTESIAN_POINT('',(25.6588335308581,-57.1623216542526,2.83404198860222));
#228242=CARTESIAN_POINT('',(25.5139139873796,-56.8368270314549,3.4042309748327));
#228243=CARTESIAN_POINT('',(24.2595822759739,-54.0195518809636,2.83404198860224));
#228244=CARTESIAN_POINT('',(0.174030409680918,0.0774833305061365,2.83404198860263));
#228245=CARTESIAN_POINT('',(24.4045020177497,-54.3450469519939,3.40423097483273));
#228246=CARTESIAN_POINT('',(24.2595822759739,-54.0195518809636,2.83404198860224));
#228247=CARTESIAN_POINT('',(24.5797300649108,-54.7386155879999,3.64303198860224));
#228248=CARTESIAN_POINT('Origin',(24.564180107187,-54.7036898111196,3.20400220587456));
#228249=CARTESIAN_POINT('',(24.7429859384147,-55.1052942852682,3.64303198860224));
#228250=CARTESIAN_POINT('',(24.773026642839,-55.1727668102967,3.64303198860224));
#228251=CARTESIAN_POINT('',(24.7942503289613,-55.2204359898052,3.42473028058442));
#228252=CARTESIAN_POINT('',(24.7429859390919,-55.1052942849667,3.64303198860224));
#228253=CARTESIAN_POINT('',(24.9284572302748,-55.5218696254668,3.23423028058442));
#228254=CARTESIAN_POINT('Origin',(24.9164875765751,-55.4949866055679,3.56425743004029));
#228255=CARTESIAN_POINT('',(24.9899591116502,-55.6600051127003,3.23423028058443));
#228256=CARTESIAN_POINT('',(24.9901741577761,-55.6604881142071,3.23423028058443));
#228257=CARTESIAN_POINT('',(25.1241659841942,-55.9614386837448,3.42473028058445));
#228258=CARTESIAN_POINT('Origin',(25.0019290044718,-55.6868911941825,3.564259129176));
#228259=CARTESIAN_POINT('',(25.1754303526582,-56.0765803405058,3.64303198860224));
#228260=CARTESIAN_POINT('',(25.1241659841942,-55.9614386837448,3.42473028058445));
#228261=CARTESIAN_POINT('',(25.3388981863712,-56.4437351063759,3.64303198860224));
#228262=CARTESIAN_POINT('Origin',(28.9669082278889,-50.553156788887,2.65878198860227));
#228263=CARTESIAN_POINT('',(29.5274749692191,-51.1126068659042,2.65878198860226));
#228264=CARTESIAN_POINT('',(31.4364195775141,-54.4189959163058,2.65878198860224));
#228265=CARTESIAN_POINT('',(29.1450842944635,-50.450286788887,2.65878198860227));
#228266=CARTESIAN_POINT('',(31.4100231232068,-54.4342359163058,2.65878198860224));
#228267=CARTESIAN_POINT('Origin',(5.57329024769379E-15,1.85123024698033E-13,
2.65878198860263));
#228268=CARTESIAN_POINT('',(29.5010785149117,-51.1278468659042,2.65878198860226));
#228269=CARTESIAN_POINT('',(29.4657269920333,-51.0666162321539,2.65878198860226));
#228270=CARTESIAN_POINT('Origin',(5.68506366753766E-15,1.85371604145838E-13,
2.65878198860263));
#228271=CARTESIAN_POINT('Origin',(-0.164977839420934,-0.0952500000000912,
42.7590319886026));
#228272=CARTESIAN_POINT('',(29.8368674217662,-52.0599703131941,3.64303198860226));
#228273=CARTESIAN_POINT('',(29.6214601680818,-51.6868740054938,3.40423097483274));
#228274=CARTESIAN_POINT('Origin',(29.8177519107049,-52.0268612768232,3.20400220531664));
#228275=CARTESIAN_POINT('',(29.4433108120869,-51.3783102685122,2.83404198860226));
#228276=CARTESIAN_POINT('',(29.6214601680818,-51.6868740054938,3.40423097483274));
#228277=CARTESIAN_POINT('',(31.1634057161447,-54.3576020372433,2.83404198860224));
#228278=CARTESIAN_POINT('',(31.2932988600179,-54.5825835619865,2.83404198860223));
#228279=CARTESIAN_POINT('',(30.9852566042328,-54.0490387253002,3.40423097483274));
#228280=CARTESIAN_POINT('',(31.1634057161447,-54.3576020372433,2.83404198860224));
#228281=CARTESIAN_POINT('',(30.7698495716387,-53.6759427993281,3.64303198860226));
#228282=CARTESIAN_POINT('Origin',(30.7889651442677,-53.7090519423374,3.20400259788206));
#228283=CARTESIAN_POINT('',(30.5691597998771,-53.328337919502,3.64303198860225));
#228284=CARTESIAN_POINT('',(-0.164977839420929,-0.0952499999998181,3.64303198860262));
#228285=CARTESIAN_POINT('',(30.506140683165,-53.219185606084,3.42473028058449));
#228286=CARTESIAN_POINT('',(30.5691598004939,-53.3283379191459,3.64303198860225));
#228287=CARTESIAN_POINT('',(30.3411606219525,-52.9334317578282,3.23423028058445));
#228288=CARTESIAN_POINT('Origin',(30.3558747754316,-52.9589163924893,3.56425722717266));
#228289=CARTESIAN_POINT('',(30.265556564115,-52.8024816883954,3.23423028058445));
#228290=CARTESIAN_POINT('',(-0.164977839420929,-0.0952499999998153,3.23423028058481));
#228291=CARTESIAN_POINT('',(30.1005764675364,-52.5167277788836,3.42473028058445));
#228292=CARTESIAN_POINT('Origin',(30.250841845591,-52.7769940214396,3.56425909741364));
#228293=CARTESIAN_POINT('',(30.0375573238938,-52.4075754202451,3.64303198860226));
#228294=CARTESIAN_POINT('',(30.1005764675364,-52.5167277788836,3.42473028058445));
#228295=CARTESIAN_POINT('',(-0.164977839420929,-0.0952499999998181,3.64303198860262));
#228296=CARTESIAN_POINT('Origin',(0.164977839420934,0.0952499999999126,
42.7590319886026));
#228297=CARTESIAN_POINT('',(31.0998052504806,-53.4854427993281,3.64303198860226));
#228298=CARTESIAN_POINT('',(31.3152122835993,-53.8585387249973,3.40423097483272));
#228299=CARTESIAN_POINT('Origin',(31.1189208229655,-53.5185519420876,3.20400259735637));
#228300=CARTESIAN_POINT('',(31.4933613953782,-54.1671020370171,2.83404198860224));
#228301=CARTESIAN_POINT('',(31.3152122835993,-53.8585387249973,3.40423097483272));
#228302=CARTESIAN_POINT('',(29.7732664904686,-51.1878102687779,2.83404198860226));
#228303=CARTESIAN_POINT('',(0.164977839420937,0.0952500000001963,2.83404198860262));
#228304=CARTESIAN_POINT('',(29.9514158463116,-51.4963740058471,3.40423097483275));
#228305=CARTESIAN_POINT('',(29.7732664904686,-51.1878102687779,2.83404198860226));
#228306=CARTESIAN_POINT('',(30.1668231006081,-51.8694703131941,3.64303198860227));
#228307=CARTESIAN_POINT('Origin',(30.1477075893944,-51.8363612765593,3.20400220587301));
#228308=CARTESIAN_POINT('',(30.3675130020933,-52.217075420616,3.64303198860227));
#228309=CARTESIAN_POINT('',(30.40444193975,-52.2810382154234,3.64303198860227));
#228310=CARTESIAN_POINT('',(30.4305321463783,-52.3262277788836,3.42473028058445));
#228311=CARTESIAN_POINT('',(30.3675130027357,-52.2170754202451,3.64303198860227));
#228312=CARTESIAN_POINT('',(30.5955122429569,-52.6119816883954,3.23423028058445));
#228313=CARTESIAN_POINT('Origin',(30.5807981195161,-52.586497106002,3.5642574300457));
#228314=CARTESIAN_POINT('',(30.6711163007943,-52.7429317578282,3.23423028058445));
#228315=CARTESIAN_POINT('',(30.6713806562803,-52.7433896349612,3.23423028058445));
#228316=CARTESIAN_POINT('',(30.8360963620068,-53.028685606084,3.42473028058447));
#228317=CARTESIAN_POINT('Origin',(30.6858309820709,-52.7684193600401,3.56425912917733));
#228318=CARTESIAN_POINT('',(30.8991154793358,-53.1378379191459,3.64303198860226));
#228319=CARTESIAN_POINT('',(30.8360963620068,-53.028685606084,3.42473028058447));
#228320=CARTESIAN_POINT('',(31.1000659426097,-53.4858943313408,3.64303198860226));
#228321=CARTESIAN_POINT('Origin',(34.09246826623,-47.248354903857,2.6587819886023));
#228322=CARTESIAN_POINT('',(34.7084426211237,-47.7461450747859,2.65878198860229));
#228323=CARTESIAN_POINT('',(36.9525415975218,-50.834882333648,2.65878198860227));
#228324=CARTESIAN_POINT('',(34.2589154226527,-47.1274239660504,2.6587819886023));
#228325=CARTESIAN_POINT('',(36.9278827595333,-50.8527980281379,2.65878198860227));
#228326=CARTESIAN_POINT('Origin',(5.5603853024461E-15,1.85114644128599E-13,
2.65878198860263));
#228327=CARTESIAN_POINT('',(34.6837837831351,-47.7640607692757,2.65878198860229));
#228328=CARTESIAN_POINT('',(34.6422255755471,-47.7068608037044,2.65878198860229));
#228329=CARTESIAN_POINT('Origin',(5.69178283801114E-15,1.85375967626163E-13,
2.65878198860263));
#228330=CARTESIAN_POINT('Origin',(-0.154117737428426,-0.111973090561807,
42.7590319886026));
#228331=CARTESIAN_POINT('',(35.1151666347447,-48.6559784483759,3.64303198860229));
#228332=CARTESIAN_POINT('',(34.8619402208396,-48.3074421904912,3.40423097483276));
#228333=CARTESIAN_POINT('Origin',(35.0926950037607,-48.6250489017661,3.20400220531733));
#228334=CARTESIAN_POINT('',(34.6525130924105,-48.0191904763605,2.83404198860228));
#228335=CARTESIAN_POINT('',(34.8619402208396,-48.3074421904912,3.40423097483276));
#228336=CARTESIAN_POINT('',(36.6746059268184,-50.8023624960585,2.83404198860226));
#228337=CARTESIAN_POINT('',(36.8273044755035,-51.0125340177509,2.83404198860226));
#228338=CARTESIAN_POINT('',(36.4651790855638,-50.5141111791242,3.40423097483275));
#228339=CARTESIAN_POINT('',(36.6746059268184,-50.8023624960585,2.83404198860226));
#228340=CARTESIAN_POINT('',(36.2119529314391,-50.1655752777666,3.64303198860229));
#228341=CARTESIAN_POINT('Origin',(36.2344246348003,-50.1965049239951,3.20400259788241));
#228342=CARTESIAN_POINT('',(35.9760279553338,-49.8408524072779,3.64303198860228));
#228343=CARTESIAN_POINT('',(-0.154117737428421,-0.111973090561534,3.64303198860262));
#228344=CARTESIAN_POINT('',(35.9019445403524,-49.7388853330806,3.42473028058451));
#228345=CARTESIAN_POINT('',(35.9760279559093,-49.8408524068598,3.64303198860228));
#228346=CARTESIAN_POINT('',(35.7079988465464,-49.4719419865727,3.23423028058448));
#228347=CARTESIAN_POINT('Origin',(35.7252962640508,-49.4957489658865,3.56425722717396));
#228348=CARTESIAN_POINT('',(35.6191209461258,-49.3496120513043,3.23423028058447));
#228349=CARTESIAN_POINT('',(-0.154117737428421,-0.111973090561531,3.23423028058481));
#228350=CARTESIAN_POINT('',(35.4251752107443,-49.0826686475729,3.42473028058447));
#228351=CARTESIAN_POINT('Origin',(35.6018226497107,-49.3258021153704,3.56425909741572));
#228352=CARTESIAN_POINT('',(35.3510917642539,-48.9807015312173,3.64303198860228));
#228353=CARTESIAN_POINT('',(35.4251752107443,-49.0826686475729,3.42473028058447));
#228354=CARTESIAN_POINT('',(-0.154117737428421,-0.111973090561534,3.64303198860262));
#228355=CARTESIAN_POINT('Origin',(0.154117737428426,0.111973090561629,42.7590319886026));
#228356=CARTESIAN_POINT('',(36.5201884062959,-49.9416290966431,3.64303198860228));
#228357=CARTESIAN_POINT('',(36.7734145609104,-50.2901649976449,3.40423097483275));
#228358=CARTESIAN_POINT('Origin',(36.5426601094879,-49.9725587426388,3.20400259735788));
#228359=CARTESIAN_POINT('',(36.9828414020409,-50.5784163146694,2.83404198860226));
#228360=CARTESIAN_POINT('',(36.7734145609104,-50.2901649976449,3.40423097483275));
#228361=CARTESIAN_POINT('',(34.9607485668371,-47.7952442955496,2.83404198860229));
#228362=CARTESIAN_POINT('',(0.154117737428429,0.111973090561912,2.83404198860262));
#228363=CARTESIAN_POINT('',(35.1701756951247,-48.0834960097832,3.40423097483277));
#228364=CARTESIAN_POINT('',(34.9607485668371,-47.7952442955496,2.83404198860229));
#228365=CARTESIAN_POINT('',(35.4234021096015,-48.4320322672525,3.6430319886023));
#228366=CARTESIAN_POINT('Origin',(35.4009304784387,-48.4011027203966,3.20400220587264));
#228367=CARTESIAN_POINT('',(35.6593272385107,-48.7567553505298,3.64303198860229));
#228368=CARTESIAN_POINT('',(35.7027398082304,-48.8165076253514,3.64303198860229));
#228369=CARTESIAN_POINT('',(35.7334106856012,-48.8587224664495,3.42473028058447));
#228370=CARTESIAN_POINT('',(35.6593272391108,-48.7567553500938,3.64303198860229));
#228371=CARTESIAN_POINT('',(35.9273564209826,-49.1256658701809,3.23423028058448));
#228372=CARTESIAN_POINT('Origin',(35.9100590388149,-49.1018589397078,3.56425743004547));
#228373=CARTESIAN_POINT('',(36.0162343214032,-49.2479958054493,3.23423028058448));
#228374=CARTESIAN_POINT('',(36.0165450899153,-49.2484235416107,3.23423028058448));
#228375=CARTESIAN_POINT('',(36.2101800152092,-49.5149391519571,3.4247302805845));
#228376=CARTESIAN_POINT('Origin',(36.0335325740078,-49.2718056808884,3.56425912917759));
#228377=CARTESIAN_POINT('',(36.2842634307661,-49.6169062257364,3.64303198860229));
#228378=CARTESIAN_POINT('',(36.2101800152092,-49.5149391519571,3.4247302805845));
#228379=CARTESIAN_POINT('',(36.5204948682736,-49.9420509053685,3.64303198860228));
#228380=CARTESIAN_POINT('Origin',(38.8445040879387,-43.4258901551464,2.65878198860232));
#228381=CARTESIAN_POINT('',(39.5091373124628,-43.856566526705,2.65878198860232));
#228382=CARTESIAN_POINT('',(42.0638038389706,-46.6938111422597,2.6587819886023));
#228383=CARTESIAN_POINT('',(38.9973987043324,-43.2882232241942,2.65878198860232));
#228384=CARTESIAN_POINT('',(42.04115278469,-46.7142062431416,2.6587819886023));
#228385=CARTESIAN_POINT('Origin',(5.54842705988295E-15,1.85104960534706E-13,
2.65878198860263));
#228386=CARTESIAN_POINT('',(39.4864862581822,-43.8769616275868,2.65878198860232));
#228387=CARTESIAN_POINT('',(39.4391766863035,-43.8244190249872,2.65878198860232));
#228388=CARTESIAN_POINT('Origin',(5.69800909227282E-15,1.85381009547451E-13,
2.65878198860263));
#228389=CARTESIAN_POINT('Origin',(-0.141569089253442,-0.127469380511453,
42.7590319886026));
#228390=CARTESIAN_POINT('',(40.0087367337519,-44.7189015017592,3.64303198860231));
#228391=CARTESIAN_POINT('',(39.7204655612079,-44.3987439298674,3.4042309748328));
#228392=CARTESIAN_POINT('Origin',(39.9831551867373,-44.6904903154961,3.20400220531642));
#228393=CARTESIAN_POINT('',(39.4820551877884,-44.1339623846885,2.83404198860231));
#228394=CARTESIAN_POINT('',(39.7204655612079,-44.3987439298674,3.4042309748328));
#228395=CARTESIAN_POINT('',(41.7839914803032,-46.690521640289,2.8340419886023));
#228396=CARTESIAN_POINT('',(41.9578224365467,-46.8835804757578,2.8340419886023));
#228397=CARTESIAN_POINT('',(41.5455814340034,-46.4257404601128,3.40423097483279));
#228398=CARTESIAN_POINT('',(41.7839914803032,-46.690521640289,2.8340419886023));
#228399=CARTESIAN_POINT('',(41.2573105570842,-46.1055832156402,3.64303198860232));
#228400=CARTESIAN_POINT('Origin',(41.2828921864925,-46.1339944934109,3.20400259788226));
#228401=CARTESIAN_POINT('',(40.9887352200427,-45.8073000862117,3.64303198860231));
#228402=CARTESIAN_POINT('',(-0.141569089253437,-0.12746938051118,3.64303198860262));
#228403=CARTESIAN_POINT('',(40.9043991801909,-45.7136354238369,3.42473028058453));
#228404=CARTESIAN_POINT('',(40.9887352205719,-45.8073000857352,3.64303198860231));
#228405=CARTESIAN_POINT('',(40.6836127633984,-45.4684272662429,3.2342302805845));
#228406=CARTESIAN_POINT('Origin',(40.7033039308027,-45.4902957559628,3.56425722717323));
#228407=CARTESIAN_POINT('',(40.5824347852705,-45.3560577375089,3.2342302805845));
#228408=CARTESIAN_POINT('',(-0.141569089253437,-0.127469380511178,3.23423028058481));
#228409=CARTESIAN_POINT('',(40.3616483211489,-45.1108495273506,3.4247302805845));
#228410=CARTESIAN_POINT('Origin',(40.5627424347182,-45.3341863992352,3.56425909741185));
#228411=CARTESIAN_POINT('',(40.2773122455534,-45.0171848263426,3.6430319886023));
#228412=CARTESIAN_POINT('',(40.3616483211489,-45.1108495273506,3.4247302805845));
#228413=CARTESIAN_POINT('',(-0.141569089253437,-0.12746938051118,3.64303198860262));
#228414=CARTESIAN_POINT('Origin',(0.141569089253442,0.127469380511275,42.7590319886026));
#228415=CARTESIAN_POINT('',(41.5404487355911,-45.8506444546175,3.64303198860231));
#228416=CARTESIAN_POINT('',(41.8287196129605,-46.1708016986847,3.40423097483278));
#228417=CARTESIAN_POINT('Origin',(41.5660303648061,-45.8790557321733,3.20400259735469));
#228418=CARTESIAN_POINT('',(42.0671296591466,-46.4355828789634,2.8340419886023));
#228419=CARTESIAN_POINT('',(41.8287196129605,-46.1708016986847,3.40423097483278));
#228420=CARTESIAN_POINT('',(39.7651933659004,-43.8790236240213,2.83404198860232));
#228421=CARTESIAN_POINT('',(0.141569089253444,0.127469380511558,2.83404198860262));
#228422=CARTESIAN_POINT('',(40.003603739189,-44.1438051693181,3.40423097483281));
#228423=CARTESIAN_POINT('',(39.7651933659004,-43.8790236240213,2.83404198860232));
#228424=CARTESIAN_POINT('',(40.2918749122587,-44.4639627407365,3.64303198860232));
#228425=CARTESIAN_POINT('Origin',(40.2662933650399,-44.4355515542465,3.20400220587391));
#228426=CARTESIAN_POINT('',(40.5604504235095,-44.7622460658158,3.64303198860232));
#228427=CARTESIAN_POINT('',(40.6098709880934,-44.817133162225,3.64303198860232));
#228428=CARTESIAN_POINT('',(40.6447864996558,-44.8559107663279,3.4247302805845));
#228429=CARTESIAN_POINT('',(40.5604504240602,-44.7622460653199,3.64303198860232));
#228430=CARTESIAN_POINT('',(40.8655729637774,-45.1011189764862,3.2342302805845));
#228431=CARTESIAN_POINT('Origin',(40.8458818366188,-45.0792505316427,3.56425743003812));
#228432=CARTESIAN_POINT('',(40.9667509419053,-45.2134885052202,3.2342302805845));
#228433=CARTESIAN_POINT('',(40.9671047185986,-45.2138814140432,3.2342302805845));
#228434=CARTESIAN_POINT('',(41.1875373586978,-45.4586966628142,3.42473028058452));
#228435=CARTESIAN_POINT('Origin',(40.9864432425628,-45.2353597879088,3.56425912917589));
#228436=CARTESIAN_POINT('',(41.2718733990788,-45.5523613247125,3.64303198860231));
#228437=CARTESIAN_POINT('',(41.1875373586978,-45.4586966628142,3.42473028058452));
#228438=CARTESIAN_POINT('',(41.5407976097559,-45.851031918631,3.64303198860231));
#228439=CARTESIAN_POINT('Origin',(43.1709513941248,-39.1276422664444,2.65878198860235));
#228440=CARTESIAN_POINT('',(43.8769616275879,-39.486486258181,2.65878198860235));
#228441=CARTESIAN_POINT('',(46.7142062431428,-42.0411527846888,2.65878198860233));
#228442=CARTESIAN_POINT('',(43.3086183250771,-38.9747476500507,2.65878198860235));
#228443=CARTESIAN_POINT('',(46.6938111422609,-42.0638038389693,2.65878198860233));
#228444=CARTESIAN_POINT('Origin',(5.5375465370123E-15,1.85094080011836E-13,
2.65878198860263));
#228445=CARTESIAN_POINT('',(43.8565665267061,-39.5091373124615,2.65878198860235));
#228446=CARTESIAN_POINT('',(43.8040239241064,-39.4618277405829,2.65878198860235));
#228447=CARTESIAN_POINT('Origin',(5.70367421417806E-15,1.85386674669356E-13,
2.65878198860263));
#228448=CARTESIAN_POINT('Origin',(-0.127469380511361,-0.141569089253534,
42.7590319886026));
#228449=CARTESIAN_POINT('',(44.4639627407376,-40.2918749122575,3.64303198860234));
#228450=CARTESIAN_POINT('',(44.1438051688458,-40.0036037397136,3.40423097483283));
#228451=CARTESIAN_POINT('Origin',(44.4355515544733,-40.2662933652418,3.2040022053198));
#228452=CARTESIAN_POINT('',(43.8790236243779,-39.7651933655044,2.83404198860234));
#228453=CARTESIAN_POINT('',(44.1438051688458,-40.0036037397136,3.40423097483283));
#228454=CARTESIAN_POINT('',(46.4355828792675,-42.0671296588088,2.83404198860233));
#228455=CARTESIAN_POINT('',(46.6286417147362,-42.2409606150523,2.83404198860233));
#228456=CARTESIAN_POINT('',(46.1708016982804,-41.8287196134095,3.4042309748328));
#228457=CARTESIAN_POINT('',(46.4355828792675,-42.0671296588088,2.83404198860233));
#228458=CARTESIAN_POINT('',(45.8506444546187,-41.5404487355899,3.64303198860235));
#228459=CARTESIAN_POINT('Origin',(45.8790557323885,-41.5660303649975,3.20400259788037));
#228460=CARTESIAN_POINT('',(45.5523613242375,-41.2718733996063,3.64303198860234));
#228461=CARTESIAN_POINT('',(-0.127469380511355,-0.141569089253261,3.64303198860262));
#228462=CARTESIAN_POINT('',(45.4586966628153,-41.1875373586965,3.42473028058456));
#228463=CARTESIAN_POINT('',(45.5523613247136,-41.2718733990775,3.64303198860234));
#228464=CARTESIAN_POINT('',(45.2134885052213,-40.9667509419041,3.23423028058453));
#228465=CARTESIAN_POINT('Origin',(45.2353576819761,-40.9864413462819,3.56425722717016));
#228466=CARTESIAN_POINT('',(45.1011189764874,-40.8655729637762,3.23423028058453));
#228467=CARTESIAN_POINT('',(-0.127469380511355,-0.141569089253258,3.23423028058481));
#228468=CARTESIAN_POINT('',(44.855910766329,-40.6447864996546,3.42473028058453));
#228469=CARTESIAN_POINT('Origin',(45.0792483253103,-40.8458798501214,3.5642590974069));
#228470=CARTESIAN_POINT('',(44.762246065321,-40.560450424059,3.64303198860234));
#228471=CARTESIAN_POINT('',(44.855910766329,-40.6447864996546,3.42473028058453));
#228472=CARTESIAN_POINT('',(-0.127469380511355,-0.141569089253261,3.64303198860262));
#228473=CARTESIAN_POINT('Origin',(0.127469380511361,0.141569089253356,42.7590319886026));
#228474=CARTESIAN_POINT('',(46.1055832156414,-41.257310557083,3.64303198860234));
#228475=CARTESIAN_POINT('',(46.4257404597086,-41.5455814344523,3.40423097483282));
#228476=CARTESIAN_POINT('Origin',(46.1339944931989,-41.2828921862993,3.20400259735935));
#228477=CARTESIAN_POINT('',(46.6905216405931,-41.7839914799656,2.83404198860233));
#228478=CARTESIAN_POINT('',(46.4257404597086,-41.5455814344523,3.40423097483282));
#228479=CARTESIAN_POINT('',(44.1339623850452,-39.4820551873923,2.83404198860234));
#228480=CARTESIAN_POINT('',(0.127469380511362,0.141569089253638,2.83404198860262));
#228481=CARTESIAN_POINT('',(44.3987439293953,-39.7204655617323,3.40423097483283));
#228482=CARTESIAN_POINT('',(44.1339623850452,-39.4820551873923,2.83404198860235));
#228483=CARTESIAN_POINT('',(44.7189015017603,-40.0087367337506,3.64303198860235));
#228484=CARTESIAN_POINT('Origin',(44.6904903152704,-39.9831551865318,3.20400220587396));
#228485=CARTESIAN_POINT('',(45.0171848258476,-40.2773122461031,3.64303198860235));
#228486=CARTESIAN_POINT('',(45.0720719232488,-40.3267328095852,3.64303198860235));
#228487=CARTESIAN_POINT('',(45.1108495273517,-40.3616483211477,3.42473028058454));
#228488=CARTESIAN_POINT('',(45.0171848263437,-40.2773122455521,3.64303198860235));
#228489=CARTESIAN_POINT('',(45.3560577375101,-40.5824347852693,3.23423028058454));
#228490=CARTESIAN_POINT('Origin',(45.3341886054736,-40.5627444213173,3.56425743003981));
#228491=CARTESIAN_POINT('',(45.4684272662441,-40.6836127633972,3.23423028058454));
#228492=CARTESIAN_POINT('',(45.468820175067,-40.6839665400904,3.23423028058454));
#228493=CARTESIAN_POINT('',(45.7136354238381,-40.9043991801896,3.42473028058456));
#228494=CARTESIAN_POINT('Origin',(45.4902978619872,-40.7033058269848,3.56425912917625));
#228495=CARTESIAN_POINT('',(45.8073000857364,-40.9887352205706,3.64303198860234));
#228496=CARTESIAN_POINT('',(45.7136354238381,-40.9043991801896,3.42473028058456));
#228497=CARTESIAN_POINT('',(46.1059706796549,-41.2576594312477,3.64303198860234));
#228498=CARTESIAN_POINT('Origin',(47.0244087227346,-34.4007037410856,2.65878198860239));
#228499=CARTESIAN_POINT('',(47.7640607692767,-34.6837837831338,2.65878198860238));
#228500=CARTESIAN_POINT('',(50.8527980281389,-36.9278827595319,2.65878198860237));
#228501=CARTESIAN_POINT('',(47.1453396605412,-34.2342565846629,2.65878198860239));
#228502=CARTESIAN_POINT('',(50.8348823336491,-36.9525415975204,2.65878198860237));
#228503=CARTESIAN_POINT('Origin',(5.52786294311959E-15,1.85082121769273E-13,
2.65878198860263));
#228504=CARTESIAN_POINT('',(47.7461450747869,-34.7084426211224,2.65878198860238));
#228505=CARTESIAN_POINT('',(47.6889451092156,-34.6668844135344,2.65878198860238));
#228506=CARTESIAN_POINT('Origin',(5.70871613546578E-15,1.85392900923618E-13,
2.65878198860263));
#228507=CARTESIAN_POINT('Origin',(-0.111973090561714,-0.154117737428518,
42.7590319886026));
#228508=CARTESIAN_POINT('',(48.4320322672535,-35.4234021096002,3.64303198860239));
#228509=CARTESIAN_POINT('',(48.0834960093688,-35.1701756956951,3.40423097483286));
#228510=CARTESIAN_POINT('Origin',(48.4011027206439,-35.4009304786163,3.20400220531683));
#228511=CARTESIAN_POINT('',(47.7952442958629,-34.960748566406,2.83404198860238));
#228512=CARTESIAN_POINT('',(48.0834960093688,-35.1701756956951,3.40423097483286));
#228513=CARTESIAN_POINT('',(50.5784163149361,-36.9828414016739,2.83404198860236));
#228514=CARTESIAN_POINT('',(50.7885878366285,-37.135539950359,2.83404198860236));
#228515=CARTESIAN_POINT('',(50.2901649972897,-36.7734145613994,3.40423097483285));
#228516=CARTESIAN_POINT('',(50.5784163149361,-36.9828414016739,2.83404198860236));
#228517=CARTESIAN_POINT('',(49.9416290966442,-36.5201884062945,3.64303198860239));
#228518=CARTESIAN_POINT('Origin',(49.9725587428726,-36.5426601096557,3.20400259788266));
#228519=CARTESIAN_POINT('',(49.6169062253194,-36.2842634313401,3.64303198860238));
#228520=CARTESIAN_POINT('',(-0.111973090561709,-0.154117737428245,3.64303198860263));
#228521=CARTESIAN_POINT('',(49.5149391519582,-36.2101800152079,3.42473028058461));
#228522=CARTESIAN_POINT('',(49.6169062257374,-36.2842634307648,3.64303198860238));
#228523=CARTESIAN_POINT('',(49.2479958054503,-36.0162343214019,3.23423028058457));
#228524=CARTESIAN_POINT('Origin',(49.2718033882774,-36.0335309082452,3.56425722717045));
#228525=CARTESIAN_POINT('',(49.1256658701819,-35.9273564209813,3.23423028058457));
#228526=CARTESIAN_POINT('',(-0.111973090561709,-0.154117737428242,3.23423028058481));
#228527=CARTESIAN_POINT('',(48.8587224664505,-35.7334106855999,3.42473028058457));
#228528=CARTESIAN_POINT('Origin',(49.1018565378152,-35.9100572938234,3.56425909741191));
#228529=CARTESIAN_POINT('',(48.7567553500948,-35.6593272391094,3.64303198860238));
#228530=CARTESIAN_POINT('',(48.8587224664505,-35.7334106855999,3.42473028058457));
#228531=CARTESIAN_POINT('',(-0.111973090561709,-0.154117737428245,3.64303198860263));
#228532=CARTESIAN_POINT('Origin',(0.111973090561714,0.15411773742834,42.7590319886026));
#228533=CARTESIAN_POINT('',(50.1655752777676,-36.2119529314377,3.64303198860238));
#228534=CARTESIAN_POINT('',(50.5141111787694,-36.4651790860522,3.40423097483286));
#228535=CARTESIAN_POINT('Origin',(50.1965049237626,-36.2344246346292,3.20400259735642));
#228536=CARTESIAN_POINT('',(50.8023624963256,-36.6746059264507,2.83404198860237));
#228537=CARTESIAN_POINT('',(50.5141111787694,-36.4651790860522,3.40423097483285));
#228538=CARTESIAN_POINT('',(48.0191904766741,-34.6525130919789,2.83404198860238));
#228539=CARTESIAN_POINT('',(0.111973090561715,0.154117737428622,2.83404198860262));
#228540=CARTESIAN_POINT('',(48.3074421900767,-34.8619402214102,3.40423097483287));
#228541=CARTESIAN_POINT('',(48.0191904766741,-34.6525130919789,2.83404198860238));
#228542=CARTESIAN_POINT('',(48.6559784483769,-35.1151666347433,3.64303198860239));
#228543=CARTESIAN_POINT('Origin',(48.6250489015204,-35.0926950035802,3.20400220587407));
#228544=CARTESIAN_POINT('',(48.9807015307823,-35.3510917648527,3.64303198860238));
#228545=CARTESIAN_POINT('',(49.0404538064758,-35.3945043333723,3.64303198860239));
#228546=CARTESIAN_POINT('',(49.0826686475739,-35.425175210743,3.42473028058457));
#228547=CARTESIAN_POINT('',(48.9807015312183,-35.3510917642526,3.64303198860239));
#228548=CARTESIAN_POINT('',(49.3496120513054,-35.6191209461244,3.23423028058457));
#228549=CARTESIAN_POINT('Origin',(49.325804517179,-35.6018243948125,3.56425743004393));
#228550=CARTESIAN_POINT('',(49.4719419865737,-35.707998846545,3.23423028058457));
#228551=CARTESIAN_POINT('',(49.4723697227352,-35.7083096150571,3.23423028058457));
#228552=CARTESIAN_POINT('',(49.7388853330816,-35.9019445403511,3.42473028058459));
#228553=CARTESIAN_POINT('Origin',(49.4957512585772,-35.7252979297049,3.56425912917973));
#228554=CARTESIAN_POINT('',(49.8408524068608,-35.9760279559079,3.64303198860239));
#228555=CARTESIAN_POINT('',(49.7388853330816,-35.9019445403511,3.42473028058459));
#228556=CARTESIAN_POINT('',(50.165997086493,-36.2122593934154,3.64303198860238));
#228557=CARTESIAN_POINT('Origin',(50.3626567888879,-29.2968639067293,2.65878198860242));
#228558=CARTESIAN_POINT('',(51.1278468659051,-29.5010785149103,2.65878198860242));
#228559=CARTESIAN_POINT('',(54.4342359163067,-31.4100231232053,2.65878198860241));
#228560=CARTESIAN_POINT('',(50.4655267888879,-29.1186878401547,2.65878198860242));
#228561=CARTESIAN_POINT('',(54.4189959163067,-31.4364195775126,2.65878198860241));
#228562=CARTESIAN_POINT('Origin',(5.51948237368594E-15,1.85069216824025E-13,
2.65878198860263));
#228563=CARTESIAN_POINT('',(51.1126068659051,-29.5274749692176,2.65878198860242));
#228564=CARTESIAN_POINT('',(51.0513762321548,-29.4921234463392,2.65878198860242));
#228565=CARTESIAN_POINT('Origin',(5.71307961579125E-15,1.85399620094091E-13,
2.65878198860263));
#228566=CARTESIAN_POINT('Origin',(-0.0952499999999979,-0.164977839421026,
42.7590319886026));
#228567=CARTESIAN_POINT('',(51.869470313195,-30.1668231006066,3.64303198860242));
#228568=CARTESIAN_POINT('',(51.4963740054947,-29.9514158469222,3.4042309748329));
#228569=CARTESIAN_POINT('Origin',(51.8363612768233,-30.1477075895448,3.20400220531909));
#228570=CARTESIAN_POINT('',(51.187810269045,-29.7732664900063,2.83404198860242));
#228571=CARTESIAN_POINT('',(51.4963740054947,-29.9514158469222,3.4042309748329));
#228572=CARTESIAN_POINT('',(54.1671020372442,-31.493361394985,2.8340419886024));
#228573=CARTESIAN_POINT('',(54.3920835619875,-31.6232545388582,2.8340419886024));
#228574=CARTESIAN_POINT('',(53.8585387246959,-31.3152122841216,3.40423097483289));
#228575=CARTESIAN_POINT('',(54.1671020372442,-31.493361394985,2.8340419886024));
#228576=CARTESIAN_POINT('',(53.4854427993291,-31.0998052504791,3.64303198860242));
#228577=CARTESIAN_POINT('Origin',(53.5185519423371,-31.1189208231074,3.20400259787966));
#228578=CARTESIAN_POINT('',(53.1378379187913,-30.8991154799502,3.64303198860242));
#228579=CARTESIAN_POINT('',(-0.0952499999999924,-0.164977839420753,3.64303198860263));
#228580=CARTESIAN_POINT('',(53.028685606085,-30.8360963620053,3.42473028058464));
#228581=CARTESIAN_POINT('',(53.1378379191468,-30.8991154793343,3.64303198860242));
#228582=CARTESIAN_POINT('',(52.7429317578291,-30.6711163007929,3.23423028058461));
#228583=CARTESIAN_POINT('Origin',(52.7684169058679,-30.685829565076,3.5642572271725));
#228584=CARTESIAN_POINT('',(52.6119816883963,-30.5955122429554,3.23423028058461));
#228585=CARTESIAN_POINT('',(-0.0952499999999923,-0.16497783942075,3.23423028058481));
#228586=CARTESIAN_POINT('',(52.3262277788845,-30.4305321463768,3.42473028058461));
#228587=CARTESIAN_POINT('Origin',(52.5864945348665,-30.5807966351502,3.56425909741314));
#228588=CARTESIAN_POINT('',(52.217075420246,-30.3675130027342,3.64303198860242));
#228589=CARTESIAN_POINT('',(52.3262277788845,-30.4305321463768,3.42473028058461));
#228590=CARTESIAN_POINT('',(-0.0952499999999924,-0.164977839420753,3.64303198860263));
#228591=CARTESIAN_POINT('Origin',(0.0952499999999979,0.164977839420847,
42.7590319886026));
#228592=CARTESIAN_POINT('',(53.675942799329,-30.7698495716372,3.64303198860242));
#228593=CARTESIAN_POINT('',(54.0490387249983,-30.9852566047559,3.40423097483289));
#228594=CARTESIAN_POINT('Origin',(53.7090519420895,-30.7889651441226,3.20400259735806));
#228595=CARTESIAN_POINT('',(54.3576020374704,-31.1634057157514,2.8340419886024));
#228596=CARTESIAN_POINT('',(54.0490387249983,-30.9852566047559,3.40423097483289));
#228597=CARTESIAN_POINT('',(51.3783102687789,-29.4433108116253,2.83404198860242));
#228598=CARTESIAN_POINT('',(0.0952499999999987,0.164977839421129,2.83404198860262));
#228599=CARTESIAN_POINT('',(51.6868740051417,-29.6214601686917,3.40423097483291));
#228600=CARTESIAN_POINT('',(51.3783102687789,-29.4433108116253,2.83404198860242));
#228601=CARTESIAN_POINT('',(52.059970313195,-29.8368674217647,3.64303198860242));
#228602=CARTESIAN_POINT('Origin',(52.0268612765608,-29.8177519105514,3.20400220587201));
#228603=CARTESIAN_POINT('',(52.4075754198753,-30.0375573245345,3.64303198860242));
#228604=CARTESIAN_POINT('',(52.4715382154243,-30.0744862609066,3.64303198860242));
#228605=CARTESIAN_POINT('',(52.5167277788845,-30.1005764675349,3.42473028058461));
#228606=CARTESIAN_POINT('',(52.407575420246,-30.0375573238923,3.64303198860242));
#228607=CARTESIAN_POINT('',(52.8024816883963,-30.2655565641136,3.23423028058461));
#228608=CARTESIAN_POINT('Origin',(52.7769965925028,-30.2508433300749,3.56425743003977));
#228609=CARTESIAN_POINT('',(52.9334317578291,-30.341160621951,3.23423028058461));
#228610=CARTESIAN_POINT('',(52.9338896349621,-30.341424977437,3.23423028058461));
#228611=CARTESIAN_POINT('',(53.219185606085,-30.5061406831635,3.42473028058463));
#228612=CARTESIAN_POINT('Origin',(52.9589188467291,-30.3558761923098,3.56425912917761));
#228613=CARTESIAN_POINT('',(53.3283379191468,-30.5691598004924,3.64303198860242));
#228614=CARTESIAN_POINT('',(53.219185606085,-30.5061406831635,3.42473028058463));
#228615=CARTESIAN_POINT('',(53.6763943313417,-30.7701102637663,3.64303198860242));
#228616=CARTESIAN_POINT('Origin',(53.1491210481986,-23.8720415006481,2.65878198860246));
#228617=CARTESIAN_POINT('',(53.9314655730807,-23.9951532569799,2.65878198860246));
#228618=CARTESIAN_POINT('',(57.4192809246792,-25.548028700571,2.65878198860245));
#228619=CARTESIAN_POINT('',(53.2328030451451,-23.6840886581928,2.65878198860246));
#228620=CARTESIAN_POINT('',(57.4068835917983,-25.5758735661199,2.65878198860245));
#228621=CARTESIAN_POINT('Origin',(5.51249664798382E-15,1.85055506565373E-13,
2.65878198860263));
#228622=CARTESIAN_POINT('',(53.9190682401998,-24.0229981225288,2.65878198860246));
#228623=CARTESIAN_POINT('',(53.8544777939072,-23.9942406030425,2.65878198860246));
#228624=CARTESIAN_POINT('Origin',(5.71671684795091E-15,1.85406758564139E-13,
2.65878198860263));
#228625=CARTESIAN_POINT('Origin',(-0.0774833305059378,-0.174030409681006,
42.7590319886026));
#228626=CARTESIAN_POINT('',(54.7386155880007,-24.5797300649093,3.64303198860246));
#228627=CARTESIAN_POINT('',(54.3450469517073,-24.4045020183937,3.40423097483294));
#228628=CARTESIAN_POINT('Origin',(54.7036898113994,-24.5641801073097,3.20400220531724));
#228629=CARTESIAN_POINT('',(54.0195518811808,-24.2595822754864,2.83404198860245));
#228630=CARTESIAN_POINT('',(54.3450469517073,-24.4045020183937,3.40423097483294));
#228631=CARTESIAN_POINT('',(57.1623216544374,-25.6588335304432,2.83404198860244));
#228632=CARTESIAN_POINT('',(57.399648237566,-25.7644981330383,2.83404198860244));
#228633=CARTESIAN_POINT('',(56.8368270312097,-25.5139139879307,3.40423097483294));
#228634=CARTESIAN_POINT('',(57.1623216544374,-25.6588335304432,2.83404198860244));
#228635=CARTESIAN_POINT('',(56.443258798156,-25.3386861202868,3.64303198860246));
#228636=CARTESIAN_POINT('Origin',(56.478184687247,-25.3542361279701,3.20400259788249));
#228637=CARTESIAN_POINT('',(56.0765803402173,-25.1754303533064,3.64303198860245));
#228638=CARTESIAN_POINT('',(-0.0774833305059323,-0.174030409680733,3.64303198860263));
#228639=CARTESIAN_POINT('',(55.9614386837456,-25.1241659841927,3.42473028058468));
#228640=CARTESIAN_POINT('',(56.0765803405066,-25.1754303526566,3.64303198860245));
#228641=CARTESIAN_POINT('',(55.6600051127011,-24.9899591116487,3.23423028058465));
#228642=CARTESIAN_POINT('Origin',(55.6868886053365,-25.0019278517695,3.56425722717436));
#228643=CARTESIAN_POINT('',(55.5218696254676,-24.9284572302733,3.23423028058465));
#228644=CARTESIAN_POINT('',(-0.0774833305059322,-0.17403040968073,3.23423028058481));
#228645=CARTESIAN_POINT('',(55.2204359898059,-24.7942503289599,3.42473028058464));
#228646=CARTESIAN_POINT('Origin',(55.4949838933612,-24.9164863690988,3.56425909741192));
#228647=CARTESIAN_POINT('',(55.1052942849675,-24.7429859390905,3.64303198860246));
#228648=CARTESIAN_POINT('',(55.2204359898059,-24.7942503289599,3.42473028058464));
#228649=CARTESIAN_POINT('',(-0.0774833305059323,-0.174030409680733,3.64303198860263));
#228650=CARTESIAN_POINT('Origin',(0.0774833305059378,0.174030409680827,
42.7590319886026));
#228651=CARTESIAN_POINT('',(56.5982254591679,-24.990625300925,3.64303198860246));
#228652=CARTESIAN_POINT('',(56.9917936924676,-25.1658531680162,3.40423097483293));
#228653=CARTESIAN_POINT('Origin',(56.6331513479955,-25.0061753084909,3.20400259735638));
#228654=CARTESIAN_POINT('',(57.3172883156333,-25.3107727106681,2.83404198860245));
#228655=CARTESIAN_POINT('',(56.9917936924676,-25.1658531680162,3.40423097483293));
#228656=CARTESIAN_POINT('',(54.1745185419763,-23.9115214566106,2.83404198860245));
#228657=CARTESIAN_POINT('',(0.0774833305059383,0.174030409681108,2.83404198860262));
#228658=CARTESIAN_POINT('',(54.5000136124319,-24.0564411996771,3.40423097483294));
#228659=CARTESIAN_POINT('',(54.1745185419763,-23.9115214566106,2.83404198860246));
#228660=CARTESIAN_POINT('',(54.8935822490125,-24.2316692455474,3.64303198860246));
#228661=CARTESIAN_POINT('Origin',(54.8586564721336,-24.2161192878243,3.20400220587174));
#228662=CARTESIAN_POINT('',(55.2602609456776,-24.3949251204063,3.64303198860247));
#228663=CARTESIAN_POINT('',(55.3277334713093,-24.4249658234757,3.64303198860246));
#228664=CARTESIAN_POINT('',(55.3754026508178,-24.446189509598,3.42473028058465));
#228665=CARTESIAN_POINT('',(55.2602609459794,-24.3949251197286,3.64303198860247));
#228666=CARTESIAN_POINT('',(55.6768362864795,-24.5803964109114,3.23423028058465));
#228667=CARTESIAN_POINT('Origin',(55.6499528488669,-24.5684276954195,3.56425743004579));
#228668=CARTESIAN_POINT('',(55.814971773713,-24.6418982922869,3.23423028058465));
#228669=CARTESIAN_POINT('',(55.8154547752198,-24.6421133384127,3.23423028058465));
#228670=CARTESIAN_POINT('',(56.1164053447575,-24.7761051648309,3.42473028058467));
#228671=CARTESIAN_POINT('Origin',(55.8418574376288,-24.6538691229756,3.56425912917798));
#228672=CARTESIAN_POINT('',(56.2315470015185,-24.8273695332948,3.64303198860246));
#228673=CARTESIAN_POINT('',(56.1164053447575,-24.7761051648309,3.42473028058467));
#228674=CARTESIAN_POINT('',(56.5987017673886,-24.9908373670079,3.64303198860246));
#228675=CARTESIAN_POINT('Origin',(55.3532724151367,-18.1856720123399,2.6587819886025));
#228676=CARTESIAN_POINT('',(56.144199857553,-18.2263320786573,2.6587819886025));
#228677=CARTESIAN_POINT('',(59.7752282754839,-19.4061247292244,2.65878198860249));
#228678=CARTESIAN_POINT('',(55.4168495715594,-17.9900016446774,2.6587819886025));
#228679=CARTESIAN_POINT('',(59.7658094374954,-19.4351129318411,2.65878198860249));
#228680=CARTESIAN_POINT('Origin',(5.50698230308587E-15,1.85041141205781E-13,
2.65878198860263));
#228681=CARTESIAN_POINT('',(56.1347810195644,-18.255320281274,2.6587819886025));
#228682=CARTESIAN_POINT('',(56.0675384271755,-18.2334718385811,2.6587819886025));
#228683=CARTESIAN_POINT('Origin',(5.71958798166808E-15,1.85414238123189E-13,
2.65878198860263));
#228684=CARTESIAN_POINT('Origin',(-0.0588677374284251,-0.181176266354317,
42.7590319886026));
#228685=CARTESIAN_POINT('',(57.0080331356325,-18.7233363629815,3.6430319886025));
#228686=CARTESIAN_POINT('',(56.5983041910848,-18.5902073587813,3.40423097483299));
#228687=CARTESIAN_POINT('Origin',(56.9716732729175,-18.7115223274331,3.20400220531805));
#228688=CARTESIAN_POINT('',(56.2594439785883,-18.4801050009127,2.8340419886025));
#228689=CARTESIAN_POINT('',(56.5983041910848,-18.5902073587813,3.40423097483299));
#228690=CARTESIAN_POINT('',(59.5312589135998,-19.5431821162857,2.83404198860249));
#228691=CARTESIAN_POINT('',(59.7783303554051,-19.6234604941049,2.83404198860249));
#228692=CARTESIAN_POINT('',(59.1923991668989,-19.4330799109579,3.40423097483297));
#228693=CARTESIAN_POINT('',(59.5312589135998,-19.5431821162857,2.83404198860249));
#228694=CARTESIAN_POINT('',(58.7826706420791,-19.2999510424997,3.6430319886025));
#228695=CARTESIAN_POINT('Origin',(58.8190306219008,-19.3117651160984,3.20400259787949));
#228696=CARTESIAN_POINT('',(58.400936012657,-19.1759179434147,3.6430319886025));
#228697=CARTESIAN_POINT('',(-0.0588677374284196,-0.181176266354044,3.64303198860263));
#228698=CARTESIAN_POINT('',(58.2810665285032,-19.1369699862874,3.42473028058473));
#228699=CARTESIAN_POINT('',(58.4009360128769,-19.1759179427377,3.6430319886025));
#228700=CARTESIAN_POINT('',(57.9672558039534,-19.0350067009921,3.23423028058469));
#228701=CARTESIAN_POINT('Origin',(57.9952431000169,-19.0440997849303,3.56425722717133));
#228702=CARTESIAN_POINT('',(57.8234483402241,-18.9882808235611,3.23423028058469));
#228703=CARTESIAN_POINT('',(-0.0588677374284196,-0.181176266354041,3.23423028058481));
#228704=CARTESIAN_POINT('',(57.5096375484039,-18.8863175164083,3.42473028058468));
#228705=CARTESIAN_POINT('Origin',(57.795458595248,-18.9791858642773,3.56425909741065));
#228706=CARTESIAN_POINT('',(57.3897680139787,-18.8473695436953,3.6430319886025));
#228707=CARTESIAN_POINT('',(57.5096375484039,-18.8863175164083,3.42473028058468));
#228708=CARTESIAN_POINT('',(-0.0588677374284196,-0.181176266354044,3.64303198860263));
#228709=CARTESIAN_POINT('Origin',(0.0588677374284251,0.181176266354138,
42.7590319886026));
#228710=CARTESIAN_POINT('',(58.9004061169359,-18.9375985097912,3.6430319886025));
#228711=CARTESIAN_POINT('',(59.3101346419426,-19.0707273776743,3.40423097483297));
#228712=CARTESIAN_POINT('Origin',(58.9367660964857,-18.9494125833016,3.20400259735816));
#228713=CARTESIAN_POINT('',(59.6489943885965,-19.1808295831467,2.83404198860249));
#228714=CARTESIAN_POINT('',(59.3101346419426,-19.0707273776743,3.40423097483297));
#228715=CARTESIAN_POINT('',(56.377179453281,-18.1177524687097,2.8340419886025));
#228716=CARTESIAN_POINT('',(0.0588677374284254,0.181176266354419,2.83404198860262));
#228717=CARTESIAN_POINT('',(56.7160396657232,-18.2278548267452,3.40423097483298));
#228718=CARTESIAN_POINT('',(56.377179453281,-18.1177524687097,2.83404198860249));
#228719=CARTESIAN_POINT('',(57.1257686104893,-18.3609838302731,3.6430319886025));
#228720=CARTESIAN_POINT('Origin',(57.0894087474848,-18.3491697946306,3.20400220587425));
#228721=CARTESIAN_POINT('',(57.5075034886063,-18.4850170116922,3.6430319886025));
#228722=CARTESIAN_POINT('',(57.5777465012101,-18.5078403492301,3.6430319886025));
#228723=CARTESIAN_POINT('',(57.6273730232608,-18.5239649836999,3.42473028058467));
#228724=CARTESIAN_POINT('',(57.5075034888355,-18.4850170109868,3.6430319886025));
#228725=CARTESIAN_POINT('',(57.941183815081,-18.6259282908527,3.23423028058469));
#228726=CARTESIAN_POINT('Origin',(57.9131965763133,-18.616835225657,3.56425743004289));
#228727=CARTESIAN_POINT('',(58.0849912788103,-18.6726541682836,3.23423028058469));
#228728=CARTESIAN_POINT('',(58.0854941128254,-18.6728175489591,3.23423028058469));
#228729=CARTESIAN_POINT('',(58.3988020033601,-18.774617453579,3.42473028058471));
#228730=CARTESIAN_POINT('Origin',(58.1129809527839,-18.6817491043768,3.5642591291744));
#228731=CARTESIAN_POINT('',(58.5186714877338,-18.8135654100293,3.64303198860251));
#228732=CARTESIAN_POINT('',(58.3988020033601,-18.774617453579,3.42473028058471));
#228733=CARTESIAN_POINT('',(58.9009019828321,-18.9377596263876,3.6430319886025));
#228734=CARTESIAN_POINT('Origin',(56.9509617460776,-12.3000564958681,2.65878198860254));
#228735=CARTESIAN_POINT('',(57.7418065394567,-12.2578193919758,2.65878198860254));
#228736=CARTESIAN_POINT('',(61.4762657165317,-13.0516031943519,2.65878198860254));
#228737=CARTESIAN_POINT('',(56.9937374973465,-12.0988124084931,2.65878198860254));
#228738=CARTESIAN_POINT('',(61.4699285681956,-13.0814171332223,2.65878198860254));
#228739=CARTESIAN_POINT('Origin',(5.50299975530876E-15,1.85026278135133E-13,
2.65878198860263));
#228740=CARTESIAN_POINT('',(57.7354693911206,-12.2876333308462,2.65878198860254));
#228741=CARTESIAN_POINT('',(57.666311376549,-12.2729333410569,2.65878198860254));
#228742=CARTESIAN_POINT('Origin',(5.72166156020094E-15,1.85421976823627E-13,
2.65878198860263));
#228743=CARTESIAN_POINT('Origin',(-0.0396071771007808,-0.18633711793988,
42.7590319886026));
#228744=CARTESIAN_POINT('',(58.6528587425324,-12.661805869751,3.64303198860255));
#228745=CARTESIAN_POINT('',(58.2314585657882,-12.5722344970951,3.40423097483302));
#228746=CARTESIAN_POINT('Origin',(58.6154631599697,-12.6538571932998,3.20400220531626));
#228747=CARTESIAN_POINT('',(57.8829458347212,-12.4981558287377,2.83404198860254));
#228748=CARTESIAN_POINT('',(58.2314585657882,-12.5722344970951,3.40423097483302));
#228749=CARTESIAN_POINT('',(61.2479592423879,-13.2134115091884,2.83404198860253));
#228750=CARTESIAN_POINT('',(61.5020685764506,-13.267424115525,2.83404198860253));
#228751=CARTESIAN_POINT('',(60.8994469905095,-13.1393329438485,3.40423097483302));
#228752=CARTESIAN_POINT('',(61.2479592423879,-13.2134115091884,2.83404198860253));
#228753=CARTESIAN_POINT('',(60.4780472453829,-13.0497616623165,3.64303198860255));
#228754=CARTESIAN_POINT('Origin',(60.51544294839,-13.057710364369,3.20400259788175));
#228755=CARTESIAN_POINT('',(60.0854388089606,-12.9663101637158,3.64303198860254));
#228756=CARTESIAN_POINT('',(-0.0396071771007753,-0.186337117939607,3.64303198860262));
#228757=CARTESIAN_POINT('',(59.9621548122773,-12.940105340544,3.42473028058477));
#228758=CARTESIAN_POINT('',(60.0854388091086,-12.9663101630194,3.64303198860254));
#228759=CARTESIAN_POINT('',(59.6394051101895,-12.8715027735882,3.23423028058473));
#228760=CARTESIAN_POINT('Origin',(59.6681895750078,-12.8776205756128,3.56425722717025));
#228761=CARTESIAN_POINT('',(59.4915012546306,-12.8400648385929,3.23423028058473));
#228762=CARTESIAN_POINT('',(-0.0396071771007752,-0.186337117939604,3.23423028058481));
#228763=CARTESIAN_POINT('',(59.1687514833562,-12.771462256931,3.42473028058473));
#228764=CARTESIAN_POINT('Origin',(59.462714158291,-12.8339454274777,3.56425909741496));
#228765=CARTESIAN_POINT('',(59.0454674350476,-12.7452574235138,3.64303198860254));
#228766=CARTESIAN_POINT('',(59.1687514833562,-12.771462256931,3.42473028058473));
#228767=CARTESIAN_POINT('',(-0.0396071771007753,-0.186337117939607,3.64303198860262));
#228768=CARTESIAN_POINT('Origin',(0.0396071771007808,0.186337117939701,
42.7590319886026));
#228769=CARTESIAN_POINT('',(60.5572615995845,-12.677087426437,3.64303198860255));
#228770=CARTESIAN_POINT('',(60.9786613448369,-12.7666587073764,3.40423097483302));
#228771=CARTESIAN_POINT('Origin',(60.594657302311,-12.6850361284297,3.20400259735834));
#228772=CARTESIAN_POINT('',(61.3271735966835,-12.8407372728664,2.83404198860253));
#228773=CARTESIAN_POINT('',(60.9786613448369,-12.7666587073764,3.40423097483302));
#228774=CARTESIAN_POINT('',(57.9621601888122,-12.1254815933782,2.83404198860254));
#228775=CARTESIAN_POINT('',(0.0396071771007809,0.186337117939981,2.83404198860263));
#228776=CARTESIAN_POINT('',(58.3106729198429,-12.1995602619066,3.40423097483303));
#228777=CARTESIAN_POINT('',(57.9621601888122,-12.1254815933782,2.83404198860254));
#228778=CARTESIAN_POINT('',(58.7320730967339,-12.2891316338714,3.64303198860255));
#228779=CARTESIAN_POINT('Origin',(58.6946775138721,-12.2811829573567,3.20400220587502));
#228780=CARTESIAN_POINT('',(59.1246817890951,-12.3725831883593,3.64303198860254));
#228781=CARTESIAN_POINT('',(59.1969256915255,-12.3879391031037,3.64303198860255));
#228782=CARTESIAN_POINT('',(59.2479658375578,-12.3987880210515,3.42473028058472));
#228783=CARTESIAN_POINT('',(59.1246817892492,-12.3725831876342,3.64303198860255));
#228784=CARTESIAN_POINT('',(59.5707156088322,-12.4673906027133,3.23423028058473));
#228785=CARTESIAN_POINT('Origin',(59.541931202957,-12.46127281334,3.5642574300457));
#228786=CARTESIAN_POINT('',(59.7186194643911,-12.4988285377087,3.23423028058473));
#228787=CARTESIAN_POINT('',(59.7191366217598,-12.4989384629008,3.23423028058473));
#228788=CARTESIAN_POINT('',(60.0413691664789,-12.5674311046645,3.42473028058476));
#228789=CARTESIAN_POINT('Origin',(59.7474064876929,-12.504947933182,3.56425912917895));
#228790=CARTESIAN_POINT('',(60.1646531633102,-12.5936359271399,3.64303198860255));
#228791=CARTESIAN_POINT('',(60.0413691664789,-12.5674311046645,3.42473028058476));
#228792=CARTESIAN_POINT('',(60.5577715903456,-12.6771958283196,3.64303198860255));
#228793=CARTESIAN_POINT('Origin',(57.9246844223736,-6.27967898647509,2.65878198860258));
#228794=CARTESIAN_POINT('',(58.7067819056644,-6.15500747092217,2.65878198860258));
#228795=CARTESIAN_POINT('',(62.5037563256536,-6.55408556365842,2.65878198860258));
#228796=CARTESIAN_POINT('',(57.9461901084063,-6.07506605172202,2.65878198860258));
#228797=CARTESIAN_POINT('',(62.5005702980932,-6.58439859102925,2.65878198860258));
#228798=CARTESIAN_POINT('Origin',(5.50059263827931E-15,1.85011080196342E-13,
2.65878198860263));
#228799=CARTESIAN_POINT('',(58.703595878104,-6.185320498293,2.65878198860258));
#228800=CARTESIAN_POINT('',(58.6332801510296,-6.1779300175717,2.65878198860258));
#228801=CARTESIAN_POINT('Origin',(5.72291486498914E-15,1.85429889878632E-13,
2.65878198860263));
#228802=CARTESIAN_POINT('Origin',(-0.0199126722524855,-0.189456421067746,
42.7590319886026));
#228803=CARTESIAN_POINT('',(59.6550713551494,-6.46154998175819,3.64303198860259));
#228804=CARTESIAN_POINT('',(59.2266168947287,-6.41651760334952,3.40423097483306));
#228805=CARTESIAN_POINT('Origin',(59.6170497665656,-6.4575537517665,3.20400220531816));
#228806=CARTESIAN_POINT('',(58.8722700235037,-6.37927424589621,2.83404198860258));
#228807=CARTESIAN_POINT('',(59.2266168947287,-6.41651760334952,3.40423097483306));
#228808=CARTESIAN_POINT('',(62.293614112757,-6.73887200051229,2.83404198860258));
#228809=CARTESIAN_POINT('',(62.5519772640373,-6.76602706194843,2.83404198860258));
#228810=CARTESIAN_POINT('',(61.9392677288638,-6.70162869542246,3.40423097483306));
#228811=CARTESIAN_POINT('',(62.293614112757,-6.73887200051229,2.83404198860258));
#228812=CARTESIAN_POINT('',(61.5108137072213,-6.65659636252282,3.64303198860259));
#228813=CARTESIAN_POINT('Origin',(61.5488354182641,-6.66059260538546,3.20400259787972));
#228814=CARTESIAN_POINT('',(61.1116329639869,-6.61464077648827,3.64303198860259));
#228815=CARTESIAN_POINT('',(-0.0199126722524799,-0.189456421067473,3.64303198860262));
#228816=CARTESIAN_POINT('',(60.9862851800405,-6.60146619279846,3.42473028058482));
#228817=CARTESIAN_POINT('',(61.1116329640613,-6.61464077578021,3.64303198860259));
#228818=CARTESIAN_POINT('',(60.6581326136905,-6.56697596826177,3.23423028058478));
#228819=CARTESIAN_POINT('Origin',(60.6873988786434,-6.5700514604533,3.56425722717));
#228820=CARTESIAN_POINT('',(60.5077528318945,-6.55117041629668,3.23423028058478));
#228821=CARTESIAN_POINT('',(-0.0199126722524799,-0.18945642106747,3.23423028058481));
#228822=CARTESIAN_POINT('',(60.1796001951996,-6.51668018436646,3.42473028058476));
#228823=CARTESIAN_POINT('Origin',(60.4784837816402,-6.54809359889815,3.56425909741463));
#228824=CARTESIAN_POINT('',(60.0542523588398,-6.50350559588366,3.64303198860259));
#228825=CARTESIAN_POINT('',(60.1796001951996,-6.51668018436646,3.42473028058476));
#228826=CARTESIAN_POINT('',(-0.0199126722524799,-0.189456421067473,3.64303198860262));
#228827=CARTESIAN_POINT('Origin',(0.0199126722524855,0.189456421067567,
42.7590319886026));
#228828=CARTESIAN_POINT('',(61.5506390517263,-6.27768352038751,3.64303198860259));
#228829=CARTESIAN_POINT('',(61.979093073432,-6.32271585268538,3.40423097483306));
#228830=CARTESIAN_POINT('Origin',(61.5886607624847,-6.28167976322025,3.20400259735804));
#228831=CARTESIAN_POINT('',(62.3334394573093,-6.35995915792693,2.83404198860258));
#228832=CARTESIAN_POINT('',(61.979093073432,-6.32271585268538,3.40423097483306));
#228833=CARTESIAN_POINT('',(58.9120953679531,-6.00036140428947,2.83404198860258));
#228834=CARTESIAN_POINT('',(0.0199126722524855,0.189456421067846,2.83404198860263));
#228835=CARTESIAN_POINT('',(59.2664422391598,-6.03760476191704,3.40423097483307));
#228836=CARTESIAN_POINT('',(58.9120953679531,-6.00036140428947,2.83404198860258));
#228837=CARTESIAN_POINT('',(59.6948966996543,-6.08263713962288,3.64303198860259));
#228838=CARTESIAN_POINT('Origin',(59.6568751107681,-6.0786409095994,3.20400220587286));
#228839=CARTESIAN_POINT('',(60.0940777032672,-6.12459275448601,3.64303198860259));
#228840=CARTESIAN_POINT('',(60.1675309762116,-6.13231300382077,3.64303198860259));
#228841=CARTESIAN_POINT('',(60.2194255397046,-6.13776734223115,3.42473028058478));
#228842=CARTESIAN_POINT('',(60.0940777033448,-6.12459275374834,3.64303198860259));
#228843=CARTESIAN_POINT('',(60.5475781763994,-6.17225757416137,3.23423028058478));
#228844=CARTESIAN_POINT('Origin',(60.5183119713881,-6.16918208839045,3.56425743004337));
#228845=CARTESIAN_POINT('',(60.6979579581955,-6.18806312612646,3.23423028058478));
#228846=CARTESIAN_POINT('',(60.6984837728334,-6.18811839147187,3.23423028058478));
#228847=CARTESIAN_POINT('',(61.0261105245455,-6.22255335066314,3.42473028058481));
#228848=CARTESIAN_POINT('Origin',(60.7272269341771,-6.1911399356034,3.56425912917777));
#228849=CARTESIAN_POINT('',(61.1514583085663,-6.2357279336449,3.64303198860259));
#228850=CARTESIAN_POINT('',(61.0261105245455,-6.22255335066314,3.42473028058481));
#228851=CARTESIAN_POINT('',(61.5511575797869,-6.27773801988278,3.64303198860259));
#228852=CARTESIAN_POINT('Origin',(57.9430040808458,6.10537907909402,2.83404198860266));
#228853=CARTESIAN_POINT('Ctrl Pts',(62.2936141127569,6.73887200051352,2.83404198860267));
#228854=CARTESIAN_POINT('Ctrl Pts',(62.3041663177857,6.73998108195344,2.82419652440025));
#228855=CARTESIAN_POINT('Ctrl Pts',(62.3147747227674,6.74025426844108,2.81438790575571));
#228856=CARTESIAN_POINT('Ctrl Pts',(62.3253809467532,6.73970068257604,2.8046678125679));
#228857=CARTESIAN_POINT('Ctrl Pts',(62.3356425316152,6.73916508495522,2.7952635645294));
#228858=CARTESIAN_POINT('Ctrl Pts',(62.345903357484,6.7378554363764,2.78594102496071));
#228859=CARTESIAN_POINT('Ctrl Pts',(62.3561113603665,6.73573381164759,2.77675109088598));
#228860=CARTESIAN_POINT('Ctrl Pts',(62.3657675025208,6.73372688529627,2.76805797913484));
#228861=CARTESIAN_POINT('Ctrl Pts',(62.3753772873503,6.73099321743756,2.75948271209948));
#228862=CARTESIAN_POINT('Ctrl Pts',(62.3848821415136,6.72746117704499,2.75108575572998));
#228863=CARTESIAN_POINT('Ctrl Pts',(62.3936367996066,6.72420791239975,2.74335155163028));
#228864=CARTESIAN_POINT('Ctrl Pts',(62.4023029415032,6.72027708243581,2.73576818685687));
#228865=CARTESIAN_POINT('Ctrl Pts',(62.4108128192423,6.71558140886142,2.72840626160229));
#228866=CARTESIAN_POINT('Ctrl Pts',(62.4132812112882,6.71421937245427,2.72627084693503));
#228867=CARTESIAN_POINT('Ctrl Pts',(62.4157362792969,6.71279278199471,2.72415424587436));
#228868=CARTESIAN_POINT('Ctrl Pts',(62.4181758915949,6.71129899689616,2.72205867173259));
#228869=CARTESIAN_POINT('Ctrl Pts',(62.4208205881801,6.70967963780687,2.71978693462864));
#228870=CARTESIAN_POINT('Ctrl Pts',(62.4234440047029,6.70798448411193,2.71754411340765));
#228871=CARTESIAN_POINT('Ctrl Pts',(62.4260429761973,6.70621108803143,2.71533341844262));
#228872=CARTESIAN_POINT('Ctrl Pts',(62.4331758738576,6.70134398857289,2.7092661487641));
#228873=CARTESIAN_POINT('Ctrl Pts',(62.4400912556838,6.69585818364714,2.70347381860428));
#228874=CARTESIAN_POINT('Ctrl Pts',(62.4466864116142,6.68976801333907,2.69804914171414));
#228875=CARTESIAN_POINT('Ctrl Pts',(62.4527206212313,6.68419583815009,2.69308585687209));
#228876=CARTESIAN_POINT('Ctrl Pts',(62.4584752900419,6.67811620689301,2.68842799053178));
#228877=CARTESIAN_POINT('Ctrl Pts',(62.4638645712592,6.67150703079137,2.684147670542));
#228878=CARTESIAN_POINT('Ctrl Pts',(62.4665117685881,6.66826062508035,2.68204519134548));
#228879=CARTESIAN_POINT('Ctrl Pts',(62.4690703232302,6.66488629457976,2.68003431778511));
#228880=CARTESIAN_POINT('Ctrl Pts',(62.4715267736419,6.6613807859173,2.67812693945273));
#228881=CARTESIAN_POINT('Ctrl Pts',(62.4719928611814,6.66071564979267,2.67776503299224));
#228882=CARTESIAN_POINT('Ctrl Pts',(62.472455189938,6.66004526561009,2.67740659639945));
#228883=CARTESIAN_POINT('Ctrl Pts',(62.4729136358129,6.65936969820877,2.67705178968876));
#228884=CARTESIAN_POINT('Ctrl Pts',(62.4733577552542,6.65871524228875,2.67670807068779));
#228885=CARTESIAN_POINT('Ctrl Pts',(62.4737982307,6.65805592206471,2.67636775825286));
#228886=CARTESIAN_POINT('Ctrl Pts',(62.474234948946,6.65739180030929,2.67603099699276));
#228887=CARTESIAN_POINT('Ctrl Pts',(62.4789942144025,6.65015433826444,2.67236104217156));
#228888=CARTESIAN_POINT('Ctrl Pts',(62.4833100626578,6.64234165497511,2.66911440541507));
#228889=CARTESIAN_POINT('Ctrl Pts',(62.4870273554125,6.63406423386216,2.66646778189666));
#228890=CARTESIAN_POINT('Ctrl Pts',(62.4885971912262,6.63056862752565,2.66535009635004));
#228891=CARTESIAN_POINT('Ctrl Pts',(62.490060506939,6.6269905114141,2.66433897912368));
#228892=CARTESIAN_POINT('Ctrl Pts',(62.4914070226221,6.6233395425202,2.66344564884813));
#228893=CARTESIAN_POINT('Ctrl Pts',(62.4936745213867,6.61719140213092,2.66194130298605));
#228894=CARTESIAN_POINT('Ctrl Pts',(62.4956084911391,6.61083770188544,2.66077206705439));
#228895=CARTESIAN_POINT('Ctrl Pts',(62.4971561593216,6.60433062536158,2.65998225155733));
#228896=CARTESIAN_POINT('Ctrl Pts',(62.4975430763672,6.60270385623062,2.65978479768306));
#228897=CARTESIAN_POINT('Ctrl Pts',(62.4979056188877,6.60106746196568,2.65961098966641));
#228898=CARTESIAN_POINT('Ctrl Pts',(62.4982426563689,6.59942221845757,2.6594613903052));
#228899=CARTESIAN_POINT('Ctrl Pts',(62.4987482125908,6.59695435319542,2.65923699126338));
#228900=CARTESIAN_POINT('Ctrl Pts',(62.4991963674669,6.59446659126617,2.6590670756246));
#228901=CARTESIAN_POINT('Ctrl Pts',(62.4995849724118,6.59196174500311,2.65895332562937));
#228902=CARTESIAN_POINT('Ctrl Pts',(62.4999735773567,6.58945689874005,2.65883957563415));
#228903=CARTESIAN_POINT('Ctrl Pts',(62.5003026407462,6.58693497617669,2.65878198860267));
#228904=CARTESIAN_POINT('Ctrl Pts',(62.5005702980931,6.58439859103048,2.65878198860267));
#228905=CARTESIAN_POINT('Ctrl Pts',(58.7035958781039,6.18532049829418,2.65878198860267));
#228906=CARTESIAN_POINT('Ctrl Pts',(58.702689976017,6.1939028191017,2.65878198860267));
#228907=CARTESIAN_POINT('Ctrl Pts',(58.7025003609929,6.20248552904377,2.65945335517858));
#228908=CARTESIAN_POINT('Ctrl Pts',(58.7029569544313,6.21093474935427,2.660725612266));
#228909=CARTESIAN_POINT('Ctrl Pts',(58.7032518669434,6.21639207873501,2.66154735980339));
#228910=CARTESIAN_POINT('Ctrl Pts',(58.7038154335198,6.22179377937528,2.66261895766886));
#228911=CARTESIAN_POINT('Ctrl Pts',(58.7046202140516,6.22710604846885,2.66391429251034));
#228912=CARTESIAN_POINT('Ctrl Pts',(58.7056869045457,6.23414715684661,2.6656311846413));
#228913=CARTESIAN_POINT('Ctrl Pts',(58.7071827955652,6.24102913891663,2.66774105138706));
#228914=CARTESIAN_POINT('Ctrl Pts',(58.709054816357,6.24767922440765,2.67016894181756));
#228915=CARTESIAN_POINT('Ctrl Pts',(58.7099908267528,6.25100426715316,2.67138288703282));
#228916=CARTESIAN_POINT('Ctrl Pts',(58.7110208470228,6.25427153376679,2.67267613167558));
#228917=CARTESIAN_POINT('Ctrl Pts',(58.7121380880307,6.25747333351535,2.6740383543256));
#228918=CARTESIAN_POINT('Ctrl Pts',(58.7126967085347,6.25907423338963,2.6747194656506));
#228919=CARTESIAN_POINT('Ctrl Pts',(58.7132771324571,6.2606587828836,2.67541781389529));
#228920=CARTESIAN_POINT('Ctrl Pts',(58.7138784999415,6.26222612320532,2.67613207244176));
#228921=CARTESIAN_POINT('Ctrl Pts',(58.7140288418126,6.26261795828575,2.67631063707837));
#228922=CARTESIAN_POINT('Ctrl Pts',(58.7141804926178,6.26300871814026,2.67649019601852));
#228923=CARTESIAN_POINT('Ctrl Pts',(58.7143334388435,6.2633983900507,2.67667072836663));
#228924=CARTESIAN_POINT('Ctrl Pts',(58.7147922775207,6.26456740578201,2.67721232541097));
#228925=CARTESIAN_POINT('Ctrl Pts',(58.715262775183,6.26572662828386,2.67776268340053));
#228926=CARTESIAN_POINT('Ctrl Pts',(58.7157445651923,6.2668757296518,2.67832123541522));
#228927=CARTESIAN_POINT('Ctrl Pts',(58.7191382318077,6.27496985131148,2.68225560368446));
#228928=CARTESIAN_POINT('Ctrl Pts',(58.7230632421217,6.28260716192764,2.68661792998883));
#228929=CARTESIAN_POINT('Ctrl Pts',(58.7274000190312,6.28978339589432,2.69130986622566));
#228930=CARTESIAN_POINT('Ctrl Pts',(58.729503351146,6.29326386161362,2.69358545023048));
#228931=CARTESIAN_POINT('Ctrl Pts',(58.731704109697,6.29663597408932,2.69593918853469));
#228932=CARTESIAN_POINT('Ctrl Pts',(58.7339915094193,6.29989941779164,2.6983630623548));
#228933=CARTESIAN_POINT('Ctrl Pts',(58.7374933585782,6.30489552208953,2.70207384382213));
#228934=CARTESIAN_POINT('Ctrl Pts',(58.7411954596217,6.30963480180888,2.70594760814213));
#228935=CARTESIAN_POINT('Ctrl Pts',(58.745053462885,6.31410463171063,2.70995196345693));
#228936=CARTESIAN_POINT('Ctrl Pts',(58.7468451395591,6.31618044384083,2.71181160678091));
#228937=CARTESIAN_POINT('Ctrl Pts',(58.7486702031823,6.31819823791544,2.71369962772084));
#228938=CARTESIAN_POINT('Ctrl Pts',(58.7505249478605,6.32015576082333,2.71561183138646));
#228939=CARTESIAN_POINT('Ctrl Pts',(58.750667106732,6.3203057972412,2.71575839426297));
#228940=CARTESIAN_POINT('Ctrl Pts',(58.7508094261759,6.32045551058207,2.71590508903194));
#228941=CARTESIAN_POINT('Ctrl Pts',(58.7509519047346,6.32060490094016,2.71605191409897));
#228942=CARTESIAN_POINT('Ctrl Pts',(58.7529532989256,6.32270338507401,2.71811436362738));
#228943=CARTESIAN_POINT('Ctrl Pts',(58.7549876922215,6.32473679726646,2.72020091026944));
#228944=CARTESIAN_POINT('Ctrl Pts',(58.757049379421,6.32670504965004,2.72230624862167));
#228945=CARTESIAN_POINT('Ctrl Pts',(58.7644422230598,6.33376285265589,2.72985561753118));
#228946=CARTESIAN_POINT('Ctrl Pts',(58.7722418109927,6.34003880538944,2.73770089914376));
#228947=CARTESIAN_POINT('Ctrl Pts',(58.780339648656,6.34560292136768,2.74574823347153));
#228948=CARTESIAN_POINT('Ctrl Pts',(58.7892383587479,6.35171732586275,2.75459144547133));
#228949=CARTESIAN_POINT('Ctrl Pts',(58.7984976730909,6.35697262978522,2.7636791175441));
#228950=CARTESIAN_POINT('Ctrl Pts',(58.8080148760667,6.36142852992898,2.77292162564898));
#228951=CARTESIAN_POINT('Ctrl Pts',(58.8182910667888,6.36623978380599,2.78290121484943));
#228952=CARTESIAN_POINT('Ctrl Pts',(58.828868892188,6.37011968263842,2.79306229500443));
#228953=CARTESIAN_POINT('Ctrl Pts',(58.8396533761915,6.37309732669917,2.8033191668555));
#228954=CARTESIAN_POINT('Ctrl Pts',(58.8503473894534,6.37604999138528,2.81348999408895));
#228955=CARTESIAN_POINT('Ctrl Pts',(58.8612460403474,6.3781155791126,2.82375635966979));
#228956=CARTESIAN_POINT('Ctrl Pts',(58.872270023448,6.37927424642597,2.83404198860267));
#228957=CARTESIAN_POINT('Origin',(0.00159301378019908,-0.0151565136852236,
2.83404198860262));
#228958=CARTESIAN_POINT('Ctrl Pts',(62.5037563256535,6.55408556365965,2.65878198860267));
#228959=CARTESIAN_POINT('Ctrl Pts',(62.5046505412978,6.54554330587399,2.65878198860267));
#228960=CARTESIAN_POINT('Ctrl Pts',(62.5048232320879,6.53700226086626,2.65944603041855));
#228961=CARTESIAN_POINT('Ctrl Pts',(62.5043472028589,6.52859457177385,2.66070439264073));
#228962=CARTESIAN_POINT('Ctrl Pts',(62.5040430428431,6.52322245869445,2.66150842619599));
#228963=CARTESIAN_POINT('Ctrl Pts',(62.5034749678471,6.51790471489591,2.66255428265372));
#228964=CARTESIAN_POINT('Ctrl Pts',(62.5026702669707,6.5126735674086,2.66381699700661));
#228965=CARTESIAN_POINT('Ctrl Pts',(62.5015720117389,6.50553410072667,2.66554034873261));
#228966=CARTESIAN_POINT('Ctrl Pts',(62.5000273428098,6.49855818190791,2.66766759643965));
#228967=CARTESIAN_POINT('Ctrl Pts',(62.4980940659029,6.49182203260195,2.6701201278314));
#228968=CARTESIAN_POINT('Ctrl Pts',(62.4971274274495,6.48845395794897,2.67134639352728));
#228969=CARTESIAN_POINT('Ctrl Pts',(62.4960636607366,6.48514561818754,2.67265375585004));
#228970=CARTESIAN_POINT('Ctrl Pts',(62.494910155573,6.48190505740182,2.67403135126931));
#228971=CARTESIAN_POINT('Ctrl Pts',(62.4943334029912,6.48028477700896,2.67472014897895));
#228972=CARTESIAN_POINT('Ctrl Pts',(62.4937342176674,6.47868142404699,2.67542649668624));
#228973=CARTESIAN_POINT('Ctrl Pts',(62.4931135352114,6.47709589524284,2.67614899656093));
#228974=CARTESIAN_POINT('Ctrl Pts',(62.4929583645974,6.47669951304181,2.6763296215296));
#228975=CARTESIAN_POINT('Ctrl Pts',(62.4928018504535,6.47630424448191,2.67651125590941));
#228976=CARTESIAN_POINT('Ctrl Pts',(62.4926440074817,6.47591010283092,2.67669387767514));
#228977=CARTESIAN_POINT('Ctrl Pts',(62.4921704785661,6.47472767787793,2.67724174297234));
#228978=CARTESIAN_POINT('Ctrl Pts',(62.4916849899864,6.47355539694487,2.67779849504738));
#228979=CARTESIAN_POINT('Ctrl Pts',(62.4911879405752,6.47239360181829,2.67836353617999));
#228980=CARTESIAN_POINT('Ctrl Pts',(62.4877530207469,6.46436487665183,2.68226832098905));
#228981=CARTESIAN_POINT('Ctrl Pts',(62.4837949925047,6.45678933786393,2.68659153751396));
#228982=CARTESIAN_POINT('Ctrl Pts',(62.4794326364365,6.44966853563983,2.69123699486192));
#228983=CARTESIAN_POINT('Ctrl Pts',(62.4772645574451,6.44612951648082,2.69354577441223));
#228984=CARTESIAN_POINT('Ctrl Pts',(62.4749960038951,6.44270272394358,2.69593478828115));
#228985=CARTESIAN_POINT('Ctrl Pts',(62.4726384024734,6.43938822718943,2.69839565261208));
#228986=CARTESIAN_POINT('Ctrl Pts',(62.4674371815967,6.43207595228373,2.70382468689034));
#228987=CARTESIAN_POINT('Ctrl Pts',(62.461813233051,6.42530381744009,2.70961155815075));
#228988=CARTESIAN_POINT('Ctrl Pts',(62.4558957623411,6.41913840445444,2.71562701361755));
#228989=CARTESIAN_POINT('Ctrl Pts',(62.4537340356675,6.41688610134083,2.71782453535845));
#228990=CARTESIAN_POINT('Ctrl Pts',(62.4515361835425,6.41470741397486,2.72005051502389));
#228991=CARTESIAN_POINT('Ctrl Pts',(62.4493074469123,6.41260146153657,2.72229986760102));
#228992=CARTESIAN_POINT('Ctrl Pts',(62.4418213564087,6.40552779014103,2.7298552048888));
#228993=CARTESIAN_POINT('Ctrl Pts',(62.4339335724862,6.39923601079887,2.7377084553455));
#228994=CARTESIAN_POINT('Ctrl Pts',(62.4257522463024,6.39365709371033,2.74576706701749));
#228995=CARTESIAN_POINT('Ctrl Pts',(62.4167599996846,6.38752520296385,2.7546244358503));
#228996=CARTESIAN_POINT('Ctrl Pts',(62.4074126717503,6.38225398283454,2.76373036323188));
#228997=CARTESIAN_POINT('Ctrl Pts',(62.3978127557445,6.37778536209576,2.77299664636831));
#228998=CARTESIAN_POINT('Ctrl Pts',(62.3874732348825,6.3729724660949,2.78297683033493));
#228999=CARTESIAN_POINT('Ctrl Pts',(62.3768396913508,6.36908997057773,2.79314401478916));
#229000=CARTESIAN_POINT('Ctrl Pts',(62.3660067738144,6.36611161569945,2.80341452427963));
#229001=CARTESIAN_POINT('Ctrl Pts',(62.3553201372418,6.36317347866838,2.81354634721382));
#229002=CARTESIAN_POINT('Ctrl Pts',(62.3444380411295,6.36111515612462,2.82378004209215));
#229003=CARTESIAN_POINT('Ctrl Pts',(62.3334394572619,6.35995915837821,2.83404198860267));
#229004=CARTESIAN_POINT('Ctrl Pts',(58.912095367953,6.00036140429066,2.83404198860266));
#229005=CARTESIAN_POINT('Ctrl Pts',(58.9015696628155,5.99925510810155,2.82422126443124));
#229006=CARTESIAN_POINT('Ctrl Pts',(58.8909945468916,5.99898299131213,2.81442815028733));
#229007=CARTESIAN_POINT('Ctrl Pts',(58.8804276387812,5.99953795195263,2.80471618166661));
#229008=CARTESIAN_POINT('Ctrl Pts',(58.8702243592828,6.00007381527864,2.79533842146637));
#229009=CARTESIAN_POINT('Ctrl Pts',(58.8600274754072,6.00138095727621,2.78603515650712));
#229010=CARTESIAN_POINT('Ctrl Pts',(58.8498890377533,6.00349883563876,2.77685887347287));
#229011=CARTESIAN_POINT('Ctrl Pts',(58.840305039008,6.00550089396986,2.76818441217135));
#229012=CARTESIAN_POINT('Ctrl Pts',(58.8307723843927,6.00822762538427,2.75962261522206));
#229013=CARTESIAN_POINT('Ctrl Pts',(58.8213500689105,6.01175153639394,2.75123537702261));
#229014=CARTESIAN_POINT('Ctrl Pts',(58.8126722744225,6.01499699931587,2.74351087134724));
#229015=CARTESIAN_POINT('Ctrl Pts',(58.8040875818613,6.01891888228952,2.73593399450453));
#229016=CARTESIAN_POINT('Ctrl Pts',(58.7956642413115,6.02360485257183,2.72857657813182));
#229017=CARTESIAN_POINT('Ctrl Pts',(58.7931525711942,6.02500211431843,2.7263827450872));
#229018=CARTESIAN_POINT('Ctrl Pts',(58.7906554330111,6.02646752363638,2.72420861709793));
#229019=CARTESIAN_POINT('Ctrl Pts',(58.7881751602884,6.02800395803723,2.72205663736713));
#229020=CARTESIAN_POINT('Ctrl Pts',(58.7857202298425,6.0295246938637,2.71992664556752));
#229021=CARTESIAN_POINT('Ctrl Pts',(58.783284225042,6.03111319985522,2.7178208992787));
#229022=CARTESIAN_POINT('Ctrl Pts',(58.7808720541407,6.03277025542048,2.71574387311232));
#229023=CARTESIAN_POINT('Ctrl Pts',(58.7807043164937,6.0328854838238,2.71559944077473));
#229024=CARTESIAN_POINT('Ctrl Pts',(58.7805366835715,6.03300103800929,2.71545515216055));
#229025=CARTESIAN_POINT('Ctrl Pts',(58.7803691562898,6.03311691890581,2.71531100781716));
#229026=CARTESIAN_POINT('Ctrl Pts',(58.7730241465597,6.03819756191456,2.70899119176059));
#229027=CARTESIAN_POINT('Ctrl Pts',(58.7659160498048,6.04393622206024,2.70298296066806));
#229028=CARTESIAN_POINT('Ctrl Pts',(58.7591607781926,6.05034076157619,2.69736727774097));
#229029=CARTESIAN_POINT('Ctrl Pts',(58.7528636909918,6.05631090550661,2.69213248525372));
#229030=CARTESIAN_POINT('Ctrl Pts',(58.7468728126818,6.06286038933392,2.68723866185397));
#229031=CARTESIAN_POINT('Ctrl Pts',(58.7413107827872,6.07000150504488,2.6827859582948));
#229032=CARTESIAN_POINT('Ctrl Pts',(58.7392761202949,6.07261381755777,2.68115710172747));
#229033=CARTESIAN_POINT('Ctrl Pts',(58.7372991657061,6.07530531160715,2.67958763637775));
#229034=CARTESIAN_POINT('Ctrl Pts',(58.735387140493,6.07807653793574,2.67808378645351));
#229035=CARTESIAN_POINT('Ctrl Pts',(58.7349273623043,6.07874292528938,2.67772216078586));
#229036=CARTESIAN_POINT('Ctrl Pts',(58.7344713442223,6.07941450700203,2.67736403603549));
#229037=CARTESIAN_POINT('Ctrl Pts',(58.7340192051468,6.08009121771094,2.67700956934465));
#229038=CARTESIAN_POINT('Ctrl Pts',(58.7335811954175,6.0807467812102,2.6766661797379));
#229039=CARTESIAN_POINT('Ctrl Pts',(58.7331468260468,6.08140715812726,2.67632622314104));
#229040=CARTESIAN_POINT('Ctrl Pts',(58.7327162055066,6.0820722852656,2.67598984158759));
#229041=CARTESIAN_POINT('Ctrl Pts',(58.7279982598322,6.08935952173602,2.67230439292219));
#229042=CARTESIAN_POINT('Ctrl Pts',(58.7237275533354,6.09722197243166,2.66904964539982));
#229043=CARTESIAN_POINT('Ctrl Pts',(58.7200553115705,6.10554709909129,2.66640203566737));
#229044=CARTESIAN_POINT('Ctrl Pts',(58.7185323234527,6.10899977726284,2.66530399299441));
#229045=CARTESIAN_POINT('Ctrl Pts',(58.7171120447817,6.11253167434587,2.66430995142251));
#229046=CARTESIAN_POINT('Ctrl Pts',(58.7158039367398,6.11613350280244,2.66343053473345));
#229047=CARTESIAN_POINT('Ctrl Pts',(58.7135728221602,6.12227679657168,2.66193059792869));
#229048=CARTESIAN_POINT('Ctrl Pts',(58.7116702942288,6.12862250657805,2.66076519817111));
#229049=CARTESIAN_POINT('Ctrl Pts',(58.7101471179289,6.13511848061118,2.65997805604443));
#229050=CARTESIAN_POINT('Ctrl Pts',(58.7093855297789,6.13836646762775,2.65958448498109));
#229051=CARTESIAN_POINT('Ctrl Pts',(58.7087202098052,6.14165223896383,2.65928526260745));
#229052=CARTESIAN_POINT('Ctrl Pts',(58.7081575578112,6.14496923836513,2.65908463971307));
#229053=CARTESIAN_POINT('Ctrl Pts',(58.7075949058173,6.14828623776644,2.6588840168187));
#229054=CARTESIAN_POINT('Ctrl Pts',(58.7071349090267,6.15163442139611,2.65878198860267));
#229055=CARTESIAN_POINT('Ctrl Pts',(58.7067819056643,6.15500747092335,2.65878198860267));
#229056=CARTESIAN_POINT('Origin',(56.9874003490102,12.1286263473646,2.83404198860271));
#229057=CARTESIAN_POINT('Ctrl Pts',(61.2479592423878,13.2134115091896,2.83404198860272));
#229058=CARTESIAN_POINT('Ctrl Pts',(61.2583377107544,13.215617520741,2.82419652440085));
#229059=CARTESIAN_POINT('Ctrl Pts',(61.2688594460195,13.2169980909549,2.81438790575682));
#229060=CARTESIAN_POINT('Ctrl Pts',(61.2794654334798,13.2175561899855,2.80466781256948));
#229061=CARTESIAN_POINT('Ctrl Pts',(61.2897267895022,13.2180961541209,2.79526356453138));
#229062=CARTESIAN_POINT('Ctrl Pts',(61.3000683010463,13.2178662282941,2.78594102496306));
#229063=CARTESIAN_POINT('Ctrl Pts',(61.310442153593,13.2168232529021,2.77675109088867));
#229064=CARTESIAN_POINT('Ctrl Pts',(61.3202551793171,13.2158366624039,2.76805797913786));
#229065=CARTESIAN_POINT('Ctrl Pts',(61.3300980668398,13.2141224659046,2.7594827121028));
#229066=CARTESIAN_POINT('Ctrl Pts',(61.3399200511715,13.2116033021985,2.75108575573356));
#229067=CARTESIAN_POINT('Ctrl Pts',(61.348966809085,13.2092829702345,2.74335155163417));
#229068=CARTESIAN_POINT('Ctrl Pts',(61.3579963605644,13.2062795322637,2.73576818686104));
#229069=CARTESIAN_POINT('Ctrl Pts',(61.3669504518452,13.2024991065236,2.72840626160669));
#229070=CARTESIAN_POINT('Ctrl Pts',(61.3695476933555,13.2014025487211,2.72627084693797));
#229071=CARTESIAN_POINT('Ctrl Pts',(61.3721384315549,13.2002403977588,2.72415424587585));
#229072=CARTESIAN_POINT('Ctrl Pts',(61.374720822464,13.1990098046949,2.72205867173268));
#229073=CARTESIAN_POINT('Ctrl Pts',(61.3775203002416,13.197675762694,2.71978693462871));
#229074=CARTESIAN_POINT('Ctrl Pts',(61.3803065372249,13.196264116926,2.71754411340771));
#229075=CARTESIAN_POINT('Ctrl Pts',(61.3830766416486,13.1947721021912,2.71533341844267));
#229076=CARTESIAN_POINT('Ctrl Pts',(61.3906792149762,13.1906772560438,2.70926614876414));
#229077=CARTESIAN_POINT('Ctrl Pts',(61.3981301363758,13.1859443571666,2.70347381860432));
#229078=CARTESIAN_POINT('Ctrl Pts',(61.4053257594953,13.1805769309631,2.69804914171418));
#229079=CARTESIAN_POINT('Ctrl Pts',(61.4119093639903,13.1756660273912,2.69308585687216));
#229080=CARTESIAN_POINT('Ctrl Pts',(61.4182680026355,13.1702212276777,2.68842799053186));
#229081=CARTESIAN_POINT('Ctrl Pts',(61.4243186078278,13.1642115906181,2.6841476705421));
#229082=CARTESIAN_POINT('Ctrl Pts',(61.4272906453329,13.1612596765259,2.68204519134556));
#229083=CARTESIAN_POINT('Ctrl Pts',(61.4301878975268,13.1581712727458,2.68003431778516));
#229084=CARTESIAN_POINT('Ctrl Pts',(61.4329973166795,13.1549417366132,2.67812693945276));
#229085=CARTESIAN_POINT('Ctrl Pts',(61.4335303765997,13.1543289635881,2.67776503299228));
#229086=CARTESIAN_POINT('Ctrl Pts',(61.4340602468995,13.1537105783546,2.67740659639948));
#229087=CARTESIAN_POINT('Ctrl Pts',(61.4345867973822,13.153086632425,2.67705178968879));
#229088=CARTESIAN_POINT('Ctrl Pts',(61.4350968931623,13.1524821848057,2.67670807068782));
#229089=CARTESIAN_POINT('Ctrl Pts',(61.4356038733673,13.1518725186283,2.6763677582529));
#229090=CARTESIAN_POINT('Ctrl Pts',(61.4361076188515,13.1512576844885,2.67603099699279));
#229091=CARTESIAN_POINT('Ctrl Pts',(61.4415973333393,13.1445573487226,2.67236104217168));
#229092=CARTESIAN_POINT('Ctrl Pts',(61.4467061867043,13.1372385931158,2.66911440541525));
#229093=CARTESIAN_POINT('Ctrl Pts',(61.4512683418492,13.1293950794811,2.66646778189688));
#229094=CARTESIAN_POINT('Ctrl Pts',(61.4531949682967,13.1260827149669,2.66535009635018));
#229095=CARTESIAN_POINT('Ctrl Pts',(61.4550242827915,13.1226771582923,2.66433897912377));
#229096=CARTESIAN_POINT('Ctrl Pts',(61.4567450522889,13.119186939003,2.66344564884816));
#229097=CARTESIAN_POINT('Ctrl Pts',(61.4596427851248,13.1133094969314,2.66194130298609));
#229098=CARTESIAN_POINT('Ctrl Pts',(61.4622303029113,13.1071927578069,2.66077206705443));
#229099=CARTESIAN_POINT('Ctrl Pts',(61.4644496675149,13.1008831031058,2.65998225155737));
#229100=CARTESIAN_POINT('Ctrl Pts',(61.4650045086658,13.0993056894305,2.6597847976831));
#229101=CARTESIAN_POINT('Ctrl Pts',(61.4655361149183,13.0977161555171,2.65961098966645));
#229102=CARTESIAN_POINT('Ctrl Pts',(61.4660432808485,13.0961151548351,2.65946139030524));
#229103=CARTESIAN_POINT('Ctrl Pts',(61.4668040297439,13.093713653812,2.65923699126343));
#229104=CARTESIAN_POINT('Ctrl Pts',(61.4675097715121,13.0912863650434,2.65906707562464));
#229105=CARTESIAN_POINT('Ctrl Pts',(61.4681580753691,13.088835860868,2.65895332562942));
#229106=CARTESIAN_POINT('Ctrl Pts',(61.4688063792261,13.0863853566926,2.6588395756342));
#229107=CARTESIAN_POINT('Ctrl Pts',(61.4693972526619,13.0839116459753,2.65878198860271));
#229108=CARTESIAN_POINT('Ctrl Pts',(61.4699285681954,13.0814171332235,2.65878198860271));
#229109=CARTESIAN_POINT('Ctrl Pts',(57.7354693911204,12.2876333308473,2.65878198860271));
#229110=CARTESIAN_POINT('Ctrl Pts',(57.7336713548546,12.2960739442509,2.65878198860271));
#229111=CARTESIAN_POINT('Ctrl Pts',(57.7325856410805,12.3045898170433,2.65945335517869));
#229112=CARTESIAN_POINT('Ctrl Pts',(57.7321565492375,12.3130404786518,2.66072561226624));
#229113=CARTESIAN_POINT('Ctrl Pts',(57.7318793999343,12.3184987389624,2.66154735980361));
#229114=CARTESIAN_POINT('Ctrl Pts',(57.7318752477671,12.3239297572691,2.662618957669));
#229115=CARTESIAN_POINT('Ctrl Pts',(57.7321203363021,12.3292970476686,2.66391429251038));
#229116=CARTESIAN_POINT('Ctrl Pts',(57.7324451871157,12.3364110836361,2.66563118464134));
#229117=CARTESIAN_POINT('Ctrl Pts',(57.7332135204776,12.3434117286777,2.66774105138709));
#229118=CARTESIAN_POINT('Ctrl Pts',(57.7343801629266,12.3502210637611,2.6701689418176));
#229119=CARTESIAN_POINT('Ctrl Pts',(57.7349634841511,12.3536257313029,2.67138288703285));
#229120=CARTESIAN_POINT('Ctrl Pts',(57.7356463395041,12.3569827659241,2.67267613167561));
#229121=CARTESIAN_POINT('Ctrl Pts',(57.7364227809415,12.3602838093643,2.67403835432563));
#229122=CARTESIAN_POINT('Ctrl Pts',(57.7368110016602,12.3619343310844,2.67471946565064));
#229123=CARTESIAN_POINT('Ctrl Pts',(57.737222615436,12.3635708710711,2.67541781389532));
#229124=CARTESIAN_POINT('Ctrl Pts',(57.7376568568912,12.3651924853575,2.67613207244178));
#229125=CARTESIAN_POINT('Ctrl Pts',(57.737765417255,12.3655978889291,2.6763106370784));
#229126=CARTESIAN_POINT('Ctrl Pts',(57.7378753917741,12.3660023599859,2.67649019601855));
#229127=CARTESIAN_POINT('Ctrl Pts',(57.7379867683384,12.3664058844668,2.67667072836666));
#229128=CARTESIAN_POINT('Ctrl Pts',(57.7383208980314,12.3676164579094,2.677212325411));
#229129=CARTESIAN_POINT('Ctrl Pts',(57.7386676465115,12.3688185104667,2.67776268340057));
#229130=CARTESIAN_POINT('Ctrl Pts',(57.7390266834246,12.3700116777064,2.67832123541526));
#229131=CARTESIAN_POINT('Ctrl Pts',(57.7415556930807,12.378416193677,2.68225560368456));
#229132=CARTESIAN_POINT('Ctrl Pts',(57.7446608854353,12.3864219416031,2.68661792998903));
#229133=CARTESIAN_POINT('Ctrl Pts',(57.7482237843187,12.3940121800353,2.69130986622596));
#229134=CARTESIAN_POINT('Ctrl Pts',(57.7499517864269,12.3976934374727,2.6935854502307));
#229135=CARTESIAN_POINT('Ctrl Pts',(57.7517880072572,12.4012771190727,2.69593918853482));
#229136=CARTESIAN_POINT('Ctrl Pts',(57.7537217536093,12.4047617836667,2.69836306235484));
#229137=CARTESIAN_POINT('Ctrl Pts',(57.7566821841675,12.4100965616936,2.70207384382218));
#229138=CARTESIAN_POINT('Ctrl Pts',(57.759868615088,12.4151968540757,2.70594760814218));
#229139=CARTESIAN_POINT('Ctrl Pts',(57.7632382593551,12.420045468934,2.70995196345698));
#229140=CARTESIAN_POINT('Ctrl Pts',(57.7648031395849,12.4222971907576,2.71181160678096));
#229141=CARTESIAN_POINT('Ctrl Pts',(57.7664072884048,12.424494702241,2.71369962772089));
#229142=CARTESIAN_POINT('Ctrl Pts',(57.7680472557362,12.4266353752445,2.71561183138651));
#229143=CARTESIAN_POINT('Ctrl Pts',(57.7681729527704,12.4267994493956,2.71575839426302));
#229144=CARTESIAN_POINT('Ctrl Pts',(57.768298843268,12.4269632190239,2.71590508903199));
#229145=CARTESIAN_POINT('Ctrl Pts',(57.7684249257697,12.4271266840708,2.71605191409901));
#229146=CARTESIAN_POINT('Ctrl Pts',(57.7701960047922,12.4294228751481,2.71811436362743));
#229147=CARTESIAN_POINT('Ctrl Pts',(57.7720067040171,12.4316578001007,2.72020091026949));
#229148=CARTESIAN_POINT('Ctrl Pts',(57.7738513586814,12.4338307751865,2.72230624862172));
#229149=CARTESIAN_POINT('Ctrl Pts',(57.7804659622463,12.4416226773929,2.72985561753045));
#229150=CARTESIAN_POINT('Ctrl Pts',(57.7875668075249,12.4486795287408,2.7377008991422));
#229151=CARTESIAN_POINT('Ctrl Pts',(57.7950386758926,12.4550596184357,2.74574823346909));
#229152=CARTESIAN_POINT('Ctrl Pts',(57.803249508613,12.4620706960736,2.75459144546791));
#229153=CARTESIAN_POINT('Ctrl Pts',(57.8119087706191,12.46826507279,2.76367911753964));
#229154=CARTESIAN_POINT('Ctrl Pts',(57.8209080689656,12.473691381648,2.77292162564346));
#229155=CARTESIAN_POINT('Ctrl Pts',(57.8306250526641,12.4795504333968,2.78290121484255));
#229156=CARTESIAN_POINT('Ctrl Pts',(57.840739371765,12.484514761571,2.79306229499614));
#229157=CARTESIAN_POINT('Ctrl Pts',(57.8511535286773,12.4886033793261,2.80331916684582));
#229158=CARTESIAN_POINT('Ctrl Pts',(57.8614803215165,12.4926576977804,2.81348999408244));
#229159=CARTESIAN_POINT('Ctrl Pts',(57.8721033557531,12.495851189233,2.82375635966655));
#229160=CARTESIAN_POINT('Ctrl Pts',(57.8829458346105,12.4981558292589,2.83404198860271));
#229161=CARTESIAN_POINT('Origin',(0.00316857416806278,-0.0149069694349949,
2.83404198860262));
#229162=CARTESIAN_POINT('Ctrl Pts',(61.4762657165316,13.0516031943531,2.65878198860271));
#229163=CARTESIAN_POINT('Ctrl Pts',(61.4780479426482,13.0432012029367,2.65878198860271));
#229164=CARTESIAN_POINT('Ctrl Pts',(61.4791124697294,13.0347249977703,2.65944603041856));
#229165=CARTESIAN_POINT('Ctrl Pts',(61.4795178910588,13.0263136082749,2.66070439264067));
#229166=CARTESIAN_POINT('Ctrl Pts',(61.4797769359881,13.0209391308139,2.66150842619593));
#229167=CARTESIAN_POINT('Ctrl Pts',(61.4797678285537,13.0155911381657,2.66255428265368));
#229168=CARTESIAN_POINT('Ctrl Pts',(61.4795143397208,13.0103045333055,2.6638169970066));
#229169=CARTESIAN_POINT('Ctrl Pts',(61.479168378327,13.0030893784374,2.6655403487326));
#229170=CARTESIAN_POINT('Ctrl Pts',(61.4783613533299,12.9959902125624,2.66766759643964));
#229171=CARTESIAN_POINT('Ctrl Pts',(61.4771427864515,12.989088882123,2.6701201278314));
#229172=CARTESIAN_POINT('Ctrl Pts',(61.4765335030122,12.9856382169033,2.67134639352728));
#229173=CARTESIAN_POINT('Ctrl Pts',(61.4758213793959,12.9822368066734,2.67265375585004));
#229174=CARTESIAN_POINT('Ctrl Pts',(61.4750129240934,12.9788934238966,2.67403135126932));
#229175=CARTESIAN_POINT('Ctrl Pts',(61.4746086964421,12.9772217325082,2.67472014897896));
#229176=CARTESIAN_POINT('Ctrl Pts',(61.4741803895393,12.9755645309604,2.67542649668625));
#229177=CARTESIAN_POINT('Ctrl Pts',(61.4737288401361,12.9739228088657,2.67614899656094));
#229178=CARTESIAN_POINT('Ctrl Pts',(61.4736159527854,12.973512378342,2.67632962152962));
#229179=CARTESIAN_POINT('Ctrl Pts',(61.4735016128575,12.9731029149217,2.67651125590943));
#229180=CARTESIAN_POINT('Ctrl Pts',(61.473385833587,12.9726944333366,2.67669387767516));
#229181=CARTESIAN_POINT('Ctrl Pts',(61.4730384957757,12.9714689885813,2.67724174297236));
#229182=CARTESIAN_POINT('Ctrl Pts',(61.4726782034777,12.9702523821507,2.6777984950474));
#229183=CARTESIAN_POINT('Ctrl Pts',(61.4723053176144,12.9690449956483,2.67836353618002));
#229184=CARTESIAN_POINT('Ctrl Pts',(61.46972844494,12.9607012057873,2.68226832098904));
#229185=CARTESIAN_POINT('Ctrl Pts',(61.4665839586185,12.9527534399839,2.68659153751391));
#229186=CARTESIAN_POINT('Ctrl Pts',(61.4629898265071,12.9452156558834,2.69123699486182));
#229187=CARTESIAN_POINT('Ctrl Pts',(61.4612035527134,12.9414693978764,2.69354577441217));
#229188=CARTESIAN_POINT('Ctrl Pts',(61.4593056238949,12.9378242492507,2.69593478828114));
#229189=CARTESIAN_POINT('Ctrl Pts',(61.4573073969127,12.9342814732029,2.69839565261212));
#229190=CARTESIAN_POINT('Ctrl Pts',(61.4528990097271,12.9264655800789,2.70382468689038));
#229191=CARTESIAN_POINT('Ctrl Pts',(61.4480137506082,12.9191426809995,2.70961155815079));
#229192=CARTESIAN_POINT('Ctrl Pts',(61.4427731575668,12.9123924986716,2.7156270136176));
#229193=CARTESIAN_POINT('Ctrl Pts',(61.4408587028414,12.9099265719429,2.71782453535851));
#229194=CARTESIAN_POINT('Ctrl Pts',(61.4389006256227,12.9075300815492,2.72005051502395));
#229195=CARTESIAN_POINT('Ctrl Pts',(61.436904230217,12.9052026993237,2.72229986760109));
#229196=CARTESIAN_POINT('Ctrl Pts',(61.4301985493013,12.8973852687042,2.72985520488861));
#229197=CARTESIAN_POINT('Ctrl Pts',(61.4230116455106,12.8903034584559,2.73770845534501));
#229198=CARTESIAN_POINT('Ctrl Pts',(61.415458293118,12.8838999218056,2.74576706701669));
#229199=CARTESIAN_POINT('Ctrl Pts',(61.407156264085,12.8768616764781,2.7546244358492));
#229200=CARTESIAN_POINT('Ctrl Pts',(61.398411134331,12.8706422708196,2.76373036323047));
#229201=CARTESIAN_POINT('Ctrl Pts',(61.3893309057286,12.8651946651853,2.77299664636657));
#229202=CARTESIAN_POINT('Ctrl Pts',(61.3795511104668,12.8593273605057,2.78297683033289));
#229203=CARTESIAN_POINT('Ctrl Pts',(61.3693816498896,12.8543546257408,2.79314401478682));
#229204=CARTESIAN_POINT('Ctrl Pts',(61.3589193990677,12.8502602383793,2.803414524277));
#229205=CARTESIAN_POINT('Ctrl Pts',(61.3485984239563,12.8462211390714,2.81354634721204));
#229206=CARTESIAN_POINT('Ctrl Pts',(61.3379910943966,12.8430366034498,2.82378004209126));
#229207=CARTESIAN_POINT('Ctrl Pts',(61.3271735965893,12.84073727331,2.83404198860272));
#229208=CARTESIAN_POINT('Ctrl Pts',(57.9621601888121,12.1254815933794,2.8340419886027));
#229209=CARTESIAN_POINT('Ctrl Pts',(57.9518077840282,12.1232811218135,2.82422126443033));
#229210=CARTESIAN_POINT('Ctrl Pts',(57.9413190436447,12.1219050950918,2.81442815028545));
#229211=CARTESIAN_POINT('Ctrl Pts',(57.9307520129786,12.1213524729337,2.80471618166379));
#229212=CARTESIAN_POINT('Ctrl Pts',(57.9205486151423,12.1208188676182,2.79533842146307));
#229213=CARTESIAN_POINT('Ctrl Pts',(57.9102709573187,12.1210529843537,2.78603515650333));
#229214=CARTESIAN_POINT('Ctrl Pts',(57.8999666805159,12.1220995054494,2.77685887346864));
#229215=CARTESIAN_POINT('Ctrl Pts',(57.8902259118376,12.1230887956349,2.76818441216703));
#229216=CARTESIAN_POINT('Ctrl Pts',(57.8804604570571,12.1248041559918,2.75962261521767));
#229217=CARTESIAN_POINT('Ctrl Pts',(57.8707214090023,12.1273238624908,2.75123537701818));
#229218=CARTESIAN_POINT('Ctrl Pts',(57.8617519091287,12.1296444699052,2.74351087134297));
#229219=CARTESIAN_POINT('Ctrl Pts',(57.8528042960114,12.1326475236727,2.73593399450044));
#229220=CARTESIAN_POINT('Ctrl Pts',(57.8439372821301,12.1364273448765,2.7285765781279));
#229221=CARTESIAN_POINT('Ctrl Pts',(57.8412933175829,12.1375544112589,2.72638274508463));
#229222=CARTESIAN_POINT('Ctrl Pts',(57.8386566820015,12.1387507708937,2.72420861709668));
#229223=CARTESIAN_POINT('Ctrl Pts',(57.8360293953471,12.1400195294492,2.72205663736717));
#229224=CARTESIAN_POINT('Ctrl Pts',(57.8334289530881,12.1412753244188,2.71992664556756));
#229225=CARTESIAN_POINT('Ctrl Pts',(57.8308402488866,12.14260049657,2.71782089927875));
#229226=CARTESIAN_POINT('Ctrl Pts',(57.8282680826381,12.143996334094,2.71574387311236));
#229227=CARTESIAN_POINT('Ctrl Pts',(57.8280892192276,12.1440933979056,2.71559944077477));
#229228=CARTESIAN_POINT('Ctrl Pts',(57.8279104259146,12.1441907966614,2.71545515216059));
#229229=CARTESIAN_POINT('Ctrl Pts',(57.8277317035128,12.144288531381,2.7153110078172));
#229230=CARTESIAN_POINT('Ctrl Pts',(57.8198958587085,12.1485735795159,2.70899119176064));
#229231=CARTESIAN_POINT('Ctrl Pts',(57.812226847525,12.1535378042503,2.70298296066811));
#229232=CARTESIAN_POINT('Ctrl Pts',(57.8048391253241,12.1592011408681,2.69736727774103));
#229233=CARTESIAN_POINT('Ctrl Pts',(57.7979524842552,12.1644803548773,2.69213248525373));
#229234=CARTESIAN_POINT('Ctrl Pts',(57.7913098171238,12.1703677426436,2.68723866185394));
#229235=CARTESIAN_POINT('Ctrl Pts',(57.7850318067596,12.1768883481381,2.68278595829474));
#229236=CARTESIAN_POINT('Ctrl Pts',(57.7827352293487,12.179273669986,2.68115710172745));
#229237=CARTESIAN_POINT('Ctrl Pts',(57.7804877669873,12.1817437717242,2.67958763637776));
#229238=CARTESIAN_POINT('Ctrl Pts',(57.7782965440189,12.1842999559277,2.67808378645355));
#229239=CARTESIAN_POINT('Ctrl Pts',(57.7777696280971,12.1849146328342,2.6777221607859));
#229240=CARTESIAN_POINT('Ctrl Pts',(57.7772459087255,12.1855348686826,2.67736403603553));
#229241=CARTESIAN_POINT('Ctrl Pts',(57.7767255109848,12.1861606108967,2.67700956934469));
#229242=CARTESIAN_POINT('Ctrl Pts',(57.7762213756734,12.1867667986667,2.67666617973794));
#229243=CARTESIAN_POINT('Ctrl Pts',(57.7757203576392,12.187378154007,2.67632622314108));
#229244=CARTESIAN_POINT('Ctrl Pts',(57.7752225713658,12.187994625406,2.67598984158763));
#229245=CARTESIAN_POINT('Ctrl Pts',(57.7697687474616,12.1947487820215,2.67230439292218));
#229246=CARTESIAN_POINT('Ctrl Pts',(57.764699586453,12.2021217510025,2.66904964539978));
#229247=CARTESIAN_POINT('Ctrl Pts',(57.7601772489165,12.2100174179589,2.6664020356673));
#229248=CARTESIAN_POINT('Ctrl Pts',(57.7583017007436,12.2132919863906,2.66530399299439));
#229249=CARTESIAN_POINT('Ctrl Pts',(57.7565200187333,12.2166560758248,2.66430995142252));
#229250=CARTESIAN_POINT('Ctrl Pts',(57.7548425830507,12.2201014385647,2.66343053473349));
#229251=CARTESIAN_POINT('Ctrl Pts',(57.7519815416931,12.2259778637495,2.66193059792872));
#229252=CARTESIAN_POINT('Ctrl Pts',(57.7494261286934,12.2320899429715,2.66076519817115));
#229253=CARTESIAN_POINT('Ctrl Pts',(57.7472322823296,12.2383911161014,2.65997805604447));
#229254=CARTESIAN_POINT('Ctrl Pts',(57.7461353591478,12.2415417026663,2.65958448498113));
#229255=CARTESIAN_POINT('Ctrl Pts',(57.745130227238,12.2447399293287,2.65928526260749));
#229256=CARTESIAN_POINT('Ctrl Pts',(57.7442239366605,12.247979944712,2.65908463971311));
#229257=CARTESIAN_POINT('Ctrl Pts',(57.7433176460829,12.2512199600952,2.65888401681874));
#229258=CARTESIAN_POINT('Ctrl Pts',(57.7425101887133,12.254501719267,2.65878198860271));
#229259=CARTESIAN_POINT('Ctrl Pts',(57.7418065394566,12.257819391977,2.65878198860271));
#229260=CARTESIAN_POINT('Origin',(55.4074307335706,18.0189898472952,2.83404198860275));
#229261=CARTESIAN_POINT('Ctrl Pts',(59.5312589135996,19.5431821162869,2.83404198860276));
#229262=CARTESIAN_POINT('Ctrl Pts',(59.5413499366335,19.5464608884258,2.82419652440055));
#229263=CARTESIAN_POINT('Ctrl Pts',(59.5516697238494,19.5489337165498,2.81438790575618));
#229264=CARTESIAN_POINT('Ctrl Pts',(59.562159273367,19.5505973858262,2.8046678125685));
#229265=CARTESIAN_POINT('Ctrl Pts',(59.5723079749865,19.5522069957576,2.79526356453009));
#229266=CARTESIAN_POINT('Ctrl Pts',(59.5826168684419,19.553059311798,2.78594102496147));
#229267=CARTESIAN_POINT('Ctrl Pts',(59.5930429125542,19.5531064127991,2.77675109088679));
#229268=CARTESIAN_POINT('Ctrl Pts',(59.6029053082857,19.5531509674457,2.76805797913568));
#229269=CARTESIAN_POINT('Ctrl Pts',(59.6128734577668,19.5524750234009,2.75948271210033));
#229270=CARTESIAN_POINT('Ctrl Pts',(59.6229049605519,19.5509963368653,2.75108575573083));
#229271=CARTESIAN_POINT('Ctrl Pts',(59.6321447001138,19.5496343596247,2.74335155163114));
#229272=CARTESIAN_POINT('Ctrl Pts',(59.6414387315215,19.5475912199412,2.73576818685772));
#229273=CARTESIAN_POINT('Ctrl Pts',(59.6507389334469,19.54476746117,2.72840626160314));
#229274=CARTESIAN_POINT('Ctrl Pts',(59.653436568497,19.54394839609,2.72627084693563));
#229275=CARTESIAN_POINT('Ctrl Pts',(59.6561345922141,19.5430634173954,2.7241542458747));
#229276=CARTESIAN_POINT('Ctrl Pts',(59.658831468516,19.542109499003,2.72205867173269));
#229277=CARTESIAN_POINT('Ctrl Pts',(59.6617550558218,19.5410753901338,2.71978693462873));
#229278=CARTESIAN_POINT('Ctrl Pts',(59.6646735866702,19.5399627185792,2.71754411340774));
#229279=CARTESIAN_POINT('Ctrl Pts',(59.6675844741794,19.5387684320157,2.71533341844271));
#229280=CARTESIAN_POINT('Ctrl Pts',(59.6755734277899,19.5354907031708,2.70926614876419));
#229281=CARTESIAN_POINT('Ctrl Pts',(59.683478254909,19.5315625649727,2.70347381860436));
#229282=CARTESIAN_POINT('Ctrl Pts',(59.6911955084649,19.5269766895185,2.69804914171422));
#229283=CARTESIAN_POINT('Ctrl Pts',(59.6982563764893,19.5227808624507,2.69308585687216));
#229284=CARTESIAN_POINT('Ctrl Pts',(59.7051493183936,19.5180305486458,2.68842799053182));
#229285=CARTESIAN_POINT('Ctrl Pts',(59.7117949558643,19.5126862934693,2.68414767054202));
#229286=CARTESIAN_POINT('Ctrl Pts',(59.7150592712806,19.5100612127846,2.68204519134552));
#229287=CARTESIAN_POINT('Ctrl Pts',(59.7182634781249,19.5072925729231,2.68003431778517));
#229288=CARTESIAN_POINT('Ctrl Pts',(59.7213950854346,19.5043743927941,2.6781269394528));
#229289=CARTESIAN_POINT('Ctrl Pts',(59.7219892774193,19.5038206965381,2.67776503299232));
#229290=CARTESIAN_POINT('Ctrl Pts',(59.7225808838923,19.5032610854118,2.67740659639953));
#229291=CARTESIAN_POINT('Ctrl Pts',(59.7231697699855,19.5026955970361,2.67705178968884));
#229292=CARTESIAN_POINT('Ctrl Pts',(59.7237402533883,19.5021477801721,2.67670807068786));
#229293=CARTESIAN_POINT('Ctrl Pts',(59.7243081837714,19.5015944476715,2.67636775825294));
#229294=CARTESIAN_POINT('Ctrl Pts',(59.724873437353,19.5010356373988,2.67603099699284));
#229295=CARTESIAN_POINT('Ctrl Pts',(59.7310334544114,19.4949458381924,2.67236104217166));
#229296=CARTESIAN_POINT('Ctrl Pts',(59.73687933922,19.4882011960857,2.66911440541519));
#229297=CARTESIAN_POINT('Ctrl Pts',(59.7422363728284,19.4808775251058,2.66646778189679));
#229298=CARTESIAN_POINT('Ctrl Pts',(59.744498681387,19.4777846933729,2.66535009635015));
#229299=CARTESIAN_POINT('Ctrl Pts',(59.7466739523113,19.4745890081272,2.66433897912378));
#229300=CARTESIAN_POINT('Ctrl Pts',(59.748750122512,19.4712977780157,2.66344564884821));
#229301=CARTESIAN_POINT('Ctrl Pts',(59.752246341252,19.465755428747,2.66194130298614));
#229302=CARTESIAN_POINT('Ctrl Pts',(59.7554590576862,19.4599426670173,2.66077206705447));
#229303=CARTESIAN_POINT('Ctrl Pts',(59.758325802888,19.4538995640364,2.65998225155741));
#229304=CARTESIAN_POINT('Ctrl Pts',(59.7590424891885,19.4523887882911,2.65978479768315));
#229305=CARTESIAN_POINT('Ctrl Pts',(59.7597373347835,19.4508635299954,2.65961098966649));
#229306=CARTESIAN_POINT('Ctrl Pts',(59.7604090725467,19.449324313038,2.65946139030529));
#229307=CARTESIAN_POINT('Ctrl Pts',(59.7614166791915,19.4470154876017,2.65923699126347));
#229308=CARTESIAN_POINT('Ctrl Pts',(59.7623722755974,19.4446752658775,2.65906707562469));
#229309=CARTESIAN_POINT('Ctrl Pts',(59.7632731754137,19.4423059520262,2.65895332562946));
#229310=CARTESIAN_POINT('Ctrl Pts',(59.76417407523,19.439936638175,2.65883957563424));
#229311=CARTESIAN_POINT('Ctrl Pts',(59.7650202849808,19.4375382417966,2.65878198860276));
#229312=CARTESIAN_POINT('Ctrl Pts',(59.7658094374968,19.4351129318428,2.65878198860276));
#229313=CARTESIAN_POINT('Ctrl Pts',(56.1347810195642,18.2553202812751,2.65878198860275));
#229314=CARTESIAN_POINT('Ctrl Pts',(56.1321105487811,18.2635267101474,2.65878198860275));
#229315=CARTESIAN_POINT('Ctrl Pts',(56.1301406315643,18.2718824441049,2.6594533551787));
#229316=CARTESIAN_POINT('Ctrl Pts',(56.1288305556598,18.2802419597938,2.66072561226618));
#229317=CARTESIAN_POINT('Ctrl Pts',(56.1279843810471,18.2856413491927,2.66154735980356));
#229318=CARTESIAN_POINT('Ctrl Pts',(56.1274125556283,18.2910421817935,2.66261895766898));
#229319=CARTESIAN_POINT('Ctrl Pts',(56.1270952669252,18.2964056883426,2.6639142925104));
#229320=CARTESIAN_POINT('Ctrl Pts',(56.1266747189247,18.3035147090331,2.66563118464136));
#229321=CARTESIAN_POINT('Ctrl Pts',(56.126707076608,18.3105573165143,2.66774105138712));
#229322=CARTESIAN_POINT('Ctrl Pts',(56.1271555587355,18.3174512966901,2.67016894181762));
#229323=CARTESIAN_POINT('Ctrl Pts',(56.1273797997992,18.320898286778,2.67138288703288));
#229324=CARTESIAN_POINT('Ctrl Pts',(56.127708008729,18.324308309033,2.67267613167564));
#229325=CARTESIAN_POINT('Ctrl Pts',(56.128135143741,18.3276724292421,2.67403835432566));
#229326=CARTESIAN_POINT('Ctrl Pts',(56.128348711247,18.3293544893466,2.67471946565067));
#229327=CARTESIAN_POINT('Ctrl Pts',(56.1285870051496,18.3310250895515,2.67541781389536));
#229328=CARTESIAN_POINT('Ctrl Pts',(56.1288493629352,18.3326832110572,2.67613207244182));
#229329=CARTESIAN_POINT('Ctrl Pts',(56.1289149523817,18.3330977414336,2.67631063707844));
#229330=CARTESIAN_POINT('Ctrl Pts',(56.1289820457109,18.3335114922231,2.67649019601858));
#229331=CARTESIAN_POINT('Ctrl Pts',(56.1290506323488,18.3339244481758,2.6766707283667));
#229332=CARTESIAN_POINT('Ctrl Pts',(56.1292563922628,18.3351633160338,2.67721232541104));
#229333=CARTESIAN_POINT('Ctrl Pts',(56.1294755925119,18.3363950287072,2.6777626834006));
#229334=CARTESIAN_POINT('Ctrl Pts',(56.1297079426452,18.3376191892287,2.67832123541529));
#229335=CARTESIAN_POINT('Ctrl Pts',(56.1313445869829,18.3462420178745,2.68225560368465));
#229336=CARTESIAN_POINT('Ctrl Pts',(56.1335959402409,18.3545284904609,2.68661792998919));
#229337=CARTESIAN_POINT('Ctrl Pts',(56.1363459252322,18.3624495731178,2.69130986622619));
#229338=CARTESIAN_POINT('Ctrl Pts',(56.1376796649813,18.3662912896467,2.69358545023088));
#229339=CARTESIAN_POINT('Ctrl Pts',(56.1391312300712,18.3700472768054,2.69593918853493));
#229340=CARTESIAN_POINT('Ctrl Pts',(56.1406901365234,18.3737149835765,2.69836306235489));
#229341=CARTESIAN_POINT('Ctrl Pts',(56.1430767133842,18.3793299863881,2.70207384382222));
#229342=CARTESIAN_POINT('Ctrl Pts',(56.1457125629779,18.3847354115623,2.70594760814222));
#229343=CARTESIAN_POINT('Ctrl Pts',(56.148556929721,18.3899096889381,2.70995196345702));
#229344=CARTESIAN_POINT('Ctrl Pts',(56.1498778683512,18.3923126501195,2.711811606781));
#229345=CARTESIAN_POINT('Ctrl Pts',(56.1512435269776,18.3946658026161,2.71369962772093));
#229346=CARTESIAN_POINT('Ctrl Pts',(56.152650749137,18.3969661720539,2.71561183138655));
#229347=CARTESIAN_POINT('Ctrl Pts',(56.1527586071708,18.3971424863074,2.71575839426306));
#229348=CARTESIAN_POINT('Ctrl Pts',(56.1528666894395,18.3973185179288,2.71590508903203));
#229349=CARTESIAN_POINT('Ctrl Pts',(56.1529749944979,18.3974942667072,2.71605191409906));
#229350=CARTESIAN_POINT('Ctrl Pts',(56.1544963540396,18.3999630071782,2.71811436362748));
#229351=CARTESIAN_POINT('Ctrl Pts',(56.1560635207938,18.4023749585854,2.72020091026954));
#229352=CARTESIAN_POINT('Ctrl Pts',(56.1576709325004,18.4047288488037,2.72230624862177));
#229353=CARTESIAN_POINT('Ctrl Pts',(56.1634348250117,18.4131694805009,2.72985561753108));
#229354=CARTESIAN_POINT('Ctrl Pts',(56.1697591292906,18.4209299141242,2.73770089914347));
#229355=CARTESIAN_POINT('Ctrl Pts',(56.1765231650109,18.4280560759389,2.74574823347102));
#229356=CARTESIAN_POINT('Ctrl Pts',(56.1839561607596,18.4358870118866,2.75459144547035));
#229357=CARTESIAN_POINT('Ctrl Pts',(56.1919204977439,18.44295259451,2.76367911754263));
#229358=CARTESIAN_POINT('Ctrl Pts',(56.2003032932669,18.4492898603071,2.77292162564701));
#229359=CARTESIAN_POINT('Ctrl Pts',(56.2093546086368,18.456132516931,2.78290121484645));
#229360=CARTESIAN_POINT('Ctrl Pts',(56.2188946068446,18.4621268842286,2.7930622950004));
#229361=CARTESIAN_POINT('Ctrl Pts',(56.2288243369853,18.4672816799261,2.80331916685042));
#229362=CARTESIAN_POINT('Ctrl Pts',(56.2386707668939,18.4723932321846,2.81348999408555));
#229363=CARTESIAN_POINT('Ctrl Pts',(56.2489017962819,18.4766796388001,2.82375635966813));
#229364=CARTESIAN_POINT('Ctrl Pts',(56.2594439784239,18.4801050014193,2.83404198860275));
#229365=CARTESIAN_POINT('Origin',(0.00470941899427448,-0.0144941013081504,
2.83404198860262));
#229366=CARTESIAN_POINT('Ctrl Pts',(59.7752282754837,19.4061247292256,2.65878198860276));
#229367=CARTESIAN_POINT('Ctrl Pts',(59.7778789856303,19.3979550581544,2.65878198860276));
#229368=CARTESIAN_POINT('Ctrl Pts',(59.7798236858212,19.3896365599065,2.65944603041863));
#229369=CARTESIAN_POINT('Ctrl Pts',(59.781106115828,19.3813136269513,2.66070439264079));
#229370=CARTESIAN_POINT('Ctrl Pts',(59.7819255275519,19.3759956690086,2.66150842619604));
#229371=CARTESIAN_POINT('Ctrl Pts',(59.7824754874621,19.3706760212378,2.66255428265377));
#229372=CARTESIAN_POINT('Ctrl Pts',(59.7827759879495,19.3653918801542,2.66381699700666));
#229373=CARTESIAN_POINT('Ctrl Pts',(59.783186110819,19.3581800878465,2.66554034873266));
#229374=CARTESIAN_POINT('Ctrl Pts',(59.7831255716887,19.3510354548622,2.6676675964397));
#229375=CARTESIAN_POINT('Ctrl Pts',(59.7826350657124,19.3440445557098,2.67012012783147));
#229376=CARTESIAN_POINT('Ctrl Pts',(59.7823898127243,19.3405491061336,2.67134639352735));
#229377=CARTESIAN_POINT('Ctrl Pts',(59.7820371343799,19.3370918919976,2.67265375585011));
#229378=CARTESIAN_POINT('Ctrl Pts',(59.7815825865439,19.3336823180311,2.67403135126939));
#229379=CARTESIAN_POINT('Ctrl Pts',(59.7813553126259,19.3319775310479,2.67472014897903));
#229380=CARTESIAN_POINT('Ctrl Pts',(59.7811025767643,19.3302846375612,2.67542649668632));
#229381=CARTESIAN_POINT('Ctrl Pts',(59.7808251076836,19.3286047092266,2.67614899656101));
#229382=CARTESIAN_POINT('Ctrl Pts',(59.7807557404135,19.328184727143,2.67632962152968));
#229383=CARTESIAN_POINT('Ctrl Pts',(59.7806848274338,19.3277655550292,2.67651125590949));
#229384=CARTESIAN_POINT('Ctrl Pts',(59.7806123803667,19.3273472089197,2.67669387767523));
#229385=CARTESIAN_POINT('Ctrl Pts',(59.7803950391653,19.3260921705914,2.67724174297243));
#229386=CARTESIAN_POINT('Ctrl Pts',(59.7801638905868,19.3248445680579,2.67779849504746));
#229387=CARTESIAN_POINT('Ctrl Pts',(59.7799192536869,19.3236048185588,2.67836353618008));
#229388=CARTESIAN_POINT('Ctrl Pts',(59.7782286609226,19.315037380311,2.68226832098912));
#229389=CARTESIAN_POINT('Ctrl Pts',(59.7759321681721,19.3068044648772,2.68659153751402));
#229390=CARTESIAN_POINT('Ctrl Pts',(59.7731456380809,19.2989322844403,2.69123699486196));
#229391=CARTESIAN_POINT('Ctrl Pts',(59.7717607402745,19.2950198323721,2.69354577441228));
#229392=CARTESIAN_POINT('Ctrl Pts',(59.7702542302928,19.2911962646692,2.69593478828122));
#229393=CARTESIAN_POINT('Ctrl Pts',(59.7686372707431,19.2874640247236,2.69839565261218));
#229394=CARTESIAN_POINT('Ctrl Pts',(59.765070016461,19.2792301459419,2.70382468689043));
#229395=CARTESIAN_POINT('Ctrl Pts',(59.7609769706902,19.2714367138416,2.70961155815084));
#229396=CARTESIAN_POINT('Ctrl Pts',(59.7564706723513,19.2641757185814,2.71562701361764));
#229397=CARTESIAN_POINT('Ctrl Pts',(59.7548244647406,19.2615231854469,2.71782453535854));
#229398=CARTESIAN_POINT('Ctrl Pts',(59.7531276155319,19.2589351484757,2.72005051502398));
#229399=CARTESIAN_POINT('Ctrl Pts',(59.7513854342766,19.2564118357497,2.72229986760111));
#229400=CARTESIAN_POINT('Ctrl Pts',(59.7455336317917,19.2479362953116,2.72985520488891));
#229401=CARTESIAN_POINT('Ctrl Pts',(59.7391263493541,19.2401420439515,2.73770845534564));
#229402=CARTESIAN_POINT('Ctrl Pts',(59.7322837268614,19.2329840462267,2.74576706701767));
#229403=CARTESIAN_POINT('Ctrl Pts',(59.72476287418,19.2251165588065,2.75462443585051));
#229404=CARTESIAN_POINT('Ctrl Pts',(59.7167157560775,19.2180171087286,2.76373036323212));
#229405=CARTESIAN_POINT('Ctrl Pts',(59.7082546997627,19.2116502033059,2.77299664636857));
#229406=CARTESIAN_POINT('Ctrl Pts',(59.6991417795841,19.2047927733655,2.78297683033519));
#229407=CARTESIAN_POINT('Ctrl Pts',(59.6895478206989,19.1987842816755,2.79314401478941));
#229408=CARTESIAN_POINT('Ctrl Pts',(59.6795708632003,19.1936187207957,2.80341452427985));
#229409=CARTESIAN_POINT('Ctrl Pts',(59.6697286283149,19.1885229124291,2.81354634721401));
#229410=CARTESIAN_POINT('Ctrl Pts',(59.6595122814319,19.1842470541691,2.8237800420923));
#229411=CARTESIAN_POINT('Ctrl Pts',(59.6489943884564,19.1808295835784,2.83404198860276));
#229412=CARTESIAN_POINT('Ctrl Pts',(56.3771794532807,18.1177524687109,2.83404198860275));
#229413=CARTESIAN_POINT('Ctrl Pts',(56.3671137719648,18.1144819305953,2.82422126443045));
#229414=CARTESIAN_POINT('Ctrl Pts',(56.3568263239572,18.1120170699781,2.81442815028565));
#229415=CARTESIAN_POINT('Ctrl Pts',(56.3463749453358,18.1103629196652,2.80471618166407));
#229416=CARTESIAN_POINT('Ctrl Pts',(56.3362832197241,18.1087656919995,2.79533842146335));
#229417=CARTESIAN_POINT('Ctrl Pts',(56.3260373921228,18.1079242184407,2.78603515650362));
#229418=CARTESIAN_POINT('Ctrl Pts',(56.3156801719846,18.107887916365,2.77685887346893));
#229419=CARTESIAN_POINT('Ctrl Pts',(56.3058893552734,18.1078535995344,2.76818441216724));
#229420=CARTESIAN_POINT('Ctrl Pts',(56.2959980926938,18.1085387949865,2.75962261521781));
#229421=CARTESIAN_POINT('Ctrl Pts',(56.286049015115,18.1100266905428,2.75123537701824));
#229422=CARTESIAN_POINT('Ctrl Pts',(56.2768860815732,18.1113970173888,2.74351087134289));
#229423=CARTESIAN_POINT('Ctrl Pts',(56.2676735798211,18.1134483398646,2.73593399450021));
#229424=CARTESIAN_POINT('Ctrl Pts',(56.2584600414676,18.1162805994777,2.72857657812754));
#229425=CARTESIAN_POINT('Ctrl Pts',(56.255712750318,18.1171251221214,2.72638274508441));
#229426=CARTESIAN_POINT('Ctrl Pts',(56.2529655048683,18.1180393245074,2.72420861709659));
#229427=CARTESIAN_POINT('Ctrl Pts',(56.2502199893832,18.1190265064342,2.72205663736722));
#229428=CARTESIAN_POINT('Ctrl Pts',(56.2475025263006,18.1200036017944,2.71992664556761));
#229429=CARTESIAN_POINT('Ctrl Pts',(56.244789485083,18.1210509212418,2.71782089927879));
#229430=CARTESIAN_POINT('Ctrl Pts',(56.242085504679,18.1221702476366,2.7157438731124));
#229431=CARTESIAN_POINT('Ctrl Pts',(56.2418974751699,18.1222480834051,2.71559944077481));
#229432=CARTESIAN_POINT('Ctrl Pts',(56.2417094803631,18.12232625961,2.71545515216063));
#229433=CARTESIAN_POINT('Ctrl Pts',(56.2415215209613,18.1224047773505,2.71531100781725));
#229434=CARTESIAN_POINT('Ctrl Pts',(56.2332806922381,18.1258472827277,2.7089911917607));
#229435=CARTESIAN_POINT('Ctrl Pts',(56.2251347899176,18.1299826829658,2.70298296066818));
#229436=CARTESIAN_POINT('Ctrl Pts',(56.2171955585582,18.1348427679843,2.69736727774111));
#229437=CARTESIAN_POINT('Ctrl Pts',(56.2097948151021,18.1393732118986,2.69213248525389));
#229438=CARTESIAN_POINT('Ctrl Pts',(56.2025731376006,18.1445340001514,2.68723866185417));
#229439=CARTESIAN_POINT('Ctrl Pts',(56.1956479299622,18.1503626543108,2.68278595829503));
#229440=CARTESIAN_POINT('Ctrl Pts',(56.1931145994154,18.1524948514087,2.68115710172765));
#229441=CARTESIAN_POINT('Ctrl Pts',(56.190621252949,18.1547164978844,2.67958763637787));
#229442=CARTESIAN_POINT('Ctrl Pts',(56.1881748397225,18.1570296338739,2.67808378645358));
#229443=CARTESIAN_POINT('Ctrl Pts',(56.1875865590689,18.1575858658044,2.67772216078593));
#229444=CARTESIAN_POINT('Ctrl Pts',(56.1870008763867,18.1581479603548,2.67736403603556));
#229445=CARTESIAN_POINT('Ctrl Pts',(56.1864179215672,18.1587158783115,2.67700956934472));
#229446=CARTESIAN_POINT('Ctrl Pts',(56.1858531840857,18.159266048832,2.67666617973797));
#229447=CARTESIAN_POINT('Ctrl Pts',(56.1852910066466,18.1598216844587,2.67632622314112));
#229448=CARTESIAN_POINT('Ctrl Pts',(56.1847315084904,18.1603827459286,2.67598984158766));
#229449=CARTESIAN_POINT('Ctrl Pts',(56.1786015595926,18.1665298227359,2.67230439292221));
#229450=CARTESIAN_POINT('Ctrl Pts',(56.172789482861,18.1733325302111,2.6690496453998));
#229451=CARTESIAN_POINT('Ctrl Pts',(56.1674665972293,18.1807122308847,2.66640203566733));
#229452=CARTESIAN_POINT('Ctrl Pts',(56.1652590378995,18.1837728127195,2.66530399299442));
#229453=CARTESIAN_POINT('Ctrl Pts',(56.1631354730308,18.1869322368373,2.66430995142256));
#229454=CARTESIAN_POINT('Ctrl Pts',(56.1611070880438,18.1901833857455,2.66343053473353));
#229455=CARTESIAN_POINT('Ctrl Pts',(56.157647466076,18.1957285590018,2.66193059792876));
#229456=CARTESIAN_POINT('Ctrl Pts',(56.1544671656478,18.2015400422205,2.66076519817119));
#229457=CARTESIAN_POINT('Ctrl Pts',(56.1516266854597,18.2075773774755,2.65997805604451));
#229458=CARTESIAN_POINT('Ctrl Pts',(56.1502064453657,18.210596045103,2.65958448498117));
#229459=CARTESIAN_POINT('Ctrl Pts',(56.1488725139556,18.2136716866512,2.65928526260753));
#229460=CARTESIAN_POINT('Ctrl Pts',(56.1476325143037,18.2167992197299,2.65908463971316));
#229461=CARTESIAN_POINT('Ctrl Pts',(56.1463925146518,18.2199267528085,2.65888401681878));
#229462=CARTESIAN_POINT('Ctrl Pts',(56.1452464433752,18.2231061318822,2.65878198860275));
#229463=CARTESIAN_POINT('Ctrl Pts',(56.1441998575527,18.2263320786585,2.65878198860275));
#229464=CARTESIAN_POINT('Origin',(53.2204057122638,23.7119335237428,2.83404198860279));
#229465=CARTESIAN_POINT('Ctrl Pts',(57.1623216544371,25.6588335304443,2.8340419886028));
#229466=CARTESIAN_POINT('Ctrl Pts',(57.1720146727781,25.663149140257,2.82419652440077));
#229467=CARTESIAN_POINT('Ctrl Pts',(57.1820194461961,25.6666871334688,2.8143879057565));
#229468=CARTESIAN_POINT('Ctrl Pts',(57.1922776320711,25.6694381454823,2.8046678125689));
#229469=CARTESIAN_POINT('Ctrl Pts',(57.2022024879886,25.6720997659865,2.79526356453055));
#229470=CARTESIAN_POINT('Ctrl Pts',(57.2123658169611,25.6740249857413,2.78594102496196));
#229471=CARTESIAN_POINT('Ctrl Pts',(57.2227298227175,25.6751616470872,2.77675109088729));
#229472=CARTESIAN_POINT('Ctrl Pts',(57.2325335339844,25.6762368587288,2.76805797913617));
#229473=CARTESIAN_POINT('Ctrl Pts',(57.2425177322919,25.676606572923,2.7594827121008));
#229474=CARTESIAN_POINT('Ctrl Pts',(57.2526488462863,25.6761845643574,2.75108575573128));
#229475=CARTESIAN_POINT('Ctrl Pts',(57.261980334976,25.675795863948,2.74335155163154));
#229476=CARTESIAN_POINT('Ctrl Pts',(57.2714370189586,25.6747354076181,2.73576818685809));
#229477=CARTESIAN_POINT('Ctrl Pts',(57.2809814365697,25.6728992535083,2.72840626160347));
#229478=CARTESIAN_POINT('Ctrl Pts',(57.2837499093069,25.6723666549987,2.72627084693586));
#229479=CARTESIAN_POINT('Ctrl Pts',(57.2865256584309,25.671768544583,2.72415424587485));
#229480=CARTESIAN_POINT('Ctrl Pts',(57.289307472586,25.6711017521907,2.72205867173275));
#229481=CARTESIAN_POINT('Ctrl Pts',(57.2923231379855,25.6703789063664,2.71978693462878));
#229482=CARTESIAN_POINT('Ctrl Pts',(57.2953419866643,25.6695773996876,2.71754411340779));
#229483=CARTESIAN_POINT('Ctrl Pts',(57.2983617649664,25.6686939261489,2.71533341844276));
#229484=CARTESIAN_POINT('Ctrl Pts',(57.3066495702123,25.6662692260896,2.70926614876423));
#229485=CARTESIAN_POINT('Ctrl Pts',(57.3149216961106,25.6631888860747,2.70347381860441));
#229486=CARTESIAN_POINT('Ctrl Pts',(57.323076028258,25.6594348051809,2.69804914171426));
#229487=CARTESIAN_POINT('Ctrl Pts',(57.3305367994641,25.6560000249768,2.69308585687221));
#229488=CARTESIAN_POINT('Ctrl Pts',(57.3378885241135,25.6519962425126,2.68842799053188));
#229489=CARTESIAN_POINT('Ctrl Pts',(57.3450563828676,25.6473759219974,2.6841476705421));
#229490=CARTESIAN_POINT('Ctrl Pts',(57.3485772116725,25.6451064356535,2.68204519134558));
#229491=CARTESIAN_POINT('Ctrl Pts',(57.3520532672065,25.6426878935082,2.68003431778521));
#229492=CARTESIAN_POINT('Ctrl Pts',(57.3554727521281,25.6401130415749,2.67812693945283));
#229493=CARTESIAN_POINT('Ctrl Pts',(57.3561215660858,25.6396244884999,2.67776503299235));
#229494=CARTESIAN_POINT('Ctrl Pts',(57.3567684269677,25.6391297826975,2.67740659639955));
#229495=CARTESIAN_POINT('Ctrl Pts',(57.3574131967122,25.6386289474846,2.67705178968887));
#229496=CARTESIAN_POINT('Ctrl Pts',(57.3580378174022,25.6381437633721,2.67670807068789));
#229497=CARTESIAN_POINT('Ctrl Pts',(57.3586604755991,25.637652826975,2.67636775825297));
#229498=CARTESIAN_POINT('Ctrl Pts',(57.3592810442415,25.6371561630117,2.67603099699287));
#229499=CARTESIAN_POINT('Ctrl Pts',(57.3660438734345,25.6317436214795,2.67236104217177));
#229500=CARTESIAN_POINT('Ctrl Pts',(57.3725627409489,25.6256469885836,2.66911440541536));
#229501=CARTESIAN_POINT('Ctrl Pts',(57.3786559602397,25.6189233999305,2.66646778189699));
#229502=CARTESIAN_POINT('Ctrl Pts',(57.3812291645836,25.6160839866904,2.66535009635028));
#229503=CARTESIAN_POINT('Ctrl Pts',(57.3837265592141,25.6131331854697,2.66433897912385));
#229504=CARTESIAN_POINT('Ctrl Pts',(57.3861353831632,25.6100770039414,2.66344564884824));
#229505=CARTESIAN_POINT('Ctrl Pts',(57.3901917825031,25.6049304706141,2.66194130298617));
#229506=CARTESIAN_POINT('Ctrl Pts',(57.3939944983914,25.5994853721131,2.66077206705451));
#229507=CARTESIAN_POINT('Ctrl Pts',(57.397477215531,25.5937750303531,2.65998225155745));
#229508=CARTESIAN_POINT('Ctrl Pts',(57.398347894816,25.5923474449131,2.65978479768319));
#229509=CARTESIAN_POINT('Ctrl Pts',(57.3991983668799,25.5909031732843,2.65961098966653));
#229510=CARTESIAN_POINT('Ctrl Pts',(57.4000273167765,25.5894426040344,2.65946139030532));
#229511=CARTESIAN_POINT('Ctrl Pts',(57.4012707416215,25.5872517501597,2.65923699126351));
#229512=CARTESIAN_POINT('Ctrl Pts',(57.4024657229508,25.5850242354387,2.65906707562473));
#229513=CARTESIAN_POINT('Ctrl Pts',(57.4036093482795,25.58276207061,2.65895332562951));
#229514=CARTESIAN_POINT('Ctrl Pts',(57.4047529736082,25.5804999057813,2.65883957563428));
#229515=CARTESIAN_POINT('Ctrl Pts',(57.4058452484196,25.5782031010733,2.6587819886028));
#229516=CARTESIAN_POINT('Ctrl Pts',(57.4068835917979,25.5758735661211,2.6587819886028));
#229517=CARTESIAN_POINT('Ctrl Pts',(53.9190682401995,24.0229981225299,2.65878198860279));
#229518=CARTESIAN_POINT('Ctrl Pts',(53.915554593136,24.0308804555186,2.65878198860279));
#229519=CARTESIAN_POINT('Ctrl Pts',(53.9127220553018,24.0389845034714,2.65945335517867));
#229520=CARTESIAN_POINT('Ctrl Pts',(53.9105453488017,24.0471612846371,2.66072561226602));
#229521=CARTESIAN_POINT('Ctrl Pts',(53.9091394197454,24.0524426462845,2.66154735980342));
#229522=CARTESIAN_POINT('Ctrl Pts',(53.9080061861139,24.0577541205273,2.66261895766892));
#229523=CARTESIAN_POINT('Ctrl Pts',(53.9071299964541,24.0630550795263,2.66391429251044));
#229524=CARTESIAN_POINT('Ctrl Pts',(53.9059686572515,24.0700811970213,2.6656311846414));
#229525=CARTESIAN_POINT('Ctrl Pts',(53.9052646847386,24.0770886066608,2.66774105138715));
#229526=CARTESIAN_POINT('Ctrl Pts',(53.9049900928804,24.0839917000394,2.67016894181766));
#229527=CARTESIAN_POINT('Ctrl Pts',(53.9048527969514,24.0874432467287,2.67138288703291));
#229528=CARTESIAN_POINT('Ctrl Pts',(53.9048227635323,24.0908688957001,2.67267613167568));
#229529=CARTESIAN_POINT('Ctrl Pts',(53.9048959123383,24.0942592346731,2.67403835432569));
#229530=CARTESIAN_POINT('Ctrl Pts',(53.9049324867413,24.0959544041596,2.6747194656507));
#229531=CARTESIAN_POINT('Ctrl Pts',(53.9049948499728,24.0976407611372,2.6754178138954));
#229532=CARTESIAN_POINT('Ctrl Pts',(53.9050824496422,24.099317223136,2.67613207244186));
#229533=CARTESIAN_POINT('Ctrl Pts',(53.9051043495595,24.0997363386357,2.67631063707847));
#229534=CARTESIAN_POINT('Ctrl Pts',(53.9051278266102,24.1001548360176,2.67649019601862));
#229535=CARTESIAN_POINT('Ctrl Pts',(53.9051528718723,24.1005726990103,2.67667072836673));
#229536=CARTESIAN_POINT('Ctrl Pts',(53.9052280076585,24.1018262879881,2.67721232541107));
#229537=CARTESIAN_POINT('Ctrl Pts',(53.9053172580728,24.1030741658758,2.67776268340064));
#229538=CARTESIAN_POINT('Ctrl Pts',(53.9054203757497,24.1043159075203,2.67832123541533));
#229539=CARTESIAN_POINT('Ctrl Pts',(53.906146723351,24.1130625753258,2.68225560368456));
#229540=CARTESIAN_POINT('Ctrl Pts',(53.9075195712149,24.1215389842443,2.68661792998894));
#229541=CARTESIAN_POINT('Ctrl Pts',(53.9094265129031,24.1297041260866,2.69130986622577));
#229542=CARTESIAN_POINT('Ctrl Pts',(53.9103513775612,24.133664211057,2.69358545023059));
#229543=CARTESIAN_POINT('Ctrl Pts',(53.91140238326,24.1375513523935,2.6959391885348));
#229544=CARTESIAN_POINT('Ctrl Pts',(53.9125693701071,24.1413619171793,2.69836306235492));
#229545=CARTESIAN_POINT('Ctrl Pts',(53.914355945435,24.1471956256297,2.70207384382226));
#229546=CARTESIAN_POINT('Ctrl Pts',(53.916412334782,24.1528469606267,2.70594760814226));
#229547=CARTESIAN_POINT('Ctrl Pts',(53.9187002605239,24.1582902100542,2.70995196345705));
#229548=CARTESIAN_POINT('Ctrl Pts',(53.9197627850745,24.1608180832479,2.71181160678103));
#229549=CARTESIAN_POINT('Ctrl Pts',(53.9208749910658,24.1633010951265,2.71369962772097));
#229550=CARTESIAN_POINT('Ctrl Pts',(53.9220340502326,24.1657359576697,2.71561183138659));
#229551=CARTESIAN_POINT('Ctrl Pts',(53.9221228875509,24.1659225802897,2.7157583942631));
#229552=CARTESIAN_POINT('Ctrl Pts',(53.9222119774187,24.1661089452649,2.71590508903207));
#229553=CARTESIAN_POINT('Ctrl Pts',(53.922301318421,24.1662950522344,2.71605191409909));
#229554=CARTESIAN_POINT('Ctrl Pts',(53.9235562901482,24.1689092940617,2.71811436362751));
#229555=CARTESIAN_POINT('Ctrl Pts',(53.9248627542249,24.1714718460794,2.72020091026957));
#229556=CARTESIAN_POINT('Ctrl Pts',(53.9262153118348,24.1739808617162,2.7223062486218));
#229557=CARTESIAN_POINT('Ctrl Pts',(53.9310653428794,24.1829777455763,2.72985561753096));
#229558=CARTESIAN_POINT('Ctrl Pts',(53.9365438157567,24.1913567365396,2.73770089914317));
#229559=CARTESIAN_POINT('Ctrl Pts',(53.9425259106379,24.1991508947534,2.74574823347055));
#229560=CARTESIAN_POINT('Ctrl Pts',(53.9490996319576,24.2077158916377,2.75459144546979));
#229561=CARTESIAN_POINT('Ctrl Pts',(53.9562817849767,24.2155752681661,2.76367911754196));
#229562=CARTESIAN_POINT('Ctrl Pts',(53.9639562340135,24.2227540584919,2.77292162564624));
#229563=CARTESIAN_POINT('Ctrl Pts',(53.9722427129493,24.2305053504132,2.78290121484572));
#229564=CARTESIAN_POINT('Ctrl Pts',(53.9811038680469,24.2374640812918,2.79306229499973));
#229565=CARTESIAN_POINT('Ctrl Pts',(53.9904403792142,24.2436285779114,2.8033191668498));
#229566=CARTESIAN_POINT('Ctrl Pts',(53.9996985666472,24.249741360739,2.81348999408515));
#229567=CARTESIAN_POINT('Ctrl Pts',(54.0094254978895,24.2550737197503,2.82375635966795));
#229568=CARTESIAN_POINT('Ctrl Pts',(54.0195518809641,24.2595822759735,2.83404198860279));
#229569=CARTESIAN_POINT('Origin',(0.00619866644047569,-0.013922432774286,
2.83404198860262));
#229570=CARTESIAN_POINT('Ctrl Pts',(57.4192809246789,25.5480287005721,2.6587819886028));
#229571=CARTESIAN_POINT('Ctrl Pts',(57.4227710771203,25.5401808584724,2.6587819886028));
#229572=CARTESIAN_POINT('Ctrl Pts',(57.4255746438785,25.5321112063512,2.65944603041859));
#229573=CARTESIAN_POINT('Ctrl Pts',(57.4277200319912,25.5239679177318,2.66070439264063));
#229574=CARTESIAN_POINT('Ctrl Pts',(57.4290908328636,25.518764743967,2.6615084261959));
#229575=CARTESIAN_POINT('Ctrl Pts',(57.4301938346425,25.5135317242471,2.66255428265371));
#229576=CARTESIAN_POINT('Ctrl Pts',(57.4310450321041,25.5083079410949,2.6638169970067));
#229577=CARTESIAN_POINT('Ctrl Pts',(57.4322067458449,25.5011785252534,2.66554034873269));
#229578=CARTESIAN_POINT('Ctrl Pts',(57.4328933558607,25.4940667032539,2.66766759643973));
#229579=CARTESIAN_POINT('Ctrl Pts',(57.4331362848728,25.4870628291426,2.67012012783149));
#229580=CARTESIAN_POINT('Ctrl Pts',(57.4332577493788,25.483560892087,2.67134639352736));
#229581=CARTESIAN_POINT('Ctrl Pts',(57.4332683803241,25.4800857520064,2.67265375585012));
#229582=CARTESIAN_POINT('Ctrl Pts',(57.4331727200758,25.4766473428561,2.6740313512694));
#229583=CARTESIAN_POINT('Ctrl Pts',(57.4331248899517,25.4749281382809,2.67472014897904));
#229584=CARTESIAN_POINT('Ctrl Pts',(57.4330504941582,25.4732181005506,2.67542649668632));
#229585=CARTESIAN_POINT('Ctrl Pts',(57.4329501454094,25.4715183716227,2.67614899656101));
#229586=CARTESIAN_POINT('Ctrl Pts',(57.4329250582222,25.4710934393907,2.67632962152968));
#229587=CARTESIAN_POINT('Ctrl Pts',(57.4328983491282,25.4706691511208,2.67651125590949));
#229588=CARTESIAN_POINT('Ctrl Pts',(57.4328700280096,25.4702455239745,2.67669387767523));
#229589=CARTESIAN_POINT('Ctrl Pts',(57.4327850646539,25.4689746425357,2.67724174297243));
#229590=CARTESIAN_POINT('Ctrl Pts',(57.432685592307,25.4677097128937,2.67779849504747));
#229591=CARTESIAN_POINT('Ctrl Pts',(57.4325718846637,25.4664511833529,2.67836353618008));
#229592=CARTESIAN_POINT('Ctrl Pts',(57.4317860942976,25.4577539633647,2.68226832098906));
#229593=CARTESIAN_POINT('Ctrl Pts',(57.4303627559732,25.4493260998451,2.68659153751387));
#229594=CARTESIAN_POINT('Ctrl Pts',(57.4284143577091,25.4412057723282,2.69123699486172));
#229595=CARTESIAN_POINT('Ctrl Pts',(57.42744600912,25.4371699918421,2.69354577441213));
#229596=CARTESIAN_POINT('Ctrl Pts',(57.4263474236138,25.4332098968698,2.69593478828116));
#229597=CARTESIAN_POINT('Ctrl Pts',(57.4251294472437,25.4293290842281,2.6983956526122));
#229598=CARTESIAN_POINT('Ctrl Pts',(57.4224424094497,25.4207674318877,2.70382468689046));
#229599=CARTESIAN_POINT('Ctrl Pts',(57.4191864212928,25.4125888532393,2.70961155815088));
#229600=CARTESIAN_POINT('Ctrl Pts',(57.4154637896041,25.4048965980306,2.71562701361769));
#229601=CARTESIAN_POINT('Ctrl Pts',(57.4141038653033,25.4020865201984,2.71782453535861));
#229602=CARTESIAN_POINT('Ctrl Pts',(57.4126868351396,25.3993352917243,2.72005051502405));
#229603=CARTESIAN_POINT('Ctrl Pts',(57.4112179557371,25.3966436944401,2.72229986760119));
#229604=CARTESIAN_POINT('Ctrl Pts',(57.406284145256,25.3876029039783,2.72985520488885));
#229605=CARTESIAN_POINT('Ctrl Pts',(57.4007266836991,25.379181606956,2.73770845534538));
#229606=CARTESIAN_POINT('Ctrl Pts',(57.3946697603107,25.3713475726778,2.74576706701718));
#229607=CARTESIAN_POINT('Ctrl Pts',(57.3880124840171,25.3627370410037,2.75462443584985));
#229608=CARTESIAN_POINT('Ctrl Pts',(57.3807515434763,25.3548353295672,2.76373036323127));
#229609=CARTESIAN_POINT('Ctrl Pts',(57.3730023605528,25.3476188815044,2.77299664636754));
#229610=CARTESIAN_POINT('Ctrl Pts',(57.364656158518,25.3398464577404,2.78297683033412));
#229611=CARTESIAN_POINT('Ctrl Pts',(57.3557428147462,25.3328680394176,2.79314401478833));
#229612=CARTESIAN_POINT('Ctrl Pts',(57.3463604602054,25.3266878999853,2.80341452427883));
#229613=CARTESIAN_POINT('Ctrl Pts',(57.33710479913,25.3205912133023,2.81354634721327));
#229614=CARTESIAN_POINT('Ctrl Pts',(57.3273913673572,25.3152708796012,2.82378004209189));
#229615=CARTESIAN_POINT('Ctrl Pts',(57.317288315449,25.3107727110825,2.8340419886028));
#229616=CARTESIAN_POINT('Ctrl Pts',(54.1745185419759,23.9115214566117,2.83404198860279));
#229617=CARTESIAN_POINT('Ctrl Pts',(54.164849865839,23.9072166846466,2.8242212644308));
#229618=CARTESIAN_POINT('Ctrl Pts',(54.1548764216408,23.9036899956627,2.8144281502863));
#229619=CARTESIAN_POINT('Ctrl Pts',(54.1446552025556,23.9009524404119,2.80471618166502));
#229620=CARTESIAN_POINT('Ctrl Pts',(54.1347857162263,23.8983090899566,2.79533842146448));
#229621=CARTESIAN_POINT('Ctrl Pts',(54.1246839742788,23.8964012454639,2.78603515650492));
#229622=CARTESIAN_POINT('Ctrl Pts',(54.1143872866766,23.89528251795,2.7768588734704));
#229623=CARTESIAN_POINT('Ctrl Pts',(54.1046536921696,23.8942249700856,2.76818441216881));
#229624=CARTESIAN_POINT('Ctrl Pts',(54.0947449925338,23.8938724934879,2.75962261521947));
#229625=CARTESIAN_POINT('Ctrl Pts',(54.0846948896071,23.8943122764064,2.75123537701999));
#229626=CARTESIAN_POINT('Ctrl Pts',(54.0754389134147,23.8947173090963,2.74351087134468));
#229627=CARTESIAN_POINT('Ctrl Pts',(54.0660624571252,23.8957944255618,2.73593399450204));
#229628=CARTESIAN_POINT('Ctrl Pts',(54.056603339754,23.8976480927549,2.7285765781294));
#229629=CARTESIAN_POINT('Ctrl Pts',(54.0537828218979,23.8982008188933,2.72638274508565));
#229630=CARTESIAN_POINT('Ctrl Pts',(54.0509550659748,23.8988228478381,2.72420861709723));
#229631=CARTESIAN_POINT('Ctrl Pts',(54.0481214021003,23.8995176373646,2.72205663736726));
#229632=CARTESIAN_POINT('Ctrl Pts',(54.0453166912883,23.9002053278541,2.71992664556764));
#229633=CARTESIAN_POINT('Ctrl Pts',(54.042509037702,23.9009633199468,2.71782089927883));
#229634=CARTESIAN_POINT('Ctrl Pts',(54.0397028685176,23.9017938716382,2.71574387311244));
#229635=CARTESIAN_POINT('Ctrl Pts',(54.0395077330006,23.9018516265785,2.71559944077485));
#229636=CARTESIAN_POINT('Ctrl Pts',(54.0393125964104,23.9019097237178,2.71545515216067));
#229637=CARTESIAN_POINT('Ctrl Pts',(54.0391174593312,23.9019681642225,2.71531100781729));
#229638=CARTESIAN_POINT('Ctrl Pts',(54.0305619349333,23.9045304100324,2.7089911917609));
#229639=CARTESIAN_POINT('Ctrl Pts',(54.0220283896864,23.9077916774637,2.70298296066853));
#229640=CARTESIAN_POINT('Ctrl Pts',(54.013624633049,23.9117952627743,2.69736727774157));
#229641=CARTESIAN_POINT('Ctrl Pts',(54.0057908713,23.9155273001022,2.69213248525463));
#229642=CARTESIAN_POINT('Ctrl Pts',(53.9980693056385,23.9199049461651,2.68723866185514));
#229643=CARTESIAN_POINT('Ctrl Pts',(53.9905727747503,23.9249777890345,2.68278595829617));
#229644=CARTESIAN_POINT('Ctrl Pts',(53.9878304467667,23.926833500585,2.68115710172839));
#229645=CARTESIAN_POINT('Ctrl Pts',(53.9851185338205,23.9287823509747,2.67958763637825));
#229646=CARTESIAN_POINT('Ctrl Pts',(53.9824437337507,23.9308270955486,2.67808378645362));
#229647=CARTESIAN_POINT('Ctrl Pts',(53.9818005336912,23.9313187883097,2.67772216078597));
#229648=CARTESIAN_POINT('Ctrl Pts',(53.9811593045604,23.9318165831367,2.6773640360356));
#229649=CARTESIAN_POINT('Ctrl Pts',(53.9805201796371,23.9323204546079,2.67700956934476));
#229650=CARTESIAN_POINT('Ctrl Pts',(53.9799010273677,23.9328085800956,2.67666617973801));
#229651=CARTESIAN_POINT('Ctrl Pts',(53.9792838498571,23.9333024083484,2.67632622314116));
#229652=CARTESIAN_POINT('Ctrl Pts',(53.9786687697971,23.9338019127825,2.6759898415877));
#229653=CARTESIAN_POINT('Ctrl Pts',(53.9719298569081,23.9392745611219,2.67230439292204));
#229654=CARTESIAN_POINT('Ctrl Pts',(53.9654385427822,23.945432475205,2.66904964539947));
#229655=CARTESIAN_POINT('Ctrl Pts',(53.9593734277039,23.9522153560514,2.66640203566691));
#229656=CARTESIAN_POINT('Ctrl Pts',(53.9568580436995,23.9550284189141,2.66530399299418));
#229657=CARTESIAN_POINT('Ctrl Pts',(53.9544158621939,23.9579485624032,2.66430995142248));
#229658=CARTESIAN_POINT('Ctrl Pts',(53.9520587513132,23.9609698772115,2.66343053473357));
#229659=CARTESIAN_POINT('Ctrl Pts',(53.9480384530775,23.9661230444607,2.6619305979288));
#229660=CARTESIAN_POINT('Ctrl Pts',(53.9442681092575,23.9715702598497,2.66076519817123));
#229661=CARTESIAN_POINT('Ctrl Pts',(53.9408121161403,23.9772776109213,2.65997805604455));
#229662=CARTESIAN_POINT('Ctrl Pts',(53.9390841195817,23.980131286457,2.65958448498121));
#229663=CARTESIAN_POINT('Ctrl Pts',(53.9374360035029,23.9830506455188,2.65928526260757));
#229664=CARTESIAN_POINT('Ctrl Pts',(53.9358758804724,23.9860314303859,2.6590846397132));
#229665=CARTESIAN_POINT('Ctrl Pts',(53.934315757442,23.9890122152531,2.65888401681882));
#229666=CARTESIAN_POINT('Ctrl Pts',(53.9328436288553,23.9920543802864,2.65878198860279));
#229667=CARTESIAN_POINT('Ctrl Pts',(53.9314655730804,23.995153256981,2.65878198860279));
#229668=CARTESIAN_POINT('Origin',(50.4502867888875,29.1450842944632,2.83404198860283));
#229669=CARTESIAN_POINT('Ctrl Pts',(54.1671020372438,31.4933613949861,2.83404198860284));
#229670=CARTESIAN_POINT('Ctrl Pts',(54.1762908521541,31.4986665597481,2.82419652440088));
#229671=CARTESIAN_POINT('Ctrl Pts',(54.1858709973828,31.5032309550536,2.81438790575673));
#229672=CARTESIAN_POINT('Ctrl Pts',(54.1957854287838,31.5070391691408,2.80466781256927));
#229673=CARTESIAN_POINT('Ctrl Pts',(54.2053777002009,31.5107236389466,2.79526356453105));
#229674=CARTESIAN_POINT('Ctrl Pts',(54.2152841131313,31.5137006693053,2.7859410249626));
#229675=CARTESIAN_POINT('Ctrl Pts',(54.2254725303159,31.5159144374965,2.77675109088808));
#229676=CARTESIAN_POINT('Ctrl Pts',(54.235110145606,31.5180085258893,2.76805797913714));
#229677=CARTESIAN_POINT('Ctrl Pts',(54.2450010037737,31.5194198476566,2.75948271210195));
#229678=CARTESIAN_POINT('Ctrl Pts',(54.2551207303723,31.5200591406751,2.75108575573259));
#229679=CARTESIAN_POINT('Ctrl Pts',(54.2644417304469,31.5206479757801,2.74335155163306));
#229680=CARTESIAN_POINT('Ctrl Pts',(54.2739574575954,31.5205818213853,2.73576818685979));
#229681=CARTESIAN_POINT('Ctrl Pts',(54.2836415202553,31.5197533892257,2.72840626160534));
#229682=CARTESIAN_POINT('Ctrl Pts',(54.2864504987137,31.5195130925472,2.72627084693712));
#229683=CARTESIAN_POINT('Ctrl Pts',(54.289273561557,31.5192084034332,2.7241542458755));
#229684=CARTESIAN_POINT('Ctrl Pts',(54.292109835428,31.5188360425581,2.7220586717328));
#229685=CARTESIAN_POINT('Ctrl Pts',(54.2951845386601,31.5184323794288,2.71978693462884));
#229686=CARTESIAN_POINT('Ctrl Pts',(54.2982706300314,31.5179508191006,2.71754411340784));
#229687=CARTESIAN_POINT('Ctrl Pts',(54.3013662138033,31.5173878381078,2.71533341844281));
#229688=CARTESIAN_POINT('Ctrl Pts',(54.3098620677559,31.5158427323553,2.70926614876428));
#229689=CARTESIAN_POINT('Ctrl Pts',(54.3184108612912,31.5136439393734,2.70347381860445));
#229690=CARTESIAN_POINT('Ctrl Pts',(54.3269129314607,31.5107627835359,2.69804914171431));
#229691=CARTESIAN_POINT('Ctrl Pts',(54.3346918640778,31.5081266823661,2.6930858568723));
#229692=CARTESIAN_POINT('Ctrl Pts',(54.3424218244385,31.5049132975211,2.68842799053201));
#229693=CARTESIAN_POINT('Ctrl Pts',(54.3500333719156,31.5010675328657,2.68414767054226));
#229694=CARTESIAN_POINT('Ctrl Pts',(54.3537721391719,31.4991785058298,2.6820451913457));
#229695=CARTESIAN_POINT('Ctrl Pts',(54.3574819590039,31.4971365594546,2.6800343177853));
#229696=CARTESIAN_POINT('Ctrl Pts',(54.3611518569451,31.4949332463336,2.67812693945288));
#229697=CARTESIAN_POINT('Ctrl Pts',(54.3618481843342,31.4945151891294,2.6777650329924));
#229698=CARTESIAN_POINT('Ctrl Pts',(54.3625432124817,31.494090808751,2.6774065963996));
#229699=CARTESIAN_POINT('Ctrl Pts',(54.3632368016453,31.4936601139564,2.67705178968892));
#229700=CARTESIAN_POINT('Ctrl Pts',(54.3639087161475,31.4932428783741,2.67670807068794));
#229701=CARTESIAN_POINT('Ctrl Pts',(54.3645792801848,31.4928197168825,2.67636775825302));
#229702=CARTESIAN_POINT('Ctrl Pts',(54.3652483648081,31.4923906407828,2.67603099699292));
#229703=CARTESIAN_POINT('Ctrl Pts',(54.372539911164,31.4877146578622,2.67236104217175));
#229704=CARTESIAN_POINT('Ctrl Pts',(54.3796603393079,31.4823328301627,2.66911440541529));
#229705=CARTESIAN_POINT('Ctrl Pts',(54.3864229856955,31.4762829888805,2.6664677818969));
#229706=CARTESIAN_POINT('Ctrl Pts',(54.3892788932593,31.473728103339,2.66535009635024));
#229707=CARTESIAN_POINT('Ctrl Pts',(54.3920710496176,31.4710545157391,2.66433897912386));
#229708=CARTESIAN_POINT('Ctrl Pts',(54.3947861357355,31.4682668669588,2.66344564884829));
#229709=CARTESIAN_POINT('Ctrl Pts',(54.3993582729152,31.4635725360689,2.66194130298621));
#229710=CARTESIAN_POINT('Ctrl Pts',(54.4037093249067,31.4585547584353,2.66077206705456));
#229711=CARTESIAN_POINT('Ctrl Pts',(54.4077698566065,31.4532397415957,2.6599822515575));
#229712=CARTESIAN_POINT('Ctrl Pts',(54.4087849895314,31.4519109873858,2.65978479768323));
#229713=CARTESIAN_POINT('Ctrl Pts',(54.4097817701143,31.4505635261659,2.65961098966658));
#229714=CARTESIAN_POINT('Ctrl Pts',(54.4107588499958,31.449197606926,2.65946139030537));
#229715=CARTESIAN_POINT('Ctrl Pts',(54.4122244698182,31.4471487280663,2.65923699126355));
#229716=CARTESIAN_POINT('Ctrl Pts',(54.4136457436054,31.445058325466,2.65906707562477));
#229717=CARTESIAN_POINT('Ctrl Pts',(54.4150195646481,31.442928094411,2.65895332562955));
#229718=CARTESIAN_POINT('Ctrl Pts',(54.4163933856907,31.4407978633561,2.65883957563432));
#229719=CARTESIAN_POINT('Ctrl Pts',(54.4177197583729,31.4386278145921,2.65878198860284));
#229720=CARTESIAN_POINT('Ctrl Pts',(54.4189959163063,31.4364195775137,2.65878198860284));
#229721=CARTESIAN_POINT('Ctrl Pts',(51.1126068659047,29.5274749692187,2.65878198860283));
#229722=CARTESIAN_POINT('Ctrl Pts',(51.108288538813,29.5349468458349,2.65878198860283));
#229723=CARTESIAN_POINT('Ctrl Pts',(51.1046244142386,29.5427104181385,2.65945335517877));
#229724=CARTESIAN_POINT('Ctrl Pts',(51.1016049255946,29.5506148782563,2.66072561226624));
#229725=CARTESIAN_POINT('Ctrl Pts',(51.099654645748,29.555720348448,2.66154735980362));
#229726=CARTESIAN_POINT('Ctrl Pts',(51.0979724198487,29.5608842707087,2.66261895766906));
#229727=CARTESIAN_POINT('Ctrl Pts',(51.0965469289497,29.5660646037407,2.6639142925105));
#229728=CARTESIAN_POINT('Ctrl Pts',(51.0946575224202,29.5729308384267,2.66563118464146));
#229729=CARTESIAN_POINT('Ctrl Pts',(51.0932249325813,29.579826275578,2.66774105138722));
#229730=CARTESIAN_POINT('Ctrl Pts',(51.0922302752234,29.5866628504239,2.67016894181773));
#229731=CARTESIAN_POINT('Ctrl Pts',(51.0917329465445,29.5900811378468,2.67138288703299));
#229732=CARTESIAN_POINT('Ctrl Pts',(51.0913449998289,29.5934848814075,2.67267613167574));
#229733=CARTESIAN_POINT('Ctrl Pts',(51.0910633609953,29.5968642938812,2.67403835432576));
#229734=CARTESIAN_POINT('Ctrl Pts',(51.0909225415785,29.598554000118,2.67471946565077));
#229735=CARTESIAN_POINT('Ctrl Pts',(51.0908082908743,29.6002376377884,2.67541781389546));
#229736=CARTESIAN_POINT('Ctrl Pts',(51.0907201726671,29.6019140726117,2.67613207244193));
#229737=CARTESIAN_POINT('Ctrl Pts',(51.0906981431153,29.6023331813176,2.67631063707854));
#229738=CARTESIAN_POINT('Ctrl Pts',(51.090677746668,29.6027518401471,2.67649019601869));
#229739=CARTESIAN_POINT('Ctrl Pts',(51.090658976153,29.6031700319853,2.6766707283668));
#229740=CARTESIAN_POINT('Ctrl Pts',(51.0906026646081,29.6044246074998,2.67721232541114));
#229741=CARTESIAN_POINT('Ctrl Pts',(51.0905609873413,29.6056749785905,2.6777626834007));
#229742=CARTESIAN_POINT('Ctrl Pts',(51.090533742783,29.6069206965766,2.67832123541539));
#229743=CARTESIAN_POINT('Ctrl Pts',(51.0903418356317,29.6156953732193,2.68225560368463));
#229744=CARTESIAN_POINT('Ctrl Pts',(51.0908211368931,29.6242688491604,2.686617929989));
#229745=CARTESIAN_POINT('Ctrl Pts',(51.091864142426,29.6325885911856,2.69130986622583));
#229746=CARTESIAN_POINT('Ctrl Pts',(51.0923699989825,29.6366236570776,2.69358545023065));
#229747=CARTESIAN_POINT('Ctrl Pts',(51.0930089302516,29.6405993642577,2.69593918853486));
#229748=CARTESIAN_POINT('Ctrl Pts',(51.0937712117414,29.6445110377127,2.69836306235497));
#229749=CARTESIAN_POINT('Ctrl Pts',(51.0949382114433,29.6504995364713,2.7020738438223));
#229750=CARTESIAN_POINT('Ctrl Pts',(51.0963926103116,29.6563348640822,2.7059476081423));
#229751=CARTESIAN_POINT('Ctrl Pts',(51.098099028059,29.6619874481817,2.7099519634571));
#229752=CARTESIAN_POINT('Ctrl Pts',(51.0988914972888,29.6646125374801,2.71181160678108));
#229753=CARTESIAN_POINT('Ctrl Pts',(51.0997380650833,29.6671982043429,2.71369962772101));
#229754=CARTESIAN_POINT('Ctrl Pts',(51.1006362623629,29.6697408831278,2.71561183138664));
#229755=CARTESIAN_POINT('Ctrl Pts',(51.1007051056453,29.669935769438,2.71575839426314));
#229756=CARTESIAN_POINT('Ctrl Pts',(51.100774227025,29.6701304259133,2.71590508903212));
#229757=CARTESIAN_POINT('Ctrl Pts',(51.1008436251324,29.6703248520471,2.71605191409914));
#229758=CARTESIAN_POINT('Ctrl Pts',(51.1018184593124,29.6730559530502,2.71811436362756));
#229759=CARTESIAN_POINT('Ctrl Pts',(51.1028499068178,29.675741029822,2.72020091026962));
#229760=CARTESIAN_POINT('Ctrl Pts',(51.1039327914267,29.6783776815771,2.72230624862184));
#229761=CARTESIAN_POINT('Ctrl Pts',(51.1078158230499,29.6878322458583,2.72985561753126));
#229762=CARTESIAN_POINT('Ctrl Pts',(51.1123884412305,29.6967379921835,2.73770089914375));
#229763=CARTESIAN_POINT('Ctrl Pts',(51.1175230541897,29.7051147523685,2.74574823347141));
#229764=CARTESIAN_POINT('Ctrl Pts',(51.1231654780142,29.7143199702913,2.75459144547089));
#229765=CARTESIAN_POINT('Ctrl Pts',(51.129486757897,29.722887031751,2.76367911754332));
#229766=CARTESIAN_POINT('Ctrl Pts',(51.1363687775784,29.7308286942766,2.77292162564785));
#229767=CARTESIAN_POINT('Ctrl Pts',(51.1437996316828,29.7394036967188,2.7829012148475));
#229768=CARTESIAN_POINT('Ctrl Pts',(51.1518848590008,29.7472505498668,2.79306229500166));
#229769=CARTESIAN_POINT('Ctrl Pts',(51.1605258584248,29.7543572078934,2.8033191668519));
#229770=CARTESIAN_POINT('Ctrl Pts',(51.1690943687425,29.7614042483616,2.81348999408657));
#229771=CARTESIAN_POINT('Ctrl Pts',(51.1782106315441,29.7677241373269,2.82375635966868));
#229772=CARTESIAN_POINT('Ctrl Pts',(51.1878102687784,29.7732664904682,2.83404198860283));
#229773=CARTESIAN_POINT('Origin',(0.00762000000000077,-0.0131982271534882,
2.83404198860262));
#229774=CARTESIAN_POINT('Ctrl Pts',(54.4342359163063,31.4100231232064,2.65878198860284));
#229775=CARTESIAN_POINT('Ctrl Pts',(54.4385272722025,31.4025830926773,2.65878198860284));
#229776=CARTESIAN_POINT('Ctrl Pts',(54.4421589890644,31.3948506994788,2.65944603041879));
#229777=CARTESIAN_POINT('Ctrl Pts',(54.4451438299621,31.3869762747681,2.6607043926411));
#229778=CARTESIAN_POINT('Ctrl Pts',(54.4470510012012,31.3819448922431,2.66150842619633));
#229779=CARTESIAN_POINT('Ctrl Pts',(54.4486949601302,31.3768558346346,2.66255428265399));
#229780=CARTESIAN_POINT('Ctrl Pts',(54.4500875286681,31.3717496422766,2.66381699700677));
#229781=CARTESIAN_POINT('Ctrl Pts',(54.4519881053013,31.3647807142731,2.66554034873277));
#229782=CARTESIAN_POINT('Ctrl Pts',(54.4534143418203,31.3577796218684,2.66766759643982));
#229783=CARTESIAN_POINT('Ctrl Pts',(54.4543880442396,31.3508395087087,2.67012012783158));
#229784=CARTESIAN_POINT('Ctrl Pts',(54.4548748954493,31.3473694521289,2.67134639352746));
#229785=CARTESIAN_POINT('Ctrl Pts',(54.4552487192094,31.3439144604656,2.67265375585022));
#229786=CARTESIAN_POINT('Ctrl Pts',(54.4555129946225,31.3404848880616,2.67403135126949));
#229787=CARTESIAN_POINT('Ctrl Pts',(54.4556451323291,31.3387701018596,2.67472014897913));
#229788=CARTESIAN_POINT('Ctrl Pts',(54.4557498916996,31.337061655417,2.67542649668642));
#229789=CARTESIAN_POINT('Ctrl Pts',(54.4558277627246,31.3353607484814,2.67614899656111));
#229790=CARTESIAN_POINT('Ctrl Pts',(54.4558472304809,31.3349355217475,2.67632962152979));
#229791=CARTESIAN_POINT('Ctrl Pts',(54.4558650179028,31.3345107659126,2.6765112559096));
#229792=CARTESIAN_POINT('Ctrl Pts',(54.4558811330249,31.3340864990772,2.67669387767533));
#229793=CARTESIAN_POINT('Ctrl Pts',(54.4559294783911,31.3328136985709,2.67724174297253));
#229794=CARTESIAN_POINT('Ctrl Pts',(54.4559627721159,31.3315453006542,2.67779849504757));
#229795=CARTESIAN_POINT('Ctrl Pts',(54.4559812395338,31.3302817797847,2.67836353618018));
#229796=CARTESIAN_POINT('Ctrl Pts',(54.4561088608496,31.321550066618,2.68226832098923));
#229797=CARTESIAN_POINT('Ctrl Pts',(54.4555742713438,31.3130195924487,2.68659153751413));
#229798=CARTESIAN_POINT('Ctrl Pts',(54.4544853519657,31.3047400858591,2.69123699486207));
#229799=CARTESIAN_POINT('Ctrl Pts',(54.4539441620239,31.3006251938109,2.69354577441238));
#229800=CARTESIAN_POINT('Ctrl Pts',(54.4532655373259,31.2965719591987,2.69593478828131));
#229801=CARTESIAN_POINT('Ctrl Pts',(54.4524598885395,31.2925850928565,2.69839565261226));
#229802=CARTESIAN_POINT('Ctrl Pts',(54.4506825069818,31.2837894702121,2.70382468689051));
#229803=CARTESIAN_POINT('Ctrl Pts',(54.4482992497266,31.2753153512349,2.70961155815092));
#229804=CARTESIAN_POINT('Ctrl Pts',(54.4454010706198,31.2672761140353,2.71562701361772));
#229805=CARTESIAN_POINT('Ctrl Pts',(54.444342329244,31.2643392793061,2.71782453535862));
#229806=CARTESIAN_POINT('Ctrl Pts',(54.4432206434043,31.2614550023641,2.72005051502406));
#229807=CARTESIAN_POINT('Ctrl Pts',(54.4420411592047,31.2586246102248,2.72229986760119));
#229808=CARTESIAN_POINT('Ctrl Pts',(54.4380793965872,31.2491176225312,2.729855204889));
#229809=CARTESIAN_POINT('Ctrl Pts',(54.4334326446224,31.2401615453387,2.73770845534573));
#229810=CARTESIAN_POINT('Ctrl Pts',(54.4282277812583,31.231737305826,2.74576706701775));
#229811=CARTESIAN_POINT('Ctrl Pts',(54.4225070198645,31.2224780686847,2.7546244358506));
#229812=CARTESIAN_POINT('Ctrl Pts',(54.4161118092692,31.2138606686935,2.76373036323222));
#229813=CARTESIAN_POINT('Ctrl Pts',(54.4091594014068,31.2058737429056,2.7729966463687));
#229814=CARTESIAN_POINT('Ctrl Pts',(54.4016713602519,31.1972714816195,2.78297683033537));
#229815=CARTESIAN_POINT('Ctrl Pts',(54.3935362880533,31.1893995936754,2.79314401478967));
#229816=CARTESIAN_POINT('Ctrl Pts',(54.3848513315099,31.1822725865916,2.80341452428021));
#229817=CARTESIAN_POINT('Ctrl Pts',(54.3762836512046,31.1752418181678,2.81354634721425));
#229818=CARTESIAN_POINT('Ctrl Pts',(54.3671795569335,31.1689352997153,2.82378004209244));
#229819=CARTESIAN_POINT('Ctrl Pts',(54.3576020372438,31.1634057161443,2.83404198860284));
#229820=CARTESIAN_POINT('Ctrl Pts',(51.3783102687784,29.4433108116264,2.83404198860283));
#229821=CARTESIAN_POINT('Ctrl Pts',(51.3691445298587,29.4380189697937,2.82422126443021));
#229822=CARTESIAN_POINT('Ctrl Pts',(51.3595943606106,29.4334690915853,2.81442815028509));
#229823=CARTESIAN_POINT('Ctrl Pts',(51.3497152868758,29.4296781246248,2.80471618166319));
#229824=CARTESIAN_POINT('Ctrl Pts',(51.3401761719858,29.4260176124805,2.79533842146225));
#229825=CARTESIAN_POINT('Ctrl Pts',(51.3303291924903,29.4230642997975,2.78603515650231));
#229826=CARTESIAN_POINT('Ctrl Pts',(51.3202058500874,29.4208754038582,2.77685887346742));
#229827=CARTESIAN_POINT('Ctrl Pts',(51.3106361210823,29.4188062116758,2.76818441216558));
#229828=CARTESIAN_POINT('Ctrl Pts',(51.3008185461766,29.4174199248361,2.75962261521601));
#229829=CARTESIAN_POINT('Ctrl Pts',(51.2907775289323,29.4168067767633,2.75123537701632));
#229830=CARTESIAN_POINT('Ctrl Pts',(51.2815299205009,29.4162420776746,2.74351087134085));
#229831=CARTESIAN_POINT('Ctrl Pts',(51.2720922400908,29.4163331870168,2.73593399449808));
#229832=CARTESIAN_POINT('Ctrl Pts',(51.2624911797709,29.4171879526247,2.72857657812533));
#229833=CARTESIAN_POINT('Ctrl Pts',(51.2596283373946,29.4174428264742,2.72638274508297));
#229834=CARTESIAN_POINT('Ctrl Pts',(51.2567510524865,29.4177658668981,2.72420861709592));
#229835=CARTESIAN_POINT('Ctrl Pts',(51.2538602864394,29.4181606517644,2.72205663736729));
#229836=CARTESIAN_POINT('Ctrl Pts',(51.2509990568967,29.4185514029024,2.71992664556768));
#229837=CARTESIAN_POINT('Ctrl Pts',(51.2481275521819,29.4190117629204,2.71782089927886));
#229838=CARTESIAN_POINT('Ctrl Pts',(51.245249939194,29.4195444402102,2.71574387311248));
#229839=CARTESIAN_POINT('Ctrl Pts',(51.2450498356145,29.4195814815471,2.71559944077488));
#229840=CARTESIAN_POINT('Ctrl Pts',(51.2448496951983,29.4196188630963,2.71545515216071));
#229841=CARTESIAN_POINT('Ctrl Pts',(51.2446495184043,29.4196565860788,2.71531100781732));
#229842=CARTESIAN_POINT('Ctrl Pts',(51.2358730344471,29.4213104998204,2.70899119176083));
#229843=CARTESIAN_POINT('Ctrl Pts',(51.2270453415808,29.4236619033166,2.70298296066837));
#229844=CARTESIAN_POINT('Ctrl Pts',(51.2182691329814,29.426765124801,2.69736727774133));
#229845=CARTESIAN_POINT('Ctrl Pts',(51.210088181272,29.4296578665608,2.69213248525424));
#229846=CARTESIAN_POINT('Ctrl Pts',(51.2019513265391,29.4332044080281,2.68723866185463));
#229847=CARTESIAN_POINT('Ctrl Pts',(51.1939656059618,29.4374658604801,2.68278595829557));
#229848=CARTESIAN_POINT('Ctrl Pts',(51.1910443260615,29.4390247549185,2.68115710172801));
#229849=CARTESIAN_POINT('Ctrl Pts',(51.1881435589221,29.4406794572088,2.67958763637807));
#229850=CARTESIAN_POINT('Ctrl Pts',(51.1852696776793,29.442433407717,2.67808378645363));
#229851=CARTESIAN_POINT('Ctrl Pts',(51.1845786052483,29.4428551742199,2.67772216078598));
#229852=CARTESIAN_POINT('Ctrl Pts',(51.1838888551095,29.443283215379,2.67736403603562));
#229853=CARTESIAN_POINT('Ctrl Pts',(51.1832005624688,29.4437175198436,2.67700956934477));
#229854=CARTESIAN_POINT('Ctrl Pts',(51.1825337789732,29.4441382522936,2.67666617973802));
#229855=CARTESIAN_POINT('Ctrl Pts',(51.1818683633172,29.4445648626868,2.67632622314117));
#229856=CARTESIAN_POINT('Ctrl Pts',(51.1812044402993,29.4449973374098,2.67598984158772));
#229857=CARTESIAN_POINT('Ctrl Pts',(51.1739303963595,29.4497355978005,2.67230439292217));
#229858=CARTESIAN_POINT('Ctrl Pts',(51.1668309650358,29.4551812510956,2.66904964539969));
#229859=CARTESIAN_POINT('Ctrl Pts',(51.1600900711812,29.4612929974521,2.66640203566718));
#229860=CARTESIAN_POINT('Ctrl Pts',(51.1572944215753,29.4638277208377,2.66530399299435));
#229861=CARTESIAN_POINT('Ctrl Pts',(51.1545603804838,29.4664765899956,2.66430995142256));
#229862=CARTESIAN_POINT('Ctrl Pts',(51.151900368709,29.4692349685474,2.66343053473359));
#229863=CARTESIAN_POINT('Ctrl Pts',(51.1473634414341,29.4739396706108,2.66193059792883));
#229864=CARTESIAN_POINT('Ctrl Pts',(51.1430443628984,29.4789629373384,2.66076519817126));
#229865=CARTESIAN_POINT('Ctrl Pts',(51.1390107214364,29.4842777732942,2.65997805604459));
#229866=CARTESIAN_POINT('Ctrl Pts',(51.1369939007054,29.486935191272,2.65958448498125));
#229867=CARTESIAN_POINT('Ctrl Pts',(51.1350496570625,29.4896662827383,2.65928526260761));
#229868=CARTESIAN_POINT('Ctrl Pts',(51.1331865036877,29.4924676612912,2.65908463971323));
#229869=CARTESIAN_POINT('Ctrl Pts',(51.1313233503128,29.495269039844,2.65888401681885));
#229870=CARTESIAN_POINT('Ctrl Pts',(51.1295412933646,29.49814066024,2.65878198860283));
#229871=CARTESIAN_POINT('Ctrl Pts',(51.1278468659047,29.5010785149114,2.65878198860283));
#229872=CARTESIAN_POINT('Origin',(47.1274239660509,34.2589154226524,2.83404198860286));
#229873=CARTESIAN_POINT('Ctrl Pts',(50.5784163149356,36.9828414016749,2.83404198860288));
#229874=CARTESIAN_POINT('Ctrl Pts',(50.5870002518361,36.9890779968908,2.82419652440103));
#229875=CARTESIAN_POINT('Ctrl Pts',(50.5960508067995,36.9946187858197,2.81438790575704));
#229876=CARTESIAN_POINT('Ctrl Pts',(50.6055128591414,36.99944247839,2.80466781256976));
#229877=CARTESIAN_POINT('Ctrl Pts',(50.614667451125,37.0041094296751,2.7952635645317));
#229878=CARTESIAN_POINT('Ctrl Pts',(50.6242084112801,37.0081056536701,2.78594102496345));
#229879=CARTESIAN_POINT('Ctrl Pts',(50.6341096134621,37.0113722741989,2.77675109088912));
#229880=CARTESIAN_POINT('Ctrl Pts',(50.6434755410454,37.0144622960723,2.76805797913836));
#229881=CARTESIAN_POINT('Ctrl Pts',(50.6531646927615,37.016899762676,2.75948271210336));
#229882=CARTESIAN_POINT('Ctrl Pts',(50.6631621581219,37.0185933530506,2.75108575573417));
#229883=CARTESIAN_POINT('Ctrl Pts',(50.6723705467539,37.0201532722693,2.74335155163484));
#229884=CARTESIAN_POINT('Ctrl Pts',(50.6818410607704,37.021082144611,2.73576818686177));
#229885=CARTESIAN_POINT('Ctrl Pts',(50.6915586678622,37.0212705108776,2.72840626160748));
#229886=CARTESIAN_POINT('Ctrl Pts',(50.6943773762862,37.0213251487712,2.72627084693853));
#229887=CARTESIAN_POINT('Ctrl Pts',(50.6972168227816,37.0213172191968,2.7241542458762));
#229888=CARTESIAN_POINT('Ctrl Pts',(50.7000764815586,37.0212433695026,2.72205867173281));
#229889=CARTESIAN_POINT('Ctrl Pts',(50.7031765355313,37.0211633116861,2.71978693462885));
#229890=CARTESIAN_POINT('Ctrl Pts',(50.7062960577322,37.0210069737843,2.71754411340786));
#229891=CARTESIAN_POINT('Ctrl Pts',(50.7094335311104,37.0207706534748,2.71533341844283));
#229892=CARTESIAN_POINT('Ctrl Pts',(50.718044351416,37.0201220705311,2.70926614876431));
#229893=CARTESIAN_POINT('Ctrl Pts',(50.7267761502172,37.0188289150183,2.70347381860448));
#229894=CARTESIAN_POINT('Ctrl Pts',(50.7355328079489,37.0168522507833,2.69804914171435));
#229895=CARTESIAN_POINT('Ctrl Pts',(50.7435446743633,37.015043710324,2.69308585687253));
#229896=CARTESIAN_POINT('Ctrl Pts',(50.7515681793718,37.0126559296151,2.68842799053241));
#229897=CARTESIAN_POINT('Ctrl Pts',(50.7595400218646,37.0096268558219,2.68414767054279));
#229898=CARTESIAN_POINT('Ctrl Pts',(50.7634557648561,37.0081389846695,2.68204519134607));
#229899=CARTESIAN_POINT('Ctrl Pts',(50.7673587034238,37.0064960060561,2.68003431778552));
#229900=CARTESIAN_POINT('Ctrl Pts',(50.771238806215,37.0046883717069,2.67812693945297));
#229901=CARTESIAN_POINT('Ctrl Pts',(50.7719750179269,37.0043453906958,2.67776503299249));
#229902=CARTESIAN_POINT('Ctrl Pts',(50.7727105984664,37.0039959853417,2.67740659639969));
#229903=CARTESIAN_POINT('Ctrl Pts',(50.7734454079409,37.0036401497476,2.677051789689));
#229904=CARTESIAN_POINT('Ctrl Pts',(50.7741572546194,37.0032954340158,2.67670807068803));
#229905=CARTESIAN_POINT('Ctrl Pts',(50.7748683776572,37.0029446836755,2.67636775825311));
#229906=CARTESIAN_POINT('Ctrl Pts',(50.7755786476302,37.0025878964871,2.67603099699301));
#229907=CARTESIAN_POINT('Ctrl Pts',(50.7833190234415,36.9986997032255,2.67236104217173));
#229908=CARTESIAN_POINT('Ctrl Pts',(50.7909629993143,36.9940916451527,2.66911440541517));
#229909=CARTESIAN_POINT('Ctrl Pts',(50.7983209798299,36.9887818345683,2.66646778189672));
#229910=CARTESIAN_POINT('Ctrl Pts',(50.8014283006924,36.9865394685862,2.66535009635016));
#229911=CARTESIAN_POINT('Ctrl Pts',(50.804484627329,36.9841723869924,2.66433897912387));
#229912=CARTESIAN_POINT('Ctrl Pts',(50.807476228564,36.9816838130236,2.66344564884836));
#229913=CARTESIAN_POINT('Ctrl Pts',(50.8125140102918,36.9774931166428,2.66194130298628));
#229914=CARTESIAN_POINT('Ctrl Pts',(50.8173657273503,36.9729576356983,2.66077206705461));
#229915=CARTESIAN_POINT('Ctrl Pts',(50.8219595855751,36.9680961762157,2.65998225155755));
#229916=CARTESIAN_POINT('Ctrl Pts',(50.8231080501312,36.966880811345,2.65978479768328));
#229917=CARTESIAN_POINT('Ctrl Pts',(50.8242402182964,36.9656449236012,2.65961098966662));
#229918=CARTESIAN_POINT('Ctrl Pts',(50.8253547230712,36.9643886196684,2.65946139030541));
#229919=CARTESIAN_POINT('Ctrl Pts',(50.8270264802334,36.9625041637692,2.6592369912636));
#229920=CARTESIAN_POINT('Ctrl Pts',(50.8286584747055,36.9605737761779,2.65906707562481));
#229921=CARTESIAN_POINT('Ctrl Pts',(50.8302474395914,36.9585988181539,2.65895332562959));
#229922=CARTESIAN_POINT('Ctrl Pts',(50.8318364044772,36.95662386013,2.65883957563436));
#229923=CARTESIAN_POINT('Ctrl Pts',(50.8333823430135,36.9546043428184,2.65878198860288));
#229924=CARTESIAN_POINT('Ctrl Pts',(50.8348823336486,36.9525415975215,2.65878198860288));
#229925=CARTESIAN_POINT('Ctrl Pts',(47.7461450747864,34.7084426211234,2.65878198860287));
#229926=CARTESIAN_POINT('Ctrl Pts',(47.7410693801618,34.715422177923,2.65878198860287));
#229927=CARTESIAN_POINT('Ctrl Pts',(47.7366138137628,34.7227602152544,2.65945335517884));
#229928=CARTESIAN_POINT('Ctrl Pts',(47.7327846251244,34.7303057514051,2.66072561226636));
#229929=CARTESIAN_POINT('Ctrl Pts',(47.7303113621616,34.7351793935413,2.66154735980373));
#229930=CARTESIAN_POINT('Ctrl Pts',(47.7280985748135,34.7401391868073,2.66261895766913));
#229931=CARTESIAN_POINT('Ctrl Pts',(47.7261394006518,34.7451421370596,2.66391429251051));
#229932=CARTESIAN_POINT('Ctrl Pts',(47.7235426275288,34.7517732610326,2.66563118464148));
#229933=CARTESIAN_POINT('Ctrl Pts',(47.721397116118,34.7584811778434,2.66774105138723));
#229934=CARTESIAN_POINT('Ctrl Pts',(47.7196932909345,34.7651763312118,2.67016894181774));
#229935=CARTESIAN_POINT('Ctrl Pts',(47.7188413783428,34.768523907896,2.671382887033));
#229936=CARTESIAN_POINT('Ctrl Pts',(47.7180997687562,34.7718684539193,2.67267613167576));
#229937=CARTESIAN_POINT('Ctrl Pts',(47.7174664279769,34.7751999143434,2.67403835432578));
#229938=CARTESIAN_POINT('Ctrl Pts',(47.7171497575873,34.7768656445554,2.67471946565078));
#229939=CARTESIAN_POINT('Ctrl Pts',(47.716860144702,34.778528116632,2.67541781389548));
#229940=CARTESIAN_POINT('Ctrl Pts',(47.7165972740597,34.7801861569092,2.67613207244195));
#229941=CARTESIAN_POINT('Ctrl Pts',(47.7165315563991,34.7806006669785,2.67631063707856));
#229942=CARTESIAN_POINT('Ctrl Pts',(47.7164675099217,34.7810149003419,2.67649019601871));
#229943=CARTESIAN_POINT('Ctrl Pts',(47.7164051292834,34.7814288392283,2.67667072836682));
#229944=CARTESIAN_POINT('Ctrl Pts',(47.7162179873684,34.7826706558876,2.67721232541116));
#229945=CARTESIAN_POINT('Ctrl Pts',(47.7160458390454,34.783909820854,2.67776268340072));
#229946=CARTESIAN_POINT('Ctrl Pts',(47.7158885307488,34.7851458668349,2.67832123541541));
#229947=CARTESIAN_POINT('Ctrl Pts',(47.7147804714199,34.7938524151214,2.68225560368475));
#229948=CARTESIAN_POINT('Ctrl Pts',(47.7143609747538,34.8024290252888,2.68661792998926));
#229949=CARTESIAN_POINT('Ctrl Pts',(47.7145286167447,34.8108122146624,2.69130986622623));
#229950=CARTESIAN_POINT('Ctrl Pts',(47.7146099229291,34.8148780524495,2.69358545023094));
#229951=CARTESIAN_POINT('Ctrl Pts',(47.7148297795039,34.8188987667931,2.69593918853502));
#229952=CARTESIAN_POINT('Ctrl Pts',(47.7151790039209,34.8228686918041,2.698363062355));
#229953=CARTESIAN_POINT('Ctrl Pts',(47.7157136421038,34.8289463696255,2.70207384382233));
#229954=CARTESIAN_POINT('Ctrl Pts',(47.7165501157951,34.8349017567798,2.70594760814235));
#229955=CARTESIAN_POINT('Ctrl Pts',(47.7176563296781,34.840701744657,2.70995196345714));
#229956=CARTESIAN_POINT('Ctrl Pts',(47.7181700611282,34.8433952890323,2.71181160678112));
#229957=CARTESIAN_POINT('Ctrl Pts',(47.7187417155521,34.8460552817721,2.71369962772105));
#229958=CARTESIAN_POINT('Ctrl Pts',(47.719369210107,34.8486779186779,2.71561183138667));
#229959=CARTESIAN_POINT('Ctrl Pts',(47.7194173050922,34.848878933463,2.71575839426318));
#229960=CARTESIAN_POINT('Ctrl Pts',(47.7194657006756,34.8490797487414,2.71590508903215));
#229961=CARTESIAN_POINT('Ctrl Pts',(47.7195143955479,34.849280363866,2.71605191409917));
#229962=CARTESIAN_POINT('Ctrl Pts',(47.7201984116934,34.8520984015308,2.71811436362759));
#229963=CARTESIAN_POINT('Ctrl Pts',(47.7209435418727,34.8548765847938,2.72020091026965));
#229964=CARTESIAN_POINT('Ctrl Pts',(47.7217448891703,34.8576119849588,2.72230624862188));
#229965=CARTESIAN_POINT('Ctrl Pts',(47.7246183780645,34.8674206434754,2.72985561753082));
#229966=CARTESIAN_POINT('Ctrl Pts',(47.7282350429865,34.8767555719414,2.7377008991428));
#229967=CARTESIAN_POINT('Ctrl Pts',(47.732465918129,34.8856231565591,2.74574823346993));
#229968=CARTESIAN_POINT('Ctrl Pts',(47.7371152248816,34.8953677412261,2.75459144546899));
#229969=CARTESIAN_POINT('Ctrl Pts',(47.7425063743624,34.9045486250985,2.76367911754097));
#229970=CARTESIAN_POINT('Ctrl Pts',(47.7485205638399,34.9131661493071,2.77292162564506));
#229971=CARTESIAN_POINT('Ctrl Pts',(47.7550143791199,34.9224709127488,2.7829012148444));
#229972=CARTESIAN_POINT('Ctrl Pts',(47.7622350952152,34.9311199164008,2.79306229499825));
#229973=CARTESIAN_POINT('Ctrl Pts',(47.7700859102974,34.9390908738021,2.80331916684818));
#229974=CARTESIAN_POINT('Ctrl Pts',(47.7778708651092,34.9469949630624,2.81348999408409));
#229975=CARTESIAN_POINT('Ctrl Pts',(47.7862765797887,34.954233139957,2.82375635966745));
#229976=CARTESIAN_POINT('Ctrl Pts',(47.7952442955502,34.9607485668368,2.83404198860287));
#229977=CARTESIAN_POINT('Origin',(0.00895784724493838,-0.012329418994088,
2.83404198860262));
#229978=CARTESIAN_POINT('Ctrl Pts',(50.8527980281385,36.9278827595329,2.65878198860288));
#229979=CARTESIAN_POINT('Ctrl Pts',(50.8578435704956,36.9209320551072,2.65878198860288));
#229980=CARTESIAN_POINT('Ctrl Pts',(50.8622636476106,36.9136216385509,2.65944603041873));
#229981=CARTESIAN_POINT('Ctrl Pts',(50.8660552387515,36.9061023515954,2.66070439264086));
#229982=CARTESIAN_POINT('Ctrl Pts',(50.8684778849907,36.9012978851886,2.66150842619611));
#229983=CARTESIAN_POINT('Ctrl Pts',(50.8706447895123,36.8964085464701,2.66255428265387));
#229984=CARTESIAN_POINT('Ctrl Pts',(50.8725634718546,36.8914758894169,2.66381699700678));
#229985=CARTESIAN_POINT('Ctrl Pts',(50.875182088265,36.8847438022849,2.66554034873278));
#229986=CARTESIAN_POINT('Ctrl Pts',(50.8773323251414,36.8779301449086,2.66766759643982));
#229987=CARTESIAN_POINT('Ctrl Pts',(50.8790261328805,36.8711298300324,2.67012012783159));
#229988=CARTESIAN_POINT('Ctrl Pts',(50.87987303675,36.8677296725944,2.67134639352747));
#229989=CARTESIAN_POINT('Ctrl Pts',(50.8806059576336,36.8643326829601,2.67265375585023));
#229990=CARTESIAN_POINT('Ctrl Pts',(50.8812272732515,36.8609495224154,2.67403135126951));
#229991=CARTESIAN_POINT('Ctrl Pts',(50.8815379310604,36.859257942143,2.67472014897915));
#229992=CARTESIAN_POINT('Ctrl Pts',(50.8818206978293,36.8575698050848,2.67542649668644));
#229993=CARTESIAN_POINT('Ctrl Pts',(50.8820759354568,36.855886355634,2.67614899656114));
#229994=CARTESIAN_POINT('Ctrl Pts',(50.8821397448637,36.8554654932713,2.67632962152981));
#229995=CARTESIAN_POINT('Ctrl Pts',(50.882201833919,36.8550449235852,2.67651125590961));
#229996=CARTESIAN_POINT('Ctrl Pts',(50.8822622087211,36.8546246654168,2.67669387767535));
#229997=CARTESIAN_POINT('Ctrl Pts',(50.8824433331273,36.8533638909117,2.67724174297255));
#229998=CARTESIAN_POINT('Ctrl Pts',(50.8826090281506,36.8521059215534,2.67779849504759));
#229999=CARTESIAN_POINT('Ctrl Pts',(50.8827594682968,36.8508512527542,2.67836353618021));
#230000=CARTESIAN_POINT('Ctrl Pts',(50.8837991030487,36.842180712886,2.68226832098921));
#230001=CARTESIAN_POINT('Ctrl Pts',(50.884159119436,36.8336410897273,2.68659153751404));
#230002=CARTESIAN_POINT('Ctrl Pts',(50.8839416093727,36.825293116072,2.69123699486192));
#230003=CARTESIAN_POINT('Ctrl Pts',(50.8838335074683,36.82114419608,2.69354577441229));
#230004=CARTESIAN_POINT('Ctrl Pts',(50.8835822787327,36.8170422299141,2.69593478828129));
#230005=CARTESIAN_POINT('Ctrl Pts',(50.8831977843866,36.8129929908133,2.6983956526123));
#230006=CARTESIAN_POINT('Ctrl Pts',(50.8823495324296,36.8040597645471,2.70382468689055));
#230007=CARTESIAN_POINT('Ctrl Pts',(50.8808651175412,36.7953829494618,2.70961155815097));
#230008=CARTESIAN_POINT('Ctrl Pts',(50.8788231440731,36.7870848098365,2.71562701361776));
#230009=CARTESIAN_POINT('Ctrl Pts',(50.8780771854145,36.7840533947863,2.71782453535866));
#230010=CARTESIAN_POINT('Ctrl Pts',(50.8772631333235,36.7810676701179,2.7200505150241));
#230011=CARTESIAN_POINT('Ctrl Pts',(50.8763859670025,36.7781294934921,2.72229986760123));
#230012=CARTESIAN_POINT('Ctrl Pts',(50.8734396581491,36.7682604691136,2.7298552048891));
#230013=CARTESIAN_POINT('Ctrl Pts',(50.8697545265637,36.7588677364069,2.7377084553459));
#230014=CARTESIAN_POINT('Ctrl Pts',(50.8654587487961,36.7499455893907,2.745767067018));
#230015=CARTESIAN_POINT('Ctrl Pts',(50.8607371801612,36.740139092922,2.75462443585091));
#230016=CARTESIAN_POINT('Ctrl Pts',(50.8552777667771,36.7309004184138,2.76373036323261));
#230017=CARTESIAN_POINT('Ctrl Pts',(50.8491983060112,36.7222305213312,2.77299664636915));
#230018=CARTESIAN_POINT('Ctrl Pts',(50.8426504662821,36.7128926706977,2.78297683033586));
#230019=CARTESIAN_POINT('Ctrl Pts',(50.8353827952099,36.7042135591838,2.79314401479019));
#230020=CARTESIAN_POINT('Ctrl Pts',(50.8274903908653,36.6962177694295,2.80341452428075));
#230021=CARTESIAN_POINT('Ctrl Pts',(50.8197045606282,36.6883299498348,2.81354634721465));
#230022=CARTESIAN_POINT('Ctrl Pts',(50.8113095502206,36.6811063421668,2.82378004209267));
#230023=CARTESIAN_POINT('Ctrl Pts',(50.8023624960591,36.6746059268181,2.83404198860288));
#230024=CARTESIAN_POINT('Ctrl Pts',(48.0191904766736,34.6525130919799,2.83404198860286));
#230025=CARTESIAN_POINT('Ctrl Pts',(48.010628096726,34.646292158807,2.824221264431));
#230026=CARTESIAN_POINT('Ctrl Pts',(48.0016058360822,34.6407689407924,2.81442815028663));
#230027=CARTESIAN_POINT('Ctrl Pts',(47.9921771448984,34.6359660967498,2.80471618166547));
#230028=CARTESIAN_POINT('Ctrl Pts',(47.9830729139875,34.6313285282538,2.79533842146496));
#230029=CARTESIAN_POINT('Ctrl Pts',(47.9735885825128,34.6273621044923,2.78603515650543));
#230030=CARTESIAN_POINT('Ctrl Pts',(47.9637494987682,34.6241270221294,2.77685887347094));
#230031=CARTESIAN_POINT('Ctrl Pts',(47.9544484832192,34.6210688561314,2.76818441216929));
#230032=CARTESIAN_POINT('Ctrl Pts',(47.9448295964494,34.618663947498,2.75962261521989));
#230033=CARTESIAN_POINT('Ctrl Pts',(47.9349076763743,34.6170045862121,2.75123537702035));
#230034=CARTESIAN_POINT('Ctrl Pts',(47.9257697544377,34.6154763423056,2.74351087134492));
#230035=CARTESIAN_POINT('Ctrl Pts',(47.916374251109,34.6145804463111,2.73593399450217));
#230036=CARTESIAN_POINT('Ctrl Pts',(47.9067364390668,34.6144269453422,2.72857657812942));
#230037=CARTESIAN_POINT('Ctrl Pts',(47.9038626380671,34.6143811744519,2.72638274508568));
#230038=CARTESIAN_POINT('Ctrl Pts',(47.9009673483059,34.6144016870566,2.72420861709728));
#230039=CARTESIAN_POINT('Ctrl Pts',(47.8980511519205,34.6144921419177,2.72205663736733));
#230040=CARTESIAN_POINT('Ctrl Pts',(47.8951647518766,34.6145816725529,2.71992664556772));
#230041=CARTESIAN_POINT('Ctrl Pts',(47.8922608568399,34.6147393566953,2.71782089927891));
#230042=CARTESIAN_POINT('Ctrl Pts',(47.8893433277785,34.6149683234597,2.71574387311252));
#230043=CARTESIAN_POINT('Ctrl Pts',(47.8891404485133,34.6149842453607,2.71559944077493));
#230044=CARTESIAN_POINT('Ctrl Pts',(47.8889374970514,34.6150005017597,2.71545515216075));
#230045=CARTESIAN_POINT('Ctrl Pts',(47.8887344737214,34.6150170939191,2.71531100781736));
#230046=CARTESIAN_POINT('Ctrl Pts',(47.8798331871999,34.6157445549672,2.70899119176091));
#230047=CARTESIAN_POINT('Ctrl Pts',(47.8708080647649,34.6171603320595,2.70298296066847));
#230048=CARTESIAN_POINT('Ctrl Pts',(47.8617555581815,34.6193291901737,2.69736727774146));
#230049=CARTESIAN_POINT('Ctrl Pts',(47.853317048731,34.6213509428812,2.69213248525445));
#230050=CARTESIAN_POINT('Ctrl Pts',(47.8448540540103,34.6240275231021,2.6872386618549));
#230051=CARTESIAN_POINT('Ctrl Pts',(47.83646663697,34.6274308957716,2.68278595829589));
#230052=CARTESIAN_POINT('Ctrl Pts',(47.8333984113064,34.6286758935244,2.68115710172822));
#230053=CARTESIAN_POINT('Ctrl Pts',(47.8303405713851,34.6300183184512,2.67958763637817));
#230054=CARTESIAN_POINT('Ctrl Pts',(47.827299095813,34.6314622582451,2.67808378645364));
#230055=CARTESIAN_POINT('Ctrl Pts',(47.8265677225447,34.6318094775277,2.67772216078599));
#230056=CARTESIAN_POINT('Ctrl Pts',(47.8258370084447,34.6321630753106,2.67736403603562));
#230057=CARTESIAN_POINT('Ctrl Pts',(47.8251070891649,34.6325230544378,2.67700956934478));
#230058=CARTESIAN_POINT('Ctrl Pts',(47.8243999798625,34.6328717842173,2.67666617973803));
#230059=CARTESIAN_POINT('Ctrl Pts',(47.8236936164943,34.6332265027182,2.67632622314117));
#230060=CARTESIAN_POINT('Ctrl Pts',(47.822988124598,34.6335872094466,2.67598984158772));
#230061=CARTESIAN_POINT('Ctrl Pts',(47.8152586455549,34.6375391685162,2.67230439292226));
#230062=CARTESIAN_POINT('Ctrl Pts',(47.8076288798887,34.6422128973063,2.66904964539986));
#230063=CARTESIAN_POINT('Ctrl Pts',(47.8002860619016,34.647586547601,2.6664020356674));
#230064=CARTESIAN_POINT('Ctrl Pts',(47.7972407764162,34.6498151605497,2.66530399299449));
#230065=CARTESIAN_POINT('Ctrl Pts',(47.7942448304652,34.6521637338115,2.66430995142263));
#230066=CARTESIAN_POINT('Ctrl Pts',(47.7913110614419,34.654628954734,2.6634305347336));
#230067=CARTESIAN_POINT('Ctrl Pts',(47.7863072126526,34.6588336459113,2.66193059792885));
#230068=CARTESIAN_POINT('Ctrl Pts',(47.7814867201293,34.6633779280161,2.66076519817129));
#230069=CARTESIAN_POINT('Ctrl Pts',(47.7769196237423,34.6682420184009,2.65997805604462));
#230070=CARTESIAN_POINT('Ctrl Pts',(47.7746360755487,34.6706740635933,2.65958448498128));
#230071=CARTESIAN_POINT('Ctrl Pts',(47.7724170058819,34.6731869650546,2.65928526260764));
#230072=CARTESIAN_POINT('Ctrl Pts',(47.7702712352611,34.6757782448035,2.65908463971327));
#230073=CARTESIAN_POINT('Ctrl Pts',(47.7681254646402,34.6783695245525,2.65888401681889));
#230074=CARTESIAN_POINT('Ctrl Pts',(47.7660530039194,34.6810391382372,2.65878198860287));
#230075=CARTESIAN_POINT('Ctrl Pts',(47.7640607692763,34.6837837831348,2.65878198860287));
#230076=CARTESIAN_POINT('Origin',(43.2882232241948,38.9973987043321,2.8340419886029));
#230077=CARTESIAN_POINT('Ctrl Pts',(46.435582879267,42.0671296588098,2.83404198860292));
#230078=CARTESIAN_POINT('Ctrl Pts',(46.4434678907493,42.0742293550379,2.82419652440087));
#230079=CARTESIAN_POINT('Ctrl Pts',(46.451889695674,42.0806858315475,2.81438790575664));
#230080=CARTESIAN_POINT('Ctrl Pts',(46.4607957007318,42.0864721532161,2.80466781256909));
#230081=CARTESIAN_POINT('Ctrl Pts',(46.469412313657,42.0920704538858,2.79526356453077));
#230082=CARTESIAN_POINT('Ctrl Pts',(46.4784832882813,42.0970420880508,2.78594102496224));
#230083=CARTESIAN_POINT('Ctrl Pts',(46.4879887958181,42.1013257711392,2.77675109088763));
#230084=CARTESIAN_POINT('Ctrl Pts',(46.4969804206325,42.1053778715667,2.76805797913658));
#230085=CARTESIAN_POINT('Ctrl Pts',(46.5063617095237,42.1088147776126,2.75948271210128));
#230086=CARTESIAN_POINT('Ctrl Pts',(46.5161273793239,42.1115441100125,2.75108575573183));
#230087=CARTESIAN_POINT('Ctrl Pts',(46.5251222674812,42.1140580225433,2.7433515516322));
#230088=CARTESIAN_POINT('Ctrl Pts',(46.534443807433,42.1159717447015,2.73576818685884));
#230089=CARTESIAN_POINT('Ctrl Pts',(46.5440884908204,42.1171748456138,2.72840626160431));
#230090=CARTESIAN_POINT('Ctrl Pts',(46.5468860468482,42.117523819455,2.72627084693645));
#230091=CARTESIAN_POINT('Ctrl Pts',(46.5497107674235,42.1178127362982,2.72415424587519));
#230092=CARTESIAN_POINT('Ctrl Pts',(46.5525624800841,42.1180382068977,2.72205867173285));
#230093=CARTESIAN_POINT('Ctrl Pts',(46.5556539199574,42.118282631524,2.71978693462889));
#230094=CARTESIAN_POINT('Ctrl Pts',(46.5587726948498,42.1184532289194,2.7175441134079));
#230095=CARTESIAN_POINT('Ctrl Pts',(46.5619176830194,42.1185461584681,2.71533341844287));
#230096=CARTESIAN_POINT('Ctrl Pts',(46.5705491277288,42.1188012043437,2.70926614876435));
#230097=CARTESIAN_POINT('Ctrl Pts',(46.5793682643811,42.1184278543823,2.70347381860453));
#230098=CARTESIAN_POINT('Ctrl Pts',(46.5882835699004,42.1173773384969,2.69804914171439));
#230099=CARTESIAN_POINT('Ctrl Pts',(46.5964405904275,42.1164161734956,2.6930858568724));
#230100=CARTESIAN_POINT('Ctrl Pts',(46.6046697328844,42.1148801579478,2.68842799053214));
#230101=CARTESIAN_POINT('Ctrl Pts',(46.612914529219,42.1127009621828,2.6841476705424));
#230102=CARTESIAN_POINT('Ctrl Pts',(46.6169643462455,42.1116305483417,2.68204519134583));
#230103=CARTESIAN_POINT('Ctrl Pts',(46.6210176421367,42.1104045383079,2.68003431778542));
#230104=CARTESIAN_POINT('Ctrl Pts',(46.6250654385592,42.109012387551,2.67812693945299));
#230105=CARTESIAN_POINT('Ctrl Pts',(46.6258334685044,42.1087482405046,2.67776503299251));
#230106=CARTESIAN_POINT('Ctrl Pts',(46.6266015422614,42.108477638333,2.67740659639971));
#230107=CARTESIAN_POINT('Ctrl Pts',(46.6273695213206,42.1082005605487,2.67705178968902));
#230108=CARTESIAN_POINT('Ctrl Pts',(46.6281135010342,42.1079321414452,2.67670807068805));
#230109=CARTESIAN_POINT('Ctrl Pts',(46.6288573918596,42.1076576451502,2.67636775825313));
#230110=CARTESIAN_POINT('Ctrl Pts',(46.6296010653159,42.1073770559081,2.67603099699302));
#230111=CARTESIAN_POINT('Ctrl Pts',(46.6377054654054,42.1043192521646,2.67236104217164));
#230112=CARTESIAN_POINT('Ctrl Pts',(46.6457892400078,42.1005354505673,2.66911440541501));
#230113=CARTESIAN_POINT('Ctrl Pts',(46.653661939077,42.0960238460767,2.66646778189653));
#230114=CARTESIAN_POINT('Ctrl Pts',(46.6569866287807,42.0941185674849,2.66535009635006));
#230115=CARTESIAN_POINT('Ctrl Pts',(46.6602736399414,42.0920839261384,2.66433897912384));
#230116=CARTESIAN_POINT('Ctrl Pts',(46.6635089796843,42.0899216923181,2.66344564884839));
#230117=CARTESIAN_POINT('Ctrl Pts',(46.6689572109695,42.0862805445928,2.66194130298631));
#230118=CARTESIAN_POINT('Ctrl Pts',(46.6742564366675,42.0822770520159,2.66077206705464));
#230119=CARTESIAN_POINT('Ctrl Pts',(46.679333290145,42.0779224130574,2.65998225155758));
#230120=CARTESIAN_POINT('Ctrl Pts',(46.6806025035143,42.0768337533177,2.65978479768331));
#230121=CARTESIAN_POINT('Ctrl Pts',(46.6818576549905,42.0757229796948,2.65961098966666));
#230122=CARTESIAN_POINT('Ctrl Pts',(46.683097373911,42.0745900553978,2.65946139030545));
#230123=CARTESIAN_POINT('Ctrl Pts',(46.6849569522919,42.0728906689523,2.65923699126363));
#230124=CARTESIAN_POINT('Ctrl Pts',(46.686781786976,42.0711414461005,2.65906707562485));
#230125=CARTESIAN_POINT('Ctrl Pts',(46.6885684866733,42.069343399161,2.65895332562962));
#230126=CARTESIAN_POINT('Ctrl Pts',(46.6903551863705,42.0675453522215,2.6588395756344));
#230127=CARTESIAN_POINT('Ctrl Pts',(46.692103753135,42.0656984926167,2.65878198860292));
#230128=CARTESIAN_POINT('Ctrl Pts',(46.6938111422604,42.0638038389703,2.65878198860292));
#230129=CARTESIAN_POINT('Ctrl Pts',(43.8565665267056,39.5091373124625,2.6587819886029));
#230130=CARTESIAN_POINT('Ctrl Pts',(43.8507890749209,39.5155480799603,2.6587819886029));
#230131=CARTESIAN_POINT('Ctrl Pts',(43.8455908828153,39.5223801852464,2.65945335517882));
#230132=CARTESIAN_POINT('Ctrl Pts',(43.8409939475747,39.5294841269563,2.66072561226625));
#230133=CARTESIAN_POINT('Ctrl Pts',(43.8380247990819,39.5340725443945,2.66154735980364));
#230134=CARTESIAN_POINT('Ctrl Pts',(43.8353056940461,39.5387738681333,2.6626189576691));
#230135=CARTESIAN_POINT('Ctrl Pts',(43.8328343017436,39.5435446222365,2.66391429251056));
#230136=CARTESIAN_POINT('Ctrl Pts',(43.8295586128169,39.5498679835146,2.66563118464153));
#230137=CARTESIAN_POINT('Ctrl Pts',(43.8267236865061,39.5563148866445,2.66774105138728));
#230138=CARTESIAN_POINT('Ctrl Pts',(43.8243293609623,39.5627952650341,2.67016894181779));
#230139=CARTESIAN_POINT('Ctrl Pts',(43.8231321981904,39.566035454229,2.67138288703305));
#230140=CARTESIAN_POINT('Ctrl Pts',(43.8220450509626,39.5692841591688,2.67267613167581));
#230141=CARTESIAN_POINT('Ctrl Pts',(43.8210669472518,39.5725311673657,2.67403835432583));
#230142=CARTESIAN_POINT('Ctrl Pts',(43.8205778953964,39.5741546714642,2.67471946565083));
#230143=CARTESIAN_POINT('Ctrl Pts',(43.8201160933895,39.5757777635549,2.67541781389553));
#230144=CARTESIAN_POINT('Ctrl Pts',(43.8196813503778,39.5773992434497,2.67613207244199));
#230145=CARTESIAN_POINT('Ctrl Pts',(43.8195726646249,39.5778046134234,2.6763106370786));
#230146=CARTESIAN_POINT('Ctrl Pts',(43.8194656698239,39.5782098828932,2.67649019601875));
#230147=CARTESIAN_POINT('Ctrl Pts',(43.8193603625175,39.5786150336268,2.67667072836686));
#230148=CARTESIAN_POINT('Ctrl Pts',(43.8190444405985,39.5798304858278,2.6772123254112));
#230149=CARTESIAN_POINT('Ctrl Pts',(43.8187437073124,39.5810448681192,2.67776268340076));
#230150=CARTESIAN_POINT('Ctrl Pts',(43.8184580587802,39.5822576997163,2.67832123541545));
#230151=CARTESIAN_POINT('Ctrl Pts',(43.8164459874035,39.5908007288813,2.6822556036847));
#230152=CARTESIAN_POINT('Ctrl Pts',(43.8151322889032,39.5992865061387,2.6866179299891));
#230153=CARTESIAN_POINT('Ctrl Pts',(43.8144227306312,39.6076412948833,2.69130986622595));
#230154=CARTESIAN_POINT('Ctrl Pts',(43.814078595636,39.6116933583963,2.69358545023075));
#230155=CARTESIAN_POINT('Ctrl Pts',(43.8138769687219,39.6157150281162,2.69593918853494));
#230156=CARTESIAN_POINT('Ctrl Pts',(43.8138093098903,39.6196997093544,2.69836306235503));
#230157=CARTESIAN_POINT('Ctrl Pts',(43.8137057289464,39.6257999779284,2.70207384382236));
#230158=CARTESIAN_POINT('Ctrl Pts',(43.8139151128799,39.6318101761583,2.70594760814237));
#230159=CARTESIAN_POINT('Ctrl Pts',(43.8144090029878,39.6376940219323,2.70995196345716));
#230160=CARTESIAN_POINT('Ctrl Pts',(43.8146383681089,39.6404265103487,2.71181160678114));
#230161=CARTESIAN_POINT('Ctrl Pts',(43.8149288459967,39.6431316855284,2.71369962772107));
#230162=CARTESIAN_POINT('Ctrl Pts',(43.8152787628653,39.6458055463963,2.71561183138669));
#230163=CARTESIAN_POINT('Ctrl Pts',(43.8153055826145,39.6460104872963,2.7157583942632));
#230164=CARTESIAN_POINT('Ctrl Pts',(43.8153327221694,39.6462152612036,2.71590508903217));
#230165=CARTESIAN_POINT('Ctrl Pts',(43.8153601802954,39.6464198673377,2.71605191409919));
#230166=CARTESIAN_POINT('Ctrl Pts',(43.8157458841823,39.6492939666539,2.71811436362761));
#230167=CARTESIAN_POINT('Ctrl Pts',(43.8161965332334,39.6521348180508,2.72020091026967));
#230168=CARTESIAN_POINT('Ctrl Pts',(43.816707563491,39.654938997009,2.7223062486219));
#230169=CARTESIAN_POINT('Ctrl Pts',(43.818540027111,39.6649942840467,2.72985561753114));
#230170=CARTESIAN_POINT('Ctrl Pts',(43.821161113837,39.6746561192247,2.73770089914344));
#230171=CARTESIAN_POINT('Ctrl Pts',(43.82444189681,39.6839173731633,2.74574823347091));
#230172=CARTESIAN_POINT('Ctrl Pts',(43.8280471477134,39.6940945608664,2.75459144547029));
#230173=CARTESIAN_POINT('Ctrl Pts',(43.8324491002309,39.703788679467,2.7636791175426));
#230174=CARTESIAN_POINT('Ctrl Pts',(43.8375295667867,39.7129876499604,2.77292162564703));
#230175=CARTESIAN_POINT('Ctrl Pts',(43.8430151956439,39.7229202294667,2.78290121484676));
#230176=CARTESIAN_POINT('Ctrl Pts',(43.8492922888407,39.7322766233291,2.79306229500101));
#230177=CARTESIAN_POINT('Ctrl Pts',(43.8562669044089,39.7410245486279,2.80331916685133));
#230178=CARTESIAN_POINT('Ctrl Pts',(43.8631830101192,39.7496990878222,2.81348999408622));
#230179=CARTESIAN_POINT('Ctrl Pts',(43.8707860819058,39.7577762496637,2.82375635966854));
#230180=CARTESIAN_POINT('Ctrl Pts',(43.8790236240219,39.7651933659001,2.8340419886029));
#230181=CARTESIAN_POINT('Origin',(0.0101975504409105,-0.0113255271400898,
2.83404198860262));
#230182=CARTESIAN_POINT('Ctrl Pts',(46.7142062431422,42.0411527846897,2.65878198860292));
#230183=CARTESIAN_POINT('Ctrl Pts',(46.7199506919426,42.0347675597391,2.65878198860292));
#230184=CARTESIAN_POINT('Ctrl Pts',(46.7251107020211,42.027959214278,2.65944603041874));
#230185=CARTESIAN_POINT('Ctrl Pts',(46.7296675019392,42.0208774479587,2.66070439264083));
#230186=CARTESIAN_POINT('Ctrl Pts',(46.7325790801594,42.0163525364098,2.66150842619609));
#230187=CARTESIAN_POINT('Ctrl Pts',(46.735245189214,42.0117164852,2.66255428265387));
#230188=CARTESIAN_POINT('Ctrl Pts',(46.7376689638753,42.0070114066747,2.66381699700683));
#230189=CARTESIAN_POINT('Ctrl Pts',(46.7409769299535,42.0005899185698,2.66554034873282));
#230190=CARTESIAN_POINT('Ctrl Pts',(46.7438276087421,41.9940383480778,2.66766759643986));
#230191=CARTESIAN_POINT('Ctrl Pts',(46.7462229640888,41.9874523371582,2.67012012783161));
#230192=CARTESIAN_POINT('Ctrl Pts',(46.7474206417622,41.9841593316984,2.67134639352748));
#230193=CARTESIAN_POINT('Ctrl Pts',(46.7485046297347,41.9808575622225,2.67265375585023));
#230194=CARTESIAN_POINT('Ctrl Pts',(46.7494761782933,41.9775578801519,2.67403135126951));
#230195=CARTESIAN_POINT('Ctrl Pts',(46.7499619525726,41.9759080391167,2.67472014897914));
#230196=CARTESIAN_POINT('Ctrl Pts',(46.7504196286881,41.9742587070257,2.67542649668643));
#230197=CARTESIAN_POINT('Ctrl Pts',(46.7508494364813,41.9726111592841,2.67614899656112));
#230198=CARTESIAN_POINT('Ctrl Pts',(46.7509568884295,41.9721992723487,2.67632962152979));
#230199=CARTESIAN_POINT('Ctrl Pts',(46.7510625988575,41.9717874966609,2.67651125590961));
#230200=CARTESIAN_POINT('Ctrl Pts',(46.7511665718606,41.971375851596,2.67669387767534));
#230201=CARTESIAN_POINT('Ctrl Pts',(46.7514784908699,41.9701409164014,2.67724174297254));
#230202=CARTESIAN_POINT('Ctrl Pts',(46.7517747718024,41.968907158177,2.67779849504757));
#230203=CARTESIAN_POINT('Ctrl Pts',(46.7520555364232,41.9676750878621,2.67836353618018));
#230204=CARTESIAN_POINT('Ctrl Pts',(46.7539957941554,41.9591607175414,2.68226832098922));
#230205=CARTESIAN_POINT('Ctrl Pts',(46.7552464720209,41.9507055072916,2.6865915375141));
#230206=CARTESIAN_POINT('Ctrl Pts',(46.755902754358,41.9423805287166,2.69123699486203));
#230207=CARTESIAN_POINT('Ctrl Pts',(46.7562289248781,41.9382430372166,2.69354577441237));
#230208=CARTESIAN_POINT('Ctrl Pts',(46.7564078446195,41.934137281497,2.69593478828134));
#230209=CARTESIAN_POINT('Ctrl Pts',(46.7564487173143,41.9300700339486,2.69839565261231));
#230210=CARTESIAN_POINT('Ctrl Pts',(46.7565388885838,41.9210970783571,2.70382468689057));
#230211=CARTESIAN_POINT('Ctrl Pts',(46.7559695796225,41.9123126321656,2.70961155815099));
#230212=CARTESIAN_POINT('Ctrl Pts',(46.7548061840817,41.9038465062687,2.71562701361779));
#230213=CARTESIAN_POINT('Ctrl Pts',(46.7543811810194,41.900753723715,2.7178245353587));
#230214=CARTESIAN_POINT('Ctrl Pts',(46.7538836816023,41.8976992635448,2.72005051502414));
#230215=CARTESIAN_POINT('Ctrl Pts',(46.7533184435777,41.8946854937103,2.72229986760127));
#230216=CARTESIAN_POINT('Ctrl Pts',(46.7514198688645,41.8845625597425,2.72985520488967));
#230217=CARTESIAN_POINT('Ctrl Pts',(46.748736732731,41.8748360802661,2.73770845534701));
#230218=CARTESIAN_POINT('Ctrl Pts',(46.7453971059998,41.8655137786555,2.74576706701967));
#230219=CARTESIAN_POINT('Ctrl Pts',(46.7417264606174,41.8552674648863,2.75462443585317));
#230220=CARTESIAN_POINT('Ctrl Pts',(46.7372626589195,41.8455087367117,2.76373036323547));
#230221=CARTESIAN_POINT('Ctrl Pts',(46.732122753094,41.8362508575405,2.77299664637264));
#230222=CARTESIAN_POINT('Ctrl Pts',(46.7265868542923,41.8262797250045,2.78297683034014));
#230223=CARTESIAN_POINT('Ctrl Pts',(46.720266210471,41.8168884800825,2.79314401479529));
#230224=CARTESIAN_POINT('Ctrl Pts',(46.713252829158,41.808111511203,2.80341452428671));
#230225=CARTESIAN_POINT('Ctrl Pts',(46.7063341521755,41.7994530610414,2.81354634721862));
#230226=CARTESIAN_POINT('Ctrl Pts',(46.6987402031235,41.7913915075168,2.82378004209465));
#230227=CARTESIAN_POINT('Ctrl Pts',(46.6905216402897,41.7839914803029,2.83404198860292));
#230228=CARTESIAN_POINT('Ctrl Pts',(44.1339623850447,39.4820551873932,2.8340419886029));
#230229=CARTESIAN_POINT('Ctrl Pts',(44.1260971752944,39.4749733207248,2.82422126443033));
#230230=CARTESIAN_POINT('Ctrl Pts',(44.1177016730292,39.4685372764357,2.81442815028527));
#230231=CARTESIAN_POINT('Ctrl Pts',(44.1088266671086,39.4627751762749,2.80471618166343));
#230232=CARTESIAN_POINT('Ctrl Pts',(44.100257068035,39.4572113615978,2.79533842146243));
#230233=CARTESIAN_POINT('Ctrl Pts',(44.0912392969003,39.4522752837263,2.78603515650242));
#230234=CARTESIAN_POINT('Ctrl Pts',(44.0817922708732,39.4480294591793,2.77685887346747));
#230235=CARTESIAN_POINT('Ctrl Pts',(44.0728618726522,39.4440158252724,2.76818441216543));
#230236=CARTESIAN_POINT('Ctrl Pts',(44.0635470605538,39.4406186435278,2.75962261521566));
#230237=CARTESIAN_POINT('Ctrl Pts',(44.0538529442796,39.4379312493386,2.75123537701578));
#230238=CARTESIAN_POINT('Ctrl Pts',(44.0449248258219,39.4354562043748,2.74351087134));
#230239=CARTESIAN_POINT('Ctrl Pts',(44.0356744386745,39.4335831186678,2.73593399449692));
#230240=CARTESIAN_POINT('Ctrl Pts',(44.0261054687948,39.4324230329116,2.72857657812389));
#230241=CARTESIAN_POINT('Ctrl Pts',(44.0232521951408,39.4320771187572,2.72638274508204));
#230242=CARTESIAN_POINT('Ctrl Pts',(44.0203706219312,39.4317948788026,2.72420861709549));
#230243=CARTESIAN_POINT('Ctrl Pts',(44.0174609456696,39.4315800126159,2.72205663736736));
#230244=CARTESIAN_POINT('Ctrl Pts',(44.0145809991274,39.4313673418319,2.71992664556775));
#230245=CARTESIAN_POINT('Ctrl Pts',(44.0116765294504,39.4312206224785,2.71782089927893));
#230246=CARTESIAN_POINT('Ctrl Pts',(44.0087510493745,39.4311433701096,2.71574387311255));
#230247=CARTESIAN_POINT('Ctrl Pts',(44.0085476172113,39.431137998131,2.71559944077495));
#230248=CARTESIAN_POINT('Ctrl Pts',(44.0083440782823,39.4311329512713,2.71545515216078));
#230249=CARTESIAN_POINT('Ctrl Pts',(44.0081404327824,39.4311282308204,2.71531100781739));
#230250=CARTESIAN_POINT('Ctrl Pts',(43.9992118680542,39.4309212689595,2.70899119176083));
#230251=CARTESIAN_POINT('Ctrl Pts',(43.9900881971803,39.4313859080979,2.70298296066829));
#230252=CARTESIAN_POINT('Ctrl Pts',(43.9808585737693,39.4325966403786,2.6973672777412));
#230253=CARTESIAN_POINT('Ctrl Pts',(43.9722549606524,39.4337252532881,2.69213248525396));
#230254=CARTESIAN_POINT('Ctrl Pts',(43.9635585482846,39.4355025470899,2.68723866185422));
#230255=CARTESIAN_POINT('Ctrl Pts',(43.9548613290769,39.438010551914,2.68278595829505));
#230256=CARTESIAN_POINT('Ctrl Pts',(43.9516797737733,39.4389280125252,2.6811571017277));
#230257=CARTESIAN_POINT('Ctrl Pts',(43.948498363405,39.4399434521997,2.67958763637796));
#230258=CARTESIAN_POINT('Ctrl Pts',(43.9453226165471,39.4410615611725,2.6780837864537));
#230259=CARTESIAN_POINT('Ctrl Pts',(43.9445589555201,39.4413304290278,2.67772216078605));
#230260=CARTESIAN_POINT('Ctrl Pts',(43.9437952833156,39.441605709343,2.67736403603568));
#230261=CARTESIAN_POINT('Ctrl Pts',(43.9430317345449,39.4418874191263,2.67700956934484));
#230262=CARTESIAN_POINT('Ctrl Pts',(43.9422920466734,39.4421603254788,2.67666617973809));
#230263=CARTESIAN_POINT('Ctrl Pts',(43.9415524746578,39.4424392657173,2.67632622314124));
#230264=CARTESIAN_POINT('Ctrl Pts',(43.9408131433999,39.4427242524727,2.67598984158778));
#230265=CARTESIAN_POINT('Ctrl Pts',(43.9327129150437,39.4458466117307,2.67230439292245));
#230266=CARTESIAN_POINT('Ctrl Pts',(43.9246364083441,39.4496972096652,2.66904964540014));
#230267=CARTESIAN_POINT('Ctrl Pts',(43.9167721156751,39.4542738890608,2.66640203566772));
#230268=CARTESIAN_POINT('Ctrl Pts',(43.9135105590952,39.4561719744227,2.6653039929947));
#230269=CARTESIAN_POINT('Ctrl Pts',(43.9102855324954,39.4581945203283,2.66430995142275));
#230270=CARTESIAN_POINT('Ctrl Pts',(43.9071101492109,39.4603395741453,2.66343053473365));
#230271=CARTESIAN_POINT('Ctrl Pts',(43.9016942021215,39.4639981869599,2.66193059792889));
#230272=CARTESIAN_POINT('Ctrl Pts',(43.8964251099356,39.4680136963363,2.66076519817133));
#230273=CARTESIAN_POINT('Ctrl Pts',(43.8913745966875,39.4723737491583,2.65997805604465));
#230274=CARTESIAN_POINT('Ctrl Pts',(43.8888493400635,39.4745537755693,2.65958448498131));
#230275=CARTESIAN_POINT('Ctrl Pts',(43.8863797569643,39.4768209551513,2.65928526260768));
#230276=CARTESIAN_POINT('Ctrl Pts',(43.8839748786094,39.479173745493,2.6590846397133));
#230277=CARTESIAN_POINT('Ctrl Pts',(43.8815700002544,39.4815265358348,2.65888401681892));
#230278=CARTESIAN_POINT('Ctrl Pts',(43.879229842074,39.483964893962,2.6587819886029));
#230279=CARTESIAN_POINT('Ctrl Pts',(43.8769616275874,39.4864862581819,2.6587819886029));
#230280=CARTESIAN_POINT('Origin',(38.9747476500513,43.3086183250769,2.83404198860292));
#230281=CARTESIAN_POINT('Ctrl Pts',(41.7839914803026,46.69052164029,2.83404198860295));
#230282=CARTESIAN_POINT('Ctrl Pts',(41.7910911765306,46.6984066517723,2.82419652440089));
#230283=CARTESIAN_POINT('Ctrl Pts',(41.7987919603591,46.7057080773548,2.81438790575666));
#230284=CARTESIAN_POINT('Ctrl Pts',(41.8070443420773,46.7123936319704,2.80466781256913));
#230285=CARTESIAN_POINT('Ctrl Pts',(41.8150285705293,46.7188619458709,2.79526356453088));
#230286=CARTESIAN_POINT('Ctrl Pts',(41.8235301761263,46.7247545199416,2.78594102496242));
#230287=CARTESIAN_POINT('Ctrl Pts',(41.8325358446879,46.7300083326612,2.77675109088789));
#230288=CARTESIAN_POINT('Ctrl Pts',(41.84105465261,46.7349781159828,2.76805797913695));
#230289=CARTESIAN_POINT('Ctrl Pts',(41.8500252953116,46.7393768060089,2.75948271210177));
#230290=CARTESIAN_POINT('Ctrl Pts',(41.8594521748292,46.7431119772975,2.75108575573242));
#230291=CARTESIAN_POINT('Ctrl Pts',(41.8681350126342,46.7465523401887,2.74335155163291));
#230292=CARTESIAN_POINT('Ctrl Pts',(41.8772054497783,46.7494299450231,2.73576818685966));
#230293=CARTESIAN_POINT('Ctrl Pts',(41.8866715402913,46.7516345991559,2.72840626160521));
#230294=CARTESIAN_POINT('Ctrl Pts',(41.8894172933155,46.7522740855145,2.72627084693707));
#230295=CARTESIAN_POINT('Ctrl Pts',(41.8921963397426,46.7528566833419,2.72415424587553));
#230296=CARTESIAN_POINT('Ctrl Pts',(41.8950088623279,46.753379003932,2.72205867173292));
#230297=CARTESIAN_POINT('Ctrl Pts',(41.8980578176395,46.7539452330338,2.71978693462894));
#230298=CARTESIAN_POINT('Ctrl Pts',(41.9011416752732,46.7544408966256,2.71754411340795));
#230299=CARTESIAN_POINT('Ctrl Pts',(41.9042597210856,46.7548620578768,2.71533341844291));
#230300=CARTESIAN_POINT('Ctrl Pts',(41.9128172222843,46.7560179382356,2.70926614876437));
#230301=CARTESIAN_POINT('Ctrl Pts',(41.921627072481,46.7565684843261,2.70347381860455));
#230302=CARTESIAN_POINT('Ctrl Pts',(41.9306033478349,46.7564556264621,2.6980491417144));
#230303=CARTESIAN_POINT('Ctrl Pts',(41.9388161524502,46.7563523676437,2.69308585687263));
#230304=CARTESIAN_POINT('Ctrl Pts',(41.9471607721481,46.7556849461649,2.68842799053256));
#230305=CARTESIAN_POINT('Ctrl Pts',(41.9555881906098,46.7543795041533,2.68414767054298));
#230306=CARTESIAN_POINT('Ctrl Pts',(41.9597277110291,46.7537382753015,2.68204519134619));
#230307=CARTESIAN_POINT('Ctrl Pts',(41.9638869554865,46.7529426662696,2.68003431778557));
#230308=CARTESIAN_POINT('Ctrl Pts',(41.9680580970364,46.7519812517997,2.67812693945295));
#230309=CARTESIAN_POINT('Ctrl Pts',(41.968849530518,46.7517988327684,2.67776503299247));
#230310=CARTESIAN_POINT('Ctrl Pts',(41.9696416823157,46.7516099985533,2.67740659639968));
#230311=CARTESIAN_POINT('Ctrl Pts',(41.9704344168203,46.751414714301,2.67705178968899));
#230312=CARTESIAN_POINT('Ctrl Pts',(41.9712023783716,46.7512255326816,2.67670807068802));
#230313=CARTESIAN_POINT('Ctrl Pts',(41.9719708867611,46.7510302978709,2.67636775825309));
#230314=CARTESIAN_POINT('Ctrl Pts',(41.9727398158587,46.7508289807696,2.67603099699299));
#230315=CARTESIAN_POINT('Ctrl Pts',(41.9811194467225,46.748635068482,2.67236104217173));
#230316=CARTESIAN_POINT('Ctrl Pts',(41.9895544525278,46.7457169794824,2.6691144054152));
#230317=CARTESIAN_POINT('Ctrl Pts',(41.9978556152118,46.742053011169,2.66646778189678));
#230318=CARTESIAN_POINT('Ctrl Pts',(42.001361247761,46.740505694598,2.6653500963502));
#230319=CARTESIAN_POINT('Ctrl Pts',(42.0048429302642,46.738825785455,2.66433897912389));
#230320=CARTESIAN_POINT('Ctrl Pts',(42.0082865614562,46.7370135816691,2.66344564884837));
#230321=CARTESIAN_POINT('Ctrl Pts',(42.0140855503366,46.7339618757758,2.6619413029863));
#230322=CARTESIAN_POINT('Ctrl Pts',(42.0197742252485,46.7305342346688,2.66077206705465));
#230323=CARTESIAN_POINT('Ctrl Pts',(42.0252784509104,46.7267341265711,2.6599822515576));
#230324=CARTESIAN_POINT('Ctrl Pts',(42.0266545073259,46.7257840995467,2.65978479768334));
#230325=CARTESIAN_POINT('Ctrl Pts',(42.0280188904107,46.7248106099128,2.65961098966668));
#230326=CARTESIAN_POINT('Ctrl Pts',(42.029370240857,46.7238134778072,2.65946139030547));
#230327=CARTESIAN_POINT('Ctrl Pts',(42.0313972665265,46.7223177796489,2.65923699126366));
#230328=CARTESIAN_POINT('Ctrl Pts',(42.0333949481518,46.720768886388,2.65906707562488));
#230329=CARTESIAN_POINT('Ctrl Pts',(42.0353598072046,46.7191674503113,2.65895332562965));
#230330=CARTESIAN_POINT('Ctrl Pts',(42.0373246662573,46.7175660142347,2.65883957563443));
#230331=CARTESIAN_POINT('Ctrl Pts',(42.0392567035874,46.7159120469178,2.65878198860295));
#230332=CARTESIAN_POINT('Ctrl Pts',(42.0411527846906,46.7142062431438,2.65878198860295));
#230333=CARTESIAN_POINT('Ctrl Pts',(39.4864862581816,43.8769616275877,2.65878198860293));
#230334=CARTESIAN_POINT('Ctrl Pts',(39.4800703482072,43.8827333680739,2.65878198860293));
#230335=CARTESIAN_POINT('Ctrl Pts',(39.4741864828752,43.8889846873401,2.65945335517889));
#230336=CARTESIAN_POINT('Ctrl Pts',(39.4688721660166,43.8955692023378,2.6607256122664));
#230337=CARTESIAN_POINT('Ctrl Pts',(39.4654396626065,43.8998221234159,2.66154735980377));
#230338=CARTESIAN_POINT('Ctrl Pts',(39.462244030967,43.9042134689402,2.66261895766919));
#230339=CARTESIAN_POINT('Ctrl Pts',(39.4592874976153,43.9086997575135,2.66391429251058));
#230340=CARTESIAN_POINT('Ctrl Pts',(39.4553687820182,43.9146460760273,2.66563118464155));
#230341=CARTESIAN_POINT('Ctrl Pts',(39.4518755008533,43.9207613318565,2.6677410513873));
#230342=CARTESIAN_POINT('Ctrl Pts',(39.4488169076809,43.9269559348856,2.67016894181782));
#230343=CARTESIAN_POINT('Ctrl Pts',(39.4472876110947,43.9300532364002,2.67138288703307));
#230344=CARTESIAN_POINT('Ctrl Pts',(39.4458668372381,43.9331705067654,2.67267613167583));
#230345=CARTESIAN_POINT('Ctrl Pts',(39.4445546869048,43.9362974878338,2.67403835432585));
#230346=CARTESIAN_POINT('Ctrl Pts',(39.4438986117382,43.9378609783681,2.67471946565086));
#230347=CARTESIAN_POINT('Ctrl Pts',(39.4432696802089,43.9394269075363,2.67541781389555));
#230348=CARTESIAN_POINT('Ctrl Pts',(39.4426678279634,43.9409940617757,2.67613207244201));
#230349=CARTESIAN_POINT('Ctrl Pts',(39.442517364902,43.9413858503355,2.67631063707863));
#230350=CARTESIAN_POINT('Ctrl Pts',(39.4423685940347,43.9417777156947,2.67649019601877));
#230351=CARTESIAN_POINT('Ctrl Pts',(39.4422215138293,43.9421696393593,2.67667072836689));
#230352=CARTESIAN_POINT('Ctrl Pts',(39.4417802732128,43.9433454103532,2.67721232541123));
#230353=CARTESIAN_POINT('Ctrl Pts',(39.4413542498604,43.9445217049431,2.67776268340079));
#230354=CARTESIAN_POINT('Ctrl Pts',(39.4409433907177,43.9456980341197,2.67832123541549));
#230355=CARTESIAN_POINT('Ctrl Pts',(39.4380493519682,43.9539839449482,2.6822556036848));
#230356=CARTESIAN_POINT('Ctrl Pts',(39.4358558447893,43.9622859173447,2.68661792998926));
#230357=CARTESIAN_POINT('Ctrl Pts',(39.4342768603234,43.9705207686467,2.69130986622619));
#230358=CARTESIAN_POINT('Ctrl Pts',(39.4335110545637,43.9745146626294,2.69358545023093));
#230359=CARTESIAN_POINT('Ctrl Pts',(39.4328901532274,43.9784932254702,2.69593918853504));
#230360=CARTESIAN_POINT('Ctrl Pts',(39.4324063524315,43.9824490059338,2.69836306235507));
#230361=CARTESIAN_POINT('Ctrl Pts',(39.4316656872152,43.9885050294414,2.70207384382239));
#230362=CARTESIAN_POINT('Ctrl Pts',(39.4312456873368,43.9945041897574,2.7059476081424));
#230363=CARTESIAN_POINT('Ctrl Pts',(39.4311218425061,44.0004074287825,2.70995196345719));
#230364=CARTESIAN_POINT('Ctrl Pts',(39.4310643283261,44.0031489235251,2.71181160678117));
#230365=CARTESIAN_POINT('Ctrl Pts',(39.4310704471411,44.0058696426793,2.7136996277211));
#230366=CARTESIAN_POINT('Ctrl Pts',(39.431138952561,44.0085654321303,2.71561183138673));
#230367=CARTESIAN_POINT('Ctrl Pts',(39.4311442032315,44.0087720537697,2.71575839426324));
#230368=CARTESIAN_POINT('Ctrl Pts',(39.4311497894112,44.0089785427601,2.7159050890322));
#230369=CARTESIAN_POINT('Ctrl Pts',(39.431155709954,44.009184898196,2.71605191409923));
#230370=CARTESIAN_POINT('Ctrl Pts',(39.4312388757299,44.0120835699301,2.71811436362764));
#230371=CARTESIAN_POINT('Ctrl Pts',(39.4313901062474,44.0149559644986,2.72020091026971));
#230372=CARTESIAN_POINT('Ctrl Pts',(39.4316052205105,44.0177981990786,2.72230624862194));
#230373=CARTESIAN_POINT('Ctrl Pts',(39.4323765820014,44.0279899468082,2.72985561753132));
#230374=CARTESIAN_POINT('Ctrl Pts',(39.4339733733565,44.0378728316098,2.73770089914377));
#230375=CARTESIAN_POINT('Ctrl Pts',(39.4362681192151,44.047426286633,2.7457482334714));
#230376=CARTESIAN_POINT('Ctrl Pts',(39.4387898143859,44.0579245739738,2.75459144547098));
#230377=CARTESIAN_POINT('Ctrl Pts',(39.442154341227,44.0680257165107,2.76367911754352));
#230378=CARTESIAN_POINT('Ctrl Pts',(39.4462454222063,44.0777053474432,2.77292162564817));
#230379=CARTESIAN_POINT('Ctrl Pts',(39.4506627629427,44.0881569195945,2.78290121484824));
#230380=CARTESIAN_POINT('Ctrl Pts',(39.4559274600944,44.0981181930583,2.79306229500285));
#230381=CARTESIAN_POINT('Ctrl Pts',(39.4619494608007,44.1075472421544,2.80331916685354));
#230382=CARTESIAN_POINT('Ctrl Pts',(39.4679209431084,44.1168971912164,2.81348999408771));
#230383=CARTESIAN_POINT('Ctrl Pts',(39.474638071157,44.1257248429294,2.8237563596693));
#230384=CARTESIAN_POINT('Ctrl Pts',(39.4820551873929,44.133962385045,2.83404198860293));
#230385=CARTESIAN_POINT('Origin',(0.0113255271402773,-0.0101975504407237,
2.83404198860262));
#230386=CARTESIAN_POINT('Ctrl Pts',(42.06380383897,46.6938111422607,2.65878198860295));
#230387=CARTESIAN_POINT('Ctrl Pts',(42.0701842568306,46.6880613546458,2.65878198860295));
#230388=CARTESIAN_POINT('Ctrl Pts',(42.0760276657225,46.6818296739374,2.6594460304188));
#230389=CARTESIAN_POINT('Ctrl Pts',(42.0812997491645,46.6752630175677,2.66070439264092));
#230390=CARTESIAN_POINT('Ctrl Pts',(42.084668359505,46.6710672367549,2.66150842619618));
#230391=CARTESIAN_POINT('Ctrl Pts',(42.0878044626438,46.6667352666012,2.66255428265393));
#230392=CARTESIAN_POINT('Ctrl Pts',(42.0907067742416,46.6623093164291,2.66381699700685));
#230393=CARTESIAN_POINT('Ctrl Pts',(42.0946678472191,46.6562687825186,2.66554034873284));
#230394=CARTESIAN_POINT('Ctrl Pts',(42.0981877352865,46.6500510792884,2.66766759643988));
#230395=CARTESIAN_POINT('Ctrl Pts',(42.1012583942265,46.643751530039,2.67012012783163));
#230396=CARTESIAN_POINT('Ctrl Pts',(42.1027937236965,46.6406017554143,2.67134639352751));
#230397=CARTESIAN_POINT('Ctrl Pts',(42.1042169023589,46.637431380974,2.67265375585027));
#230398=CARTESIAN_POINT('Ctrl Pts',(42.1055280393689,46.6342513293849,2.67403135126955));
#230399=CARTESIAN_POINT('Ctrl Pts',(42.1061836078739,46.6326613035904,2.67472014897919));
#230400=CARTESIAN_POINT('Ctrl Pts',(42.1068111789407,46.6310688468942,2.67542649668648));
#230401=CARTESIAN_POINT('Ctrl Pts',(42.1074108478354,46.6294752517396,2.67614899656117));
#230402=CARTESIAN_POINT('Ctrl Pts',(42.107560765059,46.629076852951,2.67632962152984));
#230403=CARTESIAN_POINT('Ctrl Pts',(42.1077089386741,46.628678382762,2.67651125590965));
#230404=CARTESIAN_POINT('Ctrl Pts',(42.1078553707282,46.6282798608701,2.67669387767539));
#230405=CARTESIAN_POINT('Ctrl Pts',(42.1082946668907,46.6270842951944,2.67724174297259));
#230406=CARTESIAN_POINT('Ctrl Pts',(42.1087182876164,46.6258882654173,2.67779849504762));
#230407=CARTESIAN_POINT('Ctrl Pts',(42.109126300596,46.6246922924068,2.67836353618024));
#230408=CARTESIAN_POINT('Ctrl Pts',(42.1119459234385,46.616427376857,2.68226832098914));
#230409=CARTESIAN_POINT('Ctrl Pts',(42.1140735600937,46.6081492165692,2.68659153751386));
#230410=CARTESIAN_POINT('Ctrl Pts',(42.1155964444647,46.5999384432824,2.69123699486161));
#230411=CARTESIAN_POINT('Ctrl Pts',(42.116353313817,46.5958577114966,2.6935457744121));
#230412=CARTESIAN_POINT('Ctrl Pts',(42.1169604217533,46.5917931497418,2.69593478828122));
#230413=CARTESIAN_POINT('Ctrl Pts',(42.1174262136792,46.5877524553607,2.69839565261236));
#230414=CARTESIAN_POINT('Ctrl Pts',(42.11845382024,46.5788380800231,2.70382468689062));
#230415=CARTESIAN_POINT('Ctrl Pts',(42.1188058546738,46.570042246956,2.70961155815103));
#230416=CARTESIAN_POINT('Ctrl Pts',(42.1185337834653,46.5615008914346,2.71562701361784));
#230417=CARTESIAN_POINT('Ctrl Pts',(42.1184343924219,46.5583806265504,2.71782453535875));
#230418=CARTESIAN_POINT('Ctrl Pts',(42.1182588963863,46.555290896183,2.72005051502419));
#230419=CARTESIAN_POINT('Ctrl Pts',(42.1180117795242,46.552234552633,2.72229986760133));
#230420=CARTESIAN_POINT('Ctrl Pts',(42.1171817401336,46.5419686180608,2.72985520488881));
#230421=CARTESIAN_POINT('Ctrl Pts',(42.1155299964535,46.5320149571611,2.73770845534515));
#230422=CARTESIAN_POINT('Ctrl Pts',(42.1131831104089,46.5223946380452,2.74576706701676));
#230423=CARTESIAN_POINT('Ctrl Pts',(42.1106036046389,46.511820767735,2.75462443584922));
#230424=CARTESIAN_POINT('Ctrl Pts',(42.107184320974,46.5016489045637,2.76373036323042));
#230425=CARTESIAN_POINT('Ctrl Pts',(42.103040283974,46.4919044745669,2.77299664636647));
#230426=CARTESIAN_POINT('Ctrl Pts',(42.0985769785671,46.4814093059446,2.78297683033278));
#230427=CARTESIAN_POINT('Ctrl Pts',(42.0932726122948,46.4714088200601,2.79314401478671));
#230428=CARTESIAN_POINT('Ctrl Pts',(42.0872150940887,46.4619468343642,2.80341452427691));
#230429=CARTESIAN_POINT('Ctrl Pts',(42.0812393728308,46.4526126174223,2.81354634721203));
#230430=CARTESIAN_POINT('Ctrl Pts',(42.0745296860258,46.4438014421038,2.82378004209136));
#230431=CARTESIAN_POINT('Ctrl Pts',(42.0671296588095,46.4355828792673,2.83404198860295));
#230432=CARTESIAN_POINT('Ctrl Pts',(39.7651933658998,43.8790236240223,2.83404198860292));
#230433=CARTESIAN_POINT('Ctrl Pts',(39.7581114992313,43.8711584142718,2.82422126443018));
#230434=CARTESIAN_POINT('Ctrl Pts',(39.7504347382248,43.8638800583564,2.81442815028494));
#230435=CARTESIAN_POINT('Ctrl Pts',(39.7422106539902,43.8572218328528,2.80471618166292));
#230436=CARTESIAN_POINT('Ctrl Pts',(39.734269577075,43.8507927303126,2.79533842146191));
#230437=CARTESIAN_POINT('Ctrl Pts',(39.7258171668685,43.8449410790334,2.78603515650188));
#230438=CARTESIAN_POINT('Ctrl Pts',(39.7168657021537,43.8397310304445,2.77685887346692));
#230439=CARTESIAN_POINT('Ctrl Pts',(39.7084037645731,43.8348059028418,2.76818441216503));
#230440=CARTESIAN_POINT('Ctrl Pts',(39.6994950821773,43.83045366822,2.7596226152154));
#230441=CARTESIAN_POINT('Ctrl Pts',(39.6901349804713,43.8267676847806,2.75123537701567));
#230442=CARTESIAN_POINT('Ctrl Pts',(39.6815144838276,43.8233729558699,2.74351087134018));
#230443=CARTESIAN_POINT('Ctrl Pts',(39.6725105620397,43.8205432023694,2.7359339944974));
#230444=CARTESIAN_POINT('Ctrl Pts',(39.6631152739599,43.8183892419678,2.72857657812464));
#230445=CARTESIAN_POINT('Ctrl Pts',(39.6603137887123,43.8177469744569,2.72638274508255));
#230446=CARTESIAN_POINT('Ctrl Pts',(39.6574775031707,43.8171650742228,2.72420861709576));
#230447=CARTESIAN_POINT('Ctrl Pts',(39.654606226052,43.8166472411073,2.72205663736739));
#230448=CARTESIAN_POINT('Ctrl Pts',(39.6517642863086,43.8161346989698,2.71992664556778));
#230449=CARTESIAN_POINT('Ctrl Pts',(39.6488910639689,43.8156851836084,2.71782089927897));
#230450=CARTESIAN_POINT('Ctrl Pts',(39.6459896850503,43.8153025584994,2.71574387311258));
#230451=CARTESIAN_POINT('Ctrl Pts',(39.6457879288345,43.8152759514976,2.71559944077499));
#230452=CARTESIAN_POINT('Ctrl Pts',(39.6455860324536,43.8152496566737,2.71545515216081));
#230453=CARTESIAN_POINT('Ctrl Pts',(39.6453839959665,43.8152236753308,2.71531100781743));
#230454=CARTESIAN_POINT('Ctrl Pts',(39.6365259762554,43.8140845580784,2.7089911917609));
#230455=CARTESIAN_POINT('Ctrl Pts',(39.6274037177901,43.8135929685792,2.70298296066839));
#230456=CARTESIAN_POINT('Ctrl Pts',(39.6180980992372,43.8138323099901,2.69736727774132));
#230457=CARTESIAN_POINT('Ctrl Pts',(39.6094236454403,43.8140554177823,2.69213248525419));
#230458=CARTESIAN_POINT('Ctrl Pts',(39.6005890951397,43.8149139527619,2.68723866185454));
#230459=CARTESIAN_POINT('Ctrl Pts',(39.5916773623189,43.8164991115146,2.68278595829545));
#230460=CARTESIAN_POINT('Ctrl Pts',(39.5884173351601,43.8170789830939,2.68115710172796));
#230461=CARTESIAN_POINT('Ctrl Pts',(39.5851472105417,43.8177563121468,2.67958763637809));
#230462=CARTESIAN_POINT('Ctrl Pts',(39.5818719865444,43.8185363400629,2.67808378645371));
#230463=CARTESIAN_POINT('Ctrl Pts',(39.5810844045886,43.8187239107184,2.67772216078606));
#230464=CARTESIAN_POINT('Ctrl Pts',(39.5802961412321,43.8189178575373,2.67736403603569));
#230465=CARTESIAN_POINT('Ctrl Pts',(39.5795073285708,43.8191182115053,2.67700956934485));
#230466=CARTESIAN_POINT('Ctrl Pts',(39.5787431663051,43.8193123044117,2.6766661797381));
#230467=CARTESIAN_POINT('Ctrl Pts',(39.577978488548,43.8195124102601,2.67632622314124));
#230468=CARTESIAN_POINT('Ctrl Pts',(39.5772134181964,43.8197185546681,2.67598984158779));
#230469=CARTESIAN_POINT('Ctrl Pts',(39.5688311883234,43.8219771048932,2.67230439292236));
#230470=CARTESIAN_POINT('Ctrl Pts',(39.5603964284877,43.8249623840155,2.66904964539998));
#230471=CARTESIAN_POINT('Ctrl Pts',(39.5520968239724,43.8286919494552,2.66640203566753));
#230472=CARTESIAN_POINT('Ctrl Pts',(39.5486547305949,43.8302387114097,2.6653039929946));
#230473=CARTESIAN_POINT('Ctrl Pts',(39.5452359574131,43.8319130705227,2.66430995142272));
#230474=CARTESIAN_POINT('Ctrl Pts',(39.5418537500316,43.8337144555752,2.66343053473367));
#230475=CARTESIAN_POINT('Ctrl Pts',(39.5360850428918,43.8367869054997,2.66193059792891));
#230476=CARTESIAN_POINT('Ctrl Pts',(39.5304250803199,43.8402296473865,2.66076519817135));
#230477=CARTESIAN_POINT('Ctrl Pts',(39.5249464846905,43.8440378929944,2.65997805604468));
#230478=CARTESIAN_POINT('Ctrl Pts',(39.5222071868758,43.8459420157983,2.65958448498134));
#230479=CARTESIAN_POINT('Ctrl Pts',(39.5195141476136,43.847938633807,2.65928526260771));
#230480=CARTESIAN_POINT('Ctrl Pts',(39.5168765098751,43.8500271570784,2.65908463971333));
#230481=CARTESIAN_POINT('Ctrl Pts',(39.5142388721366,43.8521156803497,2.65888401681895));
#230482=CARTESIAN_POINT('Ctrl Pts',(39.5116566557597,43.8542960677576,2.65878198860293));
#230483=CARTESIAN_POINT('Ctrl Pts',(39.5091373124622,43.8565665267059,2.65878198860293));
#230484=CARTESIAN_POINT('Origin',(34.2342565846635,47.1453396605411,2.83404198860295));
#230485=CARTESIAN_POINT('Ctrl Pts',(36.6746059268177,50.8023624960594,2.83404198860298));
#230486=CARTESIAN_POINT('Ctrl Pts',(36.6808425220336,50.8109464329599,2.82419652440128));
#230487=CARTESIAN_POINT('Ctrl Pts',(36.6877379133664,50.8190128116683,2.81438790575741));
#230488=CARTESIAN_POINT('Ctrl Pts',(36.6952462569238,50.8265243508953,2.80466781257023));
#230489=CARTESIAN_POINT('Ctrl Pts',(36.7025106240248,50.8337918098257,2.79526356453224));
#230490=CARTESIAN_POINT('Ctrl Pts',(36.7103497152242,50.8405407635273,2.78594102496402));
#230491=CARTESIAN_POINT('Ctrl Pts',(36.7187568768209,50.8467071440065,2.77675109088972));
#230492=CARTESIAN_POINT('Ctrl Pts',(36.7267095340082,50.8525401602359,2.76805797913899));
#230493=CARTESIAN_POINT('Ctrl Pts',(36.7351712462813,50.8578524412739,2.759482712104));
#230494=CARTESIAN_POINT('Ctrl Pts',(36.7441560526514,50.8625525281326,2.75108575573482));
#230495=CARTESIAN_POINT('Ctrl Pts',(36.752431709116,50.8668816480485,2.7433515516355));
#230496=CARTESIAN_POINT('Ctrl Pts',(36.7611516658447,50.8706916079184,2.73576818686243));
#230497=CARTESIAN_POINT('Ctrl Pts',(36.7703354510145,50.8738736606197,2.72840626160814));
#230498=CARTESIAN_POINT('Ctrl Pts',(36.7729993179912,50.8747966531497,2.72627084693901));
#230499=CARTESIAN_POINT('Ctrl Pts',(36.7757022424569,50.8756665488981,2.7241542458765));
#230500=CARTESIAN_POINT('Ctrl Pts',(36.7784447603818,50.8764799968255,2.72205867173293));
#230501=CARTESIAN_POINT('Ctrl Pts',(36.7814178261393,50.8773618266784,2.71978693462896));
#230502=CARTESIAN_POINT('Ctrl Pts',(36.7844329791247,50.8781771258726,2.71754411340797));
#230503=CARTESIAN_POINT('Ctrl Pts',(36.7874899206174,50.8789219044956,2.71533341844294));
#230504=CARTESIAN_POINT('Ctrl Pts',(36.7958797205316,50.8809659552705,2.70926614876441));
#230505=CARTESIAN_POINT('Ctrl Pts',(36.8045837617103,50.8824343655145,2.70347381860458));
#230506=CARTESIAN_POINT('Ctrl Pts',(36.8135226609478,50.8832604021664,2.69804914171444));
#230507=CARTESIAN_POINT('Ctrl Pts',(36.8217012684459,50.8840161808562,2.69308585687253));
#230508=CARTESIAN_POINT('Ctrl Pts',(36.8300699399858,50.8842246658556,2.68842799053233));
#230509=CARTESIAN_POINT('Ctrl Pts',(36.838587648015,50.883807280293,2.68414767054265));
#230510=CARTESIAN_POINT('Ctrl Pts',(36.8427715183746,50.8836022618681,2.68204519134601));
#230511=CARTESIAN_POINT('Ctrl Pts',(36.8469911418449,50.8832457706971,2.68003431778553));
#230512=CARTESIAN_POINT('Ctrl Pts',(36.8512399286217,50.8827256259727,2.67812693945304));
#230513=CARTESIAN_POINT('Ctrl Pts',(36.8520460945289,50.8826269335775,2.67776503299256));
#230514=CARTESIAN_POINT('Ctrl Pts',(36.8528536453865,50.8825219362261,2.67740659639976));
#230515=CARTESIAN_POINT('Ctrl Pts',(36.8536624499713,50.8824105850809,2.67705178968908));
#230516=CARTESIAN_POINT('Ctrl Pts',(36.8544459794128,50.882302713659,2.6767080706881));
#230517=CARTESIAN_POINT('Ctrl Pts',(36.8552306854278,50.8821888793659,2.67636775825318));
#230518=CARTESIAN_POINT('Ctrl Pts',(36.8560164456185,50.8820690400777,2.67603099699308));
#230519=CARTESIAN_POINT('Ctrl Pts',(36.8645794982675,50.8807630562082,2.67236104217187));
#230520=CARTESIAN_POINT('Ctrl Pts',(36.8732733195871,50.878742651,2.66911440541537));
#230521=CARTESIAN_POINT('Ctrl Pts',(36.8819119966105,50.8759664620671,2.66646778189695));
#230522=CARTESIAN_POINT('Ctrl Pts',(36.8855601635613,50.8747940602413,2.66535009635033));
#230523=CARTESIAN_POINT('Ctrl Pts',(36.8891983713647,50.873487288738,2.66433897912399));
#230524=CARTESIAN_POINT('Ctrl Pts',(36.8928125648617,50.8720449698706,2.66344564884844));
#230525=CARTESIAN_POINT('Ctrl Pts',(36.8988987764016,50.8696161409376,2.66194130298636));
#230526=CARTESIAN_POINT('Ctrl Pts',(36.9049145742147,50.8668019052538,2.6607720670547));
#230527=CARTESIAN_POINT('Ctrl Pts',(36.9107858666119,50.8635979627953,2.65998225155764));
#230528=CARTESIAN_POINT('Ctrl Pts',(36.9122536897112,50.8627969771806,2.65978479768337));
#230529=CARTESIAN_POINT('Ctrl Pts',(36.9137123559382,50.861971437292,2.65961098966672));
#230530=CARTESIAN_POINT('Ctrl Pts',(36.915160532232,50.861121022166,2.65946139030551));
#230531=CARTESIAN_POINT('Ctrl Pts',(36.9173327966728,50.859845399477,2.65923699126369));
#230532=CARTESIAN_POINT('Ctrl Pts',(36.9194814382216,50.8585138058059,2.65906707562491));
#230533=CARTESIAN_POINT('Ctrl Pts',(36.921602929223,50.8571265262611,2.65895332562968));
#230534=CARTESIAN_POINT('Ctrl Pts',(36.9237244202244,50.8557392467162,2.65883957563446));
#230535=CARTESIAN_POINT('Ctrl Pts',(36.9258187603129,50.8542962928972,2.65878198860298));
#230536=CARTESIAN_POINT('Ctrl Pts',(36.9278827595326,50.8527980281388,2.65878198860298));
#230537=CARTESIAN_POINT('Ctrl Pts',(34.6837837831345,47.7640607692766,2.65878198860296));
#230538=CARTESIAN_POINT('Ctrl Pts',(34.6767997090223,47.7691302463548,2.65878198860296));
#230539=CARTESIAN_POINT('Ctrl Pts',(34.6702946353236,47.7747322888391,2.65945335517902));
#230540=CARTESIAN_POINT('Ctrl Pts',(34.6643211616144,47.7807252358007,2.66072561226671));
#230541=CARTESIAN_POINT('Ctrl Pts',(34.6604629105129,47.784596064625,2.66154735980404));
#230542=CARTESIAN_POINT('Ctrl Pts',(34.656825764279,47.7886293194342,2.66261895766936));
#230543=CARTESIAN_POINT('Ctrl Pts',(34.6534164822763,47.792781989761,2.66391429251062));
#230544=CARTESIAN_POINT('Ctrl Pts',(34.6488976742769,47.7982861164004,2.66563118464159));
#230545=CARTESIAN_POINT('Ctrl Pts',(34.6447843113774,47.8040027249065,2.66774105138734));
#230546=CARTESIAN_POINT('Ctrl Pts',(34.6410949611633,47.809843683208,2.67016894181786));
#230547=CARTESIAN_POINT('Ctrl Pts',(34.6392502860562,47.8127641623587,2.67138288703311));
#230548=CARTESIAN_POINT('Ctrl Pts',(34.6375114518666,47.8157158446828,2.67267613167587));
#230549=CARTESIAN_POINT('Ctrl Pts',(34.6358796311044,47.8186885387639,2.67403835432589));
#230550=CARTESIAN_POINT('Ctrl Pts',(34.6350637207233,47.8201748858044,2.6747194656509));
#230551=CARTESIAN_POINT('Ctrl Pts',(34.6342745503772,47.8216664954026,2.6754178138956));
#230552=CARTESIAN_POINT('Ctrl Pts',(34.6335121829169,47.8231621539168,2.67613207244206));
#230553=CARTESIAN_POINT('Ctrl Pts',(34.6333215910518,47.8235360685453,2.67631063707867));
#230554=CARTESIAN_POINT('Ctrl Pts',(34.6331326740831,47.8239102364348,2.67649019601882));
#230555=CARTESIAN_POINT('Ctrl Pts',(34.63294543242,47.8242846390328,2.67667072836694));
#230556=CARTESIAN_POINT('Ctrl Pts',(34.6323837074307,47.8254078468266,2.67721232541128));
#230557=CARTESIAN_POINT('Ctrl Pts',(34.6318370616129,47.8265331659853,2.67776268340084));
#230558=CARTESIAN_POINT('Ctrl Pts',(34.6313054933184,47.8276601046328,2.67832123541553));
#230559=CARTESIAN_POINT('Ctrl Pts',(34.6275611948903,47.8355981149517,2.68225560368485));
#230560=CARTESIAN_POINT('Ctrl Pts',(34.6245119115566,47.8436253243401,2.68661792998933));
#230561=CARTESIAN_POINT('Ctrl Pts',(34.622080800581,47.8516500154454,2.69130986622627));
#230562=CARTESIAN_POINT('Ctrl Pts',(34.6209017143848,47.8555419819597,2.69358545023099));
#230563=CARTESIAN_POINT('Ctrl Pts',(34.6198683413513,47.8594338479544,2.69593918853509));
#230564=CARTESIAN_POINT('Ctrl Pts',(34.618973699214,47.8633173872851,2.6983630623551));
#230565=CARTESIAN_POINT('Ctrl Pts',(34.6176040646085,47.8692628146653,2.70207384382242));
#230566=CARTESIAN_POINT('Ctrl Pts',(34.6165592825246,47.8751852090115,2.70594760814242));
#230567=CARTESIAN_POINT('Ctrl Pts',(34.6158190596252,47.8810431641658,2.70995196345722));
#230568=CARTESIAN_POINT('Ctrl Pts',(34.6154752962814,47.8837636288445,2.71181160678119));
#230569=CARTESIAN_POINT('Ctrl Pts',(34.6151969889848,47.8864700832049,2.71369962772113));
#230570=CARTESIAN_POINT('Ctrl Pts',(34.6149833323962,47.8891582656054,2.71561183138676));
#230571=CARTESIAN_POINT('Ctrl Pts',(34.6149669564605,47.8893643041944,2.71575839426326));
#230572=CARTESIAN_POINT('Ctrl Pts',(34.6149509280617,47.8895702459312,2.71590508903223));
#230573=CARTESIAN_POINT('Ctrl Pts',(34.6149352461545,47.8897760897958,2.71605191409926));
#230574=CARTESIAN_POINT('Ctrl Pts',(34.6147149626377,47.8926675754935,2.71811436362768));
#230575=CARTESIAN_POINT('Ctrl Pts',(34.6145651177085,47.8955400426776,2.72020091026974));
#230576=CARTESIAN_POINT('Ctrl Pts',(34.6144819591403,47.8983891927626,2.72230624862197));
#230577=CARTESIAN_POINT('Ctrl Pts',(34.614183767304,47.9086057382621,2.72985561753074));
#230578=CARTESIAN_POINT('Ctrl Pts',(34.614738768508,47.9186013937325,2.73770089914255));
#230579=CARTESIAN_POINT('Ctrl Pts',(34.6160223355359,47.9283423801869,2.7457482334695));
#230580=CARTESIAN_POINT('Ctrl Pts',(34.6174328467539,47.9390467457313,2.75459144546827));
#230581=CARTESIAN_POINT('Ctrl Pts',(34.6197230854579,47.9494442419719,2.76367911753994));
#230582=CARTESIAN_POINT('Ctrl Pts',(34.6227799581206,47.9594984812804,2.7729216256437));
#230583=CARTESIAN_POINT('Ctrl Pts',(34.6260806134258,47.9703545364636,2.78290121484248));
#230584=CARTESIAN_POINT('Ctrl Pts',(34.6302752334074,47.9808115517308,2.79306229499576));
#230585=CARTESIAN_POINT('Ctrl Pts',(34.6352786409506,47.9908184179881,2.80331916684511));
#230586=CARTESIAN_POINT('Ctrl Pts',(34.6402400750473,48.0007413369228,2.81348999408205));
#230587=CARTESIAN_POINT('Ctrl Pts',(34.6459976650991,48.0102227609114,2.82375635966647));
#230588=CARTESIAN_POINT('Ctrl Pts',(34.6525130919796,48.0191904766739,2.83404198860296));
#230589=CARTESIAN_POINT('Origin',(0.0123294189942765,-0.00895784724475234,
2.83404198860262));
#230590=CARTESIAN_POINT('Ctrl Pts',(36.9525415975211,50.8348823336489,2.65878198860297));
#230591=CARTESIAN_POINT('Ctrl Pts',(36.9594880792487,50.8298309792461,2.65878198860297));
#230592=CARTESIAN_POINT('Ctrl Pts',(36.9659508653433,50.8242442388882,2.65944603041884));
#230593=CARTESIAN_POINT('Ctrl Pts',(36.9718804702599,50.8182646381295,2.660704392641));
#230594=CARTESIAN_POINT('Ctrl Pts',(36.975669205521,50.8144439579054,2.66150842619626));
#230595=CARTESIAN_POINT('Ctrl Pts',(36.9792409429416,50.8104635307793,2.662554282654));
#230596=CARTESIAN_POINT('Ctrl Pts',(36.9825899931428,50.8063652005967,2.6638169970069));
#230597=CARTESIAN_POINT('Ctrl Pts',(36.987160774675,50.8007718022342,2.6655403487329));
#230598=CARTESIAN_POINT('Ctrl Pts',(36.9913113073909,50.7949560887233,2.66766759643995));
#230599=CARTESIAN_POINT('Ctrl Pts',(36.9950236271423,50.7890120203241,2.67012012783171));
#230600=CARTESIAN_POINT('Ctrl Pts',(36.996879787018,50.7860399861245,2.67134639352759));
#230601=CARTESIAN_POINT('Ctrl Pts',(36.998626563727,50.7830357420057,2.67265375585035));
#230602=CARTESIAN_POINT('Ctrl Pts',(37.000262924097,50.7800101622087,2.67403135126963));
#230603=CARTESIAN_POINT('Ctrl Pts',(37.001081104282,50.7784973723102,2.67472014897927));
#230604=CARTESIAN_POINT('Ctrl Pts',(37.0018716945001,50.7769792382976,2.67542649668655));
#230605=CARTESIAN_POINT('Ctrl Pts',(37.0026346543984,50.7754570554921,2.67614899656125));
#230606=CARTESIAN_POINT('Ctrl Pts',(37.002825394373,50.7750765097907,2.67632962152992));
#230607=CARTESIAN_POINT('Ctrl Pts',(37.0030144077539,50.7746957108234,2.67651125590973));
#230608=CARTESIAN_POINT('Ctrl Pts',(37.0032016945189,50.7743146783937,2.67669387767546));
#230609=CARTESIAN_POINT('Ctrl Pts',(37.0037635548139,50.7731715811047,2.67724174297267));
#230610=CARTESIAN_POINT('Ctrl Pts',(37.0043098740556,50.7720263837273,2.6777984950477));
#230611=CARTESIAN_POINT('Ctrl Pts',(37.0048406651182,50.7708796113518,2.67836353618031));
#230612=CARTESIAN_POINT('Ctrl Pts',(37.0085087606933,50.7629547027167,2.6822683209893));
#230613=CARTESIAN_POINT('Ctrl Pts',(37.011490045306,50.7549442896469,2.68659153751414));
#230614=CARTESIAN_POINT('Ctrl Pts',(37.013862846671,50.7469376805981,2.69123699486201));
#230615=CARTESIAN_POINT('Ctrl Pts',(37.0150421224362,50.7429584178785,2.69354577441238));
#230616=CARTESIAN_POINT('Ctrl Pts',(37.0160707669658,50.738979582278,2.69593478828138));
#230617=CARTESIAN_POINT('Ctrl Pts',(37.0169563748089,50.7350097117579,2.69839565261239));
#230618=CARTESIAN_POINT('Ctrl Pts',(37.0189101579885,50.7262515844358,2.70382468689064));
#230619=CARTESIAN_POINT('Ctrl Pts',(37.0201796788545,50.717540733481,2.70961155815106));
#230620=CARTESIAN_POINT('Ctrl Pts',(37.0208019128474,50.7090177292134,2.71562701361786));
#230621=CARTESIAN_POINT('Ctrl Pts',(37.0210292227719,50.7059041682737,2.71782453535876));
#230622=CARTESIAN_POINT('Ctrl Pts',(37.0211776528892,50.7028130194417,2.72005051502421));
#230623=CARTESIAN_POINT('Ctrl Pts',(37.0212513646536,50.6997475881156,2.72229986760134));
#230624=CARTESIAN_POINT('Ctrl Pts',(37.0214989546703,50.6894511286653,2.72985520488865));
#230625=CARTESIAN_POINT('Ctrl Pts',(37.0208967002927,50.6793793407332,2.73770845534483));
#230626=CARTESIAN_POINT('Ctrl Pts',(37.0195682679088,50.6695664063405,2.74576706701628));
#230627=CARTESIAN_POINT('Ctrl Pts',(37.0181081633557,50.6587808290243,2.75462443584856));
#230628=CARTESIAN_POINT('Ctrl Pts',(37.0157708601105,50.6483072759169,2.76373036322957));
#230629=CARTESIAN_POINT('Ctrl Pts',(37.0126680948719,50.6381830571081,2.77299664636543));
#230630=CARTESIAN_POINT('Ctrl Pts',(37.009326283767,50.6272788396627,2.78297683033147));
#230631=CARTESIAN_POINT('Ctrl Pts',(37.0050963107899,50.6167786802315,2.7931440147851));
#230632=CARTESIAN_POINT('Ctrl Pts',(37.0000610231269,50.6067353452142,2.80341452427499));
#230633=CARTESIAN_POINT('Ctrl Pts',(36.9950937288478,50.5968276291287,2.81354634721077));
#230634=CARTESIAN_POINT('Ctrl Pts',(36.9893418170244,50.5873633690991,2.82378004209075));
#230635=CARTESIAN_POINT('Ctrl Pts',(36.9828414016746,50.578416314936,2.83404198860297));
#230636=CARTESIAN_POINT('Ctrl Pts',(34.9607485668365,47.7952442955505,2.83404198860296));
#230637=CARTESIAN_POINT('Ctrl Pts',(34.9545276336629,47.7866819156019,2.8242212644301));
#230638=CARTESIAN_POINT('Ctrl Pts',(34.9476537221154,47.7786409912509,2.81442815028473));
#230639=CARTESIAN_POINT('Ctrl Pts',(34.9401706643545,47.7711595893163,2.8047161816626));
#230640=CARTESIAN_POINT('Ctrl Pts',(34.9329451136982,47.7639356375058,2.7953384214615));
#230641=CARTESIAN_POINT('Ctrl Pts',(34.925150670795,47.7572325247347,2.7860351565014));
#230642=CARTESIAN_POINT('Ctrl Pts',(34.9167928415129,47.7511153344865,2.77685887346636));
#230643=CARTESIAN_POINT('Ctrl Pts',(34.9088920753314,47.7453326739165,2.76818441216439));
#230644=CARTESIAN_POINT('Ctrl Pts',(34.9004871280265,47.7400730704108,2.7596226152147));
#230645=CARTESIAN_POINT('Ctrl Pts',(34.8915635921215,47.735428882127,2.7512353770149));
#230646=CARTESIAN_POINT('Ctrl Pts',(34.8833451652565,47.7311516626297,2.74351087133933));
#230647=CARTESIAN_POINT('Ctrl Pts',(34.874686357679,47.7273962447071,2.73593399449646));
#230648=CARTESIAN_POINT('Ctrl Pts',(34.8655676881409,47.724272008901,2.72857657812362));
#230649=CARTESIAN_POINT('Ctrl Pts',(34.8628486849589,47.7233404248511,2.72638274508189));
#230650=CARTESIAN_POINT('Ctrl Pts',(34.8600887620239,47.7224652397585,2.72420861709545));
#230651=CARTESIAN_POINT('Ctrl Pts',(34.857287342362,47.7216501132022,2.72205663736741));
#230652=CARTESIAN_POINT('Ctrl Pts',(34.8545145463038,47.7208433152301,2.71992664556781));
#230653=CARTESIAN_POINT('Ctrl Pts',(34.8517040509267,47.720095928845,2.71782089927899));
#230654=CARTESIAN_POINT('Ctrl Pts',(34.84885856128,47.7194121231168,2.7157438731126));
#230655=CARTESIAN_POINT('Ctrl Pts',(34.8486606914949,47.7193645726037,2.71559944077501));
#230656=CARTESIAN_POINT('Ctrl Pts',(34.848462649681,47.7193173179072,2.71545515216084));
#230657=CARTESIAN_POINT('Ctrl Pts',(34.8482644357608,47.7192703603292,2.71531100781745));
#230658=CARTESIAN_POINT('Ctrl Pts',(34.8395740113843,47.7172115680924,2.70899119176087));
#230659=CARTESIAN_POINT('Ctrl Pts',(34.8305531107002,47.7157691359129,2.70298296066831));
#230660=CARTESIAN_POINT('Ctrl Pts',(34.8212734513094,47.7150344641794,2.6973672777412));
#230661=CARTESIAN_POINT('Ctrl Pts',(34.8126231959631,47.7143496224387,2.69213248525395));
#230662=CARTESIAN_POINT('Ctrl Pts',(34.8037473009111,47.7142799923074,2.68723866185419));
#230663=CARTESIAN_POINT('Ctrl Pts',(34.7947186932864,47.7149249376578,2.68278595829501));
#230664=CARTESIAN_POINT('Ctrl Pts',(34.7914159118127,47.7151608670108,2.68115710172771));
#230665=CARTESIAN_POINT('Ctrl Pts',(34.7880929011145,47.7154926644832,2.679587636378));
#230666=CARTESIAN_POINT('Ctrl Pts',(34.7847540840179,47.7159260651935,2.67808378645377));
#230667=CARTESIAN_POINT('Ctrl Pts',(34.7839512100461,47.7160302835857,2.67772216078612));
#230668=CARTESIAN_POINT('Ctrl Pts',(34.7831469919157,47.7161407719863,2.67736403603575));
#230669=CARTESIAN_POINT('Ctrl Pts',(34.7823415577603,47.716257575019,2.67700956934491));
#230670=CARTESIAN_POINT('Ctrl Pts',(34.7815612934223,47.7163707279569,2.67666617973816));
#230671=CARTESIAN_POINT('Ctrl Pts',(34.7807798878931,47.7164898070136,2.67632622314131));
#230672=CARTESIAN_POINT('Ctrl Pts',(34.7799974607188,47.7166148505128,2.67598984158786));
#230673=CARTESIAN_POINT('Ctrl Pts',(34.771425066794,47.7179848465561,2.67230439292247));
#230674=CARTESIAN_POINT('Ctrl Pts',(34.7627244668162,47.7200720995233,2.66904964540012));
#230675=CARTESIAN_POINT('Ctrl Pts',(34.7540804826589,47.7229136891076,2.66640203566768));
#230676=CARTESIAN_POINT('Ctrl Pts',(34.7504955647788,47.7240921810071,2.66530399299471));
#230677=CARTESIAN_POINT('Ctrl Pts',(34.7469205018091,47.7254000086987,2.66430995142279));
#230678=CARTESIAN_POINT('Ctrl Pts',(34.743368526502,47.7268379886355,2.66343053473372));
#230679=CARTESIAN_POINT('Ctrl Pts',(34.7373102624745,47.7292906132654,2.66193059792896));
#230680=CARTESIAN_POINT('Ctrl Pts',(34.731321441251,47.7321228682622,2.66076519817139));
#230681=CARTESIAN_POINT('Ctrl Pts',(34.7254747878806,47.7353375827203,2.65997805604471));
#230682=CARTESIAN_POINT('Ctrl Pts',(34.7225514611955,47.7369449399493,2.65958448498138));
#230683=CARTESIAN_POINT('Ctrl Pts',(34.7196644712719,47.7386491210201,2.65928526260774));
#230684=CARTESIAN_POINT('Ctrl Pts',(34.7168229726608,47.7404504949229,2.65908463971336));
#230685=CARTESIAN_POINT('Ctrl Pts',(34.7139814740498,47.7422518688257,2.65888401681898));
#230686=CARTESIAN_POINT('Ctrl Pts',(34.7111854907792,47.7441503967334,2.65878198860296));
#230687=CARTESIAN_POINT('Ctrl Pts',(34.7084426211231,47.7461450747867,2.65878198860296));
#230688=CARTESIAN_POINT('Origin',(29.1186878401555,50.4655267888878,2.83404198860297));
#230689=CARTESIAN_POINT('Ctrl Pts',(31.1634057161439,54.3576020372441,2.83404198860299));
#230690=CARTESIAN_POINT('Ctrl Pts',(31.1687108809056,54.3667908521539,2.824196524402));
#230691=CARTESIAN_POINT('Ctrl Pts',(31.1747253323925,54.3755338070552,2.81438790575873));
#230692=CARTESIAN_POINT('Ctrl Pts',(31.1814073748057,54.3837890328978,2.80466781257207));
#230693=CARTESIAN_POINT('Ctrl Pts',(31.1878722906296,54.3917760130573,2.7952635645345));
#230694=CARTESIAN_POINT('Ctrl Pts',(31.1949629807077,54.3993074034407,2.78594102496663));
#230695=CARTESIAN_POINT('Ctrl Pts',(31.2026795247177,54.4063187915243,2.77675109089263));
#230696=CARTESIAN_POINT('Ctrl Pts',(31.2099789001937,54.4129511329149,2.76805797914216));
#230697=CARTESIAN_POINT('Ctrl Pts',(31.2178389737478,54.4191188025019,2.75948271210739));
#230698=CARTESIAN_POINT('Ctrl Pts',(31.2262832675514,54.4247323097956,2.7510857557384));
#230699=CARTESIAN_POINT('Ctrl Pts',(31.2340610728514,54.4299027559922,2.7433515516393));
#230700=CARTESIAN_POINT('Ctrl Pts',(31.2423350114939,54.4346033281798,2.73576818686641));
#230701=CARTESIAN_POINT('Ctrl Pts',(31.2511358718481,54.4387279162142,2.7284062616123));
#230702=CARTESIAN_POINT('Ctrl Pts',(31.2536886668935,54.4399243024168,2.72627084694178));
#230703=CARTESIAN_POINT('Ctrl Pts',(31.2562858555919,54.4410719653267,2.7241542458779));
#230704=CARTESIAN_POINT('Ctrl Pts',(31.2589283212566,54.4421676282861,2.72205867173299));
#230705=CARTESIAN_POINT('Ctrl Pts',(31.2617929239294,54.4433553973776,2.71978693462901));
#230706=CARTESIAN_POINT('Ctrl Pts',(31.2647063376194,54.4444813995855,2.717544113408));
#230707=CARTESIAN_POINT('Ctrl Pts',(31.2676686823018,54.4455416356298,2.71533341844297));
#230708=CARTESIAN_POINT('Ctrl Pts',(31.2757988605279,54.4484514617728,2.70926614876443));
#230709=CARTESIAN_POINT('Ctrl Pts',(31.2843017293921,54.4508216479605,2.7034738186046));
#230710=CARTESIAN_POINT('Ctrl Pts',(31.2931053160624,54.4525775288977,2.69804914171446));
#230711=CARTESIAN_POINT('Ctrl Pts',(31.3011601199078,54.4541840646263,2.6930858568726));
#230712=CARTESIAN_POINT('Ctrl Pts',(31.3094611543727,54.4552661718987,2.68842799053244));
#230713=CARTESIAN_POINT('Ctrl Pts',(31.3179758301774,54.4557414157487,2.68414767054279));
#230714=CARTESIAN_POINT('Ctrl Pts',(31.3221582111184,54.4559748539754,2.68204519134609));
#230715=CARTESIAN_POINT('Ctrl Pts',(31.3263919825241,54.4560613864573,2.68003431778556));
#230716=CARTESIAN_POINT('Ctrl Pts',(31.3306718639313,54.4559882102926,2.67812693945302));
#230717=CARTESIAN_POINT('Ctrl Pts',(31.3314839297417,54.4559743258281,2.67776503299254));
#230718=CARTESIAN_POINT('Ctrl Pts',(31.332298031963,54.4559543157133,2.67740659639975));
#230719=CARTESIAN_POINT('Ctrl Pts',(31.3331140451957,54.4559281176617,2.67705178968906));
#230720=CARTESIAN_POINT('Ctrl Pts',(31.333904558015,54.4559027382991,2.67670807068809));
#230721=CARTESIAN_POINT('Ctrl Pts',(31.3346968642519,54.4558715517161,2.67636775825316));
#230722=CARTESIAN_POINT('Ctrl Pts',(31.3354908465828,54.4558345032253,2.67603099699306));
#230723=CARTESIAN_POINT('Ctrl Pts',(31.3441435024206,54.4554307564064,2.67236104217172));
#230724=CARTESIAN_POINT('Ctrl Pts',(31.3530008879293,54.4543301709716,2.66911440541512));
#230725=CARTESIAN_POINT('Ctrl Pts',(31.3618824321393,54.452472177926,2.66646778189666));
#230726=CARTESIAN_POINT('Ctrl Pts',(31.3656331634107,54.4516875359253,2.66535009635016));
#230727=CARTESIAN_POINT('Ctrl Pts',(31.3693880355479,54.4507682193237,2.66433897912391));
#230728=CARTESIAN_POINT('Ctrl Pts',(31.3731331934892,54.4497115877223,2.66344564884843));
#230729=CARTESIAN_POINT('Ctrl Pts',(31.3794399458813,54.4479322465077,2.66194130298636));
#230730=CARTESIAN_POINT('Ctrl Pts',(31.3857169562559,54.4457622496023,2.66077206705471));
#230731=CARTESIAN_POINT('Ctrl Pts',(31.3918909882808,54.4431895758478,2.65998225155765));
#230732=CARTESIAN_POINT('Ctrl Pts',(31.393434496287,54.4425464074092,2.65978479768339));
#230733=CARTESIAN_POINT('Ctrl Pts',(31.3949714642037,54.4418778620535,2.65961098966673));
#230734=CARTESIAN_POINT('Ctrl Pts',(31.3965005998225,54.441183481233,2.65946139030552));
#230735=CARTESIAN_POINT('Ctrl Pts',(31.3987943032508,54.4401419100023,2.65923699126371));
#230736=CARTESIAN_POINT('Ctrl Pts',(31.4010703637564,54.4390422051399,2.65906707562492));
#230737=CARTESIAN_POINT('Ctrl Pts',(31.4033252432071,54.4378842814516,2.6589533256297));
#230738=CARTESIAN_POINT('Ctrl Pts',(31.4055801226578,54.4367263577634,2.65883957563448));
#230739=CARTESIAN_POINT('Ctrl Pts',(31.4078138194781,54.4355102267488,2.658781988603));
#230740=CARTESIAN_POINT('Ctrl Pts',(31.4100231232069,54.434235916308,2.658781988603));
#230741=CARTESIAN_POINT('Ctrl Pts',(29.501078514911,51.1278468659049,2.65878198860297));
#230742=CARTESIAN_POINT('Ctrl Pts',(29.4936027956392,51.1321585373229,2.65878198860297));
#230743=CARTESIAN_POINT('Ctrl Pts',(29.4865477845229,51.1370499258751,2.65945335517901));
#230744=CARTESIAN_POINT('Ctrl Pts',(29.4799806005914,51.1423856448188,2.66072561226665));
#230745=CARTESIAN_POINT('Ctrl Pts',(29.4757388736044,51.1458319717794,2.66154735980399));
#230746=CARTESIAN_POINT('Ctrl Pts',(29.4717000621109,51.1494629466904,2.66261895766934));
#230747=CARTESIAN_POINT('Ctrl Pts',(29.4678753842639,51.1532365012462,2.66391429251063));
#230748=CARTESIAN_POINT('Ctrl Pts',(29.4628059928683,51.1582381316479,2.6656311846416));
#230749=CARTESIAN_POINT('Ctrl Pts',(29.4581176150989,51.1634934604717,2.66774105138736));
#230750=CARTESIAN_POINT('Ctrl Pts',(29.453837929136,51.1689167792842,2.67016894181786));
#230751=CARTESIAN_POINT('Ctrl Pts',(29.4516980861545,51.1716284386904,2.67138288703312));
#230752=CARTESIAN_POINT('Ctrl Pts',(29.4496602426632,51.1743821937241,2.67267613167588));
#230753=CARTESIAN_POINT('Ctrl Pts',(29.4477266300417,51.1771680313594,2.6740383543259));
#230754=CARTESIAN_POINT('Ctrl Pts',(29.446759823731,51.178560950177,2.67471946565091));
#230755=CARTESIAN_POINT('Ctrl Pts',(29.4458190608836,51.1799618978182,2.6754178138956));
#230756=CARTESIAN_POINT('Ctrl Pts',(29.4449045308659,51.1813696738594,2.67613207244206));
#230757=CARTESIAN_POINT('Ctrl Pts',(29.4446758983615,51.1817216178697,2.67631063707868));
#230758=CARTESIAN_POINT('Ctrl Pts',(29.4444489051053,51.182073988828,2.67649019601883));
#230759=CARTESIAN_POINT('Ctrl Pts',(29.4442235534434,51.1824267683261,2.67667072836694));
#230760=CARTESIAN_POINT('Ctrl Pts',(29.4435474984577,51.1834851068202,2.67721232541128));
#230761=CARTESIAN_POINT('Ctrl Pts',(29.4428862193406,51.1845471213154,2.67776268340085));
#230762=CARTESIAN_POINT('Ctrl Pts',(29.4422397658678,51.1856123224582,2.67832123541554));
#230763=CARTESIAN_POINT('Ctrl Pts',(29.4376862310783,51.1931154617652,2.68225560368482));
#230764=CARTESIAN_POINT('Ctrl Pts',(29.4338145801761,51.2007799603597,2.68661792998926));
#230765=CARTESIAN_POINT('Ctrl Pts',(29.4305579784513,51.208506571073,2.69130986622615));
#230766=CARTESIAN_POINT('Ctrl Pts',(29.4289785301339,51.2122539689196,2.69358545023091));
#230767=CARTESIAN_POINT('Ctrl Pts',(29.4275440072542,51.21601649797,2.69593918853506));
#230768=CARTESIAN_POINT('Ctrl Pts',(29.4262483256618,51.2197852472981,2.69836306235511));
#230769=CARTESIAN_POINT('Ctrl Pts',(29.4242647276705,51.2255549392046,2.70207384382244));
#230770=CARTESIAN_POINT('Ctrl Pts',(29.4226066102323,51.2313356805892,2.70594760814244));
#230771=CARTESIAN_POINT('Ctrl Pts',(29.4212581193013,51.2370841708901,2.70995196345724));
#230772=CARTESIAN_POINT('Ctrl Pts',(29.4206318731368,51.2397537995246,2.71181160678122));
#230773=CARTESIAN_POINT('Ctrl Pts',(29.4200721889214,51.2424163366107,2.71369962772114));
#230774=CARTESIAN_POINT('Ctrl Pts',(29.4195787111907,51.2450674596719,2.71561183138676));
#230775=CARTESIAN_POINT('Ctrl Pts',(29.419540888067,51.2452706578086,2.71575839426327));
#230776=CARTESIAN_POINT('Ctrl Pts',(29.4195034207002,51.2454737959511,2.71590508903225));
#230777=CARTESIAN_POINT('Ctrl Pts',(29.4194663081573,51.2456768729758,2.71605191409928));
#230778=CARTESIAN_POINT('Ctrl Pts',(29.4189449888201,51.2485294929148,2.71811436362769));
#230779=CARTESIAN_POINT('Ctrl Pts',(29.4184957101765,51.251370561363,2.72020091026976));
#230780=CARTESIAN_POINT('Ctrl Pts',(29.4181151898796,51.2541954110683,2.72230624862198));
#230781=CARTESIAN_POINT('Ctrl Pts',(29.4167507117684,51.2643248197285,2.72985561753095));
#230782=CARTESIAN_POINT('Ctrl Pts',(29.4162578421121,51.2743237313756,2.73770089914296));
#230783=CARTESIAN_POINT('Ctrl Pts',(29.4165161672808,51.2841455249762,2.74574823347012));
#230784=CARTESIAN_POINT('Ctrl Pts',(29.4168000406901,51.2949386894568,2.75459144546939));
#230785=CARTESIAN_POINT('Ctrl Pts',(29.4179908989232,51.3055186222579,2.76367911754159));
#230786=CARTESIAN_POINT('Ctrl Pts',(29.4199800715336,51.3158373135939,2.77292162564591));
#230787=CARTESIAN_POINT('Ctrl Pts',(29.4221278787387,51.3269789105989,2.78290121484585));
#230788=CARTESIAN_POINT('Ctrl Pts',(29.4252064644174,51.3378170984242,2.79306229500033));
#230789=CARTESIAN_POINT('Ctrl Pts',(29.4291364604194,51.3482921445236,2.80331916685089));
#230790=CARTESIAN_POINT('Ctrl Pts',(29.4330334877931,51.3586793157498,2.81348999408594));
#230791=CARTESIAN_POINT('Ctrl Pts',(29.4377684584844,51.368710631544,2.82375635966844));
#230792=CARTESIAN_POINT('Ctrl Pts',(29.443310811626,51.3783102687787,2.83404198860297));
#230793=CARTESIAN_POINT('Origin',(0.0131982271536777,-0.00761999999981537,
2.83404198860262));
#230794=CARTESIAN_POINT('Ctrl Pts',(31.4364195775134,54.4189959163066,2.658781988603));
#230795=CARTESIAN_POINT('Ctrl Pts',(31.443856016,54.414698338812,2.658781988603));
#230796=CARTESIAN_POINT('Ctrl Pts',(31.4508673716603,54.4098177483015,2.65944603041881));
#230797=CARTESIAN_POINT('Ctrl Pts',(31.4573895320587,54.4044907169113,2.66070439264087));
#230798=CARTESIAN_POINT('Ctrl Pts',(31.4615568820643,54.4010869974476,2.66150842619614));
#230799=CARTESIAN_POINT('Ctrl Pts',(31.4655251210645,54.3975017237413,2.66255428265392));
#230800=CARTESIAN_POINT('Ctrl Pts',(31.4692842169744,54.3937759157111,2.66381699700688));
#230801=CARTESIAN_POINT('Ctrl Pts',(31.4744146286224,54.3886909353395,2.66554034873288));
#230802=CARTESIAN_POINT('Ctrl Pts',(31.479150331882,54.3833409297223,2.66766759643993));
#230803=CARTESIAN_POINT('Ctrl Pts',(31.4834636394928,54.3778174666305,2.67012012783169));
#230804=CARTESIAN_POINT('Ctrl Pts',(31.4856202932981,54.3750557350846,2.67134639352757));
#230805=CARTESIAN_POINT('Ctrl Pts',(31.4876715300025,54.3722505364144,2.67265375585033));
#230806=CARTESIAN_POINT('Ctrl Pts',(31.4896151854259,54.369412577295,2.67403135126961));
#230807=CARTESIAN_POINT('Ctrl Pts',(31.4905870131376,54.3679935977353,2.67472014897925));
#230808=CARTESIAN_POINT('Ctrl Pts',(31.4915319606351,54.3665664194002,2.67542649668655));
#230809=CARTESIAN_POINT('Ctrl Pts',(31.4924498523887,54.3651323262971,2.67614899656124));
#230810=CARTESIAN_POINT('Ctrl Pts',(31.4926793253271,54.3647738030213,2.67632962152991));
#230811=CARTESIAN_POINT('Ctrl Pts',(31.4929071076039,54.3644148473888,2.67651125590973));
#230812=CARTESIAN_POINT('Ctrl Pts',(31.4931331971267,54.3640554790924,2.67669387767546));
#230813=CARTESIAN_POINT('Ctrl Pts',(31.4938114656952,54.3629773742031,2.67724174297266));
#230814=CARTESIAN_POINT('Ctrl Pts',(31.4944744978649,54.3618955562475,2.6777984950477));
#230815=CARTESIAN_POINT('Ctrl Pts',(31.4951222515527,54.3608105487852,2.67836353618032));
#230816=CARTESIAN_POINT('Ctrl Pts',(31.4995986314374,54.3533124740226,2.68226832098919));
#230817=CARTESIAN_POINT('Ctrl Pts',(31.5034009004293,54.3456575719331,2.68659153751388));
#230818=CARTESIAN_POINT('Ctrl Pts',(31.50659762188,54.337942849207,2.69123699486159));
#230819=CARTESIAN_POINT('Ctrl Pts',(31.5081863836663,54.3341086531882,2.6935457744121));
#230820=CARTESIAN_POINT('Ctrl Pts',(31.5096252947445,54.3302591366971,2.69593478828124));
#230821=CARTESIAN_POINT('Ctrl Pts',(31.5109210156001,54.3264035847698,2.69839565261241));
#230822=CARTESIAN_POINT('Ctrl Pts',(31.5137795693411,54.3178976613388,2.70382468689067));
#230823=CARTESIAN_POINT('Ctrl Pts',(31.515952667503,54.3093672304022,2.70961155815108));
#230824=CARTESIAN_POINT('Ctrl Pts',(31.5174623893715,54.3009559572069,2.71562701361788));
#230825=CARTESIAN_POINT('Ctrl Pts',(31.5180139098087,54.2978832130369,2.71782453535878));
#230826=CARTESIAN_POINT('Ctrl Pts',(31.5184846398474,54.2948245130136,2.72005051502421));
#230827=CARTESIAN_POINT('Ctrl Pts',(31.5188783726369,54.2917835794185,2.72229986760133));
#230828=CARTESIAN_POINT('Ctrl Pts',(31.5202008794132,54.2815694052532,2.72985520488948));
#230829=CARTESIAN_POINT('Ctrl Pts',(31.5206547127629,54.2714898389033,2.73770845534655));
#230830=CARTESIAN_POINT('Ctrl Pts',(31.5203592886226,54.2615918017952,2.74576706701893));
#230831=CARTESIAN_POINT('Ctrl Pts',(31.5200345824971,54.2507126865138,2.75462443585215));
#230832=CARTESIAN_POINT('Ctrl Pts',(31.5188048676544,54.2400521939087,2.76373036323415));
#230833=CARTESIAN_POINT('Ctrl Pts',(31.5167773687218,54.2296591093466,2.77299664637103));
#230834=CARTESIAN_POINT('Ctrl Pts',(31.5145936654999,54.2184653119648,2.78297683033819));
#230835=CARTESIAN_POINT('Ctrl Pts',(31.511484430286,54.2075805209297,2.793144014793));
#230836=CARTESIAN_POINT('Ctrl Pts',(31.5075265408301,54.1970658734701,2.80341452428409));
#230837=CARTESIAN_POINT('Ctrl Pts',(31.5036220962464,54.1866932092558,2.81354634721688));
#230838=CARTESIAN_POINT('Ctrl Pts',(31.498890978556,54.1766795569324,2.82378004209381));
#230839=CARTESIAN_POINT('Ctrl Pts',(31.4933613949858,54.1671020372441,2.834041988603));
#230840=CARTESIAN_POINT('Ctrl Pts',(29.7732664904679,51.1878102687787,2.83404198860297));
#230841=CARTESIAN_POINT('Ctrl Pts',(29.7679746486357,51.1786445298597,2.82422126443112));
#230842=CARTESIAN_POINT('Ctrl Pts',(29.7619788985611,51.1699291351237,2.81442815028676));
#230843=CARTESIAN_POINT('Ctrl Pts',(29.7553188532218,51.1617065245642,2.80471618166561));
#230844=CARTESIAN_POINT('Ctrl Pts',(29.74888799347,51.1537668706117,2.79533842146517));
#230845=CARTESIAN_POINT('Ctrl Pts',(29.7418369154183,51.1462857370554,2.78603515650572));
#230846=CARTESIAN_POINT('Ctrl Pts',(29.7341642916964,51.1393284263646,2.77685887347129));
#230847=CARTESIAN_POINT('Ctrl Pts',(29.7269112593623,51.1327515888669,2.76818441216977));
#230848=CARTESIAN_POINT('Ctrl Pts',(29.7191021335107,51.126642241794,2.75962261522049));
#230849=CARTESIAN_POINT('Ctrl Pts',(29.7107129315343,51.1210907313645,2.75123537702107));
#230850=CARTESIAN_POINT('Ctrl Pts',(29.7029866172533,51.1159778833925,2.74351087134582));
#230851=CARTESIAN_POINT('Ctrl Pts',(29.6947677915948,51.1113379461923,2.73593399450323));
#230852=CARTESIAN_POINT('Ctrl Pts',(29.6860256466511,51.1072776647628,2.72857657813064));
#230853=CARTESIAN_POINT('Ctrl Pts',(29.6834189154995,51.1060669708022,2.72638274508653));
#230854=CARTESIAN_POINT('Ctrl Pts',(29.6807655934612,51.1049080895607,2.72420861709776));
#230855=CARTESIAN_POINT('Ctrl Pts',(29.6780647241927,51.1038046002595,2.72205663736744));
#230856=CARTESIAN_POINT('Ctrl Pts',(29.6753914511536,51.1027123859002,2.71992664556783));
#230857=CARTESIAN_POINT('Ctrl Pts',(29.6726744751146,51.1016753170133,2.71782089927902));
#230858=CARTESIAN_POINT('Ctrl Pts',(29.6699160505199,51.1006978225843,2.71574387311263));
#230859=CARTESIAN_POINT('Ctrl Pts',(29.6697242350682,51.1006298495334,2.71559944077503));
#230860=CARTESIAN_POINT('Ctrl Pts',(29.6695322176089,51.1005621526965,2.71545515216086));
#230861=CARTESIAN_POINT('Ctrl Pts',(29.6693399979287,51.1004947333606,2.71531100781747));
#230862=CARTESIAN_POINT('Ctrl Pts',(29.6609123829951,51.0975388226979,2.70899119176098));
#230863=CARTESIAN_POINT('Ctrl Pts',(29.652091674968,51.095161351427,2.70298296066851));
#230864=CARTESIAN_POINT('Ctrl Pts',(29.6429396446297,51.0934607157664,2.69736727774148));
#230865=CARTESIAN_POINT('Ctrl Pts',(29.6344083617423,51.0918754277622,2.69213248525433));
#230866=CARTESIAN_POINT('Ctrl Pts',(29.6255883681029,51.0908783954021,2.68723866185465));
#230867=CARTESIAN_POINT('Ctrl Pts',(29.6165418049893,51.0905760611939,2.68278595829554));
#230868=CARTESIAN_POINT('Ctrl Pts',(29.613232455165,51.0904654634292,2.68115710172806));
#230869=CARTESIAN_POINT('Ctrl Pts',(29.6098929659868,51.0904480940786,2.67958763637819));
#230870=CARTESIAN_POINT('Ctrl Pts',(29.6065271365692,51.0905301191543,2.67808378645382));
#230871=CARTESIAN_POINT('Ctrl Pts',(29.6057177670366,51.0905498434447,2.67772216078617));
#230872=CARTESIAN_POINT('Ctrl Pts',(29.6049064053145,51.090575662893,2.6773640360358));
#230873=CARTESIAN_POINT('Ctrl Pts',(29.6040931741702,51.0906076352719,2.67700956934496));
#230874=CARTESIAN_POINT('Ctrl Pts',(29.6033053564992,51.090638608514,2.67666617973821));
#230875=CARTESIAN_POINT('Ctrl Pts',(29.6025157844404,51.0906753561241,2.67632622314135));
#230876=CARTESIAN_POINT('Ctrl Pts',(29.6017245728792,51.0907179287118,2.6759898415879));
#230877=CARTESIAN_POINT('Ctrl Pts',(29.5930559358439,51.0911843606099,2.6723043929224));
#230878=CARTESIAN_POINT('Ctrl Pts',(29.5841848213177,51.0923507190418,2.66904964539997));
#230879=CARTESIAN_POINT('Ctrl Pts',(29.5752911628173,51.0942731997207,2.66640203566747));
#230880=CARTESIAN_POINT('Ctrl Pts',(29.5716026975456,51.0950705097612,2.6653039929946));
#230881=CARTESIAN_POINT('Ctrl Pts',(29.5679105139263,51.0959974771976,2.66430995142277));
#230882=CARTESIAN_POINT('Ctrl Pts',(29.5642276868789,51.0970562972093,2.66343053473376));
#230883=CARTESIAN_POINT('Ctrl Pts',(29.5579462415721,51.098862225076,2.66193059792899));
#230884=CARTESIAN_POINT('Ctrl Pts',(29.5516941764754,51.1010529624043,2.66076519817142));
#230885=CARTESIAN_POINT('Ctrl Pts',(29.5455435225218,51.1036389246281,2.65997805604474));
#230886=CARTESIAN_POINT('Ctrl Pts',(29.542468195545,51.10493190574,2.6595844849814));
#230887=CARTESIAN_POINT('Ctrl Pts',(29.5394188854259,51.1063249785083,2.65928526260776));
#230888=CARTESIAN_POINT('Ctrl Pts',(29.5364046579957,51.1078194668133,2.65908463971338));
#230889=CARTESIAN_POINT('Ctrl Pts',(29.5333904305655,51.1093139551182,2.658884016819));
#230890=CARTESIAN_POINT('Ctrl Pts',(29.5304113137792,51.1109098228568,2.65878198860297));
#230891=CARTESIAN_POINT('Ctrl Pts',(29.5274749692184,51.1126068659049,2.65878198860297));
#230892=CARTESIAN_POINT('Origin',(23.6840886581935,53.232803045145,2.83404198860299));
#230893=CARTESIAN_POINT('Ctrl Pts',(25.3107727110821,57.3172883154492,2.83404198860302));
#230894=CARTESIAN_POINT('Ctrl Pts',(25.3150883208947,57.3269813337902,2.8241965244009));
#230895=CARTESIAN_POINT('Ctrl Pts',(25.3201559369473,57.3363050752418,2.81438790575658));
#230896=CARTESIAN_POINT('Ctrl Pts',(25.3259384683624,57.3452135417191,2.80466781256893));
#230897=CARTESIAN_POINT('Ctrl Pts',(25.3315331019393,57.3538325360824,2.79526356453053));
#230898=CARTESIAN_POINT('Ctrl Pts',(25.3377977038129,57.3620638476591,2.78594102496191));
#230899=CARTESIAN_POINT('Ctrl Pts',(25.3447390861665,57.3698434251128,2.77675109088721));
#230900=CARTESIAN_POINT('Ctrl Pts',(25.3513052064473,57.3772024263452,2.76805797913609));
#230901=CARTESIAN_POINT('Ctrl Pts',(25.3584775246731,57.384157910203,2.75948271210072));
#230902=CARTESIAN_POINT('Ctrl Pts',(25.3662887884618,57.3906233351713,2.7510857557312));
#230903=CARTESIAN_POINT('Ctrl Pts',(25.3734835273362,57.3965784591586,2.74335155163148));
#230904=CARTESIAN_POINT('Ctrl Pts',(25.3812207968911,57.4021181432118,2.73576818685804));
#230905=CARTESIAN_POINT('Ctrl Pts',(25.3895423083639,57.4071400767298,2.72840626160343));
#230906=CARTESIAN_POINT('Ctrl Pts',(25.3919560625166,57.4085967487446,2.72627084693591));
#230907=CARTESIAN_POINT('Ctrl Pts',(25.3944190600999,57.4100096047785,2.72415424587498));
#230908=CARTESIAN_POINT('Ctrl Pts',(25.3969325220924,57.4113754784548,2.72205867173297));
#230909=CARTESIAN_POINT('Ctrl Pts',(25.3996572764942,57.4128561733383,2.719786934629));
#230910=CARTESIAN_POINT('Ctrl Pts',(25.4024370309187,57.4142805418442,2.71754411340801));
#230911=CARTESIAN_POINT('Ctrl Pts',(25.4052723227226,57.4156446191419,2.71533341844298));
#230912=CARTESIAN_POINT('Ctrl Pts',(25.4130538033266,57.419388339989,2.70926614876445));
#230913=CARTESIAN_POINT('Ctrl Pts',(25.4212623406656,57.4226343338645,2.70347381860462));
#230914=CARTESIAN_POINT('Ctrl Pts',(25.4298341608309,57.4253008212881,2.69804914171448));
#230915=CARTESIAN_POINT('Ctrl Pts',(25.4376769109072,57.4277405125137,2.6930858568726));
#230916=CARTESIAN_POINT('Ctrl Pts',(25.4458193604265,57.4296843862654,2.68842799053242));
#230917=CARTESIAN_POINT('Ctrl Pts',(25.4542377154369,57.4310470526569,2.68414767054276));
#230918=CARTESIAN_POINT('Ctrl Pts',(25.4583727839184,57.4317163899371,2.68204519134607));
#230919=CARTESIAN_POINT('Ctrl Pts',(25.462574317174,57.4322449980039,2.68003431778555));
#230920=CARTESIAN_POINT('Ctrl Pts',(25.466838401935,57.4326195921324,2.67812693945303));
#230921=CARTESIAN_POINT('Ctrl Pts',(25.4676474704857,57.4326906677196,2.67776503299255));
#230922=CARTESIAN_POINT('Ctrl Pts',(25.4684592045964,57.4327558640765,2.67740659639976));
#230923=CARTESIAN_POINT('Ctrl Pts',(25.4692734860654,57.4328151061498,2.67705178968907));
#230924=CARTESIAN_POINT('Ctrl Pts',(25.4700623212384,57.4328724969082,2.67670807068809));
#230925=CARTESIAN_POINT('Ctrl Pts',(25.4708535470246,57.432924299722,2.67636775825317));
#230926=CARTESIAN_POINT('Ctrl Pts',(25.4716470524589,57.4329704479396,2.67603099699307));
#230927=CARTESIAN_POINT('Ctrl Pts',(25.4802945111773,57.4334733617059,2.67236104217173));
#230928=CARTESIAN_POINT('Ctrl Pts',(25.4892184175055,57.4333046542891,2.66911440541513));
#230929=CARTESIAN_POINT('Ctrl Pts',(25.4982455208449,57.4323852136915,2.66646778189668));
#230930=CARTESIAN_POINT('Ctrl Pts',(25.5020577226405,57.4319969282177,2.66535009635017));
#230931=CARTESIAN_POINT('Ctrl Pts',(25.5058881199468,57.4314751387429,2.66433897912392));
#230932=CARTESIAN_POINT('Ctrl Pts',(25.5097232095986,57.4308157710843,2.66344564884845));
#230933=CARTESIAN_POINT('Ctrl Pts',(25.516181404744,57.4297054124228,2.66194130298638));
#230934=CARTESIAN_POINT('Ctrl Pts',(25.5226508554408,57.4282034292358,2.66077206705473));
#230935=CARTESIAN_POINT('Ctrl Pts',(25.5290599831064,57.4262902109372,2.65998225155767));
#230936=CARTESIAN_POINT('Ctrl Pts',(25.5306622650228,57.4258119063626,2.65978479768341));
#230937=CARTESIAN_POINT('Ctrl Pts',(25.532260695287,57.4253076802627,2.65961098966675));
#230938=CARTESIAN_POINT('Ctrl Pts',(25.5338540367011,57.4247769415294,2.65946139030554));
#230939=CARTESIAN_POINT('Ctrl Pts',(25.5362440488221,57.4239808334294,2.65923699126373));
#230940=CARTESIAN_POINT('Ctrl Pts',(25.5386225912894,57.4231250659722,2.65906707562494));
#230941=CARTESIAN_POINT('Ctrl Pts',(25.5409861542582,57.4222091845949,2.65895332562972));
#230942=CARTESIAN_POINT('Ctrl Pts',(25.543349717227,57.4212933032176,2.6588395756345));
#230943=CARTESIAN_POINT('Ctrl Pts',(25.5456982979286,57.4203173191919,2.65878198860302));
#230944=CARTESIAN_POINT('Ctrl Pts',(25.5480287005724,57.4192809246807,2.65878198860302));
#230945=CARTESIAN_POINT('Ctrl Pts',(23.9951532569806,53.9314655730807,2.658781988603));
#230946=CARTESIAN_POINT('Ctrl Pts',(23.9872677980943,53.9349721992639,2.658781988603));
#230947=CARTESIAN_POINT('Ctrl Pts',(23.979740145739,53.9390993428072,2.65945335517894));
#230948=CARTESIAN_POINT('Ctrl Pts',(23.972651203027,53.9437193744794,2.6607256122664));
#230949=CARTESIAN_POINT('Ctrl Pts',(23.9680724734026,53.9467034408971,2.66154735980378));
#230950=CARTESIAN_POINT('Ctrl Pts',(23.9636762467129,53.9498923541891,2.66261895766923));
#230951=CARTESIAN_POINT('Ctrl Pts',(23.9594780769921,53.9532454491207,2.66391429251067));
#230952=CARTESIAN_POINT('Ctrl Pts',(23.9539136435132,53.9576897843755,2.66563118464163));
#230953=CARTESIAN_POINT('Ctrl Pts',(23.9487016177219,53.9624262550347,2.66774105138739));
#230954=CARTESIAN_POINT('Ctrl Pts',(23.9438784851452,53.9673725153422,2.6701689418179));
#230955=CARTESIAN_POINT('Ctrl Pts',(23.9414669188569,53.969845645496,2.67138288703315));
#230956=CARTESIAN_POINT('Ctrl Pts',(23.9391523931035,53.9723713025231,2.67267613167591));
#230957=CARTESIAN_POINT('Ctrl Pts',(23.9369381736874,53.9749397614924,2.67403835432593));
#230958=CARTESIAN_POINT('Ctrl Pts',(23.9358310639794,53.976223990977,2.67471946565094));
#230959=CARTESIAN_POINT('Ctrl Pts',(23.9347490158252,53.9775189275857,2.67541781389563));
#230960=CARTESIAN_POINT('Ctrl Pts',(23.9336923430325,53.9788233972651,2.67613207244209));
#230961=CARTESIAN_POINT('Ctrl Pts',(23.9334281748343,53.979149514685,2.6763106370787));
#230962=CARTESIAN_POINT('Ctrl Pts',(23.9331655922761,53.979476228062,2.67649019601885));
#230963=CARTESIAN_POINT('Ctrl Pts',(23.9329045996154,53.9798035193342,2.67667072836697));
#230964=CARTESIAN_POINT('Ctrl Pts',(23.9321216216332,53.9807853931505,2.6772123254113));
#230965=CARTESIAN_POINT('Ctrl Pts',(23.9313529543291,53.9817724673294,2.67776268340087));
#230966=CARTESIAN_POINT('Ctrl Pts',(23.9305986983576,53.9827642604007,2.67832123541556));
#230967=CARTESIAN_POINT('Ctrl Pts',(23.9252858166867,53.9897503227315,2.68225560368483));
#230968=CARTESIAN_POINT('Ctrl Pts',(23.9206342168334,53.9969681366817,2.68661792998925));
#230969=CARTESIAN_POINT('Ctrl Pts',(23.9165878043695,54.0043120126392,2.69130986622613));
#230970=CARTESIAN_POINT('Ctrl Pts',(23.914625298697,54.0078737845429,2.6935854502309));
#230971=CARTESIAN_POINT('Ctrl Pts',(23.9128053429042,54.0114657535934,2.69593918853507));
#230972=CARTESIAN_POINT('Ctrl Pts',(23.9111228176154,54.0150784217127,2.69836306235513));
#230973=CARTESIAN_POINT('Ctrl Pts',(23.9085469889529,54.0206091641934,2.70207384382246));
#230974=CARTESIAN_POINT('Ctrl Pts',(23.906293702842,54.0261849176041,2.70594760814246));
#230975=CARTESIAN_POINT('Ctrl Pts',(23.9043517182282,54.0317609613889,2.70995196345726));
#230976=CARTESIAN_POINT('Ctrl Pts',(23.903449850527,54.0343505049692,2.71181160678124));
#230977=CARTESIAN_POINT('Ctrl Pts',(23.9026149214104,54.0369399534677,2.71369962772117));
#230978=CARTESIAN_POINT('Ctrl Pts',(23.9018470291827,54.0395249709305,2.71561183138679));
#230979=CARTESIAN_POINT('Ctrl Pts',(23.9017881732691,54.0397231023335,2.7157583942633));
#230980=CARTESIAN_POINT('Ctrl Pts',(23.9017296774346,54.0399212112578,2.71590508903227));
#230981=CARTESIAN_POINT('Ctrl Pts',(23.9016715408688,54.0401192964882,2.7160519140993));
#230982=CARTESIAN_POINT('Ctrl Pts',(23.9008548973949,54.0429017967675,2.71811436362771));
#230983=CARTESIAN_POINT('Ctrl Pts',(23.9001111074278,54.0456803391392,2.72020091026977));
#230984=CARTESIAN_POINT('Ctrl Pts',(23.8994373944623,54.0484499388204,2.722306248622));
#230985=CARTESIAN_POINT('Ctrl Pts',(23.8970215795838,54.0583812307207,2.72985561753144));
#230986=CARTESIAN_POINT('Ctrl Pts',(23.8954862390501,54.0682738483763,2.73770089914397));
#230987=CARTESIAN_POINT('Ctrl Pts',(23.8947164920949,54.0780688394974,2.74574823347167));
#230988=CARTESIAN_POINT('Ctrl Pts',(23.8938706175192,54.0888325507453,2.75459144547126));
#230989=CARTESIAN_POINT('Ctrl Pts',(23.8939490479891,54.0994790041489,2.7636791175438));
#230990=CARTESIAN_POINT('Ctrl Pts',(23.8948487267558,54.1099490937706,2.77292162564846));
#230991=CARTESIAN_POINT('Ctrl Pts',(23.8958201540351,54.1212541629279,2.78290121484838));
#230992=CARTESIAN_POINT('Ctrl Pts',(23.8977489757816,54.1323547778562,2.79306229500283));
#230993=CARTESIAN_POINT('Ctrl Pts',(23.900562502383,54.1431832369997,2.80331916685335));
#230994=CARTESIAN_POINT('Ctrl Pts',(23.9033524263869,54.1539208564969,2.81348999408761));
#230995=CARTESIAN_POINT('Ctrl Pts',(23.9070129003886,54.1643921589027,2.82375635966928));
#230996=CARTESIAN_POINT('Ctrl Pts',(23.9115214566113,54.1745185419762,2.834041988603));
#230997=CARTESIAN_POINT('Origin',(0.0139224327744766,-0.00619866644029082,
2.83404198860263));
#230998=CARTESIAN_POINT('Ctrl Pts',(25.5758735661207,57.4068835917982,2.65878198860302));
#230999=CARTESIAN_POINT('Ctrl Pts',(25.5837184861914,57.4033868763696,2.65878198860302));
#231000=CARTESIAN_POINT('Ctrl Pts',(25.5912015935385,57.3992659084766,2.65944603041899));
#231001=CARTESIAN_POINT('Ctrl Pts',(25.5982448512655,57.3946498105247,2.66070439264133));
#231002=CARTESIAN_POINT('Ctrl Pts',(25.6027451576558,57.3917003436848,2.66150842619654));
#231003=CARTESIAN_POINT('Ctrl Pts',(25.6070664213777,57.3885495044082,2.66255428265417));
#231004=CARTESIAN_POINT('Ctrl Pts',(25.6111943775539,57.3852370392635,2.66381699700691));
#231005=CARTESIAN_POINT('Ctrl Pts',(25.6168282094541,57.3807161889919,2.6655403487329));
#231006=CARTESIAN_POINT('Ctrl Pts',(25.6220971979014,57.3758905070495,2.66766759643995));
#231007=CARTESIAN_POINT('Ctrl Pts',(25.6269642358706,57.3708481654826,2.67012012783171));
#231008=CARTESIAN_POINT('Ctrl Pts',(25.6293977548552,57.3683269946991,2.67134639352759));
#231009=CARTESIAN_POINT('Ctrl Pts',(25.6317309777765,57.3657515758213,2.67265375585036));
#231010=CARTESIAN_POINT('Ctrl Pts',(25.6339606331577,57.3631323306534,2.67403135126964));
#231011=CARTESIAN_POINT('Ctrl Pts',(25.6350754608483,57.3618227080694,2.67472014897928));
#231012=CARTESIAN_POINT('Ctrl Pts',(25.6361644125826,57.3605021218764,2.67542649668657));
#231013=CARTESIAN_POINT('Ctrl Pts',(25.6372271795775,57.3591718306998,2.67614899656126));
#231014=CARTESIAN_POINT('Ctrl Pts',(25.6374928713262,57.3588392579056,2.67632962152993));
#231015=CARTESIAN_POINT('Ctrl Pts',(25.6377569268685,57.358506078401,2.67651125590975));
#231016=CARTESIAN_POINT('Ctrl Pts',(25.638019342065,57.3581723115521,2.67669387767548));
#231017=CARTESIAN_POINT('Ctrl Pts',(25.6388065876546,57.3571710110053,2.67724174297269));
#231018=CARTESIAN_POINT('Ctrl Pts',(25.6395790684331,57.3561644250955,2.67779849504772));
#231019=CARTESIAN_POINT('Ctrl Pts',(25.6403366878211,57.3551530701152,2.67836353618034));
#231020=CARTESIAN_POINT('Ctrl Pts',(25.6455723078613,57.3481639797005,2.68226832098951));
#231021=CARTESIAN_POINT('Ctrl Pts',(25.650153902778,57.3409484572996,2.68659153751456));
#231022=CARTESIAN_POINT('Ctrl Pts',(25.6541395203654,57.333610145012,2.69123699486267));
#231023=CARTESIAN_POINT('Ctrl Pts',(25.6561203613657,57.3299630239487,2.69354577441286));
#231024=CARTESIAN_POINT('Ctrl Pts',(25.6579537739813,57.3262850026761,2.69593478828165));
#231025=CARTESIAN_POINT('Ctrl Pts',(25.6596454116603,57.3225860115761,2.69839565261244));
#231026=CARTESIAN_POINT('Ctrl Pts',(25.6633774170497,57.3144254847134,2.7038246868907));
#231027=CARTESIAN_POINT('Ctrl Pts',(25.6664302835893,57.3061689349814,2.70961155815111));
#231028=CARTESIAN_POINT('Ctrl Pts',(25.6688109525047,57.2979615485276,2.71562701361791));
#231029=CARTESIAN_POINT('Ctrl Pts',(25.6696806408813,57.2949632867554,2.71782453535882));
#231030=CARTESIAN_POINT('Ctrl Pts',(25.6704685134247,57.2919705472985,2.72005051502426));
#231031=CARTESIAN_POINT('Ctrl Pts',(25.6711779534203,57.2889874285392,2.72229986760139));
#231032=CARTESIAN_POINT('Ctrl Pts',(25.6735608872951,57.2789674482901,2.72985520488926));
#231033=CARTESIAN_POINT('Ctrl Pts',(25.6750658360792,57.2689905373625,2.73770845534603));
#231034=CARTESIAN_POINT('Ctrl Pts',(25.6758066569115,57.2591158425062,2.7457670670181));
#231035=CARTESIAN_POINT('Ctrl Pts',(25.6766209067623,57.2482623831247,2.75462443585101));
#231036=CARTESIAN_POINT('Ctrl Pts',(25.676512253336,57.2375317496112,2.76373036323268));
#231037=CARTESIAN_POINT('Ctrl Pts',(25.6755822344127,57.2269836681064,2.77299664636922));
#231038=CARTESIAN_POINT('Ctrl Pts',(25.6745805641841,57.2156229323763,2.78297683033602));
#231039=CARTESIAN_POINT('Ctrl Pts',(25.6726261321661,57.2044727657868,2.79314401479045));
#231040=CARTESIAN_POINT('Ctrl Pts',(25.6697890043839,57.1936020065639,2.80341452428115));
#231041=CARTESIAN_POINT('Ctrl Pts',(25.6669901874063,57.182878039296,2.81354634721492));
#231042=CARTESIAN_POINT('Ctrl Pts',(25.6633316989624,57.1724247063449,2.82378004209285));
#231043=CARTESIAN_POINT('Ctrl Pts',(25.658833530444,57.1623216544374,2.83404198860302));
#231044=CARTESIAN_POINT('Ctrl Pts',(24.2595822759732,54.0195518809643,2.83404198860301));
#231045=CARTESIAN_POINT('Ctrl Pts',(24.2552775040086,54.0098832048286,2.82422126443219));
#231046=CARTESIAN_POINT('Ctrl Pts',(24.2502256060994,54.0005888273964,2.81442815028887));
#231047=CARTESIAN_POINT('Ctrl Pts',(24.2444615420318,53.9917150968541,2.80471618166874));
#231048=CARTESIAN_POINT('Ctrl Pts',(24.2388958310297,53.9831467292698,2.79533842146893));
#231049=CARTESIAN_POINT('Ctrl Pts',(24.232665370916,53.9749695397932,2.78603515651008));
#231050=CARTESIAN_POINT('Ctrl Pts',(24.2257620156254,53.9672483344118,2.77685887347623));
#231051=CARTESIAN_POINT('Ctrl Pts',(24.2192361828786,53.9599493771943,2.76818441217506));
#231052=CARTESIAN_POINT('Ctrl Pts',(24.2121084368973,53.9530572218393,2.75962261522611));
#231053=CARTESIAN_POINT('Ctrl Pts',(24.2043454827017,53.9466592127743,2.75123537702697));
#231054=CARTESIAN_POINT('Ctrl Pts',(24.1971959321207,53.9407667537598,2.74351087135186));
#231055=CARTESIAN_POINT('Ctrl Pts',(24.1895071355548,53.9352931334051,2.73593399450939));
#231056=CARTESIAN_POINT('Ctrl Pts',(24.1812372959747,53.9303412916453,2.72857657813688));
#231057=CARTESIAN_POINT('Ctrl Pts',(24.178771396746,53.92886475239,2.72638274509066));
#231058=CARTESIAN_POINT('Ctrl Pts',(24.1762537459564,53.9274348719445,2.72420861709981));
#231059=CARTESIAN_POINT('Ctrl Pts',(24.1736830183708,53.9260551099578,2.72205663736747));
#231060=CARTESIAN_POINT('Ctrl Pts',(24.1711385572897,53.9246894457404,2.71992664556785));
#231061=CARTESIAN_POINT('Ctrl Pts',(24.1685448683468,53.9233740566952,2.71782089927904));
#231062=CARTESIAN_POINT('Ctrl Pts',(24.1659037306811,53.922113583199,2.71574387311265));
#231063=CARTESIAN_POINT('Ctrl Pts',(24.1657200711331,53.9220259323372,2.71559944077506));
#231064=CARTESIAN_POINT('Ctrl Pts',(24.1655361818118,53.9219385350608,2.71545515216088));
#231065=CARTESIAN_POINT('Ctrl Pts',(24.1653520623708,53.9218513926273,2.7153110078175));
#231066=CARTESIAN_POINT('Ctrl Pts',(24.1572795915927,53.9180307491144,2.708991191761));
#231067=CARTESIAN_POINT('Ctrl Pts',(24.1487557177455,53.9147442868249,2.70298296066853));
#231068=CARTESIAN_POINT('Ctrl Pts',(24.1398315880192,53.9120963197574,2.69736727774148));
#231069=CARTESIAN_POINT('Ctrl Pts',(24.1315127481111,53.9096279542368,2.6921324852544));
#231070=CARTESIAN_POINT('Ctrl Pts',(24.1228452895803,53.9077144433432,2.6872386618548));
#231071=CARTESIAN_POINT('Ctrl Pts',(24.1138798870163,53.9064681420133,2.68278595829574));
#231072=CARTESIAN_POINT('Ctrl Pts',(24.1106002267709,53.9060122288631,2.68115710172819));
#231073=CARTESIAN_POINT('Ctrl Pts',(24.1072808472552,53.9056458829918,2.67958763637825));
#231074=CARTESIAN_POINT('Ctrl Pts',(24.103924882248,53.9053756337488,2.67808378645381));
#231075=CARTESIAN_POINT('Ctrl Pts',(24.1031178847767,53.9053106478341,2.67772216078616));
#231076=CARTESIAN_POINT('Ctrl Pts',(24.1023082689118,53.9052515154468,2.67736403603579));
#231077=CARTESIAN_POINT('Ctrl Pts',(24.1014961507091,53.9051983068759,2.67700956934495));
#231078=CARTESIAN_POINT('Ctrl Pts',(24.1007094112003,53.9051467610728,2.6766661797382));
#231079=CARTESIAN_POINT('Ctrl Pts',(24.0999203233287,53.9051007746217,2.67632622314135));
#231080=CARTESIAN_POINT('Ctrl Pts',(24.0991289960601,53.9050604098636,2.67598984158789));
#231081=CARTESIAN_POINT('Ctrl Pts',(24.090459091316,53.9046181672911,2.67230439292245));
#231082=CARTESIAN_POINT('Ctrl Pts',(24.0815146560291,53.9048508523206,2.66904964540005));
#231083=CARTESIAN_POINT('Ctrl Pts',(24.0724687639696,53.9058331609933,2.66640203566758));
#231084=CARTESIAN_POINT('Ctrl Pts',(24.0687171629031,53.9062405536793,2.66530399299466));
#231085=CARTESIAN_POINT('Ctrl Pts',(24.0649483109702,53.9067765048113,2.6643099514228));
#231086=CARTESIAN_POINT('Ctrl Pts',(24.061174982006,53.9074445642444,2.66343053473376));
#231087=CARTESIAN_POINT('Ctrl Pts',(24.0547391762491,53.9085840092243,2.661930597929));
#231088=CARTESIAN_POINT('Ctrl Pts',(24.0482923662128,53.9101092267075,2.66076519817143));
#231089=CARTESIAN_POINT('Ctrl Pts',(24.0419050995277,53.9120381043536,2.65997805604476));
#231090=CARTESIAN_POINT('Ctrl Pts',(24.0387114661852,53.9130025431767,2.65958448498142));
#231091=CARTESIAN_POINT('Ctrl Pts',(24.0355332447503,53.9140692448459,2.65928526260778));
#231092=CARTESIAN_POINT('Ctrl Pts',(24.0323793130074,53.9152404736263,2.65908463971341));
#231093=CARTESIAN_POINT('Ctrl Pts',(24.0292253812646,53.9164117024068,2.65888401681903));
#231094=CARTESIAN_POINT('Ctrl Pts',(24.0260957707896,53.9176874253156,2.658781988603));
#231095=CARTESIAN_POINT('Ctrl Pts',(24.0229981225296,53.9190682401997,2.658781988603));
#231096=CARTESIAN_POINT('Origin',(17.9900016446781,55.4168495715594,2.834041988603));
#231097=CARTESIAN_POINT('Ctrl Pts',(19.180829583578,59.6489943884566,2.83404198860303));
#231098=CARTESIAN_POINT('Ctrl Pts',(19.1841083557167,59.65908541149,2.82419652440163));
#231099=CARTESIAN_POINT('Ctrl Pts',(19.1881736144722,59.6688877866282,2.81438790575802));
#231100=CARTESIAN_POINT('Ctrl Pts',(19.1929932802638,59.6783518907161,2.80466781257107));
#231101=CARTESIAN_POINT('Ctrl Pts',(19.1976563356165,59.6875084677763,2.79526356453326));
#231102=CARTESIAN_POINT('Ctrl Pts',(19.2030262129953,59.6963495165733,2.78594102496521));
#231103=CARTESIAN_POINT('Ctrl Pts',(19.2091163824534,59.7048120487176,2.77675109089105));
#231104=CARTESIAN_POINT('Ctrl Pts',(19.2148773077497,59.7128170830335,2.76805797914046));
#231105=CARTESIAN_POINT('Ctrl Pts',(19.2212832892262,59.7204841754248,2.7594827121056));
#231106=CARTESIAN_POINT('Ctrl Pts',(19.2283759411575,59.7277306815184,2.75108575573653));
#231107=CARTESIAN_POINT('Ctrl Pts',(19.2349087865398,59.7344052377112,2.74335155163732));
#231108=CARTESIAN_POINT('Ctrl Pts',(19.2420246158606,59.7407233396916,2.73576818686435));
#231109=CARTESIAN_POINT('Ctrl Pts',(19.2497756062286,59.7465875973385,2.72840626161014));
#231110=CARTESIAN_POINT('Ctrl Pts',(19.2520238738985,59.7482885955657,2.72627084694036));
#231111=CARTESIAN_POINT('Ctrl Pts',(19.2543256952557,59.7499511651806,2.72415424587721));
#231112=CARTESIAN_POINT('Ctrl Pts',(19.2566826155664,59.7515722847792,2.72205867173301));
#231113=CARTESIAN_POINT('Ctrl Pts',(19.2592376687177,59.7533296826515,2.71978693462903));
#231114=CARTESIAN_POINT('Ctrl Pts',(19.2618533083056,59.755036811776,2.71754411340803));
#231115=CARTESIAN_POINT('Ctrl Pts',(19.2645304831806,59.7566897852107,2.715333418443));
#231116=CARTESIAN_POINT('Ctrl Pts',(19.2718780106326,59.7612263837727,2.70926614876447));
#231117=CARTESIAN_POINT('Ctrl Pts',(19.2797022819936,59.7653126215478,2.70347381860464));
#231118=CARTESIAN_POINT('Ctrl Pts',(19.2879484209985,59.7688605008636,2.6980491417145));
#231119=CARTESIAN_POINT('Ctrl Pts',(19.2954931904947,59.7721066178187,2.69308585687256));
#231120=CARTESIAN_POINT('Ctrl Pts',(19.3033878446876,59.7748909605622,2.68842799053233));
#231121=CARTESIAN_POINT('Ctrl Pts',(19.3116176456448,59.7771261198371,2.68414767054262));
#231122=CARTESIAN_POINT('Ctrl Pts',(19.315660096991,59.7782240227715,2.68204519134601));
#231123=CARTESIAN_POINT('Ctrl Pts',(19.3197833592188,59.7791889148826,2.68003431778555));
#231124=CARTESIAN_POINT('Ctrl Pts',(19.3239849291286,59.7800071751725,2.67812693945308));
#231125=CARTESIAN_POINT('Ctrl Pts',(19.3247821360952,59.7801624320925,2.6777650329926));
#231126=CARTESIAN_POINT('Ctrl Pts',(19.3255826085666,59.7803121206161,2.6774065963998));
#231127=CARTESIAN_POINT('Ctrl Pts',(19.3263862368335,59.7804561537457,2.67705178968912));
#231128=CARTESIAN_POINT('Ctrl Pts',(19.3271647517172,59.7805956858399,2.67670807068814));
#231129=CARTESIAN_POINT('Ctrl Pts',(19.3279462282172,59.780729910488,2.67636775825322));
#231130=CARTESIAN_POINT('Ctrl Pts',(19.3287305629435,59.7808587498045,2.67603099699312));
#231131=CARTESIAN_POINT('Ctrl Pts',(19.3372780811749,59.7822628141275,2.67236104217182));
#231132=CARTESIAN_POINT('Ctrl Pts',(19.3461707361375,59.7830278331225,2.66911440541526));
#231133=CARTESIAN_POINT('Ctrl Pts',(19.3552444957729,59.7830570185565,2.66646778189681));
#231134=CARTESIAN_POINT('Ctrl Pts',(19.3590764008121,59.7830693437465,2.66535009635027));
#231135=CARTESIAN_POINT('Ctrl Pts',(19.3629403566533,59.7829507982332,2.66433897912399));
#231136=CARTESIAN_POINT('Ctrl Pts',(19.3668233599709,59.7826959186874,2.66344564884849));
#231137=CARTESIAN_POINT('Ctrl Pts',(19.3733622405322,59.7822667079009,2.66194130298641));
#231138=CARTESIAN_POINT('Ctrl Pts',(19.3799532508955,59.7814491944745,2.66077206705475));
#231139=CARTESIAN_POINT('Ctrl Pts',(19.3865272544576,59.7802163932511,2.65998225155769));
#231140=CARTESIAN_POINT('Ctrl Pts',(19.3881707553481,59.7799081929452,2.65978479768342));
#231141=CARTESIAN_POINT('Ctrl Pts',(19.3898131352235,59.7795738105079,2.65961098966677));
#231142=CARTESIAN_POINT('Ctrl Pts',(19.3914532254508,59.7792125287464,2.65946139030556));
#231143=CARTESIAN_POINT('Ctrl Pts',(19.3939133607917,59.7786706061042,2.65923699126375));
#231144=CARTESIAN_POINT('Ctrl Pts',(19.3963683254117,59.7780681520197,2.65906707562496));
#231145=CARTESIAN_POINT('Ctrl Pts',(19.3988146762082,59.7774043475415,2.65895332562974));
#231146=CARTESIAN_POINT('Ctrl Pts',(19.4012610270047,59.7767405430632,2.65883957563452));
#231147=CARTESIAN_POINT('Ctrl Pts',(19.4036987600453,59.7760153991104,2.65878198860303));
#231148=CARTESIAN_POINT('Ctrl Pts',(19.4061247292252,59.7752282754839,2.65878198860303));
#231149=CARTESIAN_POINT('Ctrl Pts',(18.2263320786581,56.144199857553,2.65878198860301));
#231150=CARTESIAN_POINT('Ctrl Pts',(18.2181232748938,56.1468630191717,2.65878198860301));
#231151=CARTESIAN_POINT('Ctrl Pts',(18.2102054558329,56.1501806998584,2.65945335517905));
#231152=CARTESIAN_POINT('Ctrl Pts',(18.2026724222794,56.1540344262263,2.6607256122667));
#231153=CARTESIAN_POINT('Ctrl Pts',(18.1978068555387,56.1565235380443,2.66154735980404));
#231154=CARTESIAN_POINT('Ctrl Pts',(18.1931013796334,56.1592354513152,2.66261895766939));
#231155=CARTESIAN_POINT('Ctrl Pts',(18.1885757140657,56.1621313494122,2.66391429251067));
#231156=CARTESIAN_POINT('Ctrl Pts',(18.1825772036012,56.165969696453,2.66563118464164));
#231157=CARTESIAN_POINT('Ctrl Pts',(18.1768986338333,56.1701354151838,2.6677410513874));
#231158=CARTESIAN_POINT('Ctrl Pts',(18.1715848978926,56.1745504247235,2.67016894181791));
#231159=CARTESIAN_POINT('Ctrl Pts',(18.1689280299223,56.1767579294933,2.67138288703317));
#231160=CARTESIAN_POINT('Ctrl Pts',(18.1663621803354,56.1790278168867,2.67267613167593));
#231161=CARTESIAN_POINT('Ctrl Pts',(18.1638916135759,56.1813507566161,2.67403835432595));
#231162=CARTESIAN_POINT('Ctrl Pts',(18.1626563301961,56.1825122264809,2.67471946565096));
#231163=CARTESIAN_POINT('Ctrl Pts',(18.1614448518812,56.1836869644606,2.67541781389565));
#231164=CARTESIAN_POINT('Ctrl Pts',(18.1602576134416,56.1848738357354,2.67613207244211));
#231165=CARTESIAN_POINT('Ctrl Pts',(18.1599608038317,56.1851705535541,2.67631063707873));
#231166=CARTESIAN_POINT('Ctrl Pts',(18.159665508881,56.1854680298098,2.67649019601887));
#231167=CARTESIAN_POINT('Ctrl Pts',(18.1593717347117,56.1857662469843,2.67667072836699));
#231168=CARTESIAN_POINT('Ctrl Pts',(18.1584904122037,56.1866608985079,2.67721232541133));
#231169=CARTESIAN_POINT('Ctrl Pts',(18.1576227783925,56.1875622177791,2.67776268340089));
#231170=CARTESIAN_POINT('Ctrl Pts',(18.1567689837085,56.1884697364866,2.67832123541558));
#231171=CARTESIAN_POINT('Ctrl Pts',(18.1507549641994,56.1948621810806,2.68225560368491));
#231172=CARTESIAN_POINT('Ctrl Pts',(18.1453743792964,56.2015542305064,2.68661792998941));
#231173=CARTESIAN_POINT('Ctrl Pts',(18.140582489435,56.2084349106665,2.69130986622636));
#231174=CARTESIAN_POINT('Ctrl Pts',(18.1382584280305,56.2117720331088,2.69358545023107));
#231175=CARTESIAN_POINT('Ctrl Pts',(18.136072979141,56.2151540877947,2.69593918853516));
#231176=CARTESIAN_POINT('Ctrl Pts',(18.134022044255,56.2185710935571,2.69836306235515));
#231177=CARTESIAN_POINT('Ctrl Pts',(18.1308822062392,56.22380229064,2.70207384382248));
#231178=CARTESIAN_POINT('Ctrl Pts',(18.1280584389298,56.2291119669557,2.70594760814247));
#231179=CARTESIAN_POINT('Ctrl Pts',(18.125544237423,56.2344544719218,2.70995196345727));
#231180=CARTESIAN_POINT('Ctrl Pts',(18.1243766292364,56.2369355588666,2.71181160678125));
#231181=CARTESIAN_POINT('Ctrl Pts',(18.1232756028766,56.2394235482377,2.71369962772118));
#231182=CARTESIAN_POINT('Ctrl Pts',(18.12224170934,56.2419141381099,2.7156118313868));
#231183=CARTESIAN_POINT('Ctrl Pts',(18.1221624654742,56.2421050320102,2.71575839426331));
#231184=CARTESIAN_POINT('Ctrl Pts',(18.1220835820645,56.2422959411933,2.71590508903228));
#231185=CARTESIAN_POINT('Ctrl Pts',(18.1220050584321,56.2424868643662,2.71605191409931));
#231186=CARTESIAN_POINT('Ctrl Pts',(18.1209020381385,56.2451687593305,2.71811436362772));
#231187=CARTESIAN_POINT('Ctrl Pts',(18.1198718859664,56.2478543333342,2.72020091026979));
#231188=CARTESIAN_POINT('Ctrl Pts',(18.1189123616725,56.2505383386776,2.72230624862202));
#231189=CARTESIAN_POINT('Ctrl Pts',(18.1154716782003,56.260162704504,2.72985561753083));
#231190=CARTESIAN_POINT('Ctrl Pts',(18.1129106883016,56.2698406425777,2.73770089914268));
#231191=CARTESIAN_POINT('Ctrl Pts',(18.1111213027312,56.2795015152455,2.74574823346968));
#231192=CARTESIAN_POINT('Ctrl Pts',(18.1091549477491,56.2901178437866,2.75459144546861));
#231193=CARTESIAN_POINT('Ctrl Pts',(18.1081200911551,56.3007141730203,2.76367911754047));
#231194=CARTESIAN_POINT('Ctrl Pts',(18.1079204190087,56.3112209484337,2.77292162564443));
#231195=CARTESIAN_POINT('Ctrl Pts',(18.1077048232014,56.3225656290393,2.78290121484364));
#231196=CARTESIAN_POINT('Ctrl Pts',(18.1084627484403,56.3338070504099,2.79306229499735));
#231197=CARTESIAN_POINT('Ctrl Pts',(18.1101289800542,56.3448702837326,2.80331916684715));
#231198=CARTESIAN_POINT('Ctrl Pts',(18.1117812336974,56.3558407078977,2.81348999408344));
#231199=CARTESIAN_POINT('Ctrl Pts',(18.1143271060909,56.3666372711378,2.82375635966719));
#231200=CARTESIAN_POINT('Ctrl Pts',(18.1177524687105,56.377179453281,2.83404198860301));
#231201=CARTESIAN_POINT('Origin',(0.014494101308342,-0.00470941899409004,
2.83404198860262));
#231202=CARTESIAN_POINT('Ctrl Pts',(19.4351129318419,59.7658094374954,2.65878198860303));
#231203=CARTESIAN_POINT('Ctrl Pts',(19.4432803829093,59.7631518948794,2.65878198860303));
#231204=CARTESIAN_POINT('Ctrl Pts',(19.4511532554518,59.7598356997915,2.6594460304189));
#231205=CARTESIAN_POINT('Ctrl Pts',(19.4586404431008,59.7559811102142,2.66070439264105));
#231206=CARTESIAN_POINT('Ctrl Pts',(19.4634243995787,59.7535182109732,2.6615084261963));
#231207=CARTESIAN_POINT('Ctrl Pts',(19.4680513433539,59.7508363273796,2.66255428265404));
#231208=CARTESIAN_POINT('Ctrl Pts',(19.4725029330461,59.7479734971808,2.66381699700693));
#231209=CARTESIAN_POINT('Ctrl Pts',(19.4785784597572,59.7440663083909,2.66554034873292));
#231210=CARTESIAN_POINT('Ctrl Pts',(19.4843230052521,59.7398178213045,2.66766759643996));
#231211=CARTESIAN_POINT('Ctrl Pts',(19.4896904492933,59.7353118462118,2.67012012783172));
#231212=CARTESIAN_POINT('Ctrl Pts',(19.4923741713139,59.7330588586655,2.67134639352759));
#231213=CARTESIAN_POINT('Ctrl Pts',(19.4949638171735,59.7307414364082,2.67265375585035));
#231214=CARTESIAN_POINT('Ctrl Pts',(19.4974550439415,59.72836960219,2.67403135126963));
#231215=CARTESIAN_POINT('Ctrl Pts',(19.4987006573255,59.7271836850809,2.67472014897927));
#231216=CARTESIAN_POINT('Ctrl Pts',(19.4999216825137,59.7259841596485,2.67542649668656));
#231217=CARTESIAN_POINT('Ctrl Pts',(19.5011176808521,59.7247722453469,2.67614899656125));
#231218=CARTESIAN_POINT('Ctrl Pts',(19.5014166804367,59.7244692667715,2.67632962152992));
#231219=CARTESIAN_POINT('Ctrl Pts',(19.5017141161967,59.7241655137792,2.67651125590973));
#231220=CARTESIAN_POINT('Ctrl Pts',(19.5020099819911,59.7238610051972,2.67669387767546));
#231221=CARTESIAN_POINT('Ctrl Pts',(19.5028975793744,59.7229474794513,2.67724174297267));
#231222=CARTESIAN_POINT('Ctrl Pts',(19.5037710453008,59.7220271539531,2.6777984950477));
#231223=CARTESIAN_POINT('Ctrl Pts',(19.5046302297524,59.7211005320716,2.67836353618032));
#231224=CARTESIAN_POINT('Ctrl Pts',(19.5105677273988,59.7146969999426,2.68226832098942));
#231225=CARTESIAN_POINT('Ctrl Pts',(19.5158784513273,59.7079999120045,2.6865915375144));
#231226=CARTESIAN_POINT('Ctrl Pts',(19.5206092977908,59.7011184102411,2.69123699486243));
#231227=CARTESIAN_POINT('Ctrl Pts',(19.5229605154971,59.6976983227543,2.69354577441269));
#231228=CARTESIAN_POINT('Ctrl Pts',(19.5251683423981,59.6942320938702,2.69593478828156));
#231229=CARTESIAN_POINT('Ctrl Pts',(19.5272373629643,59.6907301905173,2.69839565261244));
#231230=CARTESIAN_POINT('Ctrl Pts',(19.5318019313701,59.6830044686628,2.7038246868907));
#231231=CARTESIAN_POINT('Ctrl Pts',(19.5357011184427,59.6751122606221,2.70961155815111));
#231232=CARTESIAN_POINT('Ctrl Pts',(19.5389266512982,59.6671986827534,2.71562701361793));
#231233=CARTESIAN_POINT('Ctrl Pts',(19.5401049791264,59.6643077529625,2.71782453535883));
#231234=CARTESIAN_POINT('Ctrl Pts',(19.541201362078,59.6614137631516,2.72005051502428));
#231235=CARTESIAN_POINT('Ctrl Pts',(19.5422187365067,59.6585211429016,2.72229986760142));
#231236=CARTESIAN_POINT('Ctrl Pts',(19.5456359895577,59.6488051375692,2.72985520488895));
#231237=CARTESIAN_POINT('Ctrl Pts',(19.5481755652422,59.6390401911878,2.73770845534539));
#231238=CARTESIAN_POINT('Ctrl Pts',(19.5499445144591,59.6292970278069,2.7457670670171));
#231239=CARTESIAN_POINT('Ctrl Pts',(19.5518887991943,59.6185881370977,2.75462443584964));
#231240=CARTESIAN_POINT('Ctrl Pts',(19.552902397614,59.6079049297422,2.76373036323094));
#231241=CARTESIAN_POINT('Ctrl Pts',(19.5530800481819,59.5973174182832,2.77299664636706));
#231242=CARTESIAN_POINT('Ctrl Pts',(19.5532713854553,59.5859142148031,2.78297683033335));
#231243=CARTESIAN_POINT('Ctrl Pts',(19.5524931697994,59.574620836218,2.79314401478723));
#231244=CARTESIAN_POINT('Ctrl Pts',(19.5508078878564,59.5635130675447,2.80341452427733));
#231245=CARTESIAN_POINT('Ctrl Pts',(19.5491453629098,59.5525552912523,2.81354634721241));
#231246=CARTESIAN_POINT('Ctrl Pts',(19.5465995868775,59.5417768065764,2.82378004209164));
#231247=CARTESIAN_POINT('Ctrl Pts',(19.5431821162865,59.5312589135998,2.83404198860304));
#231248=CARTESIAN_POINT('Ctrl Pts',(18.4801050014189,56.2594439784241,2.83404198860301));
#231249=CARTESIAN_POINT('Ctrl Pts',(18.4768344633037,56.2493782971091,2.82422126443159));
#231250=CARTESIAN_POINT('Ctrl Pts',(18.4727817672096,56.2396067681233,2.81442815028768));
#231251=CARTESIAN_POINT('Ctrl Pts',(18.4679768367048,56.2301791400457,2.80471618166696));
#231252=CARTESIAN_POINT('Ctrl Pts',(18.4633372535458,56.2210759356572,2.79533842146675));
#231253=CARTESIAN_POINT('Ctrl Pts',(18.4579956735941,56.2122922812587,2.78603515650751));
#231254=CARTESIAN_POINT('Ctrl Pts',(18.4519372213388,56.203891776328,2.77685887347329));
#231255=CARTESIAN_POINT('Ctrl Pts',(18.4462100865676,56.1959506682931,2.76818441217179));
#231256=CARTESIAN_POINT('Ctrl Pts',(18.4398418135319,56.1883512165521,2.75962261522253));
#231257=CARTESIAN_POINT('Ctrl Pts',(18.4327901596667,56.1811768067775,2.75123537702312));
#231258=CARTESIAN_POINT('Ctrl Pts',(18.4262957047571,56.1745692957346,2.74351087134775));
#231259=CARTESIAN_POINT('Ctrl Pts',(18.419221177347,56.1683219623554,2.73593399450505));
#231260=CARTESIAN_POINT('Ctrl Pts',(18.4115142492222,56.1625328136801,2.72857657813234));
#231261=CARTESIAN_POINT('Ctrl Pts',(18.4092161988284,56.1608066064056,2.72638274508767));
#231262=CARTESIAN_POINT('Ctrl Pts',(18.4068618032004,56.1591213928279,2.72420861709834));
#231263=CARTESIAN_POINT('Ctrl Pts',(18.4044493827314,56.1574804751189,2.72205663736748));
#231264=CARTESIAN_POINT('Ctrl Pts',(18.4020616112563,56.1558563235463,2.71992664556786));
#231265=CARTESIAN_POINT('Ctrl Pts',(18.3996196264082,56.1542770260205,2.71782089927905));
#231266=CARTESIAN_POINT('Ctrl Pts',(18.3971247125286,56.1527473834686,2.71574387311266));
#231267=CARTESIAN_POINT('Ctrl Pts',(18.3969512210967,56.152641015117,2.71559944077507));
#231268=CARTESIAN_POINT('Ctrl Pts',(18.3967774746434,56.1525348749439,2.7154551521609));
#231269=CARTESIAN_POINT('Ctrl Pts',(18.3966034726925,56.1524289641635,2.71531100781751));
#231270=CARTESIAN_POINT('Ctrl Pts',(18.388974589749,56.1477854475703,2.70899119176095));
#231271=CARTESIAN_POINT('Ctrl Pts',(18.3808409394272,56.1436260014307,2.70298296066842));
#231272=CARTESIAN_POINT('Ctrl Pts',(18.3722424849456,56.1400597146375,2.69736727774133));
#231273=CARTESIAN_POINT('Ctrl Pts',(18.3642272309672,56.1367353155297,2.69213248525407));
#231274=CARTESIAN_POINT('Ctrl Pts',(18.355807270034,56.1339262909282,2.68723866185431));
#231275=CARTESIAN_POINT('Ctrl Pts',(18.3470212548457,56.1317496772148,2.68278595829514));
#231276=CARTESIAN_POINT('Ctrl Pts',(18.3438072168237,56.1309534437592,2.68115710172782));
#231277=CARTESIAN_POINT('Ctrl Pts',(18.3405443147877,56.1302421351292,2.6795876363781));
#231278=CARTESIAN_POINT('Ctrl Pts',(18.3372349828464,56.1296225724749,2.67808378645387));
#231279=CARTESIAN_POINT('Ctrl Pts',(18.3364391990694,56.1294735883543,2.67772216078622));
#231280=CARTESIAN_POINT('Ctrl Pts',(18.3356401993826,56.1293301519983,2.67736403603585));
#231281=CARTESIAN_POINT('Ctrl Pts',(18.3348380918585,56.1291923454417,2.67700956934501));
#231282=CARTESIAN_POINT('Ctrl Pts',(18.3340610501946,56.1290588453401,2.67666617973826));
#231283=CARTESIAN_POINT('Ctrl Pts',(18.333281091922,56.1289306286649,2.67632622314141));
#231284=CARTESIAN_POINT('Ctrl Pts',(18.3324983188931,56.128807768806,2.67598984158795));
#231285=CARTESIAN_POINT('Ctrl Pts',(18.3239221357308,56.127461697065,2.67230439292247));
#231286=CARTESIAN_POINT('Ctrl Pts',(18.3150023767875,56.1267581593461,2.66904964540004));
#231287=CARTESIAN_POINT('Ctrl Pts',(18.3059033598551,56.1267895336333,2.66640203566755));
#231288=CARTESIAN_POINT('Ctrl Pts',(18.3021297263205,56.1268025454853,2.66530399299466));
#231289=CARTESIAN_POINT('Ctrl Pts',(18.2983254984048,56.12694160832,2.66430995142282));
#231290=CARTESIAN_POINT('Ctrl Pts',(18.2945030089056,56.1272115877757,2.6634305347338));
#231291=CARTESIAN_POINT('Ctrl Pts',(18.2879833547333,56.1276720658711,2.66193059792904));
#231292=CARTESIAN_POINT('Ctrl Pts',(18.2814124323572,56.1285150529073,2.66076519817146));
#231293=CARTESIAN_POINT('Ctrl Pts',(18.2748585331713,56.1297657127891,2.65997805604477));
#231294=CARTESIAN_POINT('Ctrl Pts',(18.2715815835783,56.13039104273,2.65958448498143));
#231295=CARTESIAN_POINT('Ctrl Pts',(18.2683092720867,56.1311196862932,2.65928526260779));
#231296=CARTESIAN_POINT('Ctrl Pts',(18.2650501911674,56.1319548233215,2.65908463971341));
#231297=CARTESIAN_POINT('Ctrl Pts',(18.2617911102481,56.1327899603497,2.65888401681904));
#231298=CARTESIAN_POINT('Ctrl Pts',(18.2585452947514,56.1337315613411,2.65878198860301));
#231299=CARTESIAN_POINT('Ctrl Pts',(18.2553202812748,56.1347810195644,2.65878198860301));
#231300=CARTESIAN_POINT('Origin',(12.0988124084938,56.9937374973465,2.83404198860302));
#231301=CARTESIAN_POINT('Ctrl Pts',(12.8407372733096,61.3271735965896,2.83404198860304));
#231302=CARTESIAN_POINT('Ctrl Pts',(12.8429432848611,61.3375520649565,2.82419652440087));
#231303=CARTESIAN_POINT('Ctrl Pts',(12.8459616464944,61.347725676909,2.81438790575653));
#231304=CARTESIAN_POINT('Ctrl Pts',(12.8497656413963,61.3576417279037,2.80466781256891));
#231305=CARTESIAN_POINT('Ctrl Pts',(12.8534460291152,61.3672355662872,2.79526356453056));
#231306=CARTESIAN_POINT('Ctrl Pts',(12.8578623484999,61.3765894879247,2.785941024962));
#231307=CARTESIAN_POINT('Ctrl Pts',(12.8630345798925,61.3856422574874,2.77675109088739));
#231308=CARTESIAN_POINT('Ctrl Pts',(12.8679271923023,61.3942056200564,2.76805797913634));
#231309=CARTESIAN_POINT('Ctrl Pts',(12.8734966517572,61.4025003187132,2.75948271210106));
#231310=CARTESIAN_POINT('Ctrl Pts',(12.8797929832537,61.4104485116955,2.75108575573163));
#231311=CARTESIAN_POINT('Ctrl Pts',(12.8855923599243,61.4177693722601,2.74335155163202));
#231312=CARTESIAN_POINT('Ctrl Pts',(12.8920087864975,61.4247966697209,2.73576818685869));
#231313=CARTESIAN_POINT('Ctrl Pts',(12.8991043342901,61.431439001463,2.72840626160418));
#231314=CARTESIAN_POINT('Ctrl Pts',(12.9011624829819,61.4333656894067,2.72627084693641));
#231315=CARTESIAN_POINT('Ctrl Pts',(12.903277908872,61.4352597571387,2.72415424587524));
#231316=CARTESIAN_POINT('Ctrl Pts',(12.9054524645843,61.437118361331,2.72205867173299));
#231317=CARTESIAN_POINT('Ctrl Pts',(12.9078098227881,61.4391332077734,2.71978693462902));
#231318=CARTESIAN_POINT('Ctrl Pts',(12.9102326900447,61.4411043938525,2.71754411340803));
#231319=CARTESIAN_POINT('Ctrl Pts',(12.9127224163027,61.4430281531013,2.71533341844301));
#231320=CARTESIAN_POINT('Ctrl Pts',(12.9195554895544,61.4483079254552,2.70926614876448));
#231321=CARTESIAN_POINT('Ctrl Pts',(12.926909770583,61.4531896374538,2.70347381860465));
#231322=CARTESIAN_POINT('Ctrl Pts',(12.9347398820029,61.4575800373535,2.69804914171451));
#231323=CARTESIAN_POINT('Ctrl Pts',(12.9419040088454,61.4615970149014,2.69308585687261));
#231324=CARTESIAN_POINT('Ctrl Pts',(12.9494643722283,61.4651913207948,2.68842799053243));
#231325=CARTESIAN_POINT('Ctrl Pts',(12.9574154517105,61.4682744840804,2.68414767054275));
#231326=CARTESIAN_POINT('Ctrl Pts',(12.9613209959788,61.4697889238147,2.68204519134609));
#231327=CARTESIAN_POINT('Ctrl Pts',(12.9653208118552,61.4711795284102,2.68003431778559));
#231328=CARTESIAN_POINT('Ctrl Pts',(12.9694138336349,61.4724324898306,2.67812693945309));
#231329=CARTESIAN_POINT('Ctrl Pts',(12.970190444651,61.4726702270561,2.67776503299261));
#231330=CARTESIAN_POINT('Ctrl Pts',(12.9709708853391,61.4729027677277,2.67740659639981));
#231331=CARTESIAN_POINT('Ctrl Pts',(12.9717550556846,61.4731300138565,2.67705178968912));
#231332=CARTESIAN_POINT('Ctrl Pts',(12.9725147207069,61.4733501585437,2.67670807068815));
#231333=CARTESIAN_POINT('Ctrl Pts',(12.9732778859006,61.4735653344327,2.67636775825322));
#231334=CARTESIAN_POINT('Ctrl Pts',(12.9740444565835,61.4737754532576,2.67603099699312));
#231335=CARTESIAN_POINT('Ctrl Pts',(12.9823983859297,61.4760652849148,2.67236104217185));
#231336=CARTESIAN_POINT('Ctrl Pts',(12.9911623597379,61.4777556486133,2.66911440541531));
#231337=CARTESIAN_POINT('Ctrl Pts',(13.00018336166,61.4787331403172,2.66646778189688));
#231338=CARTESIAN_POINT('Ctrl Pts',(13.0039929867894,61.4791459411337,2.66535009635031));
#231339=CARTESIAN_POINT('Ctrl Pts',(13.0078481668565,61.4794319383913,2.66433897912401));
#231340=CARTESIAN_POINT('Ctrl Pts',(13.011736540843,61.479584339472,2.66344564884849));
#231341=CARTESIAN_POINT('Ctrl Pts',(13.0182844654763,61.4798409790836,2.66194130298642));
#231342=CARTESIAN_POINT('Ctrl Pts',(13.0249248230174,61.4797168922659,2.66077206705476));
#231343=CARTESIAN_POINT('Ctrl Pts',(13.0315916763176,61.4791780149469,2.6599822515577));
#231344=CARTESIAN_POINT('Ctrl Pts',(13.0332583896426,61.4790432956171,2.65978479768344));
#231345=CARTESIAN_POINT('Ctrl Pts',(13.0349267248715,61.4788824204062,2.65961098966678));
#231346=CARTESIAN_POINT('Ctrl Pts',(13.0365955947403,61.4786945538951,2.65946139030557));
#231347=CARTESIAN_POINT('Ctrl Pts',(13.0390988995433,61.4784127541283,2.65923699126376));
#231348=CARTESIAN_POINT('Ctrl Pts',(13.04160338921,61.4780702140294,2.65906707562498));
#231349=CARTESIAN_POINT('Ctrl Pts',(13.0441057251028,61.4776657592308,2.65895332562975));
#231350=CARTESIAN_POINT('Ctrl Pts',(13.0466080609957,61.4772613044323,2.65883957563453));
#231351=CARTESIAN_POINT('Ctrl Pts',(13.0491082380627,61.4767949453823,2.65878198860305));
#231352=CARTESIAN_POINT('Ctrl Pts',(13.0516031943527,61.4762657165318,2.65878198860305));
#231353=CARTESIAN_POINT('Ctrl Pts',(12.2578193919766,57.7418065394568,2.65878198860302));
#231354=CARTESIAN_POINT('Ctrl Pts',(12.249377180707,57.7435970583547,2.65878198860302));
#231355=CARTESIAN_POINT('Ctrl Pts',(12.2411559442237,57.7460689269806,2.65945335517902));
#231356=CARTESIAN_POINT('Ctrl Pts',(12.2332613533214,57.749114125811,2.6607256122666));
#231357=CARTESIAN_POINT('Ctrl Pts',(12.2281622576309,57.7510810117997,2.66154735980396));
#231358=CARTESIAN_POINT('Ctrl Pts',(12.223199086688,57.7532862127608,2.66261895766933));
#231359=CARTESIAN_POINT('Ctrl Pts',(12.2183955094118,57.755693185958,2.66391429251067));
#231360=CARTESIAN_POINT('Ctrl Pts',(12.2120286428976,57.7588834910513,2.66563118464164));
#231361=CARTESIAN_POINT('Ctrl Pts',(12.2059457447516,57.7624328173677,2.66774105138739));
#231362=CARTESIAN_POINT('Ctrl Pts',(12.2001996238499,57.7662682043711,2.6701689418179));
#231363=CARTESIAN_POINT('Ctrl Pts',(12.1973265633991,57.7681858978728,2.67138288703316));
#231364=CARTESIAN_POINT('Ctrl Pts',(12.1945375019637,57.7701751462712,2.67267613167592));
#231365=CARTESIAN_POINT('Ctrl Pts',(12.1918376559072,57.772227116147,2.67403835432593));
#231366=CARTESIAN_POINT('Ctrl Pts',(12.190487732879,57.7732531010849,2.67471946565094));
#231367=CARTESIAN_POINT('Ctrl Pts',(12.1891600976133,57.7742947697605,2.67541781389563));
#231368=CARTESIAN_POINT('Ctrl Pts',(12.1878553011596,57.7753510390206,2.6761320724421));
#231369=CARTESIAN_POINT('Ctrl Pts',(12.1875291020462,57.7756151063357,2.67631063707871));
#231370=CARTESIAN_POINT('Ctrl Pts',(12.1872043300163,57.7758800862579,2.67649019601886));
#231371=CARTESIAN_POINT('Ctrl Pts',(12.1868809929896,57.7761459620051,2.67667072836697));
#231372=CARTESIAN_POINT('Ctrl Pts',(12.1859109819096,57.7769435892467,2.67721232541131));
#231373=CARTESIAN_POINT('Ctrl Pts',(12.1849538875689,57.7777492785676,2.67776268340088));
#231374=CARTESIAN_POINT('Ctrl Pts',(12.1840099085256,57.7785625799464,2.67832123541557));
#231375=CARTESIAN_POINT('Ctrl Pts',(12.1773606420347,57.7842913698426,2.6822556036849));
#231376=CARTESIAN_POINT('Ctrl Pts',(12.1713100228962,57.7903843352501,2.68661792998939));
#231377=CARTESIAN_POINT('Ctrl Pts',(12.1658251565855,57.796726433441,2.69130986622634));
#231378=CARTESIAN_POINT('Ctrl Pts',(12.1631650023519,57.7998023442102,2.69358545023106));
#231379=CARTESIAN_POINT('Ctrl Pts',(12.1606380046011,57.8029374300327,2.69593918853516));
#231380=CARTESIAN_POINT('Ctrl Pts',(12.1582411305897,57.8061213360081,2.69836306235516));
#231381=CARTESIAN_POINT('Ctrl Pts',(12.1545716839429,57.8109956736034,2.70207384382249));
#231382=CARTESIAN_POINT('Ctrl Pts',(12.1512083732206,57.8159810988992,2.70594760814249));
#231383=CARTESIAN_POINT('Ctrl Pts',(12.1481495009385,57.8210315314443,2.70995196345728));
#231384=CARTESIAN_POINT('Ctrl Pts',(12.1467289448262,57.8233769784457,2.71181160678126));
#231385=CARTESIAN_POINT('Ctrl Pts',(12.1453738842984,57.8257362497573,2.71369962772119));
#231386=CARTESIAN_POINT('Ctrl Pts',(12.1440853170069,57.828105124615,2.71561183138682));
#231387=CARTESIAN_POINT('Ctrl Pts',(12.1439865534012,57.828286689539,2.71575839426332));
#231388=CARTESIAN_POINT('Ctrl Pts',(12.1438881466795,57.8284683073401,2.7159050890323));
#231389=CARTESIAN_POINT('Ctrl Pts',(12.143790096302,57.8286499766613,2.71605191409932));
#231390=CARTESIAN_POINT('Ctrl Pts',(12.1424127841096,57.8312018829081,2.71811436362774));
#231391=CARTESIAN_POINT('Ctrl Pts',(12.1411075562953,57.8337650648329,2.7202009102698));
#231392=CARTESIAN_POINT('Ctrl Pts',(12.1398727334219,57.8363340693142,2.72230624862203));
#231393=CARTESIAN_POINT('Ctrl Pts',(12.1354448782037,57.8455460625025,2.72985561753145));
#231394=CARTESIAN_POINT('Ctrl Pts',(12.1318862976809,57.8549032874811,2.73770089914395));
#231395=CARTESIAN_POINT('Ctrl Pts',(12.129096878378,57.8643241951544,2.74574823347162));
#231396=CARTESIAN_POINT('Ctrl Pts',(12.1260315867862,57.8746768262734,2.75459144547137));
#231397=CARTESIAN_POINT('Ctrl Pts',(12.1238947812338,57.8851069357383,2.76367911754407));
#231398=CARTESIAN_POINT('Ctrl Pts',(12.1225979458246,57.8955352825149,2.7729216256489));
#231399=CARTESIAN_POINT('Ctrl Pts',(12.1211976890438,57.9067952798761,2.78290121484937));
#231400=CARTESIAN_POINT('Ctrl Pts',(12.1207764137885,57.918054344326,2.79306229500438));
#231401=CARTESIAN_POINT('Ctrl Pts',(12.121277094834,57.9292311407304,2.80331916685547));
#231402=CARTESIAN_POINT('Ctrl Pts',(12.1217735756798,57.9403141752953,2.81348999408905));
#231403=CARTESIAN_POINT('Ctrl Pts',(12.1231769533538,57.9513177099582,2.82375635967002));
#231404=CARTESIAN_POINT('Ctrl Pts',(12.125481593379,57.9621601888123,2.83404198860303));
#231405=CARTESIAN_POINT('Origin',(0.0149069694351876,-0.00316857416787864,
2.83404198860262));
#231406=CARTESIAN_POINT('Ctrl Pts',(13.0814171332231,61.4699285681957,2.65878198860305));
#231407=CARTESIAN_POINT('Ctrl Pts',(13.0898176309846,61.4681393149851,2.65878198860305));
#231408=CARTESIAN_POINT('Ctrl Pts',(13.097994011884,61.4656642256292,2.65944603041891));
#231409=CARTESIAN_POINT('Ctrl Pts',(13.1058430982607,61.4626133761161,2.66070439264107));
#231410=CARTESIAN_POINT('Ctrl Pts',(13.1108582907973,61.4606640285138,2.66150842619632));
#231411=CARTESIAN_POINT('Ctrl Pts',(13.1157402208611,61.4584804838817,2.66255428265406));
#231412=CARTESIAN_POINT('Ctrl Pts',(13.1204666715205,61.4560986543958,2.66381699700696));
#231413=CARTESIAN_POINT('Ctrl Pts',(13.1269173283005,61.4528479350656,2.66554034873295));
#231414=CARTESIAN_POINT('Ctrl Pts',(13.1330744924004,61.4492231901486,2.66766759643999));
#231415=CARTESIAN_POINT('Ctrl Pts',(13.1388835356735,61.4453029499363,2.67012012783174));
#231416=CARTESIAN_POINT('Ctrl Pts',(13.1417880573101,61.4433428298302,2.67134639352762));
#231417=CARTESIAN_POINT('Ctrl Pts',(13.144605753406,61.4413087943566,2.67265375585038));
#231418=CARTESIAN_POINT('Ctrl Pts',(13.147331257159,61.4392103574001,2.67403135126966));
#231419=CARTESIAN_POINT('Ctrl Pts',(13.1486940090356,61.4381611389218,2.67472014897929));
#231420=CARTESIAN_POINT('Ctrl Pts',(13.1500337298701,61.4370958165019,2.67542649668658));
#231421=CARTESIAN_POINT('Ctrl Pts',(13.1513498559441,61.436015557062,2.67614899656127));
#231422=CARTESIAN_POINT('Ctrl Pts',(13.1516788874626,61.4357454922021,2.67632962152994));
#231423=CARTESIAN_POINT('Ctrl Pts',(13.1520064446718,61.4354744937033,2.67651125590976));
#231424=CARTESIAN_POINT('Ctrl Pts',(13.1523325194966,61.435202579648,2.67669387767549));
#231425=CARTESIAN_POINT('Ctrl Pts',(13.153310743971,61.4343868374822,2.67724174297269));
#231426=CARTESIAN_POINT('Ctrl Pts',(13.1542756251696,61.4335628556744,2.67779849504773));
#231427=CARTESIAN_POINT('Ctrl Pts',(13.1552269612802,61.4327311191549,2.67836353618034));
#231428=CARTESIAN_POINT('Ctrl Pts',(13.161801284066,61.4269833037496,2.68226832098935));
#231429=CARTESIAN_POINT('Ctrl Pts',(13.1677829516035,61.4208780249713,2.68659153751421));
#231430=CARTESIAN_POINT('Ctrl Pts',(13.1732071947994,61.4145287289055,2.69123699486212));
#231431=CARTESIAN_POINT('Ctrl Pts',(13.1759030287784,61.4113731461893,2.69354577441247));
#231432=CARTESIAN_POINT('Ctrl Pts',(13.1784610805514,61.4081566864227,2.69593478828145));
#231433=CARTESIAN_POINT('Ctrl Pts',(13.1808848153825,61.4048902384028,2.69839565261245));
#231434=CARTESIAN_POINT('Ctrl Pts',(13.1862319364381,61.397683966182,2.70382468689071));
#231435=CARTESIAN_POINT('Ctrl Pts',(13.1909347237342,61.3902425685154,2.70961155815112));
#231436=CARTESIAN_POINT('Ctrl Pts',(13.1949697809168,61.3827095020468,2.71562701361793));
#231437=CARTESIAN_POINT('Ctrl Pts',(13.1964438381903,61.3799575778689,2.71782453535884));
#231438=CARTESIAN_POINT('Ctrl Pts',(13.197836719349,61.3771940448621,2.72005051502428));
#231439=CARTESIAN_POINT('Ctrl Pts',(13.1991508816437,61.374423615274,2.72229986760141));
#231440=CARTESIAN_POINT('Ctrl Pts',(13.2035650137316,61.3651180354451,2.72985520488924));
#231441=CARTESIAN_POINT('Ctrl Pts',(13.207111392194,61.3556720404048,2.73770845534598));
#231442=CARTESIAN_POINT('Ctrl Pts',(13.2098890888177,61.3461671566351,2.745767067018));
#231443=CARTESIAN_POINT('Ctrl Pts',(13.2129421064468,61.3357201634447,2.75462443585087));
#231444=CARTESIAN_POINT('Ctrl Pts',(13.2150668515159,61.3252014297016,2.7637303632325));
#231445=CARTESIAN_POINT('Ctrl Pts',(13.216350225198,61.3146904872786,2.77299664636899));
#231446=CARTESIAN_POINT('Ctrl Pts',(13.2177324736418,61.3033697519308,2.78297683033573));
#231447=CARTESIAN_POINT('Ctrl Pts',(13.2181390006411,61.2920568939681,2.7931440147901));
#231448=CARTESIAN_POINT('Ctrl Pts',(13.2176240288385,61.2808338148818,2.80341452428073));
#231449=CARTESIAN_POINT('Ctrl Pts',(13.2171160108939,61.2697622852581,2.81354634721465));
#231450=CARTESIAN_POINT('Ctrl Pts',(13.2157108393287,61.2587767401939,2.82378004209273));
#231451=CARTESIAN_POINT('Ctrl Pts',(13.2134115091892,61.247959242388,2.83404198860305));
#231452=CARTESIAN_POINT('Ctrl Pts',(12.4981558292586,57.8829458346107,2.83404198860302));
#231453=CARTESIAN_POINT('Ctrl Pts',(12.4959553576928,57.8725934298276,2.82422126443134));
#231454=CARTESIAN_POINT('Ctrl Pts',(12.4929462656005,57.862451808205,2.81442815028716));
#231455=CARTESIAN_POINT('Ctrl Pts',(12.4891531124829,57.8525735736584,2.80471618166619));
#231456=CARTESIAN_POINT('Ctrl Pts',(12.4854904894114,57.8430352690781,2.79533842146582));
#231457=CARTESIAN_POINT('Ctrl Pts',(12.4810963130895,57.8337413853135,2.78603515650642));
#231458=CARTESIAN_POINT('Ctrl Pts',(12.4759491415405,57.8247536185236,2.77685887347205));
#231459=CARTESIAN_POINT('Ctrl Pts',(12.4710834524322,57.8162573641128,2.7681844121705));
#231460=CARTESIAN_POINT('Ctrl Pts',(12.4655444244746,57.8080338771694,2.75962261522118));
#231461=CARTESIAN_POINT('Ctrl Pts',(12.4592813303356,57.8001616710202,2.75123537702172));
#231462=CARTESIAN_POINT('Ctrl Pts',(12.4535131257047,57.7929115012227,2.74351087134634));
#231463=CARTESIAN_POINT('Ctrl Pts',(12.4471303774535,57.7859589019109,2.73593399450363));
#231464=CARTESIAN_POINT('Ctrl Pts',(12.4400707995019,57.7793958734444,2.72857657813092));
#231465=CARTESIAN_POINT('Ctrl Pts',(12.4379657758627,57.7774389108382,2.72638274508673));
#231466=CARTESIAN_POINT('Ctrl Pts',(12.4358004306464,57.7755168276804,2.72420861709788));
#231467=CARTESIAN_POINT('Ctrl Pts',(12.433572748276,57.7736327324863,2.72205663736748));
#231468=CARTESIAN_POINT('Ctrl Pts',(12.4313678273309,57.771767888103,2.71992664556787));
#231469=CARTESIAN_POINT('Ctrl Pts',(12.4291043014747,57.7699419852108,2.71782089927905));
#231470=CARTESIAN_POINT('Ctrl Pts',(12.4267829461797,57.768159932687,2.71574387311267));
#231471=CARTESIAN_POINT('Ctrl Pts',(12.4266215236723,57.7680360122397,2.71559944077507));
#231472=CARTESIAN_POINT('Ctrl Pts',(12.4264598236895,57.7679122920637,2.7154551521609));
#231473=CARTESIAN_POINT('Ctrl Pts',(12.4262978456307,57.7677887733172,2.71531100781751));
#231474=CARTESIAN_POINT('Ctrl Pts',(12.4191961341597,57.7623732589831,2.70899119176094));
#231475=CARTESIAN_POINT('Ctrl Pts',(12.4115418213385,57.7573864007559,2.7029829606684));
#231476=CARTESIAN_POINT('Ctrl Pts',(12.4033632485682,57.7529408672214,2.6973672777413));
#231477=CARTESIAN_POINT('Ctrl Pts',(12.3957393973198,57.7487968573387,2.69213248525403));
#231478=CARTESIAN_POINT('Ctrl Pts',(12.3876591848384,57.7451230952907,2.68723866185426));
#231479=CARTESIAN_POINT('Ctrl Pts',(12.3791488184472,57.7420400166291,2.68278595829508));
#231480=CARTESIAN_POINT('Ctrl Pts',(12.3760356163213,57.7409121865684,2.68115710172778));
#231481=CARTESIAN_POINT('Ctrl Pts',(12.3728649408021,57.7398637084259,2.67958763637807));
#231482=CARTESIAN_POINT('Ctrl Pts',(12.3696384996596,57.7389016204184,2.67808378645385));
#231483=CARTESIAN_POINT('Ctrl Pts',(12.3688626483506,57.7386702703931,2.6777221607862));
#231484=CARTESIAN_POINT('Ctrl Pts',(12.3680830188495,57.738444101587,2.67736403603583));
#231485=CARTESIAN_POINT('Ctrl Pts',(12.367299710062,57.7382232068823,2.67700956934499));
#231486=CARTESIAN_POINT('Ctrl Pts',(12.3665408796741,57.7380092151372,2.67666617973824));
#231487=CARTESIAN_POINT('Ctrl Pts',(12.3657785963866,57.7378001730067,2.67632622314139));
#231488=CARTESIAN_POINT('Ctrl Pts',(12.3650129538224,57.7375961641251,2.67598984158793));
#231489=CARTESIAN_POINT('Ctrl Pts',(12.3566244546995,57.7353610110593,2.67230439292252));
#231490=CARTESIAN_POINT('Ctrl Pts',(12.3478270988458,57.7337289586987,2.66904964540014));
#231491=CARTESIAN_POINT('Ctrl Pts',(12.3387746477744,57.732809054857,2.66640203566768));
#231492=CARTESIAN_POINT('Ctrl Pts',(12.3350203264901,57.7324275433144,2.66530399299474));
#231493=CARTESIAN_POINT('Ctrl Pts',(12.3312224025083,57.7321681942504,2.66430995142285));
#231494=CARTESIAN_POINT('Ctrl Pts',(12.3273926324687,57.7320371357771,2.66343053473379));
#231495=CARTESIAN_POINT('Ctrl Pts',(12.3208605605765,57.7318136018937,2.66193059792903));
#231496=CARTESIAN_POINT('Ctrl Pts',(12.3142375182613,57.7319651225405,2.66076519817146));
#231497=CARTESIAN_POINT('Ctrl Pts',(12.3075887924653,57.7325238621662,2.65997805604478));
#231498=CARTESIAN_POINT('Ctrl Pts',(12.3042644295673,57.7328032319791,2.65958448498144));
#231499=CARTESIAN_POINT('Ctrl Pts',(12.3009338801485,57.7331858342652,2.6592852626078));
#231500=CARTESIAN_POINT('Ctrl Pts',(12.2976053572253,57.7336757296052,2.65908463971342));
#231501=CARTESIAN_POINT('Ctrl Pts',(12.2942768343021,57.7341656249453,2.65888401681905));
#231502=CARTESIAN_POINT('Ctrl Pts',(12.2909503756177,57.734762787642,2.65878198860302));
#231503=CARTESIAN_POINT('Ctrl Pts',(12.2876333308469,57.7354693911207,2.65878198860302));
#231504=CARTESIAN_POINT('Origin',(6.07506605172281,57.9461901084064,2.83404198860303));
#231505=CARTESIAN_POINT('Ctrl Pts',(6.35995915837782,62.3334394572621,2.83404198860306));
#231506=CARTESIAN_POINT('Ctrl Pts',(6.36106823981771,62.3439916622907,2.82419652440113));
#231507=CARTESIAN_POINT('Ctrl Pts',(6.36300663452681,62.3544250468354,2.81438790575701));
#231508=CARTESIAN_POINT('Ctrl Pts',(6.36575328117443,62.3646844024064,2.80466781256959));
#231509=CARTESIAN_POINT('Ctrl Pts',(6.3684106781612,62.3746103900118,2.7952635645314));
#231510=CARTESIAN_POINT('Ctrl Pts',(6.37182505343177,62.3843747009663,2.785941024963));
#231511=CARTESIAN_POINT('Ctrl Pts',(6.37602267870884,62.3939185239092,2.77675109088852));
#231512=CARTESIAN_POINT('Ctrl Pts',(6.37999337374607,62.4029463927383,2.7680579791376));
#231513=CARTESIAN_POINT('Ctrl Pts',(6.38466529101529,62.411777819206,2.75948271210245));
#231514=CARTESIAN_POINT('Ctrl Pts',(6.39009631815072,62.4203406170109,2.75108575573312));
#231515=CARTESIAN_POINT('Ctrl Pts',(6.39509868692433,62.4282275730665,2.74335155163362));
#231516=CARTESIAN_POINT('Ctrl Pts',(6.40074541103664,62.4358870734658,2.73576818686039));
#231517=CARTESIAN_POINT('Ctrl Pts',(6.40710777594623,62.4432347045263,2.72840626160597));
#231518=CARTESIAN_POINT('Ctrl Pts',(6.40895325615472,62.4453659729923,2.7262708469376));
#231519=CARTESIAN_POINT('Ctrl Pts',(6.41085910953164,62.4474707870411,2.72415424587584));
#231520=CARTESIAN_POINT('Ctrl Pts',(6.41282747576062,62.4495465125726,2.72205867173302));
#231521=CARTESIAN_POINT('Ctrl Pts',(6.41496131130727,62.4517967325058,2.71978693462905));
#231522=CARTESIAN_POINT('Ctrl Pts',(6.41716486079182,62.4540103788123,2.71754411340805));
#231523=CARTESIAN_POINT('Ctrl Pts',(6.41943986047092,62.4561838467664,2.71533341844302));
#231524=CARTESIAN_POINT('Ctrl Pts',(6.4256836149418,62.4621489466213,2.70926614876449));
#231525=CARTESIAN_POINT('Ctrl Pts',(6.43248733059615,62.4677726477851,2.70347381860466));
#231526=CARTESIAN_POINT('Ctrl Pts',(6.43981562609173,62.4729574661288,2.69804914171452));
#231527=CARTESIAN_POINT('Ctrl Pts',(6.44652061860817,62.4777012934232,2.69308585687231));
#231528=CARTESIAN_POINT('Ctrl Pts',(6.45366385825839,62.4820661824992,2.68842799053185));
#231529=CARTESIAN_POINT('Ctrl Pts',(6.4612491025755,62.4859635700135,2.68414767054195));
#231530=CARTESIAN_POINT('Ctrl Pts',(6.46497494980508,62.4878779540288,2.68204519134558));
#231531=CARTESIAN_POINT('Ctrl Pts',(6.46880749650976,62.4896790353535,2.68003431778536));
#231532=CARTESIAN_POINT('Ctrl Pts',(6.47274712615552,62.4913529701967,2.6781269394531));
#231533=CARTESIAN_POINT('Ctrl Pts',(6.4734946325084,62.4916705830289,2.67776503299262));
#231534=CARTESIAN_POINT('Ctrl Pts',(6.47424649074168,62.491983428084,2.67740659639982));
#231535=CARTESIAN_POINT('Ctrl Pts',(6.4750026116314,62.4922913974559,2.67705178968914));
#231536=CARTESIAN_POINT('Ctrl Pts',(6.47573510374332,62.4925897427849,2.67670807068816));
#231537=CARTESIAN_POINT('Ctrl Pts',(6.47647159623327,62.4928835124028,2.67636775825324));
#231538=CARTESIAN_POINT('Ctrl Pts',(6.47721200416386,62.4931726086303,2.67603099699313));
#231539=CARTESIAN_POINT('Ctrl Pts',(6.4852808172263,62.4963231197467,2.67236104217204));
#231540=CARTESIAN_POINT('Ctrl Pts',(6.49382008994886,62.4989203081702,2.66911440541564));
#231541=CARTESIAN_POINT('Ctrl Pts',(6.50268949817238,62.5008353965403,2.66646778189727));
#231542=CARTESIAN_POINT('Ctrl Pts',(6.50643510434214,62.5016441502512,2.66535009635055));
#231543=CARTESIAN_POINT('Ctrl Pts',(6.5102392704761,62.5023315568341,2.66433897912412));
#231544=CARTESIAN_POINT('Ctrl Pts',(6.5140904132927,62.5028895688031,2.6634456488485));
#231545=CARTESIAN_POINT('Ctrl Pts',(6.52057564156552,62.5038292470157,2.66194130298643));
#231546=CARTESIAN_POINT('Ctrl Pts',(6.52719259313764,62.5043999463279,2.66077206705477));
#231547=CARTESIAN_POINT('Ctrl Pts',(6.53387925273587,62.5045608969645,2.6599822515577));
#231548=CARTESIAN_POINT('Ctrl Pts',(6.53555091763543,62.5046011346237,2.65978479768344));
#231549=CARTESIAN_POINT('Ctrl Pts',(6.53722692958795,62.5046155292218,2.65961098966678));
#231550=CARTESIAN_POINT('Ctrl Pts',(6.53890629461062,62.5046031362659,2.65946139030558));
#231551=CARTESIAN_POINT('Ctrl Pts',(6.54142534214461,62.5045845468321,2.65923699126377));
#231552=CARTESIAN_POINT('Ctrl Pts',(6.54395191714495,62.5045056736599,2.65906707562498));
#231553=CARTESIAN_POINT('Ctrl Pts',(6.54648282201853,62.5043649998327,2.65895332562976));
#231554=CARTESIAN_POINT('Ctrl Pts',(6.54901372689211,62.5042243260055,2.65883957563454));
#231555=CARTESIAN_POINT('Ctrl Pts',(6.5515489555224,62.5040218613863,2.65878198860305));
#231556=CARTESIAN_POINT('Ctrl Pts',(6.55408556365926,62.5037563256537,2.65878198860305));
#231557=CARTESIAN_POINT('Ctrl Pts',(6.15500747092297,58.7067819056645,2.65878198860303));
#231558=CARTESIAN_POINT('Ctrl Pts',(6.14642434678111,58.707680164542,2.65878198860303));
#231559=CARTESIAN_POINT('Ctrl Pts',(6.13798976646258,58.7092791387971,2.65945335517905));
#231560=CARTESIAN_POINT('Ctrl Pts',(6.12982011300103,58.7114824462546,2.66072561226666));
#231561=CARTESIAN_POINT('Ctrl Pts',(6.12454335512052,58.7129055567995,2.66154735980401));
#231562=CARTESIAN_POINT('Ctrl Pts',(6.11937686667978,58.7145798848073,2.66261895766938));
#231563=CARTESIAN_POINT('Ctrl Pts',(6.11434800669314,58.7164715618027,2.6639142925107));
#231564=CARTESIAN_POINT('Ctrl Pts',(6.10768254085114,58.7189788712983,2.66563118464167));
#231565=CARTESIAN_POINT('Ctrl Pts',(6.1012619598322,58.7218729180383,2.66774105138743));
#231566=CARTESIAN_POINT('Ctrl Pts',(6.09514640967254,58.7250866612028,2.67016894181794));
#231567=CARTESIAN_POINT('Ctrl Pts',(6.09208863459271,58.726693532785,2.67138288703319));
#231568=CARTESIAN_POINT('Ctrl Pts',(6.08910691884953,58.7283803475668,2.67267613167595));
#231569=CARTESIAN_POINT('Ctrl Pts',(6.08620737357446,58.7301388657776,2.67403835432597));
#231570=CARTESIAN_POINT('Ctrl Pts',(6.08475760093692,58.7310181248829,2.67471946565098));
#231571=CARTESIAN_POINT('Ctrl Pts',(6.08332835457025,58.7319153115145,2.67541781389566));
#231572=CARTESIAN_POINT('Ctrl Pts',(6.08192029572552,58.7328294060529,2.67613207244213));
#231573=CARTESIAN_POINT('Ctrl Pts',(6.08156828101434,58.7330579296875,2.67631063707874));
#231574=CARTESIAN_POINT('Ctrl Pts',(6.08121759017549,58.7332875101008,2.67649019601889));
#231575=CARTESIAN_POINT('Ctrl Pts',(6.08086823283962,58.7335181314303,2.676670728367));
#231576=CARTESIAN_POINT('Ctrl Pts',(6.07982016083201,58.7342099954188,2.67721232541134));
#231577=CARTESIAN_POINT('Ctrl Pts',(6.0787840920876,58.7349112274887,2.67776268340091));
#231578=CARTESIAN_POINT('Ctrl Pts',(6.07776027111701,58.7356214008388,2.6783212354156));
#231579=CARTESIAN_POINT('Ctrl Pts',(6.07054860839945,58.7406237702164,2.68225560368493));
#231580=CARTESIAN_POINT('Ctrl Pts',(6.06389424687488,58.7460508958015,2.68661792998942));
#231581=CARTESIAN_POINT('Ctrl Pts',(6.05777649745789,58.7517849266683,2.69130986622638));
#231582=CARTESIAN_POINT('Ctrl Pts',(6.05480939560164,58.7545659254423,2.69358545023109));
#231583=CARTESIAN_POINT('Ctrl Pts',(6.05196853530569,58.7574196937451,2.69593918853518));
#231584=CARTESIAN_POINT('Ctrl Pts',(6.04925198282213,58.7603356163933,2.69836306235517));
#231585=CARTESIAN_POINT('Ctrl Pts',(6.04509313076974,58.7647996902382,2.7020738438225));
#231586=CARTESIAN_POINT('Ctrl Pts',(6.04122712577058,58.7694062431513,2.7059476081425));
#231587=CARTESIAN_POINT('Ctrl Pts',(6.03765709635815,58.7741092696795,2.7099519634573));
#231588=CARTESIAN_POINT('Ctrl Pts',(6.03599915623014,58.7762933795294,2.71181160678127));
#231589=CARTESIAN_POINT('Ctrl Pts',(6.03440490786103,58.7784980841113,2.71369962772121));
#231590=CARTESIAN_POINT('Ctrl Pts',(6.03287578462737,58.7807192900659,2.71561183138683));
#231591=CARTESIAN_POINT('Ctrl Pts',(6.03275858335656,58.7808895367503,2.71575839426334));
#231592=CARTESIAN_POINT('Ctrl Pts',(6.03264173148759,58.7810598733267,2.71590508903231));
#231593=CARTESIAN_POINT('Ctrl Pts',(6.0325252286253,58.781230298389,2.71605191409933));
#231594=CARTESIAN_POINT('Ctrl Pts',(6.03088871465485,58.7836242566995,2.71811436362775));
#231595=CARTESIAN_POINT('Ctrl Pts',(6.02932271154744,58.7860369637879,2.72020091026982));
#231596=CARTESIAN_POINT('Ctrl Pts',(6.02782611907238,58.7884628208565,2.72230624862204));
#231597=CARTESIAN_POINT('Ctrl Pts',(6.02245960461739,58.7971615128796,2.72985561753055));
#231598=CARTESIAN_POINT('Ctrl Pts',(6.01794242202412,58.8060955050461,2.73770089914207));
#231599=CARTESIAN_POINT('Ctrl Pts',(6.01418353045067,58.8151732302872,2.74574823346872));
#231600=CARTESIAN_POINT('Ctrl Pts',(6.0100528862257,58.8251487383885,2.75459144546705));
#231601=CARTESIAN_POINT('Ctrl Pts',(6.00683754300386,58.8352983536201,2.76367911753826));
#231602=CARTESIAN_POINT('Ctrl Pts',(6.0044577527316,58.8455340166078,2.77292162564155));
#231603=CARTESIAN_POINT('Ctrl Pts',(6.00188817648357,58.8565859638331,2.78290121483949));
#231604=CARTESIAN_POINT('Ctrl Pts',(6.0002923163131,58.8677393146921,2.7930622949919));
#231605=CARTESIAN_POINT('Ctrl Pts',(5.99962196122217,58.8789072188539,2.80331916684039));
#231606=CARTESIAN_POINT('Ctrl Pts',(5.99895722972127,58.8899814357811,2.81348999407889));
#231607=CARTESIAN_POINT('Ctrl Pts',(5.99920273697632,58.901071384847,2.82375635966493));
#231608=CARTESIAN_POINT('Ctrl Pts',(6.00036140429027,58.9120953679532,2.83404198860304));
#231609=CARTESIAN_POINT('Origin',(0.0151565136854175,-0.00159301378001511,
2.83404198860263));
#231610=CARTESIAN_POINT('Ctrl Pts',(6.58439859103009,62.5005702980933,2.65878198860306));
#231611=CARTESIAN_POINT('Ctrl Pts',(6.59294009787473,62.4996689377207,2.65878198860306));
#231612=CARTESIAN_POINT('Ctrl Pts',(6.60133040499113,62.4980620716937,2.65944603041897));
#231613=CARTESIAN_POINT('Ctrl Pts',(6.60945539386287,62.4958483879903,2.66070439264121));
#231614=CARTESIAN_POINT('Ctrl Pts',(6.61464687495897,62.4944339494871,2.66150842619644));
#231615=CARTESIAN_POINT('Ctrl Pts',(6.61973030386368,62.4927726671883,2.66255428265414));
#231616=CARTESIAN_POINT('Ctrl Pts',(6.62467983150747,62.4908979342378,2.66381699700697));
#231617=CARTESIAN_POINT('Ctrl Pts',(6.63143494361075,62.4883392999285,2.66554034873297));
#231618=CARTESIAN_POINT('Ctrl Pts',(6.63793726713745,62.4853780106449,2.66766759644002));
#231619=CARTESIAN_POINT('Ctrl Pts',(6.64412426454875,62.4820864562851,2.67012012783178));
#231620=CARTESIAN_POINT('Ctrl Pts',(6.6472177632544,62.4804406791052,2.67134639352766));
#231621=CARTESIAN_POINT('Ctrl Pts',(6.65023263831854,62.4787123157336,2.67265375585042));
#231622=CARTESIAN_POINT('Ctrl Pts',(6.65316255786721,62.4769102669532,2.6740313512697));
#231623=CARTESIAN_POINT('Ctrl Pts',(6.65462751764154,62.4760092425631,2.67472014897934));
#231624=CARTESIAN_POINT('Ctrl Pts',(6.65607125586062,62.4750897950508,2.67542649668662));
#231625=CARTESIAN_POINT('Ctrl Pts',(6.65749308991742,62.4741530260212,2.67614899656132));
#231626=CARTESIAN_POINT('Ctrl Pts',(6.65784854843162,62.4739188337638,2.67632962152999));
#231627=CARTESIAN_POINT('Ctrl Pts',(6.65820263830483,62.4736835588748,2.6765112559098));
#231628=CARTESIAN_POINT('Ctrl Pts',(6.65855534961595,62.4734472184936,2.67669387767554));
#231629=CARTESIAN_POINT('Ctrl Pts',(6.65961348354928,62.4727381973497,2.67724174297274));
#231630=CARTESIAN_POINT('Ctrl Pts',(6.66065920857987,62.4720195869494,2.67779849504777));
#231631=CARTESIAN_POINT('Ctrl Pts',(6.66169227331198,62.4712918484712,2.67836353618039));
#231632=CARTESIAN_POINT('Ctrl Pts',(6.66883139158122,62.4662627240579,2.68226832098947));
#231633=CARTESIAN_POINT('Ctrl Pts',(6.67541846632676,62.4608161451509,2.68659153751441));
#231634=CARTESIAN_POINT('Ctrl Pts',(6.68147667711152,62.4550686189988,2.6912369948624));
#231635=CARTESIAN_POINT('Ctrl Pts',(6.68448759124189,62.4522121142781,2.69354577441268));
#231636=CARTESIAN_POINT('Ctrl Pts',(6.68736784133606,62.4492806638355,2.69593478828158));
#231637=CARTESIAN_POINT('Ctrl Pts',(6.69011973548588,62.4462854590371,2.69839565261248));
#231638=CARTESIAN_POINT('Ctrl Pts',(6.69619082501402,62.4396775898763,2.70382468689073));
#231639=CARTESIAN_POINT('Ctrl Pts',(6.70164568781196,62.4327685320939,2.70961155815115));
#231640=CARTESIAN_POINT('Ctrl Pts',(6.70644606039074,62.4256985108781,2.71562701361794));
#231641=CARTESIAN_POINT('Ctrl Pts',(6.70819969702964,62.4231157429703,2.71782453535885));
#231642=CARTESIAN_POINT('Ctrl Pts',(6.70987381569795,62.4205129446135,2.72005051502429));
#231643=CARTESIAN_POINT('Ctrl Pts',(6.71147036762155,62.4178950590937,2.72229986760143));
#231644=CARTESIAN_POINT('Ctrl Pts',(6.71683301659097,62.4091018586491,2.72985520488884));
#231645=CARTESIAN_POINT('Ctrl Pts',(6.72134734296653,62.4000783072495,2.73770845534518));
#231646=CARTESIAN_POINT('Ctrl Pts',(6.72510335397126,62.3909158405878,2.74576706701679));
#231647=CARTESIAN_POINT('Ctrl Pts',(6.72923165499421,62.3808452043611,2.7546244358492));
#231648=CARTESIAN_POINT('Ctrl Pts',(6.73244426756114,62.3706061896797,2.76373036323036));
#231649=CARTESIAN_POINT('Ctrl Pts',(6.73481930344695,62.3602869763786,2.77299664636633));
#231650=CARTESIAN_POINT('Ctrl Pts',(6.73737731885814,62.3491727415102,2.78297683033235));
#231651=CARTESIAN_POINT('Ctrl Pts',(6.73896413451822,62.3379643502106,2.79314401478594));
#231652=CARTESIAN_POINT('Ctrl Pts',(6.7396251149953,62.3267489231154,2.80341452427569));
#231653=CARTESIAN_POINT('Ctrl Pts',(6.74027717000429,62.3156849421522,2.81354634721137));
#231654=CARTESIAN_POINT('Ctrl Pts',(6.74002799825975,62.3046126966268,2.82378004209116));
#231655=CARTESIAN_POINT('Ctrl Pts',(6.73887200051313,62.2936141127571,2.83404198860306));
#231656=CARTESIAN_POINT('Ctrl Pts',(6.37927424642559,58.8722700234482,2.83404198860304));
#231657=CARTESIAN_POINT('Ctrl Pts',(6.37816795023625,58.8617443183085,2.82422126442954));
#231658=CARTESIAN_POINT('Ctrl Pts',(6.37623543038808,58.8513437177761,2.81442815028353));
#231659=CARTESIAN_POINT('Ctrl Pts',(6.37349561323624,58.8411231047638,2.80471618166077));
#231660=CARTESIAN_POINT('Ctrl Pts',(6.37085007871655,58.8312542036518,2.79533842145934));
#231661=CARTESIAN_POINT('Ctrl Pts',(6.36745144953932,58.8215519162556,2.78603515649892));
#231662=CARTESIAN_POINT('Ctrl Pts',(6.3632719521844,58.8120753594595,2.77685887346358));
#231663=CARTESIAN_POINT('Ctrl Pts',(6.3593210182466,58.8031170454137,2.76818441216155));
#231664=CARTESIAN_POINT('Ctrl Pts',(6.35467192211579,58.7943596215114,2.7596226152118));
#231665=CARTESIAN_POINT('Ctrl Pts',(6.34926600747212,58.7858758685252,2.75123537701197));
#231666=CARTESIAN_POINT('Ctrl Pts',(6.3442872507764,58.7780624743506,2.74351087133653));
#231667=CARTESIAN_POINT('Ctrl Pts',(6.33866621240896,58.7704807832391,2.7359339944938));
#231668=CARTESIAN_POINT('Ctrl Pts',(6.33233133084323,58.7632157808948,2.72857657812111));
#231669=CARTESIAN_POINT('Ctrl Pts',(6.33044239704028,58.7610495038516,2.72638274508025));
#231670=CARTESIAN_POINT('Ctrl Pts',(6.32848982621314,58.7589116098618,2.72420861709468));
#231671=CARTESIAN_POINT('Ctrl Pts',(6.32647128889819,58.7568049797266,2.72205663736749));
#231672=CARTESIAN_POINT('Ctrl Pts',(6.32447337605832,58.754719874158,2.71992664556788));
#231673=CARTESIAN_POINT('Ctrl Pts',(6.32241310885705,58.7526673708736,2.71782089927907));
#231674=CARTESIAN_POINT('Ctrl Pts',(6.32029074540099,58.7506524329183,2.71574387311269));
#231675=CARTESIAN_POINT('Ctrl Pts',(6.32014316039694,58.7505123180735,2.71559944077509));
#231676=CARTESIAN_POINT('Ctrl Pts',(6.31999527850335,58.7503723733989,2.71545515216091));
#231677=CARTESIAN_POINT('Ctrl Pts',(6.31984709900205,58.7502325999834,2.71531100781753));
#231678=CARTESIAN_POINT('Ctrl Pts',(6.31335036684085,58.7441044214169,2.708991191761));
#231679=CARTESIAN_POINT('Ctrl Pts',(6.30625925377316,58.7383447881643,2.70298296066851));
#231680=CARTESIAN_POINT('Ctrl Pts',(6.29859016886908,58.7330687140843,2.69736727774144));
#231681=CARTESIAN_POINT('Ctrl Pts',(6.2914412488604,58.7281504960661,2.69213248525422));
#231682=CARTESIAN_POINT('Ctrl Pts',(6.28378931332983,58.7236522470775,2.6872386618545));
#231683=CARTESIAN_POINT('Ctrl Pts',(6.2756478370909,58.7196964823227,2.68278595829534));
#231684=CARTESIAN_POINT('Ctrl Pts',(6.2726695797549,58.7182494123989,2.68115710172795));
#231685=CARTESIAN_POINT('Ctrl Pts',(6.26962586933679,58.7168752520898,2.67958763637816));
#231686=CARTESIAN_POINT('Ctrl Pts',(6.26651766855733,58.7155811795666,2.67808378645386));
#231687=CARTESIAN_POINT('Ctrl Pts',(6.26577025010559,58.7152699983559,2.67772216078621));
#231688=CARTESIAN_POINT('Ctrl Pts',(6.26501853257419,58.7149635750525,2.67736403603584));
#231689=CARTESIAN_POINT('Ctrl Pts',(6.26426260461821,58.7146620123683,2.677009569345));
#231690=CARTESIAN_POINT('Ctrl Pts',(6.26353029941086,58.714369873518,2.67666617973825));
#231691=CARTESIAN_POINT('Ctrl Pts',(6.26279404284356,58.7140822962416,2.6763262231414));
#231692=CARTESIAN_POINT('Ctrl Pts',(6.2620539192844,58.7137993735014,2.67598984158795));
#231693=CARTESIAN_POINT('Ctrl Pts',(6.25394501035235,58.7106996279154,2.67230439292247));
#231694=CARTESIAN_POINT('Ctrl Pts',(6.24536644325958,58.7081569420202,2.66904964540004));
#231695=CARTESIAN_POINT('Ctrl Pts',(6.23645973859704,58.7062958387087,2.66640203566755));
#231696=CARTESIAN_POINT('Ctrl Pts',(6.23276586269294,58.7055239836918,2.66530399299466));
#231697=CARTESIAN_POINT('Ctrl Pts',(6.22901585349541,58.7048690642117,2.66430995142282));
#231698=CARTESIAN_POINT('Ctrl Pts',(6.2252207626778,58.7043384037136,2.66343053473381));
#231699=CARTESIAN_POINT('Ctrl Pts',(6.21874783981216,58.7034333069353,2.66193059792904));
#231700=CARTESIAN_POINT('Ctrl Pts',(6.21214524099542,58.7028917011007,2.66076519817147));
#231701=CARTESIAN_POINT('Ctrl Pts',(6.20547453342055,58.7027523988022,2.65997805604479));
#231702=CARTESIAN_POINT('Ctrl Pts',(6.20213917963312,58.7026827476529,2.65958448498145));
#231703=CARTESIAN_POINT('Ctrl Pts',(6.1987868824835,58.702715116791,2.65928526260781));
#231704=CARTESIAN_POINT('Ctrl Pts',(6.19542538555007,58.702854403047,2.65908463971344));
#231705=CARTESIAN_POINT('Ctrl Pts',(6.19206388861665,58.7029936893031,2.65888401681906));
#231706=CARTESIAN_POINT('Ctrl Pts',(6.18869323212197,58.7032398710657,2.65878198860303));
#231707=CARTESIAN_POINT('Ctrl Pts',(6.1853204982938,58.7035958781041,2.65878198860303));
#231708=CARTESIAN_POINT('Origin',(-0.0152400000001978,58.2637721346187,
2.83404198860302));
#231709=CARTESIAN_POINT('Ctrl Pts',(-0.190500000000213,62.6567671111301,
2.83404198860305));
#231710=CARTESIAN_POINT('Ctrl Pts',(-0.190500000000213,62.6673774406539,
2.82419652440183));
#231711=CARTESIAN_POINT('Ctrl Pts',(-0.189662809673352,62.6779562874463,
2.8143879057583));
#231712=CARTESIAN_POINT('Ctrl Pts',(-0.188003604115546,62.6884465439469,
2.80466781257137));
#231713=CARTESIAN_POINT('Ctrl Pts',(-0.186398312858428,62.6985959295767,
2.79526356453354));
#231714=CARTESIAN_POINT('Ctrl Pts',(-0.184023290311945,62.7086636500138,
2.78594102496541));
#231715=CARTESIAN_POINT('Ctrl Pts',(-0.180846261211493,62.7185939622152,
2.77675109089116));
#231716=CARTESIAN_POINT('Ctrl Pts',(-0.17784098731263,62.7279874260844,
2.7680579791404));
#231717=CARTESIAN_POINT('Ctrl Pts',(-0.174117798732407,62.7372588214061,
2.75948271210536));
#231718=CARTESIAN_POINT('Ctrl Pts',(-0.169611579427998,62.7463424082288,
2.75108575573613));
#231719=CARTESIAN_POINT('Ctrl Pts',(-0.165461025550571,62.7547090486342,
2.74335155163674));
#231720=CARTESIAN_POINT('Ctrl Pts',(-0.160645870590254,62.7629168328825,
2.7357681868636));
#231721=CARTESIAN_POINT('Ctrl Pts',(-0.155086395965148,62.7708892610778,
2.72840626160927));
#231722=CARTESIAN_POINT('Ctrl Pts',(-0.153473803707152,62.7732017594436,
2.72627084693978));
#231723=CARTESIAN_POINT('Ctrl Pts',(-0.151798403771608,62.7754942590267,
2.72415424587693));
#231724=CARTESIAN_POINT('Ctrl Pts',(-0.150057792857872,62.7777643638148,
2.72205867173303));
#231725=CARTESIAN_POINT('Ctrl Pts',(-0.148170858717257,62.7802253033583,
2.71978693462905));
#231726=CARTESIAN_POINT('Ctrl Pts',(-0.146210769553988,62.7826571567201,
2.71754411340805));
#231727=CARTESIAN_POINT('Ctrl Pts',(-0.144175421826372,62.7850565204097,
2.71533341844303));
#231728=CARTESIAN_POINT('Ctrl Pts',(-0.138589394016844,62.7916415928832,
2.7092661487645));
#231729=CARTESIAN_POINT('Ctrl Pts',(-0.132410786669256,62.7979456687655,
2.70347381860466));
#231730=CARTESIAN_POINT('Ctrl Pts',(-0.125664597436947,62.8038680995983,
2.69804914171452));
#231731=CARTESIAN_POINT('Ctrl Pts',(-0.119492200548546,62.8092868022741,
2.69308585687263));
#231732=CARTESIAN_POINT('Ctrl Pts',(-0.112844347460444,62.8143744518941,
2.68842799053244));
#231733=CARTESIAN_POINT('Ctrl Pts',(-0.105708043833497,62.8190433630436,
2.68414767054277));
#231734=CARTESIAN_POINT('Ctrl Pts',(-0.102202714803686,62.8213367169485,
2.68204519134611));
#231735=CARTESIAN_POINT('Ctrl Pts',(-0.0985794274534979,62.823528541979,
2.68003431778561));
#231736=CARTESIAN_POINT('Ctrl Pts',(-0.0948363533474291,62.8256051102649,
2.67812693945311));
#231737=CARTESIAN_POINT('Ctrl Pts',(-0.0941261414938298,62.8259991188711,
2.67776503299263));
#231738=CARTESIAN_POINT('Ctrl Pts',(-0.093411103231482,62.8263888407141,
2.67740659639983));
#231739=CARTESIAN_POINT('Ctrl Pts',(-0.0926913160162859,62.8267741591522,
2.67705178968914));
#231740=CARTESIAN_POINT('Ctrl Pts',(-0.0919940221515648,62.8271474363891,
2.67670807068817));
#231741=CARTESIAN_POINT('Ctrl Pts',(-0.0912922715312481,62.8275165811345,
2.67636775825325));
#231742=CARTESIAN_POINT('Ctrl Pts',(-0.0905861384171587,62.8278814873657,
2.67603099699314));
#231743=CARTESIAN_POINT('Ctrl Pts',(-0.0828908452419837,62.8318581602827,
2.67236104217184));
#231744=CARTESIAN_POINT('Ctrl Pts',(-0.0746698316630847,62.8353337180915,
2.66911440541526));
#231745=CARTESIAN_POINT('Ctrl Pts',(-0.0660491922296248,62.8381654210189,
2.66646778189682));
#231746=CARTESIAN_POINT('Ctrl Pts',(-0.0624086426654321,62.8393612667491,
2.66535009635028));
#231747=CARTESIAN_POINT('Ctrl Pts',(-0.0586971697058494,62.8404425512867,
2.66433897912401));
#231748=CARTESIAN_POINT('Ctrl Pts',(-0.0549254519866898,62.8414000604481,
2.66344564884851));
#231749=CARTESIAN_POINT('Ctrl Pts',(-0.0485739735924291,62.8430124819503,
2.66194130298644));
#231750=CARTESIAN_POINT('Ctrl Pts',(-0.0420529246954851,62.8442717146913,
2.66077206705478));
#231751=CARTESIAN_POINT('Ctrl Pts',(-0.0354197192409215,62.8451307298766,
2.65998225155772));
#231752=CARTESIAN_POINT('Ctrl Pts',(-0.0337614178772805,62.8453454836729,
2.65978479768345));
#231753=CARTESIAN_POINT('Ctrl Pts',(-0.0320960919388032,62.8455349903697,
2.6596109896668));
#231754=CARTESIAN_POINT('Ctrl Pts',(-0.0304246312368016,62.8456982067487,
2.65946139030559));
#231755=CARTESIAN_POINT('Ctrl Pts',(-0.0279174401837993,62.8459430313172,
2.65923699126377));
#231756=CARTESIAN_POINT('Ctrl Pts',(-0.0253964615341803,62.8461286892225,
2.65906707562499));
#231757=CARTESIAN_POINT('Ctrl Pts',(-0.0228647168033238,62.8462533376182,
2.65895332562976));
#231758=CARTESIAN_POINT('Ctrl Pts',(-0.0203329720724672,62.8463779860139,
2.65883957563454));
#231759=CARTESIAN_POINT('Ctrl Pts',(-0.0177904683743677,62.8464416340695,
2.65878198860306));
#231760=CARTESIAN_POINT('Ctrl Pts',(-0.0152400000002138,62.8464427007198,
2.65878198860306));
#231761=CARTESIAN_POINT('Ctrl Pts',(-0.0152400000002007,59.0285534841298,
2.65878198860303));
#231762=CARTESIAN_POINT('Ctrl Pts',(-0.0238699985097207,59.0285496414746,
2.65878198860303));
#231763=CARTESIAN_POINT('Ctrl Pts',(-0.0324255116361278,59.0292582026624,
2.65945335517899));
#231764=CARTESIAN_POINT('Ctrl Pts',(-0.0407807192235719,59.0305954788492,
2.66072561226651));
#231765=CARTESIAN_POINT('Ctrl Pts',(-0.0461773260309337,59.0314592220534,
2.66154735980389));
#231766=CARTESIAN_POINT('Ctrl Pts',(-0.0514905268413882,59.0325843328201,
2.6626189576693));
#231767=CARTESIAN_POINT('Ctrl Pts',(-0.0566895722964677,59.0339399880046,
2.6639142925107));
#231768=CARTESIAN_POINT('Ctrl Pts',(-0.0635806092276745,59.035736831295,
2.66563118464166));
#231769=CARTESIAN_POINT('Ctrl Pts',(-0.070268527890346,59.037943890677,
2.66774105138742));
#231770=CARTESIAN_POINT('Ctrl Pts',(-0.0766865040606691,59.0405007795599,
2.67016894181792));
#231771=CARTESIAN_POINT('Ctrl Pts',(-0.0798954921458306,59.0417792240014,
2.67138288703317));
#231772=CARTESIAN_POINT('Ctrl Pts',(-0.0830371938951397,59.0431451240708,
2.67267613167594));
#231773=CARTESIAN_POINT('Ctrl Pts',(-0.0861046703640038,59.044590923923,
2.67403835432595));
#231774=CARTESIAN_POINT('Ctrl Pts',(-0.0876384085984359,59.0453138238491,
2.67471946565096));
#231775=CARTESIAN_POINT('Ctrl Pts',(-0.0891536069438316,59.046056698672,
2.67541781389565));
#231776=CARTESIAN_POINT('Ctrl Pts',(-0.0906495011922653,59.0468186034777,
2.67613207244211));
#231777=CARTESIAN_POINT('Ctrl Pts',(-0.0910234747543737,59.0470090796791,
2.67631063707872));
#231778=CARTESIAN_POINT('Ctrl Pts',(-0.0913962421599025,59.0472007452525,
2.67649019601887));
#231779=CARTESIAN_POINT('Ctrl Pts',(-0.091767792172904,59.0473935854288,
2.67667072836699));
#231780=CARTESIAN_POINT('Ctrl Pts',(-0.0928824422119088,59.0479721059576,
2.67721232541132));
#231781=CARTESIAN_POINT('Ctrl Pts',(-0.0939861339739926,59.0485611979311,
2.67776268340089));
#231782=CARTESIAN_POINT('Ctrl Pts',(-0.0950785796751122,59.0491604624445,
2.67832123541558));
#231783=CARTESIAN_POINT('Ctrl Pts',(-0.102773626133376,59.0533816042978,
2.68225560368486));
#231784=CARTESIAN_POINT('Ctrl Pts',(-0.10995882346653,59.0580834293368,
2.68661792998929));
#231785=CARTESIAN_POINT('Ctrl Pts',(-0.116642428646858,59.0631465696372,
2.69130986622618));
#231786=CARTESIAN_POINT('Ctrl Pts',(-0.119883969936987,59.0656021872117,
2.69358545023095));
#231787=CARTESIAN_POINT('Ctrl Pts',(-0.123007567718284,59.0681433715121,
2.69593918853511));
#231788=CARTESIAN_POINT('Ctrl Pts',(-0.126014035556611,59.0707593633745,
2.69836306235516));
#231789=CARTESIAN_POINT('Ctrl Pts',(-0.130616727761238,59.0747642641418,
2.70207384382249));
#231790=CARTESIAN_POINT('Ctrl Pts',(-0.134943070277467,59.0789414743145,
2.70594760814249));
#231791=CARTESIAN_POINT('Ctrl Pts',(-0.13898514283093,59.083245567483,2.70995196345729));
#231792=CARTESIAN_POINT('Ctrl Pts',(-0.14086230223567,59.0852444106169,
2.71181160678127));
#231793=CARTESIAN_POINT('Ctrl Pts',(-0.142678271527317,59.0872703932643,
2.7136996277212));
#231794=CARTESIAN_POINT('Ctrl Pts',(-0.14443119730894,59.0893195943185,
2.71561183138683));
#231795=CARTESIAN_POINT('Ctrl Pts',(-0.144565552163225,59.0894766575051,
2.71575839426334));
#231796=CARTESIAN_POINT('Ctrl Pts',(-0.14469956892599,59.0896338466135,
2.7159050890323));
#231797=CARTESIAN_POINT('Ctrl Pts',(-0.144833247843279,59.0897911602044,
2.71605191409933));
#231798=CARTESIAN_POINT('Ctrl Pts',(-0.146711033602286,59.0920009418703,
2.71811436362774));
#231799=CARTESIAN_POINT('Ctrl Pts',(-0.148520654545092,59.0942367399985,
2.72020091026981));
#231800=CARTESIAN_POINT('Ctrl Pts',(-0.150262619641474,59.0964928714568,
2.72230624862203));
#231801=CARTESIAN_POINT('Ctrl Pts',(-0.156508996678944,59.1045829576264,
2.72985561753118));
#231802=CARTESIAN_POINT('Ctrl Pts',(-0.16193529014577,59.112995834295,2.73770089914338));
#231803=CARTESIAN_POINT('Ctrl Pts',(-0.166622470787609,59.1216309196484,
2.74574823347074));
#231804=CARTESIAN_POINT('Ctrl Pts',(-0.171773211444,59.1311200109807,2.7545914454702));
#231805=CARTESIAN_POINT('Ctrl Pts',(-0.176031864362475,59.1408779306735,
2.7636791175426));
#231806=CARTESIAN_POINT('Ctrl Pts',(-0.179468536017355,59.1508087658097,
2.77292162564712));
#231807=CARTESIAN_POINT('Ctrl Pts',(-0.183179278917844,59.1615315754576,
2.78290121484728));
#231808=CARTESIAN_POINT('Ctrl Pts',(-0.185932239424909,59.1724570142849,
2.79306229500199));
#231809=CARTESIAN_POINT('Ctrl Pts',(-0.18776628610007,59.1834936683141,
2.80331916685278));
#231810=CARTESIAN_POINT('Ctrl Pts',(-0.189584947008031,59.1944377361557,
2.81348999408724));
#231811=CARTESIAN_POINT('Ctrl Pts',(-0.190500000000201,59.2054925958118,
2.82375635966911));
#231812=CARTESIAN_POINT('Ctrl Pts',(-0.190500000000201,59.2165773020943,
2.83404198860303));
#231813=CARTESIAN_POINT('Origin',(0.0152400000000056,1.8389786102284E-13,
2.83404198860262));
#231814=CARTESIAN_POINT('Ctrl Pts',(0.0152399999997862,62.8464427007198,
2.65878198860306));
#231815=CARTESIAN_POINT('Ctrl Pts',(0.0238289333901328,62.8464391086781,
2.65878198860306));
#231816=CARTESIAN_POINT('Ctrl Pts',(0.0323412407620547,62.8457180711407,
2.65944603041885));
#231817=CARTESIAN_POINT('Ctrl Pts',(0.040653113049661,62.8443658068293,
2.66070439264089));
#231818=CARTESIAN_POINT('Ctrl Pts',(0.0459640037530079,62.8435017743092,
2.66150842619617));
#231819=CARTESIAN_POINT('Ctrl Pts',(0.0511932363887765,62.8423809557001,
2.66255428265399));
#231820=CARTESIAN_POINT('Ctrl Pts',(0.0563116129573038,62.8410338592511,
2.66381699700699));
#231821=CARTESIAN_POINT('Ctrl Pts',(0.0632971699620762,62.8391953428956,
2.66554034873299));
#231822=CARTESIAN_POINT('Ctrl Pts',(0.0700734120982157,62.8369299537506,
2.66766759644002));
#231823=CARTESIAN_POINT('Ctrl Pts',(0.076570577609309,62.8343031482015,
2.67012012783177));
#231824=CARTESIAN_POINT('Ctrl Pts',(0.0798191603648557,62.832989745427,
2.67134639352765));
#231825=CARTESIAN_POINT('Ctrl Pts',(0.0829981827951369,62.8315859904682,
2.67265375585041));
#231826=CARTESIAN_POINT('Ctrl Pts',(0.0861004173276806,62.8301000734876,
2.67403135126968));
#231827=CARTESIAN_POINT('Ctrl Pts',(0.0876515345939525,62.8293571149973,
2.67472014897932));
#231828=CARTESIAN_POINT('Ctrl Pts',(0.0891834722995143,62.8285936160521,
2.6754264966866));
#231829=CARTESIAN_POINT('Ctrl Pts',(0.0906954364276764,62.8278106008702,
2.67614899656129));
#231830=CARTESIAN_POINT('Ctrl Pts',(0.091073427459717,62.8276148470748,
2.67632962152996));
#231831=CARTESIAN_POINT('Ctrl Pts',(0.091450170514143,62.8274178735166,
2.67651125590977));
#231832=CARTESIAN_POINT('Ctrl Pts',(0.0918256539326503,62.827219696204,
2.67669387767551));
#231833=CARTESIAN_POINT('Ctrl Pts',(0.0929521041881723,62.8266251642661,
2.67724174297271));
#231834=CARTESIAN_POINT('Ctrl Pts',(0.0940672158684541,62.8260197985192,
2.67779849504774));
#231835=CARTESIAN_POINT('Ctrl Pts',(0.0951706907486432,62.8254040313375,
2.67836353618035));
#231836=CARTESIAN_POINT('Ctrl Pts',(0.10279638682729,62.8211486980558,2.68226832098931));
#231837=CARTESIAN_POINT('Ctrl Pts',(0.109916699411163,62.8164204928787,
2.68659153751411));
#231838=CARTESIAN_POINT('Ctrl Pts',(0.116542502759446,62.8113377077399,
2.69123699486194));
#231839=CARTESIAN_POINT('Ctrl Pts',(0.119835508836179,62.8088115774778,
2.69354577441236));
#231840=CARTESIAN_POINT('Ctrl Pts',(0.123006400629086,62.8061972539435,
2.69593478828141));
#231841=CARTESIAN_POINT('Ctrl Pts',(0.126056303769763,62.8035061084567,
2.69839565261247));
#231842=CARTESIAN_POINT('Ctrl Pts',(0.132784845643074,62.7975690395534,
2.70382468689072));
#231843=CARTESIAN_POINT('Ctrl Pts',(0.138932019324473,62.791268018738,2.70961155815114));
#231844=CARTESIAN_POINT('Ctrl Pts',(0.144445113412958,62.7847385034069,
2.71562701361794));
#231845=CARTESIAN_POINT('Ctrl Pts',(0.146459116207259,62.782353189115,2.71782453535886));
#231846=CARTESIAN_POINT('Ctrl Pts',(0.148396130390776,62.7799396422117,
2.7200505150243));
#231847=CARTESIAN_POINT('Ctrl Pts',(0.150257579786286,62.7775029828618,
2.72229986760145));
#231848=CARTESIAN_POINT('Ctrl Pts',(0.156509991333296,62.769318501945,2.72985520488891));
#231849=CARTESIAN_POINT('Ctrl Pts',(0.161942805717688,62.7608162581027,
2.73770845534525));
#231850=CARTESIAN_POINT('Ctrl Pts',(0.166635979461053,62.7520965944503,
2.74576706701686));
#231851=CARTESIAN_POINT('Ctrl Pts',(0.171794333348015,62.7425126511841,
2.75462443584931));
#231852=CARTESIAN_POINT('Ctrl Pts',(0.176059615357206,62.732665536351,2.7637303632305));
#231853=CARTESIAN_POINT('Ctrl Pts',(0.179500292056429,62.7226511116311,
2.77299664636653));
#231854=CARTESIAN_POINT('Ctrl Pts',(0.18320604828279,62.7118651471238,2.78297683033276));
#231855=CARTESIAN_POINT('Ctrl Pts',(0.185955767118902,62.7008840239666,
2.79314401478659));
#231856=CARTESIAN_POINT('Ctrl Pts',(0.187785458034874,62.6897991274278,
2.80341452427665));
#231857=CARTESIAN_POINT('Ctrl Pts',(0.189590441945833,62.6788639144185,
2.81354634721193));
#231858=CARTESIAN_POINT('Ctrl Pts',(0.190499999999787,62.6678262782736,
2.82378004209139));
#231859=CARTESIAN_POINT('Ctrl Pts',(0.190499999999787,62.6567671111301,
2.83404198860305));
#231860=CARTESIAN_POINT('Ctrl Pts',(0.190499999999799,59.2165773020943,
2.83404198860303));
#231861=CARTESIAN_POINT('Ctrl Pts',(0.190499999999799,59.2059936184297,
2.82422126443103));
#231862=CARTESIAN_POINT('Ctrl Pts',(0.189665225488488,59.1954479901469,
2.81442815028654));
#231863=CARTESIAN_POINT('Ctrl Pts',(0.188008762313989,59.1849969778471,
2.80471618166525));
#231864=CARTESIAN_POINT('Ctrl Pts',(0.186409301376948,59.174905605951,2.79533842146469));
#231865=CARTESIAN_POINT('Ctrl Pts',(0.184043455438172,59.1649012152161,
2.78603515650511));
#231866=CARTESIAN_POINT('Ctrl Pts',(0.180877423726733,59.1550396955548,
2.77685887347056));
#231867=CARTESIAN_POINT('Ctrl Pts',(0.177884532219648,59.145717471038,2.76818441216891));
#231868=CARTESIAN_POINT('Ctrl Pts',(0.174176304387194,59.1365220583465,
2.75962261521951));
#231869=CARTESIAN_POINT('Ctrl Pts',(0.169686797572706,59.1275197082968,
2.75123537701997));
#231870=CARTESIAN_POINT('Ctrl Pts',(0.165552037113637,59.1192286949267,
2.74351087134457));
#231871=CARTESIAN_POINT('Ctrl Pts',(0.160754293903984,59.11110097861,2.73593399450185));
#231872=CARTESIAN_POINT('Ctrl Pts',(0.15521351501367,59.1032135992736,2.72857657812913));
#231873=CARTESIAN_POINT('Ctrl Pts',(0.153561366596213,59.1008617419722,
2.72638274508555));
#231874=CARTESIAN_POINT('Ctrl Pts',(0.151842962927752,59.0985314603585,
2.7242086170973));
#231875=CARTESIAN_POINT('Ctrl Pts',(0.150055686179941,59.0962253759572,
2.72205663736749));
#231876=CARTESIAN_POINT('Ctrl Pts',(0.148286670996507,59.0939428540561,
2.71992664556788));
#231877=CARTESIAN_POINT('Ctrl Pts',(0.146452235168703,59.091686238035,2.71782089927906));
#231878=CARTESIAN_POINT('Ctrl Pts',(0.144552116609766,59.0894604907301,
2.71574387311268));
#231879=CARTESIAN_POINT('Ctrl Pts',(0.144419986081219,59.0893057166154,
2.71559944077508));
#231880=CARTESIAN_POINT('Ctrl Pts',(0.144287542501899,59.0891510807053,
2.71545515216091));
#231881=CARTESIAN_POINT('Ctrl Pts',(0.144154785043744,59.0889965840076,
2.71531100781752));
#231882=CARTESIAN_POINT('Ctrl Pts',(0.138334211749285,59.0822228828155,
2.70899119176102));
#231883=CARTESIAN_POINT('Ctrl Pts',(0.131883990153856,59.0757535782846,
2.70298296066855));
#231884=CARTESIAN_POINT('Ctrl Pts',(0.124808417215017,59.0697047694308,
2.69736727774151));
#231885=CARTESIAN_POINT('Ctrl Pts',(0.118212753509691,59.0640662283032,
2.69213248525436));
#231886=CARTESIAN_POINT('Ctrl Pts',(0.111072931136892,59.0587927761312,
2.68723866185469));
#231887=CARTESIAN_POINT('Ctrl Pts',(0.103389544767648,59.0540076654697,
2.68278595829559));
#231888=CARTESIAN_POINT('Ctrl Pts',(0.100578862632195,59.0522572100837,
2.6811571017281));
#231889=CARTESIAN_POINT('Ctrl Pts',(0.0976954648434748,59.0505724231958,
2.67958763637823));
#231890=CARTESIAN_POINT('Ctrl Pts',(0.0947395585251495,59.0489605442862,
2.67808378645385));
#231891=CARTESIAN_POINT('Ctrl Pts',(0.0940287618036534,59.0485729412565,
2.6777221607862));
#231892=CARTESIAN_POINT('Ctrl Pts',(0.093313192216558,59.0481896206936,
2.67736403603583));
#231893=CARTESIAN_POINT('Ctrl Pts',(0.0925929271969717,59.0478106940138,
2.67700956934499));
#231894=CARTESIAN_POINT('Ctrl Pts',(0.0918951704592475,59.0474436087928,
2.67666617973824));
#231895=CARTESIAN_POINT('Ctrl Pts',(0.0911930071932301,59.0470806471273,
2.67632622314139));
#231896=CARTESIAN_POINT('Ctrl Pts',(0.0904865115876316,59.0467219102891,
2.67598984158794));
#231897=CARTESIAN_POINT('Ctrl Pts',(0.0827460357498814,59.0427915336444,
2.6723043929225));
#231898=CARTESIAN_POINT('Ctrl Pts',(0.0744802459945514,59.0393660724133,
2.66904964540011));
#231899=CARTESIAN_POINT('Ctrl Pts',(0.0658168714613306,59.0365841602693,
2.66640203566765));
#231900=CARTESIAN_POINT('Ctrl Pts',(0.0622239118146019,59.0354304183832,
2.66530399299472));
#231901=CARTESIAN_POINT('Ctrl Pts',(0.0585629032865241,59.0343871039219,
2.66430995142284));
#231902=CARTESIAN_POINT('Ctrl Pts',(0.0548440714997765,59.0334626554263,
2.6634305347338));
#231903=CARTESIAN_POINT('Ctrl Pts',(0.0485012163582087,59.0318859121829,
2.66193059792904));
#231904=CARTESIAN_POINT('Ctrl Pts',(0.0419914004942172,59.0306571138139,
2.66076519817147));
#231905=CARTESIAN_POINT('Ctrl Pts',(0.0353717968086142,59.029821295816,
2.65997805604479));
#231906=CARTESIAN_POINT('Ctrl Pts',(0.0320619949658128,59.0294033868171,
2.65958448498145));
#231907=CARTESIAN_POINT('Ctrl Pts',(0.0287246785544705,59.0290851681643,
2.65928526260781));
#231908=CARTESIAN_POINT('Ctrl Pts',(0.0253670368746644,59.0288723192869,
2.65908463971343));
#231909=CARTESIAN_POINT('Ctrl Pts',(0.0220093951948583,59.0286594704096,
2.65888401681906));
#231910=CARTESIAN_POINT('Ctrl Pts',(0.0186314705078071,59.0285519740193,
2.65878198860303));
#231911=CARTESIAN_POINT('Ctrl Pts',(0.0152399999997995,59.0285534841298,
2.65878198860303));
#231912=CARTESIAN_POINT('Origin',(-6.10537907909402,57.943004080846,2.83404198860303));
#231913=CARTESIAN_POINT('Ctrl Pts',(-6.73887200051354,62.2936141127571,
2.83404198860306));
#231914=CARTESIAN_POINT('Ctrl Pts',(-6.73998108195343,62.3041663177857,
2.82419652440124));
#231915=CARTESIAN_POINT('Ctrl Pts',(-6.74025426844111,62.314774722767,2.81438790575723));
#231916=CARTESIAN_POINT('Ctrl Pts',(-6.73970068257616,62.3253809467524,
2.80466781256989));
#231917=CARTESIAN_POINT('Ctrl Pts',(-6.73916508495544,62.3356425316142,
2.79526356453176));
#231918=CARTESIAN_POINT('Ctrl Pts',(-6.73785543637676,62.3459033574827,
2.7859410249634));
#231919=CARTESIAN_POINT('Ctrl Pts',(-6.73573381164817,62.3561113603648,
2.77675109088895));
#231920=CARTESIAN_POINT('Ctrl Pts',(-6.73372688529703,62.3657675025186,
2.76805797913806));
#231921=CARTESIAN_POINT('Ctrl Pts',(-6.73099321743857,62.3753772873478,
2.75948271210292));
#231922=CARTESIAN_POINT('Ctrl Pts',(-6.72746117704631,62.3848821415107,
2.7510857557336));
#231923=CARTESIAN_POINT('Ctrl Pts',(-6.72420791240138,62.3936367996034,
2.74335155163412));
#231924=CARTESIAN_POINT('Ctrl Pts',(-6.72027708243781,62.4023029414995,
2.7357681868609));
#231925=CARTESIAN_POINT('Ctrl Pts',(-6.71558140886385,62.4108128192383,
2.72840626160649));
#231926=CARTESIAN_POINT('Ctrl Pts',(-6.71421937245599,62.4132812112856,
2.72627084693795));
#231927=CARTESIAN_POINT('Ctrl Pts',(-6.71279278199563,62.4157362792957,
2.72415424587601));
#231928=CARTESIAN_POINT('Ctrl Pts',(-6.71129899689619,62.4181758915951,
2.72205867173302));
#231929=CARTESIAN_POINT('Ctrl Pts',(-6.7096796378069,62.4208205881803,2.71978693462904));
#231930=CARTESIAN_POINT('Ctrl Pts',(-6.70798448411195,62.4234440047031,
2.71754411340805));
#231931=CARTESIAN_POINT('Ctrl Pts',(-6.70621108803144,62.4260429761975,
2.71533341844301));
#231932=CARTESIAN_POINT('Ctrl Pts',(-6.70134398857289,62.4331758738577,
2.70926614876449));
#231933=CARTESIAN_POINT('Ctrl Pts',(-6.69585818364715,62.4400912556839,
2.70347381860466));
#231934=CARTESIAN_POINT('Ctrl Pts',(-6.68976801333909,62.4466864116143,
2.69804914171452));
#231935=CARTESIAN_POINT('Ctrl Pts',(-6.6841958381505,62.452720621231,2.69308585687282));
#231936=CARTESIAN_POINT('Ctrl Pts',(-6.67811620689388,62.4584752900412,
2.6884279905328));
#231937=CARTESIAN_POINT('Ctrl Pts',(-6.67150703079278,62.4638645712582,
2.68414767054326));
#231938=CARTESIAN_POINT('Ctrl Pts',(-6.66826062508134,62.4665117685875,
2.68204519134642));
#231939=CARTESIAN_POINT('Ctrl Pts',(-6.66488629458029,62.46907032323,2.68003431778574));
#231940=CARTESIAN_POINT('Ctrl Pts',(-6.66138078591733,62.471526773642,2.67812693945309));
#231941=CARTESIAN_POINT('Ctrl Pts',(-6.6607156497927,62.4719928611815,2.67776503299261));
#231942=CARTESIAN_POINT('Ctrl Pts',(-6.66004526561012,62.4724551899382,
2.67740659639981));
#231943=CARTESIAN_POINT('Ctrl Pts',(-6.6593696982088,62.472913635813,2.67705178968912));
#231944=CARTESIAN_POINT('Ctrl Pts',(-6.65871524228878,62.4733577552543,
2.67670807068815));
#231945=CARTESIAN_POINT('Ctrl Pts',(-6.65805592206474,62.4737982307001,
2.67636775825322));
#231946=CARTESIAN_POINT('Ctrl Pts',(-6.65739180030932,62.4742349489461,
2.67603099699312));
#231947=CARTESIAN_POINT('Ctrl Pts',(-6.65015433826405,62.4789942144028,
2.67236104217171));
#231948=CARTESIAN_POINT('Ctrl Pts',(-6.64234165497423,62.4833100626584,
2.66911440541505));
#231949=CARTESIAN_POINT('Ctrl Pts',(-6.63406423386074,62.4870273554133,
2.66646778189657));
#231950=CARTESIAN_POINT('Ctrl Pts',(-6.63056862752469,62.4885971912268,
2.66535009635012));
#231951=CARTESIAN_POINT('Ctrl Pts',(-6.62699051141362,62.4900605069393,
2.66433897912393));
#231952=CARTESIAN_POINT('Ctrl Pts',(-6.62333954252022,62.4914070226223,
2.6634456488485));
#231953=CARTESIAN_POINT('Ctrl Pts',(-6.61719140213093,62.4936745213869,
2.66194130298643));
#231954=CARTESIAN_POINT('Ctrl Pts',(-6.61083770188548,62.4956084911392,
2.66077206705477));
#231955=CARTESIAN_POINT('Ctrl Pts',(-6.60433062536177,62.4971561593227,
2.65998225155772));
#231956=CARTESIAN_POINT('Ctrl Pts',(-6.60270385623084,62.4975430763686,
2.65978479768346));
#231957=CARTESIAN_POINT('Ctrl Pts',(-6.60106746196587,62.497905618889,2.6596109896668));
#231958=CARTESIAN_POINT('Ctrl Pts',(-6.59942221845775,62.4982426563701,
2.65946139030559));
#231959=CARTESIAN_POINT('Ctrl Pts',(-6.59695435319557,62.4987482125918,
2.65923699126377));
#231960=CARTESIAN_POINT('Ctrl Pts',(-6.59446659126629,62.4991963674678,
2.65906707562499));
#231961=CARTESIAN_POINT('Ctrl Pts',(-6.5919617450032,62.4995849724125,2.65895332562977));
#231962=CARTESIAN_POINT('Ctrl Pts',(-6.58945689874012,62.4999735773573,
2.65883957563454));
#231963=CARTESIAN_POINT('Ctrl Pts',(-6.58693497617671,62.5003026407463,
2.65878198860306));
#231964=CARTESIAN_POINT('Ctrl Pts',(-6.58439859103049,62.5005702980932,
2.65878198860306));
#231965=CARTESIAN_POINT('Ctrl Pts',(-6.18532049829418,58.7035958781041,
2.65878198860303));
#231966=CARTESIAN_POINT('Ctrl Pts',(-6.19390281910233,58.7026899760171,
2.65878198860303));
#231967=CARTESIAN_POINT('Ctrl Pts',(-6.20248552904501,58.702500360993,2.65945335517904));
#231968=CARTESIAN_POINT('Ctrl Pts',(-6.21093474935611,58.7029569544316,
2.66072561226664));
#231969=CARTESIAN_POINT('Ctrl Pts',(-6.21639207873623,58.7032518669437,
2.661547359804));
#231970=CARTESIAN_POINT('Ctrl Pts',(-6.22179377937587,58.7038154335201,
2.66261895766937));
#231971=CARTESIAN_POINT('Ctrl Pts',(-6.22710604846885,58.7046202140518,
2.6639142925107));
#231972=CARTESIAN_POINT('Ctrl Pts',(-6.23414715684661,58.7056869045459,
2.66563118464166));
#231973=CARTESIAN_POINT('Ctrl Pts',(-6.24102913891663,58.7071827955654,
2.66774105138742));
#231974=CARTESIAN_POINT('Ctrl Pts',(-6.24767922440765,58.7090548163571,
2.67016894181793));
#231975=CARTESIAN_POINT('Ctrl Pts',(-6.25100426715316,58.709990826753,2.67138288703318));
#231976=CARTESIAN_POINT('Ctrl Pts',(-6.2542715337668,58.711020847023,2.67267613167594));
#231977=CARTESIAN_POINT('Ctrl Pts',(-6.25747333351535,58.7121380880309,
2.67403835432596));
#231978=CARTESIAN_POINT('Ctrl Pts',(-6.25907423338963,58.7126967085349,
2.67471946565097));
#231979=CARTESIAN_POINT('Ctrl Pts',(-6.26065878288361,58.7132771324573,
2.67541781389566));
#231980=CARTESIAN_POINT('Ctrl Pts',(-6.26222612320533,58.7138784999417,
2.67613207244212));
#231981=CARTESIAN_POINT('Ctrl Pts',(-6.26261795828575,58.7140288418128,
2.67631063707873));
#231982=CARTESIAN_POINT('Ctrl Pts',(-6.26300871814027,58.714180492618,2.67649019601888));
#231983=CARTESIAN_POINT('Ctrl Pts',(-6.26339839005071,58.7143334388437,
2.676670728367));
#231984=CARTESIAN_POINT('Ctrl Pts',(-6.26456740578202,58.7147922775209,
2.67721232541133));
#231985=CARTESIAN_POINT('Ctrl Pts',(-6.26572662828387,58.7152627751832,
2.6777626834009));
#231986=CARTESIAN_POINT('Ctrl Pts',(-6.26687572965181,58.7157445651925,
2.67832123541559));
#231987=CARTESIAN_POINT('Ctrl Pts',(-6.27496985131174,58.7191382318081,
2.68225560368494));
#231988=CARTESIAN_POINT('Ctrl Pts',(-6.28260716192813,58.7230632421221,
2.68661792998947));
#231989=CARTESIAN_POINT('Ctrl Pts',(-6.289783395895,58.7274000190317,2.69130986622646));
#231990=CARTESIAN_POINT('Ctrl Pts',(-6.29326386161406,58.7295033511465,
2.69358545023115));
#231991=CARTESIAN_POINT('Ctrl Pts',(-6.29663597408954,58.7317041096973,
2.69593918853521));
#231992=CARTESIAN_POINT('Ctrl Pts',(-6.29989941779165,58.7339915094195,
2.69836306235517));
#231993=CARTESIAN_POINT('Ctrl Pts',(-6.30489552208954,58.7374933585784,
2.7020738438225));
#231994=CARTESIAN_POINT('Ctrl Pts',(-6.30963480180889,58.7411954596219,
2.7059476081425));
#231995=CARTESIAN_POINT('Ctrl Pts',(-6.31410463171064,58.7450534628852,
2.7099519634573));
#231996=CARTESIAN_POINT('Ctrl Pts',(-6.31618044384085,58.7468451395593,
2.71181160678128));
#231997=CARTESIAN_POINT('Ctrl Pts',(-6.31819823791545,58.7486702031825,
2.71369962772121));
#231998=CARTESIAN_POINT('Ctrl Pts',(-6.32015576082334,58.7505249478607,
2.71561183138683));
#231999=CARTESIAN_POINT('Ctrl Pts',(-6.3203057972412,58.7506671067322,2.71575839426334));
#232000=CARTESIAN_POINT('Ctrl Pts',(-6.32045551058208,58.7508094261761,
2.71590508903231));
#232001=CARTESIAN_POINT('Ctrl Pts',(-6.32060490094017,58.7509519047348,
2.71605191409934));
#232002=CARTESIAN_POINT('Ctrl Pts',(-6.32270338507401,58.7529532989258,
2.71811436362775));
#232003=CARTESIAN_POINT('Ctrl Pts',(-6.32473679726646,58.7549876922217,
2.72020091026982));
#232004=CARTESIAN_POINT('Ctrl Pts',(-6.32670504965004,58.7570493794211,
2.72230624862204));
#232005=CARTESIAN_POINT('Ctrl Pts',(-6.33376285265597,58.76444222306,2.72985561753164));
#232006=CARTESIAN_POINT('Ctrl Pts',(-6.34003880538957,58.7722418109931,
2.73770089914433));
#232007=CARTESIAN_POINT('Ctrl Pts',(-6.34560292136785,58.7803396486564,
2.74574823347221));
#232008=CARTESIAN_POINT('Ctrl Pts',(-6.35171732586278,58.7892383587482,
2.75459144547185));
#232009=CARTESIAN_POINT('Ctrl Pts',(-6.35697262978514,58.798497673091,2.76367911754444));
#232010=CARTESIAN_POINT('Ctrl Pts',(-6.36142852992882,58.8080148760666,
2.77292162564914));
#232011=CARTESIAN_POINT('Ctrl Pts',(-6.3662397838055,58.8182910667879,2.78290121484888));
#232012=CARTESIAN_POINT('Ctrl Pts',(-6.37011968263775,58.8288688921864,
2.79306229500313));
#232013=CARTESIAN_POINT('Ctrl Pts',(-6.37309732669844,58.8396533761891,
2.80331916685345));
#232014=CARTESIAN_POINT('Ctrl Pts',(-6.37604999138494,58.8503473894518,
2.81348999408769));
#232015=CARTESIAN_POINT('Ctrl Pts',(-6.37811557911251,58.8612460403467,
2.82375635966934));
#232016=CARTESIAN_POINT('Ctrl Pts',(-6.37927424642597,58.8722700234482,
2.83404198860304));
#232017=CARTESIAN_POINT('Origin',(0.0151565136854187,0.00159301378038297,
2.83404198860263));
#232018=CARTESIAN_POINT('Ctrl Pts',(-6.55408556365967,62.5037563256536,
2.65878198860306));
#232019=CARTESIAN_POINT('Ctrl Pts',(-6.54554330587443,62.5046505412979,
2.65878198860306));
#232020=CARTESIAN_POINT('Ctrl Pts',(-6.53700226086713,62.504823232088,2.65944603041887));
#232021=CARTESIAN_POINT('Ctrl Pts',(-6.52859457177513,62.5043472028591,
2.66070439264094));
#232022=CARTESIAN_POINT('Ctrl Pts',(-6.52322245869536,62.5040430428433,
2.6615084261962));
#232023=CARTESIAN_POINT('Ctrl Pts',(-6.51790471489646,62.5034749678474,
2.66255428265399));
#232024=CARTESIAN_POINT('Ctrl Pts',(-6.5126735674088,62.5026702669709,2.66381699700695));
#232025=CARTESIAN_POINT('Ctrl Pts',(-6.50553410072683,62.5015720117391,
2.66554034873295));
#232026=CARTESIAN_POINT('Ctrl Pts',(-6.49855818190805,62.50002734281,2.66766759644));
#232027=CARTESIAN_POINT('Ctrl Pts',(-6.49182203260205,62.4980940659031,
2.67012012783176));
#232028=CARTESIAN_POINT('Ctrl Pts',(-6.48845395794905,62.4971274274497,
2.67134639352764));
#232029=CARTESIAN_POINT('Ctrl Pts',(-6.48514561818761,62.4960636607367,
2.6726537558504));
#232030=CARTESIAN_POINT('Ctrl Pts',(-6.48190505740187,62.4949101555731,
2.67403135126968));
#232031=CARTESIAN_POINT('Ctrl Pts',(-6.48028477700901,62.4943334029914,
2.67472014897932));
#232032=CARTESIAN_POINT('Ctrl Pts',(-6.47868142404703,62.4937342176675,
2.67542649668661));
#232033=CARTESIAN_POINT('Ctrl Pts',(-6.47709589524288,62.4931135352115,
2.67614899656131));
#232034=CARTESIAN_POINT('Ctrl Pts',(-6.47669951304184,62.4929583645975,
2.67632962152998));
#232035=CARTESIAN_POINT('Ctrl Pts',(-6.47630424448194,62.4928018504536,
2.67651125590979));
#232036=CARTESIAN_POINT('Ctrl Pts',(-6.47591010283095,62.4926440074818,
2.67669387767552));
#232037=CARTESIAN_POINT('Ctrl Pts',(-6.47472767787795,62.4921704785663,
2.67724174297273));
#232038=CARTESIAN_POINT('Ctrl Pts',(-6.47355539694488,62.4916849899866,
2.67779849504777));
#232039=CARTESIAN_POINT('Ctrl Pts',(-6.4723936018183,62.4911879405754,2.67836353618038));
#232040=CARTESIAN_POINT('Ctrl Pts',(-6.46436487665209,62.4877530207471,
2.68226832098932));
#232041=CARTESIAN_POINT('Ctrl Pts',(-6.45678933786442,62.4837949925051,
2.68659153751408));
#232042=CARTESIAN_POINT('Ctrl Pts',(-6.44966853564051,62.479432636437,2.69123699486188));
#232043=CARTESIAN_POINT('Ctrl Pts',(-6.44612951648126,62.4772645574456,
2.69354577441232));
#232044=CARTESIAN_POINT('Ctrl Pts',(-6.4427027239438,62.4749960038954,2.69593478828139));
#232045=CARTESIAN_POINT('Ctrl Pts',(-6.43938822718944,62.4726384024735,
2.69839565261248));
#232046=CARTESIAN_POINT('Ctrl Pts',(-6.43207595228374,62.4674371815969,
2.70382468689073));
#232047=CARTESIAN_POINT('Ctrl Pts',(-6.42530381744011,62.4618132330512,
2.70961155815114));
#232048=CARTESIAN_POINT('Ctrl Pts',(-6.41913840445445,62.4558957623412,
2.71562701361794));
#232049=CARTESIAN_POINT('Ctrl Pts',(-6.41688610134085,62.4537340356676,
2.71782453535884));
#232050=CARTESIAN_POINT('Ctrl Pts',(-6.41470741397488,62.4515361835427,
2.72005051502428));
#232051=CARTESIAN_POINT('Ctrl Pts',(-6.41260146153658,62.4493074469124,
2.72229986760141));
#232052=CARTESIAN_POINT('Ctrl Pts',(-6.40552779014104,62.4418213564088,
2.72985520488918));
#232053=CARTESIAN_POINT('Ctrl Pts',(-6.39923601079888,62.4339335724863,
2.73770845534586));
#232054=CARTESIAN_POINT('Ctrl Pts',(-6.39365709371034,62.4257522463025,
2.74576706701784));
#232055=CARTESIAN_POINT('Ctrl Pts',(-6.38752520296386,62.4167599996847,
2.75462443585064));
#232056=CARTESIAN_POINT('Ctrl Pts',(-6.38225398283455,62.4074126717503,
2.76373036323221));
#232057=CARTESIAN_POINT('Ctrl Pts',(-6.37778536209576,62.3978127557445,
2.77299664636864));
#232058=CARTESIAN_POINT('Ctrl Pts',(-6.37297246609489,62.3874732348825,
2.78297683033526));
#232059=CARTESIAN_POINT('Ctrl Pts',(-6.36908997057771,62.3768396913508,
2.79314401478951));
#232060=CARTESIAN_POINT('Ctrl Pts',(-6.36611161569943,62.3660067738143,
2.80341452428));
#232061=CARTESIAN_POINT('Ctrl Pts',(-6.36317347866837,62.3553201372418,
2.81354634721418));
#232062=CARTESIAN_POINT('Ctrl Pts',(-6.36111515612462,62.3444380411295,
2.82378004209251));
#232063=CARTESIAN_POINT('Ctrl Pts',(-6.35995915837823,62.3334394572621,
2.83404198860306));
#232064=CARTESIAN_POINT('Ctrl Pts',(-6.00036140429066,58.9120953679532,
2.83404198860303));
#232065=CARTESIAN_POINT('Ctrl Pts',(-5.99925510810147,58.9015696628149,
2.82422126443092));
#232066=CARTESIAN_POINT('Ctrl Pts',(-5.99898299131208,58.8909945468903,
2.8144281502863));
#232067=CARTESIAN_POINT('Ctrl Pts',(-5.99953795195273,58.8804276387792,
2.80471618166489));
#232068=CARTESIAN_POINT('Ctrl Pts',(-6.00007381527886,58.8702243592803,
2.79533842146428));
#232069=CARTESIAN_POINT('Ctrl Pts',(-6.00138095727663,58.8600274754043,
2.78603515650465));
#232070=CARTESIAN_POINT('Ctrl Pts',(-6.00349883563944,58.84988903775,2.77685887347006));
#232071=CARTESIAN_POINT('Ctrl Pts',(-6.00550089397075,58.8403050390046,
2.76818441216843));
#232072=CARTESIAN_POINT('Ctrl Pts',(-6.0082276253854,58.8307723843892,2.75962261521906));
#232073=CARTESIAN_POINT('Ctrl Pts',(-6.01175153639534,58.8213500689069,
2.75123537701956));
#232074=CARTESIAN_POINT('Ctrl Pts',(-6.01499699931747,58.8126722744189,
2.74351087134424));
#232075=CARTESIAN_POINT('Ctrl Pts',(-6.01891888229134,58.8040875818577,
2.7359339945016));
#232076=CARTESIAN_POINT('Ctrl Pts',(-6.02360485257387,58.795664241308,2.72857657812896));
#232077=CARTESIAN_POINT('Ctrl Pts',(-6.02500211431986,58.7931525711919,
2.72638274508544));
#232078=CARTESIAN_POINT('Ctrl Pts',(-6.02646752363713,58.79065543301,2.72420861709724));
#232079=CARTESIAN_POINT('Ctrl Pts',(-6.02800395803724,58.7881751602885,
2.72205663736749));
#232080=CARTESIAN_POINT('Ctrl Pts',(-6.02952469386371,58.7857202298426,
2.71992664556788));
#232081=CARTESIAN_POINT('Ctrl Pts',(-6.03111319985523,58.7832842250421,
2.71782089927907));
#232082=CARTESIAN_POINT('Ctrl Pts',(-6.03277025542048,58.7808720541409,
2.71574387311268));
#232083=CARTESIAN_POINT('Ctrl Pts',(-6.03288548382381,58.7807043164939,
2.71559944077509));
#232084=CARTESIAN_POINT('Ctrl Pts',(-6.03300103800929,58.7805366835716,
2.71545515216092));
#232085=CARTESIAN_POINT('Ctrl Pts',(-6.03311691890581,58.78036915629,2.71531100781753));
#232086=CARTESIAN_POINT('Ctrl Pts',(-6.03819756191452,58.7730241465599,
2.70899119176101));
#232087=CARTESIAN_POINT('Ctrl Pts',(-6.04393622206015,58.765916049805,2.70298296066851));
#232088=CARTESIAN_POINT('Ctrl Pts',(-6.05034076157604,58.759160778193,2.69736727774145));
#232089=CARTESIAN_POINT('Ctrl Pts',(-6.05631090550631,58.7528636909922,
2.69213248525432));
#232090=CARTESIAN_POINT('Ctrl Pts',(-6.06286038933342,58.7468728126824,
2.68723866185467));
#232091=CARTESIAN_POINT('Ctrl Pts',(-6.07000150504417,58.741310782788,2.68278595829558));
#232092=CARTESIAN_POINT('Ctrl Pts',(-6.07261381755728,58.7392761202954,
2.68115710172809));
#232093=CARTESIAN_POINT('Ctrl Pts',(-6.0753053116069,58.7372991657065,2.67958763637822));
#232094=CARTESIAN_POINT('Ctrl Pts',(-6.07807653793573,58.7353871404932,
2.67808378645384));
#232095=CARTESIAN_POINT('Ctrl Pts',(-6.07874292528937,58.7349273623045,
2.67772216078619));
#232096=CARTESIAN_POINT('Ctrl Pts',(-6.07941450700202,58.7344713442225,
2.67736403603582));
#232097=CARTESIAN_POINT('Ctrl Pts',(-6.08009121771093,58.734019205147,2.67700956934498));
#232098=CARTESIAN_POINT('Ctrl Pts',(-6.08074678121019,58.7335811954177,
2.67666617973823));
#232099=CARTESIAN_POINT('Ctrl Pts',(-6.08140715812725,58.7331468260469,
2.67632622314138));
#232100=CARTESIAN_POINT('Ctrl Pts',(-6.08207228526558,58.7327162055067,
2.67598984158792));
#232101=CARTESIAN_POINT('Ctrl Pts',(-6.08935952173624,58.7279982598322,
2.6723043929224));
#232102=CARTESIAN_POINT('Ctrl Pts',(-6.09722197243217,58.7237275533352,
2.66904964539994));
#232103=CARTESIAN_POINT('Ctrl Pts',(-6.1055470990921,58.7200553115704,2.66640203566744));
#232104=CARTESIAN_POINT('Ctrl Pts',(-6.10899977726339,58.7185323234527,
2.66530399299459));
#232105=CARTESIAN_POINT('Ctrl Pts',(-6.11253167434615,58.7171120447817,
2.66430995142278));
#232106=CARTESIAN_POINT('Ctrl Pts',(-6.11613350280244,58.71580393674,2.66343053473379));
#232107=CARTESIAN_POINT('Ctrl Pts',(-6.12227679657168,58.7135728221604,
2.66193059792903));
#232108=CARTESIAN_POINT('Ctrl Pts',(-6.12862250657805,58.711670294229,2.66076519817146));
#232109=CARTESIAN_POINT('Ctrl Pts',(-6.13511848061116,58.7101471179289,
2.65997805604479));
#232110=CARTESIAN_POINT('Ctrl Pts',(-6.13836646762772,58.7093855297788,
2.65958448498145));
#232111=CARTESIAN_POINT('Ctrl Pts',(-6.1416522389638,58.7087202098051,2.65928526260781));
#232112=CARTESIAN_POINT('Ctrl Pts',(-6.14496923836511,58.7081575578112,
2.65908463971344));
#232113=CARTESIAN_POINT('Ctrl Pts',(-6.14828623776642,58.7075949058173,
2.65888401681906));
#232114=CARTESIAN_POINT('Ctrl Pts',(-6.15163442139611,58.7071349090269,
2.65878198860303));
#232115=CARTESIAN_POINT('Ctrl Pts',(-6.15500747092336,58.7067819056644,
2.65878198860303));
#232116=CARTESIAN_POINT('Origin',(-12.1286263473646,56.9874003490103,2.83404198860302));
#232117=CARTESIAN_POINT('Ctrl Pts',(-13.2134115091896,61.2479592423879,
2.83404198860304));
#232118=CARTESIAN_POINT('Ctrl Pts',(-13.215617520741,61.2583377107545,2.82419652440144));
#232119=CARTESIAN_POINT('Ctrl Pts',(-13.2169980909549,61.2688594460195,
2.81438790575762));
#232120=CARTESIAN_POINT('Ctrl Pts',(-13.2175561899856,61.2794654334797,
2.80466781257047));
#232121=CARTESIAN_POINT('Ctrl Pts',(-13.218096154121,61.289726789502,2.7952635645325));
#232122=CARTESIAN_POINT('Ctrl Pts',(-13.2178662282942,61.3000683010459,
2.78594102496429));
#232123=CARTESIAN_POINT('Ctrl Pts',(-13.2168232529022,61.3104421535925,
2.77675109088998));
#232124=CARTESIAN_POINT('Ctrl Pts',(-13.2158366624041,61.3202551793165,
2.76805797913924));
#232125=CARTESIAN_POINT('Ctrl Pts',(-13.2141224659049,61.330098066839,2.75948271210423));
#232126=CARTESIAN_POINT('Ctrl Pts',(-13.2116033021988,61.3399200511706,
2.75108575573504));
#232127=CARTESIAN_POINT('Ctrl Pts',(-13.209282970235,61.3489668090839,2.74335155163569));
#232128=CARTESIAN_POINT('Ctrl Pts',(-13.2062795322643,61.3579963605632,
2.73576818686259));
#232129=CARTESIAN_POINT('Ctrl Pts',(-13.2024991065243,61.3669504518439,
2.72840626160828));
#232130=CARTESIAN_POINT('Ctrl Pts',(-13.2014025487215,61.3695476933546,
2.72627084693913));
#232131=CARTESIAN_POINT('Ctrl Pts',(-13.200240397759,61.3721384315545,2.7241542458766));
#232132=CARTESIAN_POINT('Ctrl Pts',(-13.1990098046949,61.3747208224641,
2.72205867173302));
#232133=CARTESIAN_POINT('Ctrl Pts',(-13.197675762694,61.3775203002418,2.71978693462904));
#232134=CARTESIAN_POINT('Ctrl Pts',(-13.196264116926,61.3803065372251,2.71754411340804));
#232135=CARTESIAN_POINT('Ctrl Pts',(-13.1947721021912,61.3830766416488,
2.71533341844301));
#232136=CARTESIAN_POINT('Ctrl Pts',(-13.1906772560438,61.3906792149762,
2.70926614876448));
#232137=CARTESIAN_POINT('Ctrl Pts',(-13.1859443571666,61.3981301363759,
2.70347381860465));
#232138=CARTESIAN_POINT('Ctrl Pts',(-13.1805769309631,61.4053257594954,
2.69804914171452));
#232139=CARTESIAN_POINT('Ctrl Pts',(-13.1756660273915,61.41190936399,2.69308585687282));
#232140=CARTESIAN_POINT('Ctrl Pts',(-13.1702212276784,61.4182680026348,
2.68842799053281));
#232141=CARTESIAN_POINT('Ctrl Pts',(-13.1642115906192,61.4243186078267,
2.68414767054327));
#232142=CARTESIAN_POINT('Ctrl Pts',(-13.1612596765268,61.4272906453322,
2.68204519134642));
#232143=CARTESIAN_POINT('Ctrl Pts',(-13.1581712727462,61.4301878975265,
2.68003431778575));
#232144=CARTESIAN_POINT('Ctrl Pts',(-13.1549417366132,61.4329973166797,
2.67812693945308));
#232145=CARTESIAN_POINT('Ctrl Pts',(-13.1543289635881,61.4335303765998,
2.6777650329926));
#232146=CARTESIAN_POINT('Ctrl Pts',(-13.1537105783546,61.4340602468996,
2.67740659639981));
#232147=CARTESIAN_POINT('Ctrl Pts',(-13.153086632425,61.4345867973823,2.67705178968912));
#232148=CARTESIAN_POINT('Ctrl Pts',(-13.1524821848057,61.4350968931624,
2.67670807068815));
#232149=CARTESIAN_POINT('Ctrl Pts',(-13.1518725186283,61.4356038733674,
2.67636775825323));
#232150=CARTESIAN_POINT('Ctrl Pts',(-13.1512576844885,61.4361076188516,
2.67603099699312));
#232151=CARTESIAN_POINT('Ctrl Pts',(-13.1445573487222,61.4415973333397,
2.67236104217181));
#232152=CARTESIAN_POINT('Ctrl Pts',(-13.137238593115,61.446706186705,2.66911440541524));
#232153=CARTESIAN_POINT('Ctrl Pts',(-13.1293950794799,61.45126834185,2.66646778189679));
#232154=CARTESIAN_POINT('Ctrl Pts',(-13.126082714966,61.4531949682972,2.66535009635026));
#232155=CARTESIAN_POINT('Ctrl Pts',(-13.1226771582919,61.4550242827918,
2.66433897912399));
#232156=CARTESIAN_POINT('Ctrl Pts',(-13.119186939003,61.456745052289,2.6634456488485));
#232157=CARTESIAN_POINT('Ctrl Pts',(-13.1133094969314,61.459642785125,2.66194130298642));
#232158=CARTESIAN_POINT('Ctrl Pts',(-13.1071927578069,61.4622303029114,
2.66077206705477));
#232159=CARTESIAN_POINT('Ctrl Pts',(-13.1008831031061,61.4644496675159,
2.65998225155771));
#232160=CARTESIAN_POINT('Ctrl Pts',(-13.0993056894308,61.4650045086671,
2.65978479768345));
#232161=CARTESIAN_POINT('Ctrl Pts',(-13.0977161555174,61.4655361149194,
2.65961098966679));
#232162=CARTESIAN_POINT('Ctrl Pts',(-13.0961151548353,61.4660432808496,
2.65946139030558));
#232163=CARTESIAN_POINT('Ctrl Pts',(-13.0937136538122,61.4668040297448,
2.65923699126377));
#232164=CARTESIAN_POINT('Ctrl Pts',(-13.0912863650436,61.467509771513,2.65906707562498));
#232165=CARTESIAN_POINT('Ctrl Pts',(-13.0888358608681,61.4681580753698,
2.65895332562976));
#232166=CARTESIAN_POINT('Ctrl Pts',(-13.0863853566927,61.4688063792266,
2.65883957563454));
#232167=CARTESIAN_POINT('Ctrl Pts',(-13.0839116459753,61.469397252662,2.65878198860305));
#232168=CARTESIAN_POINT('Ctrl Pts',(-13.0814171332235,61.4699285681956,
2.65878198860305));
#232169=CARTESIAN_POINT('Ctrl Pts',(-12.2876333308473,57.7354693911206,
2.65878198860303));
#232170=CARTESIAN_POINT('Ctrl Pts',(-12.2960739442508,57.7336713548548,
2.65878198860303));
#232171=CARTESIAN_POINT('Ctrl Pts',(-12.304589817043,57.7325856410806,2.65945335517899));
#232172=CARTESIAN_POINT('Ctrl Pts',(-12.3130404786514,57.7321565492377,
2.6607256122665));
#232173=CARTESIAN_POINT('Ctrl Pts',(-12.3184987389621,57.7318793999345,
2.66154735980387));
#232174=CARTESIAN_POINT('Ctrl Pts',(-12.3239297572689,57.7318752477673,
2.66261895766928));
#232175=CARTESIAN_POINT('Ctrl Pts',(-12.3292970476685,57.7321203363023,
2.66391429251067));
#232176=CARTESIAN_POINT('Ctrl Pts',(-12.336411083636,57.7324451871159,2.66563118464163));
#232177=CARTESIAN_POINT('Ctrl Pts',(-12.3434117286776,57.7332135204778,
2.66774105138739));
#232178=CARTESIAN_POINT('Ctrl Pts',(-12.3502210637611,57.7343801629267,
2.6701689418179));
#232179=CARTESIAN_POINT('Ctrl Pts',(-12.3536257313028,57.7349634841512,
2.67138288703315));
#232180=CARTESIAN_POINT('Ctrl Pts',(-12.356982765924,57.7356463395042,2.67267613167591));
#232181=CARTESIAN_POINT('Ctrl Pts',(-12.3602838093642,57.7364227809416,
2.67403835432593));
#232182=CARTESIAN_POINT('Ctrl Pts',(-12.3619343310843,57.7368110016603,
2.67471946565094));
#232183=CARTESIAN_POINT('Ctrl Pts',(-12.363570871071,57.7372226154361,2.67541781389564));
#232184=CARTESIAN_POINT('Ctrl Pts',(-12.3651924853575,57.7376568568913,
2.6761320724421));
#232185=CARTESIAN_POINT('Ctrl Pts',(-12.3655978889291,57.7377654172551,
2.67631063707871));
#232186=CARTESIAN_POINT('Ctrl Pts',(-12.3660023599859,57.7378753917742,
2.67649019601886));
#232187=CARTESIAN_POINT('Ctrl Pts',(-12.3664058844667,57.7379867683386,
2.67667072836698));
#232188=CARTESIAN_POINT('Ctrl Pts',(-12.3676164579094,57.7383208980315,
2.67721232541132));
#232189=CARTESIAN_POINT('Ctrl Pts',(-12.3688185104667,57.7386676465117,
2.67776268340088));
#232190=CARTESIAN_POINT('Ctrl Pts',(-12.3700116777064,57.7390266834248,
2.67832123541557));
#232191=CARTESIAN_POINT('Ctrl Pts',(-12.378416193677,57.7415556930809,2.68225560368487));
#232192=CARTESIAN_POINT('Ctrl Pts',(-12.3864219416031,57.7446608854355,
2.68661792998933));
#232193=CARTESIAN_POINT('Ctrl Pts',(-12.3940121800352,57.7482237843188,
2.69130986622625));
#232194=CARTESIAN_POINT('Ctrl Pts',(-12.3976934374727,57.7499517864271,
2.693585450231));
#232195=CARTESIAN_POINT('Ctrl Pts',(-12.4012771190727,57.7517880072573,
2.69593918853513));
#232196=CARTESIAN_POINT('Ctrl Pts',(-12.4047617836667,57.7537217536094,
2.69836306235516));
#232197=CARTESIAN_POINT('Ctrl Pts',(-12.4100965616936,57.7566821841676,
2.70207384382249));
#232198=CARTESIAN_POINT('Ctrl Pts',(-12.4151968540757,57.7598686150881,
2.7059476081425));
#232199=CARTESIAN_POINT('Ctrl Pts',(-12.420045468934,57.7632382593552,2.70995196345729));
#232200=CARTESIAN_POINT('Ctrl Pts',(-12.4222971907576,57.7648031395851,
2.71181160678127));
#232201=CARTESIAN_POINT('Ctrl Pts',(-12.424494702241,57.766407288405,2.7136996277212));
#232202=CARTESIAN_POINT('Ctrl Pts',(-12.4266353752445,57.7680472557364,
2.71561183138683));
#232203=CARTESIAN_POINT('Ctrl Pts',(-12.4267994493956,57.7681729527705,
2.71575839426333));
#232204=CARTESIAN_POINT('Ctrl Pts',(-12.4269632190239,57.7682988432681,
2.7159050890323));
#232205=CARTESIAN_POINT('Ctrl Pts',(-12.4271266840707,57.7684249257698,
2.71605191409933));
#232206=CARTESIAN_POINT('Ctrl Pts',(-12.4294228751481,57.7701960047924,
2.71811436362774));
#232207=CARTESIAN_POINT('Ctrl Pts',(-12.4316578001007,57.7720067040172,
2.72020091026981));
#232208=CARTESIAN_POINT('Ctrl Pts',(-12.4338307751865,57.7738513586815,
2.72230624862203));
#232209=CARTESIAN_POINT('Ctrl Pts',(-12.4416226773935,57.7804659622468,
2.72985561753126));
#232210=CARTESIAN_POINT('Ctrl Pts',(-12.4486795287418,57.787566807526,2.73770089914356));
#232211=CARTESIAN_POINT('Ctrl Pts',(-12.4550596184371,57.7950386758943,
2.74574823347101));
#232212=CARTESIAN_POINT('Ctrl Pts',(-12.4620706960754,57.8032495086153,
2.75459144547052));
#232213=CARTESIAN_POINT('Ctrl Pts',(-12.4682650727921,57.8119087706221,
2.76367911754298));
#232214=CARTESIAN_POINT('Ctrl Pts',(-12.4736913816503,57.8209080689694,
2.77292162564755));
#232215=CARTESIAN_POINT('Ctrl Pts',(-12.4795504333995,57.830625052669,2.7829012148477));
#232216=CARTESIAN_POINT('Ctrl Pts',(-12.4845147615739,57.8407393717711,
2.79306229500239));
#232217=CARTESIAN_POINT('Ctrl Pts',(-12.4886033793289,57.8511535286846,
2.80331916685316));
#232218=CARTESIAN_POINT('Ctrl Pts',(-12.4926576977819,57.8614803215215,
2.81348999408749));
#232219=CARTESIAN_POINT('Ctrl Pts',(-12.4958511892336,57.8721033557557,
2.82375635966924));
#232220=CARTESIAN_POINT('Ctrl Pts',(-12.4981558292589,57.8829458346107,
2.83404198860303));
#232221=CARTESIAN_POINT('Origin',(0.0149069694351899,0.00316857416824667,
2.83404198860263));
#232222=CARTESIAN_POINT('Ctrl Pts',(-13.0516031943531,61.4762657165317,
2.65878198860305));
#232223=CARTESIAN_POINT('Ctrl Pts',(-13.0432012029365,61.4780479426483,
2.65878198860305));
#232224=CARTESIAN_POINT('Ctrl Pts',(-13.0347249977699,61.4791124697295,
2.65944603041892));
#232225=CARTESIAN_POINT('Ctrl Pts',(-13.0263136082743,61.4795178910589,
2.6607043926411));
#232226=CARTESIAN_POINT('Ctrl Pts',(-13.0209391308134,61.4797769359882,
2.66150842619636));
#232227=CARTESIAN_POINT('Ctrl Pts',(-13.0155911381655,61.4797678285538,
2.66255428265409));
#232228=CARTESIAN_POINT('Ctrl Pts',(-13.0103045333054,61.479514339721,2.66381699700698));
#232229=CARTESIAN_POINT('Ctrl Pts',(-13.0030893784373,61.4791683783271,
2.66554034873298));
#232230=CARTESIAN_POINT('Ctrl Pts',(-12.9959902125623,61.47836135333,2.66766759644002));
#232231=CARTESIAN_POINT('Ctrl Pts',(-12.9890888821229,61.4771427864516,
2.67012012783178));
#232232=CARTESIAN_POINT('Ctrl Pts',(-12.9856382169032,61.4765335030124,
2.67134639352766));
#232233=CARTESIAN_POINT('Ctrl Pts',(-12.9822368066734,61.4758213793961,
2.67265375585042));
#232234=CARTESIAN_POINT('Ctrl Pts',(-12.9788934238966,61.4750129240935,
2.67403135126969));
#232235=CARTESIAN_POINT('Ctrl Pts',(-12.9772217325082,61.4746086964423,
2.67472014897933));
#232236=CARTESIAN_POINT('Ctrl Pts',(-12.9755645309604,61.4741803895394,
2.67542649668662));
#232237=CARTESIAN_POINT('Ctrl Pts',(-12.9739228088656,61.4737288401363,
2.67614899656131));
#232238=CARTESIAN_POINT('Ctrl Pts',(-12.9735123783419,61.4736159527855,
2.67632962152998));
#232239=CARTESIAN_POINT('Ctrl Pts',(-12.9731029149216,61.4735016128576,
2.67651125590979));
#232240=CARTESIAN_POINT('Ctrl Pts',(-12.9726944333366,61.4733858335872,
2.67669387767553));
#232241=CARTESIAN_POINT('Ctrl Pts',(-12.9714689885813,61.4730384957759,
2.67724174297273));
#232242=CARTESIAN_POINT('Ctrl Pts',(-12.9702523821507,61.4726782034779,
2.67779849504776));
#232243=CARTESIAN_POINT('Ctrl Pts',(-12.9690449956483,61.4723053176145,
2.67836353618037));
#232244=CARTESIAN_POINT('Ctrl Pts',(-12.9607012057874,61.4697284449401,
2.68226832098937));
#232245=CARTESIAN_POINT('Ctrl Pts',(-12.952753439984,61.4665839586187,2.68659153751421));
#232246=CARTESIAN_POINT('Ctrl Pts',(-12.9452156558836,61.4629898265073,
2.6912369948621));
#232247=CARTESIAN_POINT('Ctrl Pts',(-12.9414693978765,61.4612035527136,
2.69354577441247));
#232248=CARTESIAN_POINT('Ctrl Pts',(-12.9378242492508,61.4593056238951,
2.69593478828146));
#232249=CARTESIAN_POINT('Ctrl Pts',(-12.9342814732029,61.4573073969128,
2.69839565261247));
#232250=CARTESIAN_POINT('Ctrl Pts',(-12.9264655800789,61.4528990097272,
2.70382468689072));
#232251=CARTESIAN_POINT('Ctrl Pts',(-12.9191426809995,61.4480137506084,
2.70961155815114));
#232252=CARTESIAN_POINT('Ctrl Pts',(-12.9123924986716,61.4427731575669,
2.71562701361793));
#232253=CARTESIAN_POINT('Ctrl Pts',(-12.9099265719429,61.4408587028415,
2.71782453535884));
#232254=CARTESIAN_POINT('Ctrl Pts',(-12.9075300815492,61.4389006256228,
2.72005051502428));
#232255=CARTESIAN_POINT('Ctrl Pts',(-12.9052026993237,61.4369042302171,
2.72229986760142));
#232256=CARTESIAN_POINT('Ctrl Pts',(-12.8973852687042,61.4301985493014,
2.72985520488897));
#232257=CARTESIAN_POINT('Ctrl Pts',(-12.8903034584558,61.4230116455107,
2.73770845534543));
#232258=CARTESIAN_POINT('Ctrl Pts',(-12.8838999218055,61.415458293118,2.74576706701717));
#232259=CARTESIAN_POINT('Ctrl Pts',(-12.876861676478,61.407156264085,2.75462443584973));
#232260=CARTESIAN_POINT('Ctrl Pts',(-12.8706422708196,61.3984111343311,
2.76373036323104));
#232261=CARTESIAN_POINT('Ctrl Pts',(-12.8651946651853,61.3893309057287,
2.77299664636719));
#232262=CARTESIAN_POINT('Ctrl Pts',(-12.8593273605058,61.3795511104671,
2.78297683033348));
#232263=CARTESIAN_POINT('Ctrl Pts',(-12.8543546257409,61.3693816498899,
2.79314401478736));
#232264=CARTESIAN_POINT('Ctrl Pts',(-12.8502602383794,61.3589193990681,
2.80341452427745));
#232265=CARTESIAN_POINT('Ctrl Pts',(-12.8462211390715,61.3485984239567,
2.81354634721249));
#232266=CARTESIAN_POINT('Ctrl Pts',(-12.8430366034498,61.3379910943969,
2.82378004209168));
#232267=CARTESIAN_POINT('Ctrl Pts',(-12.84073727331,61.3271735965895,2.83404198860304));
#232268=CARTESIAN_POINT('Ctrl Pts',(-12.1254815933794,57.9621601888122,
2.83404198860302));
#232269=CARTESIAN_POINT('Ctrl Pts',(-12.1232811218133,57.9518077840276,
2.82422126442991));
#232270=CARTESIAN_POINT('Ctrl Pts',(-12.1219050950916,57.9413190436432,
2.8144281502843));
#232271=CARTESIAN_POINT('Ctrl Pts',(-12.1213524729335,57.9307520129763,
2.80471618166192));
#232272=CARTESIAN_POINT('Ctrl Pts',(-12.1208188676181,57.9205486151395,
2.79533842146069));
#232273=CARTESIAN_POINT('Ctrl Pts',(-12.1210529843538,57.9102709573153,
2.78603515650046));
#232274=CARTESIAN_POINT('Ctrl Pts',(-12.1220995054497,57.8999666805119,
2.7768588734653));
#232275=CARTESIAN_POINT('Ctrl Pts',(-12.1230887956355,57.8902259118332,
2.76818441216329));
#232276=CARTESIAN_POINT('Ctrl Pts',(-12.1248041559928,57.8804604570522,
2.75962261521355));
#232277=CARTESIAN_POINT('Ctrl Pts',(-12.1273238624922,57.8707214089969,
2.75123537701372));
#232278=CARTESIAN_POINT('Ctrl Pts',(-12.1296444699069,57.8617519091229,
2.74351087133818));
#232279=CARTESIAN_POINT('Ctrl Pts',(-12.132647523675,57.8528042960052,2.73593399449536));
#232280=CARTESIAN_POINT('Ctrl Pts',(-12.1364273448794,57.8439372821234,
2.72857657812257));
#232281=CARTESIAN_POINT('Ctrl Pts',(-12.1375544112609,57.8412933175785,
2.72638274508121));
#232282=CARTESIAN_POINT('Ctrl Pts',(-12.1387507708948,57.8386566819994,
2.72420861709514));
#232283=CARTESIAN_POINT('Ctrl Pts',(-12.1400195294492,57.8360293953472,
2.72205663736748));
#232284=CARTESIAN_POINT('Ctrl Pts',(-12.1412753244188,57.8334289530882,
2.71992664556787));
#232285=CARTESIAN_POINT('Ctrl Pts',(-12.14260049657,57.8308402488867,2.71782089927905));
#232286=CARTESIAN_POINT('Ctrl Pts',(-12.143996334094,57.8282680826383,2.71574387311267));
#232287=CARTESIAN_POINT('Ctrl Pts',(-12.1440933979056,57.8280892192277,
2.71559944077508));
#232288=CARTESIAN_POINT('Ctrl Pts',(-12.1441907966614,57.8279104259147,
2.7154551521609));
#232289=CARTESIAN_POINT('Ctrl Pts',(-12.144288531381,57.827731703513,2.71531100781751));
#232290=CARTESIAN_POINT('Ctrl Pts',(-12.1485735795159,57.8198958587086,
2.70899119176097));
#232291=CARTESIAN_POINT('Ctrl Pts',(-12.1535378042503,57.8122268475252,
2.70298296066845));
#232292=CARTESIAN_POINT('Ctrl Pts',(-12.1592011408681,57.8048391253243,
2.69736727774137));
#232293=CARTESIAN_POINT('Ctrl Pts',(-12.1644803548772,57.7979524842554,
2.69213248525412));
#232294=CARTESIAN_POINT('Ctrl Pts',(-12.1703677426435,57.791309817124,2.68723866185435));
#232295=CARTESIAN_POINT('Ctrl Pts',(-12.1768883481379,57.7850318067599,
2.68278595829518));
#232296=CARTESIAN_POINT('Ctrl Pts',(-12.1792736699859,57.782735229349,2.68115710172784));
#232297=CARTESIAN_POINT('Ctrl Pts',(-12.1817437717242,57.7804877669875,
2.6795876363781));
#232298=CARTESIAN_POINT('Ctrl Pts',(-12.1842999559277,57.778296544019,2.67808378645385));
#232299=CARTESIAN_POINT('Ctrl Pts',(-12.1849146328342,57.7777696280973,
2.67772216078621));
#232300=CARTESIAN_POINT('Ctrl Pts',(-12.1855348686826,57.7772459087257,
2.67736403603584));
#232301=CARTESIAN_POINT('Ctrl Pts',(-12.1861606108967,57.7767255109849,
2.677009569345));
#232302=CARTESIAN_POINT('Ctrl Pts',(-12.1867667986667,57.7762213756735,
2.67666617973824));
#232303=CARTESIAN_POINT('Ctrl Pts',(-12.1873781540071,57.7757203576394,
2.67632622314139));
#232304=CARTESIAN_POINT('Ctrl Pts',(-12.187994625406,57.7752225713659,2.67598984158794));
#232305=CARTESIAN_POINT('Ctrl Pts',(-12.1947487820216,57.7697687474617,
2.67230439292248));
#232306=CARTESIAN_POINT('Ctrl Pts',(-12.2021217510026,57.7646995864531,
2.66904964540006));
#232307=CARTESIAN_POINT('Ctrl Pts',(-12.210017417959,57.7601772489166,2.66640203566758));
#232308=CARTESIAN_POINT('Ctrl Pts',(-12.2132919863906,57.7583017007437,
2.66530399299468));
#232309=CARTESIAN_POINT('Ctrl Pts',(-12.2166560758249,57.7565200187334,
2.66430995142283));
#232310=CARTESIAN_POINT('Ctrl Pts',(-12.2201014385647,57.7548425830509,
2.6634305347338));
#232311=CARTESIAN_POINT('Ctrl Pts',(-12.2259778637495,57.7519815416932,
2.66193059792904));
#232312=CARTESIAN_POINT('Ctrl Pts',(-12.2320899429716,57.7494261286936,
2.66076519817147));
#232313=CARTESIAN_POINT('Ctrl Pts',(-12.2383911161013,57.7472322823297,
2.65997805604479));
#232314=CARTESIAN_POINT('Ctrl Pts',(-12.2415417026662,57.7461353591477,
2.65958448498145));
#232315=CARTESIAN_POINT('Ctrl Pts',(-12.2447399293287,57.745130227238,2.65928526260781));
#232316=CARTESIAN_POINT('Ctrl Pts',(-12.2479799447119,57.7442239366605,
2.65908463971343));
#232317=CARTESIAN_POINT('Ctrl Pts',(-12.2512199600952,57.7433176460829,
2.65888401681905));
#232318=CARTESIAN_POINT('Ctrl Pts',(-12.254501719267,57.7425101887134,2.65878198860303));
#232319=CARTESIAN_POINT('Ctrl Pts',(-12.257819391977,57.7418065394567,2.65878198860303));
#232320=CARTESIAN_POINT('Origin',(-18.0189898472952,55.4074307335707,2.83404198860299));
#232321=CARTESIAN_POINT('Ctrl Pts',(-19.5431821162869,59.5312589135997,
2.83404198860303));
#232322=CARTESIAN_POINT('Ctrl Pts',(-19.5464608884256,59.5413499366332,
2.82419652440135));
#232323=CARTESIAN_POINT('Ctrl Pts',(-19.5489337165496,59.5516697238485,
2.81438790575749));
#232324=CARTESIAN_POINT('Ctrl Pts',(-19.550597385826,59.5621592733657,2.80466781257031));
#232325=CARTESIAN_POINT('Ctrl Pts',(-19.5522069957574,59.5723079749848,
2.79526356453234));
#232326=CARTESIAN_POINT('Ctrl Pts',(-19.5530593117979,59.5826168684397,
2.78594102496414));
#232327=CARTESIAN_POINT('Ctrl Pts',(-19.5531064127991,59.5930429125516,
2.77675109088984));
#232328=CARTESIAN_POINT('Ctrl Pts',(-19.553150967446,59.6029053082826,2.76805797913912));
#232329=CARTESIAN_POINT('Ctrl Pts',(-19.5524750234014,59.6128734577632,
2.75948271210414));
#232330=CARTESIAN_POINT('Ctrl Pts',(-19.5509963368661,59.6229049605478,
2.75108575573497));
#232331=CARTESIAN_POINT('Ctrl Pts',(-19.5496343596258,59.6321447001092,
2.74335155163568));
#232332=CARTESIAN_POINT('Ctrl Pts',(-19.5475912199427,59.6414387315163,
2.73576818686263));
#232333=CARTESIAN_POINT('Ctrl Pts',(-19.544767461172,59.6507389334411,2.72840626160835));
#232334=CARTESIAN_POINT('Ctrl Pts',(-19.5439483960915,59.6534365684931,
2.72627084693917));
#232335=CARTESIAN_POINT('Ctrl Pts',(-19.5430634173963,59.6561345922123,
2.72415424587661));
#232336=CARTESIAN_POINT('Ctrl Pts',(-19.5421094990031,59.6588314685162,
2.722058671733));
#232337=CARTESIAN_POINT('Ctrl Pts',(-19.5410753901339,59.661755055822,2.71978693462902));
#232338=CARTESIAN_POINT('Ctrl Pts',(-19.5399627185792,59.6646735866704,
2.71754411340802));
#232339=CARTESIAN_POINT('Ctrl Pts',(-19.5387684320157,59.6675844741796,
2.71533341844299));
#232340=CARTESIAN_POINT('Ctrl Pts',(-19.5354907031708,59.67557342779,2.70926614876445));
#232341=CARTESIAN_POINT('Ctrl Pts',(-19.5315625649727,59.6834782549091,
2.70347381860463));
#232342=CARTESIAN_POINT('Ctrl Pts',(-19.5269766895185,59.691195508465,2.69804914171448));
#232343=CARTESIAN_POINT('Ctrl Pts',(-19.5227808624511,59.6982563764889,
2.69308585687276));
#232344=CARTESIAN_POINT('Ctrl Pts',(-19.5180305486465,59.7051493183928,
2.68842799053272));
#232345=CARTESIAN_POINT('Ctrl Pts',(-19.5126862934704,59.711794955863,2.68414767054316));
#232346=CARTESIAN_POINT('Ctrl Pts',(-19.5100612127855,59.7150592712798,
2.68204519134634));
#232347=CARTESIAN_POINT('Ctrl Pts',(-19.5072925729236,59.7182634781245,
2.68003431778569));
#232348=CARTESIAN_POINT('Ctrl Pts',(-19.5043743927941,59.7213950854346,
2.67812693945305));
#232349=CARTESIAN_POINT('Ctrl Pts',(-19.5038206965381,59.7219892774194,
2.67776503299257));
#232350=CARTESIAN_POINT('Ctrl Pts',(-19.5032610854118,59.7225808838924,
2.67740659639977));
#232351=CARTESIAN_POINT('Ctrl Pts',(-19.5026955970361,59.7231697699857,
2.67705178968908));
#232352=CARTESIAN_POINT('Ctrl Pts',(-19.5021477801721,59.7237402533885,
2.67670807068811));
#232353=CARTESIAN_POINT('Ctrl Pts',(-19.5015944476715,59.7243081837715,
2.67636775825318));
#232354=CARTESIAN_POINT('Ctrl Pts',(-19.5010356373988,59.7248734373531,
2.67603099699308));
#232355=CARTESIAN_POINT('Ctrl Pts',(-19.4949458381921,59.7310334544119,
2.67236104217171));
#232356=CARTESIAN_POINT('Ctrl Pts',(-19.488201196085,59.7368793392206,2.6691144054151));
#232357=CARTESIAN_POINT('Ctrl Pts',(-19.4808775251047,59.7422363728294,
2.66646778189663));
#232358=CARTESIAN_POINT('Ctrl Pts',(-19.4777846933722,59.7444986813877,
2.66535009635015));
#232359=CARTESIAN_POINT('Ctrl Pts',(-19.4745890081269,59.7466739523117,
2.66433897912392));
#232360=CARTESIAN_POINT('Ctrl Pts',(-19.4712977780157,59.7487501225121,
2.66344564884846));
#232361=CARTESIAN_POINT('Ctrl Pts',(-19.465755428747,59.7522463412521,2.66194130298639));
#232362=CARTESIAN_POINT('Ctrl Pts',(-19.4599426670173,59.7554590576863,
2.66077206705474));
#232363=CARTESIAN_POINT('Ctrl Pts',(-19.4538995640366,59.7583258028888,
2.65998225155768));
#232364=CARTESIAN_POINT('Ctrl Pts',(-19.4523887882915,59.7590424891894,
2.65978479768342));
#232365=CARTESIAN_POINT('Ctrl Pts',(-19.4508635299958,59.7597373347844,
2.65961098966676));
#232366=CARTESIAN_POINT('Ctrl Pts',(-19.4493243130383,59.7604090725475,
2.65946139030555));
#232367=CARTESIAN_POINT('Ctrl Pts',(-19.447015487602,59.7614166791923,2.65923699126374));
#232368=CARTESIAN_POINT('Ctrl Pts',(-19.4446752658777,59.762372275598,2.65906707562495));
#232369=CARTESIAN_POINT('Ctrl Pts',(-19.4423059520264,59.7632731754142,
2.65895332562973));
#232370=CARTESIAN_POINT('Ctrl Pts',(-19.4399366381751,59.7641740752304,
2.65883957563451));
#232371=CARTESIAN_POINT('Ctrl Pts',(-19.4375382417961,59.7650202849792,
2.65878198860303));
#232372=CARTESIAN_POINT('Ctrl Pts',(-19.4351129318423,59.7658094374952,
2.65878198860303));
#232373=CARTESIAN_POINT('Ctrl Pts',(-18.2553202812751,56.1347810195643,
2.658781988603));
#232374=CARTESIAN_POINT('Ctrl Pts',(-18.2635267101473,56.1321105487812,
2.658781988603));
#232375=CARTESIAN_POINT('Ctrl Pts',(-18.2718824441049,56.1301406315644,
2.65945335517894));
#232376=CARTESIAN_POINT('Ctrl Pts',(-18.2802419597937,56.1288305556599,
2.66072561226642));
#232377=CARTESIAN_POINT('Ctrl Pts',(-18.2856413491927,56.1279843810472,
2.66154735980379));
#232378=CARTESIAN_POINT('Ctrl Pts',(-18.2910421817934,56.1274125556284,
2.66261895766922));
#232379=CARTESIAN_POINT('Ctrl Pts',(-18.2964056883427,56.1270952669254,
2.66391429251064));
#232380=CARTESIAN_POINT('Ctrl Pts',(-18.3035147090331,56.1266747189249,
2.6656311846416));
#232381=CARTESIAN_POINT('Ctrl Pts',(-18.3105573165143,56.1267070766082,
2.66774105138735));
#232382=CARTESIAN_POINT('Ctrl Pts',(-18.3174512966901,56.1271555587356,
2.67016894181786));
#232383=CARTESIAN_POINT('Ctrl Pts',(-18.320898286778,56.1273797997993,2.67138288703311));
#232384=CARTESIAN_POINT('Ctrl Pts',(-18.324308309033,56.1277080087291,2.67267613167588));
#232385=CARTESIAN_POINT('Ctrl Pts',(-18.3276724292421,56.1281351437411,
2.6740383543259));
#232386=CARTESIAN_POINT('Ctrl Pts',(-18.3293544893466,56.1283487112471,
2.6747194656509));
#232387=CARTESIAN_POINT('Ctrl Pts',(-18.3310250895515,56.1285870051497,
2.67541781389559));
#232388=CARTESIAN_POINT('Ctrl Pts',(-18.3326832110572,56.1288493629354,
2.67613207244206));
#232389=CARTESIAN_POINT('Ctrl Pts',(-18.3330977414336,56.1289149523818,
2.67631063707867));
#232390=CARTESIAN_POINT('Ctrl Pts',(-18.3335114922231,56.128982045711,2.67649019601882));
#232391=CARTESIAN_POINT('Ctrl Pts',(-18.3339244481758,56.1290506323489,
2.67667072836693));
#232392=CARTESIAN_POINT('Ctrl Pts',(-18.3351633160338,56.1292563922629,
2.67721232541127));
#232393=CARTESIAN_POINT('Ctrl Pts',(-18.3363950287072,56.129475592512,2.67776268340084));
#232394=CARTESIAN_POINT('Ctrl Pts',(-18.3376191892287,56.1297079426454,
2.67832123541553));
#232395=CARTESIAN_POINT('Ctrl Pts',(-18.3462420178743,56.131344586983,2.68225560368481));
#232396=CARTESIAN_POINT('Ctrl Pts',(-18.3545284904605,56.1335959402409,
2.68661792998924));
#232397=CARTESIAN_POINT('Ctrl Pts',(-18.3624495731174,56.1363459252322,
2.69130986622614));
#232398=CARTESIAN_POINT('Ctrl Pts',(-18.3662912896464,56.1376796649813,
2.69358545023091));
#232399=CARTESIAN_POINT('Ctrl Pts',(-18.3700472768052,56.1391312300713,
2.69593918853507));
#232400=CARTESIAN_POINT('Ctrl Pts',(-18.3737149835765,56.1406901365235,
2.69836306235513));
#232401=CARTESIAN_POINT('Ctrl Pts',(-18.3793299863881,56.1430767133843,
2.70207384382246));
#232402=CARTESIAN_POINT('Ctrl Pts',(-18.3847354115624,56.145712562978,2.70594760814247));
#232403=CARTESIAN_POINT('Ctrl Pts',(-18.3899096889381,56.1485569297211,
2.70995196345727));
#232404=CARTESIAN_POINT('Ctrl Pts',(-18.3923126501195,56.1498778683514,
2.71181160678125));
#232405=CARTESIAN_POINT('Ctrl Pts',(-18.3946658026161,56.1512435269778,
2.71369962772117));
#232406=CARTESIAN_POINT('Ctrl Pts',(-18.396966172054,56.1526507491371,2.7156118313868));
#232407=CARTESIAN_POINT('Ctrl Pts',(-18.3971424863075,56.1527586071709,
2.71575839426331));
#232408=CARTESIAN_POINT('Ctrl Pts',(-18.3973185179288,56.1528666894396,
2.71590508903228));
#232409=CARTESIAN_POINT('Ctrl Pts',(-18.3974942667072,56.152974994498,2.7160519140993));
#232410=CARTESIAN_POINT('Ctrl Pts',(-18.3999630071782,56.1544963540397,
2.71811436362772));
#232411=CARTESIAN_POINT('Ctrl Pts',(-18.4023749585855,56.1560635207939,
2.72020091026978));
#232412=CARTESIAN_POINT('Ctrl Pts',(-18.4047288488037,56.1576709325005,
2.72230624862201));
#232413=CARTESIAN_POINT('Ctrl Pts',(-18.4131694805009,56.1634348250118,
2.72985561753131));
#232414=CARTESIAN_POINT('Ctrl Pts',(-18.4209299141242,56.1697591292907,
2.73770089914368));
#232415=CARTESIAN_POINT('Ctrl Pts',(-18.4280560759388,56.1765231650109,
2.74574823347121));
#232416=CARTESIAN_POINT('Ctrl Pts',(-18.4358870118864,56.1839561607596,
2.75459144547045));
#232417=CARTESIAN_POINT('Ctrl Pts',(-18.4429525945098,56.1919204977437,
2.76367911754261));
#232418=CARTESIAN_POINT('Ctrl Pts',(-18.4492898603068,56.2003032932666,
2.77292162564687));
#232419=CARTESIAN_POINT('Ctrl Pts',(-18.4561325169306,56.2093546086363,
2.78290121484599));
#232420=CARTESIAN_POINT('Ctrl Pts',(-18.462126884228,56.2188946068438,2.7930622949996));
#232421=CARTESIAN_POINT('Ctrl Pts',(-18.4672816799253,56.2288243369841,
2.80331916684929));
#232422=CARTESIAN_POINT('Ctrl Pts',(-18.4723932321842,56.2386707668931,
2.81348999408487));
#232423=CARTESIAN_POINT('Ctrl Pts',(-18.4766796388,56.2489017962816,2.82375635966791));
#232424=CARTESIAN_POINT('Ctrl Pts',(-18.4801050014193,56.259443978424,2.834041988603));
#232425=CARTESIAN_POINT('Origin',(0.0144941013083455,0.00470941899445838,
2.83404198860262));
#232426=CARTESIAN_POINT('Ctrl Pts',(-19.4061247292256,59.7752282754838,
2.65878198860303));
#232427=CARTESIAN_POINT('Ctrl Pts',(-19.3979550581546,59.7778789856304,
2.65878198860303));
#232428=CARTESIAN_POINT('Ctrl Pts',(-19.3896365599069,59.7798236858212,
2.65944603041887));
#232429=CARTESIAN_POINT('Ctrl Pts',(-19.3813136269518,59.7811061158281,
2.66070439264098));
#232430=CARTESIAN_POINT('Ctrl Pts',(-19.3759956690089,59.781925527552,2.66150842619625));
#232431=CARTESIAN_POINT('Ctrl Pts',(-19.3706760212379,59.7824754874622,
2.66255428265402));
#232432=CARTESIAN_POINT('Ctrl Pts',(-19.3653918801541,59.7827759879496,
2.66381699700696));
#232433=CARTESIAN_POINT('Ctrl Pts',(-19.3581800878464,59.7831861108191,
2.66554034873296));
#232434=CARTESIAN_POINT('Ctrl Pts',(-19.3510354548621,59.7831255716888,
2.66766759644));
#232435=CARTESIAN_POINT('Ctrl Pts',(-19.3440445557098,59.7826350657125,
2.67012012783176));
#232436=CARTESIAN_POINT('Ctrl Pts',(-19.3405491061336,59.7823898127244,
2.67134639352764));
#232437=CARTESIAN_POINT('Ctrl Pts',(-19.3370918919976,59.78203713438,2.6726537558504));
#232438=CARTESIAN_POINT('Ctrl Pts',(-19.3336823180311,59.781582586544,2.67403135126968));
#232439=CARTESIAN_POINT('Ctrl Pts',(-19.3319775310479,59.781355312626,2.67472014897931));
#232440=CARTESIAN_POINT('Ctrl Pts',(-19.3302846375612,59.7811025767644,
2.6754264966866));
#232441=CARTESIAN_POINT('Ctrl Pts',(-19.3286047092266,59.7808251076838,
2.67614899656129));
#232442=CARTESIAN_POINT('Ctrl Pts',(-19.328184727143,59.7807557404136,2.67632962152997));
#232443=CARTESIAN_POINT('Ctrl Pts',(-19.3277655550292,59.7806848274339,
2.67651125590978));
#232444=CARTESIAN_POINT('Ctrl Pts',(-19.3273472089198,59.7806123803668,
2.67669387767551));
#232445=CARTESIAN_POINT('Ctrl Pts',(-19.3260921705915,59.7803950391654,
2.67724174297271));
#232446=CARTESIAN_POINT('Ctrl Pts',(-19.3248445680579,59.7801638905869,
2.67779849504775));
#232447=CARTESIAN_POINT('Ctrl Pts',(-19.3236048185588,59.779919253687,2.67836353618036));
#232448=CARTESIAN_POINT('Ctrl Pts',(-19.3150373803112,59.7782286609228,
2.68226832098929));
#232449=CARTESIAN_POINT('Ctrl Pts',(-19.3068044648777,59.7759321681723,
2.68659153751405));
#232450=CARTESIAN_POINT('Ctrl Pts',(-19.298932284441,59.7731456380812,2.69123699486184));
#232451=CARTESIAN_POINT('Ctrl Pts',(-19.2950198323725,59.7717607402747,
2.69354577441228));
#232452=CARTESIAN_POINT('Ctrl Pts',(-19.2911962646694,59.770254230293,2.69593478828135));
#232453=CARTESIAN_POINT('Ctrl Pts',(-19.2874640247236,59.7686372707432,
2.69839565261244));
#232454=CARTESIAN_POINT('Ctrl Pts',(-19.2792301459419,59.7650700164611,
2.70382468689069));
#232455=CARTESIAN_POINT('Ctrl Pts',(-19.2714367138416,59.7609769706903,
2.70961155815111));
#232456=CARTESIAN_POINT('Ctrl Pts',(-19.2641757185814,59.7564706723514,
2.71562701361791));
#232457=CARTESIAN_POINT('Ctrl Pts',(-19.2615231854469,59.7548244647407,
2.71782453535881));
#232458=CARTESIAN_POINT('Ctrl Pts',(-19.2589351484757,59.753127615532,2.72005051502424));
#232459=CARTESIAN_POINT('Ctrl Pts',(-19.2564118357498,59.7513854342767,
2.72229986760136));
#232460=CARTESIAN_POINT('Ctrl Pts',(-19.2479362953115,59.7455336317917,
2.72985520488924));
#232461=CARTESIAN_POINT('Ctrl Pts',(-19.2401420439513,59.7391263493539,
2.73770845534603));
#232462=CARTESIAN_POINT('Ctrl Pts',(-19.2329840462263,59.732283726861,2.74576706701812));
#232463=CARTESIAN_POINT('Ctrl Pts',(-19.2251165588061,59.7247628741795,
2.75462443585104));
#232464=CARTESIAN_POINT('Ctrl Pts',(-19.2180171087281,59.7167157560768,
2.76373036323274));
#232465=CARTESIAN_POINT('Ctrl Pts',(-19.2116502033053,59.7082546997617,
2.77299664636931));
#232466=CARTESIAN_POINT('Ctrl Pts',(-19.2047927733647,59.6991417795828,
2.78297683033612));
#232467=CARTESIAN_POINT('Ctrl Pts',(-19.1987842816746,59.6895478206973,
2.79314401479056));
#232468=CARTESIAN_POINT('Ctrl Pts',(-19.1936187207948,59.6795708631985,
2.80341452428128));
#232469=CARTESIAN_POINT('Ctrl Pts',(-19.1885229124286,59.6697286283136,
2.81354634721501));
#232470=CARTESIAN_POINT('Ctrl Pts',(-19.1842470541688,59.6595122814313,
2.82378004209289));
#232471=CARTESIAN_POINT('Ctrl Pts',(-19.1808295835784,59.6489943884565,
2.83404198860303));
#232472=CARTESIAN_POINT('Ctrl Pts',(-18.1177524687109,56.3771794532808,
2.83404198860299));
#232473=CARTESIAN_POINT('Ctrl Pts',(-18.1144819305952,56.3671137719646,
2.8242212644304));
#232474=CARTESIAN_POINT('Ctrl Pts',(-18.112017069978,56.3568263239567,2.8144281502853));
#232475=CARTESIAN_POINT('Ctrl Pts',(-18.110362919665,56.346374945335,2.80471618166343));
#232476=CARTESIAN_POINT('Ctrl Pts',(-18.1087656919993,56.336283219723,2.79533842146253));
#232477=CARTESIAN_POINT('Ctrl Pts',(-18.1079242184406,56.3260373921216,
2.78603515650262));
#232478=CARTESIAN_POINT('Ctrl Pts',(-18.107887916365,56.3156801719831,2.77685887346776));
#232479=CARTESIAN_POINT('Ctrl Pts',(-18.1078535995344,56.3058893552718,
2.76818441216597));
#232480=CARTESIAN_POINT('Ctrl Pts',(-18.1085387949866,56.2959980926921,
2.75962261521643));
#232481=CARTESIAN_POINT('Ctrl Pts',(-18.1100266905431,56.2860490151131,
2.75123537701679));
#232482=CARTESIAN_POINT('Ctrl Pts',(-18.1113970173892,56.2768860815712,
2.7435108713414));
#232483=CARTESIAN_POINT('Ctrl Pts',(-18.1134483398652,56.2676735798191,
2.7359339944987));
#232484=CARTESIAN_POINT('Ctrl Pts',(-18.1162805994784,56.2584600414655,
2.72857657812602));
#232485=CARTESIAN_POINT('Ctrl Pts',(-18.1171251221219,56.2557127503167,
2.72638274508348));
#232486=CARTESIAN_POINT('Ctrl Pts',(-18.1180393245077,56.2529655048677,
2.72420861709626));
#232487=CARTESIAN_POINT('Ctrl Pts',(-18.1190265064342,56.2502199893833,
2.72205663736746));
#232488=CARTESIAN_POINT('Ctrl Pts',(-18.1200036017944,56.2475025263007,
2.71992664556785));
#232489=CARTESIAN_POINT('Ctrl Pts',(-18.1210509212418,56.2447894850831,
2.71782089927904));
#232490=CARTESIAN_POINT('Ctrl Pts',(-18.1221702476366,56.2420855046791,
2.71574387311265));
#232491=CARTESIAN_POINT('Ctrl Pts',(-18.1222480834051,56.24189747517,2.71559944077506));
#232492=CARTESIAN_POINT('Ctrl Pts',(-18.1223262596101,56.2417094803632,
2.71545515216088));
#232493=CARTESIAN_POINT('Ctrl Pts',(-18.1224047773506,56.2415215209615,
2.7153110078175));
#232494=CARTESIAN_POINT('Ctrl Pts',(-18.1258472827277,56.2332806922383,
2.70899119176101));
#232495=CARTESIAN_POINT('Ctrl Pts',(-18.1299826829657,56.2251347899179,
2.70298296066855));
#232496=CARTESIAN_POINT('Ctrl Pts',(-18.1348427679841,56.2171955585586,
2.69736727774152));
#232497=CARTESIAN_POINT('Ctrl Pts',(-18.1393732118984,56.2097948151027,
2.69213248525441));
#232498=CARTESIAN_POINT('Ctrl Pts',(-18.144534000151,56.2025731376012,2.68723866185478));
#232499=CARTESIAN_POINT('Ctrl Pts',(-18.1503626543103,56.195647929963,2.6827859582957));
#232500=CARTESIAN_POINT('Ctrl Pts',(-18.1524948514083,56.193114599416,2.68115710172816));
#232501=CARTESIAN_POINT('Ctrl Pts',(-18.1547164978842,56.1906212529493,
2.67958763637824));
#232502=CARTESIAN_POINT('Ctrl Pts',(-18.1570296338739,56.1881748397226,
2.67808378645381));
#232503=CARTESIAN_POINT('Ctrl Pts',(-18.1575858658044,56.187586559069,2.67772216078617));
#232504=CARTESIAN_POINT('Ctrl Pts',(-18.1581479603548,56.1870008763869,
2.6773640360358));
#232505=CARTESIAN_POINT('Ctrl Pts',(-18.1587158783115,56.1864179215673,
2.67700956934496));
#232506=CARTESIAN_POINT('Ctrl Pts',(-18.159266048832,56.1858531840859,2.67666617973821));
#232507=CARTESIAN_POINT('Ctrl Pts',(-18.1598216844587,56.1852910066467,
2.67632622314135));
#232508=CARTESIAN_POINT('Ctrl Pts',(-18.1603827459286,56.1847315084905,
2.6759898415879));
#232509=CARTESIAN_POINT('Ctrl Pts',(-18.1665298227359,56.1786015595926,
2.67230439292242));
#232510=CARTESIAN_POINT('Ctrl Pts',(-18.1733325302112,56.1727894828611,
2.6690496454));
#232511=CARTESIAN_POINT('Ctrl Pts',(-18.1807122308848,56.1674665972294,
2.66640203566752));
#232512=CARTESIAN_POINT('Ctrl Pts',(-18.1837728127196,56.1652590378996,
2.66530399299463));
#232513=CARTESIAN_POINT('Ctrl Pts',(-18.1869322368374,56.1631354730309,
2.66430995142278));
#232514=CARTESIAN_POINT('Ctrl Pts',(-18.1901833857455,56.161107088044,2.66343053473377));
#232515=CARTESIAN_POINT('Ctrl Pts',(-18.1957285590018,56.1576474660762,
2.661930597929));
#232516=CARTESIAN_POINT('Ctrl Pts',(-18.2015400422205,56.1544671656479,
2.66076519817144));
#232517=CARTESIAN_POINT('Ctrl Pts',(-18.2075773774754,56.1516266854597,
2.65997805604476));
#232518=CARTESIAN_POINT('Ctrl Pts',(-18.2105960451029,56.1502064453656,
2.65958448498142));
#232519=CARTESIAN_POINT('Ctrl Pts',(-18.2136716866512,56.1488725139555,
2.65928526260778));
#232520=CARTESIAN_POINT('Ctrl Pts',(-18.2167992197298,56.1476325143036,
2.65908463971341));
#232521=CARTESIAN_POINT('Ctrl Pts',(-18.2199267528084,56.1463925146518,
2.65888401681903));
#232522=CARTESIAN_POINT('Ctrl Pts',(-18.2231061318822,56.1452464433753,
2.658781988603));
#232523=CARTESIAN_POINT('Ctrl Pts',(-18.2263320786585,56.1441998575529,
2.658781988603));
#232524=CARTESIAN_POINT('Origin',(-23.7119335237428,53.2204057122639,2.83404198860298));
#232525=CARTESIAN_POINT('Ctrl Pts',(-25.6588335304443,57.1623216544372,
2.83404198860301));
#232526=CARTESIAN_POINT('Ctrl Pts',(-25.6631491402569,57.172014672778,2.82419652440111));
#232527=CARTESIAN_POINT('Ctrl Pts',(-25.6666871334687,57.1820194461959,
2.81438790575699));
#232528=CARTESIAN_POINT('Ctrl Pts',(-25.6694381454821,57.1922776320707,
2.80466781256952));
#232529=CARTESIAN_POINT('Ctrl Pts',(-25.6720997659863,57.2022024879881,
2.79526356453127));
#232530=CARTESIAN_POINT('Ctrl Pts',(-25.6740249857412,57.2123658169604,
2.78594102496278));
#232531=CARTESIAN_POINT('Ctrl Pts',(-25.675161647087,57.2227298227167,2.7767510908882));
#232532=CARTESIAN_POINT('Ctrl Pts',(-25.6762368587287,57.2325335339835,
2.76805797913715));
#232533=CARTESIAN_POINT('Ctrl Pts',(-25.6766065729229,57.2425177322909,
2.75948271210185));
#232534=CARTESIAN_POINT('Ctrl Pts',(-25.6761845643574,57.2526488462852,
2.7510857557324));
#232535=CARTESIAN_POINT('Ctrl Pts',(-25.6757958639481,57.2619803349748,
2.74335155163276));
#232536=CARTESIAN_POINT('Ctrl Pts',(-25.6747354076182,57.2714370189572,
2.73576818685939));
#232537=CARTESIAN_POINT('Ctrl Pts',(-25.6728992535085,57.2809814365682,
2.72840626160486));
#232538=CARTESIAN_POINT('Ctrl Pts',(-25.6723666549989,57.2837499093059,
2.72627084693685));
#232539=CARTESIAN_POINT('Ctrl Pts',(-25.6717685445831,57.2865256584305,
2.72415424587543));
#232540=CARTESIAN_POINT('Ctrl Pts',(-25.6711017521907,57.2893074725861,
2.72205867173295));
#232541=CARTESIAN_POINT('Ctrl Pts',(-25.6703789063664,57.2923231379857,
2.71978693462898));
#232542=CARTESIAN_POINT('Ctrl Pts',(-25.6695773996876,57.2953419866644,
2.71754411340799));
#232543=CARTESIAN_POINT('Ctrl Pts',(-25.6686939261489,57.2983617649665,
2.71533341844297));
#232544=CARTESIAN_POINT('Ctrl Pts',(-25.6662692260896,57.3066495702124,
2.70926614876445));
#232545=CARTESIAN_POINT('Ctrl Pts',(-25.6631888860747,57.3149216961107,
2.70347381860462));
#232546=CARTESIAN_POINT('Ctrl Pts',(-25.6594348051809,57.3230760282581,
2.69804914171448));
#232547=CARTESIAN_POINT('Ctrl Pts',(-25.656000024977,57.3305367994638,2.69308585687273));
#232548=CARTESIAN_POINT('Ctrl Pts',(-25.6519962425131,57.3378885241127,
2.68842799053268));
#232549=CARTESIAN_POINT('Ctrl Pts',(-25.6473759219982,57.3450563828664,
2.68414767054311));
#232550=CARTESIAN_POINT('Ctrl Pts',(-25.6451064356541,57.3485772116717,
2.68204519134631));
#232551=CARTESIAN_POINT('Ctrl Pts',(-25.6426878935085,57.3520532672062,
2.68003431778569));
#232552=CARTESIAN_POINT('Ctrl Pts',(-25.6401130415749,57.3554727521282,
2.67812693945307));
#232553=CARTESIAN_POINT('Ctrl Pts',(-25.6396244884999,57.3561215660859,
2.67776503299259));
#232554=CARTESIAN_POINT('Ctrl Pts',(-25.6391297826974,57.3567684269678,
2.67740659639979));
#232555=CARTESIAN_POINT('Ctrl Pts',(-25.6386289474846,57.3574131967123,
2.67705178968911));
#232556=CARTESIAN_POINT('Ctrl Pts',(-25.6381437633721,57.3580378174023,
2.67670807068813));
#232557=CARTESIAN_POINT('Ctrl Pts',(-25.637652826975,57.3586604755992,2.67636775825321));
#232558=CARTESIAN_POINT('Ctrl Pts',(-25.6371561630117,57.3592810442416,
2.67603099699311));
#232559=CARTESIAN_POINT('Ctrl Pts',(-25.6317436214791,57.366043873435,2.6723610421718));
#232560=CARTESIAN_POINT('Ctrl Pts',(-25.6256469885829,57.3725627409498,
2.66911440541522));
#232561=CARTESIAN_POINT('Ctrl Pts',(-25.6189233999294,57.3786559602409,
2.66646778189677));
#232562=CARTESIAN_POINT('Ctrl Pts',(-25.6160839866896,57.3812291645844,
2.66535009635023));
#232563=CARTESIAN_POINT('Ctrl Pts',(-25.6131331854692,57.3837265592146,
2.66433897912396));
#232564=CARTESIAN_POINT('Ctrl Pts',(-25.6100770039414,57.3861353831633,
2.66344564884847));
#232565=CARTESIAN_POINT('Ctrl Pts',(-25.6049304706141,57.3901917825032,
2.66194130298639));
#232566=CARTESIAN_POINT('Ctrl Pts',(-25.5994853721132,57.3939944983915,
2.66077206705474));
#232567=CARTESIAN_POINT('Ctrl Pts',(-25.5937750303535,57.3974772155319,
2.65998225155768));
#232568=CARTESIAN_POINT('Ctrl Pts',(-25.5923474449136,57.3983478948169,
2.65978479768341));
#232569=CARTESIAN_POINT('Ctrl Pts',(-25.5909031732847,57.3991983668808,
2.65961098966675));
#232570=CARTESIAN_POINT('Ctrl Pts',(-25.5894426040348,57.4000273167774,
2.65946139030554));
#232571=CARTESIAN_POINT('Ctrl Pts',(-25.58725175016,57.4012707416222,2.65923699126373));
#232572=CARTESIAN_POINT('Ctrl Pts',(-25.585024235439,57.4024657229514,2.65906707562494));
#232573=CARTESIAN_POINT('Ctrl Pts',(-25.5827620706102,57.40360934828,2.65895332562972));
#232574=CARTESIAN_POINT('Ctrl Pts',(-25.5804999057814,57.4047529736086,
2.65883957563449));
#232575=CARTESIAN_POINT('Ctrl Pts',(-25.5782031010741,57.4058452484213,
2.65878198860301));
#232576=CARTESIAN_POINT('Ctrl Pts',(-25.5758735661218,57.4068835917996,
2.65878198860301));
#232577=CARTESIAN_POINT('Ctrl Pts',(-24.0229981225299,53.9190682401996,
2.65878198860299));
#232578=CARTESIAN_POINT('Ctrl Pts',(-24.0308804555191,53.9155545931358,
2.65878198860299));
#232579=CARTESIAN_POINT('Ctrl Pts',(-24.0389845034724,53.9127220553016,
2.65945335517895));
#232580=CARTESIAN_POINT('Ctrl Pts',(-24.0471612846387,53.9105453488013,
2.66072561226648));
#232581=CARTESIAN_POINT('Ctrl Pts',(-24.0524426462856,53.9091394197453,
2.66154735980385));
#232582=CARTESIAN_POINT('Ctrl Pts',(-24.0577541205278,53.9080061861139,
2.66261895766927));
#232583=CARTESIAN_POINT('Ctrl Pts',(-24.0630550795263,53.9071299964542,
2.66391429251066));
#232584=CARTESIAN_POINT('Ctrl Pts',(-24.0700811970214,53.9059686572516,
2.66563118464163));
#232585=CARTESIAN_POINT('Ctrl Pts',(-24.0770886066608,53.9052646847387,
2.66774105138738));
#232586=CARTESIAN_POINT('Ctrl Pts',(-24.0839917000394,53.9049900928805,
2.67016894181789));
#232587=CARTESIAN_POINT('Ctrl Pts',(-24.0874432467287,53.9048527969514,
2.67138288703315));
#232588=CARTESIAN_POINT('Ctrl Pts',(-24.0908688957001,53.9048227635324,
2.67267613167591));
#232589=CARTESIAN_POINT('Ctrl Pts',(-24.0942592346731,53.9048959123384,
2.67403835432593));
#232590=CARTESIAN_POINT('Ctrl Pts',(-24.0959544041596,53.9049324867414,
2.67471946565094));
#232591=CARTESIAN_POINT('Ctrl Pts',(-24.0976407611372,53.9049948499729,
2.67541781389562));
#232592=CARTESIAN_POINT('Ctrl Pts',(-24.099317223136,53.9050824496423,2.67613207244208));
#232593=CARTESIAN_POINT('Ctrl Pts',(-24.0997363386357,53.9051043495596,
2.6763106370787));
#232594=CARTESIAN_POINT('Ctrl Pts',(-24.1001548360176,53.9051278266103,
2.67649019601884));
#232595=CARTESIAN_POINT('Ctrl Pts',(-24.1005726990102,53.9051528718724,
2.67667072836696));
#232596=CARTESIAN_POINT('Ctrl Pts',(-24.1018262879881,53.9052280076586,
2.67721232541129));
#232597=CARTESIAN_POINT('Ctrl Pts',(-24.1030741658757,53.9053172580729,
2.67776268340086));
#232598=CARTESIAN_POINT('Ctrl Pts',(-24.1043159075202,53.9054203757498,
2.67832123541555));
#232599=CARTESIAN_POINT('Ctrl Pts',(-24.113062575326,53.9061467233511,2.6822556036849));
#232600=CARTESIAN_POINT('Ctrl Pts',(-24.1215389842448,53.9075195712151,
2.68661792998942));
#232601=CARTESIAN_POINT('Ctrl Pts',(-24.1297041260874,53.9094265129033,
2.6913098662264));
#232602=CARTESIAN_POINT('Ctrl Pts',(-24.1336642110575,53.9103513775614,
2.69358545023109));
#232603=CARTESIAN_POINT('Ctrl Pts',(-24.1375513523937,53.9114023832601,
2.69593918853516));
#232604=CARTESIAN_POINT('Ctrl Pts',(-24.1413619171793,53.9125693701072,
2.69836306235513));
#232605=CARTESIAN_POINT('Ctrl Pts',(-24.1471956256297,53.9143559454351,
2.70207384382245));
#232606=CARTESIAN_POINT('Ctrl Pts',(-24.1528469606267,53.9164123347821,
2.70594760814245));
#232607=CARTESIAN_POINT('Ctrl Pts',(-24.1582902100542,53.9187002605239,
2.70995196345725));
#232608=CARTESIAN_POINT('Ctrl Pts',(-24.1608180832479,53.9197627850746,
2.71181160678123));
#232609=CARTESIAN_POINT('Ctrl Pts',(-24.1633010951265,53.9208749910659,
2.71369962772116));
#232610=CARTESIAN_POINT('Ctrl Pts',(-24.1657359576696,53.9220340502327,
2.71561183138678));
#232611=CARTESIAN_POINT('Ctrl Pts',(-24.1659225802897,53.922122887551,2.71575839426329));
#232612=CARTESIAN_POINT('Ctrl Pts',(-24.1661089452649,53.9222119774188,
2.71590508903226));
#232613=CARTESIAN_POINT('Ctrl Pts',(-24.1662950522344,53.9223013184211,
2.71605191409929));
#232614=CARTESIAN_POINT('Ctrl Pts',(-24.1689092940617,53.9235562901483,
2.7181143636277));
#232615=CARTESIAN_POINT('Ctrl Pts',(-24.1714718460794,53.924862754225,2.72020091026977));
#232616=CARTESIAN_POINT('Ctrl Pts',(-24.1739808617162,53.9262153118349,
2.72230624862199));
#232617=CARTESIAN_POINT('Ctrl Pts',(-24.1829777455765,53.9310653428796,
2.72985561753131));
#232618=CARTESIAN_POINT('Ctrl Pts',(-24.1913567365399,53.936543815757,2.73770089914369));
#232619=CARTESIAN_POINT('Ctrl Pts',(-24.1991508947539,53.9425259106384,
2.74574823347124));
#232620=CARTESIAN_POINT('Ctrl Pts',(-24.2077158916383,53.9490996319582,
2.75459144547067));
#232621=CARTESIAN_POINT('Ctrl Pts',(-24.2155752681668,53.9562817849775,
2.76367911754305));
#232622=CARTESIAN_POINT('Ctrl Pts',(-24.2227540584928,53.9639562340145,
2.77292162564753));
#232623=CARTESIAN_POINT('Ctrl Pts',(-24.2305053504141,53.9722427129505,
2.78290121484725));
#232624=CARTESIAN_POINT('Ctrl Pts',(-24.2374640812929,53.9811038680483,
2.79306229500149));
#232625=CARTESIAN_POINT('Ctrl Pts',(-24.2436285779125,53.9904403792159,
2.8033191668518));
#232626=CARTESIAN_POINT('Ctrl Pts',(-24.2497413607397,53.9996985666484,
2.81348999408656));
#232627=CARTESIAN_POINT('Ctrl Pts',(-24.2550737197506,54.0094254978901,
2.82375635966875));
#232628=CARTESIAN_POINT('Ctrl Pts',(-24.2595822759735,54.0195518809642,
2.83404198860299));
#232629=CARTESIAN_POINT('Origin',(0.0139224327744811,0.00619866644065959,
2.83404198860262));
#232630=CARTESIAN_POINT('Ctrl Pts',(-25.5480287005721,57.419280924679,2.65878198860301));
#232631=CARTESIAN_POINT('Ctrl Pts',(-25.5401808584718,57.4227710771206,
2.65878198860301));
#232632=CARTESIAN_POINT('Ctrl Pts',(-25.53211120635,57.425574643879,2.65944603041891));
#232633=CARTESIAN_POINT('Ctrl Pts',(-25.5239679177299,57.4277200319918,
2.66070439264113));
#232634=CARTESIAN_POINT('Ctrl Pts',(-25.5187647439657,57.4290908328639,
2.66150842619636));
#232635=CARTESIAN_POINT('Ctrl Pts',(-25.5135317242465,57.4301938346427,
2.66255428265407));
#232636=CARTESIAN_POINT('Ctrl Pts',(-25.5083079410949,57.4310450321042,
2.66381699700691));
#232637=CARTESIAN_POINT('Ctrl Pts',(-25.5011785252534,57.432206745845,2.6655403487329));
#232638=CARTESIAN_POINT('Ctrl Pts',(-25.4940667032539,57.4328933558608,
2.66766759643994));
#232639=CARTESIAN_POINT('Ctrl Pts',(-25.4870628291427,57.4331362848729,
2.67012012783169));
#232640=CARTESIAN_POINT('Ctrl Pts',(-25.483560892087,57.4332577493789,2.67134639352757));
#232641=CARTESIAN_POINT('Ctrl Pts',(-25.4800857520065,57.4332683803242,
2.67265375585033));
#232642=CARTESIAN_POINT('Ctrl Pts',(-25.4766473428561,57.4331727200759,
2.67403135126961));
#232643=CARTESIAN_POINT('Ctrl Pts',(-25.4749281382809,57.4331248899517,
2.67472014897925));
#232644=CARTESIAN_POINT('Ctrl Pts',(-25.4732181005507,57.4330504941582,
2.67542649668654));
#232645=CARTESIAN_POINT('Ctrl Pts',(-25.4715183716227,57.4329501454095,
2.67614899656123));
#232646=CARTESIAN_POINT('Ctrl Pts',(-25.4710934393907,57.4329250582223,
2.6763296215299));
#232647=CARTESIAN_POINT('Ctrl Pts',(-25.4706691511208,57.4328983491282,
2.67651125590971));
#232648=CARTESIAN_POINT('Ctrl Pts',(-25.4702455239745,57.4328700280097,
2.67669387767545));
#232649=CARTESIAN_POINT('Ctrl Pts',(-25.4689746425357,57.4327850646539,
2.67724174297265));
#232650=CARTESIAN_POINT('Ctrl Pts',(-25.4677097128937,57.4326855923071,
2.67779849504769));
#232651=CARTESIAN_POINT('Ctrl Pts',(-25.4664511833529,57.4325718846638,
2.6783635361803));
#232652=CARTESIAN_POINT('Ctrl Pts',(-25.4577539633644,57.4317860942977,
2.68226832098941));
#232653=CARTESIAN_POINT('Ctrl Pts',(-25.4493260998446,57.4303627559732,
2.68659153751438));
#232654=CARTESIAN_POINT('Ctrl Pts',(-25.4412057723274,57.428414357709,2.69123699486241));
#232655=CARTESIAN_POINT('Ctrl Pts',(-25.4371699918416,57.42744600912,2.69354577441267));
#232656=CARTESIAN_POINT('Ctrl Pts',(-25.4332098968695,57.4263474236139,
2.69593478828154));
#232657=CARTESIAN_POINT('Ctrl Pts',(-25.4293290842281,57.4251294472438,
2.69839565261242));
#232658=CARTESIAN_POINT('Ctrl Pts',(-25.4207674318877,57.4224424094498,
2.70382468689068));
#232659=CARTESIAN_POINT('Ctrl Pts',(-25.4125888532393,57.419186421293,2.70961155815109));
#232660=CARTESIAN_POINT('Ctrl Pts',(-25.4048965980306,57.4154637896042,
2.7156270136179));
#232661=CARTESIAN_POINT('Ctrl Pts',(-25.4020865201984,57.4141038653034,
2.71782453535881));
#232662=CARTESIAN_POINT('Ctrl Pts',(-25.3993352917243,57.4126868351397,
2.72005051502425));
#232663=CARTESIAN_POINT('Ctrl Pts',(-25.3966436944401,57.4112179557372,
2.72229986760139));
#232664=CARTESIAN_POINT('Ctrl Pts',(-25.3876029039784,57.4062841452561,
2.72985520488901));
#232665=CARTESIAN_POINT('Ctrl Pts',(-25.3791816069562,57.4007266836993,
2.73770845534555));
#232666=CARTESIAN_POINT('Ctrl Pts',(-25.3713475726781,57.3946697603111,
2.74576706701736));
#232667=CARTESIAN_POINT('Ctrl Pts',(-25.3627370410042,57.3880124840177,
2.75462443585));
#232668=CARTESIAN_POINT('Ctrl Pts',(-25.3548353295678,57.380751543477,2.7637303632314));
#232669=CARTESIAN_POINT('Ctrl Pts',(-25.3476188815051,57.3730023605538,
2.77299664636762));
#232670=CARTESIAN_POINT('Ctrl Pts',(-25.3398464577413,57.3646561585193,
2.78297683033401));
#232671=CARTESIAN_POINT('Ctrl Pts',(-25.3328680394185,57.3557428147478,
2.793144014788));
#232672=CARTESIAN_POINT('Ctrl Pts',(-25.3266878999863,57.3463604602072,
2.80341452427818));
#232673=CARTESIAN_POINT('Ctrl Pts',(-25.320591213303,57.3371047991314,2.81354634721299));
#232674=CARTESIAN_POINT('Ctrl Pts',(-25.3152708796015,57.327391367358,2.82378004209192));
#232675=CARTESIAN_POINT('Ctrl Pts',(-25.3107727110825,57.3172883154491,
2.83404198860301));
#232676=CARTESIAN_POINT('Ctrl Pts',(-23.9115214566117,54.174518541976,2.83404198860299));
#232677=CARTESIAN_POINT('Ctrl Pts',(-23.9072166846465,54.1648498658389,
2.82422126443081));
#232678=CARTESIAN_POINT('Ctrl Pts',(-23.9036899956625,54.1548764216405,
2.81442815028612));
#232679=CARTESIAN_POINT('Ctrl Pts',(-23.9009524404117,54.1446552025551,
2.80471618166465));
#232680=CARTESIAN_POINT('Ctrl Pts',(-23.8983090899564,54.1347857162257,
2.79533842146399));
#232681=CARTESIAN_POINT('Ctrl Pts',(-23.8964012454638,54.1246839742781,
2.78603515650431));
#232682=CARTESIAN_POINT('Ctrl Pts',(-23.8952825179499,54.1143872866757,
2.77685887346968));
#232683=CARTESIAN_POINT('Ctrl Pts',(-23.8942249700855,54.1046536921685,
2.76818441216801));
#232684=CARTESIAN_POINT('Ctrl Pts',(-23.8938724934879,54.0947449925327,
2.75962261521858));
#232685=CARTESIAN_POINT('Ctrl Pts',(-23.8943122764064,54.0846948896059,
2.75123537701903));
#232686=CARTESIAN_POINT('Ctrl Pts',(-23.8947173090964,54.0754389134133,
2.74351087134367));
#232687=CARTESIAN_POINT('Ctrl Pts',(-23.895794425562,54.0660624571237,2.73593399450098));
#232688=CARTESIAN_POINT('Ctrl Pts',(-23.8976480927552,54.0566033397524,
2.7285765781283));
#232689=CARTESIAN_POINT('Ctrl Pts',(-23.8982008188935,54.0537828218969,
2.72638274508499));
#232690=CARTESIAN_POINT('Ctrl Pts',(-23.8988228478382,54.0509550659744,
2.724208617097));
#232691=CARTESIAN_POINT('Ctrl Pts',(-23.8995176373646,54.0481214021003,
2.72205663736744));
#232692=CARTESIAN_POINT('Ctrl Pts',(-23.9002053278541,54.0453166912884,
2.71992664556783));
#232693=CARTESIAN_POINT('Ctrl Pts',(-23.9009633199468,54.0425090377021,
2.71782089927902));
#232694=CARTESIAN_POINT('Ctrl Pts',(-23.9017938716382,54.0397028685178,
2.71574387311264));
#232695=CARTESIAN_POINT('Ctrl Pts',(-23.9018516265785,54.0395077330007,
2.71559944077504));
#232696=CARTESIAN_POINT('Ctrl Pts',(-23.9019097237178,54.0393125964105,
2.71545515216087));
#232697=CARTESIAN_POINT('Ctrl Pts',(-23.9019681642225,54.0391174593313,
2.71531100781748));
#232698=CARTESIAN_POINT('Ctrl Pts',(-23.9045304100324,54.0305619349333,
2.708991191761));
#232699=CARTESIAN_POINT('Ctrl Pts',(-23.9077916774638,54.0220283896862,
2.70298296066855));
#232700=CARTESIAN_POINT('Ctrl Pts',(-23.9117952627745,54.0136246330487,
2.69736727774153));
#232701=CARTESIAN_POINT('Ctrl Pts',(-23.9155273001025,54.0057908712995,
2.69213248525441));
#232702=CARTESIAN_POINT('Ctrl Pts',(-23.9199049461656,53.9980693056377,
2.68723866185476));
#232703=CARTESIAN_POINT('Ctrl Pts',(-23.9249777890353,53.9905727747493,
2.68278595829567));
#232704=CARTESIAN_POINT('Ctrl Pts',(-23.9268335005856,53.987830446766,2.68115710172815));
#232705=CARTESIAN_POINT('Ctrl Pts',(-23.928782350975,53.9851185338202,2.67958763637824));
#232706=CARTESIAN_POINT('Ctrl Pts',(-23.9308270955486,53.9824437337508,
2.67808378645382));
#232707=CARTESIAN_POINT('Ctrl Pts',(-23.9313187883097,53.9818005336913,
2.67772216078618));
#232708=CARTESIAN_POINT('Ctrl Pts',(-23.9318165831367,53.9811593045605,
2.67736403603581));
#232709=CARTESIAN_POINT('Ctrl Pts',(-23.9323204546079,53.9805201796372,
2.67700956934497));
#232710=CARTESIAN_POINT('Ctrl Pts',(-23.9328085800956,53.9799010273677,
2.67666617973821));
#232711=CARTESIAN_POINT('Ctrl Pts',(-23.9333024083484,53.9792838498572,
2.67632622314136));
#232712=CARTESIAN_POINT('Ctrl Pts',(-23.9338019127824,53.9786687697972,
2.67598984158791));
#232713=CARTESIAN_POINT('Ctrl Pts',(-23.9392745611217,53.9719298569084,
2.67230439292238));
#232714=CARTESIAN_POINT('Ctrl Pts',(-23.9454324752045,53.9654385427828,
2.66904964539992));
#232715=CARTESIAN_POINT('Ctrl Pts',(-23.9522153560506,53.9593734277047,
2.66640203566742));
#232716=CARTESIAN_POINT('Ctrl Pts',(-23.9550284189135,53.9568580437001,
2.66530399299457));
#232717=CARTESIAN_POINT('Ctrl Pts',(-23.9579485624029,53.9544158621942,
2.66430995142276));
#232718=CARTESIAN_POINT('Ctrl Pts',(-23.9609698772114,53.9520587513133,
2.66343053473377));
#232719=CARTESIAN_POINT('Ctrl Pts',(-23.9661230444607,53.9480384530776,
2.661930597929));
#232720=CARTESIAN_POINT('Ctrl Pts',(-23.9715702598497,53.9442681092576,
2.66076519817143));
#232721=CARTESIAN_POINT('Ctrl Pts',(-23.9772776109214,53.9408121161407,
2.65997805604475));
#232722=CARTESIAN_POINT('Ctrl Pts',(-23.9801312864573,53.9390841195823,
2.65958448498141));
#232723=CARTESIAN_POINT('Ctrl Pts',(-23.983050645519,53.9374360035034,2.65928526260777));
#232724=CARTESIAN_POINT('Ctrl Pts',(-23.9860314303861,53.9358758804728,
2.65908463971339));
#232725=CARTESIAN_POINT('Ctrl Pts',(-23.9890122152532,53.9343157574423,
2.65888401681901));
#232726=CARTESIAN_POINT('Ctrl Pts',(-23.9920543802863,53.9328436288554,
2.65878198860299));
#232727=CARTESIAN_POINT('Ctrl Pts',(-23.995153256981,53.9314655730805,2.65878198860299));
#232728=CARTESIAN_POINT('Origin',(-29.1450842944632,50.4502867888876,2.83404198860296));
#232729=CARTESIAN_POINT('Ctrl Pts',(-31.4933613949861,54.1671020372439,
2.83404198860299));
#232730=CARTESIAN_POINT('Ctrl Pts',(-31.4986665597483,54.1762908521544,
2.82419652440102));
#232731=CARTESIAN_POINT('Ctrl Pts',(-31.5032309550538,54.1858709973833,
2.81438790575682));
#232732=CARTESIAN_POINT('Ctrl Pts',(-31.507039169141,54.1957854287845,2.80466781256928));
#232733=CARTESIAN_POINT('Ctrl Pts',(-31.5107236389469,54.2053777002017,
2.79526356453096));
#232734=CARTESIAN_POINT('Ctrl Pts',(-31.5137006693056,54.2152841131322,
2.7859410249624));
#232735=CARTESIAN_POINT('Ctrl Pts',(-31.5159144374967,54.2254725303169,
2.77675109088775));
#232736=CARTESIAN_POINT('Ctrl Pts',(-31.5180085258895,54.2351101456071,
2.76805797913666));
#232737=CARTESIAN_POINT('Ctrl Pts',(-31.5194198476568,54.245001003775,2.75948271210131));
#232738=CARTESIAN_POINT('Ctrl Pts',(-31.5200591406753,54.2551207303737,
2.7510857557318));
#232739=CARTESIAN_POINT('Ctrl Pts',(-31.5206479757801,54.2644417304484,
2.7433515516321));
#232740=CARTESIAN_POINT('Ctrl Pts',(-31.5205818213852,54.2739574575971,
2.73576818685868));
#232741=CARTESIAN_POINT('Ctrl Pts',(-31.5197533892255,54.2836415202572,
2.7284062616041));
#232742=CARTESIAN_POINT('Ctrl Pts',(-31.5195130925471,54.286450498715,2.72627084693634));
#232743=CARTESIAN_POINT('Ctrl Pts',(-31.5192084034331,54.2892735615577,
2.72415424587518));
#232744=CARTESIAN_POINT('Ctrl Pts',(-31.5188360425581,54.2921098354281,
2.72205867173294));
#232745=CARTESIAN_POINT('Ctrl Pts',(-31.5184323794288,54.2951845386602,
2.71978693462897));
#232746=CARTESIAN_POINT('Ctrl Pts',(-31.5179508191006,54.2982706300314,
2.71754411340797));
#232747=CARTESIAN_POINT('Ctrl Pts',(-31.5173878381078,54.3013662138034,
2.71533341844295));
#232748=CARTESIAN_POINT('Ctrl Pts',(-31.5158427323552,54.309862067756,2.70926614876442));
#232749=CARTESIAN_POINT('Ctrl Pts',(-31.5136439393734,54.3184108612912,
2.70347381860459));
#232750=CARTESIAN_POINT('Ctrl Pts',(-31.5107627835359,54.3269129314608,
2.69804914171445));
#232751=CARTESIAN_POINT('Ctrl Pts',(-31.5081266823661,54.3346918640778,
2.69308585687251));
#232752=CARTESIAN_POINT('Ctrl Pts',(-31.5049132975212,54.3424218244384,
2.68842799053229));
#232753=CARTESIAN_POINT('Ctrl Pts',(-31.5010675328659,54.3500333719153,
2.68414767054259));
#232754=CARTESIAN_POINT('Ctrl Pts',(-31.4991785058299,54.3537721391718,
2.68204519134596));
#232755=CARTESIAN_POINT('Ctrl Pts',(-31.4971365594547,54.3574819590038,
2.68003431778549));
#232756=CARTESIAN_POINT('Ctrl Pts',(-31.4949332463336,54.3611518569451,
2.67812693945301));
#232757=CARTESIAN_POINT('Ctrl Pts',(-31.4945151891294,54.3618481843342,
2.67776503299253));
#232758=CARTESIAN_POINT('Ctrl Pts',(-31.494090808751,54.3625432124818,2.67740659639973));
#232759=CARTESIAN_POINT('Ctrl Pts',(-31.4936601139564,54.3632368016453,
2.67705178968905));
#232760=CARTESIAN_POINT('Ctrl Pts',(-31.4932428783741,54.3639087161475,
2.67670807068807));
#232761=CARTESIAN_POINT('Ctrl Pts',(-31.4928197168825,54.3645792801848,
2.67636775825315));
#232762=CARTESIAN_POINT('Ctrl Pts',(-31.4923906407828,54.3652483648081,
2.67603099699304));
#232763=CARTESIAN_POINT('Ctrl Pts',(-31.4877146578621,54.3725399111642,
2.67236104217182));
#232764=CARTESIAN_POINT('Ctrl Pts',(-31.4823328301625,54.3796603393082,
2.66911440541531));
#232765=CARTESIAN_POINT('Ctrl Pts',(-31.4762829888801,54.386422985696,2.66646778189689));
#232766=CARTESIAN_POINT('Ctrl Pts',(-31.4737281033388,54.3892788932596,
2.66535009635029));
#232767=CARTESIAN_POINT('Ctrl Pts',(-31.471054515739,54.3920710496178,2.66433897912396));
#232768=CARTESIAN_POINT('Ctrl Pts',(-31.4682668669588,54.3947861357356,
2.66344564884842));
#232769=CARTESIAN_POINT('Ctrl Pts',(-31.4635725360689,54.3993582729153,
2.66194130298635));
#232770=CARTESIAN_POINT('Ctrl Pts',(-31.4585547584354,54.4037093249068,
2.6607720670547));
#232771=CARTESIAN_POINT('Ctrl Pts',(-31.4532397415958,54.4077698566067,
2.65998225155764));
#232772=CARTESIAN_POINT('Ctrl Pts',(-31.4519109873859,54.4087849895317,
2.65978479768338));
#232773=CARTESIAN_POINT('Ctrl Pts',(-31.450563526166,54.4097817701145,2.65961098966672));
#232774=CARTESIAN_POINT('Ctrl Pts',(-31.4491976069262,54.4107588499961,
2.65946139030551));
#232775=CARTESIAN_POINT('Ctrl Pts',(-31.4471487280664,54.4122244698184,
2.6592369912637));
#232776=CARTESIAN_POINT('Ctrl Pts',(-31.4450583254661,54.4136457436056,
2.65906707562491));
#232777=CARTESIAN_POINT('Ctrl Pts',(-31.4429280944111,54.4150195646482,
2.65895332562969));
#232778=CARTESIAN_POINT('Ctrl Pts',(-31.4407978633561,54.4163933856909,
2.65883957563447));
#232779=CARTESIAN_POINT('Ctrl Pts',(-31.438627814593,54.4177197583745,2.65878198860299));
#232780=CARTESIAN_POINT('Ctrl Pts',(-31.4364195775146,54.4189959163078,
2.65878198860299));
#232781=CARTESIAN_POINT('Ctrl Pts',(-29.5274749692187,51.1126068659047,
2.65878198860297));
#232782=CARTESIAN_POINT('Ctrl Pts',(-29.5349468458355,51.1082885388127,
2.65878198860297));
#232783=CARTESIAN_POINT('Ctrl Pts',(-29.5427104181398,51.104624414238,2.65945335517903));
#232784=CARTESIAN_POINT('Ctrl Pts',(-29.5506148782584,51.1016049255938,
2.66072561226672));
#232785=CARTESIAN_POINT('Ctrl Pts',(-29.5557203484494,51.0996546457476,
2.66154735980405));
#232786=CARTESIAN_POINT('Ctrl Pts',(-29.5608842707094,51.0979724198486,
2.66261895766938));
#232787=CARTESIAN_POINT('Ctrl Pts',(-29.5660646037407,51.0965469289498,
2.66391429251063));
#232788=CARTESIAN_POINT('Ctrl Pts',(-29.5729308384267,51.0946575224203,
2.6656311846416));
#232789=CARTESIAN_POINT('Ctrl Pts',(-29.579826275578,51.0932249325814,2.66774105138736));
#232790=CARTESIAN_POINT('Ctrl Pts',(-29.5866628504239,51.0922302752235,
2.67016894181786));
#232791=CARTESIAN_POINT('Ctrl Pts',(-29.5900811378468,51.0917329465446,
2.67138288703312));
#232792=CARTESIAN_POINT('Ctrl Pts',(-29.5934848814075,51.091344999829,2.67267613167588));
#232793=CARTESIAN_POINT('Ctrl Pts',(-29.5968642938812,51.0910633609954,
2.6740383543259));
#232794=CARTESIAN_POINT('Ctrl Pts',(-29.598554000118,51.0909225415785,2.6747194656509));
#232795=CARTESIAN_POINT('Ctrl Pts',(-29.6002376377884,51.0908082908744,
2.67541781389559));
#232796=CARTESIAN_POINT('Ctrl Pts',(-29.6019140726117,51.0907201726672,
2.67613207244205));
#232797=CARTESIAN_POINT('Ctrl Pts',(-29.6023331813176,51.0906981431154,
2.67631063707867));
#232798=CARTESIAN_POINT('Ctrl Pts',(-29.6027518401471,51.0906777466681,
2.67649019601882));
#232799=CARTESIAN_POINT('Ctrl Pts',(-29.6031700319853,51.0906589761531,
2.67667072836693));
#232800=CARTESIAN_POINT('Ctrl Pts',(-29.6044246074998,51.0906026646082,
2.67721232541127));
#232801=CARTESIAN_POINT('Ctrl Pts',(-29.6056749785905,51.0905609873414,
2.67776268340083));
#232802=CARTESIAN_POINT('Ctrl Pts',(-29.6069206965766,51.090533742783,2.67832123541552));
#232803=CARTESIAN_POINT('Ctrl Pts',(-29.6156953732194,51.0903418356318,
2.68225560368482));
#232804=CARTESIAN_POINT('Ctrl Pts',(-29.6242688491607,51.0908211368932,
2.68661792998926));
#232805=CARTESIAN_POINT('Ctrl Pts',(-29.632588591186,51.0918641424261,2.69130986622617));
#232806=CARTESIAN_POINT('Ctrl Pts',(-29.6366236570778,51.0923699989826,
2.69358545023092));
#232807=CARTESIAN_POINT('Ctrl Pts',(-29.6405993642578,51.0930089302517,
2.69593918853506));
#232808=CARTESIAN_POINT('Ctrl Pts',(-29.6445110377126,51.0937712117415,
2.6983630623551));
#232809=CARTESIAN_POINT('Ctrl Pts',(-29.6504995364713,51.0949382114433,
2.70207384382243));
#232810=CARTESIAN_POINT('Ctrl Pts',(-29.6563348640822,51.0963926103117,
2.70594760814243));
#232811=CARTESIAN_POINT('Ctrl Pts',(-29.6619874481817,51.0980990280591,
2.70995196345723));
#232812=CARTESIAN_POINT('Ctrl Pts',(-29.66461253748,51.0988914972889,2.71181160678121));
#232813=CARTESIAN_POINT('Ctrl Pts',(-29.6671982043428,51.0997380650834,
2.71369962772114));
#232814=CARTESIAN_POINT('Ctrl Pts',(-29.6697408831278,51.1006362623629,
2.71561183138676));
#232815=CARTESIAN_POINT('Ctrl Pts',(-29.669935769438,51.1007051056453,2.71575839426327));
#232816=CARTESIAN_POINT('Ctrl Pts',(-29.6701304259133,51.1007742270251,
2.71590508903224));
#232817=CARTESIAN_POINT('Ctrl Pts',(-29.670324852047,51.1008436251325,2.71605191409926));
#232818=CARTESIAN_POINT('Ctrl Pts',(-29.6730559530502,51.1018184593125,
2.71811436362768));
#232819=CARTESIAN_POINT('Ctrl Pts',(-29.675741029822,51.1028499068179,2.72020091026974));
#232820=CARTESIAN_POINT('Ctrl Pts',(-29.6783776815771,51.1039327914268,
2.72230624862197));
#232821=CARTESIAN_POINT('Ctrl Pts',(-29.687832245858,51.1078158230498,2.72985561753114));
#232822=CARTESIAN_POINT('Ctrl Pts',(-29.6967379921829,51.1123884412303,
2.73770089914337));
#232823=CARTESIAN_POINT('Ctrl Pts',(-29.7051147523676,51.1175230541893,
2.74574823347076));
#232824=CARTESIAN_POINT('Ctrl Pts',(-29.7143199702903,51.1231654780136,
2.75459144547006));
#232825=CARTESIAN_POINT('Ctrl Pts',(-29.7228870317499,51.1294867578963,
2.76367911754229));
#232826=CARTESIAN_POINT('Ctrl Pts',(-29.7308286942754,51.1363687775774,
2.77292162564662));
#232827=CARTESIAN_POINT('Ctrl Pts',(-29.7394036967177,51.1437996316818,
2.78290121484625));
#232828=CARTESIAN_POINT('Ctrl Pts',(-29.7472505498657,51.1518848589997,
2.79306229500039));
#232829=CARTESIAN_POINT('Ctrl Pts',(-29.7543572078924,51.1605258584237,
2.80331916685061));
#232830=CARTESIAN_POINT('Ctrl Pts',(-29.761404248361,51.1690943687417,2.81348999408575));
#232831=CARTESIAN_POINT('Ctrl Pts',(-29.7677241373266,51.1782106315437,
2.82375635966834));
#232832=CARTESIAN_POINT('Ctrl Pts',(-29.7732664904682,51.1878102687785,
2.83404198860297));
#232833=CARTESIAN_POINT('Origin',(0.0131982271536832,0.00762000000018464,
2.83404198860262));
#232834=CARTESIAN_POINT('Ctrl Pts',(-31.4100231232064,54.4342359163063,
2.65878198860299));
#232835=CARTESIAN_POINT('Ctrl Pts',(-31.402583092678,54.4385272722022,2.65878198860299));
#232836=CARTESIAN_POINT('Ctrl Pts',(-31.3948506994804,54.4421589890637,
2.6594460304188));
#232837=CARTESIAN_POINT('Ctrl Pts',(-31.3869762747706,54.4451438299612,
2.66070439264085));
#232838=CARTESIAN_POINT('Ctrl Pts',(-31.3819448922448,54.4470510012007,
2.66150842619612));
#232839=CARTESIAN_POINT('Ctrl Pts',(-31.3768558346355,54.44869496013,2.66255428265391));
#232840=CARTESIAN_POINT('Ctrl Pts',(-31.3717496422766,54.4500875286681,
2.66381699700688));
#232841=CARTESIAN_POINT('Ctrl Pts',(-31.3647807142731,54.4519881053014,
2.66554034873288));
#232842=CARTESIAN_POINT('Ctrl Pts',(-31.3577796218685,54.4534143418204,
2.66766759643993));
#232843=CARTESIAN_POINT('Ctrl Pts',(-31.3508395087087,54.4543880442397,
2.67012012783169));
#232844=CARTESIAN_POINT('Ctrl Pts',(-31.3473694521289,54.4548748954494,
2.67134639352757));
#232845=CARTESIAN_POINT('Ctrl Pts',(-31.3439144604656,54.4552487192095,
2.67265375585033));
#232846=CARTESIAN_POINT('Ctrl Pts',(-31.3404848880616,54.4555129946226,
2.67403135126961));
#232847=CARTESIAN_POINT('Ctrl Pts',(-31.3387701018596,54.4556451323291,
2.67472014897925));
#232848=CARTESIAN_POINT('Ctrl Pts',(-31.337061655417,54.4557498916997,2.67542649668654));
#232849=CARTESIAN_POINT('Ctrl Pts',(-31.3353607484814,54.4558277627247,
2.67614899656123));
#232850=CARTESIAN_POINT('Ctrl Pts',(-31.3349355217475,54.4558472304809,
2.6763296215299));
#232851=CARTESIAN_POINT('Ctrl Pts',(-31.3345107659126,54.4558650179029,
2.67651125590971));
#232852=CARTESIAN_POINT('Ctrl Pts',(-31.3340864990772,54.455881133025,2.67669387767544));
#232853=CARTESIAN_POINT('Ctrl Pts',(-31.3328136985709,54.4559294783912,
2.67724174297265));
#232854=CARTESIAN_POINT('Ctrl Pts',(-31.3315453006542,54.4559627721159,
2.67779849504768));
#232855=CARTESIAN_POINT('Ctrl Pts',(-31.3302817797847,54.4559812395338,
2.6783635361803));
#232856=CARTESIAN_POINT('Ctrl Pts',(-31.3215500666182,54.4561088608497,
2.68226832098925));
#232857=CARTESIAN_POINT('Ctrl Pts',(-31.3130195924491,54.4555742713439,
2.68659153751404));
#232858=CARTESIAN_POINT('Ctrl Pts',(-31.3047400858596,54.4544853519659,
2.69123699486187));
#232859=CARTESIAN_POINT('Ctrl Pts',(-31.3006251938113,54.453944162024,2.69354577441229));
#232860=CARTESIAN_POINT('Ctrl Pts',(-31.2965719591988,54.453265537326,2.69593478828134));
#232861=CARTESIAN_POINT('Ctrl Pts',(-31.2925850928565,54.4524598885396,
2.6983956526124));
#232862=CARTESIAN_POINT('Ctrl Pts',(-31.2837894702121,54.4506825069819,
2.70382468689065));
#232863=CARTESIAN_POINT('Ctrl Pts',(-31.2753153512349,54.4482992497267,
2.70961155815107));
#232864=CARTESIAN_POINT('Ctrl Pts',(-31.2672761140353,54.4454010706198,
2.71562701361788));
#232865=CARTESIAN_POINT('Ctrl Pts',(-31.2643392793061,54.4443423292442,
2.71782453535879));
#232866=CARTESIAN_POINT('Ctrl Pts',(-31.2614550023641,54.4432206434044,
2.72005051502424));
#232867=CARTESIAN_POINT('Ctrl Pts',(-31.2586246102248,54.4420411592048,
2.72229986760139));
#232868=CARTESIAN_POINT('Ctrl Pts',(-31.2491176225323,54.4380793965878,
2.72985520488848));
#232869=CARTESIAN_POINT('Ctrl Pts',(-31.2401615453407,54.4334326446238,
2.73770845534446));
#232870=CARTESIAN_POINT('Ctrl Pts',(-31.2317373058287,54.4282277812603,
2.74576706701568));
#232871=CARTESIAN_POINT('Ctrl Pts',(-31.2224780686882,54.4225070198673,
2.75462443584773));
#232872=CARTESIAN_POINT('Ctrl Pts',(-31.2138606686978,54.4161118092728,
2.7637303632285));
#232873=CARTESIAN_POINT('Ctrl Pts',(-31.2058737429104,54.4091594014113,
2.77299664636408));
#232874=CARTESIAN_POINT('Ctrl Pts',(-31.1972714816249,54.4016713602574,
2.78297683032974));
#232875=CARTESIAN_POINT('Ctrl Pts',(-31.1893995936812,54.3935362880598,
2.79314401478298));
#232876=CARTESIAN_POINT('Ctrl Pts',(-31.1822725865976,54.3848513315174,
2.80341452427241));
#232877=CARTESIAN_POINT('Ctrl Pts',(-31.1752418181714,54.37628365121,2.8135463472091));
#232878=CARTESIAN_POINT('Ctrl Pts',(-31.168935299717,54.3671795569364,2.82378004208997));
#232879=CARTESIAN_POINT('Ctrl Pts',(-31.1634057161443,54.3576020372439,
2.83404198860299));
#232880=CARTESIAN_POINT('Ctrl Pts',(-29.4433108116264,51.3783102687785,
2.83404198860296));
#232881=CARTESIAN_POINT('Ctrl Pts',(-29.4380189697941,51.3691445298594,
2.82422126443104));
#232882=CARTESIAN_POINT('Ctrl Pts',(-29.4334690915859,51.3595943606121,
2.81442815028661));
#232883=CARTESIAN_POINT('Ctrl Pts',(-29.4296781246256,51.349715286878,2.8047161816654));
#232884=CARTESIAN_POINT('Ctrl Pts',(-29.4260176124813,51.3401761719884,
2.79533842146481));
#232885=CARTESIAN_POINT('Ctrl Pts',(-29.4230642997983,51.3303291924932,
2.7860351565052));
#232886=CARTESIAN_POINT('Ctrl Pts',(-29.4208754038589,51.3202058500908,
2.77685887347063));
#232887=CARTESIAN_POINT('Ctrl Pts',(-29.4188062116764,51.3106361210858,
2.76818441216884));
#232888=CARTESIAN_POINT('Ctrl Pts',(-29.4174199248365,51.3008185461803,
2.75962261521931));
#232889=CARTESIAN_POINT('Ctrl Pts',(-29.4168067767635,51.2907775289361,
2.75123537701965));
#232890=CARTESIAN_POINT('Ctrl Pts',(-29.4162420776746,51.2815299205047,
2.74351087134404));
#232891=CARTESIAN_POINT('Ctrl Pts',(-29.4163331870167,51.2720922400945,
2.73593399450111));
#232892=CARTESIAN_POINT('Ctrl Pts',(-29.4171879526243,51.2624911797745,
2.7285765781282));
#232893=CARTESIAN_POINT('Ctrl Pts',(-29.417442826474,51.2596283373971,2.72638274508491));
#232894=CARTESIAN_POINT('Ctrl Pts',(-29.4177658668979,51.2567510524878,
2.72420861709695));
#232895=CARTESIAN_POINT('Ctrl Pts',(-29.4181606517644,51.2538602864394,
2.72205663736742));
#232896=CARTESIAN_POINT('Ctrl Pts',(-29.4185514029024,51.2509990568967,
2.71992664556781));
#232897=CARTESIAN_POINT('Ctrl Pts',(-29.4190117629203,51.2481275521819,
2.717820899279));
#232898=CARTESIAN_POINT('Ctrl Pts',(-29.4195444402101,51.245249939194,2.71574387311261));
#232899=CARTESIAN_POINT('Ctrl Pts',(-29.4195814815471,51.2450498356146,
2.71559944077502));
#232900=CARTESIAN_POINT('Ctrl Pts',(-29.4196188630963,51.2448496951984,
2.71545515216085));
#232901=CARTESIAN_POINT('Ctrl Pts',(-29.4196565860788,51.2446495184043,
2.71531100781746));
#232902=CARTESIAN_POINT('Ctrl Pts',(-29.4213104998203,51.235873034447,2.70899119176089));
#232903=CARTESIAN_POINT('Ctrl Pts',(-29.4236619033166,51.2270453415807,
2.70298296066835));
#232904=CARTESIAN_POINT('Ctrl Pts',(-29.4267651248011,51.2182691329811,
2.69736727774125));
#232905=CARTESIAN_POINT('Ctrl Pts',(-29.429657866561,51.2100881812714,2.69213248525397));
#232906=CARTESIAN_POINT('Ctrl Pts',(-29.4332044080285,51.2019513265382,
2.68723866185419));
#232907=CARTESIAN_POINT('Ctrl Pts',(-29.4374658604808,51.1939656059606,
2.682785958295));
#232908=CARTESIAN_POINT('Ctrl Pts',(-29.4390247549189,51.1910443260608,
2.6811571017277));
#232909=CARTESIAN_POINT('Ctrl Pts',(-29.4406794572091,51.1881435589218,
2.679587636378));
#232910=CARTESIAN_POINT('Ctrl Pts',(-29.4424334077169,51.1852696776794,
2.67808378645378));
#232911=CARTESIAN_POINT('Ctrl Pts',(-29.4428551742198,51.1845786052484,
2.67772216078613));
#232912=CARTESIAN_POINT('Ctrl Pts',(-29.443283215379,51.1838888551096,2.67736403603576));
#232913=CARTESIAN_POINT('Ctrl Pts',(-29.4437175198435,51.1832005624689,
2.67700956934492));
#232914=CARTESIAN_POINT('Ctrl Pts',(-29.4441382522935,51.1825337789733,
2.67666617973817));
#232915=CARTESIAN_POINT('Ctrl Pts',(-29.4445648626867,51.1818683633173,
2.67632622314131));
#232916=CARTESIAN_POINT('Ctrl Pts',(-29.4449973374098,51.1812044402994,
2.67598984158786));
#232917=CARTESIAN_POINT('Ctrl Pts',(-29.4497355978001,51.17393039636,2.67230439292256));
#232918=CARTESIAN_POINT('Ctrl Pts',(-29.4551812510948,51.1668309650368,
2.66904964540027));
#232919=CARTESIAN_POINT('Ctrl Pts',(-29.4612929974509,51.1600900711827,
2.66640203566786));
#232920=CARTESIAN_POINT('Ctrl Pts',(-29.4638277208368,51.1572944215763,
2.66530399299482));
#232921=CARTESIAN_POINT('Ctrl Pts',(-29.4664765899952,51.1545603804843,
2.66430995142285));
#232922=CARTESIAN_POINT('Ctrl Pts',(-29.4692349685474,51.1519003687091,
2.66343053473373));
#232923=CARTESIAN_POINT('Ctrl Pts',(-29.4739396706108,51.1473634414342,
2.66193059792897));
#232924=CARTESIAN_POINT('Ctrl Pts',(-29.4789629373384,51.1430443628985,
2.6607651981714));
#232925=CARTESIAN_POINT('Ctrl Pts',(-29.4842777732943,51.1390107214368,
2.65997805604472));
#232926=CARTESIAN_POINT('Ctrl Pts',(-29.4869351912723,51.1369939007059,
2.65958448498138));
#232927=CARTESIAN_POINT('Ctrl Pts',(-29.4896662827385,51.1350496570629,
2.65928526260775));
#232928=CARTESIAN_POINT('Ctrl Pts',(-29.4924676612913,51.133186503688,2.65908463971337));
#232929=CARTESIAN_POINT('Ctrl Pts',(-29.4952690398441,51.1313233503131,
2.65888401681899));
#232930=CARTESIAN_POINT('Ctrl Pts',(-29.49814066024,51.1295412933646,2.65878198860297));
#232931=CARTESIAN_POINT('Ctrl Pts',(-29.5010785149114,51.1278468659047,
2.65878198860297));
#232932=CARTESIAN_POINT('Origin',(-34.2589154226524,47.1274239660509,2.83404198860294));
#232933=CARTESIAN_POINT('Ctrl Pts',(-36.9828414016749,50.5784163149357,
2.83404198860297));
#232934=CARTESIAN_POINT('Ctrl Pts',(-36.989077996891,50.5870002518364,2.82419652440097));
#232935=CARTESIAN_POINT('Ctrl Pts',(-36.99461878582,50.5960508068001,2.81438790575681));
#232936=CARTESIAN_POINT('Ctrl Pts',(-36.9994424783905,50.6055128591422,
2.80466781256934));
#232937=CARTESIAN_POINT('Ctrl Pts',(-37.0041094296756,50.6146674511261,
2.79526356453112));
#232938=CARTESIAN_POINT('Ctrl Pts',(-37.0081056536707,50.6242084112814,
2.78594102496269));
#232939=CARTESIAN_POINT('Ctrl Pts',(-37.0113722741995,50.6341096134636,
2.77675109088818));
#232940=CARTESIAN_POINT('Ctrl Pts',(-37.0144622960728,50.6434755410471,
2.76805797913724));
#232941=CARTESIAN_POINT('Ctrl Pts',(-37.0168997626765,50.6531646927634,
2.75948271210207));
#232942=CARTESIAN_POINT('Ctrl Pts',(-37.0185933530511,50.663162158124,2.75108575573272));
#232943=CARTESIAN_POINT('Ctrl Pts',(-37.0201532722696,50.6723705467562,
2.74335155163321));
#232944=CARTESIAN_POINT('Ctrl Pts',(-37.0210821446113,50.681841060773,2.73576818685996));
#232945=CARTESIAN_POINT('Ctrl Pts',(-37.0212705108777,50.691558667865,2.72840626160552));
#232946=CARTESIAN_POINT('Ctrl Pts',(-37.0213251487713,50.6943773762881,
2.72627084693727));
#232947=CARTESIAN_POINT('Ctrl Pts',(-37.0213172191968,50.6972168227826,
2.72415424587563));
#232948=CARTESIAN_POINT('Ctrl Pts',(-37.0212433695026,50.7000764815586,
2.72205867173291));
#232949=CARTESIAN_POINT('Ctrl Pts',(-37.0211633116861,50.7031765355314,
2.71978693462894));
#232950=CARTESIAN_POINT('Ctrl Pts',(-37.0210069737843,50.7062960577322,
2.71754411340795));
#232951=CARTESIAN_POINT('Ctrl Pts',(-37.0207706534748,50.7094335311104,
2.71533341844292));
#232952=CARTESIAN_POINT('Ctrl Pts',(-37.0201220705311,50.718044351416,2.70926614876439));
#232953=CARTESIAN_POINT('Ctrl Pts',(-37.0188289150183,50.7267761502173,
2.70347381860456));
#232954=CARTESIAN_POINT('Ctrl Pts',(-37.0168522507833,50.735532807949,2.69804914171442));
#232955=CARTESIAN_POINT('Ctrl Pts',(-37.015043710324,50.7435446743633,2.69308585687257));
#232956=CARTESIAN_POINT('Ctrl Pts',(-37.0126559296151,50.7515681793719,
2.68842799053243));
#232957=CARTESIAN_POINT('Ctrl Pts',(-37.0096268558218,50.7595400218647,
2.68414767054279));
#232958=CARTESIAN_POINT('Ctrl Pts',(-37.0081389846695,50.7634557648562,
2.68204519134608));
#232959=CARTESIAN_POINT('Ctrl Pts',(-37.0064960060561,50.7673587034239,
2.68003431778554));
#232960=CARTESIAN_POINT('Ctrl Pts',(-37.0046883717069,50.771238806215,2.678126939453));
#232961=CARTESIAN_POINT('Ctrl Pts',(-37.0043453906958,50.7719750179269,
2.67776503299252));
#232962=CARTESIAN_POINT('Ctrl Pts',(-37.0039959853417,50.7727105984664,
2.67740659639972));
#232963=CARTESIAN_POINT('Ctrl Pts',(-37.0036401497476,50.7734454079409,
2.67705178968904));
#232964=CARTESIAN_POINT('Ctrl Pts',(-37.0032954340158,50.7741572546194,
2.67670807068806));
#232965=CARTESIAN_POINT('Ctrl Pts',(-37.0029446836755,50.7748683776572,
2.67636775825313));
#232966=CARTESIAN_POINT('Ctrl Pts',(-37.0025878964871,50.7755786476302,
2.67603099699303));
#232967=CARTESIAN_POINT('Ctrl Pts',(-36.9986997032254,50.7833190234416,
2.6723610421717));
#232968=CARTESIAN_POINT('Ctrl Pts',(-36.9940916451526,50.7909629993146,
2.6691144054151));
#232969=CARTESIAN_POINT('Ctrl Pts',(-36.9887818345681,50.7983209798302,
2.66646778189665));
#232970=CARTESIAN_POINT('Ctrl Pts',(-36.9865394685861,50.8014283006926,
2.66535009635014));
#232971=CARTESIAN_POINT('Ctrl Pts',(-36.9841723869924,50.8044846273291,
2.66433897912389));
#232972=CARTESIAN_POINT('Ctrl Pts',(-36.9816838130236,50.807476228564,2.66344564884841));
#232973=CARTESIAN_POINT('Ctrl Pts',(-36.9774931166428,50.8125140102919,
2.66194130298634));
#232974=CARTESIAN_POINT('Ctrl Pts',(-36.9729576356984,50.8173657273503,
2.66077206705468));
#232975=CARTESIAN_POINT('Ctrl Pts',(-36.9680961762159,50.8219595855753,
2.65998225155762));
#232976=CARTESIAN_POINT('Ctrl Pts',(-36.9668808113453,50.8231080501316,
2.65978479768336));
#232977=CARTESIAN_POINT('Ctrl Pts',(-36.9656449236015,50.8242402182967,
2.6596109896667));
#232978=CARTESIAN_POINT('Ctrl Pts',(-36.9643886196686,50.8253547230715,
2.65946139030549));
#232979=CARTESIAN_POINT('Ctrl Pts',(-36.9625041637694,50.8270264802337,
2.65923699126368));
#232980=CARTESIAN_POINT('Ctrl Pts',(-36.9605737761781,50.8286584747058,
2.65906707562489));
#232981=CARTESIAN_POINT('Ctrl Pts',(-36.9585988181541,50.8302474395916,
2.65895332562967));
#232982=CARTESIAN_POINT('Ctrl Pts',(-36.9566238601301,50.8318364044774,
2.65883957563445));
#232983=CARTESIAN_POINT('Ctrl Pts',(-36.9546043428184,50.8333823430136,
2.65878198860296));
#232984=CARTESIAN_POINT('Ctrl Pts',(-36.9525415975215,50.8348823336486,
2.65878198860296));
#232985=CARTESIAN_POINT('Ctrl Pts',(-34.7084426211234,47.7461450747865,
2.65878198860294));
#232986=CARTESIAN_POINT('Ctrl Pts',(-34.7154221779232,47.7410693801617,
2.65878198860294));
#232987=CARTESIAN_POINT('Ctrl Pts',(-34.7227602152549,47.7366138137626,
2.65945335517896));
#232988=CARTESIAN_POINT('Ctrl Pts',(-34.7303057514058,47.732784625124,2.66072561226656));
#232989=CARTESIAN_POINT('Ctrl Pts',(-34.7351793935418,47.7303113621614,
2.66154735980391));
#232990=CARTESIAN_POINT('Ctrl Pts',(-34.7401391868075,47.7280985748135,
2.66261895766927));
#232991=CARTESIAN_POINT('Ctrl Pts',(-34.7451421370596,47.7261394006519,
2.66391429251058));
#232992=CARTESIAN_POINT('Ctrl Pts',(-34.7517732610326,47.7235426275289,
2.66563118464155));
#232993=CARTESIAN_POINT('Ctrl Pts',(-34.7584811778433,47.721397116118,2.6677410513873));
#232994=CARTESIAN_POINT('Ctrl Pts',(-34.7651763312118,47.7196932909346,
2.67016894181781));
#232995=CARTESIAN_POINT('Ctrl Pts',(-34.768523907896,47.7188413783428,2.67138288703307));
#232996=CARTESIAN_POINT('Ctrl Pts',(-34.7718684539193,47.7180997687562,
2.67267613167583));
#232997=CARTESIAN_POINT('Ctrl Pts',(-34.7751999143434,47.717466427977,2.67403835432585));
#232998=CARTESIAN_POINT('Ctrl Pts',(-34.7768656445554,47.7171497575874,
2.67471946565086));
#232999=CARTESIAN_POINT('Ctrl Pts',(-34.7785281166319,47.7168601447021,
2.67541781389555));
#233000=CARTESIAN_POINT('Ctrl Pts',(-34.7801861569091,47.7165972740598,
2.67613207244201));
#233001=CARTESIAN_POINT('Ctrl Pts',(-34.7806006669785,47.7165315563992,
2.67631063707863));
#233002=CARTESIAN_POINT('Ctrl Pts',(-34.7810149003418,47.7164675099217,
2.67649019601877));
#233003=CARTESIAN_POINT('Ctrl Pts',(-34.7814288392283,47.7164051292834,
2.67667072836689));
#233004=CARTESIAN_POINT('Ctrl Pts',(-34.7826706558876,47.7162179873685,
2.67721232541123));
#233005=CARTESIAN_POINT('Ctrl Pts',(-34.783909820854,47.7160458390455,2.67776268340079));
#233006=CARTESIAN_POINT('Ctrl Pts',(-34.7851458668348,47.7158885307489,
2.67832123541548));
#233007=CARTESIAN_POINT('Ctrl Pts',(-34.7938524151213,47.7147804714199,
2.68225560368478));
#233008=CARTESIAN_POINT('Ctrl Pts',(-34.8024290252886,47.7143609747538,
2.68661792998924));
#233009=CARTESIAN_POINT('Ctrl Pts',(-34.8108122146621,47.7145286167447,
2.69130986622615));
#233010=CARTESIAN_POINT('Ctrl Pts',(-34.8148780524493,47.7146099229291,
2.6935854502309));
#233011=CARTESIAN_POINT('Ctrl Pts',(-34.818898766793,47.714829779504,2.69593918853504));
#233012=CARTESIAN_POINT('Ctrl Pts',(-34.8228686918041,47.715179003921,2.69836306235508));
#233013=CARTESIAN_POINT('Ctrl Pts',(-34.8289463696254,47.7157136421038,
2.70207384382241));
#233014=CARTESIAN_POINT('Ctrl Pts',(-34.8349017567798,47.7165501157952,
2.70594760814241));
#233015=CARTESIAN_POINT('Ctrl Pts',(-34.8407017446569,47.7176563296782,
2.70995196345721));
#233016=CARTESIAN_POINT('Ctrl Pts',(-34.8433952890323,47.7181700611283,
2.71181160678119));
#233017=CARTESIAN_POINT('Ctrl Pts',(-34.846055281772,47.7187417155522,2.71369962772112));
#233018=CARTESIAN_POINT('Ctrl Pts',(-34.8486779186779,47.7193692101071,
2.71561183138674));
#233019=CARTESIAN_POINT('Ctrl Pts',(-34.848878933463,47.7194173050923,2.71575839426325));
#233020=CARTESIAN_POINT('Ctrl Pts',(-34.8490797487414,47.7194657006757,
2.71590508903222));
#233021=CARTESIAN_POINT('Ctrl Pts',(-34.849280363866,47.719514395548,2.71605191409925));
#233022=CARTESIAN_POINT('Ctrl Pts',(-34.8520984015308,47.7201984116934,
2.71811436362766));
#233023=CARTESIAN_POINT('Ctrl Pts',(-34.8548765847938,47.7209435418727,
2.72020091026972));
#233024=CARTESIAN_POINT('Ctrl Pts',(-34.8576119849587,47.7217448891703,
2.72230624862195));
#233025=CARTESIAN_POINT('Ctrl Pts',(-34.8674206434757,47.7246183780647,
2.72985561753111));
#233026=CARTESIAN_POINT('Ctrl Pts',(-34.8767555719419,47.7282350429867,
2.73770089914333));
#233027=CARTESIAN_POINT('Ctrl Pts',(-34.88562315656,47.7324659181295,2.74574823347071));
#233028=CARTESIAN_POINT('Ctrl Pts',(-34.8953677412274,47.7371152248823,
2.75459144547016));
#233029=CARTESIAN_POINT('Ctrl Pts',(-34.9045486251,47.7425063743634,2.76367911754256));
#233030=CARTESIAN_POINT('Ctrl Pts',(-34.9131661493089,47.7485205638412,
2.77292162564708));
#233031=CARTESIAN_POINT('Ctrl Pts',(-34.9224709127513,47.7550143791218,
2.78290121484722));
#233032=CARTESIAN_POINT('Ctrl Pts',(-34.9311199164039,47.7622350952179,
2.7930622950019));
#233033=CARTESIAN_POINT('Ctrl Pts',(-34.9390908738055,47.7700859103008,
2.80331916685266));
#233034=CARTESIAN_POINT('Ctrl Pts',(-34.9469949630644,47.7778708651116,
2.81348999408713));
#233035=CARTESIAN_POINT('Ctrl Pts',(-34.9542331399579,47.78627657979,2.82375635966901));
#233036=CARTESIAN_POINT('Ctrl Pts',(-34.9607485668368,47.7952442955502,
2.83404198860294));
#233037=CARTESIAN_POINT('Origin',(0.0123294189942831,0.00895784724512226,
2.83404198860262));
#233038=CARTESIAN_POINT('Ctrl Pts',(-36.9278827595329,50.8527980281385,
2.65878198860296));
#233039=CARTESIAN_POINT('Ctrl Pts',(-36.9209320551072,50.8578435704956,
2.65878198860297));
#233040=CARTESIAN_POINT('Ctrl Pts',(-36.9136216385509,50.8622636476106,
2.6594460304188));
#233041=CARTESIAN_POINT('Ctrl Pts',(-36.9061023515955,50.8660552387515,
2.66070439264092));
#233042=CARTESIAN_POINT('Ctrl Pts',(-36.9012978851887,50.8684778849908,
2.66150842619618));
#233043=CARTESIAN_POINT('Ctrl Pts',(-36.8964085464701,50.8706447895124,
2.66255428265394));
#233044=CARTESIAN_POINT('Ctrl Pts',(-36.8914758894168,50.8725634718547,
2.66381699700687));
#233045=CARTESIAN_POINT('Ctrl Pts',(-36.8847438022849,50.8751820882651,
2.66554034873287));
#233046=CARTESIAN_POINT('Ctrl Pts',(-36.8779301449085,50.8773323251415,
2.66766759643992));
#233047=CARTESIAN_POINT('Ctrl Pts',(-36.8711298300324,50.8790261328805,
2.67012012783168));
#233048=CARTESIAN_POINT('Ctrl Pts',(-36.8677296725943,50.8798730367501,
2.67134639352755));
#233049=CARTESIAN_POINT('Ctrl Pts',(-36.8643326829601,50.8806059576337,
2.67265375585032));
#233050=CARTESIAN_POINT('Ctrl Pts',(-36.8609495224154,50.8812272732515,
2.6740313512696));
#233051=CARTESIAN_POINT('Ctrl Pts',(-36.859257942143,50.8815379310604,2.67472014897924));
#233052=CARTESIAN_POINT('Ctrl Pts',(-36.8575698050848,50.8818206978293,
2.67542649668652));
#233053=CARTESIAN_POINT('Ctrl Pts',(-36.855886355634,50.8820759354569,2.67614899656121));
#233054=CARTESIAN_POINT('Ctrl Pts',(-36.8554654932713,50.8821397448637,
2.67632962152989));
#233055=CARTESIAN_POINT('Ctrl Pts',(-36.8550449235851,50.882201833919,2.6765112559097));
#233056=CARTESIAN_POINT('Ctrl Pts',(-36.8546246654168,50.8822622087211,
2.67669387767543));
#233057=CARTESIAN_POINT('Ctrl Pts',(-36.8533638909116,50.8824433331273,
2.67724174297264));
#233058=CARTESIAN_POINT('Ctrl Pts',(-36.8521059215534,50.8826090281506,
2.67779849504767));
#233059=CARTESIAN_POINT('Ctrl Pts',(-36.8508512527542,50.8827594682968,
2.67836353618029));
#233060=CARTESIAN_POINT('Ctrl Pts',(-36.8421807128859,50.8837991030488,
2.68226832098931));
#233061=CARTESIAN_POINT('Ctrl Pts',(-36.8336410897272,50.8841591194361,
2.68659153751419));
#233062=CARTESIAN_POINT('Ctrl Pts',(-36.8252931160718,50.8839416093727,
2.69123699486211));
#233063=CARTESIAN_POINT('Ctrl Pts',(-36.8211441960798,50.8838335074683,
2.69354577441245));
#233064=CARTESIAN_POINT('Ctrl Pts',(-36.817042229914,50.8835822787328,2.69593478828141));
#233065=CARTESIAN_POINT('Ctrl Pts',(-36.8129929908132,50.8831977843867,
2.69839565261238));
#233066=CARTESIAN_POINT('Ctrl Pts',(-36.8040597645471,50.8823495324296,
2.70382468689064));
#233067=CARTESIAN_POINT('Ctrl Pts',(-36.7953829494618,50.8808651175413,
2.70961155815105));
#233068=CARTESIAN_POINT('Ctrl Pts',(-36.7870848098364,50.8788231440731,
2.71562701361785));
#233069=CARTESIAN_POINT('Ctrl Pts',(-36.7840533947862,50.8780771854145,
2.71782453535875));
#233070=CARTESIAN_POINT('Ctrl Pts',(-36.7810676701179,50.8772631333236,
2.72005051502419));
#233071=CARTESIAN_POINT('Ctrl Pts',(-36.7781294934921,50.8763859670026,
2.72229986760131));
#233072=CARTESIAN_POINT('Ctrl Pts',(-36.7682604691134,50.873439658149,2.72985520488929));
#233073=CARTESIAN_POINT('Ctrl Pts',(-36.7588677364065,50.8697545265635,
2.73770845534619));
#233074=CARTESIAN_POINT('Ctrl Pts',(-36.7499455893901,50.8654587487958,
2.7457670670184));
#233075=CARTESIAN_POINT('Ctrl Pts',(-36.7401390929213,50.8607371801608,
2.75462443585143));
#233076=CARTESIAN_POINT('Ctrl Pts',(-36.7309004184129,50.8552777667765,
2.76373036323325));
#233077=CARTESIAN_POINT('Ctrl Pts',(-36.7222305213302,50.8491983060104,
2.77299664636993));
#233078=CARTESIAN_POINT('Ctrl Pts',(-36.7128926706964,50.8426504662811,
2.78297683033686));
#233079=CARTESIAN_POINT('Ctrl Pts',(-36.7042135591824,50.8353827952087,
2.79314401479143));
#233080=CARTESIAN_POINT('Ctrl Pts',(-36.696217769428,50.8274903908639,2.80341452428226));
#233081=CARTESIAN_POINT('Ctrl Pts',(-36.6883299498338,50.8197045606271,
2.81354634721565));
#233082=CARTESIAN_POINT('Ctrl Pts',(-36.6811063421663,50.81130955022,2.82378004209319));
#233083=CARTESIAN_POINT('Ctrl Pts',(-36.674605926818,50.8023624960591,2.83404198860297));
#233084=CARTESIAN_POINT('Ctrl Pts',(-34.6525130919799,48.0191904766737,
2.83404198860294));
#233085=CARTESIAN_POINT('Ctrl Pts',(-34.6462921588072,48.0106280967263,
2.82422126443143));
#233086=CARTESIAN_POINT('Ctrl Pts',(-34.6407689407928,48.0016058360829,
2.81442815028741));
#233087=CARTESIAN_POINT('Ctrl Pts',(-34.6359660967503,47.9921771448995,
2.80471618166661));
#233088=CARTESIAN_POINT('Ctrl Pts',(-34.6313285282544,47.9830729139888,
2.79533842146634));
#233089=CARTESIAN_POINT('Ctrl Pts',(-34.6273621044929,47.9735885825143,
2.78603515650706));
#233090=CARTESIAN_POINT('Ctrl Pts',(-34.62412702213,47.9637494987701,2.77685887347279));
#233091=CARTESIAN_POINT('Ctrl Pts',(-34.621068856132,47.9544484832213,2.7681844121713));
#233092=CARTESIAN_POINT('Ctrl Pts',(-34.6186639474985,47.9448295964517,
2.75962261522204));
#233093=CARTESIAN_POINT('Ctrl Pts',(-34.6170045862125,47.9349076763769,
2.75123537702263));
#233094=CARTESIAN_POINT('Ctrl Pts',(-34.615476342306,47.9257697544405,2.7435108713473));
#233095=CARTESIAN_POINT('Ctrl Pts',(-34.6145804463113,47.9163742511121,
2.73593399450464));
#233096=CARTESIAN_POINT('Ctrl Pts',(-34.6144269453422,47.9067364390701,
2.72857657813196));
#233097=CARTESIAN_POINT('Ctrl Pts',(-34.6143811744519,47.9038626380693,
2.72638274508739));
#233098=CARTESIAN_POINT('Ctrl Pts',(-34.6144016870566,47.9009673483071,
2.72420861709817));
#233099=CARTESIAN_POINT('Ctrl Pts',(-34.6144921419176,47.8980511519206,
2.72205663736741));
#233100=CARTESIAN_POINT('Ctrl Pts',(-34.6145816725529,47.8951647518767,
2.7199266455678));
#233101=CARTESIAN_POINT('Ctrl Pts',(-34.6147393566953,47.8922608568399,
2.71782089927899));
#233102=CARTESIAN_POINT('Ctrl Pts',(-34.6149683234597,47.8893433277786,
2.71574387311261));
#233103=CARTESIAN_POINT('Ctrl Pts',(-34.6149842453607,47.8891404485134,
2.71559944077501));
#233104=CARTESIAN_POINT('Ctrl Pts',(-34.6150005017597,47.8889374970515,
2.71545515216083));
#233105=CARTESIAN_POINT('Ctrl Pts',(-34.6150170939191,47.8887344737214,
2.71531100781743));
#233106=CARTESIAN_POINT('Ctrl Pts',(-34.6157445549672,47.8798331871998,
2.70899119176089));
#233107=CARTESIAN_POINT('Ctrl Pts',(-34.6171603320595,47.8708080647646,
2.70298296066838));
#233108=CARTESIAN_POINT('Ctrl Pts',(-34.6193291901738,47.8617555581811,
2.69736727774131));
#233109=CARTESIAN_POINT('Ctrl Pts',(-34.6213509428814,47.85331704873,2.69213248525403));
#233110=CARTESIAN_POINT('Ctrl Pts',(-34.6240275231026,47.8448540540089,
2.68723866185425));
#233111=CARTESIAN_POINT('Ctrl Pts',(-34.6274308957724,47.8364666369681,
2.68278595829506));
#233112=CARTESIAN_POINT('Ctrl Pts',(-34.628675893525,47.8333984113051,2.68115710172776));
#233113=CARTESIAN_POINT('Ctrl Pts',(-34.6300183184515,47.8303405713845,
2.67958763637807));
#233114=CARTESIAN_POINT('Ctrl Pts',(-34.6314622582451,47.827299095813,2.67808378645385));
#233115=CARTESIAN_POINT('Ctrl Pts',(-34.6318094775277,47.8265677225447,
2.6777221607862));
#233116=CARTESIAN_POINT('Ctrl Pts',(-34.6321630753106,47.8258370084447,
2.67736403603583));
#233117=CARTESIAN_POINT('Ctrl Pts',(-34.6325230544378,47.8251070891649,
2.67700956934499));
#233118=CARTESIAN_POINT('Ctrl Pts',(-34.6328717842173,47.8243999798626,
2.67666617973824));
#233119=CARTESIAN_POINT('Ctrl Pts',(-34.6332265027182,47.8236936164944,
2.67632622314139));
#233120=CARTESIAN_POINT('Ctrl Pts',(-34.6335872094466,47.822988124598,2.67598984158793));
#233121=CARTESIAN_POINT('Ctrl Pts',(-34.6375391685163,47.8152586455548,
2.67230439292241));
#233122=CARTESIAN_POINT('Ctrl Pts',(-34.6422128973065,47.8076288798884,
2.66904964539994));
#233123=CARTESIAN_POINT('Ctrl Pts',(-34.6475865476013,47.8002860619011,
2.66640203566743));
#233124=CARTESIAN_POINT('Ctrl Pts',(-34.6498151605499,47.7972407764159,
2.66530399299458));
#233125=CARTESIAN_POINT('Ctrl Pts',(-34.6521637338116,47.7942448304651,
2.66430995142276));
#233126=CARTESIAN_POINT('Ctrl Pts',(-34.654628954734,47.7913110614419,2.66343053473377));
#233127=CARTESIAN_POINT('Ctrl Pts',(-34.6588336459112,47.7863072126526,
2.661930597929));
#233128=CARTESIAN_POINT('Ctrl Pts',(-34.6633779280161,47.7814867201294,
2.66076519817141));
#233129=CARTESIAN_POINT('Ctrl Pts',(-34.6682420184012,47.7769196237427,
2.65997805604472));
#233130=CARTESIAN_POINT('Ctrl Pts',(-34.6706740635937,47.7746360755494,
2.65958448498137));
#233131=CARTESIAN_POINT('Ctrl Pts',(-34.6731869650549,47.7724170058824,
2.65928526260773));
#233132=CARTESIAN_POINT('Ctrl Pts',(-34.6757782448038,47.7702712352615,
2.65908463971335));
#233133=CARTESIAN_POINT('Ctrl Pts',(-34.6783695245527,47.7681254646406,
2.65888401681897));
#233134=CARTESIAN_POINT('Ctrl Pts',(-34.6810391382372,47.7660530039194,
2.65878198860294));
#233135=CARTESIAN_POINT('Ctrl Pts',(-34.6837837831348,47.7640607692763,
2.65878198860294));
#233136=CARTESIAN_POINT('Origin',(-38.9973987043321,43.2882232241948,2.83404198860291));
#233137=CARTESIAN_POINT('Ctrl Pts',(-42.0671296588098,46.435582879267,2.83404198860294));
#233138=CARTESIAN_POINT('Ctrl Pts',(-42.0742293550376,46.443467890749,2.82419652440176));
#233139=CARTESIAN_POINT('Ctrl Pts',(-42.0806858315469,46.4518896956732,
2.81438790575831));
#233140=CARTESIAN_POINT('Ctrl Pts',(-42.0864721532152,46.4607957007304,
2.80466781257148));
#233141=CARTESIAN_POINT('Ctrl Pts',(-42.0920704538847,46.4694123136551,
2.79526356453374));
#233142=CARTESIAN_POINT('Ctrl Pts',(-42.0970420880496,46.4784832882788,
2.78594102496572));
#233143=CARTESIAN_POINT('Ctrl Pts',(-42.1013257711378,46.487988795815,2.77675109089158));
#233144=CARTESIAN_POINT('Ctrl Pts',(-42.1053778715653,46.4969804206287,
2.76805797914095));
#233145=CARTESIAN_POINT('Ctrl Pts',(-42.1088147776111,46.5063617095192,
2.75948271210603));
#233146=CARTESIAN_POINT('Ctrl Pts',(-42.1115441100112,46.5161273793187,
2.75108575573691));
#233147=CARTESIAN_POINT('Ctrl Pts',(-42.114058022542,46.5251222674751,2.74335155163766));
#233148=CARTESIAN_POINT('Ctrl Pts',(-42.1159717447004,46.5344438074261,
2.73576818686464));
#233149=CARTESIAN_POINT('Ctrl Pts',(-42.1171748456129,46.5440884908126,
2.72840626161042));
#233150=CARTESIAN_POINT('Ctrl Pts',(-42.1175238194546,46.5468860468431,
2.72627084694051));
#233151=CARTESIAN_POINT('Ctrl Pts',(-42.117812736298,46.5497107674209,2.72415424587722));
#233152=CARTESIAN_POINT('Ctrl Pts',(-42.1180382068977,46.5525624800842,
2.7220586717329));
#233153=CARTESIAN_POINT('Ctrl Pts',(-42.118282631524,46.5556539199574,2.71978693462893));
#233154=CARTESIAN_POINT('Ctrl Pts',(-42.1184532289195,46.5587726948499,
2.71754411340793));
#233155=CARTESIAN_POINT('Ctrl Pts',(-42.1185461584681,46.5619176830194,
2.7153334184429));
#233156=CARTESIAN_POINT('Ctrl Pts',(-42.1188012043436,46.5705491277289,
2.70926614876438));
#233157=CARTESIAN_POINT('Ctrl Pts',(-42.1184278543823,46.5793682643812,
2.70347381860455));
#233158=CARTESIAN_POINT('Ctrl Pts',(-42.1173773384969,46.5882835699004,
2.69804914171441));
#233159=CARTESIAN_POINT('Ctrl Pts',(-42.1164161734955,46.5964405904275,
2.6930858568724));
#233160=CARTESIAN_POINT('Ctrl Pts',(-42.1148801579477,46.6046697328845,
2.68842799053211));
#233161=CARTESIAN_POINT('Ctrl Pts',(-42.1127009621827,46.6129145292191,
2.68414767054235));
#233162=CARTESIAN_POINT('Ctrl Pts',(-42.1116305483417,46.6169643462456,
2.6820451913458));
#233163=CARTESIAN_POINT('Ctrl Pts',(-42.1104045383079,46.6210176421368,
2.68003431778541));
#233164=CARTESIAN_POINT('Ctrl Pts',(-42.1090123875509,46.6250654385593,
2.678126939453));
#233165=CARTESIAN_POINT('Ctrl Pts',(-42.1087482405045,46.6258334685044,
2.67776503299252));
#233166=CARTESIAN_POINT('Ctrl Pts',(-42.108477638333,46.6266015422614,2.67740659639973));
#233167=CARTESIAN_POINT('Ctrl Pts',(-42.1082005605487,46.6273695213206,
2.67705178968904));
#233168=CARTESIAN_POINT('Ctrl Pts',(-42.1079321414451,46.6281135010342,
2.67670807068807));
#233169=CARTESIAN_POINT('Ctrl Pts',(-42.1076576451502,46.6288573918597,
2.67636775825315));
#233170=CARTESIAN_POINT('Ctrl Pts',(-42.1073770559081,46.629601065316,2.67603099699304));
#233171=CARTESIAN_POINT('Ctrl Pts',(-42.1043192521646,46.6377054654054,
2.6723610421717));
#233172=CARTESIAN_POINT('Ctrl Pts',(-42.1005354505673,46.6457892400076,
2.6691144054151));
#233173=CARTESIAN_POINT('Ctrl Pts',(-42.0960238460768,46.6536619390768,
2.66646778189663));
#233174=CARTESIAN_POINT('Ctrl Pts',(-42.0941185674849,46.6569866287806,
2.66535009635013));
#233175=CARTESIAN_POINT('Ctrl Pts',(-42.0920839261384,46.6602736399414,
2.66433897912388));
#233176=CARTESIAN_POINT('Ctrl Pts',(-42.089921692318,46.6635089796844,2.66344564884841));
#233177=CARTESIAN_POINT('Ctrl Pts',(-42.0862805445927,46.6689572109695,
2.66194130298633));
#233178=CARTESIAN_POINT('Ctrl Pts',(-42.0822770520158,46.6742564366676,
2.66077206705466));
#233179=CARTESIAN_POINT('Ctrl Pts',(-42.0779224130575,46.6793332901452,
2.6599822515576));
#233180=CARTESIAN_POINT('Ctrl Pts',(-42.0768337533179,46.6806025035146,
2.65978479768333));
#233181=CARTESIAN_POINT('Ctrl Pts',(-42.0757229796949,46.6818576549907,
2.65961098966667));
#233182=CARTESIAN_POINT('Ctrl Pts',(-42.0745900553979,46.6830973739112,
2.65946139030547));
#233183=CARTESIAN_POINT('Ctrl Pts',(-42.0728906689524,46.6849569522921,
2.65923699126365));
#233184=CARTESIAN_POINT('Ctrl Pts',(-42.0711414461006,46.6867817869761,
2.65906707562487));
#233185=CARTESIAN_POINT('Ctrl Pts',(-42.0693433991611,46.6885684866734,
2.65895332562964));
#233186=CARTESIAN_POINT('Ctrl Pts',(-42.0675453522216,46.6903551863706,
2.65883957563442));
#233187=CARTESIAN_POINT('Ctrl Pts',(-42.0656984926167,46.692103753135,2.65878198860294));
#233188=CARTESIAN_POINT('Ctrl Pts',(-42.0638038389703,46.6938111422604,
2.65878198860294));
#233189=CARTESIAN_POINT('Ctrl Pts',(-39.5091373124624,43.8565665267056,
2.65878198860292));
#233190=CARTESIAN_POINT('Ctrl Pts',(-39.5155480799604,43.8507890749208,
2.65878198860291));
#233191=CARTESIAN_POINT('Ctrl Pts',(-39.5223801852468,43.8455908828151,
2.65945335517887));
#233192=CARTESIAN_POINT('Ctrl Pts',(-39.5294841269569,43.8409939475743,
2.66072561226636));
#233193=CARTESIAN_POINT('Ctrl Pts',(-39.5340725443949,43.8380247990817,
2.66154735980374));
#233194=CARTESIAN_POINT('Ctrl Pts',(-39.5387738681336,43.835305694046,2.66261895766918));
#233195=CARTESIAN_POINT('Ctrl Pts',(-39.5435446222367,43.8328343017436,
2.6639142925106));
#233196=CARTESIAN_POINT('Ctrl Pts',(-39.5498679835147,43.8295586128169,
2.66563118464156));
#233197=CARTESIAN_POINT('Ctrl Pts',(-39.5563148866446,43.8267236865061,
2.66774105138731));
#233198=CARTESIAN_POINT('Ctrl Pts',(-39.5627952650342,43.8243293609623,
2.67016894181781));
#233199=CARTESIAN_POINT('Ctrl Pts',(-39.566035454229,43.8231321981904,2.67138288703306));
#233200=CARTESIAN_POINT('Ctrl Pts',(-39.5692841591688,43.8220450509626,
2.67267613167582));
#233201=CARTESIAN_POINT('Ctrl Pts',(-39.5725311673657,43.8210669472518,
2.67403835432583));
#233202=CARTESIAN_POINT('Ctrl Pts',(-39.5741546714642,43.8205778953965,
2.67471946565084));
#233203=CARTESIAN_POINT('Ctrl Pts',(-39.5757777635549,43.8201160933895,
2.67541781389553));
#233204=CARTESIAN_POINT('Ctrl Pts',(-39.5773992434497,43.8196813503779,
2.67613207244199));
#233205=CARTESIAN_POINT('Ctrl Pts',(-39.5778046134234,43.819572664625,2.6763106370786));
#233206=CARTESIAN_POINT('Ctrl Pts',(-39.5782098828932,43.8194656698239,
2.67649019601875));
#233207=CARTESIAN_POINT('Ctrl Pts',(-39.5786150336268,43.8193603625176,
2.67667072836686));
#233208=CARTESIAN_POINT('Ctrl Pts',(-39.5798304858278,43.8190444405985,
2.6772123254112));
#233209=CARTESIAN_POINT('Ctrl Pts',(-39.5810448681192,43.8187437073124,
2.67776268340076));
#233210=CARTESIAN_POINT('Ctrl Pts',(-39.5822576997163,43.8184580587802,
2.67832123541545));
#233211=CARTESIAN_POINT('Ctrl Pts',(-39.5908007288816,43.8164459874034,
2.68225560368484));
#233212=CARTESIAN_POINT('Ctrl Pts',(-39.5992865061393,43.8151322889031,
2.68661792998942));
#233213=CARTESIAN_POINT('Ctrl Pts',(-39.6076412948842,43.8144227306311,
2.69130986622647));
#233214=CARTESIAN_POINT('Ctrl Pts',(-39.6116933583969,43.814078595636,2.69358545023111));
#233215=CARTESIAN_POINT('Ctrl Pts',(-39.6157150281164,43.8138769687219,
2.69593918853513));
#233216=CARTESIAN_POINT('Ctrl Pts',(-39.6196997093544,43.8138093098904,
2.69836306235505));
#233217=CARTESIAN_POINT('Ctrl Pts',(-39.6257999779284,43.8137057289464,
2.70207384382238));
#233218=CARTESIAN_POINT('Ctrl Pts',(-39.6318101761583,43.81391511288,2.70594760814237));
#233219=CARTESIAN_POINT('Ctrl Pts',(-39.6376940219322,43.8144090029878,
2.70995196345717));
#233220=CARTESIAN_POINT('Ctrl Pts',(-39.6404265103486,43.814638368109,2.71181160678115));
#233221=CARTESIAN_POINT('Ctrl Pts',(-39.6431316855283,43.8149288459967,
2.71369962772109));
#233222=CARTESIAN_POINT('Ctrl Pts',(-39.6458055463963,43.8152787628653,
2.71561183138671));
#233223=CARTESIAN_POINT('Ctrl Pts',(-39.6460104872963,43.8153055826146,
2.71575839426322));
#233224=CARTESIAN_POINT('Ctrl Pts',(-39.6462152612035,43.8153327221694,
2.71590508903219));
#233225=CARTESIAN_POINT('Ctrl Pts',(-39.6464198673376,43.8153601802954,
2.71605191409921));
#233226=CARTESIAN_POINT('Ctrl Pts',(-39.6492939666538,43.8157458841824,
2.71811436362762));
#233227=CARTESIAN_POINT('Ctrl Pts',(-39.6521348180508,43.8161965332334,
2.72020091026968));
#233228=CARTESIAN_POINT('Ctrl Pts',(-39.654938997009,43.816707563491,2.72230624862191));
#233229=CARTESIAN_POINT('Ctrl Pts',(-39.6649942840473,43.8185400271112,
2.72985561753159));
#233230=CARTESIAN_POINT('Ctrl Pts',(-39.6746561192258,43.8211611138373,
2.73770089914436));
#233231=CARTESIAN_POINT('Ctrl Pts',(-39.6839173731649,43.8244418968106,
2.74574823347232));
#233232=CARTESIAN_POINT('Ctrl Pts',(-39.6940945608685,43.8280471477143,
2.75459144547224));
#233233=CARTESIAN_POINT('Ctrl Pts',(-39.7037886794696,43.8324491002322,
2.76367911754513));
#233234=CARTESIAN_POINT('Ctrl Pts',(-39.7129876499635,43.8375295667884,
2.77292162565014));
#233235=CARTESIAN_POINT('Ctrl Pts',(-39.7229202294704,43.8430151956461,
2.7829012148506));
#233236=CARTESIAN_POINT('Ctrl Pts',(-39.7322766233333,43.8492922888436,
2.79306229500561));
#233237=CARTESIAN_POINT('Ctrl Pts',(-39.7410245486324,43.8562669044125,
2.8033191668567));
#233238=CARTESIAN_POINT('Ctrl Pts',(-39.749699087825,43.8631830101219,2.81348999408983));
#233239=CARTESIAN_POINT('Ctrl Pts',(-39.7577762496649,43.8707860819073,
2.82375635967035));
#233240=CARTESIAN_POINT('Ctrl Pts',(-39.7651933659001,43.879023624022,2.83404198860291));
#233241=CARTESIAN_POINT('Origin',(0.0113255271402848,0.0101975504410943,
2.83404198860262));
#233242=CARTESIAN_POINT('Ctrl Pts',(-42.0411527846897,46.7142062431422,
2.65878198860294));
#233243=CARTESIAN_POINT('Ctrl Pts',(-42.034767559739,46.7199506919427,2.65878198860294));
#233244=CARTESIAN_POINT('Ctrl Pts',(-42.0279592142777,46.7251107020213,
2.6594460304188));
#233245=CARTESIAN_POINT('Ctrl Pts',(-42.0208774479582,46.7296675019396,
2.66070439264095));
#233246=CARTESIAN_POINT('Ctrl Pts',(-42.0163525364096,46.7325790801595,
2.6615084261962));
#233247=CARTESIAN_POINT('Ctrl Pts',(-42.0117164851999,46.735245189214,2.66255428265394));
#233248=CARTESIAN_POINT('Ctrl Pts',(-42.0070114066749,46.7376689638752,
2.66381699700683));
#233249=CARTESIAN_POINT('Ctrl Pts',(-42.00058991857,46.7409769299535,2.66554034873283));
#233250=CARTESIAN_POINT('Ctrl Pts',(-41.994038348078,46.743827608742,2.66766759643987));
#233251=CARTESIAN_POINT('Ctrl Pts',(-41.9874523371583,46.7462229640888,
2.67012012783163));
#233252=CARTESIAN_POINT('Ctrl Pts',(-41.9841593316985,46.7474206417622,
2.67134639352751));
#233253=CARTESIAN_POINT('Ctrl Pts',(-41.9808575622225,46.7485046297347,
2.67265375585028));
#233254=CARTESIAN_POINT('Ctrl Pts',(-41.977557880152,46.7494761782933,2.67403135126956));
#233255=CARTESIAN_POINT('Ctrl Pts',(-41.9759080391167,46.7499619525726,
2.6747201489792));
#233256=CARTESIAN_POINT('Ctrl Pts',(-41.9742587070257,46.7504196286881,
2.67542649668649));
#233257=CARTESIAN_POINT('Ctrl Pts',(-41.9726111592841,46.7508494364813,
2.67614899656118));
#233258=CARTESIAN_POINT('Ctrl Pts',(-41.9721992723487,46.7509568884296,
2.67632962152986));
#233259=CARTESIAN_POINT('Ctrl Pts',(-41.9717874966609,46.7510625988575,
2.67651125590967));
#233260=CARTESIAN_POINT('Ctrl Pts',(-41.971375851596,46.7511665718606,2.67669387767541));
#233261=CARTESIAN_POINT('Ctrl Pts',(-41.9701409164014,46.7514784908699,
2.67724174297261));
#233262=CARTESIAN_POINT('Ctrl Pts',(-41.968907158177,46.7517747718024,2.67779849504765));
#233263=CARTESIAN_POINT('Ctrl Pts',(-41.9676750878621,46.7520555364233,
2.67836353618026));
#233264=CARTESIAN_POINT('Ctrl Pts',(-41.9591607175417,46.7539957941553,
2.68226832098917));
#233265=CARTESIAN_POINT('Ctrl Pts',(-41.9507055072921,46.7552464720208,
2.6865915375139));
#233266=CARTESIAN_POINT('Ctrl Pts',(-41.9423805287174,46.755902754358,2.69123699486167));
#233267=CARTESIAN_POINT('Ctrl Pts',(-41.9382430372171,46.7562289248781,
2.69354577441213));
#233268=CARTESIAN_POINT('Ctrl Pts',(-41.9341372814972,46.7564078446195,
2.69593478828123));
#233269=CARTESIAN_POINT('Ctrl Pts',(-41.9300700339485,46.7564487173143,
2.69839565261235));
#233270=CARTESIAN_POINT('Ctrl Pts',(-41.9210970783571,46.7565388885839,
2.7038246868906));
#233271=CARTESIAN_POINT('Ctrl Pts',(-41.9123126321656,46.7559695796225,
2.70961155815102));
#233272=CARTESIAN_POINT('Ctrl Pts',(-41.9038465062686,46.7548061840817,
2.71562701361782));
#233273=CARTESIAN_POINT('Ctrl Pts',(-41.900753723715,46.7543811810195,2.71782453535872));
#233274=CARTESIAN_POINT('Ctrl Pts',(-41.8976992635448,46.7538836816024,
2.72005051502417));
#233275=CARTESIAN_POINT('Ctrl Pts',(-41.8946854937103,46.7533184435778,
2.7222998676013));
#233276=CARTESIAN_POINT('Ctrl Pts',(-41.8845625597437,46.7514198688648,
2.72985520488883));
#233277=CARTESIAN_POINT('Ctrl Pts',(-41.8748360802685,46.7487367327317,
2.73770845534526));
#233278=CARTESIAN_POINT('Ctrl Pts',(-41.865513778659,46.7453971060011,2.74576706701696));
#233279=CARTESIAN_POINT('Ctrl Pts',(-41.8552674648909,46.7417264606194,
2.75462443584949));
#233280=CARTESIAN_POINT('Ctrl Pts',(-41.8455087367173,46.7372626589223,
2.76373036323078));
#233281=CARTESIAN_POINT('Ctrl Pts',(-41.836250857547,46.7321227530976,2.7729966463669));
#233282=CARTESIAN_POINT('Ctrl Pts',(-41.826279725012,46.726586854297,2.78297683033316));
#233283=CARTESIAN_POINT('Ctrl Pts',(-41.8168884800907,46.7202662104769,
2.79314401478702));
#233284=CARTESIAN_POINT('Ctrl Pts',(-41.8081115112118,46.7132528291651,
2.80341452427711));
#233285=CARTESIAN_POINT('Ctrl Pts',(-41.799453061047,46.7063341521808,2.81354634721222));
#233286=CARTESIAN_POINT('Ctrl Pts',(-41.7913915075194,46.6987402031264,
2.82378004209149));
#233287=CARTESIAN_POINT('Ctrl Pts',(-41.7839914803029,46.6905216402897,
2.83404198860294));
#233288=CARTESIAN_POINT('Ctrl Pts',(-39.4820551873932,44.1339623850447,
2.83404198860292));
#233289=CARTESIAN_POINT('Ctrl Pts',(-39.4749733207252,44.1260971752949,
2.82422126443095));
#233290=CARTESIAN_POINT('Ctrl Pts',(-39.4685372764365,44.1177016730302,
2.81442815028649));
#233291=CARTESIAN_POINT('Ctrl Pts',(-39.462775176276,44.1088266671103,2.80471618166523));
#233292=CARTESIAN_POINT('Ctrl Pts',(-39.4572113615991,44.1002570680371,
2.79533842146471));
#233293=CARTESIAN_POINT('Ctrl Pts',(-39.4522752837277,44.091239296903,2.78603515650518));
#233294=CARTESIAN_POINT('Ctrl Pts',(-39.4480294591808,44.0817922708765,
2.77685887347067));
#233295=CARTESIAN_POINT('Ctrl Pts',(-39.4440158252739,44.0728618726561,
2.76818441216905));
#233296=CARTESIAN_POINT('Ctrl Pts',(-39.4406186435293,44.0635470605582,
2.75962261521967));
#233297=CARTESIAN_POINT('Ctrl Pts',(-39.43793124934,44.0538529442847,2.75123537702016));
#233298=CARTESIAN_POINT('Ctrl Pts',(-39.4354562043761,44.0449248258277,
2.74351087134483));
#233299=CARTESIAN_POINT('Ctrl Pts',(-39.433583118669,44.035674438681,2.73593399450217));
#233300=CARTESIAN_POINT('Ctrl Pts',(-39.4324230329125,44.0261054688021,
2.72857657812951));
#233301=CARTESIAN_POINT('Ctrl Pts',(-39.4320771187576,44.0232521951457,
2.72638274508576));
#233302=CARTESIAN_POINT('Ctrl Pts',(-39.4317948788027,44.0203706219338,
2.72420861709734));
#233303=CARTESIAN_POINT('Ctrl Pts',(-39.4315800126158,44.0174609456696,
2.72205663736736));
#233304=CARTESIAN_POINT('Ctrl Pts',(-39.4313673418319,44.0145809991274,
2.71992664556775));
#233305=CARTESIAN_POINT('Ctrl Pts',(-39.4312206224784,44.0116765294505,
2.71782089927894));
#233306=CARTESIAN_POINT('Ctrl Pts',(-39.4311433701096,44.0087510493745,
2.71574387311255));
#233307=CARTESIAN_POINT('Ctrl Pts',(-39.4311379981309,44.0085476172114,
2.71559944077496));
#233308=CARTESIAN_POINT('Ctrl Pts',(-39.4311329512713,44.0083440782824,
2.71545515216079));
#233309=CARTESIAN_POINT('Ctrl Pts',(-39.4311282308204,44.0081404327825,
2.71531100781741));
#233310=CARTESIAN_POINT('Ctrl Pts',(-39.4309212689595,43.9992118680545,
2.70899119176099));
#233311=CARTESIAN_POINT('Ctrl Pts',(-39.4313859080979,43.9900881971808,
2.70298296066859));
#233312=CARTESIAN_POINT('Ctrl Pts',(-39.4325966403785,43.98085857377,2.69736727774161));
#233313=CARTESIAN_POINT('Ctrl Pts',(-39.4337252532879,43.9722549606535,
2.6921324852546));
#233314=CARTESIAN_POINT('Ctrl Pts',(-39.4355025470896,43.9635585482861,
2.68723866185504));
#233315=CARTESIAN_POINT('Ctrl Pts',(-39.4380105519135,43.9548613290787,
2.68278595829602));
#233316=CARTESIAN_POINT('Ctrl Pts',(-39.4389280125248,43.9516797737745,
2.68115710172835));
#233317=CARTESIAN_POINT('Ctrl Pts',(-39.4399434521994,43.9484983634056,
2.67958763637829));
#233318=CARTESIAN_POINT('Ctrl Pts',(-39.4410615611725,43.9453226165472,
2.67808378645375));
#233319=CARTESIAN_POINT('Ctrl Pts',(-39.4413304290277,43.9445589555201,
2.6777221607861));
#233320=CARTESIAN_POINT('Ctrl Pts',(-39.441605709343,43.9437952833156,2.67736403603573));
#233321=CARTESIAN_POINT('Ctrl Pts',(-39.4418874191263,43.943031734545,2.67700956934489));
#233322=CARTESIAN_POINT('Ctrl Pts',(-39.4421603254788,43.9422920466734,
2.67666617973814));
#233323=CARTESIAN_POINT('Ctrl Pts',(-39.4424392657172,43.9415524746579,
2.67632622314129));
#233324=CARTESIAN_POINT('Ctrl Pts',(-39.4427242524727,43.9408131433999,
2.67598984158783));
#233325=CARTESIAN_POINT('Ctrl Pts',(-39.445846611731,43.9327129150429,2.67230439292216));
#233326=CARTESIAN_POINT('Ctrl Pts',(-39.4496972096658,43.9246364083426,
2.66904964539959));
#233327=CARTESIAN_POINT('Ctrl Pts',(-39.454273889062,43.9167721156729,2.66640203566703));
#233328=CARTESIAN_POINT('Ctrl Pts',(-39.4561719744235,43.9135105590938,
2.66530399299431));
#233329=CARTESIAN_POINT('Ctrl Pts',(-39.4581945203288,43.9102855324947,
2.6643099514226));
#233330=CARTESIAN_POINT('Ctrl Pts',(-39.4603395741452,43.9071101492109,
2.6634305347337));
#233331=CARTESIAN_POINT('Ctrl Pts',(-39.4639981869599,43.9016942021215,
2.66193059792893));
#233332=CARTESIAN_POINT('Ctrl Pts',(-39.4680136963362,43.8964251099357,
2.66076519817136));
#233333=CARTESIAN_POINT('Ctrl Pts',(-39.4723737491581,43.8913745966874,
2.65997805604468));
#233334=CARTESIAN_POINT('Ctrl Pts',(-39.474553775569,43.8888493400633,2.65958448498134));
#233335=CARTESIAN_POINT('Ctrl Pts',(-39.476820955151,43.8863797569641,2.6592852626077));
#233336=CARTESIAN_POINT('Ctrl Pts',(-39.4791737454928,43.8839748786092,
2.65908463971332));
#233337=CARTESIAN_POINT('Ctrl Pts',(-39.4815265358346,43.8815700002543,
2.65888401681894));
#233338=CARTESIAN_POINT('Ctrl Pts',(-39.4839648939619,43.8792298420741,
2.65878198860292));
#233339=CARTESIAN_POINT('Ctrl Pts',(-39.4864862581819,43.8769616275874,
2.65878198860292));
#233340=CARTESIAN_POINT('Origin',(-43.3086183250768,38.9747476500513,2.83404198860288));
#233341=CARTESIAN_POINT('Ctrl Pts',(-46.6905216402899,41.7839914803026,
2.8340419886029));
#233342=CARTESIAN_POINT('Ctrl Pts',(-46.6984066517724,41.7910911765308,
2.82419652440036));
#233343=CARTESIAN_POINT('Ctrl Pts',(-46.705708077355,41.7987919603594,2.8143879057557));
#233344=CARTESIAN_POINT('Ctrl Pts',(-46.7123936319708,41.8070443420779,
2.80466781256778));
#233345=CARTESIAN_POINT('Ctrl Pts',(-46.7188619458713,41.8150285705302,
2.79526356452918));
#233346=CARTESIAN_POINT('Ctrl Pts',(-46.7247545199422,41.8235301761275,
2.7859410249604));
#233347=CARTESIAN_POINT('Ctrl Pts',(-46.7300083326618,41.8325358446895,
2.77675109088559));
#233348=CARTESIAN_POINT('Ctrl Pts',(-46.7349781159835,41.8410546526119,
2.76805797913439));
#233349=CARTESIAN_POINT('Ctrl Pts',(-46.7393768060097,41.8500252953139,
2.75948271209897));
#233350=CARTESIAN_POINT('Ctrl Pts',(-46.7431119772982,41.859452174832,2.75108575572942));
#233351=CARTESIAN_POINT('Ctrl Pts',(-46.7465523401895,41.8681350126375,
2.74335155162965));
#233352=CARTESIAN_POINT('Ctrl Pts',(-46.7494299450239,41.8772054497821,
2.73576818685618));
#233353=CARTESIAN_POINT('Ctrl Pts',(-46.7516345991567,41.8866715402957,
2.72840626160154));
#233354=CARTESIAN_POINT('Ctrl Pts',(-46.7522740855149,41.8894172933185,
2.72627084693461));
#233355=CARTESIAN_POINT('Ctrl Pts',(-46.752856683342,41.8921963397441,2.72415424587426));
#233356=CARTESIAN_POINT('Ctrl Pts',(-46.7533790039318,41.8950088623279,
2.72205867173281));
#233357=CARTESIAN_POINT('Ctrl Pts',(-46.7539452330337,41.8980578176395,
2.71978693462886));
#233358=CARTESIAN_POINT('Ctrl Pts',(-46.7544408966255,41.9011416752732,
2.71754411340787));
#233359=CARTESIAN_POINT('Ctrl Pts',(-46.7548620578768,41.9042597210856,
2.71533341844285));
#233360=CARTESIAN_POINT('Ctrl Pts',(-46.7560179382356,41.9128172222844,
2.70926614876433));
#233361=CARTESIAN_POINT('Ctrl Pts',(-46.756568484326,41.921627072481,2.70347381860451));
#233362=CARTESIAN_POINT('Ctrl Pts',(-46.756455626462,41.930603347835,2.69804914171437));
#233363=CARTESIAN_POINT('Ctrl Pts',(-46.7563523676437,41.9388161524504,
2.69308585687251));
#233364=CARTESIAN_POINT('Ctrl Pts',(-46.7556849461648,41.9471607721486,
2.68842799053235));
#233365=CARTESIAN_POINT('Ctrl Pts',(-46.7543795041531,41.9555881906104,
2.6841476705427));
#233366=CARTESIAN_POINT('Ctrl Pts',(-46.7537382753014,41.9597277110295,
2.68204519134602));
#233367=CARTESIAN_POINT('Ctrl Pts',(-46.7529426662695,41.9638869554867,
2.6800343177855));
#233368=CARTESIAN_POINT('Ctrl Pts',(-46.7519812517997,41.9680580970364,
2.67812693945298));
#233369=CARTESIAN_POINT('Ctrl Pts',(-46.7517988327683,41.968849530518,2.6777650329925));
#233370=CARTESIAN_POINT('Ctrl Pts',(-46.7516099985532,41.9696416823158,
2.6774065963997));
#233371=CARTESIAN_POINT('Ctrl Pts',(-46.7514147143009,41.9704344168203,
2.67705178968901));
#233372=CARTESIAN_POINT('Ctrl Pts',(-46.7512255326815,41.9712023783716,
2.67670807068804));
#233373=CARTESIAN_POINT('Ctrl Pts',(-46.7510302978708,41.9719708867612,
2.67636775825311));
#233374=CARTESIAN_POINT('Ctrl Pts',(-46.7508289807695,41.9727398158588,
2.676030996993));
#233375=CARTESIAN_POINT('Ctrl Pts',(-46.748635068482,41.9811194467226,2.67236104217174));
#233376=CARTESIAN_POINT('Ctrl Pts',(-46.7457169794823,41.9895544525279,
2.6691144054152));
#233377=CARTESIAN_POINT('Ctrl Pts',(-46.7420530111689,41.9978556152119,
2.66646778189676));
#233378=CARTESIAN_POINT('Ctrl Pts',(-46.740505694598,42.0013612477611,2.66535009635019));
#233379=CARTESIAN_POINT('Ctrl Pts',(-46.7388257854549,42.0048429302643,
2.66433897912389));
#233380=CARTESIAN_POINT('Ctrl Pts',(-46.7370135816691,42.0082865614563,
2.66344564884837));
#233381=CARTESIAN_POINT('Ctrl Pts',(-46.7339618757758,42.0140855503366,
2.6619413029863));
#233382=CARTESIAN_POINT('Ctrl Pts',(-46.7305342346688,42.0197742252486,
2.66077206705463));
#233383=CARTESIAN_POINT('Ctrl Pts',(-46.7267341265708,42.0252784509102,
2.65998225155757));
#233384=CARTESIAN_POINT('Ctrl Pts',(-46.7257840995463,42.0266545073256,
2.6597847976833));
#233385=CARTESIAN_POINT('Ctrl Pts',(-46.7248106099124,42.0280188904105,
2.65961098966665));
#233386=CARTESIAN_POINT('Ctrl Pts',(-46.7238134778068,42.0293702408568,
2.65946139030544));
#233387=CARTESIAN_POINT('Ctrl Pts',(-46.7223177796485,42.0313972665263,
2.65923699126362));
#233388=CARTESIAN_POINT('Ctrl Pts',(-46.7207688863877,42.0333949481517,
2.65906707562484));
#233389=CARTESIAN_POINT('Ctrl Pts',(-46.7191674503111,42.0353598072044,
2.65895332562961));
#233390=CARTESIAN_POINT('Ctrl Pts',(-46.7175660142345,42.0373246662572,
2.65883957563439));
#233391=CARTESIAN_POINT('Ctrl Pts',(-46.7159120469178,42.0392567035874,
2.6587819886029));
#233392=CARTESIAN_POINT('Ctrl Pts',(-46.7142062431438,42.0411527846906,
2.6587819886029));
#233393=CARTESIAN_POINT('Ctrl Pts',(-43.8769616275876,39.4864862581816,
2.65878198860288));
#233394=CARTESIAN_POINT('Ctrl Pts',(-43.8827333680737,39.4800703482073,
2.65878198860288));
#233395=CARTESIAN_POINT('Ctrl Pts',(-43.8889846873398,39.4741864828755,
2.65945335517881));
#233396=CARTESIAN_POINT('Ctrl Pts',(-43.8955692023373,39.4688721660169,
2.66072561226626));
#233397=CARTESIAN_POINT('Ctrl Pts',(-43.8998221234155,39.4654396626067,
2.66154735980364));
#233398=CARTESIAN_POINT('Ctrl Pts',(-43.90421346894,39.4622440309671,2.66261895766907));
#233399=CARTESIAN_POINT('Ctrl Pts',(-43.9086997575135,39.4592874976153,
2.66391429251051));
#233400=CARTESIAN_POINT('Ctrl Pts',(-43.9146460760272,39.4553687820182,
2.66563118464146));
#233401=CARTESIAN_POINT('Ctrl Pts',(-43.9207613318565,39.4518755008533,
2.66774105138722));
#233402=CARTESIAN_POINT('Ctrl Pts',(-43.9269559348856,39.4488169076809,
2.67016894181773));
#233403=CARTESIAN_POINT('Ctrl Pts',(-43.9300532364002,39.4472876110947,
2.67138288703298));
#233404=CARTESIAN_POINT('Ctrl Pts',(-43.9331705067653,39.4458668372382,
2.67267613167573));
#233405=CARTESIAN_POINT('Ctrl Pts',(-43.9362974878338,39.4445546869048,
2.67403835432575));
#233406=CARTESIAN_POINT('Ctrl Pts',(-43.937860978368,39.4438986117382,2.67471946565076));
#233407=CARTESIAN_POINT('Ctrl Pts',(-43.9394269075363,39.443269680209,2.67541781389545));
#233408=CARTESIAN_POINT('Ctrl Pts',(-43.9409940617757,39.4426678279634,
2.67613207244191));
#233409=CARTESIAN_POINT('Ctrl Pts',(-43.9413858503355,39.442517364902,2.67631063707853));
#233410=CARTESIAN_POINT('Ctrl Pts',(-43.9417777156946,39.4423685940347,
2.67649019601868));
#233411=CARTESIAN_POINT('Ctrl Pts',(-43.9421696393593,39.4422215138293,
2.67667072836679));
#233412=CARTESIAN_POINT('Ctrl Pts',(-43.9433454103532,39.4417802732128,
2.67721232541113));
#233413=CARTESIAN_POINT('Ctrl Pts',(-43.944521704943,39.4413542498604,2.6777626834007));
#233414=CARTESIAN_POINT('Ctrl Pts',(-43.9456980341197,39.4409433907177,
2.67832123541539));
#233415=CARTESIAN_POINT('Ctrl Pts',(-43.953983944948,39.4380493519682,2.68225560368463));
#233416=CARTESIAN_POINT('Ctrl Pts',(-43.9622859173443,39.4358558447894,
2.68661792998902));
#233417=CARTESIAN_POINT('Ctrl Pts',(-43.9705207686461,39.4342768603235,
2.69130986622586));
#233418=CARTESIAN_POINT('Ctrl Pts',(-43.974514662629,39.4335110545637,2.69358545023068));
#233419=CARTESIAN_POINT('Ctrl Pts',(-43.9784932254699,39.4328901532274,
2.69593918853489));
#233420=CARTESIAN_POINT('Ctrl Pts',(-43.9824490059337,39.4324063524315,
2.698363062355));
#233421=CARTESIAN_POINT('Ctrl Pts',(-43.9885050294413,39.4316656872153,
2.70207384382234));
#233422=CARTESIAN_POINT('Ctrl Pts',(-43.9945041897573,39.4312456873368,
2.70594760814234));
#233423=CARTESIAN_POINT('Ctrl Pts',(-44.0004074287825,39.4311218425062,
2.70995196345714));
#233424=CARTESIAN_POINT('Ctrl Pts',(-44.003148923525,39.4310643283261,2.71181160678112));
#233425=CARTESIAN_POINT('Ctrl Pts',(-44.0058696426793,39.4310704471412,
2.71369962772106));
#233426=CARTESIAN_POINT('Ctrl Pts',(-44.0085654321302,39.4311389525611,
2.71561183138668));
#233427=CARTESIAN_POINT('Ctrl Pts',(-44.0087720537697,39.4311442032316,
2.71575839426319));
#233428=CARTESIAN_POINT('Ctrl Pts',(-44.00897854276,39.4311497894113,2.71590508903216));
#233429=CARTESIAN_POINT('Ctrl Pts',(-44.009184898196,39.431155709954,2.71605191409918));
#233430=CARTESIAN_POINT('Ctrl Pts',(-44.01208356993,39.4312388757299,2.7181143636276));
#233431=CARTESIAN_POINT('Ctrl Pts',(-44.0149559644985,39.4313901062474,
2.72020091026966));
#233432=CARTESIAN_POINT('Ctrl Pts',(-44.0177981990785,39.4316052205106,
2.72230624862189));
#233433=CARTESIAN_POINT('Ctrl Pts',(-44.0279899468081,39.4323765820014,
2.72985561753128));
#233434=CARTESIAN_POINT('Ctrl Pts',(-44.0378728316098,39.4339733733566,
2.73770089914376));
#233435=CARTESIAN_POINT('Ctrl Pts',(-44.047426286633,39.4362681192151,2.7457482334714));
#233436=CARTESIAN_POINT('Ctrl Pts',(-44.0579245739736,39.4387898143859,
2.75459144547082));
#233437=CARTESIAN_POINT('Ctrl Pts',(-44.0680257165102,39.4421543412269,
2.76367911754317));
#233438=CARTESIAN_POINT('Ctrl Pts',(-44.0777053474426,39.4462454222061,
2.77292162564763));
#233439=CARTESIAN_POINT('Ctrl Pts',(-44.0881569195933,39.4506627629422,
2.78290121484711));
#233440=CARTESIAN_POINT('Ctrl Pts',(-44.0981181930565,39.4559274600935,
2.7930622950011));
#233441=CARTESIAN_POINT('Ctrl Pts',(-44.1075472421522,39.4619494607994,
2.80331916685116));
#233442=CARTESIAN_POINT('Ctrl Pts',(-44.1168971912149,39.4679209431074,
2.81348999408609));
#233443=CARTESIAN_POINT('Ctrl Pts',(-44.1257248429287,39.4746380711565,
2.82375635966846));
#233444=CARTESIAN_POINT('Ctrl Pts',(-44.1339623850449,39.482055187393,2.83404198860288));
#233445=CARTESIAN_POINT('Origin',(0.0101975504409187,0.0113255271404612,
2.83404198860262));
#233446=CARTESIAN_POINT('Ctrl Pts',(-46.6938111422607,42.06380383897,2.6587819886029));
#233447=CARTESIAN_POINT('Ctrl Pts',(-46.688061354646,42.0701842568303,2.6587819886029));
#233448=CARTESIAN_POINT('Ctrl Pts',(-46.6818296739378,42.076027665722,2.6594460304187));
#233449=CARTESIAN_POINT('Ctrl Pts',(-46.6752630175683,42.081299749164,2.66070439264073));
#233450=CARTESIAN_POINT('Ctrl Pts',(-46.6710672367553,42.0846683595047,
2.661508426196));
#233451=CARTESIAN_POINT('Ctrl Pts',(-46.6667352666014,42.0878044626436,
2.6625542826538));
#233452=CARTESIAN_POINT('Ctrl Pts',(-46.6623093164291,42.0907067742417,
2.66381699700679));
#233453=CARTESIAN_POINT('Ctrl Pts',(-46.6562687825186,42.0946678472191,
2.66554034873278));
#233454=CARTESIAN_POINT('Ctrl Pts',(-46.6500510792883,42.0981877352865,
2.66766759643983));
#233455=CARTESIAN_POINT('Ctrl Pts',(-46.6437515300389,42.1012583942265,
2.67012012783158));
#233456=CARTESIAN_POINT('Ctrl Pts',(-46.6406017554143,42.1027937236966,
2.67134639352746));
#233457=CARTESIAN_POINT('Ctrl Pts',(-46.637431380974,42.1042169023589,2.67265375585022));
#233458=CARTESIAN_POINT('Ctrl Pts',(-46.6342513293849,42.105528039369,2.6740313512695));
#233459=CARTESIAN_POINT('Ctrl Pts',(-46.6326613035903,42.106183607874,2.67472014897914));
#233460=CARTESIAN_POINT('Ctrl Pts',(-46.6310688468941,42.1068111789407,
2.67542649668642));
#233461=CARTESIAN_POINT('Ctrl Pts',(-46.6294752517396,42.1074108478354,
2.67614899656111));
#233462=CARTESIAN_POINT('Ctrl Pts',(-46.6290768529509,42.1075607650591,
2.67632962152979));
#233463=CARTESIAN_POINT('Ctrl Pts',(-46.628678382762,42.1077089386741,2.67651125590961));
#233464=CARTESIAN_POINT('Ctrl Pts',(-46.6282798608701,42.1078553707283,
2.67669387767534));
#233465=CARTESIAN_POINT('Ctrl Pts',(-46.6270842951944,42.1082946668907,
2.67724174297254));
#233466=CARTESIAN_POINT('Ctrl Pts',(-46.6258882654172,42.1087182876165,
2.67779849504758));
#233467=CARTESIAN_POINT('Ctrl Pts',(-46.6246922924067,42.109126300596,2.67836353618019));
#233468=CARTESIAN_POINT('Ctrl Pts',(-46.6164273768569,42.1119459234385,
2.68226832098911));
#233469=CARTESIAN_POINT('Ctrl Pts',(-46.6081492165691,42.1140735600938,
2.68659153751385));
#233470=CARTESIAN_POINT('Ctrl Pts',(-46.5999384432822,42.1155964444648,
2.69123699486162));
#233471=CARTESIAN_POINT('Ctrl Pts',(-46.5958577114965,42.116353313817,2.69354577441209));
#233472=CARTESIAN_POINT('Ctrl Pts',(-46.5917931497417,42.1169604217533,
2.69593478828119));
#233473=CARTESIAN_POINT('Ctrl Pts',(-46.5877524553606,42.1174262136792,
2.69839565261231));
#233474=CARTESIAN_POINT('Ctrl Pts',(-46.578838080023,42.11845382024,2.70382468689056));
#233475=CARTESIAN_POINT('Ctrl Pts',(-46.570042246956,42.1188058546738,2.70961155815098));
#233476=CARTESIAN_POINT('Ctrl Pts',(-46.5615008914345,42.1185337834653,
2.71562701361779));
#233477=CARTESIAN_POINT('Ctrl Pts',(-46.5583806265504,42.1184343924219,
2.7178245353587));
#233478=CARTESIAN_POINT('Ctrl Pts',(-46.555290896183,42.1182588963864,2.72005051502415));
#233479=CARTESIAN_POINT('Ctrl Pts',(-46.552234552633,42.1180117795243,2.72229986760129));
#233480=CARTESIAN_POINT('Ctrl Pts',(-46.5419686180608,42.1171817401336,
2.72985520488875));
#233481=CARTESIAN_POINT('Ctrl Pts',(-46.5320149571612,42.1155299964536,
2.73770845534509));
#233482=CARTESIAN_POINT('Ctrl Pts',(-46.5223946380453,42.113183110409,2.74576706701668));
#233483=CARTESIAN_POINT('Ctrl Pts',(-46.5118207677352,42.1106036046391,
2.75462443584913));
#233484=CARTESIAN_POINT('Ctrl Pts',(-46.5016489045639,42.1071843209742,
2.76373036323031));
#233485=CARTESIAN_POINT('Ctrl Pts',(-46.4919044745672,42.1030402839742,
2.77299664636633));
#233486=CARTESIAN_POINT('Ctrl Pts',(-46.481409305945,42.0985769785674,2.78297683033259));
#233487=CARTESIAN_POINT('Ctrl Pts',(-46.4714088200605,42.0932726122952,
2.79314401478644));
#233488=CARTESIAN_POINT('Ctrl Pts',(-46.4619468343647,42.0872150940891,
2.80341452427655));
#233489=CARTESIAN_POINT('Ctrl Pts',(-46.4526126174226,42.0812393728311,
2.8135463472118));
#233490=CARTESIAN_POINT('Ctrl Pts',(-46.443801442104,42.074529686026,2.82378004209123));
#233491=CARTESIAN_POINT('Ctrl Pts',(-46.4355828792672,42.0671296588095,
2.8340419886029));
#233492=CARTESIAN_POINT('Ctrl Pts',(-43.8790236240222,39.7651933658998,
2.83404198860289));
#233493=CARTESIAN_POINT('Ctrl Pts',(-43.8711584142718,39.7581114992313,
2.82422126443015));
#233494=CARTESIAN_POINT('Ctrl Pts',(-43.8638800583564,39.7504347382249,
2.81442815028492));
#233495=CARTESIAN_POINT('Ctrl Pts',(-43.8572218328527,39.7422106539902,
2.80471618166291));
#233496=CARTESIAN_POINT('Ctrl Pts',(-43.8507927303126,39.734269577075,2.79533842146186));
#233497=CARTESIAN_POINT('Ctrl Pts',(-43.8449410790333,39.7258171668685,
2.78603515650181));
#233498=CARTESIAN_POINT('Ctrl Pts',(-43.8397310304444,39.7168657021537,
2.77685887346682));
#233499=CARTESIAN_POINT('Ctrl Pts',(-43.8348059028416,39.708403764573,2.76818441216487));
#233500=CARTESIAN_POINT('Ctrl Pts',(-43.8304536682199,39.6994950821771,
2.75962261521518));
#233501=CARTESIAN_POINT('Ctrl Pts',(-43.8267676847805,39.6901349804711,
2.75123537701539));
#233502=CARTESIAN_POINT('Ctrl Pts',(-43.8233729558698,39.6815144838273,
2.74351087133981));
#233503=CARTESIAN_POINT('Ctrl Pts',(-43.8205432023692,39.6725105620392,
2.73593399449693));
#233504=CARTESIAN_POINT('Ctrl Pts',(-43.8183892419676,39.6631152739593,
2.72857657812408));
#233505=CARTESIAN_POINT('Ctrl Pts',(-43.8177469744568,39.6603137887119,
2.72638274508216));
#233506=CARTESIAN_POINT('Ctrl Pts',(-43.8171650742227,39.6574775031705,
2.72420861709555));
#233507=CARTESIAN_POINT('Ctrl Pts',(-43.8166472411072,39.654606226052,2.72205663736734));
#233508=CARTESIAN_POINT('Ctrl Pts',(-43.8161346989697,39.6517642863086,
2.71992664556774));
#233509=CARTESIAN_POINT('Ctrl Pts',(-43.8156851836083,39.648891063969,2.71782089927893));
#233510=CARTESIAN_POINT('Ctrl Pts',(-43.8153025584993,39.6459896850504,
2.71574387311254));
#233511=CARTESIAN_POINT('Ctrl Pts',(-43.8152759514976,39.6457879288346,
2.71559944077495));
#233512=CARTESIAN_POINT('Ctrl Pts',(-43.8152496566737,39.6455860324536,
2.71545515216077));
#233513=CARTESIAN_POINT('Ctrl Pts',(-43.8152236753307,39.6453839959665,
2.71531100781738));
#233514=CARTESIAN_POINT('Ctrl Pts',(-43.8140845580784,39.6365259762555,
2.70899119176088));
#233515=CARTESIAN_POINT('Ctrl Pts',(-43.8135929685791,39.6274037177902,
2.70298296066839));
#233516=CARTESIAN_POINT('Ctrl Pts',(-43.81383230999,39.6180980992373,2.69736727774133));
#233517=CARTESIAN_POINT('Ctrl Pts',(-43.8140554177822,39.6094236454405,
2.69213248525425));
#233518=CARTESIAN_POINT('Ctrl Pts',(-43.8149139527618,39.60058909514,2.68723866185465));
#233519=CARTESIAN_POINT('Ctrl Pts',(-43.8164991115145,39.5916773623193,
2.6827859582956));
#233520=CARTESIAN_POINT('Ctrl Pts',(-43.8170789830938,39.5884173351603,
2.68115710172805));
#233521=CARTESIAN_POINT('Ctrl Pts',(-43.8177563121467,39.5851472105418,
2.67958763637811));
#233522=CARTESIAN_POINT('Ctrl Pts',(-43.8185363400629,39.5818719865445,
2.67808378645368));
#233523=CARTESIAN_POINT('Ctrl Pts',(-43.8187239107183,39.5810844045887,
2.67772216078603));
#233524=CARTESIAN_POINT('Ctrl Pts',(-43.8189178575372,39.5802961412321,
2.67736403603566));
#233525=CARTESIAN_POINT('Ctrl Pts',(-43.8191182115052,39.5795073285708,
2.67700956934482));
#233526=CARTESIAN_POINT('Ctrl Pts',(-43.8193123044117,39.5787431663051,
2.67666617973807));
#233527=CARTESIAN_POINT('Ctrl Pts',(-43.81951241026,39.577978488548,2.67632622314121));
#233528=CARTESIAN_POINT('Ctrl Pts',(-43.819718554668,39.5772134181965,2.67598984158776));
#233529=CARTESIAN_POINT('Ctrl Pts',(-43.8219771048932,39.5688311883232,
2.67230439292224));
#233530=CARTESIAN_POINT('Ctrl Pts',(-43.8249623840156,39.5603964284873,
2.66904964539979));
#233531=CARTESIAN_POINT('Ctrl Pts',(-43.8286919494555,39.5520968239718,
2.6664020356673));
#233532=CARTESIAN_POINT('Ctrl Pts',(-43.8302387114098,39.5486547305946,
2.66530399299444));
#233533=CARTESIAN_POINT('Ctrl Pts',(-43.8319130705227,39.545235957413,2.66430995142263));
#233534=CARTESIAN_POINT('Ctrl Pts',(-43.8337144555752,39.5418537500316,
2.66343053473364));
#233535=CARTESIAN_POINT('Ctrl Pts',(-43.8367869054996,39.5360850428919,
2.66193059792888));
#233536=CARTESIAN_POINT('Ctrl Pts',(-43.8402296473865,39.5304250803199,
2.66076519817131));
#233537=CARTESIAN_POINT('Ctrl Pts',(-43.8440378929942,39.5249464846904,
2.65997805604464));
#233538=CARTESIAN_POINT('Ctrl Pts',(-43.845942015798,39.5222071868757,2.6595844849813));
#233539=CARTESIAN_POINT('Ctrl Pts',(-43.8479386338068,39.5195141476135,
2.65928526260766));
#233540=CARTESIAN_POINT('Ctrl Pts',(-43.8500271570782,39.516876509875,2.65908463971329));
#233541=CARTESIAN_POINT('Ctrl Pts',(-43.8521156803496,39.5142388721366,
2.65888401681891));
#233542=CARTESIAN_POINT('Ctrl Pts',(-43.8542960677575,39.5116566557598,
2.65878198860288));
#233543=CARTESIAN_POINT('Ctrl Pts',(-43.8565665267058,39.5091373124622,
2.65878198860288));
#233544=CARTESIAN_POINT('Origin',(-47.145339660541,34.2342565846636,2.83404198860285));
#233545=CARTESIAN_POINT('Ctrl Pts',(-50.8023624960593,36.6746059268177,
2.83404198860287));
#233546=CARTESIAN_POINT('Ctrl Pts',(-50.8109464329599,36.6808425220338,
2.82419652440154));
#233547=CARTESIAN_POINT('Ctrl Pts',(-50.8190128116684,36.6877379133665,
2.81438790575794));
#233548=CARTESIAN_POINT('Ctrl Pts',(-50.8265243508953,36.6952462569238,
2.80466781257097));
#233549=CARTESIAN_POINT('Ctrl Pts',(-50.8337918098257,36.7025106240248,
2.79526356453312));
#233550=CARTESIAN_POINT('Ctrl Pts',(-50.8405407635273,36.710349715224,2.78594102496499));
#233551=CARTESIAN_POINT('Ctrl Pts',(-50.8467071440063,36.7187568768206,
2.77675109089075));
#233552=CARTESIAN_POINT('Ctrl Pts',(-50.8525401602357,36.7267095340077,
2.76805797914004));
#233553=CARTESIAN_POINT('Ctrl Pts',(-50.8578524412736,36.7351712462807,
2.75948271210505));
#233554=CARTESIAN_POINT('Ctrl Pts',(-50.8625525281323,36.7441560526506,
2.75108575573587));
#233555=CARTESIAN_POINT('Ctrl Pts',(-50.8668816480481,36.752431709115,2.74335155163653));
#233556=CARTESIAN_POINT('Ctrl Pts',(-50.870691607918,36.7611516658436,2.73576818686343));
#233557=CARTESIAN_POINT('Ctrl Pts',(-50.8738736606193,36.7703354510133,
2.72840626160913));
#233558=CARTESIAN_POINT('Ctrl Pts',(-50.8747966531494,36.7729993179904,
2.72627084693963));
#233559=CARTESIAN_POINT('Ctrl Pts',(-50.8756665488979,36.7757022424564,
2.72415424587676));
#233560=CARTESIAN_POINT('Ctrl Pts',(-50.8764799968254,36.7784447603819,
2.72205867173284));
#233561=CARTESIAN_POINT('Ctrl Pts',(-50.8773618266783,36.7814178261393,
2.71978693462886));
#233562=CARTESIAN_POINT('Ctrl Pts',(-50.8781771258725,36.7844329791247,
2.71754411340786));
#233563=CARTESIAN_POINT('Ctrl Pts',(-50.8789219044955,36.7874899206174,
2.71533341844283));
#233564=CARTESIAN_POINT('Ctrl Pts',(-50.8809659552704,36.7958797205316,
2.7092661487643));
#233565=CARTESIAN_POINT('Ctrl Pts',(-50.8824343655145,36.8045837617103,
2.70347381860447));
#233566=CARTESIAN_POINT('Ctrl Pts',(-50.8832604021663,36.8135226609478,
2.69804914171433));
#233567=CARTESIAN_POINT('Ctrl Pts',(-50.8840161808561,36.821701268446,2.69308585687238));
#233568=CARTESIAN_POINT('Ctrl Pts',(-50.8842246658556,36.8300699399859,
2.68842799053215));
#233569=CARTESIAN_POINT('Ctrl Pts',(-50.8838072802929,36.8385876480152,
2.68414767054244));
#233570=CARTESIAN_POINT('Ctrl Pts',(-50.883602261868,36.8427715183747,2.68204519134583));
#233571=CARTESIAN_POINT('Ctrl Pts',(-50.8832457706971,36.8469911418449,
2.68003431778538));
#233572=CARTESIAN_POINT('Ctrl Pts',(-50.8827256259726,36.8512399286217,
2.67812693945291));
#233573=CARTESIAN_POINT('Ctrl Pts',(-50.8826269335774,36.8520460945289,
2.67776503299243));
#233574=CARTESIAN_POINT('Ctrl Pts',(-50.882521936226,36.8528536453865,2.67740659639964));
#233575=CARTESIAN_POINT('Ctrl Pts',(-50.8824105850808,36.8536624499713,
2.67705178968895));
#233576=CARTESIAN_POINT('Ctrl Pts',(-50.8823027136589,36.8544459794128,
2.67670807068798));
#233577=CARTESIAN_POINT('Ctrl Pts',(-50.8821888793658,36.8552306854278,
2.67636775825305));
#233578=CARTESIAN_POINT('Ctrl Pts',(-50.8820690400776,36.8560164456185,
2.67603099699295));
#233579=CARTESIAN_POINT('Ctrl Pts',(-50.8807630562081,36.8645794982675,
2.67236104217174));
#233580=CARTESIAN_POINT('Ctrl Pts',(-50.8787426509999,36.8732733195871,
2.66911440541524));
#233581=CARTESIAN_POINT('Ctrl Pts',(-50.875966462067,36.8819119966105,2.66646778189683));
#233582=CARTESIAN_POINT('Ctrl Pts',(-50.8747940602413,36.8855601635613,
2.66535009635021));
#233583=CARTESIAN_POINT('Ctrl Pts',(-50.8734872887379,36.8891983713647,
2.66433897912387));
#233584=CARTESIAN_POINT('Ctrl Pts',(-50.8720449698705,36.8928125648617,
2.66344564884832));
#233585=CARTESIAN_POINT('Ctrl Pts',(-50.8696161409375,36.8988987764016,
2.66194130298624));
#233586=CARTESIAN_POINT('Ctrl Pts',(-50.8668019052538,36.9049145742147,
2.66077206705458));
#233587=CARTESIAN_POINT('Ctrl Pts',(-50.8635979627953,36.9107858666119,
2.65998225155752));
#233588=CARTESIAN_POINT('Ctrl Pts',(-50.8627969771806,36.9122536897112,
2.65978479768326));
#233589=CARTESIAN_POINT('Ctrl Pts',(-50.861971437292,36.9137123559382,2.6596109896666));
#233590=CARTESIAN_POINT('Ctrl Pts',(-50.861121022166,36.9151605322321,2.65946139030539));
#233591=CARTESIAN_POINT('Ctrl Pts',(-50.8598453994769,36.9173327966729,
2.65923699126358));
#233592=CARTESIAN_POINT('Ctrl Pts',(-50.8585138058059,36.9194814382216,
2.65906707562479));
#233593=CARTESIAN_POINT('Ctrl Pts',(-50.857126526261,36.921602929223,2.65895332562957));
#233594=CARTESIAN_POINT('Ctrl Pts',(-50.8557392467161,36.9237244202245,
2.65883957563435));
#233595=CARTESIAN_POINT('Ctrl Pts',(-50.8542962928972,36.9258187603129,
2.65878198860287));
#233596=CARTESIAN_POINT('Ctrl Pts',(-50.8527980281387,36.9278827595326,
2.65878198860287));
#233597=CARTESIAN_POINT('Ctrl Pts',(-47.7640607692765,34.6837837831345,
2.65878198860285));
#233598=CARTESIAN_POINT('Ctrl Pts',(-47.7691302463546,34.6767997090225,
2.65878198860285));
#233599=CARTESIAN_POINT('Ctrl Pts',(-47.7747322888389,34.6702946353238,
2.65945335517889));
#233600=CARTESIAN_POINT('Ctrl Pts',(-47.7807252358003,34.6643211616146,
2.66072561226654));
#233601=CARTESIAN_POINT('Ctrl Pts',(-47.7845960646247,34.6604629105131,
2.66154735980388));
#233602=CARTESIAN_POINT('Ctrl Pts',(-47.788629319434,34.6568257642791,2.66261895766922));
#233603=CARTESIAN_POINT('Ctrl Pts',(-47.7927819897609,34.6534164822764,
2.66391429251049));
#233604=CARTESIAN_POINT('Ctrl Pts',(-47.7982861164003,34.648897674277,2.66563118464146));
#233605=CARTESIAN_POINT('Ctrl Pts',(-47.8040027249063,34.6447843113775,
2.66774105138722));
#233606=CARTESIAN_POINT('Ctrl Pts',(-47.8098436832079,34.6410949611633,
2.67016894181774));
#233607=CARTESIAN_POINT('Ctrl Pts',(-47.8127641623586,34.6392502860563,
2.67138288703299));
#233608=CARTESIAN_POINT('Ctrl Pts',(-47.8157158446827,34.6375114518667,
2.67267613167576));
#233609=CARTESIAN_POINT('Ctrl Pts',(-47.8186885387638,34.6358796311044,
2.67403835432578));
#233610=CARTESIAN_POINT('Ctrl Pts',(-47.8201748858043,34.6350637207233,
2.67471946565079));
#233611=CARTESIAN_POINT('Ctrl Pts',(-47.8216664954025,34.6342745503772,
2.67541781389548));
#233612=CARTESIAN_POINT('Ctrl Pts',(-47.8231621539167,34.6335121829169,
2.67613207244195));
#233613=CARTESIAN_POINT('Ctrl Pts',(-47.8235360685452,34.6333215910518,
2.67631063707856));
#233614=CARTESIAN_POINT('Ctrl Pts',(-47.8239102364347,34.6331326740832,
2.67649019601871));
#233615=CARTESIAN_POINT('Ctrl Pts',(-47.8242846390327,34.6329454324201,
2.67667072836683));
#233616=CARTESIAN_POINT('Ctrl Pts',(-47.8254078468265,34.6323837074307,
2.67721232541117));
#233617=CARTESIAN_POINT('Ctrl Pts',(-47.8265331659852,34.6318370616129,
2.67776268340073));
#233618=CARTESIAN_POINT('Ctrl Pts',(-47.8276601046327,34.6313054933185,
2.67832123541542));
#233619=CARTESIAN_POINT('Ctrl Pts',(-47.8355981149515,34.6275611948904,
2.68225560368471));
#233620=CARTESIAN_POINT('Ctrl Pts',(-47.8436253243399,34.6245119115567,
2.68661792998915));
#233621=CARTESIAN_POINT('Ctrl Pts',(-47.851650015445,34.6220808005811,2.69130986622604));
#233622=CARTESIAN_POINT('Ctrl Pts',(-47.8555419819595,34.6209017143849,
2.6935854502308));
#233623=CARTESIAN_POINT('Ctrl Pts',(-47.8594338479543,34.6198683413514,
2.69593918853494));
#233624=CARTESIAN_POINT('Ctrl Pts',(-47.863317387285,34.618973699214,2.69836306235499));
#233625=CARTESIAN_POINT('Ctrl Pts',(-47.8692628146652,34.6176040646085,
2.70207384382232));
#233626=CARTESIAN_POINT('Ctrl Pts',(-47.8751852090114,34.6165592825246,
2.70594760814232));
#233627=CARTESIAN_POINT('Ctrl Pts',(-47.8810431641657,34.6158190596253,
2.70995196345712));
#233628=CARTESIAN_POINT('Ctrl Pts',(-47.8837636288444,34.6154752962814,
2.7118116067811));
#233629=CARTESIAN_POINT('Ctrl Pts',(-47.8864700832048,34.6151969889848,
2.71369962772103));
#233630=CARTESIAN_POINT('Ctrl Pts',(-47.8891582656053,34.6149833323962,
2.71561183138665));
#233631=CARTESIAN_POINT('Ctrl Pts',(-47.8893643041943,34.6149669564605,
2.71575839426316));
#233632=CARTESIAN_POINT('Ctrl Pts',(-47.8895702459311,34.6149509280617,
2.71590508903212));
#233633=CARTESIAN_POINT('Ctrl Pts',(-47.8897760897957,34.6149352461545,
2.71605191409915));
#233634=CARTESIAN_POINT('Ctrl Pts',(-47.8926675754934,34.6147149626377,
2.71811436362756));
#233635=CARTESIAN_POINT('Ctrl Pts',(-47.8955400426775,34.6145651177085,
2.72020091026963));
#233636=CARTESIAN_POINT('Ctrl Pts',(-47.8983891927624,34.6144819591403,
2.72230624862186));
#233637=CARTESIAN_POINT('Ctrl Pts',(-47.9086057382621,34.614183767304,2.72985561753071));
#233638=CARTESIAN_POINT('Ctrl Pts',(-47.9186013937326,34.614738768508,2.73770089914259));
#233639=CARTESIAN_POINT('Ctrl Pts',(-47.9283423801871,34.616022335536,2.74574823346962));
#233640=CARTESIAN_POINT('Ctrl Pts',(-47.9390467457316,34.617432846754,2.75459144546848));
#233641=CARTESIAN_POINT('Ctrl Pts',(-47.9494442419723,34.619723085458,2.76367911754026));
#233642=CARTESIAN_POINT('Ctrl Pts',(-47.959498481281,34.6227799581208,2.77292162564413));
#233643=CARTESIAN_POINT('Ctrl Pts',(-47.9703545364643,34.6260806134262,
2.78290121484312));
#233644=CARTESIAN_POINT('Ctrl Pts',(-47.9808115517317,34.6302752334078,
2.79306229499661));
#233645=CARTESIAN_POINT('Ctrl Pts',(-47.9908184179891,34.6352786409512,
2.80331916684618));
#233646=CARTESIAN_POINT('Ctrl Pts',(-48.0007413369235,34.6402400750478,
2.81348999408273));
#233647=CARTESIAN_POINT('Ctrl Pts',(-48.0102227609117,34.6459976650994,
2.82375635966676));
#233648=CARTESIAN_POINT('Ctrl Pts',(-48.0191904766738,34.6525130919796,
2.83404198860285));
#233649=CARTESIAN_POINT('Origin',(0.00895784724494739,0.0123294189944604,
2.83404198860262));
#233650=CARTESIAN_POINT('Ctrl Pts',(-50.8348823336488,36.9525415975211,
2.65878198860287));
#233651=CARTESIAN_POINT('Ctrl Pts',(-50.8298309792461,36.9594880792486,
2.65878198860287));
#233652=CARTESIAN_POINT('Ctrl Pts',(-50.8242442388883,36.9659508653432,
2.65944603041871));
#233653=CARTESIAN_POINT('Ctrl Pts',(-50.8182646381297,36.9718804702597,
2.66070439264082));
#233654=CARTESIAN_POINT('Ctrl Pts',(-50.8144439579055,36.9756692055208,
2.66150842619607));
#233655=CARTESIAN_POINT('Ctrl Pts',(-50.8104635307793,36.9792409429415,
2.66255428265383));
#233656=CARTESIAN_POINT('Ctrl Pts',(-50.8063652005966,36.9825899931428,
2.66381699700674));
#233657=CARTESIAN_POINT('Ctrl Pts',(-50.8007718022341,36.987160774675,2.66554034873273));
#233658=CARTESIAN_POINT('Ctrl Pts',(-50.7949560887232,36.9913113073909,
2.66766759643977));
#233659=CARTESIAN_POINT('Ctrl Pts',(-50.789012020324,36.9950236271423,2.67012012783152));
#233660=CARTESIAN_POINT('Ctrl Pts',(-50.7860399861244,36.9968797870181,
2.6713463935274));
#233661=CARTESIAN_POINT('Ctrl Pts',(-50.7830357420056,36.998626563727,2.67265375585016));
#233662=CARTESIAN_POINT('Ctrl Pts',(-50.7800101622086,37.0002629240971,
2.67403135126944));
#233663=CARTESIAN_POINT('Ctrl Pts',(-50.7784973723101,37.0010811042821,
2.67472014897908));
#233664=CARTESIAN_POINT('Ctrl Pts',(-50.7769792382975,37.0018716945001,
2.67542649668636));
#233665=CARTESIAN_POINT('Ctrl Pts',(-50.775457055492,37.0026346543984,2.67614899656106));
#233666=CARTESIAN_POINT('Ctrl Pts',(-50.7750765097906,37.002825394373,2.67632962152973));
#233667=CARTESIAN_POINT('Ctrl Pts',(-50.7746957108233,37.003014407754,2.67651125590955));
#233668=CARTESIAN_POINT('Ctrl Pts',(-50.7743146783936,37.0032016945189,
2.67669387767528));
#233669=CARTESIAN_POINT('Ctrl Pts',(-50.7731715811046,37.0037635548139,
2.67724174297248));
#233670=CARTESIAN_POINT('Ctrl Pts',(-50.7720263837272,37.0043098740556,
2.67779849504752));
#233671=CARTESIAN_POINT('Ctrl Pts',(-50.7708796113517,37.0048406651183,
2.67836353618014));
#233672=CARTESIAN_POINT('Ctrl Pts',(-50.7629547027164,37.0085087606934,
2.68226832098921));
#233673=CARTESIAN_POINT('Ctrl Pts',(-50.7549442896465,37.0114900453061,
2.68659153751414));
#233674=CARTESIAN_POINT('Ctrl Pts',(-50.7469376805975,37.0138628466712,
2.69123699486213));
#233675=CARTESIAN_POINT('Ctrl Pts',(-50.7429584178781,37.0150421224363,
2.69354577441243));
#233676=CARTESIAN_POINT('Ctrl Pts',(-50.7389795822777,37.0160707669658,
2.69593478828134));
#233677=CARTESIAN_POINT('Ctrl Pts',(-50.7350097117578,37.0169563748089,
2.69839565261227));
#233678=CARTESIAN_POINT('Ctrl Pts',(-50.7262515844356,37.0189101579885,
2.70382468689053));
#233679=CARTESIAN_POINT('Ctrl Pts',(-50.7175407334809,37.0201796788545,
2.70961155815094));
#233680=CARTESIAN_POINT('Ctrl Pts',(-50.7090177292134,37.0208019128475,
2.71562701361775));
#233681=CARTESIAN_POINT('Ctrl Pts',(-50.7059041682737,37.0210292227719,
2.71782453535867));
#233682=CARTESIAN_POINT('Ctrl Pts',(-50.7028130194416,37.0211776528892,
2.72005051502411));
#233683=CARTESIAN_POINT('Ctrl Pts',(-50.6997475881155,37.0212513646536,
2.72229986760125));
#233684=CARTESIAN_POINT('Ctrl Pts',(-50.6894511286645,37.0214989546704,
2.7298552048891));
#233685=CARTESIAN_POINT('Ctrl Pts',(-50.6793793407316,37.0208967002927,
2.73770845534585));
#233686=CARTESIAN_POINT('Ctrl Pts',(-50.6695664063382,37.0195682679086,
2.74576706701788));
#233687=CARTESIAN_POINT('Ctrl Pts',(-50.6587808290213,37.0181081633553,
2.75462443585076));
#233688=CARTESIAN_POINT('Ctrl Pts',(-50.6483072759133,37.0157708601097,
2.7637303632324));
#233689=CARTESIAN_POINT('Ctrl Pts',(-50.6381830571039,37.0126680948707,
2.77299664636891));
#233690=CARTESIAN_POINT('Ctrl Pts',(-50.6272788396577,37.0093262837653,
2.78297683033572));
#233691=CARTESIAN_POINT('Ctrl Pts',(-50.6167786802258,37.0050963107875,
2.79314401479016));
#233692=CARTESIAN_POINT('Ctrl Pts',(-50.606735345208,37.0000610231238,2.80341452428089));
#233693=CARTESIAN_POINT('Ctrl Pts',(-50.5968276291246,36.9950937288454,
2.81354634721468));
#233694=CARTESIAN_POINT('Ctrl Pts',(-50.5873633690971,36.9893418170231,
2.82378004209264));
#233695=CARTESIAN_POINT('Ctrl Pts',(-50.5784163149359,36.9828414016746,
2.83404198860287));
#233696=CARTESIAN_POINT('Ctrl Pts',(-47.7952442955504,34.9607485668365,
2.83404198860285));
#233697=CARTESIAN_POINT('Ctrl Pts',(-47.7866819156023,34.9545276336633,
2.82422126443049));
#233698=CARTESIAN_POINT('Ctrl Pts',(-47.7786409912516,34.9476537221161,
2.81442815028562));
#233699=CARTESIAN_POINT('Ctrl Pts',(-47.7711595893173,34.9401706643557,
2.80471618166397));
#233700=CARTESIAN_POINT('Ctrl Pts',(-47.7639356375071,34.9329451136996,
2.79533842146316));
#233701=CARTESIAN_POINT('Ctrl Pts',(-47.7572325247361,34.9251506707967,
2.78603515650334));
#233702=CARTESIAN_POINT('Ctrl Pts',(-47.7511153344879,34.916792841515,2.77685887346856));
#233703=CARTESIAN_POINT('Ctrl Pts',(-47.745332673918,34.9088920753337,2.76818441216674));
#233704=CARTESIAN_POINT('Ctrl Pts',(-47.7400730704123,34.9004871280291,
2.75962261521719));
#233705=CARTESIAN_POINT('Ctrl Pts',(-47.7354288821284,34.8915635921244,
2.75123537701751));
#233706=CARTESIAN_POINT('Ctrl Pts',(-47.7311516626311,34.8833451652596,
2.743510871342));
#233707=CARTESIAN_POINT('Ctrl Pts',(-47.7273962447083,34.8746863576823,
2.73593399449919));
#233708=CARTESIAN_POINT('Ctrl Pts',(-47.7242720089021,34.8655676881445,
2.72857657812639));
#233709=CARTESIAN_POINT('Ctrl Pts',(-47.7233404248517,34.8628486849613,
2.72638274508368));
#233710=CARTESIAN_POINT('Ctrl Pts',(-47.7224652397587,34.8600887620252,
2.72420861709628));
#233711=CARTESIAN_POINT('Ctrl Pts',(-47.7216501132021,34.857287342362,2.72205663736731));
#233712=CARTESIAN_POINT('Ctrl Pts',(-47.72084331523,34.8545145463038,2.7199266455677));
#233713=CARTESIAN_POINT('Ctrl Pts',(-47.720095928845,34.8517040509267,2.71782089927888));
#233714=CARTESIAN_POINT('Ctrl Pts',(-47.7194121231167,34.8488585612801,
2.7157438731125));
#233715=CARTESIAN_POINT('Ctrl Pts',(-47.7193645726037,34.8486606914949,
2.7155994407749));
#233716=CARTESIAN_POINT('Ctrl Pts',(-47.7193173179071,34.848462649681,2.71545515216073));
#233717=CARTESIAN_POINT('Ctrl Pts',(-47.7192703603292,34.8482644357608,
2.71531100781734));
#233718=CARTESIAN_POINT('Ctrl Pts',(-47.7172115680923,34.8395740113844,
2.70899119176081));
#233719=CARTESIAN_POINT('Ctrl Pts',(-47.7157691359129,34.8305531107004,
2.70298296066831));
#233720=CARTESIAN_POINT('Ctrl Pts',(-47.7150344641794,34.8212734513097,
2.69736727774125));
#233721=CARTESIAN_POINT('Ctrl Pts',(-47.7143496224387,34.8126231959635,
2.69213248525408));
#233722=CARTESIAN_POINT('Ctrl Pts',(-47.7142799923073,34.8037473009117,
2.68723866185439));
#233723=CARTESIAN_POINT('Ctrl Pts',(-47.7149249376576,34.7947186932872,
2.68278595829527));
#233724=CARTESIAN_POINT('Ctrl Pts',(-47.7151608670106,34.7914159118132,
2.68115710172783));
#233725=CARTESIAN_POINT('Ctrl Pts',(-47.7154926644831,34.7880929011147,
2.679587636378));
#233726=CARTESIAN_POINT('Ctrl Pts',(-47.7159260651934,34.784754084018,2.67808378645366));
#233727=CARTESIAN_POINT('Ctrl Pts',(-47.7160302835856,34.7839512100461,
2.67772216078602));
#233728=CARTESIAN_POINT('Ctrl Pts',(-47.7161407719862,34.7831469919158,
2.67736403603564));
#233729=CARTESIAN_POINT('Ctrl Pts',(-47.7162575750189,34.7823415577604,
2.6770095693448));
#233730=CARTESIAN_POINT('Ctrl Pts',(-47.7163707279568,34.7815612934223,
2.67666617973805));
#233731=CARTESIAN_POINT('Ctrl Pts',(-47.7164898070135,34.7807798878932,
2.67632622314121));
#233732=CARTESIAN_POINT('Ctrl Pts',(-47.7166148505127,34.7799974607189,
2.67598984158775));
#233733=CARTESIAN_POINT('Ctrl Pts',(-47.717984846556,34.771425066794,2.67230439292235));
#233734=CARTESIAN_POINT('Ctrl Pts',(-47.7200720995232,34.7627244668161,
2.66904964539999));
#233735=CARTESIAN_POINT('Ctrl Pts',(-47.7229136891076,34.7540804826588,
2.66640203566754));
#233736=CARTESIAN_POINT('Ctrl Pts',(-47.724092181007,34.7504955647788,2.66530399299458));
#233737=CARTESIAN_POINT('Ctrl Pts',(-47.7254000086987,34.7469205018091,
2.66430995142268));
#233738=CARTESIAN_POINT('Ctrl Pts',(-47.7268379886354,34.7433685265021,
2.66343053473362));
#233739=CARTESIAN_POINT('Ctrl Pts',(-47.7292906132653,34.7373102624746,
2.66193059792886));
#233740=CARTESIAN_POINT('Ctrl Pts',(-47.7321228682621,34.731321441251,2.66076519817129));
#233741=CARTESIAN_POINT('Ctrl Pts',(-47.7353375827201,34.7254747878806,
2.65997805604461));
#233742=CARTESIAN_POINT('Ctrl Pts',(-47.7369449399491,34.7225514611954,
2.65958448498127));
#233743=CARTESIAN_POINT('Ctrl Pts',(-47.7386491210198,34.7196644712719,
2.65928526260763));
#233744=CARTESIAN_POINT('Ctrl Pts',(-47.7404504949227,34.7168229726608,
2.65908463971326));
#233745=CARTESIAN_POINT('Ctrl Pts',(-47.7422518688256,34.7139814740497,
2.65888401681888));
#233746=CARTESIAN_POINT('Ctrl Pts',(-47.7441503967333,34.7111854907793,
2.65878198860285));
#233747=CARTESIAN_POINT('Ctrl Pts',(-47.7461450747866,34.7084426211231,
2.65878198860285));
#233748=CARTESIAN_POINT('Origin',(-50.4655267888877,29.1186878401555,2.83404198860281));
#233749=CARTESIAN_POINT('Ctrl Pts',(-54.357602037244,31.1634057161439,2.83404198860283));
#233750=CARTESIAN_POINT('Ctrl Pts',(-54.3667908521538,31.1687108809056,
2.8241965244016));
#233751=CARTESIAN_POINT('Ctrl Pts',(-54.3755338070552,31.1747253323926,
2.81438790575814));
#233752=CARTESIAN_POINT('Ctrl Pts',(-54.3837890328979,31.1814073748059,
2.80466781257132));
#233753=CARTESIAN_POINT('Ctrl Pts',(-54.3917760130574,31.1878722906298,
2.79526356453362));
#233754=CARTESIAN_POINT('Ctrl Pts',(-54.3993074034408,31.194962980708,2.78594102496565));
#233755=CARTESIAN_POINT('Ctrl Pts',(-54.4063187915245,31.2026795247181,
2.77675109089157));
#233756=CARTESIAN_POINT('Ctrl Pts',(-54.4129511329153,31.2099789001943,
2.76805797914105));
#233757=CARTESIAN_POINT('Ctrl Pts',(-54.4191188025023,31.2178389737485,
2.75948271210624));
#233758=CARTESIAN_POINT('Ctrl Pts',(-54.424732309796,31.2262832675523,2.75108575573722));
#233759=CARTESIAN_POINT('Ctrl Pts',(-54.4299027559926,31.2340610728523,
2.74335155163808));
#233760=CARTESIAN_POINT('Ctrl Pts',(-54.4346033281803,31.242335011495,2.73576818686516));
#233761=CARTESIAN_POINT('Ctrl Pts',(-54.4387279162147,31.2511358718494,
2.72840626161101));
#233762=CARTESIAN_POINT('Ctrl Pts',(-54.439924302417,31.2536886668944,2.72627084694087));
#233763=CARTESIAN_POINT('Ctrl Pts',(-54.4410719653267,31.2562858555924,
2.72415424587736));
#233764=CARTESIAN_POINT('Ctrl Pts',(-54.4421676282859,31.2589283212566,
2.72205867173281));
#233765=CARTESIAN_POINT('Ctrl Pts',(-54.4433553973774,31.2617929239294,
2.71978693462883));
#233766=CARTESIAN_POINT('Ctrl Pts',(-54.4444813995854,31.2647063376194,
2.71754411340783));
#233767=CARTESIAN_POINT('Ctrl Pts',(-54.4455416356297,31.2676686823018,
2.7153334184428));
#233768=CARTESIAN_POINT('Ctrl Pts',(-54.4484514617727,31.2757988605279,
2.70926614876426));
#233769=CARTESIAN_POINT('Ctrl Pts',(-54.4508216479604,31.2843017293921,
2.70347381860443));
#233770=CARTESIAN_POINT('Ctrl Pts',(-54.4525775288976,31.2931053160624,
2.69804914171429));
#233771=CARTESIAN_POINT('Ctrl Pts',(-54.4541840646262,31.3011601199081,
2.69308585687222));
#233772=CARTESIAN_POINT('Ctrl Pts',(-54.4552661718987,31.3094611543733,
2.68842799053189));
#233773=CARTESIAN_POINT('Ctrl Pts',(-54.4557414157487,31.3179758301784,
2.68414767054209));
#233774=CARTESIAN_POINT('Ctrl Pts',(-54.4559748539753,31.3221582111191,
2.68204519134559));
#233775=CARTESIAN_POINT('Ctrl Pts',(-54.4560613864572,31.3263919825245,
2.68003431778523));
#233776=CARTESIAN_POINT('Ctrl Pts',(-54.4559882102925,31.3306718639313,
2.67812693945286));
#233777=CARTESIAN_POINT('Ctrl Pts',(-54.455974325828,31.3314839297417,2.67776503299238));
#233778=CARTESIAN_POINT('Ctrl Pts',(-54.4559543157132,31.332298031963,2.67740659639959));
#233779=CARTESIAN_POINT('Ctrl Pts',(-54.4559281176616,31.3331140451957,
2.6770517896889));
#233780=CARTESIAN_POINT('Ctrl Pts',(-54.455902738299,31.3339045580149,2.67670807068793));
#233781=CARTESIAN_POINT('Ctrl Pts',(-54.455871551716,31.3346968642519,2.676367758253));
#233782=CARTESIAN_POINT('Ctrl Pts',(-54.4558345032252,31.3354908465828,
2.6760309969929));
#233783=CARTESIAN_POINT('Ctrl Pts',(-54.4554307564063,31.34414350242,2.67236104217183));
#233784=CARTESIAN_POINT('Ctrl Pts',(-54.4543301709717,31.353000887928,2.66911440541543));
#233785=CARTESIAN_POINT('Ctrl Pts',(-54.4524721779263,31.3618824321374,
2.66646778189708));
#233786=CARTESIAN_POINT('Ctrl Pts',(-54.4516875359255,31.3656331634094,
2.66535009635034));
#233787=CARTESIAN_POINT('Ctrl Pts',(-54.4507682193238,31.3693880355472,
2.6643389791239));
#233788=CARTESIAN_POINT('Ctrl Pts',(-54.4497115877222,31.3731331934892,
2.66344564884827));
#233789=CARTESIAN_POINT('Ctrl Pts',(-54.4479322465076,31.3794399458813,
2.6619413029862));
#233790=CARTESIAN_POINT('Ctrl Pts',(-54.4457622496022,31.3857169562559,
2.66077206705454));
#233791=CARTESIAN_POINT('Ctrl Pts',(-54.4431895758471,31.3918909882805,
2.65998225155748));
#233792=CARTESIAN_POINT('Ctrl Pts',(-54.4425464074084,31.3934344962866,
2.65978479768321));
#233793=CARTESIAN_POINT('Ctrl Pts',(-54.4418778620527,31.3949714642033,
2.65961098966656));
#233794=CARTESIAN_POINT('Ctrl Pts',(-54.4411834812323,31.3965005998222,
2.65946139030535));
#233795=CARTESIAN_POINT('Ctrl Pts',(-54.4401419100017,31.3987943032506,
2.65923699126354));
#233796=CARTESIAN_POINT('Ctrl Pts',(-54.4390422051394,31.4010703637562,
2.65906707562476));
#233797=CARTESIAN_POINT('Ctrl Pts',(-54.4378842814512,31.4033252432069,
2.65895332562953));
#233798=CARTESIAN_POINT('Ctrl Pts',(-54.4367263577631,31.4055801226576,
2.65883957563431));
#233799=CARTESIAN_POINT('Ctrl Pts',(-54.4355102267473,31.4078138194773,
2.65878198860283));
#233800=CARTESIAN_POINT('Ctrl Pts',(-54.4342359163065,31.410023123206,2.65878198860283));
#233801=CARTESIAN_POINT('Ctrl Pts',(-51.1278468659049,29.501078514911,2.65878198860281));
#233802=CARTESIAN_POINT('Ctrl Pts',(-51.1321585373225,29.4936027956397,
2.65878198860281));
#233803=CARTESIAN_POINT('Ctrl Pts',(-51.1370499258744,29.4865477845238,
2.65945335517875));
#233804=CARTESIAN_POINT('Ctrl Pts',(-51.1423856448177,29.4799806005927,
2.66072561226622));
#233805=CARTESIAN_POINT('Ctrl Pts',(-51.1458319717786,29.4757388736053,
2.66154735980359));
#233806=CARTESIAN_POINT('Ctrl Pts',(-51.1494629466899,29.4717000621112,
2.66261895766902));
#233807=CARTESIAN_POINT('Ctrl Pts',(-51.1532365012461,29.4678753842639,
2.66391429251045));
#233808=CARTESIAN_POINT('Ctrl Pts',(-51.1582381316478,29.4628059928683,
2.66563118464141));
#233809=CARTESIAN_POINT('Ctrl Pts',(-51.1634934604717,29.4581176150989,
2.66774105138716));
#233810=CARTESIAN_POINT('Ctrl Pts',(-51.1689167792841,29.453837929136,2.67016894181767));
#233811=CARTESIAN_POINT('Ctrl Pts',(-51.1716284386903,29.4516980861545,
2.67138288703292));
#233812=CARTESIAN_POINT('Ctrl Pts',(-51.174382193724,29.4496602426632,2.67267613167568));
#233813=CARTESIAN_POINT('Ctrl Pts',(-51.1771680313593,29.4477266300417,
2.6740383543257));
#233814=CARTESIAN_POINT('Ctrl Pts',(-51.1785609501769,29.446759823731,2.67471946565071));
#233815=CARTESIAN_POINT('Ctrl Pts',(-51.1799618978181,29.4458190608836,
2.6754178138954));
#233816=CARTESIAN_POINT('Ctrl Pts',(-51.1813696738594,29.4449045308659,
2.67613207244186));
#233817=CARTESIAN_POINT('Ctrl Pts',(-51.1817216178697,29.4446758983615,
2.67631063707848));
#233818=CARTESIAN_POINT('Ctrl Pts',(-51.1820739888279,29.4444489051053,
2.67649019601863));
#233819=CARTESIAN_POINT('Ctrl Pts',(-51.182426768326,29.4442235534434,2.67667072836674));
#233820=CARTESIAN_POINT('Ctrl Pts',(-51.1834851068201,29.4435474984577,
2.67721232541108));
#233821=CARTESIAN_POINT('Ctrl Pts',(-51.1845471213153,29.4428862193406,
2.67776268340065));
#233822=CARTESIAN_POINT('Ctrl Pts',(-51.1856123224581,29.4422397658678,
2.67832123541534));
#233823=CARTESIAN_POINT('Ctrl Pts',(-51.1931154617651,29.4376862310783,
2.68225560368461));
#233824=CARTESIAN_POINT('Ctrl Pts',(-51.2007799603596,29.4338145801761,
2.68661792998903));
#233825=CARTESIAN_POINT('Ctrl Pts',(-51.2085065710728,29.4305579784513,
2.69130986622591));
#233826=CARTESIAN_POINT('Ctrl Pts',(-51.2122539689194,29.4289785301339,
2.6935854502307));
#233827=CARTESIAN_POINT('Ctrl Pts',(-51.2160164979699,29.4275440072542,
2.69593918853487));
#233828=CARTESIAN_POINT('Ctrl Pts',(-51.219785247298,29.4262483256618,2.69836306235495));
#233829=CARTESIAN_POINT('Ctrl Pts',(-51.2255549392045,29.4242647276705,
2.70207384382228));
#233830=CARTESIAN_POINT('Ctrl Pts',(-51.2313356805891,29.4226066102323,
2.70594760814228));
#233831=CARTESIAN_POINT('Ctrl Pts',(-51.23708417089,29.4212581193013,2.70995196345707));
#233832=CARTESIAN_POINT('Ctrl Pts',(-51.2397537995244,29.4206318731367,
2.71181160678105));
#233833=CARTESIAN_POINT('Ctrl Pts',(-51.2424163366106,29.4200721889214,
2.713699627721));
#233834=CARTESIAN_POINT('Ctrl Pts',(-51.2450674596718,29.4195787111907,
2.71561183138662));
#233835=CARTESIAN_POINT('Ctrl Pts',(-51.2452706578085,29.419540888067,2.71575839426313));
#233836=CARTESIAN_POINT('Ctrl Pts',(-51.245473795951,29.4195034207002,2.7159050890321));
#233837=CARTESIAN_POINT('Ctrl Pts',(-51.2456768729757,29.4194663081573,
2.71605191409912));
#233838=CARTESIAN_POINT('Ctrl Pts',(-51.2485294929147,29.4189449888201,
2.71811436362754));
#233839=CARTESIAN_POINT('Ctrl Pts',(-51.2513705613629,29.4184957101765,
2.7202009102696));
#233840=CARTESIAN_POINT('Ctrl Pts',(-51.2541954110682,29.4181151898796,
2.72230624862182));
#233841=CARTESIAN_POINT('Ctrl Pts',(-51.264324819729,29.4167507117684,2.72985561753119));
#233842=CARTESIAN_POINT('Ctrl Pts',(-51.2743237313766,29.416257842112,2.73770089914364));
#233843=CARTESIAN_POINT('Ctrl Pts',(-51.2841455249777,29.4165161672808,
2.74574823347125));
#233844=CARTESIAN_POINT('Ctrl Pts',(-51.2949386894587,29.4168000406903,
2.75459144547095));
#233845=CARTESIAN_POINT('Ctrl Pts',(-51.3055186222603,29.4179908989235,
2.7636791175436));
#233846=CARTESIAN_POINT('Ctrl Pts',(-51.3158373135967,29.4199800715341,
2.77292162564838));
#233847=CARTESIAN_POINT('Ctrl Pts',(-51.3269789106022,29.4221278787395,
2.78290121484878));
#233848=CARTESIAN_POINT('Ctrl Pts',(-51.3378170984279,29.4252064644185,
2.79306229500373));
#233849=CARTESIAN_POINT('Ctrl Pts',(-51.3482921445277,29.4291364604209,
2.80331916685476));
#233850=CARTESIAN_POINT('Ctrl Pts',(-51.3586793157524,29.4330334877944,
2.8134899940885));
#233851=CARTESIAN_POINT('Ctrl Pts',(-51.3687106315452,29.4377684584852,
2.82375635966964));
#233852=CARTESIAN_POINT('Ctrl Pts',(-51.3783102687786,29.443310811626,2.83404198860281));
#233853=CARTESIAN_POINT('Origin',(0.00762000000001041,0.0131982271538616,
2.83404198860262));
#233854=CARTESIAN_POINT('Ctrl Pts',(-54.4189959163065,31.4364195775134,
2.65878198860283));
#233855=CARTESIAN_POINT('Ctrl Pts',(-54.4146983388117,31.4438560160004,
2.65878198860283));
#233856=CARTESIAN_POINT('Ctrl Pts',(-54.4098177483009,31.4508673716611,
2.65944603041872));
#233857=CARTESIAN_POINT('Ctrl Pts',(-54.4044907169104,31.4573895320598,
2.66070439264092));
#233858=CARTESIAN_POINT('Ctrl Pts',(-54.4010869974469,31.4615568820651,
2.66150842619617));
#233859=CARTESIAN_POINT('Ctrl Pts',(-54.3975017237409,31.4655251210649,
2.6625542826539));
#233860=CARTESIAN_POINT('Ctrl Pts',(-54.3937759157109,31.4692842169745,
2.66381699700676));
#233861=CARTESIAN_POINT('Ctrl Pts',(-54.3886909353394,31.4744146286225,
2.66554034873276));
#233862=CARTESIAN_POINT('Ctrl Pts',(-54.3833409297222,31.4791503318821,
2.66766759643981));
#233863=CARTESIAN_POINT('Ctrl Pts',(-54.3778174666304,31.4834636394928,
2.67012012783157));
#233864=CARTESIAN_POINT('Ctrl Pts',(-54.3750557350845,31.4856202932981,
2.67134639352745));
#233865=CARTESIAN_POINT('Ctrl Pts',(-54.3722505364143,31.4876715300026,
2.67265375585021));
#233866=CARTESIAN_POINT('Ctrl Pts',(-54.3694125772949,31.4896151854259,
2.67403135126949));
#233867=CARTESIAN_POINT('Ctrl Pts',(-54.3679935977352,31.4905870131376,
2.67472014897913));
#233868=CARTESIAN_POINT('Ctrl Pts',(-54.3665664194001,31.4915319606351,
2.67542649668641));
#233869=CARTESIAN_POINT('Ctrl Pts',(-54.365132326297,31.4924498523887,2.6761489965611));
#233870=CARTESIAN_POINT('Ctrl Pts',(-54.3647738030212,31.4926793253271,
2.67632962152978));
#233871=CARTESIAN_POINT('Ctrl Pts',(-54.3644148473887,31.4929071076039,
2.67651125590959));
#233872=CARTESIAN_POINT('Ctrl Pts',(-54.3640554790923,31.4931331971267,
2.67669387767532));
#233873=CARTESIAN_POINT('Ctrl Pts',(-54.362977374203,31.4938114656952,2.67724174297252));
#233874=CARTESIAN_POINT('Ctrl Pts',(-54.3618955562474,31.4944744978649,
2.67779849504756));
#233875=CARTESIAN_POINT('Ctrl Pts',(-54.3608105487851,31.4951222515527,
2.67836353618017));
#233876=CARTESIAN_POINT('Ctrl Pts',(-54.3533124740222,31.4995986314376,
2.68226832098918));
#233877=CARTESIAN_POINT('Ctrl Pts',(-54.3456575719325,31.5034009004296,
2.68659153751403));
#233878=CARTESIAN_POINT('Ctrl Pts',(-54.3379428492061,31.5065976218803,
2.69123699486192));
#233879=CARTESIAN_POINT('Ctrl Pts',(-54.3341086531876,31.5081863836665,
2.69354577441228));
#233880=CARTESIAN_POINT('Ctrl Pts',(-54.3302591366968,31.5096252947446,
2.69593478828126));
#233881=CARTESIAN_POINT('Ctrl Pts',(-54.3264035847697,31.5109210156001,
2.69839565261225));
#233882=CARTESIAN_POINT('Ctrl Pts',(-54.3178976613387,31.5137795693411,
2.7038246868905));
#233883=CARTESIAN_POINT('Ctrl Pts',(-54.3093672304021,31.515952667503,2.70961155815091));
#233884=CARTESIAN_POINT('Ctrl Pts',(-54.3009559572068,31.5174623893716,
2.71562701361771));
#233885=CARTESIAN_POINT('Ctrl Pts',(-54.2978832130368,31.5180139098087,
2.71782453535861));
#233886=CARTESIAN_POINT('Ctrl Pts',(-54.2948245130135,31.5184846398475,
2.72005051502405));
#233887=CARTESIAN_POINT('Ctrl Pts',(-54.2917835794184,31.5188783726369,
2.72229986760117));
#233888=CARTESIAN_POINT('Ctrl Pts',(-54.2815694052537,31.5202008794131,
2.72985520488892));
#233889=CARTESIAN_POINT('Ctrl Pts',(-54.2714898389044,31.5206547127628,
2.73770845534556));
#233890=CARTESIAN_POINT('Ctrl Pts',(-54.2615918017967,31.5203592886226,
2.74576706701748));
#233891=CARTESIAN_POINT('Ctrl Pts',(-54.2507126865158,31.5200345824972,
2.75462443585025));
#233892=CARTESIAN_POINT('Ctrl Pts',(-54.2400521939113,31.5188048676547,
2.76373036323178));
#233893=CARTESIAN_POINT('Ctrl Pts',(-54.2296591093496,31.5167773687224,
2.77299664636818));
#233894=CARTESIAN_POINT('Ctrl Pts',(-54.2184653119684,31.5145936655007,
2.78297683033481));
#233895=CARTESIAN_POINT('Ctrl Pts',(-54.2075805209337,31.5114844302872,
2.79314401478908));
#233896=CARTESIAN_POINT('Ctrl Pts',(-54.1970658734745,31.5075265408318,
2.80341452427962));
#233897=CARTESIAN_POINT('Ctrl Pts',(-54.1866932092586,31.5036220962478,
2.81354634721382));
#233898=CARTESIAN_POINT('Ctrl Pts',(-54.1766795569337,31.4988909785568,
2.82378004209219));
#233899=CARTESIAN_POINT('Ctrl Pts',(-54.167102037244,31.4933613949858,2.83404198860283));
#233900=CARTESIAN_POINT('Ctrl Pts',(-51.1878102687787,29.7732664904679,
2.83404198860282));
#233901=CARTESIAN_POINT('Ctrl Pts',(-51.1786445298589,29.7679746486352,
2.82422126443019));
#233902=CARTESIAN_POINT('Ctrl Pts',(-51.1699291351222,29.7619788985602,
2.81442815028505));
#233903=CARTESIAN_POINT('Ctrl Pts',(-51.1617065245621,29.7553188532202,
2.80471618166315));
#233904=CARTESIAN_POINT('Ctrl Pts',(-51.1537668706094,29.7488879934681,
2.79533842146229));
#233905=CARTESIAN_POINT('Ctrl Pts',(-51.1462857370529,29.7418369154159,
2.78603515650242));
#233906=CARTESIAN_POINT('Ctrl Pts',(-51.1393284263618,29.7341642916936,
2.77685887346761));
#233907=CARTESIAN_POINT('Ctrl Pts',(-51.1327515888641,29.7269112593592,
2.76818441216595));
#233908=CARTESIAN_POINT('Ctrl Pts',(-51.1266422417913,29.7191021335073,
2.75962261521655));
#233909=CARTESIAN_POINT('Ctrl Pts',(-51.1210907313619,29.7107129315305,
2.75123537701703));
#233910=CARTESIAN_POINT('Ctrl Pts',(-51.11597788339,29.7029866172493,2.7435108713418));
#233911=CARTESIAN_POINT('Ctrl Pts',(-51.1113379461899,29.6947677915906,
2.73593399449926));
#233912=CARTESIAN_POINT('Ctrl Pts',(-51.1072776647607,29.6860256466467,
2.72857657812672));
#233913=CARTESIAN_POINT('Ctrl Pts',(-51.1060669708008,29.6834189154965,
2.72638274508388));
#233914=CARTESIAN_POINT('Ctrl Pts',(-51.1049080895599,29.6807655934596,
2.72420861709636));
#233915=CARTESIAN_POINT('Ctrl Pts',(-51.1038046002594,29.6780647241927,
2.72205663736728));
#233916=CARTESIAN_POINT('Ctrl Pts',(-51.1027123859001,29.6753914511536,
2.71992664556767));
#233917=CARTESIAN_POINT('Ctrl Pts',(-51.1016753170131,29.6726744751146,
2.71782089927885));
#233918=CARTESIAN_POINT('Ctrl Pts',(-51.1006978225842,29.6699160505199,
2.71574387311247));
#233919=CARTESIAN_POINT('Ctrl Pts',(-51.1006298495333,29.6697242350682,
2.71559944077487));
#233920=CARTESIAN_POINT('Ctrl Pts',(-51.1005621526964,29.6695322176089,
2.7154551521607));
#233921=CARTESIAN_POINT('Ctrl Pts',(-51.1004947333605,29.6693399979287,
2.71531100781731));
#233922=CARTESIAN_POINT('Ctrl Pts',(-51.0975388226978,29.6609123829952,
2.70899119176091));
#233923=CARTESIAN_POINT('Ctrl Pts',(-51.095161351427,29.6520916749682,2.70298296066852));
#233924=CARTESIAN_POINT('Ctrl Pts',(-51.0934607157664,29.6429396446301,
2.69736727774156));
#233925=CARTESIAN_POINT('Ctrl Pts',(-51.0918754277622,29.6344083617429,
2.69213248525455));
#233926=CARTESIAN_POINT('Ctrl Pts',(-51.0908783954021,29.6255883681038,
2.68723866185501));
#233927=CARTESIAN_POINT('Ctrl Pts',(-51.0905760611938,29.6165418049905,
2.68278595829599));
#233928=CARTESIAN_POINT('Ctrl Pts',(-51.0904654634291,29.6132324551658,
2.6811571017283));
#233929=CARTESIAN_POINT('Ctrl Pts',(-51.0904480940785,29.6098929659872,
2.67958763637823));
#233930=CARTESIAN_POINT('Ctrl Pts',(-51.0905301191542,29.6065271365691,
2.67808378645367));
#233931=CARTESIAN_POINT('Ctrl Pts',(-51.0905498434446,29.6057177670366,
2.67772216078603));
#233932=CARTESIAN_POINT('Ctrl Pts',(-51.0905756628929,29.6049064053145,
2.67736403603566));
#233933=CARTESIAN_POINT('Ctrl Pts',(-51.0906076352719,29.6040931741702,
2.67700956934482));
#233934=CARTESIAN_POINT('Ctrl Pts',(-51.0906386085139,29.6033053564991,
2.67666617973806));
#233935=CARTESIAN_POINT('Ctrl Pts',(-51.090675356124,29.6025157844404,2.67632622314122));
#233936=CARTESIAN_POINT('Ctrl Pts',(-51.0907179287117,29.6017245728792,
2.67598984158776));
#233937=CARTESIAN_POINT('Ctrl Pts',(-51.0911843606098,29.5930559358438,
2.67230439292223));
#233938=CARTESIAN_POINT('Ctrl Pts',(-51.0923507190417,29.5841848213175,
2.66904964539975));
#233939=CARTESIAN_POINT('Ctrl Pts',(-51.0942731997207,29.575291162817,2.66640203566724));
#233940=CARTESIAN_POINT('Ctrl Pts',(-51.0950705097612,29.5716026975454,
2.6653039929944));
#233941=CARTESIAN_POINT('Ctrl Pts',(-51.0959974771975,29.5679105139262,
2.6643099514226));
#233942=CARTESIAN_POINT('Ctrl Pts',(-51.0970562972092,29.5642276868789,
2.66343053473361));
#233943=CARTESIAN_POINT('Ctrl Pts',(-51.0988622250759,29.5579462415721,
2.66193059792884));
#233944=CARTESIAN_POINT('Ctrl Pts',(-51.1010529624042,29.5516941764754,
2.66076519817127));
#233945=CARTESIAN_POINT('Ctrl Pts',(-51.1036389246278,29.5455435225217,
2.65997805604458));
#233946=CARTESIAN_POINT('Ctrl Pts',(-51.1049319057396,29.5424681955448,
2.65958448498124));
#233947=CARTESIAN_POINT('Ctrl Pts',(-51.106324978508,29.5394188854257,2.6592852626076));
#233948=CARTESIAN_POINT('Ctrl Pts',(-51.107819466813,29.5364046579956,2.65908463971322));
#233949=CARTESIAN_POINT('Ctrl Pts',(-51.109313955118,29.5333904305654,2.65888401681884));
#233950=CARTESIAN_POINT('Ctrl Pts',(-51.1109098228568,29.5304113137792,
2.65878198860281));
#233951=CARTESIAN_POINT('Ctrl Pts',(-51.1126068659049,29.5274749692184,
2.65878198860281));
#233952=CARTESIAN_POINT('Origin',(-53.2328030451449,23.6840886581935,2.83404198860278));
#233953=CARTESIAN_POINT('Ctrl Pts',(-57.3172883154491,25.3107727110821,
2.83404198860279));
#233954=CARTESIAN_POINT('Ctrl Pts',(-57.3269813337898,25.3150883208946,
2.82419652440072));
#233955=CARTESIAN_POINT('Ctrl Pts',(-57.3363050752412,25.320155936947,2.81438790575652));
#233956=CARTESIAN_POINT('Ctrl Pts',(-57.3452135417184,25.325938468362,2.80466781256901));
#233957=CARTESIAN_POINT('Ctrl Pts',(-57.3538325360815,25.3315331019387,
2.79526356453079));
#233958=CARTESIAN_POINT('Ctrl Pts',(-57.3620638476581,25.3377977038122,
2.78594102496236));
#233959=CARTESIAN_POINT('Ctrl Pts',(-57.3698434251117,25.3447390861656,
2.77675109088786));
#233960=CARTESIAN_POINT('Ctrl Pts',(-57.377202426344,25.3513052064463,2.76805797913696));
#233961=CARTESIAN_POINT('Ctrl Pts',(-57.3841579102018,25.3584775246719,
2.75948271210182));
#233962=CARTESIAN_POINT('Ctrl Pts',(-57.3906233351701,25.3662887884603,
2.7510857557325));
#233963=CARTESIAN_POINT('Ctrl Pts',(-57.3965784591573,25.3734835273345,
2.74335155163304));
#233964=CARTESIAN_POINT('Ctrl Pts',(-57.4021181432104,25.381220796889,2.73576818685985));
#233965=CARTESIAN_POINT('Ctrl Pts',(-57.4071400767283,25.3895423083614,
2.72840626160544));
#233966=CARTESIAN_POINT('Ctrl Pts',(-57.4085967487436,25.3919560625149,
2.72627084693717));
#233967=CARTESIAN_POINT('Ctrl Pts',(-57.410009604778,25.3944190600991,2.7241542458755));
#233968=CARTESIAN_POINT('Ctrl Pts',(-57.4113754784548,25.3969325220924,
2.72205867173276));
#233969=CARTESIAN_POINT('Ctrl Pts',(-57.4128561733382,25.3996572764942,
2.71978693462878));
#233970=CARTESIAN_POINT('Ctrl Pts',(-57.4142805418441,25.4024370309187,
2.71754411340779));
#233971=CARTESIAN_POINT('Ctrl Pts',(-57.4156446191418,25.4052723227226,
2.71533341844275));
#233972=CARTESIAN_POINT('Ctrl Pts',(-57.4193883399888,25.4130538033265,
2.70926614876421));
#233973=CARTESIAN_POINT('Ctrl Pts',(-57.4226343338643,25.4212623406656,
2.70347381860439));
#233974=CARTESIAN_POINT('Ctrl Pts',(-57.4253008212879,25.4298341608309,
2.69804914171424));
#233975=CARTESIAN_POINT('Ctrl Pts',(-57.4277405125135,25.4376769109071,
2.69308585687241));
#233976=CARTESIAN_POINT('Ctrl Pts',(-57.4296843862653,25.4458193604263,
2.68842799053228));
#233977=CARTESIAN_POINT('Ctrl Pts',(-57.4310470526568,25.4542377154367,
2.68414767054265));
#233978=CARTESIAN_POINT('Ctrl Pts',(-57.431716389937,25.4583727839182,2.68204519134592));
#233979=CARTESIAN_POINT('Ctrl Pts',(-57.4322449980039,25.4625743171739,
2.68003431778535));
#233980=CARTESIAN_POINT('Ctrl Pts',(-57.4326195921323,25.466838401935,2.67812693945279));
#233981=CARTESIAN_POINT('Ctrl Pts',(-57.4326906677196,25.4676474704857,
2.67776503299231));
#233982=CARTESIAN_POINT('Ctrl Pts',(-57.4327558640764,25.4684592045964,
2.67740659639951));
#233983=CARTESIAN_POINT('Ctrl Pts',(-57.4328151061497,25.4692734860654,
2.67705178968882));
#233984=CARTESIAN_POINT('Ctrl Pts',(-57.4328724969081,25.4700623212384,
2.67670807068784));
#233985=CARTESIAN_POINT('Ctrl Pts',(-57.4329242997219,25.4708535470245,
2.67636775825292));
#233986=CARTESIAN_POINT('Ctrl Pts',(-57.4329704479395,25.4716470524589,
2.67603099699282));
#233987=CARTESIAN_POINT('Ctrl Pts',(-57.4334733617058,25.4802945111771,
2.67236104217153));
#233988=CARTESIAN_POINT('Ctrl Pts',(-57.433304654289,25.4892184175053,2.66911440541498));
#233989=CARTESIAN_POINT('Ctrl Pts',(-57.4323852136914,25.4982455208445,
2.66646778189654));
#233990=CARTESIAN_POINT('Ctrl Pts',(-57.4319969282176,25.5020577226402,
2.66535009634999));
#233991=CARTESIAN_POINT('Ctrl Pts',(-57.4314751387428,25.5058881199466,
2.66433897912371));
#233992=CARTESIAN_POINT('Ctrl Pts',(-57.4308157710841,25.5097232095986,
2.66344564884821));
#233993=CARTESIAN_POINT('Ctrl Pts',(-57.4297054124227,25.516181404744,2.66194130298614));
#233994=CARTESIAN_POINT('Ctrl Pts',(-57.4282034292357,25.5226508554408,
2.66077206705449));
#233995=CARTESIAN_POINT('Ctrl Pts',(-57.4262902109369,25.5290599831063,
2.65998225155744));
#233996=CARTESIAN_POINT('Ctrl Pts',(-57.4258119063623,25.5306622650227,
2.65978479768317));
#233997=CARTESIAN_POINT('Ctrl Pts',(-57.4253076802624,25.5322606952869,
2.65961098966652));
#233998=CARTESIAN_POINT('Ctrl Pts',(-57.4247769415291,25.533854036701,2.65946139030531));
#233999=CARTESIAN_POINT('Ctrl Pts',(-57.4239808334291,25.536244048822,2.6592369912635));
#234000=CARTESIAN_POINT('Ctrl Pts',(-57.423125065972,25.5386225912894,2.65906707562471));
#234001=CARTESIAN_POINT('Ctrl Pts',(-57.4222091845947,25.5409861542582,
2.65895332562949));
#234002=CARTESIAN_POINT('Ctrl Pts',(-57.4212933032174,25.543349717227,2.65883957563427));
#234003=CARTESIAN_POINT('Ctrl Pts',(-57.4203173191902,25.5456982979278,
2.65878198860279));
#234004=CARTESIAN_POINT('Ctrl Pts',(-57.419280924679,25.5480287005717,2.65878198860279));
#234005=CARTESIAN_POINT('Ctrl Pts',(-53.9314655730806,23.9951532569806,
2.65878198860278));
#234006=CARTESIAN_POINT('Ctrl Pts',(-53.9349721992637,23.9872677980945,
2.65878198860278));
#234007=CARTESIAN_POINT('Ctrl Pts',(-53.9390993428069,23.9797401457393,
2.65945335517867));
#234008=CARTESIAN_POINT('Ctrl Pts',(-53.943719374479,23.9726512030275,2.66072561226607));
#234009=CARTESIAN_POINT('Ctrl Pts',(-53.9467034408968,23.968072473403,2.66154735980347));
#234010=CARTESIAN_POINT('Ctrl Pts',(-53.9498923541889,23.963676246713,2.66261895766895));
#234011=CARTESIAN_POINT('Ctrl Pts',(-53.9532454491207,23.959478076992,2.66391429251045));
#234012=CARTESIAN_POINT('Ctrl Pts',(-53.9576897843755,23.9539136435132,
2.66563118464141));
#234013=CARTESIAN_POINT('Ctrl Pts',(-53.9624262550346,23.9487016177219,
2.66774105138716));
#234014=CARTESIAN_POINT('Ctrl Pts',(-53.9673725153422,23.9438784851452,
2.67016894181766));
#234015=CARTESIAN_POINT('Ctrl Pts',(-53.9698456454959,23.9414669188569,
2.67138288703291));
#234016=CARTESIAN_POINT('Ctrl Pts',(-53.972371302523,23.9391523931035,2.67267613167568));
#234017=CARTESIAN_POINT('Ctrl Pts',(-53.9749397614923,23.9369381736874,
2.67403835432569));
#234018=CARTESIAN_POINT('Ctrl Pts',(-53.9762239909769,23.9358310639794,
2.6747194656507));
#234019=CARTESIAN_POINT('Ctrl Pts',(-53.9775189275857,23.9347490158252,
2.67541781389539));
#234020=CARTESIAN_POINT('Ctrl Pts',(-53.9788233972651,23.9336923430325,
2.67613207244185));
#234021=CARTESIAN_POINT('Ctrl Pts',(-53.9791495146849,23.9334281748343,
2.67631063707846));
#234022=CARTESIAN_POINT('Ctrl Pts',(-53.979476228062,23.9331655922761,2.67649019601861));
#234023=CARTESIAN_POINT('Ctrl Pts',(-53.9798035193341,23.9329045996154,
2.67667072836672));
#234024=CARTESIAN_POINT('Ctrl Pts',(-53.9807853931504,23.9321216216332,
2.67721232541106));
#234025=CARTESIAN_POINT('Ctrl Pts',(-53.9817724673293,23.9313529543291,
2.67776268340063));
#234026=CARTESIAN_POINT('Ctrl Pts',(-53.9827642604006,23.9305986983576,
2.67832123541532));
#234027=CARTESIAN_POINT('Ctrl Pts',(-53.9897503227314,23.9252858166867,
2.68225560368453));
#234028=CARTESIAN_POINT('Ctrl Pts',(-53.9969681366814,23.9206342168335,
2.68661792998889));
#234029=CARTESIAN_POINT('Ctrl Pts',(-54.0043120126388,23.9165878043696,
2.6913098662257));
#234030=CARTESIAN_POINT('Ctrl Pts',(-54.0078737845426,23.9146252986971,
2.69358545023054));
#234031=CARTESIAN_POINT('Ctrl Pts',(-54.0114657535932,23.9128053429042,
2.69593918853477));
#234032=CARTESIAN_POINT('Ctrl Pts',(-54.0150784217126,23.9111228176154,
2.69836306235491));
#234033=CARTESIAN_POINT('Ctrl Pts',(-54.0206091641933,23.9085469889529,
2.70207384382224));
#234034=CARTESIAN_POINT('Ctrl Pts',(-54.026184917604,23.906293702842,2.70594760814225));
#234035=CARTESIAN_POINT('Ctrl Pts',(-54.0317609613888,23.9043517182282,
2.70995196345704));
#234036=CARTESIAN_POINT('Ctrl Pts',(-54.0343505049691,23.903449850527,2.71181160678102));
#234037=CARTESIAN_POINT('Ctrl Pts',(-54.0369399534675,23.9026149214104,
2.71369962772095));
#234038=CARTESIAN_POINT('Ctrl Pts',(-54.0395249709304,23.9018470291827,
2.71561183138658));
#234039=CARTESIAN_POINT('Ctrl Pts',(-54.0397231023334,23.9017881732691,
2.71575839426308));
#234040=CARTESIAN_POINT('Ctrl Pts',(-54.0399212112576,23.9017296774346,
2.71590508903205));
#234041=CARTESIAN_POINT('Ctrl Pts',(-54.040119296488,23.9016715408687,2.71605191409908));
#234042=CARTESIAN_POINT('Ctrl Pts',(-54.0429017967674,23.9008548973949,
2.71811436362749));
#234043=CARTESIAN_POINT('Ctrl Pts',(-54.0456803391391,23.9001111074278,
2.72020091026955));
#234044=CARTESIAN_POINT('Ctrl Pts',(-54.0484499388203,23.8994373944623,
2.72230624862178));
#234045=CARTESIAN_POINT('Ctrl Pts',(-54.0583812307207,23.8970215795837,
2.72985561753132));
#234046=CARTESIAN_POINT('Ctrl Pts',(-54.0682738483765,23.89548623905,2.73770089914395));
#234047=CARTESIAN_POINT('Ctrl Pts',(-54.0780688394977,23.8947164920949,
2.74574823347176));
#234048=CARTESIAN_POINT('Ctrl Pts',(-54.0888325507458,23.8938706175191,
2.75459144547153));
#234049=CARTESIAN_POINT('Ctrl Pts',(-54.0994790041496,23.8939490479891,
2.76367911754426));
#234050=CARTESIAN_POINT('Ctrl Pts',(-54.1099490937715,23.8948487267558,
2.77292162564911));
#234051=CARTESIAN_POINT('Ctrl Pts',(-54.1212541629292,23.8958201540353,
2.78290121484939));
#234052=CARTESIAN_POINT('Ctrl Pts',(-54.1323547778578,23.8977489757819,
2.7930622950042));
#234053=CARTESIAN_POINT('Ctrl Pts',(-54.1431832370017,23.9005625023835,
2.80331916685509));
#234054=CARTESIAN_POINT('Ctrl Pts',(-54.1539208564981,23.9033524263874,
2.81348999408871));
#234055=CARTESIAN_POINT('Ctrl Pts',(-54.1643921589032,23.9070129003889,
2.82375635966972));
#234056=CARTESIAN_POINT('Ctrl Pts',(-54.1745185419761,23.9115214566113,
2.83404198860278));
#234057=CARTESIAN_POINT('Origin',(0.00619866644048587,0.0139224327746604,
2.83404198860262));
#234058=CARTESIAN_POINT('Ctrl Pts',(-57.4068835917981,25.5758735661207,
2.65878198860279));
#234059=CARTESIAN_POINT('Ctrl Pts',(-57.4033868763699,25.5837184861905,
2.65878198860279));
#234060=CARTESIAN_POINT('Ctrl Pts',(-57.3992659084775,25.5912015935367,
2.6594460304186));
#234061=CARTESIAN_POINT('Ctrl Pts',(-57.3946498105263,25.598244851263,2.66070439264066));
#234062=CARTESIAN_POINT('Ctrl Pts',(-57.3917003436859,25.6027451576543,
2.66150842619593));
#234063=CARTESIAN_POINT('Ctrl Pts',(-57.3885495044087,25.607066421377,2.66255428265373));
#234064=CARTESIAN_POINT('Ctrl Pts',(-57.3852370392633,25.611194377554,2.6638169970067));
#234065=CARTESIAN_POINT('Ctrl Pts',(-57.3807161889918,25.6168282094542,
2.6655403487327));
#234066=CARTESIAN_POINT('Ctrl Pts',(-57.3758905070494,25.6220971979014,
2.66766759643975));
#234067=CARTESIAN_POINT('Ctrl Pts',(-57.3708481654825,25.6269642358706,
2.67012012783151));
#234068=CARTESIAN_POINT('Ctrl Pts',(-57.368326994699,25.6293977548552,2.67134639352739));
#234069=CARTESIAN_POINT('Ctrl Pts',(-57.3657515758212,25.6317309777765,
2.67265375585015));
#234070=CARTESIAN_POINT('Ctrl Pts',(-57.3631323306533,25.6339606331577,
2.67403135126943));
#234071=CARTESIAN_POINT('Ctrl Pts',(-57.3618227080693,25.6350754608483,
2.67472014897907));
#234072=CARTESIAN_POINT('Ctrl Pts',(-57.3605021218763,25.6361644125826,
2.67542649668636));
#234073=CARTESIAN_POINT('Ctrl Pts',(-57.3591718306997,25.6372271795775,
2.67614899656105));
#234074=CARTESIAN_POINT('Ctrl Pts',(-57.3588392579055,25.6374928713262,
2.67632962152972));
#234075=CARTESIAN_POINT('Ctrl Pts',(-57.3585060784009,25.6377569268684,
2.67651125590953));
#234076=CARTESIAN_POINT('Ctrl Pts',(-57.358172311552,25.638019342065,2.67669387767526));
#234077=CARTESIAN_POINT('Ctrl Pts',(-57.3571710110052,25.6388065876546,
2.67724174297247));
#234078=CARTESIAN_POINT('Ctrl Pts',(-57.3561644250954,25.6395790684331,
2.6777984950475));
#234079=CARTESIAN_POINT('Ctrl Pts',(-57.3551530701151,25.6403366878211,
2.67836353618012));
#234080=CARTESIAN_POINT('Ctrl Pts',(-57.3481639797007,25.645572307861,2.68226832098908));
#234081=CARTESIAN_POINT('Ctrl Pts',(-57.3409484573003,25.6501539027775,
2.68659153751388));
#234082=CARTESIAN_POINT('Ctrl Pts',(-57.333610145013,25.6541395203647,2.69123699486171));
#234083=CARTESIAN_POINT('Ctrl Pts',(-57.3299630239494,25.6561203613653,
2.69354577441212));
#234084=CARTESIAN_POINT('Ctrl Pts',(-57.3262850026764,25.6579537739811,
2.69593478828116));
#234085=CARTESIAN_POINT('Ctrl Pts',(-57.322586011576,25.6596454116602,2.69839565261221));
#234086=CARTESIAN_POINT('Ctrl Pts',(-57.3144254847133,25.6633774170497,
2.70382468689046));
#234087=CARTESIAN_POINT('Ctrl Pts',(-57.3061689349813,25.6664302835893,
2.70961155815087));
#234088=CARTESIAN_POINT('Ctrl Pts',(-57.2979615485275,25.6688109525047,
2.71562701361767));
#234089=CARTESIAN_POINT('Ctrl Pts',(-57.2949632867553,25.6696806408813,
2.71782453535858));
#234090=CARTESIAN_POINT('Ctrl Pts',(-57.2919705472984,25.6704685134247,
2.72005051502402));
#234091=CARTESIAN_POINT('Ctrl Pts',(-57.2889874285391,25.6711779534203,
2.72229986760115));
#234092=CARTESIAN_POINT('Ctrl Pts',(-57.2789674482906,25.673560887295,2.72985520488863));
#234093=CARTESIAN_POINT('Ctrl Pts',(-57.2689905373634,25.675065836079,2.73770845534497));
#234094=CARTESIAN_POINT('Ctrl Pts',(-57.2591158425076,25.6758066569114,
2.74576706701659));
#234095=CARTESIAN_POINT('Ctrl Pts',(-57.2482623831266,25.6766209067622,
2.75462443584905));
#234096=CARTESIAN_POINT('Ctrl Pts',(-57.2375317496135,25.676512253336,2.76373036323026));
#234097=CARTESIAN_POINT('Ctrl Pts',(-57.2269836681092,25.6755822344129,
2.77299664636632));
#234098=CARTESIAN_POINT('Ctrl Pts',(-57.2156229323795,25.6745805641845,
2.78297683033263));
#234099=CARTESIAN_POINT('Ctrl Pts',(-57.2044727657904,25.6726261321668,
2.79314401478657));
#234100=CARTESIAN_POINT('Ctrl Pts',(-57.1936020065678,25.6697890043849,
2.80341452427681));
#234101=CARTESIAN_POINT('Ctrl Pts',(-57.1828780392985,25.6669901874072,
2.81354634721189));
#234102=CARTESIAN_POINT('Ctrl Pts',(-57.1724247063461,25.6633316989629,
2.82378004209119));
#234103=CARTESIAN_POINT('Ctrl Pts',(-57.1623216544372,25.658833530444,2.83404198860278));
#234104=CARTESIAN_POINT('Ctrl Pts',(-54.0195518809642,24.2595822759732,
2.83404198860278));
#234105=CARTESIAN_POINT('Ctrl Pts',(-54.0098832048258,24.2552775040074,
2.82422126442931));
#234106=CARTESIAN_POINT('Ctrl Pts',(-54.0005888273912,24.2502256060967,
2.81442815028334));
#234107=CARTESIAN_POINT('Ctrl Pts',(-53.9917150968467,24.2444615420273,
2.80471618166061));
#234108=CARTESIAN_POINT('Ctrl Pts',(-53.9831467292612,24.2388958310238,
2.79533842145915));
#234109=CARTESIAN_POINT('Ctrl Pts',(-53.9749695397835,24.2326653709086,
2.7860351564987));
#234110=CARTESIAN_POINT('Ctrl Pts',(-53.9672483344011,24.2257620156162,
2.77685887346333));
#234111=CARTESIAN_POINT('Ctrl Pts',(-53.9599493771831,24.219236182868,2.76818441216119));
#234112=CARTESIAN_POINT('Ctrl Pts',(-53.9530572218277,24.2121084368851,
2.75962261521134));
#234113=CARTESIAN_POINT('Ctrl Pts',(-53.9466592127625,24.2043454826878,
2.75123537701141));
#234114=CARTESIAN_POINT('Ctrl Pts',(-53.9407667537481,24.1971959321054,
2.74351087133577));
#234115=CARTESIAN_POINT('Ctrl Pts',(-53.9352931333934,24.1895071355379,
2.73593399449286));
#234116=CARTESIAN_POINT('Ctrl Pts',(-53.930341291634,24.181237295956,2.72857657812));
#234117=CARTESIAN_POINT('Ctrl Pts',(-53.9288647523826,24.1787713967333,
2.72638274507943));
#234118=CARTESIAN_POINT('Ctrl Pts',(-53.9274348719409,24.1762537459499,
2.72420861709414));
#234119=CARTESIAN_POINT('Ctrl Pts',(-53.9260551099577,24.1736830183709,
2.72205663736723));
#234120=CARTESIAN_POINT('Ctrl Pts',(-53.9246894457403,24.1711385572897,
2.71992664556762));
#234121=CARTESIAN_POINT('Ctrl Pts',(-53.9233740566951,24.1685448683468,
2.71782089927881));
#234122=CARTESIAN_POINT('Ctrl Pts',(-53.9221135831989,24.1659037306811,
2.71574387311243));
#234123=CARTESIAN_POINT('Ctrl Pts',(-53.9220259323371,24.1657200711331,
2.71559944077483));
#234124=CARTESIAN_POINT('Ctrl Pts',(-53.9219385350607,24.1655361818119,
2.71545515216065));
#234125=CARTESIAN_POINT('Ctrl Pts',(-53.9218513926272,24.1653520623708,
2.71531100781727));
#234126=CARTESIAN_POINT('Ctrl Pts',(-53.9180307491143,24.1572795915927,
2.70899119176075));
#234127=CARTESIAN_POINT('Ctrl Pts',(-53.9147442868248,24.1487557177454,
2.70298296066826));
#234128=CARTESIAN_POINT('Ctrl Pts',(-53.9120963197572,24.1398315880191,
2.6973672777412));
#234129=CARTESIAN_POINT('Ctrl Pts',(-53.9096279542367,24.1315127481108,
2.69213248525402));
#234130=CARTESIAN_POINT('Ctrl Pts',(-53.9077144433429,24.1228452895799,
2.68723866185433));
#234131=CARTESIAN_POINT('Ctrl Pts',(-53.9064681420131,24.1138798870157,
2.6827859582952));
#234132=CARTESIAN_POINT('Ctrl Pts',(-53.9060122288629,24.1106002267705,
2.68115710172776));
#234133=CARTESIAN_POINT('Ctrl Pts',(-53.9056458829916,24.107280847255,2.67958763637793));
#234134=CARTESIAN_POINT('Ctrl Pts',(-53.9053756337487,24.103924882248,2.6780837864536));
#234135=CARTESIAN_POINT('Ctrl Pts',(-53.905310647834,24.1031178847767,2.67772216078595));
#234136=CARTESIAN_POINT('Ctrl Pts',(-53.9052515154467,24.1023082689118,
2.67736403603558));
#234137=CARTESIAN_POINT('Ctrl Pts',(-53.9051983068757,24.1014961507091,
2.67700956934474));
#234138=CARTESIAN_POINT('Ctrl Pts',(-53.9051467610726,24.1007094112003,
2.67666617973799));
#234139=CARTESIAN_POINT('Ctrl Pts',(-53.9051007746215,24.0999203233287,
2.67632622314114));
#234140=CARTESIAN_POINT('Ctrl Pts',(-53.9050604098635,24.0991289960601,
2.67598984158768));
#234141=CARTESIAN_POINT('Ctrl Pts',(-53.904618167291,24.0904590913162,2.67230439292231));
#234142=CARTESIAN_POINT('Ctrl Pts',(-53.9048508523205,24.0815146560294,
2.66904964539997));
#234143=CARTESIAN_POINT('Ctrl Pts',(-53.9058331609931,24.0724687639701,
2.66640203566752));
#234144=CARTESIAN_POINT('Ctrl Pts',(-53.9062405536792,24.0687171629035,
2.66530399299454));
#234145=CARTESIAN_POINT('Ctrl Pts',(-53.9067765048111,24.0649483109704,
2.66430995142262));
#234146=CARTESIAN_POINT('Ctrl Pts',(-53.9074445642443,24.061174982006,2.66343053473355));
#234147=CARTESIAN_POINT('Ctrl Pts',(-53.9085840092242,24.0547391762491,
2.66193059792878));
#234148=CARTESIAN_POINT('Ctrl Pts',(-53.9101092267074,24.0482923662128,
2.66076519817121));
#234149=CARTESIAN_POINT('Ctrl Pts',(-53.9120381043537,24.0419050995278,
2.65997805604453));
#234150=CARTESIAN_POINT('Ctrl Pts',(-53.9130025431768,24.0387114661853,
2.6595844849812));
#234151=CARTESIAN_POINT('Ctrl Pts',(-53.914069244846,24.0355332447503,2.65928526260756));
#234152=CARTESIAN_POINT('Ctrl Pts',(-53.9152404736264,24.0323793130075,
2.65908463971318));
#234153=CARTESIAN_POINT('Ctrl Pts',(-53.9164117024068,24.0292253812647,
2.6588840168188));
#234154=CARTESIAN_POINT('Ctrl Pts',(-53.9176874253155,24.0260957707896,
2.65878198860278));
#234155=CARTESIAN_POINT('Ctrl Pts',(-53.9190682401996,24.0229981225296,
2.65878198860278));
#234156=CARTESIAN_POINT('Origin',(-55.4168495715593,17.9900016446781,2.83404198860273));
#234157=CARTESIAN_POINT('Ctrl Pts',(-59.6489943884565,19.180829583578,2.83404198860275));
#234158=CARTESIAN_POINT('Ctrl Pts',(-59.6590854114905,19.1841083557169,
2.82419652440111));
#234159=CARTESIAN_POINT('Ctrl Pts',(-59.668887786629,19.1881736144725,2.81438790575719));
#234160=CARTESIAN_POINT('Ctrl Pts',(-59.6783518907173,19.1929932802644,
2.80466781256988));
#234161=CARTESIAN_POINT('Ctrl Pts',(-59.6875084677778,19.1976563356173,
2.79526356453173));
#234162=CARTESIAN_POINT('Ctrl Pts',(-59.696349516575,19.2030262129964,2.78594102496329));
#234163=CARTESIAN_POINT('Ctrl Pts',(-59.7048120487195,19.2091163824548,
2.77675109088875));
#234164=CARTESIAN_POINT('Ctrl Pts',(-59.7128170830356,19.2148773077515,
2.7680579791377));
#234165=CARTESIAN_POINT('Ctrl Pts',(-59.7204841754272,19.2212832892285,
2.75948271210239));
#234166=CARTESIAN_POINT('Ctrl Pts',(-59.727730681521,19.2283759411603,2.75108575573291));
#234167=CARTESIAN_POINT('Ctrl Pts',(-59.734405237714,19.2349087865432,2.74335155163326));
#234168=CARTESIAN_POINT('Ctrl Pts',(-59.7407233396947,19.2420246158646,
2.73576818685987));
#234169=CARTESIAN_POINT('Ctrl Pts',(-59.7465875973417,19.2497756062333,
2.72840626160534));
#234170=CARTESIAN_POINT('Ctrl Pts',(-59.7482885955677,19.2520238739017,
2.72627084693707));
#234171=CARTESIAN_POINT('Ctrl Pts',(-59.7499511651814,19.2543256952573,
2.72415424587541));
#234172=CARTESIAN_POINT('Ctrl Pts',(-59.751572284779,19.2566826155664,2.72205867173268));
#234173=CARTESIAN_POINT('Ctrl Pts',(-59.7533296826513,19.2592376687177,
2.71978693462871));
#234174=CARTESIAN_POINT('Ctrl Pts',(-59.7550368117758,19.2618533083055,
2.71754411340772));
#234175=CARTESIAN_POINT('Ctrl Pts',(-59.7566897852105,19.2645304831806,
2.7153334184427));
#234176=CARTESIAN_POINT('Ctrl Pts',(-59.7612263837726,19.2718780106326,
2.70926614876418));
#234177=CARTESIAN_POINT('Ctrl Pts',(-59.7653126215477,19.2797022819936,
2.70347381860435));
#234178=CARTESIAN_POINT('Ctrl Pts',(-59.7688605008635,19.2879484209985,
2.69804914171422));
#234179=CARTESIAN_POINT('Ctrl Pts',(-59.7721066178187,19.2954931904948,
2.6930858568722));
#234180=CARTESIAN_POINT('Ctrl Pts',(-59.7748909605621,19.3033878446879,
2.6884279905319));
#234181=CARTESIAN_POINT('Ctrl Pts',(-59.7771261198371,19.3116176456452,
2.68414767054214));
#234182=CARTESIAN_POINT('Ctrl Pts',(-59.7782240227714,19.3156600969913,
2.6820451913456));
#234183=CARTESIAN_POINT('Ctrl Pts',(-59.7791889148824,19.319783359219,2.68003431778522));
#234184=CARTESIAN_POINT('Ctrl Pts',(-59.7800071751723,19.3239849291286,
2.67812693945282));
#234185=CARTESIAN_POINT('Ctrl Pts',(-59.7801624320924,19.3247821360952,
2.67776503299234));
#234186=CARTESIAN_POINT('Ctrl Pts',(-59.780312120616,19.3255826085666,2.67740659639954));
#234187=CARTESIAN_POINT('Ctrl Pts',(-59.7804561537455,19.3263862368335,
2.67705178968885));
#234188=CARTESIAN_POINT('Ctrl Pts',(-59.7805956858398,19.3271647517172,
2.67670807068788));
#234189=CARTESIAN_POINT('Ctrl Pts',(-59.7807299104879,19.3279462282172,
2.67636775825295));
#234190=CARTESIAN_POINT('Ctrl Pts',(-59.7808587498043,19.3287305629435,
2.67603099699285));
#234191=CARTESIAN_POINT('Ctrl Pts',(-59.7822628141274,19.3372780811748,
2.6723610421716));
#234192=CARTESIAN_POINT('Ctrl Pts',(-59.7830278331223,19.3461707361373,
2.66911440541507));
#234193=CARTESIAN_POINT('Ctrl Pts',(-59.7830570185564,19.3552444957726,
2.66646778189664));
#234194=CARTESIAN_POINT('Ctrl Pts',(-59.7830693437464,19.3590764008119,
2.66535009635006));
#234195=CARTESIAN_POINT('Ctrl Pts',(-59.7829507982331,19.3629403566532,
2.66433897912374));
#234196=CARTESIAN_POINT('Ctrl Pts',(-59.7826959186873,19.3668233599709,
2.66344564884821));
#234197=CARTESIAN_POINT('Ctrl Pts',(-59.7822667079008,19.3733622405321,
2.66194130298614));
#234198=CARTESIAN_POINT('Ctrl Pts',(-59.7814491944743,19.3799532508955,
2.66077206705447));
#234199=CARTESIAN_POINT('Ctrl Pts',(-59.7802163932509,19.3865272544576,
2.65998225155741));
#234200=CARTESIAN_POINT('Ctrl Pts',(-59.7799081929451,19.3881707553481,
2.65978479768314));
#234201=CARTESIAN_POINT('Ctrl Pts',(-59.7795738105078,19.3898131352235,
2.65961098966648));
#234202=CARTESIAN_POINT('Ctrl Pts',(-59.7792125287463,19.3914532254508,
2.65946139030528));
#234203=CARTESIAN_POINT('Ctrl Pts',(-59.7786706061041,19.3939133607916,
2.65923699126346));
#234204=CARTESIAN_POINT('Ctrl Pts',(-59.7780681520195,19.3963683254117,
2.65906707562467));
#234205=CARTESIAN_POINT('Ctrl Pts',(-59.7774043475413,19.3988146762082,
2.65895332562945));
#234206=CARTESIAN_POINT('Ctrl Pts',(-59.7767405430631,19.4012610270047,
2.65883957563423));
#234207=CARTESIAN_POINT('Ctrl Pts',(-59.7760153991119,19.4036987600458,
2.65878198860274));
#234208=CARTESIAN_POINT('Ctrl Pts',(-59.7752282754854,19.4061247292258,
2.65878198860274));
#234209=CARTESIAN_POINT('Ctrl Pts',(-56.1441998575528,18.2263320786581,
2.65878198860274));
#234210=CARTESIAN_POINT('Ctrl Pts',(-56.1468630191714,18.2181232748943,
2.65878198860274));
#234211=CARTESIAN_POINT('Ctrl Pts',(-56.1501806998579,18.2102054558339,
2.65945335517868));
#234212=CARTESIAN_POINT('Ctrl Pts',(-56.1540344262254,18.2026724222809,
2.66072561226617));
#234213=CARTESIAN_POINT('Ctrl Pts',(-56.1565235380436,18.1978068555396,
2.66154735980354));
#234214=CARTESIAN_POINT('Ctrl Pts',(-56.1592354513148,18.1931013796338,
2.66261895766897));
#234215=CARTESIAN_POINT('Ctrl Pts',(-56.1621313494121,18.1885757140657,
2.66391429251038));
#234216=CARTESIAN_POINT('Ctrl Pts',(-56.1659696964528,18.1825772036012,
2.66563118464135));
#234217=CARTESIAN_POINT('Ctrl Pts',(-56.1701354151837,18.1768986338332,
2.6677410513871));
#234218=CARTESIAN_POINT('Ctrl Pts',(-56.1745504247233,18.1715848978926,
2.67016894181761));
#234219=CARTESIAN_POINT('Ctrl Pts',(-56.1767579294932,18.1689280299222,
2.67138288703287));
#234220=CARTESIAN_POINT('Ctrl Pts',(-56.1790278168866,18.1663621803354,
2.67267613167563));
#234221=CARTESIAN_POINT('Ctrl Pts',(-56.181350756616,18.1638916135758,2.67403835432565));
#234222=CARTESIAN_POINT('Ctrl Pts',(-56.1825122264807,18.1626563301961,
2.67471946565066));
#234223=CARTESIAN_POINT('Ctrl Pts',(-56.1836869644605,18.1614448518812,
2.67541781389535));
#234224=CARTESIAN_POINT('Ctrl Pts',(-56.1848738357353,18.1602576134416,
2.67613207244181));
#234225=CARTESIAN_POINT('Ctrl Pts',(-56.185170553554,18.1599608038317,2.67631063707843));
#234226=CARTESIAN_POINT('Ctrl Pts',(-56.1854680298097,18.159665508881,2.67649019601858));
#234227=CARTESIAN_POINT('Ctrl Pts',(-56.1857662469842,18.1593717347117,
2.67667072836669));
#234228=CARTESIAN_POINT('Ctrl Pts',(-56.1866608985078,18.1584904122037,
2.67721232541103));
#234229=CARTESIAN_POINT('Ctrl Pts',(-56.187562217779,18.1576227783924,2.67776268340059));
#234230=CARTESIAN_POINT('Ctrl Pts',(-56.1884697364865,18.1567689837085,
2.67832123541529));
#234231=CARTESIAN_POINT('Ctrl Pts',(-56.1948621810803,18.1507549641995,
2.68225560368456));
#234232=CARTESIAN_POINT('Ctrl Pts',(-56.201554230506,18.1453743792965,2.68661792998898));
#234233=CARTESIAN_POINT('Ctrl Pts',(-56.2084349106661,18.1405824894352,
2.69130986622586));
#234234=CARTESIAN_POINT('Ctrl Pts',(-56.2117720331085,18.1382584280306,
2.69358545023064));
#234235=CARTESIAN_POINT('Ctrl Pts',(-56.2151540877945,18.136072979141,2.6959391885348));
#234236=CARTESIAN_POINT('Ctrl Pts',(-56.2185710935569,18.134022044255,2.69836306235487));
#234237=CARTESIAN_POINT('Ctrl Pts',(-56.2238022906399,18.1308822062392,
2.7020738438222));
#234238=CARTESIAN_POINT('Ctrl Pts',(-56.2291119669556,18.1280584389298,
2.7059476081422));
#234239=CARTESIAN_POINT('Ctrl Pts',(-56.2344544719217,18.1255442374229,
2.70995196345699));
#234240=CARTESIAN_POINT('Ctrl Pts',(-56.2369355588664,18.1243766292364,
2.71181160678098));
#234241=CARTESIAN_POINT('Ctrl Pts',(-56.2394235482376,18.1232756028766,
2.71369962772091));
#234242=CARTESIAN_POINT('Ctrl Pts',(-56.2419141381098,18.12224170934,2.71561183138654));
#234243=CARTESIAN_POINT('Ctrl Pts',(-56.24210503201,18.1221624654742,2.71575839426304));
#234244=CARTESIAN_POINT('Ctrl Pts',(-56.2422959411932,18.1220835820645,
2.71590508903201));
#234245=CARTESIAN_POINT('Ctrl Pts',(-56.2424868643661,18.1220050584321,
2.71605191409903));
#234246=CARTESIAN_POINT('Ctrl Pts',(-56.2451687593304,18.1209020381385,
2.71811436362744));
#234247=CARTESIAN_POINT('Ctrl Pts',(-56.247854333334,18.1198718859664,2.72020091026951));
#234248=CARTESIAN_POINT('Ctrl Pts',(-56.2505383386774,18.1189123616724,
2.72230624862174));
#234249=CARTESIAN_POINT('Ctrl Pts',(-56.2601627045042,18.1154716782002,
2.72985561753078));
#234250=CARTESIAN_POINT('Ctrl Pts',(-56.2698406425782,18.1129106883014,
2.73770089914286));
#234251=CARTESIAN_POINT('Ctrl Pts',(-56.2795015152462,18.111121302731,2.7457482334701));
#234252=CARTESIAN_POINT('Ctrl Pts',(-56.2901178437877,18.1091549477489,
2.75459144546933));
#234253=CARTESIAN_POINT('Ctrl Pts',(-56.3007141730217,18.108120091155,2.76367911754151));
#234254=CARTESIAN_POINT('Ctrl Pts',(-56.3112209484354,18.1079204190086,
2.77292162564579));
#234255=CARTESIAN_POINT('Ctrl Pts',(-56.3225656290416,18.1077048232014,
2.78290121484551));
#234256=CARTESIAN_POINT('Ctrl Pts',(-56.3338070504127,18.1084627484405,
2.79306229499976));
#234257=CARTESIAN_POINT('Ctrl Pts',(-56.3448702837359,18.1101289800547,
2.80331916685008));
#234258=CARTESIAN_POINT('Ctrl Pts',(-56.3558407078999,18.1117812336979,
2.81348999408533));
#234259=CARTESIAN_POINT('Ctrl Pts',(-56.3666372711388,18.1143271060913,
2.82375635966801));
#234260=CARTESIAN_POINT('Ctrl Pts',(-56.3771794532808,18.1177524687105,
2.83404198860274));
#234261=CARTESIAN_POINT('Origin',(0.00470941899428508,0.0144941013085259,
2.83404198860262));
#234262=CARTESIAN_POINT('Ctrl Pts',(-59.7658094374952,19.4351129318419,
2.65878198860274));
#234263=CARTESIAN_POINT('Ctrl Pts',(-59.7631518948791,19.4432803829098,
2.65878198860274));
#234264=CARTESIAN_POINT('Ctrl Pts',(-59.759835699791,19.4511532554527,2.65944603041869));
#234265=CARTESIAN_POINT('Ctrl Pts',(-59.7559811102134,19.4586404431021,
2.66070439264099));
#234266=CARTESIAN_POINT('Ctrl Pts',(-59.7535182109726,19.4634243995795,
2.66150842619621));
#234267=CARTESIAN_POINT('Ctrl Pts',(-59.7508363273793,19.4680513433543,
2.66255428265387));
#234268=CARTESIAN_POINT('Ctrl Pts',(-59.7479734971807,19.472502933046,2.66381699700665));
#234269=CARTESIAN_POINT('Ctrl Pts',(-59.7440663083908,19.4785784597571,
2.66554034873265));
#234270=CARTESIAN_POINT('Ctrl Pts',(-59.7398178213044,19.484323005252,2.66766759643969));
#234271=CARTESIAN_POINT('Ctrl Pts',(-59.7353118462117,19.4896904492932,
2.67012012783145));
#234272=CARTESIAN_POINT('Ctrl Pts',(-59.7330588586654,19.4923741713139,
2.67134639352733));
#234273=CARTESIAN_POINT('Ctrl Pts',(-59.7307414364081,19.4949638171734,
2.67265375585009));
#234274=CARTESIAN_POINT('Ctrl Pts',(-59.7283696021899,19.4974550439414,
2.67403135126937));
#234275=CARTESIAN_POINT('Ctrl Pts',(-59.7271836850808,19.4987006573255,
2.67472014897901));
#234276=CARTESIAN_POINT('Ctrl Pts',(-59.7259841596484,19.4999216825137,
2.67542649668629));
#234277=CARTESIAN_POINT('Ctrl Pts',(-59.7247722453468,19.5011176808521,
2.67614899656099));
#234278=CARTESIAN_POINT('Ctrl Pts',(-59.7244692667715,19.5014166804367,
2.67632962152966));
#234279=CARTESIAN_POINT('Ctrl Pts',(-59.7241655137791,19.5017141161967,
2.67651125590947));
#234280=CARTESIAN_POINT('Ctrl Pts',(-59.7238610051971,19.5020099819911,
2.67669387767521));
#234281=CARTESIAN_POINT('Ctrl Pts',(-59.7229474794512,19.5028975793744,
2.67724174297241));
#234282=CARTESIAN_POINT('Ctrl Pts',(-59.722027153953,19.5037710453007,2.67779849504745));
#234283=CARTESIAN_POINT('Ctrl Pts',(-59.7211005320715,19.5046302297524,
2.67836353618006));
#234284=CARTESIAN_POINT('Ctrl Pts',(-59.7146969999424,19.5105677273987,
2.68226832098917));
#234285=CARTESIAN_POINT('Ctrl Pts',(-59.7079999120044,19.5158784513273,
2.68659153751416));
#234286=CARTESIAN_POINT('Ctrl Pts',(-59.7011184102409,19.5206092977908,
2.6912369948622));
#234287=CARTESIAN_POINT('Ctrl Pts',(-59.6976983227541,19.5229605154971,
2.69354577441244));
#234288=CARTESIAN_POINT('Ctrl Pts',(-59.69423209387,19.5251683423981,2.6959347882813));
#234289=CARTESIAN_POINT('Ctrl Pts',(-59.6907301905172,19.5272373629642,
2.69839565261216));
#234290=CARTESIAN_POINT('Ctrl Pts',(-59.6830044686627,19.5318019313701,
2.70382468689042));
#234291=CARTESIAN_POINT('Ctrl Pts',(-59.675112260622,19.5357011184427,2.70961155815083));
#234292=CARTESIAN_POINT('Ctrl Pts',(-59.6671986827532,19.5389266512982,
2.71562701361763));
#234293=CARTESIAN_POINT('Ctrl Pts',(-59.6643077529623,19.5401049791264,
2.71782453535853));
#234294=CARTESIAN_POINT('Ctrl Pts',(-59.6614137631514,19.5412013620779,
2.72005051502397));
#234295=CARTESIAN_POINT('Ctrl Pts',(-59.6585211429014,19.5422187365067,
2.7222998676011));
#234296=CARTESIAN_POINT('Ctrl Pts',(-59.6488051375685,19.5456359895577,
2.72985520488895));
#234297=CARTESIAN_POINT('Ctrl Pts',(-59.6390401911866,19.5481755652423,
2.73770845534571));
#234298=CARTESIAN_POINT('Ctrl Pts',(-59.6292970278052,19.5499445144592,
2.74576706701776));
#234299=CARTESIAN_POINT('Ctrl Pts',(-59.6185881370955,19.5518887991944,
2.75462443585063));
#234300=CARTESIAN_POINT('Ctrl Pts',(-59.6079049297395,19.552902397614,2.76373036323228));
#234301=CARTESIAN_POINT('Ctrl Pts',(-59.5973174182801,19.5530800481818,
2.77299664636878));
#234302=CARTESIAN_POINT('Ctrl Pts',(-59.5859142147994,19.553271385455,2.78297683033552));
#234303=CARTESIAN_POINT('Ctrl Pts',(-59.5746208362138,19.5524931697989,
2.79314401478987));
#234304=CARTESIAN_POINT('Ctrl Pts',(-59.5635130675402,19.5508078878557,
2.80341452428049));
#234305=CARTESIAN_POINT('Ctrl Pts',(-59.5525552912493,19.549145362909,2.8135463472144));
#234306=CARTESIAN_POINT('Ctrl Pts',(-59.5417768065748,19.546599586877,2.82378004209245));
#234307=CARTESIAN_POINT('Ctrl Pts',(-59.5312589135997,19.5431821162865,
2.83404198860274));
#234308=CARTESIAN_POINT('Ctrl Pts',(-56.259443978424,18.4801050014189,2.83404198860274));
#234309=CARTESIAN_POINT('Ctrl Pts',(-56.2493782971086,18.4768344633036,
2.82422126443099));
#234310=CARTESIAN_POINT('Ctrl Pts',(-56.2396067681225,18.4727817672093,
2.81442815028674));
#234311=CARTESIAN_POINT('Ctrl Pts',(-56.2301791400446,18.4679768367043,
2.80471618166571));
#234312=CARTESIAN_POINT('Ctrl Pts',(-56.2210759356559,18.4633372535452,
2.79533842146523));
#234313=CARTESIAN_POINT('Ctrl Pts',(-56.2122922812571,18.4579956735932,
2.78603515650573));
#234314=CARTESIAN_POINT('Ctrl Pts',(-56.2038917763263,18.4519372213376,
2.77685887347126));
#234315=CARTESIAN_POINT('Ctrl Pts',(-56.1959506682911,18.4462100865662,
2.76818441216954));
#234316=CARTESIAN_POINT('Ctrl Pts',(-56.18835121655,18.4398418135303,2.75962261522005));
#234317=CARTESIAN_POINT('Ctrl Pts',(-56.1811768067752,18.4327901596647,
2.75123537702043));
#234318=CARTESIAN_POINT('Ctrl Pts',(-56.1745692957322,18.4262957047547,
2.74351087134483));
#234319=CARTESIAN_POINT('Ctrl Pts',(-56.1683219623528,18.4192211773442,
2.7359339945019));
#234320=CARTESIAN_POINT('Ctrl Pts',(-56.1625328136775,18.411514249219,2.728576578129));
#234321=CARTESIAN_POINT('Ctrl Pts',(-56.1608066064038,18.4092161988262,
2.72638274508536));
#234322=CARTESIAN_POINT('Ctrl Pts',(-56.159121392827,18.4068618031993,2.72420861709706));
#234323=CARTESIAN_POINT('Ctrl Pts',(-56.1574804751187,18.4044493827313,
2.7220566373672));
#234324=CARTESIAN_POINT('Ctrl Pts',(-56.1558563235461,18.4020616112562,
2.71992664556759));
#234325=CARTESIAN_POINT('Ctrl Pts',(-56.1542770260203,18.3996196264082,
2.71782089927877));
#234326=CARTESIAN_POINT('Ctrl Pts',(-56.1527473834684,18.3971247125286,
2.71574387311239));
#234327=CARTESIAN_POINT('Ctrl Pts',(-56.1526410151169,18.3969512210967,
2.71559944077479));
#234328=CARTESIAN_POINT('Ctrl Pts',(-56.1525348749437,18.3967774746433,
2.71545515216062));
#234329=CARTESIAN_POINT('Ctrl Pts',(-56.1524289641634,18.3966034726925,
2.71531100781723));
#234330=CARTESIAN_POINT('Ctrl Pts',(-56.1477854475702,18.3889745897491,
2.70899119176072));
#234331=CARTESIAN_POINT('Ctrl Pts',(-56.1436260014307,18.3808409394273,
2.70298296066823));
#234332=CARTESIAN_POINT('Ctrl Pts',(-56.1400597146375,18.3722424849457,
2.69736727774118));
#234333=CARTESIAN_POINT('Ctrl Pts',(-56.1367353155297,18.3642272309675,
2.69213248525402));
#234334=CARTESIAN_POINT('Ctrl Pts',(-56.1339262909282,18.3558072700345,
2.68723866185434));
#234335=CARTESIAN_POINT('Ctrl Pts',(-56.1317496772148,18.3470212548464,
2.68278595829523));
#234336=CARTESIAN_POINT('Ctrl Pts',(-56.1309534437592,18.3438072168241,
2.68115710172778));
#234337=CARTESIAN_POINT('Ctrl Pts',(-56.1302421351291,18.3405443147879,
2.67958763637794));
#234338=CARTESIAN_POINT('Ctrl Pts',(-56.1296225724748,18.3372349828464,
2.67808378645359));
#234339=CARTESIAN_POINT('Ctrl Pts',(-56.1294735883542,18.3364391990694,
2.67772216078594));
#234340=CARTESIAN_POINT('Ctrl Pts',(-56.1293301519981,18.3356401993825,
2.67736403603557));
#234341=CARTESIAN_POINT('Ctrl Pts',(-56.1291923454416,18.3348380918585,
2.67700956934473));
#234342=CARTESIAN_POINT('Ctrl Pts',(-56.12905884534,18.3340610501946,2.67666617973798));
#234343=CARTESIAN_POINT('Ctrl Pts',(-56.1289306286648,18.333281091922,2.67632622314113));
#234344=CARTESIAN_POINT('Ctrl Pts',(-56.1288077688058,18.3324983188931,
2.67598984158768));
#234345=CARTESIAN_POINT('Ctrl Pts',(-56.1274616970648,18.3239221357307,
2.67230439292216));
#234346=CARTESIAN_POINT('Ctrl Pts',(-56.126758159346,18.3150023767874,2.6690496453997));
#234347=CARTESIAN_POINT('Ctrl Pts',(-56.1267895336332,18.3059033598549,
2.6664020356672));
#234348=CARTESIAN_POINT('Ctrl Pts',(-56.1268025454852,18.3021297263203,
2.66530399299434));
#234349=CARTESIAN_POINT('Ctrl Pts',(-56.1269416083199,18.2983254984047,
2.66430995142253));
#234350=CARTESIAN_POINT('Ctrl Pts',(-56.1272115877755,18.2945030089055,
2.66343053473353));
#234351=CARTESIAN_POINT('Ctrl Pts',(-56.127672065871,18.2879833547333,2.66193059792876));
#234352=CARTESIAN_POINT('Ctrl Pts',(-56.1285150529071,18.2814124323572,
2.66076519817119));
#234353=CARTESIAN_POINT('Ctrl Pts',(-56.1297657127887,18.2748585331712,
2.65997805604451));
#234354=CARTESIAN_POINT('Ctrl Pts',(-56.1303910427295,18.2715815835782,
2.65958448498116));
#234355=CARTESIAN_POINT('Ctrl Pts',(-56.1311196862928,18.2683092720866,
2.65928526260752));
#234356=CARTESIAN_POINT('Ctrl Pts',(-56.1319548233211,18.2650501911673,
2.65908463971314));
#234357=CARTESIAN_POINT('Ctrl Pts',(-56.1327899603494,18.261791110248,2.65888401681877));
#234358=CARTESIAN_POINT('Ctrl Pts',(-56.1337315613409,18.2585452947514,
2.65878198860274));
#234359=CARTESIAN_POINT('Ctrl Pts',(-56.1347810195643,18.2553202812748,
2.65878198860274));
#234360=CARTESIAN_POINT('Origin',(-56.9937374973464,12.0988124084938,2.83404198860269));
#234361=CARTESIAN_POINT('Ctrl Pts',(-61.3271735965894,12.8407372733096,
2.83404198860269));
#234362=CARTESIAN_POINT('Ctrl Pts',(-61.3375520649563,12.8429432848611,
2.8241965244006));
#234363=CARTESIAN_POINT('Ctrl Pts',(-61.3477256769088,12.8459616464943,
2.81438790575634));
#234364=CARTESIAN_POINT('Ctrl Pts',(-61.3576417279035,12.8497656413963,
2.80466781256877));
#234365=CARTESIAN_POINT('Ctrl Pts',(-61.367235566287,12.8534460291152,2.79526356453046));
#234366=CARTESIAN_POINT('Ctrl Pts',(-61.3765894879244,12.8578623484998,
2.78594102496194));
#234367=CARTESIAN_POINT('Ctrl Pts',(-61.3856422574871,12.8630345798924,
2.77675109088735));
#234368=CARTESIAN_POINT('Ctrl Pts',(-61.394205620056,12.8679271923021,2.76805797913634));
#234369=CARTESIAN_POINT('Ctrl Pts',(-61.4025003187128,12.873496651757,2.75948271210109));
#234370=CARTESIAN_POINT('Ctrl Pts',(-61.410448511695,12.8797929832534,2.75108575573169));
#234371=CARTESIAN_POINT('Ctrl Pts',(-61.4177693722596,12.885592359924,2.74335155163209));
#234372=CARTESIAN_POINT('Ctrl Pts',(-61.4247966697204,12.8920087864971,
2.73576818685876));
#234373=CARTESIAN_POINT('Ctrl Pts',(-61.4314390014625,12.8991043342896,
2.72840626160425));
#234374=CARTESIAN_POINT('Ctrl Pts',(-61.4333656894063,12.9011624829816,
2.72627084693634));
#234375=CARTESIAN_POINT('Ctrl Pts',(-61.4352597571384,12.9032779088719,
2.72415424587503));
#234376=CARTESIAN_POINT('Ctrl Pts',(-61.4371183613309,12.9054524645842,
2.72205867173264));
#234377=CARTESIAN_POINT('Ctrl Pts',(-61.4391332077732,12.9078098227881,
2.71978693462867));
#234378=CARTESIAN_POINT('Ctrl Pts',(-61.4411043938524,12.9102326900447,
2.71754411340768));
#234379=CARTESIAN_POINT('Ctrl Pts',(-61.4430281531012,12.9127224163027,
2.71533341844265));
#234380=CARTESIAN_POINT('Ctrl Pts',(-61.448307925455,12.9195554895544,2.70926614876412));
#234381=CARTESIAN_POINT('Ctrl Pts',(-61.4531896374536,12.926909770583,2.7034738186043));
#234382=CARTESIAN_POINT('Ctrl Pts',(-61.4575800373534,12.9347398820029,
2.69804914171416));
#234383=CARTESIAN_POINT('Ctrl Pts',(-61.4615970149014,12.9419040088456,
2.69308585687211));
#234384=CARTESIAN_POINT('Ctrl Pts',(-61.4651913207949,12.9494643722288,
2.68842799053179));
#234385=CARTESIAN_POINT('Ctrl Pts',(-61.4682744840805,12.9574154517112,
2.684147670542));
#234386=CARTESIAN_POINT('Ctrl Pts',(-61.4697889238147,12.9613209959793,
2.68204519134549));
#234387=CARTESIAN_POINT('Ctrl Pts',(-61.4711795284101,12.9653208118555,
2.68003431778512));
#234388=CARTESIAN_POINT('Ctrl Pts',(-61.4724324898305,12.9694138336349,
2.67812693945274));
#234389=CARTESIAN_POINT('Ctrl Pts',(-61.472670227056,12.970190444651,2.67776503299226));
#234390=CARTESIAN_POINT('Ctrl Pts',(-61.4729027677275,12.9709708853391,
2.67740659639946));
#234391=CARTESIAN_POINT('Ctrl Pts',(-61.4731300138563,12.9717550556846,
2.67705178968878));
#234392=CARTESIAN_POINT('Ctrl Pts',(-61.4733501585436,12.9725147207069,
2.6767080706878));
#234393=CARTESIAN_POINT('Ctrl Pts',(-61.4735653344326,12.9732778859006,
2.67636775825288));
#234394=CARTESIAN_POINT('Ctrl Pts',(-61.4737754532575,12.9740444565835,
2.67603099699278));
#234395=CARTESIAN_POINT('Ctrl Pts',(-61.4760652849146,12.9823983859294,
2.6723610421716));
#234396=CARTESIAN_POINT('Ctrl Pts',(-61.4777556486131,12.9911623597375,
2.66911440541513));
#234397=CARTESIAN_POINT('Ctrl Pts',(-61.478733140317,13.0001833616593,2.66646778189674));
#234398=CARTESIAN_POINT('Ctrl Pts',(-61.4791459411335,13.0039929867889,
2.66535009635009));
#234399=CARTESIAN_POINT('Ctrl Pts',(-61.4794319383912,13.0078481668563,
2.66433897912372));
#234400=CARTESIAN_POINT('Ctrl Pts',(-61.4795843394718,13.011736540843,2.66344564884815));
#234401=CARTESIAN_POINT('Ctrl Pts',(-61.4798409790835,13.0182844654763,
2.66194130298608));
#234402=CARTESIAN_POINT('Ctrl Pts',(-61.4797168922658,13.0249248230174,
2.66077206705441));
#234403=CARTESIAN_POINT('Ctrl Pts',(-61.4791780149463,13.0315916763175,
2.65998225155735));
#234404=CARTESIAN_POINT('Ctrl Pts',(-61.4790432956164,13.0332583896425,
2.65978479768309));
#234405=CARTESIAN_POINT('Ctrl Pts',(-61.4788824204055,13.0349267248714,
2.65961098966643));
#234406=CARTESIAN_POINT('Ctrl Pts',(-61.4786945538944,13.0365955947402,
2.65946139030523));
#234407=CARTESIAN_POINT('Ctrl Pts',(-61.4784127541277,13.0390988995432,
2.65923699126341));
#234408=CARTESIAN_POINT('Ctrl Pts',(-61.4780702140289,13.0416033892099,
2.65906707562463));
#234409=CARTESIAN_POINT('Ctrl Pts',(-61.4776657592304,13.0441057251027,
2.65895332562941));
#234410=CARTESIAN_POINT('Ctrl Pts',(-61.477261304432,13.0466080609956,2.65883957563418));
#234411=CARTESIAN_POINT('Ctrl Pts',(-61.4767949453822,13.0491082380627,
2.6587819886027));
#234412=CARTESIAN_POINT('Ctrl Pts',(-61.4762657165316,13.0516031943527,
2.6587819886027));
#234413=CARTESIAN_POINT('Ctrl Pts',(-57.7418065394566,12.2578193919766,
2.6587819886027));
#234414=CARTESIAN_POINT('Ctrl Pts',(-57.7435970583545,12.2493771807076,
2.6587819886027));
#234415=CARTESIAN_POINT('Ctrl Pts',(-57.74606892698,12.241155944225,2.65945335517859));
#234416=CARTESIAN_POINT('Ctrl Pts',(-57.7491141258101,12.2332613533232,
2.66072561226599));
#234417=CARTESIAN_POINT('Ctrl Pts',(-57.7510810117991,12.228162257632,2.66154735980339));
#234418=CARTESIAN_POINT('Ctrl Pts',(-57.7532862127603,12.2231990866885,
2.66261895766887));
#234419=CARTESIAN_POINT('Ctrl Pts',(-57.7556931859579,12.2183955094118,
2.66391429251036));
#234420=CARTESIAN_POINT('Ctrl Pts',(-57.7588834910512,12.2120286428976,
2.66563118464133));
#234421=CARTESIAN_POINT('Ctrl Pts',(-57.7624328173675,12.2059457447516,
2.66774105138708));
#234422=CARTESIAN_POINT('Ctrl Pts',(-57.7662682043709,12.2001996238499,
2.67016894181759));
#234423=CARTESIAN_POINT('Ctrl Pts',(-57.7681858978726,12.1973265633991,
2.67138288703284));
#234424=CARTESIAN_POINT('Ctrl Pts',(-57.770175146271,12.1945375019637,2.6726761316756));
#234425=CARTESIAN_POINT('Ctrl Pts',(-57.7722271161468,12.1918376559072,
2.67403835432562));
#234426=CARTESIAN_POINT('Ctrl Pts',(-57.7732531010847,12.190487732879,2.67471946565063));
#234427=CARTESIAN_POINT('Ctrl Pts',(-57.7742947697603,12.1891600976133,
2.67541781389532));
#234428=CARTESIAN_POINT('Ctrl Pts',(-57.7753510390205,12.1878553011596,
2.67613207244178));
#234429=CARTESIAN_POINT('Ctrl Pts',(-57.7756151063355,12.1875291020462,
2.6763106370784));
#234430=CARTESIAN_POINT('Ctrl Pts',(-57.7758800862578,12.1872043300163,
2.67649019601855));
#234431=CARTESIAN_POINT('Ctrl Pts',(-57.776145962005,12.1868809929896,2.67667072836666));
#234432=CARTESIAN_POINT('Ctrl Pts',(-57.7769435892465,12.1859109819096,
2.677212325411));
#234433=CARTESIAN_POINT('Ctrl Pts',(-57.7777492785674,12.1849538875689,
2.67776268340056));
#234434=CARTESIAN_POINT('Ctrl Pts',(-57.7785625799462,12.1840099085256,
2.67832123541525));
#234435=CARTESIAN_POINT('Ctrl Pts',(-57.7842913698424,12.1773606420349,
2.6822556036845));
#234436=CARTESIAN_POINT('Ctrl Pts',(-57.7903843352497,12.1713100228965,
2.6866179299889));
#234437=CARTESIAN_POINT('Ctrl Pts',(-57.7967264334405,12.1658251565858,
2.69130986622575));
#234438=CARTESIAN_POINT('Ctrl Pts',(-57.7998023442099,12.1631650023521,
2.69358545023055));
#234439=CARTESIAN_POINT('Ctrl Pts',(-57.8029374300324,12.1606380046012,
2.69593918853474));
#234440=CARTESIAN_POINT('Ctrl Pts',(-57.8061213360079,12.1582411305897,
2.69836306235483));
#234441=CARTESIAN_POINT('Ctrl Pts',(-57.8109956736033,12.1545716839429,
2.70207384382216));
#234442=CARTESIAN_POINT('Ctrl Pts',(-57.815981098899,12.1512083732206,2.70594760814216));
#234443=CARTESIAN_POINT('Ctrl Pts',(-57.8210315314441,12.1481495009385,
2.70995196345695));
#234444=CARTESIAN_POINT('Ctrl Pts',(-57.8233769784455,12.1467289448262,
2.71181160678094));
#234445=CARTESIAN_POINT('Ctrl Pts',(-57.8257362497572,12.1453738842984,
2.71369962772087));
#234446=CARTESIAN_POINT('Ctrl Pts',(-57.8281051246149,12.1440853170068,
2.7156118313865));
#234447=CARTESIAN_POINT('Ctrl Pts',(-57.8282866895389,12.1439865534012,
2.715758394263));
#234448=CARTESIAN_POINT('Ctrl Pts',(-57.8284683073399,12.1438881466795,
2.71590508903197));
#234449=CARTESIAN_POINT('Ctrl Pts',(-57.8286499766611,12.143790096302,2.71605191409899));
#234450=CARTESIAN_POINT('Ctrl Pts',(-57.8312018829079,12.1424127841096,
2.71811436362741));
#234451=CARTESIAN_POINT('Ctrl Pts',(-57.8337650648327,12.1411075562953,
2.72020091026947));
#234452=CARTESIAN_POINT('Ctrl Pts',(-57.8363340693141,12.1398727334219,
2.72230624862169));
#234453=CARTESIAN_POINT('Ctrl Pts',(-57.845546062502,12.1354448782039,2.72985561753081));
#234454=CARTESIAN_POINT('Ctrl Pts',(-57.8549032874801,12.1318862976812,
2.73770089914296));
#234455=CARTESIAN_POINT('Ctrl Pts',(-57.8643241951531,12.1290968783784,
2.74574823347028));
#234456=CARTESIAN_POINT('Ctrl Pts',(-57.8746768262717,12.1260315867866,
2.75459144546973));
#234457=CARTESIAN_POINT('Ctrl Pts',(-57.8851069357363,12.1238947812342,
2.76367911754212));
#234458=CARTESIAN_POINT('Ctrl Pts',(-57.8955352825126,12.1225979458249,
2.77292162564662));
#234459=CARTESIAN_POINT('Ctrl Pts',(-57.9067952798735,12.121197689044,2.78290121484685));
#234460=CARTESIAN_POINT('Ctrl Pts',(-57.9180543443232,12.1207764137886,
2.79306229500162));
#234461=CARTESIAN_POINT('Ctrl Pts',(-57.9292311407273,12.1212770948338,
2.80331916685248));
#234462=CARTESIAN_POINT('Ctrl Pts',(-57.9403141752932,12.1217735756795,
2.81348999408692));
#234463=CARTESIAN_POINT('Ctrl Pts',(-57.9513177099571,12.1231769533536,
2.82375635966879));
#234464=CARTESIAN_POINT('Ctrl Pts',(-57.9621601888121,12.125481593379,2.83404198860269));
#234465=CARTESIAN_POINT('Origin',(0.00316857416807368,0.0149069694353715,
2.83404198860262));
#234466=CARTESIAN_POINT('Ctrl Pts',(-61.4699285681955,13.081417133223,2.65878198860269));
#234467=CARTESIAN_POINT('Ctrl Pts',(-61.4681393149849,13.0898176309847,
2.65878198860269));
#234468=CARTESIAN_POINT('Ctrl Pts',(-61.465664225629,13.0979940118842,2.65944603041858));
#234469=CARTESIAN_POINT('Ctrl Pts',(-61.4626133761159,13.105843098261,2.66070439264076));
#234470=CARTESIAN_POINT('Ctrl Pts',(-61.4606640285136,13.1108582907975,
2.66150842619601));
#234471=CARTESIAN_POINT('Ctrl Pts',(-61.4584804838815,13.1157402208611,
2.66255428265373));
#234472=CARTESIAN_POINT('Ctrl Pts',(-61.4560986543957,13.1204666715204,
2.66381699700659));
#234473=CARTESIAN_POINT('Ctrl Pts',(-61.4528479350655,13.1269173283004,
2.66554034873259));
#234474=CARTESIAN_POINT('Ctrl Pts',(-61.4492231901485,13.1330744924003,
2.66766759643963));
#234475=CARTESIAN_POINT('Ctrl Pts',(-61.4453029499362,13.1388835356735,
2.67012012783139));
#234476=CARTESIAN_POINT('Ctrl Pts',(-61.4433428298301,13.14178805731,2.67134639352727));
#234477=CARTESIAN_POINT('Ctrl Pts',(-61.4413087943565,13.1446057534059,
2.67265375585004));
#234478=CARTESIAN_POINT('Ctrl Pts',(-61.4392103574,13.147331257159,2.67403135126932));
#234479=CARTESIAN_POINT('Ctrl Pts',(-61.4381611389217,13.1486940090355,
2.67472014897896));
#234480=CARTESIAN_POINT('Ctrl Pts',(-61.4370958165018,13.1500337298701,
2.67542649668624));
#234481=CARTESIAN_POINT('Ctrl Pts',(-61.4360155570619,13.1513498559441,
2.67614899656094));
#234482=CARTESIAN_POINT('Ctrl Pts',(-61.4357454922019,13.1516788874625,
2.67632962152961));
#234483=CARTESIAN_POINT('Ctrl Pts',(-61.4354744937032,13.1520064446718,
2.67651125590942));
#234484=CARTESIAN_POINT('Ctrl Pts',(-61.4352025796479,13.1523325194966,
2.67669387767516));
#234485=CARTESIAN_POINT('Ctrl Pts',(-61.4343868374821,13.1533107439709,
2.67724174297236));
#234486=CARTESIAN_POINT('Ctrl Pts',(-61.4335628556743,13.1542756251696,
2.6777984950474));
#234487=CARTESIAN_POINT('Ctrl Pts',(-61.4327311191547,13.1552269612802,
2.67836353618001));
#234488=CARTESIAN_POINT('Ctrl Pts',(-61.4269833037494,13.161801284066,2.68226832098907));
#234489=CARTESIAN_POINT('Ctrl Pts',(-61.420878024971,13.1677829516036,2.68659153751398));
#234490=CARTESIAN_POINT('Ctrl Pts',(-61.4145287289051,13.1732071947995,
2.69123699486195));
#234491=CARTESIAN_POINT('Ctrl Pts',(-61.411373146189,13.1759030287785,2.69354577441226));
#234492=CARTESIAN_POINT('Ctrl Pts',(-61.4081566864225,13.1784610805514,
2.69593478828118));
#234493=CARTESIAN_POINT('Ctrl Pts',(-61.4048902384027,13.1808848153825,
2.69839565261211));
#234494=CARTESIAN_POINT('Ctrl Pts',(-61.3976839661819,13.1862319364381,
2.70382468689037));
#234495=CARTESIAN_POINT('Ctrl Pts',(-61.3902425685153,13.1909347237342,
2.70961155815078));
#234496=CARTESIAN_POINT('Ctrl Pts',(-61.3827095020467,13.1949697809168,
2.71562701361759));
#234497=CARTESIAN_POINT('Ctrl Pts',(-61.3799575778687,13.1964438381903,
2.7178245353585));
#234498=CARTESIAN_POINT('Ctrl Pts',(-61.377194044862,13.197836719349,2.72005051502394));
#234499=CARTESIAN_POINT('Ctrl Pts',(-61.3744236152739,13.1991508816437,
2.72229986760107));
#234500=CARTESIAN_POINT('Ctrl Pts',(-61.3651180354454,13.2035650137314,
2.72985520488854));
#234501=CARTESIAN_POINT('Ctrl Pts',(-61.3556720404057,13.2071113921937,
2.73770845534488));
#234502=CARTESIAN_POINT('Ctrl Pts',(-61.3461671566365,13.2098890888172,
2.74576706701649));
#234503=CARTESIAN_POINT('Ctrl Pts',(-61.3357201634466,13.2129421064463,
2.75462443584895));
#234504=CARTESIAN_POINT('Ctrl Pts',(-61.3252014297039,13.2150668515154,
2.76373036323015));
#234505=CARTESIAN_POINT('Ctrl Pts',(-61.3146904872814,13.2163502251976,
2.77299664636619));
#234506=CARTESIAN_POINT('Ctrl Pts',(-61.3033697519341,13.2177324736415,
2.78297683033245));
#234507=CARTESIAN_POINT('Ctrl Pts',(-61.2920568939719,13.218139000641,2.79314401478632));
#234508=CARTESIAN_POINT('Ctrl Pts',(-61.2808338148861,13.2176240288386,
2.80341452427645));
#234509=CARTESIAN_POINT('Ctrl Pts',(-61.2697622852609,13.2171160108943,
2.81354634721166));
#234510=CARTESIAN_POINT('Ctrl Pts',(-61.2587767401952,13.215710839329,2.82378004209106));
#234511=CARTESIAN_POINT('Ctrl Pts',(-61.2479592423879,13.2134115091892,
2.8340419886027));
#234512=CARTESIAN_POINT('Ctrl Pts',(-57.8829458346106,12.4981558292586,
2.83404198860269));
#234513=CARTESIAN_POINT('Ctrl Pts',(-57.8725934298279,12.4959553576929,
2.82422126443142));
#234514=CARTESIAN_POINT('Ctrl Pts',(-57.8624518082056,12.4929462656008,
2.81442815028765));
#234515=CARTESIAN_POINT('Ctrl Pts',(-57.8525735736594,12.4891531124833,
2.80471618166709));
#234516=CARTESIAN_POINT('Ctrl Pts',(-57.8430352690793,12.4854904894119,
2.79533842146691));
#234517=CARTESIAN_POINT('Ctrl Pts',(-57.8337413853149,12.4810963130903,
2.7860351565077));
#234518=CARTESIAN_POINT('Ctrl Pts',(-57.8247536185252,12.4759491415414,
2.77685887347351));
#234519=CARTESIAN_POINT('Ctrl Pts',(-57.8162573641143,12.4710834524333,
2.76818441217196));
#234520=CARTESIAN_POINT('Ctrl Pts',(-57.8080338771709,12.4655444244758,
2.75962261522265));
#234521=CARTESIAN_POINT('Ctrl Pts',(-57.8001616710216,12.4592813303369,
2.75123537702318));
#234522=CARTESIAN_POINT('Ctrl Pts',(-57.7929115012241,12.453513125706,2.74351087134769));
#234523=CARTESIAN_POINT('Ctrl Pts',(-57.7859589019121,12.4471303774549,
2.73593399450487));
#234524=CARTESIAN_POINT('Ctrl Pts',(-57.7793958734455,12.4400707995033,
2.72857657813204));
#234525=CARTESIAN_POINT('Ctrl Pts',(-57.7774389108389,12.4379657758637,
2.72638274508736));
#234526=CARTESIAN_POINT('Ctrl Pts',(-57.7755168276806,12.4358004306468,
2.72420861709803));
#234527=CARTESIAN_POINT('Ctrl Pts',(-57.7736327324861,12.433572748276,2.72205663736716));
#234528=CARTESIAN_POINT('Ctrl Pts',(-57.7717678881028,12.4313678273309,
2.71992664556755));
#234529=CARTESIAN_POINT('Ctrl Pts',(-57.7699419852106,12.4291043014747,
2.71782089927873));
#234530=CARTESIAN_POINT('Ctrl Pts',(-57.7681599326868,12.4267829461797,
2.71574387311234));
#234531=CARTESIAN_POINT('Ctrl Pts',(-57.7680360122395,12.4266215236723,
2.71559944077475));
#234532=CARTESIAN_POINT('Ctrl Pts',(-57.7679122920635,12.4264598236895,
2.71545515216057));
#234533=CARTESIAN_POINT('Ctrl Pts',(-57.767788773317,12.4262978456306,2.71531100781719));
#234534=CARTESIAN_POINT('Ctrl Pts',(-57.762373258983,12.4191961341598,2.70899119176065));
#234535=CARTESIAN_POINT('Ctrl Pts',(-57.7573864007557,12.4115418213385,
2.70298296066813));
#234536=CARTESIAN_POINT('Ctrl Pts',(-57.7529408672213,12.4033632485683,
2.69736727774106));
#234537=CARTESIAN_POINT('Ctrl Pts',(-57.7487968573386,12.39573939732,2.69213248525386));
#234538=CARTESIAN_POINT('Ctrl Pts',(-57.7451230952907,12.3876591848387,
2.68723866185414));
#234539=CARTESIAN_POINT('Ctrl Pts',(-57.7420400166291,12.3791488184476,
2.682785958295));
#234540=CARTESIAN_POINT('Ctrl Pts',(-57.7409121865683,12.3760356163216,
2.68115710172761));
#234541=CARTESIAN_POINT('Ctrl Pts',(-57.7398637084258,12.3728649408022,
2.67958763637783));
#234542=CARTESIAN_POINT('Ctrl Pts',(-57.7389016204182,12.3696384996596,
2.67808378645353));
#234543=CARTESIAN_POINT('Ctrl Pts',(-57.7386702703929,12.3688626483506,
2.67772216078589));
#234544=CARTESIAN_POINT('Ctrl Pts',(-57.7384441015868,12.3680830188495,
2.67736403603552));
#234545=CARTESIAN_POINT('Ctrl Pts',(-57.7382232068821,12.367299710062,2.67700956934467));
#234546=CARTESIAN_POINT('Ctrl Pts',(-57.738009215137,12.3665408796741,2.67666617973792));
#234547=CARTESIAN_POINT('Ctrl Pts',(-57.7378001730066,12.3657785963866,
2.67632622314107));
#234548=CARTESIAN_POINT('Ctrl Pts',(-57.737596164125,12.3650129538224,2.67598984158762));
#234549=CARTESIAN_POINT('Ctrl Pts',(-57.7353610110592,12.3566244546995,
2.6723043929222));
#234550=CARTESIAN_POINT('Ctrl Pts',(-57.7337289586985,12.3478270988458,
2.66904964539982));
#234551=CARTESIAN_POINT('Ctrl Pts',(-57.7328090548569,12.3387746477743,
2.66640203566736));
#234552=CARTESIAN_POINT('Ctrl Pts',(-57.7324275433143,12.33502032649,2.66530399299442));
#234553=CARTESIAN_POINT('Ctrl Pts',(-57.7321681942503,12.3312224025083,
2.66430995142253));
#234554=CARTESIAN_POINT('Ctrl Pts',(-57.732037135777,12.3273926324687,2.66343053473348));
#234555=CARTESIAN_POINT('Ctrl Pts',(-57.7318136018935,12.3208605605765,
2.66193059792871));
#234556=CARTESIAN_POINT('Ctrl Pts',(-57.7319651225403,12.3142375182613,
2.66076519817114));
#234557=CARTESIAN_POINT('Ctrl Pts',(-57.7325238621659,12.3075887924653,
2.65997805604446));
#234558=CARTESIAN_POINT('Ctrl Pts',(-57.7328032319787,12.3042644295673,
2.65958448498112));
#234559=CARTESIAN_POINT('Ctrl Pts',(-57.7331858342648,12.3009338801485,
2.65928526260748));
#234560=CARTESIAN_POINT('Ctrl Pts',(-57.7336757296049,12.2976053572253,
2.6590846397131));
#234561=CARTESIAN_POINT('Ctrl Pts',(-57.734165624945,12.294276834302,2.65888401681872));
#234562=CARTESIAN_POINT('Ctrl Pts',(-57.7347627876418,12.2909503756177,
2.6587819886027));
#234563=CARTESIAN_POINT('Ctrl Pts',(-57.7354693911205,12.2876333308469,
2.6587819886027));
#234564=CARTESIAN_POINT('Origin',(-57.9461901084062,6.07506605172281,2.83404198860265));
#234565=CARTESIAN_POINT('Ctrl Pts',(-62.3334394572619,6.3599591583778,2.83404198860264));
#234566=CARTESIAN_POINT('Ctrl Pts',(-62.3439916622905,6.36106823981769,
2.82419652440062));
#234567=CARTESIAN_POINT('Ctrl Pts',(-62.3544250468353,6.3630066345268,2.81438790575644));
#234568=CARTESIAN_POINT('Ctrl Pts',(-62.3646844024063,6.36575328117444,
2.80466781256896));
#234569=CARTESIAN_POINT('Ctrl Pts',(-62.3746103900118,6.36841067816123,
2.79526356453073));
#234570=CARTESIAN_POINT('Ctrl Pts',(-62.3843747009663,6.37182505343183,
2.78594102496229));
#234571=CARTESIAN_POINT('Ctrl Pts',(-62.3939185239092,6.37602267870893,
2.77675109088779));
#234572=CARTESIAN_POINT('Ctrl Pts',(-62.4029463927384,6.37999337374618,
2.76805797913686));
#234573=CARTESIAN_POINT('Ctrl Pts',(-62.4117778192061,6.38466529101543,
2.7594827121017));
#234574=CARTESIAN_POINT('Ctrl Pts',(-62.420340617011,6.3900963181509,2.75108575573236));
#234575=CARTESIAN_POINT('Ctrl Pts',(-62.4282275730666,6.39509868692453,
2.74335155163287));
#234576=CARTESIAN_POINT('Ctrl Pts',(-62.4358870734659,6.40074541103687,
2.73576818685965));
#234577=CARTESIAN_POINT('Ctrl Pts',(-62.4432347045264,6.40710777594649,
2.72840626160522));
#234578=CARTESIAN_POINT('Ctrl Pts',(-62.4453659729924,6.40895325615489,
2.72627084693697));
#234579=CARTESIAN_POINT('Ctrl Pts',(-62.4474707870411,6.41085910953172,
2.72415424587532));
#234580=CARTESIAN_POINT('Ctrl Pts',(-62.4495465125725,6.41282747576061,
2.72205867173261));
#234581=CARTESIAN_POINT('Ctrl Pts',(-62.4517967325057,6.41496131130725,
2.71978693462864));
#234582=CARTESIAN_POINT('Ctrl Pts',(-62.4540103788122,6.4171648607918,2.71754411340765));
#234583=CARTESIAN_POINT('Ctrl Pts',(-62.4561838467663,6.4194398604709,2.71533341844262));
#234584=CARTESIAN_POINT('Ctrl Pts',(-62.4621489466211,6.42568361494178,
2.70926614876408));
#234585=CARTESIAN_POINT('Ctrl Pts',(-62.467772647785,6.43248733059613,2.70347381860426));
#234586=CARTESIAN_POINT('Ctrl Pts',(-62.4729574661286,6.43981562609172,
2.69804914171411));
#234587=CARTESIAN_POINT('Ctrl Pts',(-62.477701293423,6.44652061860809,2.69308585687195));
#234588=CARTESIAN_POINT('Ctrl Pts',(-62.4820661824989,6.45366385825823,
2.68842799053153));
#234589=CARTESIAN_POINT('Ctrl Pts',(-62.4859635700132,6.46124910257527,
2.68414767054166));
#234590=CARTESIAN_POINT('Ctrl Pts',(-62.4878779540286,6.46497494980492,
2.68204519134525));
#234591=CARTESIAN_POINT('Ctrl Pts',(-62.4896790353533,6.46880749650967,
2.68003431778498));
#234592=CARTESIAN_POINT('Ctrl Pts',(-62.4913529701965,6.47274712615551,
2.67812693945269));
#234593=CARTESIAN_POINT('Ctrl Pts',(-62.4916705830287,6.47349463250838,
2.67776503299221));
#234594=CARTESIAN_POINT('Ctrl Pts',(-62.4919834280838,6.47424649074166,
2.67740659639941));
#234595=CARTESIAN_POINT('Ctrl Pts',(-62.4922913974557,6.47500261163138,
2.67705178968873));
#234596=CARTESIAN_POINT('Ctrl Pts',(-62.4925897427848,6.4757351037433,2.67670807068775));
#234597=CARTESIAN_POINT('Ctrl Pts',(-62.4928835124027,6.47647159623325,
2.67636775825283));
#234598=CARTESIAN_POINT('Ctrl Pts',(-62.4931726086301,6.47721200416384,
2.67603099699273));
#234599=CARTESIAN_POINT('Ctrl Pts',(-62.4963231197466,6.48528081722631,
2.67236104217163));
#234600=CARTESIAN_POINT('Ctrl Pts',(-62.49892030817,6.49382008994889,2.66911440541521));
#234601=CARTESIAN_POINT('Ctrl Pts',(-62.5008353965401,6.50268949817244,
2.66646778189685));
#234602=CARTESIAN_POINT('Ctrl Pts',(-62.5016441502511,6.50643510434217,
2.66535009635013));
#234603=CARTESIAN_POINT('Ctrl Pts',(-62.502331556834,6.51023927047611,2.66433897912371));
#234604=CARTESIAN_POINT('Ctrl Pts',(-62.502889568803,6.51409041329268,2.6634456488481));
#234605=CARTESIAN_POINT('Ctrl Pts',(-62.5038292470155,6.5205756415655,2.66194130298603));
#234606=CARTESIAN_POINT('Ctrl Pts',(-62.5043999463277,6.52719259313761,
2.66077206705437));
#234607=CARTESIAN_POINT('Ctrl Pts',(-62.5045608969645,6.53387925273585,
2.6599822515573));
#234608=CARTESIAN_POINT('Ctrl Pts',(-62.5046011346237,6.53555091763541,
2.65978479768304));
#234609=CARTESIAN_POINT('Ctrl Pts',(-62.5046155292218,6.53722692958794,
2.65961098966639));
#234610=CARTESIAN_POINT('Ctrl Pts',(-62.5046031362659,6.53890629461061,
2.65946139030518));
#234611=CARTESIAN_POINT('Ctrl Pts',(-62.504584546832,6.5414253421446,2.65923699126337));
#234612=CARTESIAN_POINT('Ctrl Pts',(-62.5045056736598,6.54395191714494,
2.65906707562458));
#234613=CARTESIAN_POINT('Ctrl Pts',(-62.5043649998326,6.54648282201852,
2.65895332562936));
#234614=CARTESIAN_POINT('Ctrl Pts',(-62.5042243260054,6.5490137268921,2.65883957563414));
#234615=CARTESIAN_POINT('Ctrl Pts',(-62.5040218613861,6.55154895552238,
2.65878198860265));
#234616=CARTESIAN_POINT('Ctrl Pts',(-62.5037563256535,6.55408556365924,
2.65878198860265));
#234617=CARTESIAN_POINT('Ctrl Pts',(-58.7067819056643,6.15500747092296,
2.65878198860265));
#234618=CARTESIAN_POINT('Ctrl Pts',(-58.7076801645418,6.14642434678151,
2.65878198860265));
#234619=CARTESIAN_POINT('Ctrl Pts',(-58.7092791387968,6.13798976646338,
2.6594533551786));
#234620=CARTESIAN_POINT('Ctrl Pts',(-58.7114824462541,6.12982011300218,
2.6607256122661));
#234621=CARTESIAN_POINT('Ctrl Pts',(-58.7129055567991,6.12454335512125,
2.66154735980348));
#234622=CARTESIAN_POINT('Ctrl Pts',(-58.714579884807,6.1193768666801,2.66261895766891));
#234623=CARTESIAN_POINT('Ctrl Pts',(-58.7164715618025,6.11434800669306,
2.66391429251034));
#234624=CARTESIAN_POINT('Ctrl Pts',(-58.7189788712982,6.10768254085107,
2.6656311846413));
#234625=CARTESIAN_POINT('Ctrl Pts',(-58.7218729180382,6.10126195983215,
2.66774105138706));
#234626=CARTESIAN_POINT('Ctrl Pts',(-58.7250866612026,6.0951464096725,2.67016894181756));
#234627=CARTESIAN_POINT('Ctrl Pts',(-58.7266935327849,6.09208863459267,
2.67138288703281));
#234628=CARTESIAN_POINT('Ctrl Pts',(-58.7283803475666,6.0891069188495,2.67267613167557));
#234629=CARTESIAN_POINT('Ctrl Pts',(-58.7301388657773,6.08620737357443,
2.67403835432559));
#234630=CARTESIAN_POINT('Ctrl Pts',(-58.7310181248827,6.0847576009369,2.6747194656506));
#234631=CARTESIAN_POINT('Ctrl Pts',(-58.7319153115143,6.08332835457022,
2.67541781389528));
#234632=CARTESIAN_POINT('Ctrl Pts',(-58.7328294060527,6.0819202957255,2.67613207244175));
#234633=CARTESIAN_POINT('Ctrl Pts',(-58.7330579296874,6.08156828101432,
2.67631063707836));
#234634=CARTESIAN_POINT('Ctrl Pts',(-58.7332875101006,6.08121759017548,
2.67649019601851));
#234635=CARTESIAN_POINT('Ctrl Pts',(-58.7335181314301,6.08086823283961,
2.67667072836662));
#234636=CARTESIAN_POINT('Ctrl Pts',(-58.7342099954186,6.07982016083199,
2.67721232541096));
#234637=CARTESIAN_POINT('Ctrl Pts',(-58.7349112274885,6.07878409208758,
2.67776268340052));
#234638=CARTESIAN_POINT('Ctrl Pts',(-58.7356214008386,6.07776027111699,
2.67832123541521));
#234639=CARTESIAN_POINT('Ctrl Pts',(-58.7406237702161,6.07054860839961,
2.68225560368445));
#234640=CARTESIAN_POINT('Ctrl Pts',(-58.746050895801,6.06389424687519,2.68661792998883));
#234641=CARTESIAN_POINT('Ctrl Pts',(-58.7517849266677,6.05777649745833,
2.69130986622566));
#234642=CARTESIAN_POINT('Ctrl Pts',(-58.7545659254419,6.05480939560192,
2.69358545023047));
#234643=CARTESIAN_POINT('Ctrl Pts',(-58.7574196937447,6.05196853530582,
2.69593918853468));
#234644=CARTESIAN_POINT('Ctrl Pts',(-58.7603356163931,6.04925198282212,
2.69836306235479));
#234645=CARTESIAN_POINT('Ctrl Pts',(-58.7647996902381,6.04509313076973,
2.70207384382212));
#234646=CARTESIAN_POINT('Ctrl Pts',(-58.7694062431511,6.04122712577057,
2.70594760814212));
#234647=CARTESIAN_POINT('Ctrl Pts',(-58.7741092696793,6.03765709635814,
2.70995196345691));
#234648=CARTESIAN_POINT('Ctrl Pts',(-58.7762933795292,6.03599915623013,
2.71181160678089));
#234649=CARTESIAN_POINT('Ctrl Pts',(-58.7784980841112,6.03440490786102,
2.71369962772083));
#234650=CARTESIAN_POINT('Ctrl Pts',(-58.7807192900657,6.03287578462736,
2.71561183138645));
#234651=CARTESIAN_POINT('Ctrl Pts',(-58.7808895367502,6.03275858335655,
2.71575839426296));
#234652=CARTESIAN_POINT('Ctrl Pts',(-58.7810598733265,6.03264173148758,
2.71590508903193));
#234653=CARTESIAN_POINT('Ctrl Pts',(-58.7812302983888,6.03252522862529,
2.71605191409895));
#234654=CARTESIAN_POINT('Ctrl Pts',(-58.7836242566993,6.03088871465484,
2.71811436362737));
#234655=CARTESIAN_POINT('Ctrl Pts',(-58.7860369637877,6.02932271154743,
2.72020091026943));
#234656=CARTESIAN_POINT('Ctrl Pts',(-58.7884628208564,6.02782611907237,
2.72230624862166));
#234657=CARTESIAN_POINT('Ctrl Pts',(-58.7971615128801,6.02245960461699,
2.72985561753071));
#234658=CARTESIAN_POINT('Ctrl Pts',(-58.8060955050472,6.01794242202343,
2.7377008991428));
#234659=CARTESIAN_POINT('Ctrl Pts',(-58.815173230289,6.0141835304498,2.74574823347006));
#234660=CARTESIAN_POINT('Ctrl Pts',(-58.825148738391,6.01005288622463,2.75459144546905));
#234661=CARTESIAN_POINT('Ctrl Pts',(-58.8352983536234,6.00683754300273,
2.76367911754095));
#234662=CARTESIAN_POINT('Ctrl Pts',(-58.8455340166119,6.00445775273053,
2.77292162564495));
#234663=CARTESIAN_POINT('Ctrl Pts',(-58.8565859638382,6.00188817648251,
2.78290121484389));
#234664=CARTESIAN_POINT('Ctrl Pts',(-58.8677393146984,6.00029231631224,
2.79306229499733));
#234665=CARTESIAN_POINT('Ctrl Pts',(-58.8789072188612,5.99962196122167,
2.80331916684684));
#234666=CARTESIAN_POINT('Ctrl Pts',(-58.889981435786,5.99895722972136,2.81348999408311));
#234667=CARTESIAN_POINT('Ctrl Pts',(-58.9010713848493,5.99920273697657,
2.82375635966685));
#234668=CARTESIAN_POINT('Ctrl Pts',(-58.912095367953,6.00036140429026,2.83404198860265));
#234669=CARTESIAN_POINT('Origin',(0.00159301378021015,0.0151565136856013,
2.83404198860262));
#234670=CARTESIAN_POINT('Ctrl Pts',(-62.5005702980931,6.58439859103007,
2.65878198860265));
#234671=CARTESIAN_POINT('Ctrl Pts',(-62.4996689377206,6.59294009787421,
2.65878198860265));
#234672=CARTESIAN_POINT('Ctrl Pts',(-62.4980620716937,6.60133040499013,
2.65944603041847));
#234673=CARTESIAN_POINT('Ctrl Pts',(-62.4958483879906,6.60945539386143,
2.66070439264056));
#234674=CARTESIAN_POINT('Ctrl Pts',(-62.4944339494872,6.61464687495804,
2.66150842619583));
#234675=CARTESIAN_POINT('Ctrl Pts',(-62.4927726671883,6.61973030386325,
2.6625542826536));
#234676=CARTESIAN_POINT('Ctrl Pts',(-62.4908979342376,6.62467983150749,
2.66381699700655));
#234677=CARTESIAN_POINT('Ctrl Pts',(-62.4883392999283,6.63143494361077,
2.66554034873254));
#234678=CARTESIAN_POINT('Ctrl Pts',(-62.4853780106447,6.63793726713746,
2.66766759643958));
#234679=CARTESIAN_POINT('Ctrl Pts',(-62.4820864562849,6.64412426454875,
2.67012012783134));
#234680=CARTESIAN_POINT('Ctrl Pts',(-62.480440679105,6.6472177632544,2.67134639352722));
#234681=CARTESIAN_POINT('Ctrl Pts',(-62.4787123157334,6.65023263831855,
2.67265375584998));
#234682=CARTESIAN_POINT('Ctrl Pts',(-62.476910266953,6.65316255786721,2.67403135126925));
#234683=CARTESIAN_POINT('Ctrl Pts',(-62.4760092425629,6.65462751764154,
2.67472014897889));
#234684=CARTESIAN_POINT('Ctrl Pts',(-62.4750897950506,6.65607125586062,
2.67542649668618));
#234685=CARTESIAN_POINT('Ctrl Pts',(-62.474153026021,6.65749308991742,2.67614899656087));
#234686=CARTESIAN_POINT('Ctrl Pts',(-62.4739188337636,6.65784854843162,
2.67632962152955));
#234687=CARTESIAN_POINT('Ctrl Pts',(-62.4736835588747,6.65820263830483,
2.67651125590936));
#234688=CARTESIAN_POINT('Ctrl Pts',(-62.4734472184934,6.65855534961595,
2.67669387767509));
#234689=CARTESIAN_POINT('Ctrl Pts',(-62.4727381973496,6.65961348354928,
2.67724174297229));
#234690=CARTESIAN_POINT('Ctrl Pts',(-62.4720195869492,6.66065920857987,
2.67779849504733));
#234691=CARTESIAN_POINT('Ctrl Pts',(-62.4712918484711,6.66169227331197,
2.67836353617994));
#234692=CARTESIAN_POINT('Ctrl Pts',(-62.4662627240579,6.66883139158105,
2.68226832098894));
#234693=CARTESIAN_POINT('Ctrl Pts',(-62.460816145151,6.67541846632645,2.68659153751377));
#234694=CARTESIAN_POINT('Ctrl Pts',(-62.455068618999,6.68147667711109,2.69123699486165));
#234695=CARTESIAN_POINT('Ctrl Pts',(-62.4522121142781,6.68448759124161,
2.69354577441203));
#234696=CARTESIAN_POINT('Ctrl Pts',(-62.4492806638354,6.68736784133592,
2.69593478828104));
#234697=CARTESIAN_POINT('Ctrl Pts',(-62.4462854590369,6.69011973548587,
2.69839565261206));
#234698=CARTESIAN_POINT('Ctrl Pts',(-62.4396775898761,6.696190825014,2.70382468689032));
#234699=CARTESIAN_POINT('Ctrl Pts',(-62.4327685320937,6.70164568781193,
2.70961155815073));
#234700=CARTESIAN_POINT('Ctrl Pts',(-62.4256985108779,6.70644606039072,
2.71562701361754));
#234701=CARTESIAN_POINT('Ctrl Pts',(-62.4231157429701,6.70819969702963,
2.71782453535844));
#234702=CARTESIAN_POINT('Ctrl Pts',(-62.4205129446133,6.70987381569794,
2.72005051502389));
#234703=CARTESIAN_POINT('Ctrl Pts',(-62.4178950590935,6.71147036762155,
2.72229986760102));
#234704=CARTESIAN_POINT('Ctrl Pts',(-62.4091018586484,6.71683301659127,
2.72985520488883));
#234705=CARTESIAN_POINT('Ctrl Pts',(-62.4000783072482,6.72134734296704,
2.73770845534555));
#234706=CARTESIAN_POINT('Ctrl Pts',(-62.3909158405859,6.7251033539719,2.74576706701756));
#234707=CARTESIAN_POINT('Ctrl Pts',(-62.3808452043584,6.72923165499498,
2.7546244358504));
#234708=CARTESIAN_POINT('Ctrl Pts',(-62.3706061896764,6.73244426756195,
2.76373036323201));
#234709=CARTESIAN_POINT('Ctrl Pts',(-62.3602869763746,6.73481930344769,
2.77299664636847));
#234710=CARTESIAN_POINT('Ctrl Pts',(-62.3491727415053,6.73737731885886,
2.78297683033515));
#234711=CARTESIAN_POINT('Ctrl Pts',(-62.3379643502049,6.73896413451877,
2.79314401478945));
#234712=CARTESIAN_POINT('Ctrl Pts',(-62.326748923109,6.73962511499558,2.80341452427999));
#234713=CARTESIAN_POINT('Ctrl Pts',(-62.3156849421477,6.74027717000414,
2.81354634721404));
#234714=CARTESIAN_POINT('Ctrl Pts',(-62.3046126966243,6.74002799825949,
2.82378004209224));
#234715=CARTESIAN_POINT('Ctrl Pts',(-62.293614112757,6.73887200051311,2.83404198860265));
#234716=CARTESIAN_POINT('Ctrl Pts',(-58.872270023448,6.37927424642558,2.83404198860265));
#234717=CARTESIAN_POINT('Ctrl Pts',(-58.8617443183093,6.37816795023634,
2.82422126443007));
#234718=CARTESIAN_POINT('Ctrl Pts',(-58.8513437177779,6.3762354303884,2.81442815028499));
#234719=CARTESIAN_POINT('Ctrl Pts',(-58.8411231047665,6.37349561323695,
2.80471618166313));
#234720=CARTESIAN_POINT('Ctrl Pts',(-58.831254203655,6.37085007871755,2.79533842146225));
#234721=CARTESIAN_POINT('Ctrl Pts',(-58.8215519162594,6.3674514495407,2.78603515650236));
#234722=CARTESIAN_POINT('Ctrl Pts',(-58.8120753594638,6.36327195218627,
2.77685887346753));
#234723=CARTESIAN_POINT('Ctrl Pts',(-58.8031170454182,6.35932101824884,
2.76818441216578));
#234724=CARTESIAN_POINT('Ctrl Pts',(-58.7943596215162,6.35467192211847,
2.75962261521629));
#234725=CARTESIAN_POINT('Ctrl Pts',(-58.7858758685301,6.34926600747531,
2.75123537701669));
#234726=CARTESIAN_POINT('Ctrl Pts',(-58.7780624743556,6.34428725078,2.74351087134135));
#234727=CARTESIAN_POINT('Ctrl Pts',(-58.7704807832442,6.33866621241302,
2.73593399449869));
#234728=CARTESIAN_POINT('Ctrl Pts',(-58.7632157808999,6.33233133084779,
2.72857657812605));
#234729=CARTESIAN_POINT('Ctrl Pts',(-58.7610495038549,6.33044239704342,
2.72638274508339));
#234730=CARTESIAN_POINT('Ctrl Pts',(-58.7589116098633,6.32848982621476,
2.72420861709603));
#234731=CARTESIAN_POINT('Ctrl Pts',(-58.7568049797265,6.32647128889817,
2.72205663736711));
#234732=CARTESIAN_POINT('Ctrl Pts',(-58.7547198741578,6.32447337605831,
2.7199266455675));
#234733=CARTESIAN_POINT('Ctrl Pts',(-58.7526673708734,6.32241310885704,
2.71782089927869));
#234734=CARTESIAN_POINT('Ctrl Pts',(-58.7506524329181,6.32029074540098,
2.7157438731123));
#234735=CARTESIAN_POINT('Ctrl Pts',(-58.7505123180733,6.32014316039693,
2.71559944077471));
#234736=CARTESIAN_POINT('Ctrl Pts',(-58.7503723733987,6.31999527850334,
2.71545515216053));
#234737=CARTESIAN_POINT('Ctrl Pts',(-58.7502325999832,6.31984709900204,
2.71531100781714));
#234738=CARTESIAN_POINT('Ctrl Pts',(-58.7441044214168,6.31335036684086,
2.70899119176064));
#234739=CARTESIAN_POINT('Ctrl Pts',(-58.7383447881641,6.3062592537732,2.70298296066816));
#234740=CARTESIAN_POINT('Ctrl Pts',(-58.7330687140841,6.29859016886915,
2.69736727774112));
#234741=CARTESIAN_POINT('Ctrl Pts',(-58.728150496066,6.29144124886053,2.69213248525394));
#234742=CARTESIAN_POINT('Ctrl Pts',(-58.7236522470775,6.28378931333004,
2.68723866185425));
#234743=CARTESIAN_POINT('Ctrl Pts',(-58.7196964823227,6.27564783709119,
2.68278595829512));
#234744=CARTESIAN_POINT('Ctrl Pts',(-58.7182494123989,6.2726695797551,2.68115710172767));
#234745=CARTESIAN_POINT('Ctrl Pts',(-58.7168752520897,6.26962586933689,
2.67958763637783));
#234746=CARTESIAN_POINT('Ctrl Pts',(-58.7155811795664,6.26651766855731,
2.67808378645348));
#234747=CARTESIAN_POINT('Ctrl Pts',(-58.7152699983557,6.26577025010558,
2.67772216078583));
#234748=CARTESIAN_POINT('Ctrl Pts',(-58.7149635750523,6.26501853257418,
2.67736403603546));
#234749=CARTESIAN_POINT('Ctrl Pts',(-58.7146620123681,6.2642626046182,2.67700956934462));
#234750=CARTESIAN_POINT('Ctrl Pts',(-58.7143698735178,6.26353029941084,
2.67666617973787));
#234751=CARTESIAN_POINT('Ctrl Pts',(-58.7140822962414,6.26279404284355,
2.67632622314102));
#234752=CARTESIAN_POINT('Ctrl Pts',(-58.7137993735012,6.26205391928439,
2.67598984158756));
#234753=CARTESIAN_POINT('Ctrl Pts',(-58.7106996279152,6.25394501035232,
2.67230439292207));
#234754=CARTESIAN_POINT('Ctrl Pts',(-58.70815694202,6.24536644325953,2.66904964539964));
#234755=CARTESIAN_POINT('Ctrl Pts',(-58.7062958387084,6.23645973859696,
2.66640203566715));
#234756=CARTESIAN_POINT('Ctrl Pts',(-58.7055239836916,6.23276586269288,
2.66530399299427));
#234757=CARTESIAN_POINT('Ctrl Pts',(-58.7048690642115,6.22901585349537,
2.66430995142244));
#234758=CARTESIAN_POINT('Ctrl Pts',(-58.7043384037134,6.22522076267779,
2.66343053473343));
#234759=CARTESIAN_POINT('Ctrl Pts',(-58.7034333069351,6.21874783981215,
2.66193059792867));
#234760=CARTESIAN_POINT('Ctrl Pts',(-58.7028917011005,6.21214524099541,
2.66076519817109));
#234761=CARTESIAN_POINT('Ctrl Pts',(-58.7027523988019,6.20547453342054,
2.65997805604441));
#234762=CARTESIAN_POINT('Ctrl Pts',(-58.7026827476526,6.2021391796331,2.65958448498108));
#234763=CARTESIAN_POINT('Ctrl Pts',(-58.7027151167907,6.19878688248349,
2.65928526260744));
#234764=CARTESIAN_POINT('Ctrl Pts',(-58.7028544030468,6.19542538555006,
2.65908463971306));
#234765=CARTESIAN_POINT('Ctrl Pts',(-58.7029936893028,6.19206388861664,
2.65888401681868));
#234766=CARTESIAN_POINT('Ctrl Pts',(-58.7032398710655,6.18869323212196,
2.65878198860265));
#234767=CARTESIAN_POINT('Ctrl Pts',(-58.7035958781039,6.18532049829379,
2.65878198860265));
#234768=CARTESIAN_POINT('Origin',(-58.2637721346185,-0.0152399999998105,
2.83404198860261));
#234769=CARTESIAN_POINT('Ctrl Pts',(-62.6567671111299,-0.190499999999811,
2.8340419886026));
#234770=CARTESIAN_POINT('Ctrl Pts',(-62.667377440654,-0.19049999999981,
2.82419652440118));
#234771=CARTESIAN_POINT('Ctrl Pts',(-62.6779562874467,-0.189662809672919,
2.81438790575745));
#234772=CARTESIAN_POINT('Ctrl Pts',(-62.6884465439475,-0.188003604115047,
2.80466781257031));
#234773=CARTESIAN_POINT('Ctrl Pts',(-62.6985959295775,-0.186398312857871,
2.79526356453232));
#234774=CARTESIAN_POINT('Ctrl Pts',(-62.7086636500148,-0.184023290311302,
2.78594102496403));
#234775=CARTESIAN_POINT('Ctrl Pts',(-62.7185939622164,-0.180846261210727,
2.77675109088961));
#234776=CARTESIAN_POINT('Ctrl Pts',(-62.7279874260857,-0.177840987311753,
2.76805797913871));
#234777=CARTESIAN_POINT('Ctrl Pts',(-62.7372588214076,-0.174117798731389,
2.75948271210353));
#234778=CARTESIAN_POINT('Ctrl Pts',(-62.7463424082304,-0.169611579426802,
2.75108575573417));
#234779=CARTESIAN_POINT('Ctrl Pts',(-62.7547090486359,-0.165461025549195,
2.74335155163464));
#234780=CARTESIAN_POINT('Ctrl Pts',(-62.7629168328844,-0.16064587058866,
2.73576818686135));
#234781=CARTESIAN_POINT('Ctrl Pts',(-62.7708892610798,-0.155086395963295,
2.7284062616069));
#234782=CARTESIAN_POINT('Ctrl Pts',(-62.7732017594448,-0.153473803705747,
2.72627084693807));
#234783=CARTESIAN_POINT('Ctrl Pts',(-62.7754942590272,-0.151798403770687,
2.72415424587586));
#234784=CARTESIAN_POINT('Ctrl Pts',(-62.7777643638146,-0.150057792857475,
2.72205867173259));
#234785=CARTESIAN_POINT('Ctrl Pts',(-62.780225303358,-0.148170858716853,
2.7197869346286));
#234786=CARTESIAN_POINT('Ctrl Pts',(-62.7826571567199,-0.146210769553579,
2.7175441134076));
#234787=CARTESIAN_POINT('Ctrl Pts',(-62.7850565204095,-0.144175421825956,
2.71533341844257));
#234788=CARTESIAN_POINT('Ctrl Pts',(-62.791641592883,-0.138589394016422,
2.70926614876403));
#234789=CARTESIAN_POINT('Ctrl Pts',(-62.7979456687653,-0.132410786668851,
2.7034738186042));
#234790=CARTESIAN_POINT('Ctrl Pts',(-62.8038680995981,-0.125664597436552,
2.69804914171406));
#234791=CARTESIAN_POINT('Ctrl Pts',(-62.8092868022739,-0.119492200548109,
2.69308585687212));
#234792=CARTESIAN_POINT('Ctrl Pts',(-62.814374451894,-0.112844347459958,
2.68842799053189));
#234793=CARTESIAN_POINT('Ctrl Pts',(-62.8190433630435,-0.105708043832951,
2.68414767054218));
#234794=CARTESIAN_POINT('Ctrl Pts',(-62.8213367169484,-0.102202714803191,
2.68204519134556));
#234795=CARTESIAN_POINT('Ctrl Pts',(-62.8235285419788,-0.098579427453058,
2.68003431778509));
#234796=CARTESIAN_POINT('Ctrl Pts',(-62.8256051102647,-0.0948363533470471,
2.67812693945261));
#234797=CARTESIAN_POINT('Ctrl Pts',(-62.8259991188709,-0.0941261414934478,
2.67776503299213));
#234798=CARTESIAN_POINT('Ctrl Pts',(-62.8263888407139,-0.0934111032311,
2.67740659639934));
#234799=CARTESIAN_POINT('Ctrl Pts',(-62.826774159152,-0.0926913160159039,
2.67705178968865));
#234800=CARTESIAN_POINT('Ctrl Pts',(-62.8271474363889,-0.0919940221511827,
2.67670807068767));
#234801=CARTESIAN_POINT('Ctrl Pts',(-62.8275165811343,-0.0912922715308663,
2.67636775825275));
#234802=CARTESIAN_POINT('Ctrl Pts',(-62.8278814873655,-0.0905861384167767,
2.67603099699265));
#234803=CARTESIAN_POINT('Ctrl Pts',(-62.8318581602824,-0.0828908452418365,
2.67236104217145));
#234804=CARTESIAN_POINT('Ctrl Pts',(-62.8353337180911,-0.0746698316632022,
2.66911440541497));
#234805=CARTESIAN_POINT('Ctrl Pts',(-62.8381654210184,-0.0660491922300273,
2.66646778189657));
#234806=CARTESIAN_POINT('Ctrl Pts',(-62.8393612667488,-0.0624086426655782,
2.66535009634994));
#234807=CARTESIAN_POINT('Ctrl Pts',(-62.8404425512864,-0.0586971697057279,
2.66433897912359));
#234808=CARTESIAN_POINT('Ctrl Pts',(-62.8414000604479,-0.0549254519862922,
2.66344564884803));
#234809=CARTESIAN_POINT('Ctrl Pts',(-62.8430124819501,-0.0485739735920286,
2.66194130298596));
#234810=CARTESIAN_POINT('Ctrl Pts',(-62.8442717146911,-0.0420529246950825,
2.66077206705431));
#234811=CARTESIAN_POINT('Ctrl Pts',(-62.8451307298764,-0.0354197192405181,
2.65998225155726));
#234812=CARTESIAN_POINT('Ctrl Pts',(-62.8453454836727,-0.0337614178768769,
2.659784797683));
#234813=CARTESIAN_POINT('Ctrl Pts',(-62.8455349903695,-0.0320960919383993,
2.65961098966634));
#234814=CARTESIAN_POINT('Ctrl Pts',(-62.8456982067485,-0.0304246312363976,
2.65946139030513));
#234815=CARTESIAN_POINT('Ctrl Pts',(-62.845943031317,-0.027917440183395,
2.65923699126332));
#234816=CARTESIAN_POINT('Ctrl Pts',(-62.8461286892223,-0.0253964615337772,
2.65906707562454));
#234817=CARTESIAN_POINT('Ctrl Pts',(-62.846253337618,-0.0228647168029203,
2.65895332562931));
#234818=CARTESIAN_POINT('Ctrl Pts',(-62.8463779860137,-0.0203329720720634,
2.65883957563409));
#234819=CARTESIAN_POINT('Ctrl Pts',(-62.8464416340693,-0.0177904683739631,
2.65878198860261));
#234820=CARTESIAN_POINT('Ctrl Pts',(-62.8464427007196,-0.0152399999998093,
2.65878198860261));
#234821=CARTESIAN_POINT('Ctrl Pts',(-59.0285534841296,-0.0152399999998097,
2.65878198860261));
#234822=CARTESIAN_POINT('Ctrl Pts',(-59.0285496414744,-0.0238699985093663,
2.65878198860261));
#234823=CARTESIAN_POINT('Ctrl Pts',(-59.0292582026622,-0.0324255116358099,
2.65945335517858));
#234824=CARTESIAN_POINT('Ctrl Pts',(-59.0305954788491,-0.0407807192232887,
2.66072561226611));
#234825=CARTESIAN_POINT('Ctrl Pts',(-59.0314592220532,-0.0461773260306079,
2.66154735980347));
#234826=CARTESIAN_POINT('Ctrl Pts',(-59.0325843328199,-0.051490526841021,
2.66261895766888));
#234827=CARTESIAN_POINT('Ctrl Pts',(-59.0339399880044,-0.0566895722960612,
2.66391429251027));
#234828=CARTESIAN_POINT('Ctrl Pts',(-59.0357368312948,-0.0635806092272726,
2.66563118464123));
#234829=CARTESIAN_POINT('Ctrl Pts',(-59.0379438906768,-0.0702685278899484,
2.66774105138698));
#234830=CARTESIAN_POINT('Ctrl Pts',(-59.0405007795597,-0.0766865040602752,
2.67016894181749));
#234831=CARTESIAN_POINT('Ctrl Pts',(-59.0417792240012,-0.0798954921454386,
2.67138288703274));
#234832=CARTESIAN_POINT('Ctrl Pts',(-59.0431451240706,-0.0830371938947498,
2.6726761316755));
#234833=CARTESIAN_POINT('Ctrl Pts',(-59.0445909239228,-0.0861046703636156,
2.67403835432552));
#234834=CARTESIAN_POINT('Ctrl Pts',(-59.0453138238489,-0.0876384085980485,
2.67471946565053));
#234835=CARTESIAN_POINT('Ctrl Pts',(-59.0460566986718,-0.0891536069434453,
2.67541781389522));
#234836=CARTESIAN_POINT('Ctrl Pts',(-59.0468186034775,-0.0906495011918796,
2.67613207244168));
#234837=CARTESIAN_POINT('Ctrl Pts',(-59.047009079679,-0.0910234747539882,
2.67631063707829));
#234838=CARTESIAN_POINT('Ctrl Pts',(-59.0472007452523,-0.0913962421595167,
2.67649019601844));
#234839=CARTESIAN_POINT('Ctrl Pts',(-59.0473935854286,-0.0917677921725184,
2.67667072836655));
#234840=CARTESIAN_POINT('Ctrl Pts',(-59.0479721059574,-0.0928824422115236,
2.67721232541089));
#234841=CARTESIAN_POINT('Ctrl Pts',(-59.0485611979309,-0.0939861339736083,
2.67776268340046));
#234842=CARTESIAN_POINT('Ctrl Pts',(-59.0491604624443,-0.0950785796747284,
2.67832123541515));
#234843=CARTESIAN_POINT('Ctrl Pts',(-59.0533816042976,-0.102773626133062,
2.68225560368446));
#234844=CARTESIAN_POINT('Ctrl Pts',(-59.0580834293367,-0.109958823466275,
2.68661792998894));
#234845=CARTESIAN_POINT('Ctrl Pts',(-59.0631465696372,-0.116642428646653,
2.69130986622588));
#234846=CARTESIAN_POINT('Ctrl Pts',(-59.0656021872116,-0.119883969936718,
2.69358545023061));
#234847=CARTESIAN_POINT('Ctrl Pts',(-59.0681433715119,-0.123007567717954,
2.69593918853473));
#234848=CARTESIAN_POINT('Ctrl Pts',(-59.0707593633743,-0.126014035556225,
2.69836306235474));
#234849=CARTESIAN_POINT('Ctrl Pts',(-59.0747642641416,-0.130616727760851,
2.70207384382207));
#234850=CARTESIAN_POINT('Ctrl Pts',(-59.0789414743143,-0.134943070277078,
2.70594760814207));
#234851=CARTESIAN_POINT('Ctrl Pts',(-59.0832455674828,-0.138985142830541,
2.70995196345687));
#234852=CARTESIAN_POINT('Ctrl Pts',(-59.0852444106167,-0.140862302235282,
2.71181160678085));
#234853=CARTESIAN_POINT('Ctrl Pts',(-59.0872703932641,-0.142678271526929,
2.71369962772079));
#234854=CARTESIAN_POINT('Ctrl Pts',(-59.0893195943183,-0.144431197308552,
2.71561183138641));
#234855=CARTESIAN_POINT('Ctrl Pts',(-59.0894766575048,-0.144565552162836,
2.71575839426292));
#234856=CARTESIAN_POINT('Ctrl Pts',(-59.0896338466133,-0.144699568925602,
2.71590508903189));
#234857=CARTESIAN_POINT('Ctrl Pts',(-59.0897911602042,-0.144833247842891,
2.71605191409891));
#234858=CARTESIAN_POINT('Ctrl Pts',(-59.0920009418701,-0.146711033601897,
2.71811436362732));
#234859=CARTESIAN_POINT('Ctrl Pts',(-59.0942367399983,-0.148520654544703,
2.72020091026939));
#234860=CARTESIAN_POINT('Ctrl Pts',(-59.0964928714565,-0.150262619641085,
2.72230624862161));
#234861=CARTESIAN_POINT('Ctrl Pts',(-59.1045829576263,-0.156508996678588,
2.7298556175308));
#234862=CARTESIAN_POINT('Ctrl Pts',(-59.1129958342949,-0.161935290145438,
2.73770089914304));
#234863=CARTESIAN_POINT('Ctrl Pts',(-59.1216309196483,-0.166622470787294,
2.74574823347045));
#234864=CARTESIAN_POINT('Ctrl Pts',(-59.1311200109807,-0.171773211443692,
2.75459144546993));
#234865=CARTESIAN_POINT('Ctrl Pts',(-59.1408779306735,-0.176031864362169,
2.76367911754237));
#234866=CARTESIAN_POINT('Ctrl Pts',(-59.1508087658098,-0.179468536017047,
2.77292162564692));
#234867=CARTESIAN_POINT('Ctrl Pts',(-59.1615315754577,-0.183179278917524,
2.78290121484709));
#234868=CARTESIAN_POINT('Ctrl Pts',(-59.172457014285,-0.185932239424576,
2.79306229500181));
#234869=CARTESIAN_POINT('Ctrl Pts',(-59.1834936683142,-0.187766286099724,
2.80331916685261));
#234870=CARTESIAN_POINT('Ctrl Pts',(-59.1944377361557,-0.189584947007655,
2.81348999408699));
#234871=CARTESIAN_POINT('Ctrl Pts',(-59.2054925958117,-0.19049999999981,
2.82375635966878));
#234872=CARTESIAN_POINT('Ctrl Pts',(-59.2165773020941,-0.190499999999811,
2.83404198860261));
#234873=CARTESIAN_POINT('Origin',(1.12442271988212E-14,0.0152400000001895,
2.83404198860262));
#234874=CARTESIAN_POINT('Ctrl Pts',(-62.8464427007196,0.0152400000001907,
2.6587819886026));
#234875=CARTESIAN_POINT('Ctrl Pts',(-62.8464391086779,0.023828933390642,
2.6587819886026));
#234876=CARTESIAN_POINT('Ctrl Pts',(-62.8457180711405,0.0323412407626657,
2.65944603041842));
#234877=CARTESIAN_POINT('Ctrl Pts',(-62.8443658068291,0.0406531130503683,
2.66070439264048));
#234878=CARTESIAN_POINT('Ctrl Pts',(-62.8435017743089,0.0459640037535742,
2.66150842619575));
#234879=CARTESIAN_POINT('Ctrl Pts',(-62.8423809556999,0.0511932363892055,
2.66255428265354));
#234880=CARTESIAN_POINT('Ctrl Pts',(-62.841033859251,0.0563116129576012,
2.66381699700651));
#234881=CARTESIAN_POINT('Ctrl Pts',(-62.8391953428955,0.063297169962393,
2.66554034873251));
#234882=CARTESIAN_POINT('Ctrl Pts',(-62.8369299537504,0.0700734120985513,
2.66766759643955));
#234883=CARTESIAN_POINT('Ctrl Pts',(-62.8343031482014,0.0765705776096623,
2.6701201278313));
#234884=CARTESIAN_POINT('Ctrl Pts',(-62.8329897454269,0.0798191603652178,
2.67134639352718));
#234885=CARTESIAN_POINT('Ctrl Pts',(-62.8315859904681,0.0829981827955089,
2.67265375584994));
#234886=CARTESIAN_POINT('Ctrl Pts',(-62.8301000734874,0.0861004173280608,
2.67403135126922));
#234887=CARTESIAN_POINT('Ctrl Pts',(-62.8293571149971,0.0876515345943367,
2.67472014897886));
#234888=CARTESIAN_POINT('Ctrl Pts',(-62.8285936160519,0.0891834722999017,
2.67542649668614));
#234889=CARTESIAN_POINT('Ctrl Pts',(-62.82781060087,0.0906954364280678,
2.67614899656084));
#234890=CARTESIAN_POINT('Ctrl Pts',(-62.8276148470745,0.0910734274601094,
2.67632962152951));
#234891=CARTESIAN_POINT('Ctrl Pts',(-62.8274178735164,0.0914501705145361,
2.67651125590932));
#234892=CARTESIAN_POINT('Ctrl Pts',(-62.8272196962038,0.0918256539330444,
2.67669387767505));
#234893=CARTESIAN_POINT('Ctrl Pts',(-62.8266251642659,0.0929521041885693,
2.67724174297226));
#234894=CARTESIAN_POINT('Ctrl Pts',(-62.826019798519,0.0940672158688541,
2.67779849504729));
#234895=CARTESIAN_POINT('Ctrl Pts',(-62.8254040313373,0.0951706907490459,
2.6783635361799));
#234896=CARTESIAN_POINT('Ctrl Pts',(-62.8211486980556,0.102796386827685,
2.68226832098886));
#234897=CARTESIAN_POINT('Ctrl Pts',(-62.8164204928785,0.109916699411551,
2.68659153751365));
#234898=CARTESIAN_POINT('Ctrl Pts',(-62.8113377077397,0.116542502759829,
2.69123699486148));
#234899=CARTESIAN_POINT('Ctrl Pts',(-62.8088115774776,0.119835508836568,
2.6935457744119));
#234900=CARTESIAN_POINT('Ctrl Pts',(-62.8061972539433,0.123006400629482,
2.69593478828095));
#234901=CARTESIAN_POINT('Ctrl Pts',(-62.8035061084566,0.126056303770164,
2.69839565261202));
#234902=CARTESIAN_POINT('Ctrl Pts',(-62.7975690395532,0.132784845643478,
2.70382468689028));
#234903=CARTESIAN_POINT('Ctrl Pts',(-62.7912680187378,0.138932019324877,
2.70961155815069));
#234904=CARTESIAN_POINT('Ctrl Pts',(-62.7847385034067,0.144445113413363,
2.7156270136175));
#234905=CARTESIAN_POINT('Ctrl Pts',(-62.7823531891148,0.146459116207659,
2.7178245353584));
#234906=CARTESIAN_POINT('Ctrl Pts',(-62.7799396422115,0.148396130391172,
2.72005051502385));
#234907=CARTESIAN_POINT('Ctrl Pts',(-62.7775029828616,0.150257579786679,
2.72229986760099));
#234908=CARTESIAN_POINT('Ctrl Pts',(-62.7693185019449,0.156509991333616,
2.72985520488837));
#234909=CARTESIAN_POINT('Ctrl Pts',(-62.7608162581028,0.161942805717951,
2.73770845534464));
#234910=CARTESIAN_POINT('Ctrl Pts',(-62.7520965944505,0.166635979461278,
2.74576706701618));
#234911=CARTESIAN_POINT('Ctrl Pts',(-62.7425126511845,0.171794333348195,
2.75462443584854));
#234912=CARTESIAN_POINT('Ctrl Pts',(-62.7326655363515,0.176059615357362,
2.76373036322965));
#234913=CARTESIAN_POINT('Ctrl Pts',(-62.7226511116318,0.179500292056582,
2.77299664636558));
#234914=CARTESIAN_POINT('Ctrl Pts',(-62.7118651471247,0.183206048282925,
2.78297683033166));
#234915=CARTESIAN_POINT('Ctrl Pts',(-62.7008840239677,0.185955767119051,
2.79314401478533));
#234916=CARTESIAN_POINT('Ctrl Pts',(-62.689799127429,0.187785458035066,
2.80341452427521));
#234917=CARTESIAN_POINT('Ctrl Pts',(-62.6788639144194,0.189590441946164,
2.81354634721084));
#234918=CARTESIAN_POINT('Ctrl Pts',(-62.667826278274,0.190500000000189,
2.82378004209064));
#234919=CARTESIAN_POINT('Ctrl Pts',(-62.6567671111299,0.190500000000189,
2.83404198860261));
#234920=CARTESIAN_POINT('Ctrl Pts',(-59.2165773020941,0.190500000000189,
2.8340419886026));
#234921=CARTESIAN_POINT('Ctrl Pts',(-59.2059936184299,0.190500000000189,
2.82422126443094));
#234922=CARTESIAN_POINT('Ctrl Pts',(-59.1954479901474,0.189665225488926,
2.81442815028678));
#234923=CARTESIAN_POINT('Ctrl Pts',(-59.1849969778479,0.188008762314532,
2.80471618166582));
#234924=CARTESIAN_POINT('Ctrl Pts',(-59.174905605952,0.186409301377575,
2.79533842146548));
#234925=CARTESIAN_POINT('Ctrl Pts',(-59.1649012152174,0.184043455438921,
2.78603515650611));
#234926=CARTESIAN_POINT('Ctrl Pts',(-59.1550396955563,0.180877423727649,
2.77685887347177));
#234927=CARTESIAN_POINT('Ctrl Pts',(-59.1457174710397,0.17788453222071,
2.76818441217027));
#234928=CARTESIAN_POINT('Ctrl Pts',(-59.1365220583483,0.174176304388436,
2.75962261522101));
#234929=CARTESIAN_POINT('Ctrl Pts',(-59.1275197082988,0.169686797574166,
2.7512353770216));
#234930=CARTESIAN_POINT('Ctrl Pts',(-59.1192286949288,0.165552037115291,
2.74351087134631));
#234931=CARTESIAN_POINT('Ctrl Pts',(-59.1111009786121,0.160754293905865,
2.73593399450368));
#234932=CARTESIAN_POINT('Ctrl Pts',(-59.1032135992758,0.155213515015811,
2.72857657813105));
#234933=CARTESIAN_POINT('Ctrl Pts',(-59.1008617419736,0.153561366597817,
2.72638274508667));
#234934=CARTESIAN_POINT('Ctrl Pts',(-59.0985314603591,0.151842962928774,
2.72420861709764));
#234935=CARTESIAN_POINT('Ctrl Pts',(-59.096225375957,0.15005568618033,2.72205663736707));
#234936=CARTESIAN_POINT('Ctrl Pts',(-59.0939428540559,0.148286670996897,
2.71992664556746));
#234937=CARTESIAN_POINT('Ctrl Pts',(-59.0916862380348,0.146452235169095,
2.71782089927864));
#234938=CARTESIAN_POINT('Ctrl Pts',(-59.0894604907299,0.144552116610158,
2.71574387311226));
#234939=CARTESIAN_POINT('Ctrl Pts',(-59.0893057166152,0.144419986081611,
2.71559944077466));
#234940=CARTESIAN_POINT('Ctrl Pts',(-59.0891510807051,0.144287542502291,
2.71545515216049));
#234941=CARTESIAN_POINT('Ctrl Pts',(-59.0889965840074,0.144154785044136,
2.7153110078171));
#234942=CARTESIAN_POINT('Ctrl Pts',(-59.0822228828154,0.13833421174979,
2.70899119176073));
#234943=CARTESIAN_POINT('Ctrl Pts',(-59.0757535782847,0.131883990154492,
2.70298296066836));
#234944=CARTESIAN_POINT('Ctrl Pts',(-59.069704769431,0.124808417215811,
2.69736727774142));
#234945=CARTESIAN_POINT('Ctrl Pts',(-59.0640662283035,0.118212753510756,
2.69213248525446));
#234946=CARTESIAN_POINT('Ctrl Pts',(-59.0587927761317,0.111072931138274,
2.68723866185495));
#234947=CARTESIAN_POINT('Ctrl Pts',(-59.0540076654703,0.103389544769389,
2.68278595829597));
#234948=CARTESIAN_POINT('Ctrl Pts',(-59.052257210084,0.100578862633506,
2.6811571017282));
#234949=CARTESIAN_POINT('Ctrl Pts',(-59.0505724231959,0.0976954648443338,
2.67958763637807));
#234950=CARTESIAN_POINT('Ctrl Pts',(-59.048960544286,0.0947395585255326,
2.67808378645345));
#234951=CARTESIAN_POINT('Ctrl Pts',(-59.0485729412563,0.0940287618040365,
2.6777221607858));
#234952=CARTESIAN_POINT('Ctrl Pts',(-59.0481896206935,0.0933131922169409,
2.67736403603543));
#234953=CARTESIAN_POINT('Ctrl Pts',(-59.0478106940137,0.0925929271973547,
2.67700956934459));
#234954=CARTESIAN_POINT('Ctrl Pts',(-59.0474436087926,0.0918951704596305,
2.67666617973784));
#234955=CARTESIAN_POINT('Ctrl Pts',(-59.047080647127,0.0911930071936125,
2.67632622314099));
#234956=CARTESIAN_POINT('Ctrl Pts',(-59.0467219102889,0.0904865115880142,
2.67598984158753));
#234957=CARTESIAN_POINT('Ctrl Pts',(-59.042791533644,0.0827460357498325,
2.6723043929219));
#234958=CARTESIAN_POINT('Ctrl Pts',(-59.0393660724128,0.0744802459940113,
2.66904964539934));
#234959=CARTESIAN_POINT('Ctrl Pts',(-59.0365841602687,0.0658168714602655,
2.6664020356668));
#234960=CARTESIAN_POINT('Ctrl Pts',(-59.0354304183828,0.0622239118140033,
2.66530399299404));
#234961=CARTESIAN_POINT('Ctrl Pts',(-59.0343871039216,0.0585629032864118,
2.66430995142232));
#234962=CARTESIAN_POINT('Ctrl Pts',(-59.0334626554261,0.0548440715001653,
2.66343053473339));
#234963=CARTESIAN_POINT('Ctrl Pts',(-59.0318859121827,0.0485012163585984,
2.66193059792863));
#234964=CARTESIAN_POINT('Ctrl Pts',(-59.0306571138137,0.0419914004946155,
2.66076519817106));
#234965=CARTESIAN_POINT('Ctrl Pts',(-59.0298212958155,0.0353717968090289,
2.65997805604438));
#234966=CARTESIAN_POINT('Ctrl Pts',(-59.0294033868165,0.0320619949662357,
2.65958448498104));
#234967=CARTESIAN_POINT('Ctrl Pts',(-59.0290851681637,0.02872467855488,
2.65928526260739));
#234968=CARTESIAN_POINT('Ctrl Pts',(-59.0288723192864,0.025367036875067,
2.65908463971302));
#234969=CARTESIAN_POINT('Ctrl Pts',(-59.0286594704092,0.022009395195254,
2.65888401681864));
#234970=CARTESIAN_POINT('Ctrl Pts',(-59.0285519740191,0.0186314705081981,
2.65878198860261));
#234971=CARTESIAN_POINT('Ctrl Pts',(-59.0285534841296,0.0152400000001907,
2.65878198860261));
#234972=CARTESIAN_POINT('Origin',(-57.9430040808457,-6.10537907909404,2.83404198860257));
#234973=CARTESIAN_POINT('Ctrl Pts',(-62.2936141127569,-6.73887200051357,
2.83404198860256));
#234974=CARTESIAN_POINT('Ctrl Pts',(-62.3041663177858,-6.7399810819535,
2.82419652440043));
#234975=CARTESIAN_POINT('Ctrl Pts',(-62.3147747227674,-6.74025426844116,
2.81438790575611));
#234976=CARTESIAN_POINT('Ctrl Pts',(-62.3253809467531,-6.73970068257615,
2.80466781256847));
#234977=CARTESIAN_POINT('Ctrl Pts',(-62.3356425316152,-6.73916508495536,
2.7952635645301));
#234978=CARTESIAN_POINT('Ctrl Pts',(-62.3459033574839,-6.73785543637658,
2.7859410249615));
#234979=CARTESIAN_POINT('Ctrl Pts',(-62.3561113603662,-6.73573381164783,
2.77675109088682));
#234980=CARTESIAN_POINT('Ctrl Pts',(-62.3657675025203,-6.73372688529656,
2.7680579791357));
#234981=CARTESIAN_POINT('Ctrl Pts',(-62.3753772873497,-6.7309932174379,
2.75948271210035));
#234982=CARTESIAN_POINT('Ctrl Pts',(-62.3848821415129,-6.7274611770454,
2.75108575573083));
#234983=CARTESIAN_POINT('Ctrl Pts',(-62.3936367996058,-6.72420791240022,
2.74335155163112));
#234984=CARTESIAN_POINT('Ctrl Pts',(-62.4023029415022,-6.72027708243635,
2.73576818685769));
#234985=CARTESIAN_POINT('Ctrl Pts',(-62.4108128192413,-6.71558140886203,
2.72840626160309));
#234986=CARTESIAN_POINT('Ctrl Pts',(-62.4132812112875,-6.71421937245472,
2.72627084693553));
#234987=CARTESIAN_POINT('Ctrl Pts',(-62.4157362792965,-6.71279278199497,
2.72415424587456));
#234988=CARTESIAN_POINT('Ctrl Pts',(-62.4181758915949,-6.71129899689621,
2.72205867173251));
#234989=CARTESIAN_POINT('Ctrl Pts',(-62.42082058818,-6.70967963780692,2.71978693462854));
#234990=CARTESIAN_POINT('Ctrl Pts',(-62.4234440047028,-6.70798448411198,
2.71754411340754));
#234991=CARTESIAN_POINT('Ctrl Pts',(-62.4260429761973,-6.70621108803147,
2.71533341844251));
#234992=CARTESIAN_POINT('Ctrl Pts',(-62.4331758738575,-6.70134398857293,
2.70926614876399));
#234993=CARTESIAN_POINT('Ctrl Pts',(-62.4400912556837,-6.69585818364719,
2.70347381860416));
#234994=CARTESIAN_POINT('Ctrl Pts',(-62.4466864116141,-6.68976801333912,
2.69804914171402));
#234995=CARTESIAN_POINT('Ctrl Pts',(-62.4527206212311,-6.68419583815025,
2.69308585687207));
#234996=CARTESIAN_POINT('Ctrl Pts',(-62.4584752900415,-6.6781162068933,
2.68842799053184));
#234997=CARTESIAN_POINT('Ctrl Pts',(-62.4638645712588,-6.67150703079182,
2.68414767054212));
#234998=CARTESIAN_POINT('Ctrl Pts',(-62.4665117685878,-6.66826062508068,
2.68204519134551));
#234999=CARTESIAN_POINT('Ctrl Pts',(-62.46907032323,-6.66488629457996,2.68003431778505));
#235000=CARTESIAN_POINT('Ctrl Pts',(-62.4715267736418,-6.66138078591736,
2.67812693945259));
#235001=CARTESIAN_POINT('Ctrl Pts',(-62.4719928611813,-6.66071564979273,
2.67776503299211));
#235002=CARTESIAN_POINT('Ctrl Pts',(-62.4724551899379,-6.66004526561014,
2.67740659639931));
#235003=CARTESIAN_POINT('Ctrl Pts',(-62.4729136358128,-6.65936969820883,
2.67705178968862));
#235004=CARTESIAN_POINT('Ctrl Pts',(-62.4733577552541,-6.6587152422888,
2.67670807068765));
#235005=CARTESIAN_POINT('Ctrl Pts',(-62.4737982306998,-6.65805592206477,
2.67636775825272));
#235006=CARTESIAN_POINT('Ctrl Pts',(-62.4742349489458,-6.65739180030934,
2.67603099699262));
#235007=CARTESIAN_POINT('Ctrl Pts',(-62.4789942144024,-6.65015433826441,
2.67236104217138));
#235008=CARTESIAN_POINT('Ctrl Pts',(-62.4833100626577,-6.64234165497498,
2.66911440541486));
#235009=CARTESIAN_POINT('Ctrl Pts',(-62.4870273554126,-6.63406423386192,
2.66646778189644));
#235010=CARTESIAN_POINT('Ctrl Pts',(-62.4885971912262,-6.63056862752551,
2.66535009634985));
#235011=CARTESIAN_POINT('Ctrl Pts',(-62.4900605069389,-6.62699051141405,
2.66433897912353));
#235012=CARTESIAN_POINT('Ctrl Pts',(-62.491407022622,-6.62333954252025,
2.663445648848));
#235013=CARTESIAN_POINT('Ctrl Pts',(-62.4936745213867,-6.61719140213097,
2.66194130298593));
#235014=CARTESIAN_POINT('Ctrl Pts',(-62.495608491139,-6.6108377018855,2.66077206705428));
#235015=CARTESIAN_POINT('Ctrl Pts',(-62.497156159322,-6.6043306253617,2.65998225155722));
#235016=CARTESIAN_POINT('Ctrl Pts',(-62.4975430763677,-6.60270385623075,
2.65978479768295));
#235017=CARTESIAN_POINT('Ctrl Pts',(-62.4979056188881,-6.60106746196581,
2.6596109896663));
#235018=CARTESIAN_POINT('Ctrl Pts',(-62.4982426563693,-6.5994222184577,
2.65946139030509));
#235019=CARTESIAN_POINT('Ctrl Pts',(-62.4987482125911,-6.59695435319553,
2.65923699126328));
#235020=CARTESIAN_POINT('Ctrl Pts',(-62.4991963674672,-6.59446659126626,
2.65906707562449));
#235021=CARTESIAN_POINT('Ctrl Pts',(-62.499584972412,-6.59196174500319,
2.65895332562927));
#235022=CARTESIAN_POINT('Ctrl Pts',(-62.4999735773569,-6.58945689874012,
2.65883957563405));
#235023=CARTESIAN_POINT('Ctrl Pts',(-62.5003026407461,-6.58693497617675,
2.65878198860256));
#235024=CARTESIAN_POINT('Ctrl Pts',(-62.500570298093,-6.58439859103053,
2.65878198860256));
#235025=CARTESIAN_POINT('Ctrl Pts',(-58.7035958781038,-6.1853204982942,
2.65878198860256));
#235026=CARTESIAN_POINT('Ctrl Pts',(-58.7026899760169,-6.19390281910169,
2.65878198860256));
#235027=CARTESIAN_POINT('Ctrl Pts',(-58.7025003609928,-6.20248552904371,
2.65945335517847));
#235028=CARTESIAN_POINT('Ctrl Pts',(-58.7029569544313,-6.21093474935418,
2.66072561226587));
#235029=CARTESIAN_POINT('Ctrl Pts',(-58.7032518669434,-6.21639207873494,
2.66154735980326));
#235030=CARTESIAN_POINT('Ctrl Pts',(-58.7038154335198,-6.22179377937522,
2.66261895766873));
#235031=CARTESIAN_POINT('Ctrl Pts',(-58.7046202140516,-6.22710604846881,
2.66391429251021));
#235032=CARTESIAN_POINT('Ctrl Pts',(-58.7056869045457,-6.23414715684659,
2.66563118464117));
#235033=CARTESIAN_POINT('Ctrl Pts',(-58.7071827955652,-6.24102913891662,
2.66774105138693));
#235034=CARTESIAN_POINT('Ctrl Pts',(-58.7090548163569,-6.24767922440765,
2.67016894181744));
#235035=CARTESIAN_POINT('Ctrl Pts',(-58.7099908267528,-6.25100426715317,
2.67138288703269));
#235036=CARTESIAN_POINT('Ctrl Pts',(-58.7110208470228,-6.25427153376681,
2.67267613167545));
#235037=CARTESIAN_POINT('Ctrl Pts',(-58.7121380880307,-6.25747333351537,
2.67403835432547));
#235038=CARTESIAN_POINT('Ctrl Pts',(-58.7126967085347,-6.25907423338965,
2.67471946565048));
#235039=CARTESIAN_POINT('Ctrl Pts',(-58.7132771324571,-6.26065878288363,
2.67541781389518));
#235040=CARTESIAN_POINT('Ctrl Pts',(-58.7138784999415,-6.26222612320535,
2.67613207244164));
#235041=CARTESIAN_POINT('Ctrl Pts',(-58.7140288418126,-6.26261795828578,
2.67631063707825));
#235042=CARTESIAN_POINT('Ctrl Pts',(-58.7141804926178,-6.26300871814029,
2.6764901960184));
#235043=CARTESIAN_POINT('Ctrl Pts',(-58.7143334388435,-6.26339839005073,
2.67667072836651));
#235044=CARTESIAN_POINT('Ctrl Pts',(-58.7147922775207,-6.26456740578205,
2.67721232541085));
#235045=CARTESIAN_POINT('Ctrl Pts',(-58.715262775183,-6.2657266282839,2.67776268340042));
#235046=CARTESIAN_POINT('Ctrl Pts',(-58.7157445651923,-6.26687572965184,
2.67832123541511));
#235047=CARTESIAN_POINT('Ctrl Pts',(-58.7191382318077,-6.27496985131151,
2.68225560368434));
#235048=CARTESIAN_POINT('Ctrl Pts',(-58.7230632421216,-6.28260716192766,
2.68661792998871));
#235049=CARTESIAN_POINT('Ctrl Pts',(-58.7274000190311,-6.28978339589433,
2.69130986622554));
#235050=CARTESIAN_POINT('Ctrl Pts',(-58.729503351146,-6.29326386161364,
2.69358545023036));
#235051=CARTESIAN_POINT('Ctrl Pts',(-58.7317041096969,-6.29663597408935,
2.69593918853458));
#235052=CARTESIAN_POINT('Ctrl Pts',(-58.7339915094193,-6.29989941779167,
2.6983630623547));
#235053=CARTESIAN_POINT('Ctrl Pts',(-58.7374933585782,-6.30489552208956,
2.70207384382203));
#235054=CARTESIAN_POINT('Ctrl Pts',(-58.7411954596216,-6.30963480180892,
2.70594760814204));
#235055=CARTESIAN_POINT('Ctrl Pts',(-58.7450534628849,-6.31410463171066,
2.70995196345684));
#235056=CARTESIAN_POINT('Ctrl Pts',(-58.7468451395591,-6.31618044384087,
2.71181160678082));
#235057=CARTESIAN_POINT('Ctrl Pts',(-58.7486702031823,-6.31819823791547,
2.71369962772075));
#235058=CARTESIAN_POINT('Ctrl Pts',(-58.7505249478605,-6.32015576082336,
2.71561183138637));
#235059=CARTESIAN_POINT('Ctrl Pts',(-58.750667106732,-6.32030579724123,
2.71575839426288));
#235060=CARTESIAN_POINT('Ctrl Pts',(-58.7508094261758,-6.3204555105821,
2.71590508903185));
#235061=CARTESIAN_POINT('Ctrl Pts',(-58.7509519047345,-6.32060490094019,
2.71605191409887));
#235062=CARTESIAN_POINT('Ctrl Pts',(-58.7529532989256,-6.32270338507403,
2.71811436362729));
#235063=CARTESIAN_POINT('Ctrl Pts',(-58.7549876922214,-6.32473679726649,
2.72020091026935));
#235064=CARTESIAN_POINT('Ctrl Pts',(-58.7570493794209,-6.32670504965006,
2.72230624862158));
#235065=CARTESIAN_POINT('Ctrl Pts',(-58.7644422230593,-6.33376285265554,
2.7298556175307));
#235066=CARTESIAN_POINT('Ctrl Pts',(-58.7722418109919,-6.34003880538879,
2.73770089914288));
#235067=CARTESIAN_POINT('Ctrl Pts',(-58.7803396486547,-6.3456029213668,
2.74574823347021));
#235068=CARTESIAN_POINT('Ctrl Pts',(-58.7892383587461,-6.35171732586157,
2.75459144546946));
#235069=CARTESIAN_POINT('Ctrl Pts',(-58.7984976730884,-6.35697262978384,
2.76367911754164));
#235070=CARTESIAN_POINT('Ctrl Pts',(-58.8080148760636,-6.3614285299275,
2.77292162564593));
#235071=CARTESIAN_POINT('Ctrl Pts',(-58.8182910667848,-6.36623978380432,
2.78290121484556));
#235072=CARTESIAN_POINT('Ctrl Pts',(-58.8288688921832,-6.37011968263671,
2.79306229499971));
#235073=CARTESIAN_POINT('Ctrl Pts',(-58.8396533761857,-6.37309732669757,
2.80331916684993));
#235074=CARTESIAN_POINT('Ctrl Pts',(-58.8503473894494,-6.37604999138454,
2.81348999408516));
#235075=CARTESIAN_POINT('Ctrl Pts',(-58.8612460403454,-6.37811557911242,
2.82375635966784));
#235076=CARTESIAN_POINT('Ctrl Pts',(-58.872270023448,-6.37927424642599,
2.83404198860256));
#235077=CARTESIAN_POINT('Origin',(-0.00159301378018793,0.0151565136856025,
2.83404198860262));
#235078=CARTESIAN_POINT('Ctrl Pts',(-62.5037563256534,-6.5540855636597,
2.65878198860256));
#235079=CARTESIAN_POINT('Ctrl Pts',(-62.5046505412977,-6.54554330587448,
2.65878198860256));
#235080=CARTESIAN_POINT('Ctrl Pts',(-62.5048232320878,-6.53700226086719,
2.65944603041837));
#235081=CARTESIAN_POINT('Ctrl Pts',(-62.5043472028589,-6.5285945717752,
2.66070439264043));
#235082=CARTESIAN_POINT('Ctrl Pts',(-62.5040430428431,-6.5232224586954,
2.6615084261957));
#235083=CARTESIAN_POINT('Ctrl Pts',(-62.5034749678471,-6.51790471489647,
2.66255428265349));
#235084=CARTESIAN_POINT('Ctrl Pts',(-62.5026702669707,-6.51267356740878,
2.66381699700646));
#235085=CARTESIAN_POINT('Ctrl Pts',(-62.5015720117389,-6.50553410072683,
2.66554034873246));
#235086=CARTESIAN_POINT('Ctrl Pts',(-62.5000273428098,-6.49855818190805,
2.66766759643951));
#235087=CARTESIAN_POINT('Ctrl Pts',(-62.4980940659029,-6.49182203260206,
2.67012012783127));
#235088=CARTESIAN_POINT('Ctrl Pts',(-62.4971274274494,-6.48845395794907,
2.67134639352714));
#235089=CARTESIAN_POINT('Ctrl Pts',(-62.4960636607365,-6.48514561818763,
2.67265375584991));
#235090=CARTESIAN_POINT('Ctrl Pts',(-62.4949101555729,-6.4819050574019,
2.67403135126919));
#235091=CARTESIAN_POINT('Ctrl Pts',(-62.4943334029911,-6.48028477700904,
2.67472014897882));
#235092=CARTESIAN_POINT('Ctrl Pts',(-62.4937342176673,-6.47868142404706,
2.67542649668611));
#235093=CARTESIAN_POINT('Ctrl Pts',(-62.4931135352113,-6.47709589524291,
2.67614899656081));
#235094=CARTESIAN_POINT('Ctrl Pts',(-62.4929583645973,-6.47669951304187,
2.67632962152948));
#235095=CARTESIAN_POINT('Ctrl Pts',(-62.4928018504534,-6.47630424448198,
2.67651125590929));
#235096=CARTESIAN_POINT('Ctrl Pts',(-62.4926440074816,-6.47591010283098,
2.67669387767502));
#235097=CARTESIAN_POINT('Ctrl Pts',(-62.492170478566,-6.47472767787799,
2.67724174297223));
#235098=CARTESIAN_POINT('Ctrl Pts',(-62.4916849899864,-6.47355539694492,
2.67779849504726));
#235099=CARTESIAN_POINT('Ctrl Pts',(-62.4911879405752,-6.47239360181834,
2.67836353617988));
#235100=CARTESIAN_POINT('Ctrl Pts',(-62.4877530207469,-6.46436487665208,
2.68226832098884));
#235101=CARTESIAN_POINT('Ctrl Pts',(-62.4837949925048,-6.45678933786437,
2.68659153751363));
#235102=CARTESIAN_POINT('Ctrl Pts',(-62.4794326364367,-6.44966853564042,
2.69123699486146));
#235103=CARTESIAN_POINT('Ctrl Pts',(-62.4772645574453,-6.44612951648122,
2.69354577441187));
#235104=CARTESIAN_POINT('Ctrl Pts',(-62.4749960038951,-6.4427027239438,
2.69593478828092));
#235105=CARTESIAN_POINT('Ctrl Pts',(-62.4726384024733,-6.43938822718948,
2.69839565261198));
#235106=CARTESIAN_POINT('Ctrl Pts',(-62.4674371815967,-6.43207595228378,
2.70382468689023));
#235107=CARTESIAN_POINT('Ctrl Pts',(-62.4618132330509,-6.42530381744014,
2.70961155815065));
#235108=CARTESIAN_POINT('Ctrl Pts',(-62.455895762341,-6.41913840445449,
2.71562701361744));
#235109=CARTESIAN_POINT('Ctrl Pts',(-62.4537340356674,-6.41688610134088,
2.71782453535834));
#235110=CARTESIAN_POINT('Ctrl Pts',(-62.4515361835425,-6.41470741397492,
2.72005051502378));
#235111=CARTESIAN_POINT('Ctrl Pts',(-62.4493074469122,-6.41260146153662,
2.72229986760091));
#235112=CARTESIAN_POINT('Ctrl Pts',(-62.4418213564087,-6.40552779014116,
2.72985520488862));
#235113=CARTESIAN_POINT('Ctrl Pts',(-62.4339335724863,-6.39923601079906,
2.73770845534524));
#235114=CARTESIAN_POINT('Ctrl Pts',(-62.4257522463026,-6.39365709371056,
2.74576706701716));
#235115=CARTESIAN_POINT('Ctrl Pts',(-62.416759999685,-6.38752520296414,
2.75462443584989));
#235116=CARTESIAN_POINT('Ctrl Pts',(-62.4074126717507,-6.38225398283486,
2.76373036323139));
#235117=CARTESIAN_POINT('Ctrl Pts',(-62.3978127557451,-6.37778536209609,
2.77299664636773));
#235118=CARTESIAN_POINT('Ctrl Pts',(-62.3874732348832,-6.37297246609526,
2.78297683033423));
#235119=CARTESIAN_POINT('Ctrl Pts',(-62.3768396913517,-6.36908997057808,
2.79314401478834));
#235120=CARTESIAN_POINT('Ctrl Pts',(-62.3660067738154,-6.36611161569978,
2.80341452427867));
#235121=CARTESIAN_POINT('Ctrl Pts',(-62.3553201372425,-6.36317347866857,
2.81354634721315));
#235122=CARTESIAN_POINT('Ctrl Pts',(-62.3444380411298,-6.36111515612471,
2.82378004209176));
#235123=CARTESIAN_POINT('Ctrl Pts',(-62.3334394572619,-6.35995915837826,
2.83404198860256));
#235124=CARTESIAN_POINT('Ctrl Pts',(-58.9120953679529,-6.00036140429068,
2.83404198860256));
#235125=CARTESIAN_POINT('Ctrl Pts',(-58.9015696628148,-5.9992551081015,
2.82422126443049));
#235126=CARTESIAN_POINT('Ctrl Pts',(-58.8909945468901,-5.9989829913121,
2.81442815028591));
#235127=CARTESIAN_POINT('Ctrl Pts',(-58.8804276387791,-5.99953795195274,
2.80471618166455));
#235128=CARTESIAN_POINT('Ctrl Pts',(-58.8702243592803,-6.00007381527886,
2.79533842146398));
#235129=CARTESIAN_POINT('Ctrl Pts',(-58.8600274754043,-6.00138095727662,
2.7860351565044));
#235130=CARTESIAN_POINT('Ctrl Pts',(-58.8498890377501,-6.00349883563941,
2.77685887346985));
#235131=CARTESIAN_POINT('Ctrl Pts',(-58.8403050390047,-6.00550089397069,
2.76818441216827));
#235132=CARTESIAN_POINT('Ctrl Pts',(-58.8307723843893,-6.0082276253853,
2.75962261521893));
#235133=CARTESIAN_POINT('Ctrl Pts',(-58.8213500689071,-6.0117515363952,
2.75123537701946));
#235134=CARTESIAN_POINT('Ctrl Pts',(-58.8126722744191,-6.01499699931729,
2.74351087134419));
#235135=CARTESIAN_POINT('Ctrl Pts',(-58.804087581858,-6.01891888229111,
2.7359339945016));
#235136=CARTESIAN_POINT('Ctrl Pts',(-58.7956642413083,-6.02360485257358,
2.72857657812899));
#235137=CARTESIAN_POINT('Ctrl Pts',(-58.793152571192,-6.02500211431966,
2.7263827450853));
#235138=CARTESIAN_POINT('Ctrl Pts',(-58.7906554330099,-6.02646752363703,
2.72420861709694));
#235139=CARTESIAN_POINT('Ctrl Pts',(-58.7881751602883,-6.02800395803725,
2.72205663736702));
#235140=CARTESIAN_POINT('Ctrl Pts',(-58.7857202298424,-6.02952469386373,
2.71992664556741));
#235141=CARTESIAN_POINT('Ctrl Pts',(-58.7832842250419,-6.03111319985525,
2.7178208992786));
#235142=CARTESIAN_POINT('Ctrl Pts',(-58.7808720541407,-6.03277025542051,
2.71574387311221));
#235143=CARTESIAN_POINT('Ctrl Pts',(-58.7807043164936,-6.03288548382383,
2.71559944077462));
#235144=CARTESIAN_POINT('Ctrl Pts',(-58.7805366835714,-6.03300103800931,
2.71545515216044));
#235145=CARTESIAN_POINT('Ctrl Pts',(-58.7803691562897,-6.03311691890583,
2.71531100781706));
#235146=CARTESIAN_POINT('Ctrl Pts',(-58.7730241465597,-6.03819756191456,
2.70899119176053));
#235147=CARTESIAN_POINT('Ctrl Pts',(-58.7659160498048,-6.0439362220602,
2.70298296066802));
#235148=CARTESIAN_POINT('Ctrl Pts',(-58.7591607781927,-6.05034076157611,
2.69736727774095));
#235149=CARTESIAN_POINT('Ctrl Pts',(-58.7528636909919,-6.05631090550645,
2.69213248525377));
#235150=CARTESIAN_POINT('Ctrl Pts',(-58.746872812682,-6.06286038933366,
2.68723866185407));
#235151=CARTESIAN_POINT('Ctrl Pts',(-58.7413107827875,-6.0700015050445,
2.68278595829494));
#235152=CARTESIAN_POINT('Ctrl Pts',(-58.739276120295,-6.07261381755752,
2.68115710172752));
#235153=CARTESIAN_POINT('Ctrl Pts',(-58.7372991657062,-6.07530531160704,
2.67958763637771));
#235154=CARTESIAN_POINT('Ctrl Pts',(-58.735387140493,-6.07807653793576,
2.67808378645339));
#235155=CARTESIAN_POINT('Ctrl Pts',(-58.7349273623043,-6.0787429252894,
2.67772216078575));
#235156=CARTESIAN_POINT('Ctrl Pts',(-58.7344713442222,-6.07941450700205,
2.67736403603538));
#235157=CARTESIAN_POINT('Ctrl Pts',(-58.7340192051468,-6.08009121771096,
2.67700956934454));
#235158=CARTESIAN_POINT('Ctrl Pts',(-58.7335811954174,-6.08074678121022,
2.67666617973778));
#235159=CARTESIAN_POINT('Ctrl Pts',(-58.7331468260467,-6.08140715812728,
2.67632622314093));
#235160=CARTESIAN_POINT('Ctrl Pts',(-58.7327162055066,-6.08207228526562,
2.67598984158748));
#235161=CARTESIAN_POINT('Ctrl Pts',(-58.7279982598321,-6.08935952173613,
2.67230439292203));
#235162=CARTESIAN_POINT('Ctrl Pts',(-58.7237275533352,-6.09722197243188,
2.66904964539963));
#235163=CARTESIAN_POINT('Ctrl Pts',(-58.7200553115703,-6.10554709909163,
2.66640203566715));
#235164=CARTESIAN_POINT('Ctrl Pts',(-58.7185323234525,-6.10899977726308,
2.66530399299424));
#235165=CARTESIAN_POINT('Ctrl Pts',(-58.7171120447815,-6.112531674346,2.66430995142237));
#235166=CARTESIAN_POINT('Ctrl Pts',(-58.7158039367398,-6.11613350280247,
2.66343053473334));
#235167=CARTESIAN_POINT('Ctrl Pts',(-58.7135728221601,-6.1222767965717,
2.66193059792858));
#235168=CARTESIAN_POINT('Ctrl Pts',(-58.7116702942287,-6.12862250657808,
2.660765198171));
#235169=CARTESIAN_POINT('Ctrl Pts',(-58.7101471179288,-6.1351184806112,
2.65997805604432));
#235170=CARTESIAN_POINT('Ctrl Pts',(-58.7093855297788,-6.13836646762777,
2.65958448498099));
#235171=CARTESIAN_POINT('Ctrl Pts',(-58.7087202098051,-6.14165223896384,
2.65928526260735));
#235172=CARTESIAN_POINT('Ctrl Pts',(-58.7081575578111,-6.14496923836515,
2.65908463971297));
#235173=CARTESIAN_POINT('Ctrl Pts',(-58.7075949058172,-6.14828623776645,
2.65888401681859));
#235174=CARTESIAN_POINT('Ctrl Pts',(-58.7071349090266,-6.15163442139613,
2.65878198860256));
#235175=CARTESIAN_POINT('Ctrl Pts',(-58.7067819056642,-6.15500747092338,
2.65878198860256));
#235176=CARTESIAN_POINT('Origin',(-56.9874003490101,-12.1286263473646,2.83404198860252));
#235177=CARTESIAN_POINT('Ctrl Pts',(-61.2479592423877,-13.2134115091896,
2.83404198860251));
#235178=CARTESIAN_POINT('Ctrl Pts',(-61.2583377107547,-13.2156175207411,
2.82419652440056));
#235179=CARTESIAN_POINT('Ctrl Pts',(-61.26885944602,-13.2169980909551,2.81438790575639));
#235180=CARTESIAN_POINT('Ctrl Pts',(-61.2794654334806,-13.2175561899857,
2.80466781256888));
#235181=CARTESIAN_POINT('Ctrl Pts',(-61.2897267895032,-13.218096154121,
2.79526356453059));
#235182=CARTESIAN_POINT('Ctrl Pts',(-61.3000683010475,-13.2178662282941,
2.78594102496206));
#235183=CARTESIAN_POINT('Ctrl Pts',(-61.3104421535944,-13.216823252902,
2.77675109088744));
#235184=CARTESIAN_POINT('Ctrl Pts',(-61.3202551793187,-13.2158366624037,
2.76805797913636));
#235185=CARTESIAN_POINT('Ctrl Pts',(-61.3300980668416,-13.2141224659042,
2.75948271210104));
#235186=CARTESIAN_POINT('Ctrl Pts',(-61.3399200511735,-13.2116033021979,
2.75108575573156));
#235187=CARTESIAN_POINT('Ctrl Pts',(-61.3489668090872,-13.2092829702338,
2.74335155163188));
#235188=CARTESIAN_POINT('Ctrl Pts',(-61.357996360567,-13.2062795322627,
2.73576818685848));
#235189=CARTESIAN_POINT('Ctrl Pts',(-61.3669504518481,-13.2024991065223,
2.72840626160392));
#235190=CARTESIAN_POINT('Ctrl Pts',(-61.3695476933574,-13.2014025487201,
2.72627084693605));
#235191=CARTESIAN_POINT('Ctrl Pts',(-61.3721384315557,-13.2002403977583,
2.72415424587479));
#235192=CARTESIAN_POINT('Ctrl Pts',(-61.3747208224638,-13.1990098046949,
2.72205867173245));
#235193=CARTESIAN_POINT('Ctrl Pts',(-61.3775203002415,-13.197675762694,
2.71978693462848));
#235194=CARTESIAN_POINT('Ctrl Pts',(-61.3803065372248,-13.196264116926,
2.71754411340749));
#235195=CARTESIAN_POINT('Ctrl Pts',(-61.3830766416485,-13.1947721021912,
2.71533341844247));
#235196=CARTESIAN_POINT('Ctrl Pts',(-61.3906792149761,-13.1906772560438,
2.70926614876395));
#235197=CARTESIAN_POINT('Ctrl Pts',(-61.3981301363757,-13.1859443571666,
2.70347381860412));
#235198=CARTESIAN_POINT('Ctrl Pts',(-61.4053257594952,-13.1805769309632,
2.69804914171398));
#235199=CARTESIAN_POINT('Ctrl Pts',(-61.4119093639901,-13.1756660273913,
2.69308585687203));
#235200=CARTESIAN_POINT('Ctrl Pts',(-61.4182680026353,-13.1702212276778,
2.68842799053179));
#235201=CARTESIAN_POINT('Ctrl Pts',(-61.4243186078275,-13.1642115906183,
2.68414767054208));
#235202=CARTESIAN_POINT('Ctrl Pts',(-61.4272906453326,-13.1612596765261,
2.68204519134548));
#235203=CARTESIAN_POINT('Ctrl Pts',(-61.4301878975266,-13.1581712727459,
2.68003431778503));
#235204=CARTESIAN_POINT('Ctrl Pts',(-61.4329973166795,-13.1549417366132,
2.67812693945258));
#235205=CARTESIAN_POINT('Ctrl Pts',(-61.4335303765996,-13.1543289635881,
2.6777650329921));
#235206=CARTESIAN_POINT('Ctrl Pts',(-61.4340602468994,-13.1537105783546,
2.6774065963993));
#235207=CARTESIAN_POINT('Ctrl Pts',(-61.434586797382,-13.153086632425,2.67705178968862));
#235208=CARTESIAN_POINT('Ctrl Pts',(-61.4350968931622,-13.1524821848057,
2.67670807068764));
#235209=CARTESIAN_POINT('Ctrl Pts',(-61.4356038733672,-13.1518725186283,
2.67636775825272));
#235210=CARTESIAN_POINT('Ctrl Pts',(-61.4361076188514,-13.1512576844885,
2.67603099699261));
#235211=CARTESIAN_POINT('Ctrl Pts',(-61.4415973333394,-13.1445573487223,
2.67236104217134));
#235212=CARTESIAN_POINT('Ctrl Pts',(-61.4467061867047,-13.1372385931151,
2.6691144054148));
#235213=CARTESIAN_POINT('Ctrl Pts',(-61.4512683418497,-13.1293950794801,
2.66646778189636));
#235214=CARTESIAN_POINT('Ctrl Pts',(-61.453194968297,-13.1260827149662,
2.66535009634979));
#235215=CARTESIAN_POINT('Ctrl Pts',(-61.4550242827916,-13.122677158292,
2.6643389791235));
#235216=CARTESIAN_POINT('Ctrl Pts',(-61.4567450522888,-13.119186939003,
2.66344564884798));
#235217=CARTESIAN_POINT('Ctrl Pts',(-61.4596427851247,-13.1133094969314,
2.66194130298591));
#235218=CARTESIAN_POINT('Ctrl Pts',(-61.4622303029112,-13.1071927578069,
2.66077206705424));
#235219=CARTESIAN_POINT('Ctrl Pts',(-61.4644496675151,-13.1008831031059,
2.65998225155718));
#235220=CARTESIAN_POINT('Ctrl Pts',(-61.4650045086661,-13.0993056894307,
2.65978479768292));
#235221=CARTESIAN_POINT('Ctrl Pts',(-61.4655361149185,-13.0977161555173,
2.65961098966626));
#235222=CARTESIAN_POINT('Ctrl Pts',(-61.4660432808487,-13.0961151548352,
2.65946139030505));
#235223=CARTESIAN_POINT('Ctrl Pts',(-61.4668040297441,-13.0937136538121,
2.65923699126324));
#235224=CARTESIAN_POINT('Ctrl Pts',(-61.4675097715122,-13.0912863650435,
2.65906707562445));
#235225=CARTESIAN_POINT('Ctrl Pts',(-61.4681580753692,-13.0888358608681,
2.65895332562923));
#235226=CARTESIAN_POINT('Ctrl Pts',(-61.4688063792261,-13.0863853566926,
2.658839575634));
#235227=CARTESIAN_POINT('Ctrl Pts',(-61.4693972526618,-13.0839116459753,
2.65878198860252));
#235228=CARTESIAN_POINT('Ctrl Pts',(-61.4699285681953,-13.0814171332235,
2.65878198860252));
#235229=CARTESIAN_POINT('Ctrl Pts',(-57.7354693911204,-12.2876333308473,
2.65878198860252));
#235230=CARTESIAN_POINT('Ctrl Pts',(-57.7336713548546,-12.2960739442503,
2.65878198860252));
#235231=CARTESIAN_POINT('Ctrl Pts',(-57.7325856410806,-12.3045898170421,
2.65945335517841));
#235232=CARTESIAN_POINT('Ctrl Pts',(-57.7321565492375,-12.31304047865,2.66072561226578));
#235233=CARTESIAN_POINT('Ctrl Pts',(-57.7318793999343,-12.3184987389612,
2.66154735980318));
#235234=CARTESIAN_POINT('Ctrl Pts',(-57.7318752477671,-12.3239297572686,
2.66261895766868));
#235235=CARTESIAN_POINT('Ctrl Pts',(-57.7321203363021,-12.3292970476686,
2.66391429251019));
#235236=CARTESIAN_POINT('Ctrl Pts',(-57.7324451871156,-12.3364110836361,
2.66563118464116));
#235237=CARTESIAN_POINT('Ctrl Pts',(-57.7332135204776,-12.3434117286777,
2.66774105138691));
#235238=CARTESIAN_POINT('Ctrl Pts',(-57.7343801629265,-12.3502210637612,
2.67016894181741));
#235239=CARTESIAN_POINT('Ctrl Pts',(-57.734963484151,-12.3536257313029,
2.67138288703267));
#235240=CARTESIAN_POINT('Ctrl Pts',(-57.735646339504,-12.3569827659241,
2.67267613167543));
#235241=CARTESIAN_POINT('Ctrl Pts',(-57.7364227809414,-12.3602838093643,
2.67403835432544));
#235242=CARTESIAN_POINT('Ctrl Pts',(-57.7368110016601,-12.3619343310844,
2.67471946565045));
#235243=CARTESIAN_POINT('Ctrl Pts',(-57.7372226154359,-12.3635708710711,
2.67541781389514));
#235244=CARTESIAN_POINT('Ctrl Pts',(-57.7376568568911,-12.3651924853575,
2.6761320724416));
#235245=CARTESIAN_POINT('Ctrl Pts',(-57.7377654172549,-12.3655978889291,
2.67631063707821));
#235246=CARTESIAN_POINT('Ctrl Pts',(-57.737875391774,-12.3660023599859,
2.67649019601836));
#235247=CARTESIAN_POINT('Ctrl Pts',(-57.7379867683383,-12.3664058844668,
2.67667072836647));
#235248=CARTESIAN_POINT('Ctrl Pts',(-57.7383208980313,-12.3676164579094,
2.67721232541081));
#235249=CARTESIAN_POINT('Ctrl Pts',(-57.7386676465114,-12.3688185104667,
2.67776268340038));
#235250=CARTESIAN_POINT('Ctrl Pts',(-57.7390266834246,-12.3700116777064,
2.67832123541507));
#235251=CARTESIAN_POINT('Ctrl Pts',(-57.7415556930806,-12.3784161936769,
2.68225560368429));
#235252=CARTESIAN_POINT('Ctrl Pts',(-57.7446608854351,-12.3864219416028,
2.68661792998865));
#235253=CARTESIAN_POINT('Ctrl Pts',(-57.7482237843183,-12.3940121800348,
2.69130986622546));
#235254=CARTESIAN_POINT('Ctrl Pts',(-57.7499517864267,-12.3976934374724,
2.6935854502303));
#235255=CARTESIAN_POINT('Ctrl Pts',(-57.751788007257,-12.4012771190725,
2.69593918853452));
#235256=CARTESIAN_POINT('Ctrl Pts',(-57.7537217536092,-12.4047617836667,
2.69836306235466));
#235257=CARTESIAN_POINT('Ctrl Pts',(-57.7566821841673,-12.4100965616936,
2.70207384382199));
#235258=CARTESIAN_POINT('Ctrl Pts',(-57.7598686150879,-12.4151968540757,
2.70594760814199));
#235259=CARTESIAN_POINT('Ctrl Pts',(-57.7632382593549,-12.420045468934,
2.70995196345679));
#235260=CARTESIAN_POINT('Ctrl Pts',(-57.7648031395848,-12.4222971907576,
2.71181160678077));
#235261=CARTESIAN_POINT('Ctrl Pts',(-57.7664072884047,-12.424494702241,
2.7136996277207));
#235262=CARTESIAN_POINT('Ctrl Pts',(-57.7680472557361,-12.4266353752446,
2.71561183138632));
#235263=CARTESIAN_POINT('Ctrl Pts',(-57.7681729527703,-12.4267994493956,
2.71575839426283));
#235264=CARTESIAN_POINT('Ctrl Pts',(-57.7682988432679,-12.4269632190239,
2.7159050890318));
#235265=CARTESIAN_POINT('Ctrl Pts',(-57.7684249257696,-12.4271266840708,
2.71605191409882));
#235266=CARTESIAN_POINT('Ctrl Pts',(-57.7701960047921,-12.4294228751481,
2.71811436362724));
#235267=CARTESIAN_POINT('Ctrl Pts',(-57.772006704017,-12.4316578001007,
2.7202009102693));
#235268=CARTESIAN_POINT('Ctrl Pts',(-57.7738513586812,-12.4338307751865,
2.72230624862153));
#235269=CARTESIAN_POINT('Ctrl Pts',(-57.7804659622465,-12.4416226773934,
2.72985561753072));
#235270=CARTESIAN_POINT('Ctrl Pts',(-57.7875668075256,-12.4486795287417,
2.73770089914296));
#235271=CARTESIAN_POINT('Ctrl Pts',(-57.7950386758939,-12.4550596184369,
2.74574823347037));
#235272=CARTESIAN_POINT('Ctrl Pts',(-57.8032495086148,-12.4620706960752,
2.75459144546979));
#235273=CARTESIAN_POINT('Ctrl Pts',(-57.8119087706216,-12.4682650727919,
2.76367911754215));
#235274=CARTESIAN_POINT('Ctrl Pts',(-57.8209080689687,-12.47369138165,2.77292162564663));
#235275=CARTESIAN_POINT('Ctrl Pts',(-57.8306250526682,-12.4795504333992,
2.78290121484661));
#235276=CARTESIAN_POINT('Ctrl Pts',(-57.84073937177,-12.4845147615735,2.79306229500112));
#235277=CARTESIAN_POINT('Ctrl Pts',(-57.8511535286833,-12.4886033793286,
2.80331916685171));
#235278=CARTESIAN_POINT('Ctrl Pts',(-57.8614803215206,-12.4926576977817,
2.81348999408635));
#235279=CARTESIAN_POINT('Ctrl Pts',(-57.8721033557551,-12.4958511892335,
2.82375635966841));
#235280=CARTESIAN_POINT('Ctrl Pts',(-57.8829458346104,-12.498155829259,
2.83404198860252));
#235281=CARTESIAN_POINT('Origin',(-0.00316857416805164,0.0149069694353738,
2.83404198860262));
#235282=CARTESIAN_POINT('Ctrl Pts',(-61.4762657165315,-13.0516031943531,
2.65878198860251));
#235283=CARTESIAN_POINT('Ctrl Pts',(-61.4780479426481,-13.0432012029363,
2.65878198860251));
#235284=CARTESIAN_POINT('Ctrl Pts',(-61.4791124697294,-13.0347249977694,
2.65944603041843));
#235285=CARTESIAN_POINT('Ctrl Pts',(-61.4795178910587,-13.0263136082735,
2.6607043926407));
#235286=CARTESIAN_POINT('Ctrl Pts',(-61.479776935988,-13.0209391308129,
2.66150842619592));
#235287=CARTESIAN_POINT('Ctrl Pts',(-61.4797678285536,-13.0155911381653,
2.66255428265361));
#235288=CARTESIAN_POINT('Ctrl Pts',(-61.4795143397208,-13.0103045333056,
2.66381699700642));
#235289=CARTESIAN_POINT('Ctrl Pts',(-61.4791683783269,-13.0030893784374,
2.66554034873241));
#235290=CARTESIAN_POINT('Ctrl Pts',(-61.4783613533298,-12.9959902125624,
2.66766759643946));
#235291=CARTESIAN_POINT('Ctrl Pts',(-61.4771427864514,-12.989088882123,
2.67012012783122));
#235292=CARTESIAN_POINT('Ctrl Pts',(-61.4765335030122,-12.9856382169033,
2.6713463935271));
#235293=CARTESIAN_POINT('Ctrl Pts',(-61.4758213793958,-12.9822368066735,
2.67265375584987));
#235294=CARTESIAN_POINT('Ctrl Pts',(-61.4750129240933,-12.9788934238967,
2.67403135126914));
#235295=CARTESIAN_POINT('Ctrl Pts',(-61.474608696442,-12.9772217325083,
2.67472014897878));
#235296=CARTESIAN_POINT('Ctrl Pts',(-61.4741803895392,-12.9755645309605,
2.67542649668607));
#235297=CARTESIAN_POINT('Ctrl Pts',(-61.4737288401361,-12.9739228088657,
2.67614899656076));
#235298=CARTESIAN_POINT('Ctrl Pts',(-61.4736159527853,-12.973512378342,
2.67632962152944));
#235299=CARTESIAN_POINT('Ctrl Pts',(-61.4735016128574,-12.9731029149217,
2.67651125590925));
#235300=CARTESIAN_POINT('Ctrl Pts',(-61.473385833587,-12.9726944333366,
2.67669387767498));
#235301=CARTESIAN_POINT('Ctrl Pts',(-61.4730384957756,-12.9714689885814,
2.67724174297219));
#235302=CARTESIAN_POINT('Ctrl Pts',(-61.4726782034776,-12.9702523821508,
2.67779849504722));
#235303=CARTESIAN_POINT('Ctrl Pts',(-61.4723053176143,-12.9690449956483,
2.67836353617984));
#235304=CARTESIAN_POINT('Ctrl Pts',(-61.4697284449399,-12.9607012057873,
2.6822683209889));
#235305=CARTESIAN_POINT('Ctrl Pts',(-61.4665839586184,-12.9527534399837,
2.68659153751382));
#235306=CARTESIAN_POINT('Ctrl Pts',(-61.4629898265069,-12.9452156558832,
2.69123699486179));
#235307=CARTESIAN_POINT('Ctrl Pts',(-61.4612035527133,-12.9414693978763,
2.69354577441209));
#235308=CARTESIAN_POINT('Ctrl Pts',(-61.4593056238948,-12.9378242492507,
2.69593478828101));
#235309=CARTESIAN_POINT('Ctrl Pts',(-61.4573073969126,-12.934281473203,
2.69839565261194));
#235310=CARTESIAN_POINT('Ctrl Pts',(-61.452899009727,-12.9264655800789,
2.70382468689019));
#235311=CARTESIAN_POINT('Ctrl Pts',(-61.4480137506081,-12.9191426809996,
2.7096115581506));
#235312=CARTESIAN_POINT('Ctrl Pts',(-61.4427731575667,-12.9123924986716,
2.71562701361741));
#235313=CARTESIAN_POINT('Ctrl Pts',(-61.4408587028413,-12.9099265719429,
2.71782453535831));
#235314=CARTESIAN_POINT('Ctrl Pts',(-61.4389006256226,-12.9075300815492,
2.72005051502376));
#235315=CARTESIAN_POINT('Ctrl Pts',(-61.4369042302169,-12.9052026993237,
2.7222998676009));
#235316=CARTESIAN_POINT('Ctrl Pts',(-61.4301985493014,-12.8973852687044,
2.72985520488827));
#235317=CARTESIAN_POINT('Ctrl Pts',(-61.4230116455109,-12.8903034584562,
2.73770845534453));
#235318=CARTESIAN_POINT('Ctrl Pts',(-61.4154582931184,-12.883899921806,
2.74576706701605));
#235319=CARTESIAN_POINT('Ctrl Pts',(-61.4071562640857,-12.8768616764787,
2.7546244358484));
#235320=CARTESIAN_POINT('Ctrl Pts',(-61.3984111343319,-12.8706422708203,
2.76373036322949));
#235321=CARTESIAN_POINT('Ctrl Pts',(-61.3893309057297,-12.865194665186,
2.77299664636542));
#235322=CARTESIAN_POINT('Ctrl Pts',(-61.3795511104683,-12.8593273605066,
2.7829768303315));
#235323=CARTESIAN_POINT('Ctrl Pts',(-61.3693816498913,-12.8543546257416,
2.79314401478517));
#235324=CARTESIAN_POINT('Ctrl Pts',(-61.3589193990697,-12.8502602383802,
2.80341452427506));
#235325=CARTESIAN_POINT('Ctrl Pts',(-61.3485984239577,-12.8462211390719,
2.8135463472107));
#235326=CARTESIAN_POINT('Ctrl Pts',(-61.3379910943973,-12.84303660345,2.82378004209051));
#235327=CARTESIAN_POINT('Ctrl Pts',(-61.3271735965892,-12.8407372733101,
2.83404198860251));
#235328=CARTESIAN_POINT('Ctrl Pts',(-57.962160188812,-12.1254815933794,
2.83404198860251));
#235329=CARTESIAN_POINT('Ctrl Pts',(-57.9518077840286,-12.1232811218136,
2.82422126443056));
#235330=CARTESIAN_POINT('Ctrl Pts',(-57.9413190436454,-12.121905095092,
2.8144281502861));
#235331=CARTESIAN_POINT('Ctrl Pts',(-57.9307520129798,-12.1213524729338,
2.80471618166485));
#235332=CARTESIAN_POINT('Ctrl Pts',(-57.9205486151437,-12.1208188676182,
2.79533842146432));
#235333=CARTESIAN_POINT('Ctrl Pts',(-57.9102709573203,-12.1210529843537,
2.78603515650477));
#235334=CARTESIAN_POINT('Ctrl Pts',(-57.8999666805177,-12.1220995054492,
2.77685887347025));
#235335=CARTESIAN_POINT('Ctrl Pts',(-57.8902259118395,-12.1230887956347,
2.76818441216864));
#235336=CARTESIAN_POINT('Ctrl Pts',(-57.880460457059,-12.1248041559915,
2.75962261521927));
#235337=CARTESIAN_POINT('Ctrl Pts',(-57.8707214090042,-12.1273238624903,
2.75123537701976));
#235338=CARTESIAN_POINT('Ctrl Pts',(-57.8617519091305,-12.1296444699046,
2.7435108713444));
#235339=CARTESIAN_POINT('Ctrl Pts',(-57.852804296013,-12.1326475236721,
2.73593399450171));
#235340=CARTESIAN_POINT('Ctrl Pts',(-57.8439372821316,-12.1364273448759,
2.72857657812902));
#235341=CARTESIAN_POINT('Ctrl Pts',(-57.8412933175838,-12.1375544112584,
2.7263827450853));
#235342=CARTESIAN_POINT('Ctrl Pts',(-57.838656682002,-12.1387507708935,
2.72420861709692));
#235343=CARTESIAN_POINT('Ctrl Pts',(-57.836029395347,-12.1400195294493,
2.72205663736698));
#235344=CARTESIAN_POINT('Ctrl Pts',(-57.833428953088,-12.1412753244188,
2.71992664556737));
#235345=CARTESIAN_POINT('Ctrl Pts',(-57.8308402488865,-12.14260049657,2.71782089927855));
#235346=CARTESIAN_POINT('Ctrl Pts',(-57.828268082638,-12.143996334094,2.71574387311217));
#235347=CARTESIAN_POINT('Ctrl Pts',(-57.8280892192275,-12.1440933979056,
2.71559944077458));
#235348=CARTESIAN_POINT('Ctrl Pts',(-57.8279104259145,-12.1441907966614,
2.7154551521604));
#235349=CARTESIAN_POINT('Ctrl Pts',(-57.8277317035127,-12.144288531381,
2.71531100781701));
#235350=CARTESIAN_POINT('Ctrl Pts',(-57.8198958587084,-12.1485735795159,
2.70899119176053));
#235351=CARTESIAN_POINT('Ctrl Pts',(-57.8122268475251,-12.1535378042502,
2.70298296066807));
#235352=CARTESIAN_POINT('Ctrl Pts',(-57.8048391253242,-12.1592011408679,
2.69736727774104));
#235353=CARTESIAN_POINT('Ctrl Pts',(-57.7979524842555,-12.164480354877,
2.69213248525387));
#235354=CARTESIAN_POINT('Ctrl Pts',(-57.7913098171242,-12.1703677426431,
2.68723866185419));
#235355=CARTESIAN_POINT('Ctrl Pts',(-57.7850318067602,-12.1768883481373,
2.68278595829508));
#235356=CARTESIAN_POINT('Ctrl Pts',(-57.7827352293491,-12.1792736699855,
2.6811571017276));
#235357=CARTESIAN_POINT('Ctrl Pts',(-57.7804877669874,-12.181743771724,
2.67958763637773));
#235358=CARTESIAN_POINT('Ctrl Pts',(-57.7782965440187,-12.1842999559277,
2.67808378645336));
#235359=CARTESIAN_POINT('Ctrl Pts',(-57.777769628097,-12.1849146328342,
2.67772216078571));
#235360=CARTESIAN_POINT('Ctrl Pts',(-57.7772459087254,-12.1855348686826,
2.67736403603534));
#235361=CARTESIAN_POINT('Ctrl Pts',(-57.7767255109846,-12.1861606108967,
2.6770095693445));
#235362=CARTESIAN_POINT('Ctrl Pts',(-57.7762213756733,-12.1867667986667,
2.67666617973775));
#235363=CARTESIAN_POINT('Ctrl Pts',(-57.7757203576391,-12.1873781540071,
2.6763262231409));
#235364=CARTESIAN_POINT('Ctrl Pts',(-57.7752225713656,-12.187994625406,
2.67598984158744));
#235365=CARTESIAN_POINT('Ctrl Pts',(-57.7697687474615,-12.1947487820215,
2.67230439292199));
#235366=CARTESIAN_POINT('Ctrl Pts',(-57.7646995864529,-12.2021217510025,
2.66904964539959));
#235367=CARTESIAN_POINT('Ctrl Pts',(-57.7601772489164,-12.2100174179589,
2.66640203566711));
#235368=CARTESIAN_POINT('Ctrl Pts',(-57.7583017007435,-12.2132919863906,
2.6653039929942));
#235369=CARTESIAN_POINT('Ctrl Pts',(-57.7565200187332,-12.2166560758248,
2.66430995142233));
#235370=CARTESIAN_POINT('Ctrl Pts',(-57.7548425830506,-12.2201014385648,
2.6634305347333));
#235371=CARTESIAN_POINT('Ctrl Pts',(-57.751981541693,-12.2259778637496,
2.66193059792854));
#235372=CARTESIAN_POINT('Ctrl Pts',(-57.7494261286933,-12.2320899429716,
2.66076519817096));
#235373=CARTESIAN_POINT('Ctrl Pts',(-57.7472322823293,-12.2383911161013,
2.65997805604428));
#235374=CARTESIAN_POINT('Ctrl Pts',(-57.7461353591473,-12.2415417026662,
2.65958448498095));
#235375=CARTESIAN_POINT('Ctrl Pts',(-57.7451302272376,-12.2447399293286,
2.6592852626073));
#235376=CARTESIAN_POINT('Ctrl Pts',(-57.7442239366601,-12.2479799447119,
2.65908463971293));
#235377=CARTESIAN_POINT('Ctrl Pts',(-57.7433176460826,-12.2512199600951,
2.65888401681855));
#235378=CARTESIAN_POINT('Ctrl Pts',(-57.7425101887131,-12.254501719267,
2.65878198860252));
#235379=CARTESIAN_POINT('Ctrl Pts',(-57.7418065394565,-12.257819391977,
2.65878198860252));
#235380=CARTESIAN_POINT('Origin',(-55.4074307335705,-18.0189898472952,2.83404198860248));
#235381=CARTESIAN_POINT('Ctrl Pts',(-59.5312589135994,-19.5431821162869,
2.83404198860247));
#235382=CARTESIAN_POINT('Ctrl Pts',(-59.5413499366331,-19.5464608884257,
2.82419652440051));
#235383=CARTESIAN_POINT('Ctrl Pts',(-59.5516697238487,-19.5489337165497,
2.81438790575637));
#235384=CARTESIAN_POINT('Ctrl Pts',(-59.5621592733661,-19.5505973858261,
2.80466781256894));
#235385=CARTESIAN_POINT('Ctrl Pts',(-59.5723079749853,-19.5522069957575,
2.79526356453074));
#235386=CARTESIAN_POINT('Ctrl Pts',(-59.5826168684405,-19.553059311798,
2.78594102496233));
#235387=CARTESIAN_POINT('Ctrl Pts',(-59.5930429125526,-19.5531064127991,
2.77675109088785));
#235388=CARTESIAN_POINT('Ctrl Pts',(-59.6029053082839,-19.5531509674459,
2.76805797913694));
#235389=CARTESIAN_POINT('Ctrl Pts',(-59.6128734577647,-19.5524750234011,
2.75948271210179));
#235390=CARTESIAN_POINT('Ctrl Pts',(-59.6229049605496,-19.5509963368657,
2.75108575573247));
#235391=CARTESIAN_POINT('Ctrl Pts',(-59.6321447001112,-19.5496343596252,
2.74335155163298));
#235392=CARTESIAN_POINT('Ctrl Pts',(-59.6414387315187,-19.5475912199419,
2.73576818685976));
#235393=CARTESIAN_POINT('Ctrl Pts',(-59.6507389334438,-19.544767461171,
2.72840626160533));
#235394=CARTESIAN_POINT('Ctrl Pts',(-59.6534365684948,-19.5439483960908,
2.72627084693698));
#235395=CARTESIAN_POINT('Ctrl Pts',(-59.656134592213,-19.5430634173959,
2.72415424587524));
#235396=CARTESIAN_POINT('Ctrl Pts',(-59.6588314685159,-19.542109499003,
2.72205867173243));
#235397=CARTESIAN_POINT('Ctrl Pts',(-59.6617550558217,-19.5410753901339,
2.71978693462846));
#235398=CARTESIAN_POINT('Ctrl Pts',(-59.6646735866701,-19.5399627185792,
2.71754411340746));
#235399=CARTESIAN_POINT('Ctrl Pts',(-59.6675844741793,-19.5387684320157,
2.71533341844243));
#235400=CARTESIAN_POINT('Ctrl Pts',(-59.6755734277898,-19.5354907031708,
2.7092661487639));
#235401=CARTESIAN_POINT('Ctrl Pts',(-59.6834782549088,-19.5315625649727,
2.70347381860408));
#235402=CARTESIAN_POINT('Ctrl Pts',(-59.6911955084647,-19.5269766895185,
2.69804914171394));
#235403=CARTESIAN_POINT('Ctrl Pts',(-59.6982563764891,-19.5227808624508,
2.6930858568719));
#235404=CARTESIAN_POINT('Ctrl Pts',(-59.7051493183934,-19.5180305486459,
2.68842799053159));
#235405=CARTESIAN_POINT('Ctrl Pts',(-59.711794955864,-19.5126862934694,
2.68414767054182));
#235406=CARTESIAN_POINT('Ctrl Pts',(-59.7150592712804,-19.5100612127847,
2.68204519134529));
#235407=CARTESIAN_POINT('Ctrl Pts',(-59.7182634781247,-19.5072925729232,
2.68003431778491));
#235408=CARTESIAN_POINT('Ctrl Pts',(-59.7213950854344,-19.5043743927941,
2.67812693945252));
#235409=CARTESIAN_POINT('Ctrl Pts',(-59.7219892774192,-19.5038206965381,
2.67776503299204));
#235410=CARTESIAN_POINT('Ctrl Pts',(-59.7225808838921,-19.5032610854118,
2.67740659639924));
#235411=CARTESIAN_POINT('Ctrl Pts',(-59.7231697699854,-19.5026955970361,
2.67705178968855));
#235412=CARTESIAN_POINT('Ctrl Pts',(-59.7237402533882,-19.5021477801721,
2.67670807068758));
#235413=CARTESIAN_POINT('Ctrl Pts',(-59.7243081837712,-19.5015944476715,
2.67636775825266));
#235414=CARTESIAN_POINT('Ctrl Pts',(-59.7248734373528,-19.5010356373988,
2.67603099699255));
#235415=CARTESIAN_POINT('Ctrl Pts',(-59.7310334544115,-19.4949458381922,
2.67236104217125));
#235416=CARTESIAN_POINT('Ctrl Pts',(-59.7368793392202,-19.4882011960853,
2.66911440541469));
#235417=CARTESIAN_POINT('Ctrl Pts',(-59.7422363728288,-19.4808775251051,
2.66646778189624));
#235418=CARTESIAN_POINT('Ctrl Pts',(-59.7444986813872,-19.4777846933724,
2.6653500963497));
#235419=CARTESIAN_POINT('Ctrl Pts',(-59.7466739523113,-19.474589008127,
2.66433897912342));
#235420=CARTESIAN_POINT('Ctrl Pts',(-59.7487501225119,-19.4712977780157,
2.66344564884792));
#235421=CARTESIAN_POINT('Ctrl Pts',(-59.7522463412519,-19.465755428747,
2.66194130298585));
#235422=CARTESIAN_POINT('Ctrl Pts',(-59.755459057686,-19.4599426670173,
2.66077206705419));
#235423=CARTESIAN_POINT('Ctrl Pts',(-59.758325802888,-19.4538995640364,
2.65998225155713));
#235424=CARTESIAN_POINT('Ctrl Pts',(-59.7590424891884,-19.4523887882912,
2.65978479768286));
#235425=CARTESIAN_POINT('Ctrl Pts',(-59.7597373347835,-19.4508635299955,
2.65961098966621));
#235426=CARTESIAN_POINT('Ctrl Pts',(-59.7604090725467,-19.449324313038,
2.659461390305));
#235427=CARTESIAN_POINT('Ctrl Pts',(-59.7614166791914,-19.4470154876018,
2.65923699126319));
#235428=CARTESIAN_POINT('Ctrl Pts',(-59.7623722755973,-19.4446752658775,
2.6590670756244));
#235429=CARTESIAN_POINT('Ctrl Pts',(-59.7632731754136,-19.4423059520263,
2.65895332562918));
#235430=CARTESIAN_POINT('Ctrl Pts',(-59.7641740752299,-19.439936638175,
2.65883957563396));
#235431=CARTESIAN_POINT('Ctrl Pts',(-59.7650202849806,-19.4375382417966,
2.65878198860247));
#235432=CARTESIAN_POINT('Ctrl Pts',(-59.7658094374966,-19.4351129318429,
2.65878198860247));
#235433=CARTESIAN_POINT('Ctrl Pts',(-56.134781019564,-18.2553202812751,
2.65878198860248));
#235434=CARTESIAN_POINT('Ctrl Pts',(-56.1321105487809,-18.2635267101474,
2.65878198860248));
#235435=CARTESIAN_POINT('Ctrl Pts',(-56.1301406315641,-18.271882444105,
2.65945335517843));
#235436=CARTESIAN_POINT('Ctrl Pts',(-56.1288305556596,-18.2802419597938,
2.66072561226593));
#235437=CARTESIAN_POINT('Ctrl Pts',(-56.1279843810469,-18.2856413491928,
2.6615473598033));
#235438=CARTESIAN_POINT('Ctrl Pts',(-56.1274125556282,-18.2910421817935,
2.66261895766873));
#235439=CARTESIAN_POINT('Ctrl Pts',(-56.1270952669251,-18.2964056883427,
2.66391429251015));
#235440=CARTESIAN_POINT('Ctrl Pts',(-56.1266747189246,-18.3035147090331,
2.66563118464111));
#235441=CARTESIAN_POINT('Ctrl Pts',(-56.1267070766079,-18.3105573165144,
2.66774105138687));
#235442=CARTESIAN_POINT('Ctrl Pts',(-56.1271555587354,-18.3174512966901,
2.67016894181738));
#235443=CARTESIAN_POINT('Ctrl Pts',(-56.1273797997991,-18.320898286778,
2.67138288703263));
#235444=CARTESIAN_POINT('Ctrl Pts',(-56.1277080087289,-18.324308309033,
2.67267613167539));
#235445=CARTESIAN_POINT('Ctrl Pts',(-56.1281351437408,-18.3276724292421,
2.6740383543254));
#235446=CARTESIAN_POINT('Ctrl Pts',(-56.1283487112468,-18.3293544893466,
2.67471946565041));
#235447=CARTESIAN_POINT('Ctrl Pts',(-56.1285870051494,-18.3310250895515,
2.6754178138951));
#235448=CARTESIAN_POINT('Ctrl Pts',(-56.1288493629351,-18.3326832110572,
2.67613207244156));
#235449=CARTESIAN_POINT('Ctrl Pts',(-56.1289149523815,-18.3330977414336,
2.67631063707818));
#235450=CARTESIAN_POINT('Ctrl Pts',(-56.1289820457107,-18.3335114922231,
2.67649019601833));
#235451=CARTESIAN_POINT('Ctrl Pts',(-56.1290506323487,-18.3339244481758,
2.67667072836644));
#235452=CARTESIAN_POINT('Ctrl Pts',(-56.1292563922626,-18.3351633160338,
2.67721232541078));
#235453=CARTESIAN_POINT('Ctrl Pts',(-56.1294755925117,-18.3363950287072,
2.67776268340034));
#235454=CARTESIAN_POINT('Ctrl Pts',(-56.1297079426451,-18.3376191892287,
2.67832123541503));
#235455=CARTESIAN_POINT('Ctrl Pts',(-56.1313445869827,-18.3462420178744,
2.68225560368434));
#235456=CARTESIAN_POINT('Ctrl Pts',(-56.1335959402407,-18.3545284904606,
2.6866179299888));
#235457=CARTESIAN_POINT('Ctrl Pts',(-56.136345925232,-18.3624495731175,
2.69130986622573));
#235458=CARTESIAN_POINT('Ctrl Pts',(-56.1376796649811,-18.3662912896465,
2.69358545023047));
#235459=CARTESIAN_POINT('Ctrl Pts',(-56.139131230071,-18.3700472768053,
2.69593918853459));
#235460=CARTESIAN_POINT('Ctrl Pts',(-56.1406901365233,-18.3737149835765,
2.69836306235462));
#235461=CARTESIAN_POINT('Ctrl Pts',(-56.143076713384,-18.3793299863881,
2.70207384382195));
#235462=CARTESIAN_POINT('Ctrl Pts',(-56.1457125629777,-18.3847354115623,
2.70594760814195));
#235463=CARTESIAN_POINT('Ctrl Pts',(-56.1485569297208,-18.3899096889381,
2.70995196345674));
#235464=CARTESIAN_POINT('Ctrl Pts',(-56.1498778683511,-18.3923126501195,
2.71181160678072));
#235465=CARTESIAN_POINT('Ctrl Pts',(-56.1512435269775,-18.3946658026161,
2.71369962772066));
#235466=CARTESIAN_POINT('Ctrl Pts',(-56.1526507491369,-18.396966172054,
2.71561183138628));
#235467=CARTESIAN_POINT('Ctrl Pts',(-56.1527586071707,-18.3971424863075,
2.71575839426279));
#235468=CARTESIAN_POINT('Ctrl Pts',(-56.1528666894394,-18.3973185179288,
2.71590508903176));
#235469=CARTESIAN_POINT('Ctrl Pts',(-56.1529749944978,-18.3974942667072,
2.71605191409879));
#235470=CARTESIAN_POINT('Ctrl Pts',(-56.1544963540395,-18.3999630071782,
2.7181143636272));
#235471=CARTESIAN_POINT('Ctrl Pts',(-56.1560635207937,-18.4023749585854,
2.72020091026926));
#235472=CARTESIAN_POINT('Ctrl Pts',(-56.1576709325003,-18.4047288488037,
2.72230624862149));
#235473=CARTESIAN_POINT('Ctrl Pts',(-56.1634348250117,-18.4131694805011,
2.72985561753089));
#235474=CARTESIAN_POINT('Ctrl Pts',(-56.1697591292906,-18.4209299141244,
2.73770089914337));
#235475=CARTESIAN_POINT('Ctrl Pts',(-56.176523165011,-18.4280560759392,
2.74574823347102));
#235476=CARTESIAN_POINT('Ctrl Pts',(-56.18395616076,-18.4358870118871,2.75459144547062));
#235477=CARTESIAN_POINT('Ctrl Pts',(-56.1919204977445,-18.4429525945107,
2.76367911754316));
#235478=CARTESIAN_POINT('Ctrl Pts',(-56.2003032932677,-18.4492898603079,
2.77292162564782));
#235479=CARTESIAN_POINT('Ctrl Pts',(-56.2093546086383,-18.4561325169322,
2.78290121484784));
#235480=CARTESIAN_POINT('Ctrl Pts',(-56.2188946068467,-18.46212688423,2.79306229500239));
#235481=CARTESIAN_POINT('Ctrl Pts',(-56.228824336988,-18.4672816799275,
2.80331916685301));
#235482=CARTESIAN_POINT('Ctrl Pts',(-56.2386707668957,-18.4723932321854,
2.81348999408721));
#235483=CARTESIAN_POINT('Ctrl Pts',(-56.2489017962828,-18.4766796388004,
2.82375635966882));
#235484=CARTESIAN_POINT('Ctrl Pts',(-56.2594439784237,-18.4801050014193,
2.83404198860248));
#235485=CARTESIAN_POINT('Origin',(-0.00470941899426334,0.0144941013085293,
2.83404198860262));
#235486=CARTESIAN_POINT('Ctrl Pts',(-59.7752282754835,-19.4061247292256,
2.65878198860247));
#235487=CARTESIAN_POINT('Ctrl Pts',(-59.7778789856301,-19.3979550581547,
2.65878198860247));
#235488=CARTESIAN_POINT('Ctrl Pts',(-59.7798236858209,-19.3896365599071,
2.65944603041829));
#235489=CARTESIAN_POINT('Ctrl Pts',(-59.7811061158277,-19.3813136269522,
2.66070439264036));
#235490=CARTESIAN_POINT('Ctrl Pts',(-59.7819255275517,-19.3759956690092,
2.66150842619563));
#235491=CARTESIAN_POINT('Ctrl Pts',(-59.7824754874619,-19.370676021238,
2.66255428265342));
#235492=CARTESIAN_POINT('Ctrl Pts',(-59.7827759879494,-19.3653918801541,
2.66381699700638));
#235493=CARTESIAN_POINT('Ctrl Pts',(-59.7831861108188,-19.3581800878464,
2.66554034873238));
#235494=CARTESIAN_POINT('Ctrl Pts',(-59.7831255716885,-19.3510354548621,
2.66766759643942));
#235495=CARTESIAN_POINT('Ctrl Pts',(-59.7826350657123,-19.3440445557098,
2.67012012783117));
#235496=CARTESIAN_POINT('Ctrl Pts',(-59.7823898127242,-19.3405491061336,
2.67134639352705));
#235497=CARTESIAN_POINT('Ctrl Pts',(-59.7820371343798,-19.3370918919976,
2.67265375584981));
#235498=CARTESIAN_POINT('Ctrl Pts',(-59.7815825865437,-19.3336823180311,
2.67403135126909));
#235499=CARTESIAN_POINT('Ctrl Pts',(-59.7813553126257,-19.3319775310478,
2.67472014897873));
#235500=CARTESIAN_POINT('Ctrl Pts',(-59.7811025767641,-19.3302846375612,
2.67542649668602));
#235501=CARTESIAN_POINT('Ctrl Pts',(-59.7808251076835,-19.3286047092266,
2.67614899656071));
#235502=CARTESIAN_POINT('Ctrl Pts',(-59.7807557404133,-19.328184727143,
2.67632962152938));
#235503=CARTESIAN_POINT('Ctrl Pts',(-59.7806848274336,-19.3277655550292,
2.67651125590919));
#235504=CARTESIAN_POINT('Ctrl Pts',(-59.7806123803665,-19.3273472089197,
2.67669387767492));
#235505=CARTESIAN_POINT('Ctrl Pts',(-59.7803950391652,-19.3260921705914,
2.67724174297213));
#235506=CARTESIAN_POINT('Ctrl Pts',(-59.7801638905866,-19.3248445680579,
2.67779849504716));
#235507=CARTESIAN_POINT('Ctrl Pts',(-59.7799192536868,-19.3236048185588,
2.67836353617977));
#235508=CARTESIAN_POINT('Ctrl Pts',(-59.7782286609225,-19.3150373803111,
2.68226832098874));
#235509=CARTESIAN_POINT('Ctrl Pts',(-59.775932168172,-19.3068044648775,
2.68659153751355));
#235510=CARTESIAN_POINT('Ctrl Pts',(-59.7731456380809,-19.2989322844408,
2.69123699486139));
#235511=CARTESIAN_POINT('Ctrl Pts',(-59.7717607402744,-19.2950198323724,
2.6935457744118));
#235512=CARTESIAN_POINT('Ctrl Pts',(-59.7702542302927,-19.2911962646694,
2.69593478828083));
#235513=CARTESIAN_POINT('Ctrl Pts',(-59.7686372707429,-19.2874640247236,
2.69839565261188));
#235514=CARTESIAN_POINT('Ctrl Pts',(-59.7650700164609,-19.2792301459419,
2.70382468689013));
#235515=CARTESIAN_POINT('Ctrl Pts',(-59.76097697069,-19.2714367138416,2.70961155815055));
#235516=CARTESIAN_POINT('Ctrl Pts',(-59.7564706723511,-19.2641757185814,
2.71562701361736));
#235517=CARTESIAN_POINT('Ctrl Pts',(-59.7548244647405,-19.261523185447,
2.71782453535826));
#235518=CARTESIAN_POINT('Ctrl Pts',(-59.7531276155318,-19.2589351484757,
2.72005051502371));
#235519=CARTESIAN_POINT('Ctrl Pts',(-59.7513854342765,-19.2564118357498,
2.72229986760084));
#235520=CARTESIAN_POINT('Ctrl Pts',(-59.7455336317917,-19.2479362953117,
2.72985520488853));
#235521=CARTESIAN_POINT('Ctrl Pts',(-59.7391263493542,-19.2401420439518,
2.73770845534514));
#235522=CARTESIAN_POINT('Ctrl Pts',(-59.7322837268617,-19.2329840462271,
2.74576706701703));
#235523=CARTESIAN_POINT('Ctrl Pts',(-59.7247628741805,-19.225116558807,
2.75462443584975));
#235524=CARTESIAN_POINT('Ctrl Pts',(-59.7167157560781,-19.2180171087292,
2.76373036323122));
#235525=CARTESIAN_POINT('Ctrl Pts',(-59.7082546997633,-19.2116502033065,
2.77299664636754));
#235526=CARTESIAN_POINT('Ctrl Pts',(-59.6991417795849,-19.2047927733661,
2.78297683033402));
#235527=CARTESIAN_POINT('Ctrl Pts',(-59.6895478206998,-19.1987842816761,
2.7931440147881));
#235528=CARTESIAN_POINT('Ctrl Pts',(-59.6795708632013,-19.1936187207963,
2.8034145242784));
#235529=CARTESIAN_POINT('Ctrl Pts',(-59.6697286283156,-19.1885229124295,
2.81354634721295));
#235530=CARTESIAN_POINT('Ctrl Pts',(-59.6595122814322,-19.1842470541692,
2.82378004209163));
#235531=CARTESIAN_POINT('Ctrl Pts',(-59.6489943884562,-19.1808295835784,
2.83404198860248));
#235532=CARTESIAN_POINT('Ctrl Pts',(-56.3771794532806,-18.1177524687109,
2.83404198860248));
#235533=CARTESIAN_POINT('Ctrl Pts',(-56.3671137719635,-18.1144819305949,
2.82422126442906));
#235534=CARTESIAN_POINT('Ctrl Pts',(-56.3568263239547,-18.1120170699775,
2.81442815028313));
#235535=CARTESIAN_POINT('Ctrl Pts',(-56.3463749453321,-18.1103629196645,
2.80471618166045));
#235536=CARTESIAN_POINT('Ctrl Pts',(-56.3362832197196,-18.1087656919989,
2.79533842145905));
#235537=CARTESIAN_POINT('Ctrl Pts',(-56.3260373921176,-18.1079242184403,
2.78603515649865));
#235538=CARTESIAN_POINT('Ctrl Pts',(-56.3156801719786,-18.1078879163649,
2.77685887346334));
#235539=CARTESIAN_POINT('Ctrl Pts',(-56.305889355267,-18.1078535995346,
2.76818441216131));
#235540=CARTESIAN_POINT('Ctrl Pts',(-56.2959980926869,-18.108538794987,
2.75962261521157));
#235541=CARTESIAN_POINT('Ctrl Pts',(-56.2860490151076,-18.1100266905438,
2.75123537701174));
#235542=CARTESIAN_POINT('Ctrl Pts',(-56.2768860815655,-18.1113970173903,
2.74351087133627));
#235543=CARTESIAN_POINT('Ctrl Pts',(-56.2676735798131,-18.1134483398666,
2.7359339944935));
#235544=CARTESIAN_POINT('Ctrl Pts',(-56.2584600414594,-18.1162805994802,
2.72857657812077));
#235545=CARTESIAN_POINT('Ctrl Pts',(-56.2557127503125,-18.1171251221232,
2.72638274507984));
#235546=CARTESIAN_POINT('Ctrl Pts',(-56.2529655048655,-18.1180393245084,
2.72420861709419));
#235547=CARTESIAN_POINT('Ctrl Pts',(-56.250219989383,-18.1190265064342,
2.72205663736694));
#235548=CARTESIAN_POINT('Ctrl Pts',(-56.2475025263005,-18.1200036017944,
2.71992664556733));
#235549=CARTESIAN_POINT('Ctrl Pts',(-56.2447894850829,-18.1210509212418,
2.71782089927852));
#235550=CARTESIAN_POINT('Ctrl Pts',(-56.2420855046789,-18.1221702476366,
2.71574387311213));
#235551=CARTESIAN_POINT('Ctrl Pts',(-56.2418974751698,-18.1222480834051,
2.71559944077454));
#235552=CARTESIAN_POINT('Ctrl Pts',(-56.241709480363,-18.12232625961,2.71545515216036));
#235553=CARTESIAN_POINT('Ctrl Pts',(-56.2415215209612,-18.1224047773506,
2.71531100781698));
#235554=CARTESIAN_POINT('Ctrl Pts',(-56.2332806922381,-18.1258472827276,
2.70899119176049));
#235555=CARTESIAN_POINT('Ctrl Pts',(-56.2251347899176,-18.1299826829657,
2.70298296066802));
#235556=CARTESIAN_POINT('Ctrl Pts',(-56.2171955585584,-18.1348427679841,
2.69736727774099));
#235557=CARTESIAN_POINT('Ctrl Pts',(-56.2097948151024,-18.1393732118984,
2.69213248525389));
#235558=CARTESIAN_POINT('Ctrl Pts',(-56.202573137601,-18.144534000151,2.68723866185426));
#235559=CARTESIAN_POINT('Ctrl Pts',(-56.1956479299628,-18.1503626543102,
2.68278595829519));
#235560=CARTESIAN_POINT('Ctrl Pts',(-56.1931145994157,-18.1524948514083,
2.68115710172764));
#235561=CARTESIAN_POINT('Ctrl Pts',(-56.1906212529491,-18.1547164978841,
2.67958763637771));
#235562=CARTESIAN_POINT('Ctrl Pts',(-56.1881748397224,-18.1570296338739,
2.67808378645328));
#235563=CARTESIAN_POINT('Ctrl Pts',(-56.1875865590688,-18.1575858658044,
2.67772216078563));
#235564=CARTESIAN_POINT('Ctrl Pts',(-56.1870008763866,-18.1581479603548,
2.67736403603526));
#235565=CARTESIAN_POINT('Ctrl Pts',(-56.186417921567,-18.1587158783115,
2.67700956934442));
#235566=CARTESIAN_POINT('Ctrl Pts',(-56.1858531840856,-18.159266048832,
2.67666617973767));
#235567=CARTESIAN_POINT('Ctrl Pts',(-56.1852910066464,-18.1598216844587,
2.67632622314082));
#235568=CARTESIAN_POINT('Ctrl Pts',(-56.1847315084903,-18.1603827459286,
2.67598984158737));
#235569=CARTESIAN_POINT('Ctrl Pts',(-56.1786015595924,-18.1665298227359,
2.67230439292192));
#235570=CARTESIAN_POINT('Ctrl Pts',(-56.172789482861,-18.173332530211,2.66904964539951));
#235571=CARTESIAN_POINT('Ctrl Pts',(-56.1674665972293,-18.1807122308847,
2.66640203566705));
#235572=CARTESIAN_POINT('Ctrl Pts',(-56.1652590378994,-18.1837728127195,
2.66530399299413));
#235573=CARTESIAN_POINT('Ctrl Pts',(-56.1631354730307,-18.1869322368373,
2.66430995142227));
#235574=CARTESIAN_POINT('Ctrl Pts',(-56.1611070880437,-18.1901833857455,
2.66343053473324));
#235575=CARTESIAN_POINT('Ctrl Pts',(-56.1576474660759,-18.1957285590018,
2.66193059792848));
#235576=CARTESIAN_POINT('Ctrl Pts',(-56.1544671656476,-18.2015400422205,
2.66076519817091));
#235577=CARTESIAN_POINT('Ctrl Pts',(-56.1516266854594,-18.2075773774754,
2.65997805604424));
#235578=CARTESIAN_POINT('Ctrl Pts',(-56.1502064453653,-18.2105960451028,
2.6595844849809));
#235579=CARTESIAN_POINT('Ctrl Pts',(-56.1488725139552,-18.2136716866511,
2.65928526260726));
#235580=CARTESIAN_POINT('Ctrl Pts',(-56.1476325143033,-18.2167992197298,
2.65908463971288));
#235581=CARTESIAN_POINT('Ctrl Pts',(-56.1463925146515,-18.2199267528084,
2.65888401681851));
#235582=CARTESIAN_POINT('Ctrl Pts',(-56.145246443375,-18.2231061318822,
2.65878198860248));
#235583=CARTESIAN_POINT('Ctrl Pts',(-56.1441998575526,-18.2263320786585,
2.65878198860248));
#235584=CARTESIAN_POINT('Origin',(-53.2204057122636,-23.7119335237428,2.83404198860244));
#235585=CARTESIAN_POINT('Ctrl Pts',(-57.1623216544369,-25.6588335304443,
2.83404198860243));
#235586=CARTESIAN_POINT('Ctrl Pts',(-57.1720146727776,-25.6631491402568,
2.82419652440027));
#235587=CARTESIAN_POINT('Ctrl Pts',(-57.1820194461954,-25.6666871334686,
2.81438790575597));
#235588=CARTESIAN_POINT('Ctrl Pts',(-57.1922776320702,-25.669438145482,
2.80466781256838));
#235589=CARTESIAN_POINT('Ctrl Pts',(-57.2022024879876,-25.6720997659862,
2.79526356453007));
#235590=CARTESIAN_POINT('Ctrl Pts',(-57.2123658169601,-25.6740249857411,
2.78594102496156));
#235591=CARTESIAN_POINT('Ctrl Pts',(-57.2227298227165,-25.675161647087,
2.776751090887));
#235592=CARTESIAN_POINT('Ctrl Pts',(-57.2325335339833,-25.6762368587286,
2.76805797913601));
#235593=CARTESIAN_POINT('Ctrl Pts',(-57.2425177322908,-25.6766065729229,
2.75948271210079));
#235594=CARTESIAN_POINT('Ctrl Pts',(-57.2526488462851,-25.6761845643573,
2.75108575573142));
#235595=CARTESIAN_POINT('Ctrl Pts',(-57.2619803349747,-25.675795863948,
2.74335155163188));
#235596=CARTESIAN_POINT('Ctrl Pts',(-57.2714370189571,-25.6747354076182,
2.7357681868586));
#235597=CARTESIAN_POINT('Ctrl Pts',(-57.2809814365681,-25.6728992535085,
2.72840626160414));
#235598=CARTESIAN_POINT('Ctrl Pts',(-57.2837499093058,-25.6723666549989,
2.72627084693618));
#235599=CARTESIAN_POINT('Ctrl Pts',(-57.2865256584302,-25.6717685445831,
2.72415424587481));
#235600=CARTESIAN_POINT('Ctrl Pts',(-57.2893074725858,-25.6711017521907,
2.72205867173237));
#235601=CARTESIAN_POINT('Ctrl Pts',(-57.2923231379854,-25.6703789063664,
2.71978693462841));
#235602=CARTESIAN_POINT('Ctrl Pts',(-57.2953419866641,-25.6695773996876,
2.71754411340741));
#235603=CARTESIAN_POINT('Ctrl Pts',(-57.2983617649662,-25.6686939261489,
2.71533341844238));
#235604=CARTESIAN_POINT('Ctrl Pts',(-57.306649570212,-25.6662692260896,
2.70926614876386));
#235605=CARTESIAN_POINT('Ctrl Pts',(-57.3149216961104,-25.6631888860747,
2.70347381860404));
#235606=CARTESIAN_POINT('Ctrl Pts',(-57.3230760282578,-25.6594348051809,
2.6980491417139));
#235607=CARTESIAN_POINT('Ctrl Pts',(-57.3305367994637,-25.6560000249769,
2.69308585687203));
#235608=CARTESIAN_POINT('Ctrl Pts',(-57.3378885241128,-25.6519962425129,
2.68842799053186));
#235609=CARTESIAN_POINT('Ctrl Pts',(-57.3450563828667,-25.6473759219979,
2.6841476705422));
#235610=CARTESIAN_POINT('Ctrl Pts',(-57.3485772116718,-25.6451064356538,
2.68204519134552));
#235611=CARTESIAN_POINT('Ctrl Pts',(-57.3520532672061,-25.6426878935084,
2.680034317785));
#235612=CARTESIAN_POINT('Ctrl Pts',(-57.3554727521279,-25.6401130415749,
2.67812693945248));
#235613=CARTESIAN_POINT('Ctrl Pts',(-57.3561215660856,-25.6396244884999,
2.677765032992));
#235614=CARTESIAN_POINT('Ctrl Pts',(-57.3567684269675,-25.6391297826974,
2.6774065963992));
#235615=CARTESIAN_POINT('Ctrl Pts',(-57.357413196712,-25.6386289474846,
2.67705178968851));
#235616=CARTESIAN_POINT('Ctrl Pts',(-57.358037817402,-25.6381437633721,
2.67670807068754));
#235617=CARTESIAN_POINT('Ctrl Pts',(-57.3586604755989,-25.637652826975,
2.67636775825261));
#235618=CARTESIAN_POINT('Ctrl Pts',(-57.3592810442413,-25.6371561630117,
2.67603099699251));
#235619=CARTESIAN_POINT('Ctrl Pts',(-57.3660438734346,-25.6317436214792,
2.67236104217124));
#235620=CARTESIAN_POINT('Ctrl Pts',(-57.3725627409493,-25.625646988583,
2.6691144054147));
#235621=CARTESIAN_POINT('Ctrl Pts',(-57.3786559602403,-25.6189233999296,
2.66646778189627));
#235622=CARTESIAN_POINT('Ctrl Pts',(-57.381229164584,-25.6160839866898,
2.6653500963497));
#235623=CARTESIAN_POINT('Ctrl Pts',(-57.3837265592142,-25.6131331854693,
2.6643389791234));
#235624=CARTESIAN_POINT('Ctrl Pts',(-57.386135383163,-25.6100770039414,
2.66344564884788));
#235625=CARTESIAN_POINT('Ctrl Pts',(-57.3901917825028,-25.6049304706141,
2.66194130298581));
#235626=CARTESIAN_POINT('Ctrl Pts',(-57.3939944983912,-25.5994853721131,
2.66077206705415));
#235627=CARTESIAN_POINT('Ctrl Pts',(-57.3974772155311,-25.5937750303533,
2.65998225155709));
#235628=CARTESIAN_POINT('Ctrl Pts',(-57.3983478948161,-25.5923474449133,
2.65978479768283));
#235629=CARTESIAN_POINT('Ctrl Pts',(-57.39919836688,-25.5909031732844,2.65961098966617));
#235630=CARTESIAN_POINT('Ctrl Pts',(-57.4000273167766,-25.5894426040346,
2.65946139030496));
#235631=CARTESIAN_POINT('Ctrl Pts',(-57.4012707416215,-25.5872517501598,
2.65923699126315));
#235632=CARTESIAN_POINT('Ctrl Pts',(-57.4024657229508,-25.5850242354388,
2.65906707562436));
#235633=CARTESIAN_POINT('Ctrl Pts',(-57.4036093482795,-25.58276207061,2.65895332562914));
#235634=CARTESIAN_POINT('Ctrl Pts',(-57.4047529736081,-25.5804999057813,
2.65883957563392));
#235635=CARTESIAN_POINT('Ctrl Pts',(-57.405845248421,-25.578203101074,2.65878198860243));
#235636=CARTESIAN_POINT('Ctrl Pts',(-57.4068835917993,-25.5758735661218,
2.65878198860243));
#235637=CARTESIAN_POINT('Ctrl Pts',(-53.9190682401993,-24.0229981225299,
2.65878198860244));
#235638=CARTESIAN_POINT('Ctrl Pts',(-53.9155545931357,-24.0308804555188,
2.65878198860244));
#235639=CARTESIAN_POINT('Ctrl Pts',(-53.9127220553015,-24.0389845034719,
2.65945335517837));
#235640=CARTESIAN_POINT('Ctrl Pts',(-53.9105453488013,-24.0471612846379,
2.66072561226581));
#235641=CARTESIAN_POINT('Ctrl Pts',(-53.9091394197451,-24.0524426462851,
2.6615473598032));
#235642=CARTESIAN_POINT('Ctrl Pts',(-53.9080061861137,-24.0577541205276,
2.66261895766866));
#235643=CARTESIAN_POINT('Ctrl Pts',(-53.907129996454,-24.0630550795264,
2.66391429251012));
#235644=CARTESIAN_POINT('Ctrl Pts',(-53.9059686572513,-24.0700811970214,
2.66563118464108));
#235645=CARTESIAN_POINT('Ctrl Pts',(-53.9052646847384,-24.0770886066608,
2.66774105138683));
#235646=CARTESIAN_POINT('Ctrl Pts',(-53.9049900928802,-24.0839917000395,
2.67016894181734));
#235647=CARTESIAN_POINT('Ctrl Pts',(-53.9048527969511,-24.0874432467288,
2.67138288703259));
#235648=CARTESIAN_POINT('Ctrl Pts',(-53.9048227635321,-24.0908688957001,
2.67267613167535));
#235649=CARTESIAN_POINT('Ctrl Pts',(-53.9048959123381,-24.0942592346731,
2.67403835432537));
#235650=CARTESIAN_POINT('Ctrl Pts',(-53.9049324867411,-24.0959544041596,
2.67471946565037));
#235651=CARTESIAN_POINT('Ctrl Pts',(-53.9049948499726,-24.0976407611372,
2.67541781389506));
#235652=CARTESIAN_POINT('Ctrl Pts',(-53.905082449642,-24.099317223136,2.67613207244152));
#235653=CARTESIAN_POINT('Ctrl Pts',(-53.9051043495593,-24.0997363386357,
2.67631063707814));
#235654=CARTESIAN_POINT('Ctrl Pts',(-53.90512782661,-24.1001548360176,2.67649019601829));
#235655=CARTESIAN_POINT('Ctrl Pts',(-53.9051528718721,-24.1005726990102,
2.6766707283664));
#235656=CARTESIAN_POINT('Ctrl Pts',(-53.9052280076583,-24.1018262879881,
2.67721232541074));
#235657=CARTESIAN_POINT('Ctrl Pts',(-53.9053172580726,-24.1030741658757,
2.6777626834003));
#235658=CARTESIAN_POINT('Ctrl Pts',(-53.9054203757495,-24.1043159075202,
2.67832123541499));
#235659=CARTESIAN_POINT('Ctrl Pts',(-53.9061467233508,-24.1130625753257,
2.68225560368422));
#235660=CARTESIAN_POINT('Ctrl Pts',(-53.9075195712147,-24.1215389842443,
2.6866179299886));
#235661=CARTESIAN_POINT('Ctrl Pts',(-53.9094265129029,-24.1297041260866,
2.69130986622543));
#235662=CARTESIAN_POINT('Ctrl Pts',(-53.910351377561,-24.133664211057,2.69358545023025));
#235663=CARTESIAN_POINT('Ctrl Pts',(-53.9114023832598,-24.1375513523935,
2.69593918853446));
#235664=CARTESIAN_POINT('Ctrl Pts',(-53.9125693701069,-24.1413619171792,
2.69836306235458));
#235665=CARTESIAN_POINT('Ctrl Pts',(-53.9143559454348,-24.1471956256297,
2.70207384382191));
#235666=CARTESIAN_POINT('Ctrl Pts',(-53.9164123347818,-24.1528469606266,
2.7059476081419));
#235667=CARTESIAN_POINT('Ctrl Pts',(-53.9187002605237,-24.1582902100541,
2.7099519634567));
#235668=CARTESIAN_POINT('Ctrl Pts',(-53.9197627850744,-24.1608180832479,
2.71181160678068));
#235669=CARTESIAN_POINT('Ctrl Pts',(-53.9208749910656,-24.1633010951265,
2.71369962772062));
#235670=CARTESIAN_POINT('Ctrl Pts',(-53.9220340502325,-24.1657359576696,
2.71561183138624));
#235671=CARTESIAN_POINT('Ctrl Pts',(-53.9221228875507,-24.1659225802897,
2.71575839426275));
#235672=CARTESIAN_POINT('Ctrl Pts',(-53.9222119774185,-24.1661089452649,
2.71590508903172));
#235673=CARTESIAN_POINT('Ctrl Pts',(-53.9223013184208,-24.1662950522344,
2.71605191409874));
#235674=CARTESIAN_POINT('Ctrl Pts',(-53.9235562901481,-24.1689092940617,
2.71811436362715));
#235675=CARTESIAN_POINT('Ctrl Pts',(-53.9248627542248,-24.1714718460793,
2.72020091026922));
#235676=CARTESIAN_POINT('Ctrl Pts',(-53.9262153118346,-24.1739808617162,
2.72230624862144));
#235677=CARTESIAN_POINT('Ctrl Pts',(-53.9310653428794,-24.1829777455767,
2.72985561753085));
#235678=CARTESIAN_POINT('Ctrl Pts',(-53.9365438157569,-24.1913567365402,
2.73770089914333));
#235679=CARTESIAN_POINT('Ctrl Pts',(-53.9425259106384,-24.1991508947542,
2.74574823347098));
#235680=CARTESIAN_POINT('Ctrl Pts',(-53.9490996319585,-24.207715891639,
2.75459144547082));
#235681=CARTESIAN_POINT('Ctrl Pts',(-53.9562817849782,-24.2155752681679,
2.76367911754364));
#235682=CARTESIAN_POINT('Ctrl Pts',(-53.9639562340156,-24.2227540584941,
2.77292162564857));
#235683=CARTESIAN_POINT('Ctrl Pts',(-53.9722427129526,-24.2305053504162,
2.78290121484941));
#235684=CARTESIAN_POINT('Ctrl Pts',(-53.9811038680515,-24.2374640812955,
2.7930622950048));
#235685=CARTESIAN_POINT('Ctrl Pts',(-53.9904403792203,-24.2436285779155,
2.80331916685628));
#235686=CARTESIAN_POINT('Ctrl Pts',(-53.9996985666513,-24.2497413607414,
2.8134899940894));
#235687=CARTESIAN_POINT('Ctrl Pts',(-54.0094254978916,-24.2550737197513,
2.82375635966991));
#235688=CARTESIAN_POINT('Ctrl Pts',(-54.0195518809639,-24.2595822759735,
2.83404198860244));
#235689=CARTESIAN_POINT('Origin',(-0.00619866644046454,0.0139224327746649,
2.83404198860262));
#235690=CARTESIAN_POINT('Ctrl Pts',(-57.4192809246787,-25.5480287005721,
2.65878198860243));
#235691=CARTESIAN_POINT('Ctrl Pts',(-57.4227710771204,-25.5401808584717,
2.65878198860243));
#235692=CARTESIAN_POINT('Ctrl Pts',(-57.4255746438787,-25.5321112063499,
2.65944603041834));
#235693=CARTESIAN_POINT('Ctrl Pts',(-57.4277200319916,-25.5239679177298,
2.66070439264058));
#235694=CARTESIAN_POINT('Ctrl Pts',(-57.4290908328637,-25.5187647439657,
2.66150842619582));
#235695=CARTESIAN_POINT('Ctrl Pts',(-57.4301938346425,-25.5135317242465,
2.66255428265352));
#235696=CARTESIAN_POINT('Ctrl Pts',(-57.4310450321039,-25.508307941095,
2.66381699700635));
#235697=CARTESIAN_POINT('Ctrl Pts',(-57.4322067458447,-25.5011785252535,
2.66554034873234));
#235698=CARTESIAN_POINT('Ctrl Pts',(-57.4328933558605,-25.4940667032539,
2.66766759643938));
#235699=CARTESIAN_POINT('Ctrl Pts',(-57.4331362848726,-25.4870628291427,
2.67012012783114));
#235700=CARTESIAN_POINT('Ctrl Pts',(-57.4332577493786,-25.4835608920871,
2.67134639352702));
#235701=CARTESIAN_POINT('Ctrl Pts',(-57.4332683803239,-25.4800857520065,
2.67265375584979));
#235702=CARTESIAN_POINT('Ctrl Pts',(-57.4331727200756,-25.4766473428561,
2.67403135126906));
#235703=CARTESIAN_POINT('Ctrl Pts',(-57.4331248899515,-25.4749281382809,
2.6747201489787));
#235704=CARTESIAN_POINT('Ctrl Pts',(-57.433050494158,-25.4732181005507,
2.67542649668599));
#235705=CARTESIAN_POINT('Ctrl Pts',(-57.4329501454092,-25.4715183716227,
2.67614899656068));
#235706=CARTESIAN_POINT('Ctrl Pts',(-57.4329250582221,-25.4710934393907,
2.67632962152936));
#235707=CARTESIAN_POINT('Ctrl Pts',(-57.432898349128,-25.4706691511208,
2.67651125590916));
#235708=CARTESIAN_POINT('Ctrl Pts',(-57.4328700280094,-25.4702455239746,
2.6766938776749));
#235709=CARTESIAN_POINT('Ctrl Pts',(-57.4327850646537,-25.4689746425358,
2.6772417429721));
#235710=CARTESIAN_POINT('Ctrl Pts',(-57.4326855923069,-25.4677097128937,
2.67779849504714));
#235711=CARTESIAN_POINT('Ctrl Pts',(-57.4325718846635,-25.4664511833529,
2.67836353617975));
#235712=CARTESIAN_POINT('Ctrl Pts',(-57.4317860942974,-25.4577539633644,
2.68226832098887));
#235713=CARTESIAN_POINT('Ctrl Pts',(-57.430362755973,-25.4493260998445,
2.68659153751386));
#235714=CARTESIAN_POINT('Ctrl Pts',(-57.4284143577087,-25.4412057723273,
2.69123699486191));
#235715=CARTESIAN_POINT('Ctrl Pts',(-57.4274460091197,-25.4371699918415,
2.69354577441215));
#235716=CARTESIAN_POINT('Ctrl Pts',(-57.4263474236136,-25.4332098968695,
2.69593478828099));
#235717=CARTESIAN_POINT('Ctrl Pts',(-57.4251294472436,-25.4293290842281,
2.69839565261185));
#235718=CARTESIAN_POINT('Ctrl Pts',(-57.4224424094495,-25.4207674318877,
2.7038246868901));
#235719=CARTESIAN_POINT('Ctrl Pts',(-57.4191864212927,-25.4125888532393,
2.70961155815051));
#235720=CARTESIAN_POINT('Ctrl Pts',(-57.4154637896039,-25.4048965980306,
2.71562701361731));
#235721=CARTESIAN_POINT('Ctrl Pts',(-57.4141038653031,-25.4020865201984,
2.71782453535822));
#235722=CARTESIAN_POINT('Ctrl Pts',(-57.4126868351393,-25.3993352917243,
2.72005051502366));
#235723=CARTESIAN_POINT('Ctrl Pts',(-57.4112179557368,-25.3966436944401,
2.72229986760078));
#235724=CARTESIAN_POINT('Ctrl Pts',(-57.4062841452555,-25.3876029039779,
2.72985520488874));
#235725=CARTESIAN_POINT('Ctrl Pts',(-57.4007266836983,-25.3791816069552,
2.73770845534561));
#235726=CARTESIAN_POINT('Ctrl Pts',(-57.3946697603096,-25.3713475726768,
2.74576706701778));
#235727=CARTESIAN_POINT('Ctrl Pts',(-57.3880124840157,-25.3627370410024,
2.75462443585078));
#235728=CARTESIAN_POINT('Ctrl Pts',(-57.3807515434745,-25.3548353295657,
2.76373036323256));
#235729=CARTESIAN_POINT('Ctrl Pts',(-57.3730023605507,-25.3476188815027,
2.77299664636921));
#235730=CARTESIAN_POINT('Ctrl Pts',(-57.3646561585156,-25.3398464577386,
2.78297683033614));
#235731=CARTESIAN_POINT('Ctrl Pts',(-57.3557428147435,-25.3328680394157,
2.7931440147907));
#235732=CARTESIAN_POINT('Ctrl Pts',(-57.3463604602023,-25.3266878999834,
2.80341452428155));
#235733=CARTESIAN_POINT('Ctrl Pts',(-57.3371047991278,-25.3205912133012,
2.81354634721498));
#235734=CARTESIAN_POINT('Ctrl Pts',(-57.327391367356,-25.3152708796007,
2.82378004209258));
#235735=CARTESIAN_POINT('Ctrl Pts',(-57.3172883154488,-25.3107727110825,
2.83404198860243));
#235736=CARTESIAN_POINT('Ctrl Pts',(-54.1745185419758,-23.9115214566117,
2.83404198860244));
#235737=CARTESIAN_POINT('Ctrl Pts',(-54.1648498658387,-23.9072166846465,
2.8242212644303));
#235738=CARTESIAN_POINT('Ctrl Pts',(-54.1548764216403,-23.9036899956625,
2.81442815028565));
#235739=CARTESIAN_POINT('Ctrl Pts',(-54.144655202555,-23.9009524404118,
2.80471618166422));
#235740=CARTESIAN_POINT('Ctrl Pts',(-54.1347857162255,-23.8983090899564,
2.79533842146358));
#235741=CARTESIAN_POINT('Ctrl Pts',(-54.124683974278,-23.8964012454638,
2.78603515650393));
#235742=CARTESIAN_POINT('Ctrl Pts',(-54.1143872866757,-23.8952825179499,
2.77685887346932));
#235743=CARTESIAN_POINT('Ctrl Pts',(-54.1046536921685,-23.8942249700855,
2.76818441216765));
#235744=CARTESIAN_POINT('Ctrl Pts',(-54.0947449925326,-23.8938724934879,
2.75962261521823));
#235745=CARTESIAN_POINT('Ctrl Pts',(-54.0846948896058,-23.8943122764064,
2.75123537701868));
#235746=CARTESIAN_POINT('Ctrl Pts',(-54.0754389134133,-23.8947173090964,
2.74351087134334));
#235747=CARTESIAN_POINT('Ctrl Pts',(-54.0660624571237,-23.895794425562,
2.73593399450066));
#235748=CARTESIAN_POINT('Ctrl Pts',(-54.0566033397524,-23.8976480927551,
2.728576578128));
#235749=CARTESIAN_POINT('Ctrl Pts',(-54.0537828218968,-23.8982008188934,
2.7263827450846));
#235750=CARTESIAN_POINT('Ctrl Pts',(-54.0509550659742,-23.8988228478381,
2.72420861709654));
#235751=CARTESIAN_POINT('Ctrl Pts',(-54.0481214021001,-23.8995176373646,
2.72205663736691));
#235752=CARTESIAN_POINT('Ctrl Pts',(-54.0453166912881,-23.9002053278541,
2.7199266455673));
#235753=CARTESIAN_POINT('Ctrl Pts',(-54.0425090377018,-23.9009633199468,
2.71782089927848));
#235754=CARTESIAN_POINT('Ctrl Pts',(-54.0397028685175,-23.9017938716382,
2.7157438731121));
#235755=CARTESIAN_POINT('Ctrl Pts',(-54.0395077330004,-23.9018516265785,
2.7155994407745));
#235756=CARTESIAN_POINT('Ctrl Pts',(-54.0393125964103,-23.9019097237178,
2.71545515216033));
#235757=CARTESIAN_POINT('Ctrl Pts',(-54.039117459331,-23.9019681642225,
2.71531100781694));
#235758=CARTESIAN_POINT('Ctrl Pts',(-54.0305619349331,-23.9045304100324,
2.70899119176051));
#235759=CARTESIAN_POINT('Ctrl Pts',(-54.0220283896861,-23.9077916774637,
2.70298296066809));
#235760=CARTESIAN_POINT('Ctrl Pts',(-54.0136246330487,-23.9117952627744,
2.6973672777411));
#235761=CARTESIAN_POINT('Ctrl Pts',(-54.0057908712997,-23.9155273001022,
2.69213248525413));
#235762=CARTESIAN_POINT('Ctrl Pts',(-53.9980693056381,-23.9199049461652,
2.68723866185462));
#235763=CARTESIAN_POINT('Ctrl Pts',(-53.9905727747499,-23.9249777890347,
2.68278595829563));
#235764=CARTESIAN_POINT('Ctrl Pts',(-53.9878304467663,-23.9268335005851,
2.68115710172792));
#235765=CARTESIAN_POINT('Ctrl Pts',(-53.9851185338202,-23.9287823509747,
2.67958763637783));
#235766=CARTESIAN_POINT('Ctrl Pts',(-53.9824437337505,-23.9308270955486,
2.67808378645326));
#235767=CARTESIAN_POINT('Ctrl Pts',(-53.981800533691,-23.9313187883097,
2.67772216078561));
#235768=CARTESIAN_POINT('Ctrl Pts',(-53.9811593045602,-23.9318165831366,
2.67736403603524));
#235769=CARTESIAN_POINT('Ctrl Pts',(-53.9805201796369,-23.9323204546078,
2.6770095693444));
#235770=CARTESIAN_POINT('Ctrl Pts',(-53.9799010273675,-23.9328085800956,
2.67666617973765));
#235771=CARTESIAN_POINT('Ctrl Pts',(-53.9792838498569,-23.9333024083484,
2.6763262231408));
#235772=CARTESIAN_POINT('Ctrl Pts',(-53.978668769797,-23.9338019127824,
2.67598984158734));
#235773=CARTESIAN_POINT('Ctrl Pts',(-53.971929856908,-23.9392745611218,
2.67230439292171));
#235774=CARTESIAN_POINT('Ctrl Pts',(-53.9654385427822,-23.9454324752049,
2.66904964539916));
#235775=CARTESIAN_POINT('Ctrl Pts',(-53.9593734277039,-23.9522153560512,
2.66640203566662));
#235776=CARTESIAN_POINT('Ctrl Pts',(-53.9568580436994,-23.9550284189139,
2.66530399299386));
#235777=CARTESIAN_POINT('Ctrl Pts',(-53.9544158621937,-23.9579485624031,
2.66430995142214));
#235778=CARTESIAN_POINT('Ctrl Pts',(-53.952058751313,-23.9609698772114,
2.66343053473321));
#235779=CARTESIAN_POINT('Ctrl Pts',(-53.9480384530773,-23.9661230444607,
2.66193059792845));
#235780=CARTESIAN_POINT('Ctrl Pts',(-53.9442681092574,-23.9715702598497,
2.66076519817088));
#235781=CARTESIAN_POINT('Ctrl Pts',(-53.9408121161402,-23.9772776109212,
2.6599780560442));
#235782=CARTESIAN_POINT('Ctrl Pts',(-53.9390841195816,-23.980131286457,
2.65958448498087));
#235783=CARTESIAN_POINT('Ctrl Pts',(-53.9374360035028,-23.9830506455188,
2.65928526260722));
#235784=CARTESIAN_POINT('Ctrl Pts',(-53.9358758804723,-23.9860314303859,
2.65908463971285));
#235785=CARTESIAN_POINT('Ctrl Pts',(-53.9343157574418,-23.9890122152531,
2.65888401681847));
#235786=CARTESIAN_POINT('Ctrl Pts',(-53.9328436288551,-23.9920543802863,
2.65878198860244));
#235787=CARTESIAN_POINT('Ctrl Pts',(-53.9314655730802,-23.995153256981,
2.65878198860244));
#235788=CARTESIAN_POINT('Origin',(-50.4502867888873,-29.1450842944631,2.8340419886024));
#235789=CARTESIAN_POINT('Ctrl Pts',(-54.1671020372436,-31.4933613949861,
2.83404198860239));
#235790=CARTESIAN_POINT('Ctrl Pts',(-54.176290852154,-31.4986665597482,
2.82419652440023));
#235791=CARTESIAN_POINT('Ctrl Pts',(-54.1858709973829,-31.5032309550537,
2.81438790575588));
#235792=CARTESIAN_POINT('Ctrl Pts',(-54.1957854287842,-31.507039169141,
2.80466781256822));
#235793=CARTESIAN_POINT('Ctrl Pts',(-54.2053777002014,-31.5107236389468,
2.79526356452981));
#235794=CARTESIAN_POINT('Ctrl Pts',(-54.215284113132,-31.5137006693056,
2.78594102496119));
#235795=CARTESIAN_POINT('Ctrl Pts',(-54.2254725303168,-31.5159144374967,
2.77675109088649));
#235796=CARTESIAN_POINT('Ctrl Pts',(-54.2351101456071,-31.5180085258895,
2.76805797913536));
#235797=CARTESIAN_POINT('Ctrl Pts',(-54.2450010037751,-31.5194198476567,
2.75948271209998));
#235798=CARTESIAN_POINT('Ctrl Pts',(-54.2551207303739,-31.5200591406752,
2.75108575573045));
#235799=CARTESIAN_POINT('Ctrl Pts',(-54.2644417304488,-31.52064797578,2.74335155163073));
#235800=CARTESIAN_POINT('Ctrl Pts',(-54.2739574575976,-31.5205818213851,
2.7357681868573));
#235801=CARTESIAN_POINT('Ctrl Pts',(-54.2836415202578,-31.5197533892253,
2.7284062616027));
#235802=CARTESIAN_POINT('Ctrl Pts',(-54.2864504987153,-31.519513092547,
2.72627084693521));
#235803=CARTESIAN_POINT('Ctrl Pts',(-54.2892735615577,-31.519208403433,
2.72415424587431));
#235804=CARTESIAN_POINT('Ctrl Pts',(-54.2921098354277,-31.518836042558,
2.72205867173232));
#235805=CARTESIAN_POINT('Ctrl Pts',(-54.2951845386599,-31.5184323794287,
2.71978693462836));
#235806=CARTESIAN_POINT('Ctrl Pts',(-54.2982706300311,-31.5179508191006,
2.71754411340737));
#235807=CARTESIAN_POINT('Ctrl Pts',(-54.301366213803,-31.5173878381077,
2.71533341844234));
#235808=CARTESIAN_POINT('Ctrl Pts',(-54.3098620677557,-31.5158427323552,
2.70926614876382));
#235809=CARTESIAN_POINT('Ctrl Pts',(-54.3184108612909,-31.5136439393734,
2.70347381860399));
#235810=CARTESIAN_POINT('Ctrl Pts',(-54.3269129314605,-31.5107627835359,
2.69804914171385));
#235811=CARTESIAN_POINT('Ctrl Pts',(-54.3346918640777,-31.508126682366,
2.69308585687177));
#235812=CARTESIAN_POINT('Ctrl Pts',(-54.3424218244386,-31.504913297521,
2.68842799053142));
#235813=CARTESIAN_POINT('Ctrl Pts',(-54.3500333719158,-31.5010675328655,
2.68414767054161));
#235814=CARTESIAN_POINT('Ctrl Pts',(-54.3537721391719,-31.4991785058296,
2.68204519134513));
#235815=CARTESIAN_POINT('Ctrl Pts',(-54.3574819590038,-31.4971365594545,
2.6800343177848));
#235816=CARTESIAN_POINT('Ctrl Pts',(-54.3611518569448,-31.4949332463336,
2.67812693945244));
#235817=CARTESIAN_POINT('Ctrl Pts',(-54.3618481843339,-31.4945151891294,
2.67776503299196));
#235818=CARTESIAN_POINT('Ctrl Pts',(-54.3625432124815,-31.494090808751,
2.67740659639916));
#235819=CARTESIAN_POINT('Ctrl Pts',(-54.363236801645,-31.4936601139564,
2.67705178968848));
#235820=CARTESIAN_POINT('Ctrl Pts',(-54.3639087161472,-31.4932428783741,
2.6767080706875));
#235821=CARTESIAN_POINT('Ctrl Pts',(-54.3645792801846,-31.4928197168825,
2.67636775825258));
#235822=CARTESIAN_POINT('Ctrl Pts',(-54.3652483648078,-31.4923906407828,
2.67603099699248));
#235823=CARTESIAN_POINT('Ctrl Pts',(-54.3725399111639,-31.4877146578621,
2.67236104217126));
#235824=CARTESIAN_POINT('Ctrl Pts',(-54.3796603393079,-31.4823328301625,
2.66911440541476));
#235825=CARTESIAN_POINT('Ctrl Pts',(-54.3864229856956,-31.4762829888802,
2.66646778189635));
#235826=CARTESIAN_POINT('Ctrl Pts',(-54.3892788932593,-31.4737281033388,
2.66535009634973));
#235827=CARTESIAN_POINT('Ctrl Pts',(-54.3920710496174,-31.471054515739,
2.66433897912339));
#235828=CARTESIAN_POINT('Ctrl Pts',(-54.3947861357353,-31.4682668669588,
2.66344564884785));
#235829=CARTESIAN_POINT('Ctrl Pts',(-54.399358272915,-31.4635725360689,
2.66194130298577));
#235830=CARTESIAN_POINT('Ctrl Pts',(-54.4037093249065,-31.4585547584354,
2.66077206705411));
#235831=CARTESIAN_POINT('Ctrl Pts',(-54.4077698566061,-31.4532397415956,
2.65998225155705));
#235832=CARTESIAN_POINT('Ctrl Pts',(-54.4087849895311,-31.4519109873857,
2.65978479768278));
#235833=CARTESIAN_POINT('Ctrl Pts',(-54.4097817701139,-31.4505635261658,
2.65961098966613));
#235834=CARTESIAN_POINT('Ctrl Pts',(-54.4107588499955,-31.4491976069259,
2.65946139030492));
#235835=CARTESIAN_POINT('Ctrl Pts',(-54.4122244698178,-31.4471487280662,
2.65923699126311));
#235836=CARTESIAN_POINT('Ctrl Pts',(-54.4136457436051,-31.4450583254659,
2.65906707562432));
#235837=CARTESIAN_POINT('Ctrl Pts',(-54.4150195646478,-31.442928094411,
2.6589533256291));
#235838=CARTESIAN_POINT('Ctrl Pts',(-54.4163933856905,-31.440797863356,
2.65883957563387));
#235839=CARTESIAN_POINT('Ctrl Pts',(-54.4177197583742,-31.438627814593,
2.65878198860239));
#235840=CARTESIAN_POINT('Ctrl Pts',(-54.4189959163076,-31.4364195775146,
2.65878198860239));
#235841=CARTESIAN_POINT('Ctrl Pts',(-51.1126068659044,-29.5274749692187,
2.65878198860241));
#235842=CARTESIAN_POINT('Ctrl Pts',(-51.1082885388128,-29.5349468458348,
2.65878198860241));
#235843=CARTESIAN_POINT('Ctrl Pts',(-51.1046244142384,-29.5427104181385,
2.65945335517834));
#235844=CARTESIAN_POINT('Ctrl Pts',(-51.1016049255943,-29.5506148782564,
2.66072561226581));
#235845=CARTESIAN_POINT('Ctrl Pts',(-51.0996546457477,-29.555720348448,
2.66154735980319));
#235846=CARTESIAN_POINT('Ctrl Pts',(-51.0979724198485,-29.5608842707088,
2.66261895766863));
#235847=CARTESIAN_POINT('Ctrl Pts',(-51.0965469289495,-29.5660646037407,
2.66391429251007));
#235848=CARTESIAN_POINT('Ctrl Pts',(-51.09465752242,-29.5729308384268,2.66563118464103));
#235849=CARTESIAN_POINT('Ctrl Pts',(-51.0932249325811,-29.5798262755781,
2.66774105138678));
#235850=CARTESIAN_POINT('Ctrl Pts',(-51.0922302752232,-29.5866628504239,
2.67016894181728));
#235851=CARTESIAN_POINT('Ctrl Pts',(-51.0917329465442,-29.5900811378468,
2.67138288703254));
#235852=CARTESIAN_POINT('Ctrl Pts',(-51.0913449998287,-29.5934848814075,
2.67267613167529));
#235853=CARTESIAN_POINT('Ctrl Pts',(-51.0910633609951,-29.5968642938812,
2.67403835432531));
#235854=CARTESIAN_POINT('Ctrl Pts',(-51.0909225415783,-29.598554000118,
2.67471946565032));
#235855=CARTESIAN_POINT('Ctrl Pts',(-51.0908082908741,-29.6002376377884,
2.67541781389501));
#235856=CARTESIAN_POINT('Ctrl Pts',(-51.0907201726669,-29.6019140726117,
2.67613207244147));
#235857=CARTESIAN_POINT('Ctrl Pts',(-51.090698143115,-29.6023331813176,
2.67631063707808));
#235858=CARTESIAN_POINT('Ctrl Pts',(-51.0906777466678,-29.6027518401471,
2.67649019601823));
#235859=CARTESIAN_POINT('Ctrl Pts',(-51.0906589761528,-29.6031700319853,
2.67667072836634));
#235860=CARTESIAN_POINT('Ctrl Pts',(-51.0906026646079,-29.6044246074998,
2.67721232541068));
#235861=CARTESIAN_POINT('Ctrl Pts',(-51.0905609873411,-29.6056749785905,
2.67776268340025));
#235862=CARTESIAN_POINT('Ctrl Pts',(-51.0905337427828,-29.6069206965766,
2.67832123541494));
#235863=CARTESIAN_POINT('Ctrl Pts',(-51.0903418356315,-29.6156953732194,
2.68225560368422));
#235864=CARTESIAN_POINT('Ctrl Pts',(-51.0908211368928,-29.6242688491606,
2.68661792998866));
#235865=CARTESIAN_POINT('Ctrl Pts',(-51.0918641424258,-29.6325885911859,
2.69130986622556));
#235866=CARTESIAN_POINT('Ctrl Pts',(-51.0923699989822,-29.6366236570778,
2.69358545023033));
#235867=CARTESIAN_POINT('Ctrl Pts',(-51.0930089302514,-29.6405993642578,
2.69593918853448));
#235868=CARTESIAN_POINT('Ctrl Pts',(-51.0937712117412,-29.6445110377126,
2.69836306235454));
#235869=CARTESIAN_POINT('Ctrl Pts',(-51.094938211443,-29.6504995364713,
2.70207384382187));
#235870=CARTESIAN_POINT('Ctrl Pts',(-51.0963926103114,-29.6563348640822,
2.70594760814187));
#235871=CARTESIAN_POINT('Ctrl Pts',(-51.0980990280588,-29.6619874481817,
2.70995196345666));
#235872=CARTESIAN_POINT('Ctrl Pts',(-51.0988914972886,-29.66461253748,2.71181160678064));
#235873=CARTESIAN_POINT('Ctrl Pts',(-51.0997380650831,-29.6671982043428,
2.71369962772058));
#235874=CARTESIAN_POINT('Ctrl Pts',(-51.1006362623626,-29.6697408831278,
2.7156118313862));
#235875=CARTESIAN_POINT('Ctrl Pts',(-51.100705105645,-29.669935769438,2.71575839426271));
#235876=CARTESIAN_POINT('Ctrl Pts',(-51.1007742270248,-29.6701304259133,
2.71590508903168));
#235877=CARTESIAN_POINT('Ctrl Pts',(-51.1008436251322,-29.670324852047,
2.71605191409871));
#235878=CARTESIAN_POINT('Ctrl Pts',(-51.1018184593122,-29.6730559530502,
2.71811436362713));
#235879=CARTESIAN_POINT('Ctrl Pts',(-51.1028499068176,-29.675741029822,
2.72020091026919));
#235880=CARTESIAN_POINT('Ctrl Pts',(-51.1039327914265,-29.678377681577,
2.72230624862142));
#235881=CARTESIAN_POINT('Ctrl Pts',(-51.1078158230492,-29.6878322458573,
2.72985561753005));
#235882=CARTESIAN_POINT('Ctrl Pts',(-51.1123884412293,-29.6967379921816,
2.7377008991417));
#235883=CARTESIAN_POINT('Ctrl Pts',(-51.1175230541879,-29.7051147523657,
2.74574823346848));
#235884=CARTESIAN_POINT('Ctrl Pts',(-51.1231654780116,-29.7143199702877,
2.75459144546698));
#235885=CARTESIAN_POINT('Ctrl Pts',(-51.1294867578937,-29.7228870317466,
2.76367911753838));
#235886=CARTESIAN_POINT('Ctrl Pts',(-51.1363687775741,-29.7308286942717,
2.77292162564186));
#235887=CARTESIAN_POINT('Ctrl Pts',(-51.1437996316773,-29.739403696713,
2.78290121484013));
#235888=CARTESIAN_POINT('Ctrl Pts',(-51.1518848589938,-29.7472505498604,
2.79306229499288));
#235889=CARTESIAN_POINT('Ctrl Pts',(-51.1605258584163,-29.7543572078866,
2.80331916684171));
#235890=CARTESIAN_POINT('Ctrl Pts',(-51.1690943687365,-29.7614042483575,
2.81348999407958));
#235891=CARTESIAN_POINT('Ctrl Pts',(-51.1782106315408,-29.7677241373251,
2.82375635966496));
#235892=CARTESIAN_POINT('Ctrl Pts',(-51.1878102687782,-29.7732664904682,
2.8340419886024));
#235893=CARTESIAN_POINT('Origin',(-0.00761999999998962,0.0131982271538671,
2.83404198860262));
#235894=CARTESIAN_POINT('Ctrl Pts',(-54.4342359163061,-31.4100231232064,
2.65878198860239));
#235895=CARTESIAN_POINT('Ctrl Pts',(-54.4385272722018,-31.4025830926782,
2.65878198860239));
#235896=CARTESIAN_POINT('Ctrl Pts',(-54.4421589890632,-31.3948506994807,
2.65944603041817));
#235897=CARTESIAN_POINT('Ctrl Pts',(-54.4451438299607,-31.386976274771,
2.66070439264018));
#235898=CARTESIAN_POINT('Ctrl Pts',(-54.4470510012003,-31.3819448922451,
2.66150842619546));
#235899=CARTESIAN_POINT('Ctrl Pts',(-54.4486949601297,-31.3768558346356,
2.66255428265328));
#235900=CARTESIAN_POINT('Ctrl Pts',(-54.4500875286678,-31.3717496422766,
2.66381699700629));
#235901=CARTESIAN_POINT('Ctrl Pts',(-54.4519881053011,-31.3647807142731,
2.66554034873229));
#235902=CARTESIAN_POINT('Ctrl Pts',(-54.4534143418201,-31.3577796218685,
2.66766759643933));
#235903=CARTESIAN_POINT('Ctrl Pts',(-54.4543880442394,-31.3508395087087,
2.67012012783109));
#235904=CARTESIAN_POINT('Ctrl Pts',(-54.454874895449,-31.3473694521289,
2.67134639352697));
#235905=CARTESIAN_POINT('Ctrl Pts',(-54.4552487192092,-31.3439144604656,
2.67265375584973));
#235906=CARTESIAN_POINT('Ctrl Pts',(-54.4555129946223,-31.3404848880616,
2.67403135126901));
#235907=CARTESIAN_POINT('Ctrl Pts',(-54.4556451323288,-31.3387701018596,
2.67472014897865));
#235908=CARTESIAN_POINT('Ctrl Pts',(-54.4557498916994,-31.337061655417,
2.67542649668594));
#235909=CARTESIAN_POINT('Ctrl Pts',(-54.4558277627244,-31.3353607484814,
2.67614899656063));
#235910=CARTESIAN_POINT('Ctrl Pts',(-54.4558472304807,-31.3349355217476,
2.67632962152931));
#235911=CARTESIAN_POINT('Ctrl Pts',(-54.4558650179026,-31.3345107659126,
2.67651125590912));
#235912=CARTESIAN_POINT('Ctrl Pts',(-54.4558811330247,-31.3340864990772,
2.67669387767485));
#235913=CARTESIAN_POINT('Ctrl Pts',(-54.4559294783909,-31.3328136985709,
2.67724174297205));
#235914=CARTESIAN_POINT('Ctrl Pts',(-54.4559627721156,-31.3315453006542,
2.67779849504709));
#235915=CARTESIAN_POINT('Ctrl Pts',(-54.4559812395335,-31.3302817797847,
2.6783635361797));
#235916=CARTESIAN_POINT('Ctrl Pts',(-54.4561088608494,-31.3215500666183,
2.68226832098864));
#235917=CARTESIAN_POINT('Ctrl Pts',(-54.4555742713436,-31.3130195924492,
2.68659153751341));
#235918=CARTESIAN_POINT('Ctrl Pts',(-54.4544853519656,-31.3047400858598,
2.69123699486121));
#235919=CARTESIAN_POINT('Ctrl Pts',(-54.4539441620237,-31.3006251938114,
2.69354577441165));
#235920=CARTESIAN_POINT('Ctrl Pts',(-54.4532655373257,-31.2965719591989,
2.69593478828072));
#235921=CARTESIAN_POINT('Ctrl Pts',(-54.4524598885392,-31.2925850928566,
2.6983956526118));
#235922=CARTESIAN_POINT('Ctrl Pts',(-54.4506825069816,-31.2837894702122,
2.70382468689006));
#235923=CARTESIAN_POINT('Ctrl Pts',(-54.4482992497263,-31.2753153512349,
2.70961155815047));
#235924=CARTESIAN_POINT('Ctrl Pts',(-54.4454010706195,-31.2672761140353,
2.71562701361727));
#235925=CARTESIAN_POINT('Ctrl Pts',(-54.4443423292438,-31.2643392793062,
2.71782453535817));
#235926=CARTESIAN_POINT('Ctrl Pts',(-54.4432206434041,-31.2614550023641,
2.72005051502361));
#235927=CARTESIAN_POINT('Ctrl Pts',(-54.4420411592045,-31.2586246102248,
2.72229986760075));
#235928=CARTESIAN_POINT('Ctrl Pts',(-54.4380793965871,-31.2491176225315,
2.72985520488836));
#235929=CARTESIAN_POINT('Ctrl Pts',(-54.4334326446226,-31.2401615453393,
2.73770845534488));
#235930=CARTESIAN_POINT('Ctrl Pts',(-54.4282277812587,-31.2317373058268,
2.74576706701668));
#235931=CARTESIAN_POINT('Ctrl Pts',(-54.4225070198651,-31.2224780686857,
2.7546244358493));
#235932=CARTESIAN_POINT('Ctrl Pts',(-54.4161118092701,-31.2138606686948,
2.76373036323069));
#235933=CARTESIAN_POINT('Ctrl Pts',(-54.4091594014079,-31.205873742907,
2.77299664636691));
#235934=CARTESIAN_POINT('Ctrl Pts',(-54.4016713602533,-31.1972714816211,
2.7829768303333));
#235935=CARTESIAN_POINT('Ctrl Pts',(-54.3935362880549,-31.1893995936771,
2.79314401478729));
#235936=CARTESIAN_POINT('Ctrl Pts',(-54.3848513315118,-31.1822725865933,
2.80341452427751));
#235937=CARTESIAN_POINT('Ctrl Pts',(-54.3762836512059,-31.1752418181688,
2.81354634721231));
#235938=CARTESIAN_POINT('Ctrl Pts',(-54.3671795569341,-31.1689352997158,
2.82378004209125));
#235939=CARTESIAN_POINT('Ctrl Pts',(-54.3576020372436,-31.1634057161443,
2.83404198860239));
#235940=CARTESIAN_POINT('Ctrl Pts',(-51.3783102687782,-29.4433108116264,
2.8340419886024));
#235941=CARTESIAN_POINT('Ctrl Pts',(-51.3691445298591,-29.4380189697941,
2.82422126443045));
#235942=CARTESIAN_POINT('Ctrl Pts',(-51.3595943606117,-29.4334690915859,
2.814428150286));
#235943=CARTESIAN_POINT('Ctrl Pts',(-51.3497152868776,-29.4296781246256,
2.80471618166476));
#235944=CARTESIAN_POINT('Ctrl Pts',(-51.3401761719881,-29.4260176124814,
2.79533842146423));
#235945=CARTESIAN_POINT('Ctrl Pts',(-51.330329192493,-29.4230642997984,
2.78603515650469));
#235946=CARTESIAN_POINT('Ctrl Pts',(-51.3202058500907,-29.420875403859,
2.77685887347017));
#235947=CARTESIAN_POINT('Ctrl Pts',(-51.3106361210858,-29.4188062116765,
2.76818441216856));
#235948=CARTESIAN_POINT('Ctrl Pts',(-51.3008185461805,-29.4174199248366,
2.75962261521919));
#235949=CARTESIAN_POINT('Ctrl Pts',(-51.2907775289365,-29.4168067767636,
2.75123537701968));
#235950=CARTESIAN_POINT('Ctrl Pts',(-51.2815299205054,-29.4162420776746,
2.74351087134432));
#235951=CARTESIAN_POINT('Ctrl Pts',(-51.2720922400956,-29.4163331870166,
2.73593399450163));
#235952=CARTESIAN_POINT('Ctrl Pts',(-51.2624911797759,-29.4171879526242,
2.72857657812894));
#235953=CARTESIAN_POINT('Ctrl Pts',(-51.2596283373979,-29.4174428264738,
2.72638274508521));
#235954=CARTESIAN_POINT('Ctrl Pts',(-51.256751052488,-29.4177658668978,
2.72420861709681));
#235955=CARTESIAN_POINT('Ctrl Pts',(-51.2538602864392,-29.4181606517644,
2.72205663736687));
#235956=CARTESIAN_POINT('Ctrl Pts',(-51.2509990568964,-29.4185514029024,
2.71992664556726));
#235957=CARTESIAN_POINT('Ctrl Pts',(-51.2481275521816,-29.4190117629203,
2.71782089927845));
#235958=CARTESIAN_POINT('Ctrl Pts',(-51.2452499391937,-29.4195444402101,
2.71574387311206));
#235959=CARTESIAN_POINT('Ctrl Pts',(-51.2450498356143,-29.4195814815471,
2.71559944077446));
#235960=CARTESIAN_POINT('Ctrl Pts',(-51.2448496951981,-29.4196188630963,
2.71545515216028));
#235961=CARTESIAN_POINT('Ctrl Pts',(-51.244649518404,-29.4196565860788,
2.71531100781689));
#235962=CARTESIAN_POINT('Ctrl Pts',(-51.2358730344469,-29.4213104998203,
2.70899119176044));
#235963=CARTESIAN_POINT('Ctrl Pts',(-51.2270453415807,-29.4236619033165,
2.70298296066801));
#235964=CARTESIAN_POINT('Ctrl Pts',(-51.2182691329813,-29.426765124801,
2.697367277741));
#235965=CARTESIAN_POINT('Ctrl Pts',(-51.2100881812719,-29.4296578665607,
2.69213248525393));
#235966=CARTESIAN_POINT('Ctrl Pts',(-51.2019513265391,-29.433204408028,
2.68723866185434));
#235967=CARTESIAN_POINT('Ctrl Pts',(-51.1939656059618,-29.43746586048,2.68278595829528));
#235968=CARTESIAN_POINT('Ctrl Pts',(-51.1910443260614,-29.4390247549184,
2.68115710172768));
#235969=CARTESIAN_POINT('Ctrl Pts',(-51.188143558922,-29.4406794572088,
2.6795876363777));
#235970=CARTESIAN_POINT('Ctrl Pts',(-51.1852696776791,-29.4424334077169,
2.67808378645323));
#235971=CARTESIAN_POINT('Ctrl Pts',(-51.1845786052481,-29.4428551742199,
2.67772216078558));
#235972=CARTESIAN_POINT('Ctrl Pts',(-51.1838888551093,-29.443283215379,
2.67736403603521));
#235973=CARTESIAN_POINT('Ctrl Pts',(-51.1832005624686,-29.4437175198435,
2.67700956934437));
#235974=CARTESIAN_POINT('Ctrl Pts',(-51.1825337789729,-29.4441382522935,
2.67666617973762));
#235975=CARTESIAN_POINT('Ctrl Pts',(-51.181868363317,-29.4445648626868,
2.67632622314077));
#235976=CARTESIAN_POINT('Ctrl Pts',(-51.1812044402991,-29.4449973374098,
2.67598984158731));
#235977=CARTESIAN_POINT('Ctrl Pts',(-51.1739303963593,-29.4497355978005,
2.67230439292177));
#235978=CARTESIAN_POINT('Ctrl Pts',(-51.1668309650356,-29.4551812510955,
2.6690496453993));
#235979=CARTESIAN_POINT('Ctrl Pts',(-51.160090071181,-29.461292997452,2.6664020356668));
#235980=CARTESIAN_POINT('Ctrl Pts',(-51.1572944215751,-29.4638277208377,
2.66530399299396));
#235981=CARTESIAN_POINT('Ctrl Pts',(-51.1545603804836,-29.4664765899956,
2.66430995142216));
#235982=CARTESIAN_POINT('Ctrl Pts',(-51.1519003687088,-29.4692349685474,
2.66343053473318));
#235983=CARTESIAN_POINT('Ctrl Pts',(-51.1473634414339,-29.4739396706108,
2.66193059792842));
#235984=CARTESIAN_POINT('Ctrl Pts',(-51.1430443628982,-29.4789629373384,
2.66076519817084));
#235985=CARTESIAN_POINT('Ctrl Pts',(-51.1390107214362,-29.4842777732941,
2.65997805604417));
#235986=CARTESIAN_POINT('Ctrl Pts',(-51.1369939007052,-29.486935191272,
2.65958448498083));
#235987=CARTESIAN_POINT('Ctrl Pts',(-51.1350496570623,-29.4896662827383,
2.65928526260719));
#235988=CARTESIAN_POINT('Ctrl Pts',(-51.1331865036874,-29.4924676612912,
2.65908463971281));
#235989=CARTESIAN_POINT('Ctrl Pts',(-51.1313233503126,-29.495269039844,
2.65888401681843));
#235990=CARTESIAN_POINT('Ctrl Pts',(-51.1295412933643,-29.49814066024,2.65878198860241));
#235991=CARTESIAN_POINT('Ctrl Pts',(-51.1278468659044,-29.5010785149114,
2.65878198860241));
#235992=CARTESIAN_POINT('Origin',(-47.1274239660506,-34.2589154226524,2.83404198860237));
#235993=CARTESIAN_POINT('Ctrl Pts',(-50.5784163149354,-36.9828414016749,
2.83404198860235));
#235994=CARTESIAN_POINT('Ctrl Pts',(-50.5870002518359,-36.9890779968908,
2.82419652440062));
#235995=CARTESIAN_POINT('Ctrl Pts',(-50.5960508067993,-36.9946187858197,
2.81438790575672));
#235996=CARTESIAN_POINT('Ctrl Pts',(-50.6055128591412,-36.9994424783901,
2.80466781256952));
#235997=CARTESIAN_POINT('Ctrl Pts',(-50.6146674511248,-37.0041094296751,
2.7952635645315));
#235998=CARTESIAN_POINT('Ctrl Pts',(-50.6242084112798,-37.0081056536702,
2.78594102496327));
#235999=CARTESIAN_POINT('Ctrl Pts',(-50.6341096134618,-37.011372274199,
2.77675109088895));
#236000=CARTESIAN_POINT('Ctrl Pts',(-50.643475541045,-37.0144622960723,
2.7680579791382));
#236001=CARTESIAN_POINT('Ctrl Pts',(-50.653164692761,-37.016899762676,2.7594827121032));
#236002=CARTESIAN_POINT('Ctrl Pts',(-50.6631621581214,-37.0185933530506,
2.75108575573402));
#236003=CARTESIAN_POINT('Ctrl Pts',(-50.6723705467533,-37.0201532722692,
2.74335155163468));
#236004=CARTESIAN_POINT('Ctrl Pts',(-50.6818410607698,-37.021082144611,
2.73576818686159));
#236005=CARTESIAN_POINT('Ctrl Pts',(-50.6915586678615,-37.0212705108776,
2.7284062616073));
#236006=CARTESIAN_POINT('Ctrl Pts',(-50.6943773762856,-37.0213251487712,
2.72627084693823));
#236007=CARTESIAN_POINT('Ctrl Pts',(-50.6972168227812,-37.0213172191968,
2.72415424587578));
#236008=CARTESIAN_POINT('Ctrl Pts',(-50.7000764815583,-37.0212433695026,
2.72205867173228));
#236009=CARTESIAN_POINT('Ctrl Pts',(-50.703176535531,-37.021163311686,2.71978693462832));
#236010=CARTESIAN_POINT('Ctrl Pts',(-50.7062960577319,-37.0210069737843,
2.71754411340733));
#236011=CARTESIAN_POINT('Ctrl Pts',(-50.7094335311101,-37.0207706534748,
2.71533341844231));
#236012=CARTESIAN_POINT('Ctrl Pts',(-50.7180443514157,-37.0201220705311,
2.70926614876378));
#236013=CARTESIAN_POINT('Ctrl Pts',(-50.726776150217,-37.0188289150183,
2.70347381860395));
#236014=CARTESIAN_POINT('Ctrl Pts',(-50.7355328079487,-37.0168522507833,
2.69804914171382));
#236015=CARTESIAN_POINT('Ctrl Pts',(-50.7435446743631,-37.0150437103239,
2.69308585687193));
#236016=CARTESIAN_POINT('Ctrl Pts',(-50.7515681793717,-37.012655929615,
2.68842799053176));
#236017=CARTESIAN_POINT('Ctrl Pts',(-50.7595400218646,-37.0096268558217,
2.68414767054209));
#236018=CARTESIAN_POINT('Ctrl Pts',(-50.763455764856,-37.0081389846694,
2.68204519134543));
#236019=CARTESIAN_POINT('Ctrl Pts',(-50.7673587034236,-37.006496006056,
2.68003431778493));
#236020=CARTESIAN_POINT('Ctrl Pts',(-50.7712388062147,-37.0046883717069,
2.67812693945242));
#236021=CARTESIAN_POINT('Ctrl Pts',(-50.7719750179266,-37.0043453906957,
2.67776503299194));
#236022=CARTESIAN_POINT('Ctrl Pts',(-50.7727105984661,-37.0039959853417,
2.67740659639915));
#236023=CARTESIAN_POINT('Ctrl Pts',(-50.7734454079406,-37.0036401497476,
2.67705178968846));
#236024=CARTESIAN_POINT('Ctrl Pts',(-50.7741572546191,-37.0032954340158,
2.67670807068748));
#236025=CARTESIAN_POINT('Ctrl Pts',(-50.7748683776569,-37.0029446836755,
2.67636775825256));
#236026=CARTESIAN_POINT('Ctrl Pts',(-50.7755786476299,-37.0025878964871,
2.67603099699246));
#236027=CARTESIAN_POINT('Ctrl Pts',(-50.7833190234414,-36.9986997032254,
2.6723610421711));
#236028=CARTESIAN_POINT('Ctrl Pts',(-50.7909629993144,-36.9940916451525,
2.66911440541448));
#236029=CARTESIAN_POINT('Ctrl Pts',(-50.7983209798301,-36.9887818345679,
2.666467781896));
#236030=CARTESIAN_POINT('Ctrl Pts',(-50.8014283006924,-36.986539468586,
2.66535009634952));
#236031=CARTESIAN_POINT('Ctrl Pts',(-50.8044846273289,-36.9841723869923,
2.66433897912328));
#236032=CARTESIAN_POINT('Ctrl Pts',(-50.8074762285637,-36.9816838130236,
2.66344564884782));
#236033=CARTESIAN_POINT('Ctrl Pts',(-50.8125140102916,-36.9774931166427,
2.66194130298574));
#236034=CARTESIAN_POINT('Ctrl Pts',(-50.81736572735,-36.9729576356983,2.66077206705408));
#236035=CARTESIAN_POINT('Ctrl Pts',(-50.8219595855748,-36.9680961762157,
2.65998225155702));
#236036=CARTESIAN_POINT('Ctrl Pts',(-50.823108050131,-36.966880811345,2.65978479768275));
#236037=CARTESIAN_POINT('Ctrl Pts',(-50.8242402182961,-36.9656449236012,
2.65961098966609));
#236038=CARTESIAN_POINT('Ctrl Pts',(-50.8253547230709,-36.9643886196684,
2.65946139030488));
#236039=CARTESIAN_POINT('Ctrl Pts',(-50.8270264802332,-36.9625041637692,
2.65923699126307));
#236040=CARTESIAN_POINT('Ctrl Pts',(-50.8286584747053,-36.9605737761779,
2.65906707562428));
#236041=CARTESIAN_POINT('Ctrl Pts',(-50.8302474395911,-36.9585988181539,
2.65895332562906));
#236042=CARTESIAN_POINT('Ctrl Pts',(-50.831836404477,-36.95662386013,2.65883957563384));
#236043=CARTESIAN_POINT('Ctrl Pts',(-50.8333823430133,-36.9546043428184,
2.65878198860235));
#236044=CARTESIAN_POINT('Ctrl Pts',(-50.8348823336483,-36.9525415975215,
2.65878198860235));
#236045=CARTESIAN_POINT('Ctrl Pts',(-47.7461450747862,-34.7084426211234,
2.65878198860237));
#236046=CARTESIAN_POINT('Ctrl Pts',(-47.7410693801616,-34.7154221779229,
2.65878198860237));
#236047=CARTESIAN_POINT('Ctrl Pts',(-47.7366138137626,-34.7227602152543,
2.65945335517834));
#236048=CARTESIAN_POINT('Ctrl Pts',(-47.7327846251241,-34.730305751405,
2.66072561226586));
#236049=CARTESIAN_POINT('Ctrl Pts',(-47.7303113621613,-34.7351793935413,
2.66154735980324));
#236050=CARTESIAN_POINT('Ctrl Pts',(-47.7280985748133,-34.7401391868073,
2.66261895766866));
#236051=CARTESIAN_POINT('Ctrl Pts',(-47.7261394006516,-34.7451421370596,
2.66391429251006));
#236052=CARTESIAN_POINT('Ctrl Pts',(-47.7235426275286,-34.7517732610326,
2.66563118464103));
#236053=CARTESIAN_POINT('Ctrl Pts',(-47.7213971161177,-34.7584811778434,
2.66774105138679));
#236054=CARTESIAN_POINT('Ctrl Pts',(-47.7196932909343,-34.7651763312118,
2.67016894181729));
#236055=CARTESIAN_POINT('Ctrl Pts',(-47.7188413783425,-34.768523907896,
2.67138288703255));
#236056=CARTESIAN_POINT('Ctrl Pts',(-47.7180997687559,-34.7718684539193,
2.67267613167531));
#236057=CARTESIAN_POINT('Ctrl Pts',(-47.7174664279767,-34.7751999143434,
2.67403835432532));
#236058=CARTESIAN_POINT('Ctrl Pts',(-47.7171497575871,-34.7768656445554,
2.67471946565033));
#236059=CARTESIAN_POINT('Ctrl Pts',(-47.7168601447018,-34.7785281166319,
2.67541781389502));
#236060=CARTESIAN_POINT('Ctrl Pts',(-47.7165972740595,-34.7801861569091,
2.67613207244148));
#236061=CARTESIAN_POINT('Ctrl Pts',(-47.7165315563989,-34.7806006669784,
2.67631063707809));
#236062=CARTESIAN_POINT('Ctrl Pts',(-47.7164675099215,-34.7810149003418,
2.67649019601824));
#236063=CARTESIAN_POINT('Ctrl Pts',(-47.7164051292831,-34.7814288392283,
2.67667072836636));
#236064=CARTESIAN_POINT('Ctrl Pts',(-47.7162179873682,-34.7826706558876,
2.67721232541069));
#236065=CARTESIAN_POINT('Ctrl Pts',(-47.7160458390452,-34.783909820854,
2.67776268340026));
#236066=CARTESIAN_POINT('Ctrl Pts',(-47.7158885307486,-34.7851458668348,
2.67832123541495));
#236067=CARTESIAN_POINT('Ctrl Pts',(-47.7147804714197,-34.7938524151211,
2.68225560368418));
#236068=CARTESIAN_POINT('Ctrl Pts',(-47.7143609747536,-34.8024290252883,
2.68661792998856));
#236069=CARTESIAN_POINT('Ctrl Pts',(-47.7145286167444,-34.8108122146617,
2.69130986622539));
#236070=CARTESIAN_POINT('Ctrl Pts',(-47.7146099229288,-34.814878052449,
2.69358545023021));
#236071=CARTESIAN_POINT('Ctrl Pts',(-47.7148297795037,-34.8188987667929,
2.69593918853441));
#236072=CARTESIAN_POINT('Ctrl Pts',(-47.7151790039207,-34.8228686918041,
2.69836306235452));
#236073=CARTESIAN_POINT('Ctrl Pts',(-47.7157136421035,-34.8289463696254,
2.70207384382184));
#236074=CARTESIAN_POINT('Ctrl Pts',(-47.7165501157949,-34.8349017567798,
2.70594760814185));
#236075=CARTESIAN_POINT('Ctrl Pts',(-47.7176563296779,-34.8407017446569,
2.70995196345664));
#236076=CARTESIAN_POINT('Ctrl Pts',(-47.718170061128,-34.8433952890322,
2.71181160678062));
#236077=CARTESIAN_POINT('Ctrl Pts',(-47.7187417155519,-34.846055281772,
2.71369962772054));
#236078=CARTESIAN_POINT('Ctrl Pts',(-47.7193692101068,-34.8486779186779,
2.71561183138616));
#236079=CARTESIAN_POINT('Ctrl Pts',(-47.719417305092,-34.848878933463,2.71575839426267));
#236080=CARTESIAN_POINT('Ctrl Pts',(-47.7194657006753,-34.8490797487414,
2.71590508903165));
#236081=CARTESIAN_POINT('Ctrl Pts',(-47.7195143955476,-34.8492803638659,
2.71605191409867));
#236082=CARTESIAN_POINT('Ctrl Pts',(-47.7201984116931,-34.8520984015308,
2.71811436362709));
#236083=CARTESIAN_POINT('Ctrl Pts',(-47.7209435418724,-34.8548765847938,
2.72020091026915));
#236084=CARTESIAN_POINT('Ctrl Pts',(-47.72174488917,-34.8576119849587,2.72230624862138));
#236085=CARTESIAN_POINT('Ctrl Pts',(-47.7246183780643,-34.8674206434752,
2.72985561753025));
#236086=CARTESIAN_POINT('Ctrl Pts',(-47.7282350429861,-34.8767555719411,
2.73770089914216));
#236087=CARTESIAN_POINT('Ctrl Pts',(-47.7324659181287,-34.8856231565588,
2.74574823346921));
#236088=CARTESIAN_POINT('Ctrl Pts',(-47.7371152248811,-34.8953677412255,
2.75459144546802));
#236089=CARTESIAN_POINT('Ctrl Pts',(-47.7425063743617,-34.9045486250976,
2.76367911753973));
#236090=CARTESIAN_POINT('Ctrl Pts',(-47.7485205638389,-34.913166149306,
2.77292162564353));
#236091=CARTESIAN_POINT('Ctrl Pts',(-47.7550143791185,-34.9224709127472,
2.78290121484226));
#236092=CARTESIAN_POINT('Ctrl Pts',(-47.7622350952133,-34.9311199163988,
2.79306229499547));
#236093=CARTESIAN_POINT('Ctrl Pts',(-47.7700859102949,-34.9390908737997,
2.80331916684477));
#236094=CARTESIAN_POINT('Ctrl Pts',(-47.7778708651073,-34.9469949630609,
2.81348999408162));
#236095=CARTESIAN_POINT('Ctrl Pts',(-47.7862765797875,-34.9542331399563,
2.82375635966596));
#236096=CARTESIAN_POINT('Ctrl Pts',(-47.7952442955499,-34.9607485668368,
2.83404198860237));
#236097=CARTESIAN_POINT('Origin',(-0.00895784724492722,0.0123294189944669,
2.83404198860262));
#236098=CARTESIAN_POINT('Ctrl Pts',(-50.8527980281382,-36.9278827595329,
2.65878198860235));
#236099=CARTESIAN_POINT('Ctrl Pts',(-50.8578435704952,-36.9209320551073,
2.65878198860235));
#236100=CARTESIAN_POINT('Ctrl Pts',(-50.8622636476101,-36.9136216385511,
2.65944603041817));
#236101=CARTESIAN_POINT('Ctrl Pts',(-50.866055238751,-36.9061023515958,
2.66070439264024));
#236102=CARTESIAN_POINT('Ctrl Pts',(-50.8684778849904,-36.9012978851888,
2.66150842619551));
#236103=CARTESIAN_POINT('Ctrl Pts',(-50.870644789512,-36.8964085464702,
2.66255428265329));
#236104=CARTESIAN_POINT('Ctrl Pts',(-50.8725634718544,-36.8914758894167,
2.66381699700625));
#236105=CARTESIAN_POINT('Ctrl Pts',(-50.8751820882648,-36.8847438022848,
2.66554034873224));
#236106=CARTESIAN_POINT('Ctrl Pts',(-50.8773323251411,-36.8779301449084,
2.66766759643928));
#236107=CARTESIAN_POINT('Ctrl Pts',(-50.8790261328802,-36.8711298300323,
2.67012012783103));
#236108=CARTESIAN_POINT('Ctrl Pts',(-50.8798730367497,-36.8677296725943,
2.67134639352691));
#236109=CARTESIAN_POINT('Ctrl Pts',(-50.8806059576334,-36.86433268296,2.67265375584968));
#236110=CARTESIAN_POINT('Ctrl Pts',(-50.8812272732512,-36.8609495224153,
2.67403135126895));
#236111=CARTESIAN_POINT('Ctrl Pts',(-50.8815379310601,-36.859257942143,
2.67472014897859));
#236112=CARTESIAN_POINT('Ctrl Pts',(-50.881820697829,-36.8575698050847,
2.67542649668587));
#236113=CARTESIAN_POINT('Ctrl Pts',(-50.8820759354566,-36.8558863556339,
2.67614899656056));
#236114=CARTESIAN_POINT('Ctrl Pts',(-50.8821397448634,-36.8554654932712,
2.67632962152924));
#236115=CARTESIAN_POINT('Ctrl Pts',(-50.8822018339187,-36.8550449235851,
2.67651125590905));
#236116=CARTESIAN_POINT('Ctrl Pts',(-50.8822622087208,-36.8546246654167,
2.67669387767478));
#236117=CARTESIAN_POINT('Ctrl Pts',(-50.882443333127,-36.8533638909116,
2.67724174297199));
#236118=CARTESIAN_POINT('Ctrl Pts',(-50.8826090281503,-36.8521059215534,
2.67779849504702));
#236119=CARTESIAN_POINT('Ctrl Pts',(-50.8827594682965,-36.8508512527541,
2.67836353617963));
#236120=CARTESIAN_POINT('Ctrl Pts',(-50.8837991030485,-36.8421807128858,
2.68226832098869));
#236121=CARTESIAN_POINT('Ctrl Pts',(-50.8841591194358,-36.8336410897271,
2.6865915375136));
#236122=CARTESIAN_POINT('Ctrl Pts',(-50.8839416093724,-36.8252931160716,
2.69123699486157));
#236123=CARTESIAN_POINT('Ctrl Pts',(-50.883833507468,-36.8211441960797,
2.69354577441188));
#236124=CARTESIAN_POINT('Ctrl Pts',(-50.8835822787324,-36.8170422299139,
2.69593478828082));
#236125=CARTESIAN_POINT('Ctrl Pts',(-50.8831977843863,-36.8129929908132,
2.69839565261176));
#236126=CARTESIAN_POINT('Ctrl Pts',(-50.8823495324293,-36.8040597645471,
2.70382468689002));
#236127=CARTESIAN_POINT('Ctrl Pts',(-50.8808651175409,-36.7953829494618,
2.70961155815043));
#236128=CARTESIAN_POINT('Ctrl Pts',(-50.8788231440728,-36.7870848098364,
2.71562701361724));
#236129=CARTESIAN_POINT('Ctrl Pts',(-50.8780771854143,-36.7840533947862,
2.71782453535815));
#236130=CARTESIAN_POINT('Ctrl Pts',(-50.8772631333233,-36.7810676701179,
2.7200505150236));
#236131=CARTESIAN_POINT('Ctrl Pts',(-50.8763859670024,-36.7781294934921,
2.72229986760074));
#236132=CARTESIAN_POINT('Ctrl Pts',(-50.8734396581491,-36.7682604691141,
2.72985520488826));
#236133=CARTESIAN_POINT('Ctrl Pts',(-50.869754526564,-36.7588677364079,
2.73770845534467));
#236134=CARTESIAN_POINT('Ctrl Pts',(-50.8654587487966,-36.749945589392,
2.74576706701634));
#236135=CARTESIAN_POINT('Ctrl Pts',(-50.860737180162,-36.7401390929237,
2.75462443584886));
#236136=CARTESIAN_POINT('Ctrl Pts',(-50.8552777667782,-36.7309004184158,
2.76373036323012));
#236137=CARTESIAN_POINT('Ctrl Pts',(-50.8491983060126,-36.7222305213335,
2.77299664636622));
#236138=CARTESIAN_POINT('Ctrl Pts',(-50.8426504662838,-36.7128926707001,
2.78297683033255));
#236139=CARTESIAN_POINT('Ctrl Pts',(-50.835382795212,-36.7042135591864,
2.79314401478649));
#236140=CARTESIAN_POINT('Ctrl Pts',(-50.8274903908677,-36.6962177694322,
2.80341452427668));
#236141=CARTESIAN_POINT('Ctrl Pts',(-50.8197045606298,-36.6883299498364,
2.81354634721171));
#236142=CARTESIAN_POINT('Ctrl Pts',(-50.8113095502213,-36.6811063421674,
2.82378004209092));
#236143=CARTESIAN_POINT('Ctrl Pts',(-50.8023624960588,-36.674605926818,
2.83404198860235));
#236144=CARTESIAN_POINT('Ctrl Pts',(-48.0191904766733,-34.6525130919799,
2.83404198860237));
#236145=CARTESIAN_POINT('Ctrl Pts',(-48.0106280967249,-34.6462921588064,
2.82422126442958));
#236146=CARTESIAN_POINT('Ctrl Pts',(-48.0016058360802,-34.6407689407913,
2.8144281502843));
#236147=CARTESIAN_POINT('Ctrl Pts',(-47.9921771448955,-34.6359660967484,
2.80471618166224));
#236148=CARTESIAN_POINT('Ctrl Pts',(-47.9830729139841,-34.6313285282523,
2.79533842146122));
#236149=CARTESIAN_POINT('Ctrl Pts',(-47.9735885825087,-34.6273621044907,
2.78603515650119));
#236150=CARTESIAN_POINT('Ctrl Pts',(-47.9637494987635,-34.6241270221279,
2.77685887346622));
#236151=CARTESIAN_POINT('Ctrl Pts',(-47.9544484832141,-34.62106885613,2.76818441216434));
#236152=CARTESIAN_POINT('Ctrl Pts',(-47.9448295964439,-34.6186639474967,
2.75962261521474));
#236153=CARTESIAN_POINT('Ctrl Pts',(-47.9349076763684,-34.6170045862111,
2.75123537701502));
#236154=CARTESIAN_POINT('Ctrl Pts',(-47.9257697544315,-34.6154763423049,
2.74351087133956));
#236155=CARTESIAN_POINT('Ctrl Pts',(-47.9163742511026,-34.6145804463106,
2.73593399449679));
#236156=CARTESIAN_POINT('Ctrl Pts',(-47.9067364390602,-34.614426945342,
2.72857657812405));
#236157=CARTESIAN_POINT('Ctrl Pts',(-47.9038626380626,-34.6143811744519,
2.72638274508197));
#236158=CARTESIAN_POINT('Ctrl Pts',(-47.9009673483035,-34.6144016870566,
2.72420861709519));
#236159=CARTESIAN_POINT('Ctrl Pts',(-47.8980511519203,-34.6144921419176,
2.72205663736682));
#236160=CARTESIAN_POINT('Ctrl Pts',(-47.8951647518764,-34.6145816725528,
2.71992664556721));
#236161=CARTESIAN_POINT('Ctrl Pts',(-47.8922608568396,-34.6147393566953,
2.7178208992784));
#236162=CARTESIAN_POINT('Ctrl Pts',(-47.8893433277782,-34.6149683234597,
2.71574387311201));
#236163=CARTESIAN_POINT('Ctrl Pts',(-47.8891404485131,-34.6149842453607,
2.71559944077442));
#236164=CARTESIAN_POINT('Ctrl Pts',(-47.8889374970512,-34.6150005017597,
2.71545515216025));
#236165=CARTESIAN_POINT('Ctrl Pts',(-47.8887344737211,-34.6150170939191,
2.71531100781686));
#236166=CARTESIAN_POINT('Ctrl Pts',(-47.8798331871996,-34.6157445549671,
2.7089911917604));
#236167=CARTESIAN_POINT('Ctrl Pts',(-47.8708080647646,-34.6171603320595,
2.70298296066797));
#236168=CARTESIAN_POINT('Ctrl Pts',(-47.8617555581812,-34.6193291901737,
2.69736727774096));
#236169=CARTESIAN_POINT('Ctrl Pts',(-47.8533170487304,-34.6213509428812,
2.69213248525385));
#236170=CARTESIAN_POINT('Ctrl Pts',(-47.8448540540096,-34.6240275231022,
2.68723866185421));
#236171=CARTESIAN_POINT('Ctrl Pts',(-47.836466636969,-34.6274308957718,
2.68278595829513));
#236172=CARTESIAN_POINT('Ctrl Pts',(-47.8333984113057,-34.6286758935246,
2.68115710172758));
#236173=CARTESIAN_POINT('Ctrl Pts',(-47.8303405713846,-34.6300183184512,
2.67958763637765));
#236174=CARTESIAN_POINT('Ctrl Pts',(-47.8272990958127,-34.631462258245,
2.67808378645322));
#236175=CARTESIAN_POINT('Ctrl Pts',(-47.8265677225444,-34.6318094775277,
2.67772216078557));
#236176=CARTESIAN_POINT('Ctrl Pts',(-47.8258370084444,-34.6321630753106,
2.6773640360352));
#236177=CARTESIAN_POINT('Ctrl Pts',(-47.8251070891646,-34.6325230544378,
2.67700956934436));
#236178=CARTESIAN_POINT('Ctrl Pts',(-47.8243999798622,-34.6328717842173,
2.67666617973761));
#236179=CARTESIAN_POINT('Ctrl Pts',(-47.823693616494,-34.6332265027181,
2.67632622314076));
#236180=CARTESIAN_POINT('Ctrl Pts',(-47.8229881245977,-34.6335872094466,
2.6759898415873));
#236181=CARTESIAN_POINT('Ctrl Pts',(-47.8152586455542,-34.6375391685165,
2.67230439292162));
#236182=CARTESIAN_POINT('Ctrl Pts',(-47.8076288798874,-34.6422128973069,
2.66904964539903));
#236183=CARTESIAN_POINT('Ctrl Pts',(-47.8002860618999,-34.647586547602,
2.66640203566646));
#236184=CARTESIAN_POINT('Ctrl Pts',(-47.797240776415,-34.6498151605503,
2.66530399299375));
#236185=CARTESIAN_POINT('Ctrl Pts',(-47.7942448304645,-34.6521637338119,
2.66430995142206));
#236186=CARTESIAN_POINT('Ctrl Pts',(-47.7913110614416,-34.654628954734,
2.66343053473316));
#236187=CARTESIAN_POINT('Ctrl Pts',(-47.7863072126523,-34.6588336459112,
2.66193059792839));
#236188=CARTESIAN_POINT('Ctrl Pts',(-47.7814867201291,-34.6633779280161,
2.66076519817082));
#236189=CARTESIAN_POINT('Ctrl Pts',(-47.7769196237422,-34.668242018401,
2.65997805604413));
#236190=CARTESIAN_POINT('Ctrl Pts',(-47.7746360755487,-34.6706740635934,
2.65958448498079));
#236191=CARTESIAN_POINT('Ctrl Pts',(-47.7724170058818,-34.6731869650547,
2.65928526260715));
#236192=CARTESIAN_POINT('Ctrl Pts',(-47.770271235261,-34.6757782448036,
2.65908463971277));
#236193=CARTESIAN_POINT('Ctrl Pts',(-47.7681254646401,-34.6783695245525,
2.65888401681839));
#236194=CARTESIAN_POINT('Ctrl Pts',(-47.7660530039191,-34.6810391382372,
2.65878198860237));
#236195=CARTESIAN_POINT('Ctrl Pts',(-47.764060769276,-34.6837837831348,
2.65878198860237));
#236196=CARTESIAN_POINT('Origin',(-43.2882232241945,-38.9973987043321,2.83404198860233));
#236197=CARTESIAN_POINT('Ctrl Pts',(-46.4355828792667,-42.0671296588098,
2.83404198860232));
#236198=CARTESIAN_POINT('Ctrl Pts',(-46.4434678907489,-42.0742293550377,
2.82419652440029));
#236199=CARTESIAN_POINT('Ctrl Pts',(-46.4518896956734,-42.0806858315472,
2.81438790575613));
#236200=CARTESIAN_POINT('Ctrl Pts',(-46.4607957007311,-42.0864721532157,
2.80466781256868));
#236201=CARTESIAN_POINT('Ctrl Pts',(-46.4694123136561,-42.0920704538853,
2.79526356453048));
#236202=CARTESIAN_POINT('Ctrl Pts',(-46.4784832882803,-42.0970420880504,
2.78594102496209));
#236203=CARTESIAN_POINT('Ctrl Pts',(-46.487988795817,-42.1013257711387,
2.77675109088763));
#236204=CARTESIAN_POINT('Ctrl Pts',(-46.4969804206313,-42.1053778715663,
2.76805797913676));
#236205=CARTESIAN_POINT('Ctrl Pts',(-46.5063617095223,-42.1088147776121,
2.75948271210165));
#236206=CARTESIAN_POINT('Ctrl Pts',(-46.5161273793223,-42.1115441100122,
2.75108575573236));
#236207=CARTESIAN_POINT('Ctrl Pts',(-46.5251222674793,-42.1140580225429,
2.74335155163292));
#236208=CARTESIAN_POINT('Ctrl Pts',(-46.5344438074308,-42.1159717447012,
2.73576818685973));
#236209=CARTESIAN_POINT('Ctrl Pts',(-46.544088490818,-42.1171748456135,
2.72840626160534));
#236210=CARTESIAN_POINT('Ctrl Pts',(-46.5468860468465,-42.1175238194549,
2.72627084693694));
#236211=CARTESIAN_POINT('Ctrl Pts',(-46.5497107674225,-42.1178127362981,
2.72415424587514));
#236212=CARTESIAN_POINT('Ctrl Pts',(-46.5525624800838,-42.1180382068977,
2.72205867173227));
#236213=CARTESIAN_POINT('Ctrl Pts',(-46.5556539199571,-42.118282631524,
2.7197869346283));
#236214=CARTESIAN_POINT('Ctrl Pts',(-46.5587726948496,-42.1184532289194,
2.7175441134073));
#236215=CARTESIAN_POINT('Ctrl Pts',(-46.5619176830191,-42.1185461584681,
2.71533341844227));
#236216=CARTESIAN_POINT('Ctrl Pts',(-46.5705491277285,-42.1188012043436,
2.70926614876374));
#236217=CARTESIAN_POINT('Ctrl Pts',(-46.5793682643808,-42.1184278543823,
2.70347381860392));
#236218=CARTESIAN_POINT('Ctrl Pts',(-46.5882835699001,-42.1173773384969,
2.69804914171379));
#236219=CARTESIAN_POINT('Ctrl Pts',(-46.596440590427,-42.1164161734956,
2.69308585687187));
#236220=CARTESIAN_POINT('Ctrl Pts',(-46.6046697328839,-42.1148801579478,
2.68842799053166));
#236221=CARTESIAN_POINT('Ctrl Pts',(-46.6129145292183,-42.1127009621828,
2.68414767054197));
#236222=CARTESIAN_POINT('Ctrl Pts',(-46.6169643462449,-42.1116305483418,
2.68204519134533));
#236223=CARTESIAN_POINT('Ctrl Pts',(-46.6210176421363,-42.1104045383079,
2.68003431778485));
#236224=CARTESIAN_POINT('Ctrl Pts',(-46.6250654385589,-42.109012387551,
2.67812693945236));
#236225=CARTESIAN_POINT('Ctrl Pts',(-46.6258334685041,-42.1087482405045,
2.67776503299188));
#236226=CARTESIAN_POINT('Ctrl Pts',(-46.6266015422611,-42.1084776383329,
2.67740659639909));
#236227=CARTESIAN_POINT('Ctrl Pts',(-46.6273695213203,-42.1082005605487,
2.6770517896884));
#236228=CARTESIAN_POINT('Ctrl Pts',(-46.6281135010339,-42.1079321414451,
2.67670807068742));
#236229=CARTESIAN_POINT('Ctrl Pts',(-46.6288573918593,-42.1076576451502,
2.6763677582525));
#236230=CARTESIAN_POINT('Ctrl Pts',(-46.6296010653156,-42.1073770559081,
2.6760309969924));
#236231=CARTESIAN_POINT('Ctrl Pts',(-46.637705465405,-42.1043192521647,
2.67236104217107));
#236232=CARTESIAN_POINT('Ctrl Pts',(-46.6457892400072,-42.1005354505673,
2.66911440541448));
#236233=CARTESIAN_POINT('Ctrl Pts',(-46.6536619390764,-42.0960238460769,
2.66646778189602));
#236234=CARTESIAN_POINT('Ctrl Pts',(-46.6569866287802,-42.0941185674849,
2.6653500963495));
#236235=CARTESIAN_POINT('Ctrl Pts',(-46.660273639941,-42.0920839261384,
2.66433897912325));
#236236=CARTESIAN_POINT('Ctrl Pts',(-46.663508979684,-42.089921692318,2.66344564884777));
#236237=CARTESIAN_POINT('Ctrl Pts',(-46.6689572109692,-42.0862805445927,
2.66194130298569));
#236238=CARTESIAN_POINT('Ctrl Pts',(-46.6742564366672,-42.0822770520158,
2.66077206705403));
#236239=CARTESIAN_POINT('Ctrl Pts',(-46.6793332901452,-42.0779224130578,
2.65998225155697));
#236240=CARTESIAN_POINT('Ctrl Pts',(-46.6806025035146,-42.0768337533183,
2.65978479768271));
#236241=CARTESIAN_POINT('Ctrl Pts',(-46.6818576549907,-42.0757229796953,
2.65961098966605));
#236242=CARTESIAN_POINT('Ctrl Pts',(-46.6830973739112,-42.0745900553982,
2.65946139030484));
#236243=CARTESIAN_POINT('Ctrl Pts',(-46.684956952292,-42.0728906689527,
2.65923699126303));
#236244=CARTESIAN_POINT('Ctrl Pts',(-46.6867817869761,-42.0711414461008,
2.65906707562424));
#236245=CARTESIAN_POINT('Ctrl Pts',(-46.6885684866732,-42.0693433991612,
2.65895332562902));
#236246=CARTESIAN_POINT('Ctrl Pts',(-46.6903551863704,-42.0675453522217,
2.6588395756338));
#236247=CARTESIAN_POINT('Ctrl Pts',(-46.6921037531347,-42.0656984926166,
2.65878198860231));
#236248=CARTESIAN_POINT('Ctrl Pts',(-46.6938111422601,-42.0638038389702,
2.65878198860231));
#236249=CARTESIAN_POINT('Ctrl Pts',(-43.8565665267053,-39.5091373124624,
2.65878198860234));
#236250=CARTESIAN_POINT('Ctrl Pts',(-43.8507890749206,-39.5155480799602,
2.65878198860234));
#236251=CARTESIAN_POINT('Ctrl Pts',(-43.845590882815,-39.5223801852464,
2.65945335517826));
#236252=CARTESIAN_POINT('Ctrl Pts',(-43.8409939475743,-39.5294841269563,
2.6607256122657));
#236253=CARTESIAN_POINT('Ctrl Pts',(-43.8380247990816,-39.5340725443945,
2.66154735980308));
#236254=CARTESIAN_POINT('Ctrl Pts',(-43.8353056940458,-39.5387738681332,
2.66261895766853));
#236255=CARTESIAN_POINT('Ctrl Pts',(-43.8328343017434,-39.5435446222364,
2.66391429250998));
#236256=CARTESIAN_POINT('Ctrl Pts',(-43.8295586128166,-39.5498679835145,
2.66563118464094));
#236257=CARTESIAN_POINT('Ctrl Pts',(-43.8267236865058,-39.5563148866444,
2.6677410513867));
#236258=CARTESIAN_POINT('Ctrl Pts',(-43.824329360962,-39.5627952650341,
2.67016894181721));
#236259=CARTESIAN_POINT('Ctrl Pts',(-43.8231321981901,-39.5660354542289,
2.67138288703246));
#236260=CARTESIAN_POINT('Ctrl Pts',(-43.8220450509623,-39.5692841591687,
2.67267613167523));
#236261=CARTESIAN_POINT('Ctrl Pts',(-43.8210669472515,-39.5725311673656,
2.67403835432525));
#236262=CARTESIAN_POINT('Ctrl Pts',(-43.8205778953961,-39.5741546714641,
2.67471946565026));
#236263=CARTESIAN_POINT('Ctrl Pts',(-43.8201160933892,-39.5757777635548,
2.67541781389494));
#236264=CARTESIAN_POINT('Ctrl Pts',(-43.8196813503776,-39.5773992434496,
2.67613207244141));
#236265=CARTESIAN_POINT('Ctrl Pts',(-43.8195726646246,-39.5778046134233,
2.67631063707802));
#236266=CARTESIAN_POINT('Ctrl Pts',(-43.8194656698236,-39.5782098828931,
2.67649019601817));
#236267=CARTESIAN_POINT('Ctrl Pts',(-43.8193603625172,-39.5786150336268,
2.67667072836628));
#236268=CARTESIAN_POINT('Ctrl Pts',(-43.8190444405982,-39.5798304858277,
2.67721232541062));
#236269=CARTESIAN_POINT('Ctrl Pts',(-43.8187437073121,-39.5810448681191,
2.67776268340019));
#236270=CARTESIAN_POINT('Ctrl Pts',(-43.8184580587799,-39.5822576997162,
2.67832123541488));
#236271=CARTESIAN_POINT('Ctrl Pts',(-43.8164459874031,-39.5908007288813,
2.68225560368418));
#236272=CARTESIAN_POINT('Ctrl Pts',(-43.8151322889028,-39.5992865061389,
2.68661792998865));
#236273=CARTESIAN_POINT('Ctrl Pts',(-43.8144227306308,-39.6076412948836,
2.69130986622557));
#236274=CARTESIAN_POINT('Ctrl Pts',(-43.8140785956356,-39.6116933583964,
2.69358545023032));
#236275=CARTESIAN_POINT('Ctrl Pts',(-43.8138769687216,-39.6157150281162,
2.69593918853444));
#236276=CARTESIAN_POINT('Ctrl Pts',(-43.81380930989,-39.6196997093543,2.69836306235448));
#236277=CARTESIAN_POINT('Ctrl Pts',(-43.8137057289461,-39.6257999779283,
2.7020738438218));
#236278=CARTESIAN_POINT('Ctrl Pts',(-43.8139151128796,-39.6318101761582,
2.7059476081418));
#236279=CARTESIAN_POINT('Ctrl Pts',(-43.8144090029875,-39.6376940219322,
2.7099519634566));
#236280=CARTESIAN_POINT('Ctrl Pts',(-43.8146383681086,-39.6404265103486,
2.71181160678058));
#236281=CARTESIAN_POINT('Ctrl Pts',(-43.8149288459964,-39.6431316855283,
2.71369962772051));
#236282=CARTESIAN_POINT('Ctrl Pts',(-43.815278762865,-39.6458055463962,
2.71561183138613));
#236283=CARTESIAN_POINT('Ctrl Pts',(-43.8153055826142,-39.6460104872962,
2.71575839426264));
#236284=CARTESIAN_POINT('Ctrl Pts',(-43.8153327221691,-39.6462152612035,
2.71590508903161));
#236285=CARTESIAN_POINT('Ctrl Pts',(-43.8153601802951,-39.6464198673376,
2.71605191409863));
#236286=CARTESIAN_POINT('Ctrl Pts',(-43.815745884182,-39.6492939666538,
2.71811436362705));
#236287=CARTESIAN_POINT('Ctrl Pts',(-43.8161965332331,-39.6521348180507,
2.72020091026911));
#236288=CARTESIAN_POINT('Ctrl Pts',(-43.8167075634907,-39.6549389970089,
2.72230624862134));
#236289=CARTESIAN_POINT('Ctrl Pts',(-43.8185400271108,-39.6649942840468,
2.72985561753065));
#236290=CARTESIAN_POINT('Ctrl Pts',(-43.8211611138367,-39.6746561192248,
2.73770089914302));
#236291=CARTESIAN_POINT('Ctrl Pts',(-43.8244418968098,-39.6839173731636,
2.74574823347057));
#236292=CARTESIAN_POINT('Ctrl Pts',(-43.8280471477134,-39.694094560867,
2.75459144547026));
#236293=CARTESIAN_POINT('Ctrl Pts',(-43.8324491002311,-39.7037886794679,
2.76367911754291));
#236294=CARTESIAN_POINT('Ctrl Pts',(-43.8375295667871,-39.7129876499616,
2.77292162564768));
#236295=CARTESIAN_POINT('Ctrl Pts',(-43.8430151956447,-39.7229202294687,
2.78290121484821));
#236296=CARTESIAN_POINT('Ctrl Pts',(-43.8492922888422,-39.7322766233317,
2.7930622950033));
#236297=CARTESIAN_POINT('Ctrl Pts',(-43.8562669044111,-39.741024548631,
2.80331916685446));
#236298=CARTESIAN_POINT('Ctrl Pts',(-43.8631830101207,-39.7496990878241,
2.81348999408814));
#236299=CARTESIAN_POINT('Ctrl Pts',(-43.8707860819065,-39.7577762496645,
2.82375635966922));
#236300=CARTESIAN_POINT('Ctrl Pts',(-43.8790236240217,-39.7651933659001,
2.83404198860233));
#236301=CARTESIAN_POINT('Origin',(-0.0101975504408993,0.0113255271404686,
2.83404198860262));
#236302=CARTESIAN_POINT('Ctrl Pts',(-46.7142062431419,-42.0411527846897,
2.65878198860231));
#236303=CARTESIAN_POINT('Ctrl Pts',(-46.7199506919425,-42.0347675597389,
2.65878198860232));
#236304=CARTESIAN_POINT('Ctrl Pts',(-46.7251107020211,-42.0279592142775,
2.65944603041819));
#236305=CARTESIAN_POINT('Ctrl Pts',(-46.7296675019394,-42.0208774479579,
2.66070439264037));
#236306=CARTESIAN_POINT('Ctrl Pts',(-46.7325790801593,-42.0163525364093,
2.66150842619562));
#236307=CARTESIAN_POINT('Ctrl Pts',(-46.7352451892138,-42.0117164851998,
2.66255428265335));
#236308=CARTESIAN_POINT('Ctrl Pts',(-46.737668963875,-42.0070114066748,
2.66381699700623));
#236309=CARTESIAN_POINT('Ctrl Pts',(-46.7409769299532,-42.0005899185698,
2.66554034873222));
#236310=CARTESIAN_POINT('Ctrl Pts',(-46.7438276087417,-41.9940383480779,
2.66766759643927));
#236311=CARTESIAN_POINT('Ctrl Pts',(-46.7462229640885,-41.9874523371582,
2.67012012783103));
#236312=CARTESIAN_POINT('Ctrl Pts',(-46.7474206417619,-41.9841593316984,
2.67134639352691));
#236313=CARTESIAN_POINT('Ctrl Pts',(-46.7485046297344,-41.9808575622225,
2.67265375584967));
#236314=CARTESIAN_POINT('Ctrl Pts',(-46.749476178293,-41.9775578801519,
2.67403135126894));
#236315=CARTESIAN_POINT('Ctrl Pts',(-46.7499619525723,-41.9759080391167,
2.67472014897858));
#236316=CARTESIAN_POINT('Ctrl Pts',(-46.7504196286878,-41.9742587070257,
2.67542649668587));
#236317=CARTESIAN_POINT('Ctrl Pts',(-46.7508494364809,-41.9726111592841,
2.67614899656056));
#236318=CARTESIAN_POINT('Ctrl Pts',(-46.7509568884292,-41.9721992723487,
2.67632962152923));
#236319=CARTESIAN_POINT('Ctrl Pts',(-46.7510625988572,-41.9717874966608,
2.67651125590905));
#236320=CARTESIAN_POINT('Ctrl Pts',(-46.7511665718603,-41.9713758515959,
2.67669387767478));
#236321=CARTESIAN_POINT('Ctrl Pts',(-46.7514784908696,-41.9701409164013,
2.67724174297198));
#236322=CARTESIAN_POINT('Ctrl Pts',(-46.7517747718021,-41.968907158177,
2.67779849504701));
#236323=CARTESIAN_POINT('Ctrl Pts',(-46.7520555364229,-41.9676750878621,
2.67836353617963));
#236324=CARTESIAN_POINT('Ctrl Pts',(-46.7539957941551,-41.9591607175413,
2.68226832098868));
#236325=CARTESIAN_POINT('Ctrl Pts',(-46.7552464720206,-41.9507055072914,
2.6865915375136));
#236326=CARTESIAN_POINT('Ctrl Pts',(-46.7559027543577,-41.9423805287164,
2.69123699486156));
#236327=CARTESIAN_POINT('Ctrl Pts',(-46.7562289248778,-41.9382430372165,
2.69354577441186));
#236328=CARTESIAN_POINT('Ctrl Pts',(-46.7564078446192,-41.9341372814969,
2.69593478828079));
#236329=CARTESIAN_POINT('Ctrl Pts',(-46.756448717314,-41.9300700339485,
2.69839565261173));
#236330=CARTESIAN_POINT('Ctrl Pts',(-46.7565388885836,-41.921097078357,
2.70382468688998));
#236331=CARTESIAN_POINT('Ctrl Pts',(-46.7559695796222,-41.9123126321655,
2.7096115581504));
#236332=CARTESIAN_POINT('Ctrl Pts',(-46.7548061840814,-41.9038465062686,
2.7156270136172));
#236333=CARTESIAN_POINT('Ctrl Pts',(-46.7543811810191,-41.900753723715,
2.7178245353581));
#236334=CARTESIAN_POINT('Ctrl Pts',(-46.753883681602,-41.8976992635447,
2.72005051502353));
#236335=CARTESIAN_POINT('Ctrl Pts',(-46.7533184435774,-41.8946854937103,
2.72229986760065));
#236336=CARTESIAN_POINT('Ctrl Pts',(-46.7514198688642,-41.8845625597427,
2.72985520488882));
#236337=CARTESIAN_POINT('Ctrl Pts',(-46.7487367327308,-41.8748360802666,
2.73770845534592));
#236338=CARTESIAN_POINT('Ctrl Pts',(-46.7453971059997,-41.8655137786563,
2.74576706701833));
#236339=CARTESIAN_POINT('Ctrl Pts',(-46.7417264606175,-41.8552674648873,
2.75462443585157));
#236340=CARTESIAN_POINT('Ctrl Pts',(-46.7372626589198,-41.845508736713,
2.76373036323361));
#236341=CARTESIAN_POINT('Ctrl Pts',(-46.7321227530945,-41.8362508575421,
2.77299664637051));
#236342=CARTESIAN_POINT('Ctrl Pts',(-46.7265868542931,-41.8262797250063,
2.78297683033768));
#236343=CARTESIAN_POINT('Ctrl Pts',(-46.7202662104721,-41.8168884800845,
2.79314401479249));
#236344=CARTESIAN_POINT('Ctrl Pts',(-46.7132528291595,-41.8081115112052,
2.80341452428356));
#236345=CARTESIAN_POINT('Ctrl Pts',(-46.7063341521765,-41.7994530610428,
2.81354634721632));
#236346=CARTESIAN_POINT('Ctrl Pts',(-46.698740203124,-41.7913915075174,
2.8237800420932));
#236347=CARTESIAN_POINT('Ctrl Pts',(-46.6905216402894,-41.7839914803029,
2.83404198860232));
#236348=CARTESIAN_POINT('Ctrl Pts',(-44.1339623850444,-39.4820551873932,
2.83404198860233));
#236349=CARTESIAN_POINT('Ctrl Pts',(-44.1260971752942,-39.4749733207249,
2.82422126442994));
#236350=CARTESIAN_POINT('Ctrl Pts',(-44.1177016730292,-39.4685372764358,
2.81442815028504));
#236351=CARTESIAN_POINT('Ctrl Pts',(-44.1088266671088,-39.4627751762752,
2.80471618166336));
#236352=CARTESIAN_POINT('Ctrl Pts',(-44.1002570680353,-39.4572113615981,
2.79533842146256));
#236353=CARTESIAN_POINT('Ctrl Pts',(-44.0912392969009,-39.4522752837267,
2.78603515650274));
#236354=CARTESIAN_POINT('Ctrl Pts',(-44.0817922708741,-39.4480294591797,
2.77685887346798));
#236355=CARTESIAN_POINT('Ctrl Pts',(-44.0728618726534,-39.4440158252729,
2.76818441216621));
#236356=CARTESIAN_POINT('Ctrl Pts',(-44.0635470605553,-39.4406186435284,
2.75962261521671));
#236357=CARTESIAN_POINT('Ctrl Pts',(-44.0538529442815,-39.4379312493392,
2.75123537701709));
#236358=CARTESIAN_POINT('Ctrl Pts',(-44.0449248258243,-39.4354562043754,
2.74351087134168));
#236359=CARTESIAN_POINT('Ctrl Pts',(-44.0356744386774,-39.4335831186684,
2.73593399449895));
#236360=CARTESIAN_POINT('Ctrl Pts',(-44.0261054687983,-39.432423032912,
2.72857657812624));
#236361=CARTESIAN_POINT('Ctrl Pts',(-44.0232521951431,-39.4320771187574,
2.7263827450834));
#236362=CARTESIAN_POINT('Ctrl Pts',(-44.0203706219322,-39.4317948788026,
2.72420861709588));
#236363=CARTESIAN_POINT('Ctrl Pts',(-44.0174609456693,-39.4315800126158,
2.72205663736679));
#236364=CARTESIAN_POINT('Ctrl Pts',(-44.0145809991271,-39.4313673418319,
2.71992664556718));
#236365=CARTESIAN_POINT('Ctrl Pts',(-44.0116765294501,-39.4312206224784,
2.71782089927837));
#236366=CARTESIAN_POINT('Ctrl Pts',(-44.0087510493742,-39.4311433701096,
2.71574387311198));
#236367=CARTESIAN_POINT('Ctrl Pts',(-44.008547617211,-39.4311379981309,
2.71559944077439));
#236368=CARTESIAN_POINT('Ctrl Pts',(-44.0083440782821,-39.4311329512713,
2.71545515216021));
#236369=CARTESIAN_POINT('Ctrl Pts',(-44.0081404327822,-39.4311282308203,
2.71531100781682));
#236370=CARTESIAN_POINT('Ctrl Pts',(-43.9992118680541,-39.4309212689595,
2.70899119176038));
#236371=CARTESIAN_POINT('Ctrl Pts',(-43.9900881971804,-39.4313859080978,
2.70298296066795));
#236372=CARTESIAN_POINT('Ctrl Pts',(-43.9808585737696,-39.4325966403785,
2.69736727774094));
#236373=CARTESIAN_POINT('Ctrl Pts',(-43.972254960653,-39.4337252532879,
2.69213248525389));
#236374=CARTESIAN_POINT('Ctrl Pts',(-43.9635585482856,-39.4355025470896,
2.6872386618543));
#236375=CARTESIAN_POINT('Ctrl Pts',(-43.9548613290782,-39.4380105519135,
2.68278595829526));
#236376=CARTESIAN_POINT('Ctrl Pts',(-43.951679773774,-39.4389280125248,
2.68115710172762));
#236377=CARTESIAN_POINT('Ctrl Pts',(-43.9484983634052,-39.4399434521994,
2.67958763637761));
#236378=CARTESIAN_POINT('Ctrl Pts',(-43.9453226165469,-39.4410615611724,
2.6780837864531));
#236379=CARTESIAN_POINT('Ctrl Pts',(-43.9445589555198,-39.4413304290277,
2.67772216078546));
#236380=CARTESIAN_POINT('Ctrl Pts',(-43.9437952833153,-39.441605709343,
2.67736403603508));
#236381=CARTESIAN_POINT('Ctrl Pts',(-43.9430317345446,-39.4418874191262,
2.67700956934424));
#236382=CARTESIAN_POINT('Ctrl Pts',(-43.9422920466731,-39.4421603254787,
2.67666617973749));
#236383=CARTESIAN_POINT('Ctrl Pts',(-43.9415524746576,-39.4424392657172,
2.67632622314064));
#236384=CARTESIAN_POINT('Ctrl Pts',(-43.9408131433996,-39.4427242524727,
2.67598984158719));
#236385=CARTESIAN_POINT('Ctrl Pts',(-43.9327129150434,-39.4458466117307,
2.67230439292187));
#236386=CARTESIAN_POINT('Ctrl Pts',(-43.9246364083439,-39.449697209665,
2.66904964539958));
#236387=CARTESIAN_POINT('Ctrl Pts',(-43.9167721156749,-39.4542738890606,
2.66640203566717));
#236388=CARTESIAN_POINT('Ctrl Pts',(-43.913510559095,-39.4561719744226,
2.66530399299414));
#236389=CARTESIAN_POINT('Ctrl Pts',(-43.9102855324951,-39.4581945203282,
2.66430995142218));
#236390=CARTESIAN_POINT('Ctrl Pts',(-43.9071101492106,-39.4603395741452,
2.66343053473307));
#236391=CARTESIAN_POINT('Ctrl Pts',(-43.9016942021212,-39.4639981869598,
2.66193059792832));
#236392=CARTESIAN_POINT('Ctrl Pts',(-43.8964251099354,-39.4680136963362,
2.66076519817075));
#236393=CARTESIAN_POINT('Ctrl Pts',(-43.8913745966871,-39.4723737491581,
2.65997805604408));
#236394=CARTESIAN_POINT('Ctrl Pts',(-43.8888493400629,-39.474553775569,
2.65958448498075));
#236395=CARTESIAN_POINT('Ctrl Pts',(-43.8863797569638,-39.4768209551509,
2.65928526260711));
#236396=CARTESIAN_POINT('Ctrl Pts',(-43.8839748786089,-39.4791737454928,
2.65908463971274));
#236397=CARTESIAN_POINT('Ctrl Pts',(-43.881570000254,-39.4815265358346,
2.65888401681836));
#236398=CARTESIAN_POINT('Ctrl Pts',(-43.8792298420738,-39.4839648939619,
2.65878198860234));
#236399=CARTESIAN_POINT('Ctrl Pts',(-43.8769616275871,-39.4864862581818,
2.65878198860234));
#236400=CARTESIAN_POINT('Origin',(-38.974747650051,-43.3086183250768,2.83404198860231));
#236401=CARTESIAN_POINT('Ctrl Pts',(-41.7839914803023,-46.6905216402899,
2.83404198860228));
#236402=CARTESIAN_POINT('Ctrl Pts',(-41.7910911765302,-46.6984066517721,
2.82419652440022));
#236403=CARTESIAN_POINT('Ctrl Pts',(-41.7987919603585,-46.7057080773545,
2.81438790575603));
#236404=CARTESIAN_POINT('Ctrl Pts',(-41.8070443420767,-46.7123936319701,
2.80466781256855));
#236405=CARTESIAN_POINT('Ctrl Pts',(-41.8150285705287,-46.7188619458705,
2.79526356453034));
#236406=CARTESIAN_POINT('Ctrl Pts',(-41.8235301761256,-46.7247545199412,
2.78594102496193));
#236407=CARTESIAN_POINT('Ctrl Pts',(-41.8325358446871,-46.7300083326608,
2.77675109088745));
#236408=CARTESIAN_POINT('Ctrl Pts',(-41.8410546526091,-46.7349781159824,
2.76805797913658));
#236409=CARTESIAN_POINT('Ctrl Pts',(-41.8500252953107,-46.7393768060085,
2.75948271210147));
#236410=CARTESIAN_POINT('Ctrl Pts',(-41.8594521748282,-46.7431119772971,
2.75108575573218));
#236411=CARTESIAN_POINT('Ctrl Pts',(-41.8681350126332,-46.7465523401883,
2.74335155163274));
#236412=CARTESIAN_POINT('Ctrl Pts',(-41.8772054497772,-46.7494299450228,
2.73576818685956));
#236413=CARTESIAN_POINT('Ctrl Pts',(-41.8866715402901,-46.7516345991556,
2.72840626160516));
#236414=CARTESIAN_POINT('Ctrl Pts',(-41.8894172933146,-46.7522740855142,
2.72627084693681));
#236415=CARTESIAN_POINT('Ctrl Pts',(-41.892196339742,-46.7528566833417,
2.72415424587506));
#236416=CARTESIAN_POINT('Ctrl Pts',(-41.8950088623276,-46.7533790039319,
2.72205867173224));
#236417=CARTESIAN_POINT('Ctrl Pts',(-41.8980578176392,-46.7539452330337,
2.71978693462827));
#236418=CARTESIAN_POINT('Ctrl Pts',(-41.9011416752729,-46.7544408966255,
2.71754411340727));
#236419=CARTESIAN_POINT('Ctrl Pts',(-41.9042597210852,-46.7548620578767,
2.71533341844224));
#236420=CARTESIAN_POINT('Ctrl Pts',(-41.912817222284,-46.7560179382355,
2.70926614876371));
#236421=CARTESIAN_POINT('Ctrl Pts',(-41.9216270724807,-46.756568484326,
2.70347381860389));
#236422=CARTESIAN_POINT('Ctrl Pts',(-41.9306033478346,-46.756455626462,
2.69804914171375));
#236423=CARTESIAN_POINT('Ctrl Pts',(-41.9388161524499,-46.7563523676437,
2.69308585687201));
#236424=CARTESIAN_POINT('Ctrl Pts',(-41.9471607721478,-46.7556849461648,
2.68842799053196));
#236425=CARTESIAN_POINT('Ctrl Pts',(-41.9555881906094,-46.7543795041532,
2.68414767054239));
#236426=CARTESIAN_POINT('Ctrl Pts',(-41.9597277110287,-46.7537382753014,
2.68204519134558));
#236427=CARTESIAN_POINT('Ctrl Pts',(-41.9638869554862,-46.7529426662695,
2.68003431778494));
#236428=CARTESIAN_POINT('Ctrl Pts',(-41.9680580970361,-46.7519812517996,
2.67812693945231));
#236429=CARTESIAN_POINT('Ctrl Pts',(-41.9688495305177,-46.7517988327683,
2.67776503299183));
#236430=CARTESIAN_POINT('Ctrl Pts',(-41.9696416823154,-46.7516099985532,
2.67740659639904));
#236431=CARTESIAN_POINT('Ctrl Pts',(-41.97043441682,-46.7514147143009,2.67705178968835));
#236432=CARTESIAN_POINT('Ctrl Pts',(-41.9712023783712,-46.7512255326815,
2.67670807068737));
#236433=CARTESIAN_POINT('Ctrl Pts',(-41.9719708867608,-46.7510302978708,
2.67636775825245));
#236434=CARTESIAN_POINT('Ctrl Pts',(-41.9727398158584,-46.7508289807695,
2.67603099699235));
#236435=CARTESIAN_POINT('Ctrl Pts',(-41.9811194467226,-46.7486350684818,
2.67236104217089));
#236436=CARTESIAN_POINT('Ctrl Pts',(-41.9895544525284,-46.745716979482,
2.6691144054142));
#236437=CARTESIAN_POINT('Ctrl Pts',(-41.9978556152128,-46.7420530111683,
2.6664677818957));
#236438=CARTESIAN_POINT('Ctrl Pts',(-42.0013612477616,-46.7405056945975,
2.66535009634929));
#236439=CARTESIAN_POINT('Ctrl Pts',(-42.0048429302643,-46.7388257854547,
2.66433897912313));
#236440=CARTESIAN_POINT('Ctrl Pts',(-42.0082865614559,-46.7370135816691,
2.66344564884772));
#236441=CARTESIAN_POINT('Ctrl Pts',(-42.0140855503362,-46.7339618757757,
2.66194130298565));
#236442=CARTESIAN_POINT('Ctrl Pts',(-42.0197742252482,-46.7305342346688,
2.660772067054));
#236443=CARTESIAN_POINT('Ctrl Pts',(-42.0252784509102,-46.7267341265712,
2.65998225155694));
#236444=CARTESIAN_POINT('Ctrl Pts',(-42.0266545073257,-46.7257840995468,
2.65978479768268));
#236445=CARTESIAN_POINT('Ctrl Pts',(-42.0280188904105,-46.7248106099129,
2.65961098966602));
#236446=CARTESIAN_POINT('Ctrl Pts',(-42.0293702408568,-46.7238134778073,
2.65946139030481));
#236447=CARTESIAN_POINT('Ctrl Pts',(-42.0313972665263,-46.7223177796489,
2.659236991263));
#236448=CARTESIAN_POINT('Ctrl Pts',(-42.0333949481516,-46.720768886388,
2.65906707562421));
#236449=CARTESIAN_POINT('Ctrl Pts',(-42.0353598072043,-46.7191674503113,
2.65895332562899));
#236450=CARTESIAN_POINT('Ctrl Pts',(-42.037324666257,-46.7175660142346,
2.65883957563377));
#236451=CARTESIAN_POINT('Ctrl Pts',(-42.039256703587,-46.7159120469177,
2.65878198860228));
#236452=CARTESIAN_POINT('Ctrl Pts',(-42.0411527846902,-46.7142062431437,
2.65878198860228));
#236453=CARTESIAN_POINT('Ctrl Pts',(-39.4864862581813,-43.8769616275876,
2.6587819886023));
#236454=CARTESIAN_POINT('Ctrl Pts',(-39.4800703482071,-43.8827333680736,
2.6587819886023));
#236455=CARTESIAN_POINT('Ctrl Pts',(-39.4741864828754,-43.8889846873395,
2.65945335517821));
#236456=CARTESIAN_POINT('Ctrl Pts',(-39.4688721660169,-43.895569202337,
2.66072561226562));
#236457=CARTESIAN_POINT('Ctrl Pts',(-39.4654396626066,-43.8998221234152,
2.66154735980301));
#236458=CARTESIAN_POINT('Ctrl Pts',(-39.4622440309669,-43.9042134689398,
2.66261895766847));
#236459=CARTESIAN_POINT('Ctrl Pts',(-39.459287497615,-43.9086997575135,
2.66391429250995));
#236460=CARTESIAN_POINT('Ctrl Pts',(-39.4553687820178,-43.9146460760272,
2.66563118464091));
#236461=CARTESIAN_POINT('Ctrl Pts',(-39.4518755008529,-43.9207613318564,
2.66774105138666));
#236462=CARTESIAN_POINT('Ctrl Pts',(-39.4488169076805,-43.9269559348855,
2.67016894181717));
#236463=CARTESIAN_POINT('Ctrl Pts',(-39.4472876110943,-43.9300532364001,
2.67138288703242));
#236464=CARTESIAN_POINT('Ctrl Pts',(-39.4458668372378,-43.9331705067653,
2.67267613167517));
#236465=CARTESIAN_POINT('Ctrl Pts',(-39.4445546869045,-43.9362974878338,
2.67403835432519));
#236466=CARTESIAN_POINT('Ctrl Pts',(-39.4438986117378,-43.937860978368,
2.6747194656502));
#236467=CARTESIAN_POINT('Ctrl Pts',(-39.4432696802086,-43.9394269075363,
2.67541781389489));
#236468=CARTESIAN_POINT('Ctrl Pts',(-39.442667827963,-43.9409940617756,
2.67613207244135));
#236469=CARTESIAN_POINT('Ctrl Pts',(-39.4425173649017,-43.9413858503355,
2.67631063707797));
#236470=CARTESIAN_POINT('Ctrl Pts',(-39.4423685940344,-43.9417777156946,
2.67649019601812));
#236471=CARTESIAN_POINT('Ctrl Pts',(-39.4422215138289,-43.9421696393592,
2.67667072836623));
#236472=CARTESIAN_POINT('Ctrl Pts',(-39.4417802732125,-43.9433454103531,
2.67721232541057));
#236473=CARTESIAN_POINT('Ctrl Pts',(-39.44135424986,-43.944521704943,2.67776268340013));
#236474=CARTESIAN_POINT('Ctrl Pts',(-39.4409433907174,-43.9456980341196,
2.67832123541482));
#236475=CARTESIAN_POINT('Ctrl Pts',(-39.4380493519679,-43.9539839449479,
2.68225560368404));
#236476=CARTESIAN_POINT('Ctrl Pts',(-39.4358558447891,-43.9622859173441,
2.6866179299884));
#236477=CARTESIAN_POINT('Ctrl Pts',(-39.4342768603232,-43.9705207686459,
2.69130986622521));
#236478=CARTESIAN_POINT('Ctrl Pts',(-39.4335110545634,-43.9745146626289,
2.69358545023006));
#236479=CARTESIAN_POINT('Ctrl Pts',(-39.4328901532271,-43.9784932254698,
2.69593918853429));
#236480=CARTESIAN_POINT('Ctrl Pts',(-39.4324063524312,-43.9824490059337,
2.69836306235443));
#236481=CARTESIAN_POINT('Ctrl Pts',(-39.4316656872149,-43.9885050294413,
2.70207384382176));
#236482=CARTESIAN_POINT('Ctrl Pts',(-39.4312456873365,-43.9945041897572,
2.70594760814177));
#236483=CARTESIAN_POINT('Ctrl Pts',(-39.4311218425058,-44.0004074287824,
2.70995196345657));
#236484=CARTESIAN_POINT('Ctrl Pts',(-39.4310643283258,-44.003148923525,
2.71181160678055));
#236485=CARTESIAN_POINT('Ctrl Pts',(-39.4310704471408,-44.0058696426792,
2.71369962772048));
#236486=CARTESIAN_POINT('Ctrl Pts',(-39.4311389525607,-44.0085654321301,
2.7156118313861));
#236487=CARTESIAN_POINT('Ctrl Pts',(-39.4311442032312,-44.0087720537696,
2.71575839426261));
#236488=CARTESIAN_POINT('Ctrl Pts',(-39.4311497894109,-44.00897854276,2.71590508903158));
#236489=CARTESIAN_POINT('Ctrl Pts',(-39.4311557099537,-44.0091848981959,
2.71605191409861));
#236490=CARTESIAN_POINT('Ctrl Pts',(-39.4312388757296,-44.01208356993,2.71811436362702));
#236491=CARTESIAN_POINT('Ctrl Pts',(-39.4313901062471,-44.0149559644985,
2.72020091026908));
#236492=CARTESIAN_POINT('Ctrl Pts',(-39.4316052205102,-44.0177981990785,
2.72230624862131));
#236493=CARTESIAN_POINT('Ctrl Pts',(-39.432376582001,-44.0279899468077,
2.72985561753042));
#236494=CARTESIAN_POINT('Ctrl Pts',(-39.4339733733561,-44.037872831609,
2.73770089914259));
#236495=CARTESIAN_POINT('Ctrl Pts',(-39.4362681192145,-44.0474262866319,
2.74574823346991));
#236496=CARTESIAN_POINT('Ctrl Pts',(-39.4387898143852,-44.0579245739722,
2.75459144546905));
#236497=CARTESIAN_POINT('Ctrl Pts',(-39.4421543412261,-44.0680257165085,
2.76367911754111));
#236498=CARTESIAN_POINT('Ctrl Pts',(-39.446245422205,-44.0777053474406,
2.77292162564527));
#236499=CARTESIAN_POINT('Ctrl Pts',(-39.4506627629409,-44.0881569195912,
2.78290121484453));
#236500=CARTESIAN_POINT('Ctrl Pts',(-39.455927460092,-44.0981181930543,
2.7930622949983));
#236501=CARTESIAN_POINT('Ctrl Pts',(-39.4619494607976,-44.1075472421499,
2.80331916684814));
#236502=CARTESIAN_POINT('Ctrl Pts',(-39.467920943106,-44.1168971912135,
2.81348999408387));
#236503=CARTESIAN_POINT('Ctrl Pts',(-39.4746380711555,-44.125724842928,
2.82375635966706));
#236504=CARTESIAN_POINT('Ctrl Pts',(-39.4820551873926,-44.1339623850449,
2.8340419886023));
#236505=CARTESIAN_POINT('Origin',(-0.0113255271402662,0.0101975504411025,
2.83404198860262));
#236506=CARTESIAN_POINT('Ctrl Pts',(-42.0638038389696,-46.6938111422606,
2.65878198860228));
#236507=CARTESIAN_POINT('Ctrl Pts',(-42.0701842568304,-46.6880613546456,
2.65878198860228));
#236508=CARTESIAN_POINT('Ctrl Pts',(-42.0760276657224,-46.681829673937,
2.65944603041817));
#236509=CARTESIAN_POINT('Ctrl Pts',(-42.0812997491646,-46.6752630175671,
2.66070439264036));
#236510=CARTESIAN_POINT('Ctrl Pts',(-42.0846683595049,-46.6710672367545,
2.6615084261956));
#236511=CARTESIAN_POINT('Ctrl Pts',(-42.0878044626435,-46.6667352666009,
2.66255428265333));
#236512=CARTESIAN_POINT('Ctrl Pts',(-42.0907067742413,-46.6623093164291,
2.6638169970062));
#236513=CARTESIAN_POINT('Ctrl Pts',(-42.0946678472187,-46.6562687825186,
2.6655403487322));
#236514=CARTESIAN_POINT('Ctrl Pts',(-42.0981877352861,-46.6500510792883,
2.66766759643925));
#236515=CARTESIAN_POINT('Ctrl Pts',(-42.1012583942262,-46.6437515300389,
2.67012012783101));
#236516=CARTESIAN_POINT('Ctrl Pts',(-42.1027937236962,-46.6406017554143,
2.67134639352689));
#236517=CARTESIAN_POINT('Ctrl Pts',(-42.1042169023586,-46.637431380974,
2.67265375584965));
#236518=CARTESIAN_POINT('Ctrl Pts',(-42.1055280393686,-46.6342513293849,
2.67403135126893));
#236519=CARTESIAN_POINT('Ctrl Pts',(-42.1061836078736,-46.6326613035903,
2.67472014897856));
#236520=CARTESIAN_POINT('Ctrl Pts',(-42.1068111789403,-46.6310688468941,
2.67542649668585));
#236521=CARTESIAN_POINT('Ctrl Pts',(-42.107410847835,-46.6294752517396,
2.67614899656055));
#236522=CARTESIAN_POINT('Ctrl Pts',(-42.1075607650587,-46.6290768529509,
2.67632962152922));
#236523=CARTESIAN_POINT('Ctrl Pts',(-42.1077089386737,-46.628678382762,
2.67651125590904));
#236524=CARTESIAN_POINT('Ctrl Pts',(-42.1078553707279,-46.6282798608701,
2.67669387767477));
#236525=CARTESIAN_POINT('Ctrl Pts',(-42.1082946668904,-46.6270842951944,
2.67724174297197));
#236526=CARTESIAN_POINT('Ctrl Pts',(-42.1087182876161,-46.6258882654172,
2.67779849504701));
#236527=CARTESIAN_POINT('Ctrl Pts',(-42.1091263005957,-46.6246922924067,
2.67836353617962));
#236528=CARTESIAN_POINT('Ctrl Pts',(-42.1119459234382,-46.6164273768568,
2.68226832098856));
#236529=CARTESIAN_POINT('Ctrl Pts',(-42.1140735600934,-46.6081492165689,
2.68659153751333));
#236530=CARTESIAN_POINT('Ctrl Pts',(-42.1155964444645,-46.599938443282,
2.69123699486112));
#236531=CARTESIAN_POINT('Ctrl Pts',(-42.1163533138166,-46.5958577114964,
2.69354577441156));
#236532=CARTESIAN_POINT('Ctrl Pts',(-42.1169604217529,-46.5917931497416,
2.69593478828063));
#236533=CARTESIAN_POINT('Ctrl Pts',(-42.1174262136788,-46.5877524553606,
2.69839565261171));
#236534=CARTESIAN_POINT('Ctrl Pts',(-42.1184538202397,-46.5788380800229,
2.70382468688996));
#236535=CARTESIAN_POINT('Ctrl Pts',(-42.1188058546734,-46.5700422469559,
2.70961155815037));
#236536=CARTESIAN_POINT('Ctrl Pts',(-42.118533783465,-46.5615008914345,
2.71562701361717));
#236537=CARTESIAN_POINT('Ctrl Pts',(-42.1184343924215,-46.5583806265503,
2.71782453535807));
#236538=CARTESIAN_POINT('Ctrl Pts',(-42.118258896386,-46.5552908961829,
2.72005051502352));
#236539=CARTESIAN_POINT('Ctrl Pts',(-42.1180117795239,-46.5522345526329,
2.72229986760066));
#236540=CARTESIAN_POINT('Ctrl Pts',(-42.1171817401332,-46.5419686180612,
2.72985520488781));
#236541=CARTESIAN_POINT('Ctrl Pts',(-42.1155299964533,-46.532014957162,
2.73770845534385));
#236542=CARTESIAN_POINT('Ctrl Pts',(-42.1131831104089,-46.5223946380466,
2.74576706701515));
#236543=CARTESIAN_POINT('Ctrl Pts',(-42.1106036046392,-46.5118207677369,
2.75462443584726));
#236544=CARTESIAN_POINT('Ctrl Pts',(-42.1071843209746,-46.5016489045661,
2.7637303632281));
#236545=CARTESIAN_POINT('Ctrl Pts',(-42.103040283975,-46.4919044745698,
2.77299664636376));
#236546=CARTESIAN_POINT('Ctrl Pts',(-42.0985769785686,-46.4814093059481,
2.78297683032949));
#236547=CARTESIAN_POINT('Ctrl Pts',(-42.0932726122969,-46.4714088200642,
2.79314401478278));
#236548=CARTESIAN_POINT('Ctrl Pts',(-42.0872150940914,-46.4619468343687,
2.80341452427227));
#236549=CARTESIAN_POINT('Ctrl Pts',(-42.0812393728328,-46.4526126174252,
2.81354634720878));
#236550=CARTESIAN_POINT('Ctrl Pts',(-42.0745296860268,-46.4438014421052,
2.82378004208946));
#236551=CARTESIAN_POINT('Ctrl Pts',(-42.0671296588092,-46.4355828792672,
2.83404198860229));
#236552=CARTESIAN_POINT('Ctrl Pts',(-39.7651933658995,-43.8790236240221,
2.8340419886023));
#236553=CARTESIAN_POINT('Ctrl Pts',(-39.7581114992311,-43.8711584142718,
2.82422126442972));
#236554=CARTESIAN_POINT('Ctrl Pts',(-39.7504347382248,-43.8638800583566,
2.81442815028464));
#236555=CARTESIAN_POINT('Ctrl Pts',(-39.7422106539903,-43.857221832853,
2.80471618166279));
#236556=CARTESIAN_POINT('Ctrl Pts',(-39.7342695770751,-43.8507927303129,
2.79533842146186));
#236557=CARTESIAN_POINT('Ctrl Pts',(-39.7258171668688,-43.8449410790337,
2.78603515650193));
#236558=CARTESIAN_POINT('Ctrl Pts',(-39.7168657021541,-43.8397310304448,
2.77685887346705));
#236559=CARTESIAN_POINT('Ctrl Pts',(-39.7084037645735,-43.8348059028421,
2.76818441216518));
#236560=CARTESIAN_POINT('Ctrl Pts',(-39.6994950821778,-43.8304536682203,
2.75962261521558));
#236561=CARTESIAN_POINT('Ctrl Pts',(-39.6901349804719,-43.8267676847809,
2.75123537701587));
#236562=CARTESIAN_POINT('Ctrl Pts',(-39.6815144838282,-43.8233729558701,
2.74351087134036));
#236563=CARTESIAN_POINT('Ctrl Pts',(-39.6725105620403,-43.8205432023696,
2.73593399449755));
#236564=CARTESIAN_POINT('Ctrl Pts',(-39.6631152739606,-43.8183892419679,
2.72857657812477));
#236565=CARTESIAN_POINT('Ctrl Pts',(-39.6603137887126,-43.8177469744569,
2.72638274508242));
#236566=CARTESIAN_POINT('Ctrl Pts',(-39.6574775031707,-43.8171650742228,
2.72420861709538));
#236567=CARTESIAN_POINT('Ctrl Pts',(-39.6546062260517,-43.8166472411071,
2.72205663736677));
#236568=CARTESIAN_POINT('Ctrl Pts',(-39.6517642863082,-43.8161346989697,
2.71992664556715));
#236569=CARTESIAN_POINT('Ctrl Pts',(-39.6488910639686,-43.8156851836083,
2.71782089927834));
#236570=CARTESIAN_POINT('Ctrl Pts',(-39.64598968505,-43.8153025584993,2.71574387311195));
#236571=CARTESIAN_POINT('Ctrl Pts',(-39.6457879288342,-43.8152759514975,
2.71559944077436));
#236572=CARTESIAN_POINT('Ctrl Pts',(-39.6455860324533,-43.8152496566736,
2.71545515216019));
#236573=CARTESIAN_POINT('Ctrl Pts',(-39.6453839959662,-43.8152236753307,
2.7153110078168));
#236574=CARTESIAN_POINT('Ctrl Pts',(-39.6365259762553,-43.8140845580783,
2.70899119176042));
#236575=CARTESIAN_POINT('Ctrl Pts',(-39.6274037177902,-43.8135929685791,
2.70298296066806));
#236576=CARTESIAN_POINT('Ctrl Pts',(-39.6180980992375,-43.81383230999,2.69736727774111));
#236577=CARTESIAN_POINT('Ctrl Pts',(-39.6094236454411,-43.8140554177821,
2.69213248525421));
#236578=CARTESIAN_POINT('Ctrl Pts',(-39.6005890951409,-43.8149139527617,
2.68723866185477));
#236579=CARTESIAN_POINT('Ctrl Pts',(-39.5916773623205,-43.8164991115142,
2.68278595829582));
#236580=CARTESIAN_POINT('Ctrl Pts',(-39.588417335161,-43.8170789830935,
2.68115710172799));
#236581=CARTESIAN_POINT('Ctrl Pts',(-39.585147210542,-43.8177563121465,
2.6795876363778));
#236582=CARTESIAN_POINT('Ctrl Pts',(-39.5818719865441,-43.8185363400628,
2.67808378645312));
#236583=CARTESIAN_POINT('Ctrl Pts',(-39.5810844045883,-43.8187239107183,
2.67772216078547));
#236584=CARTESIAN_POINT('Ctrl Pts',(-39.5802961412317,-43.8189178575372,
2.6773640360351));
#236585=CARTESIAN_POINT('Ctrl Pts',(-39.5795073285704,-43.8191182115052,
2.67700956934426));
#236586=CARTESIAN_POINT('Ctrl Pts',(-39.5787431663048,-43.8193123044116,
2.67666617973751));
#236587=CARTESIAN_POINT('Ctrl Pts',(-39.5779784885477,-43.81951241026,2.67632622314066));
#236588=CARTESIAN_POINT('Ctrl Pts',(-39.5772134181961,-43.819718554668,
2.6759898415872));
#236589=CARTESIAN_POINT('Ctrl Pts',(-39.5688311883227,-43.8219771048932,
2.67230439292161));
#236590=CARTESIAN_POINT('Ctrl Pts',(-39.5603964284866,-43.8249623840156,
2.66904964539909));
#236591=CARTESIAN_POINT('Ctrl Pts',(-39.5520968239709,-43.8286919494557,
2.66640203566656));
#236592=CARTESIAN_POINT('Ctrl Pts',(-39.5486547305939,-43.83023871141,2.66530399299378));
#236593=CARTESIAN_POINT('Ctrl Pts',(-39.5452359574124,-43.8319130705228,
2.66430995142202));
#236594=CARTESIAN_POINT('Ctrl Pts',(-39.5418537500312,-43.8337144555751,
2.66343053473307));
#236595=CARTESIAN_POINT('Ctrl Pts',(-39.5360850428915,-43.8367869054996,
2.66193059792831));
#236596=CARTESIAN_POINT('Ctrl Pts',(-39.5304250803196,-43.8402296473864,
2.66076519817074));
#236597=CARTESIAN_POINT('Ctrl Pts',(-39.52494648469,-43.844037892994,2.65997805604407));
#236598=CARTESIAN_POINT('Ctrl Pts',(-39.5222071868751,-43.8459420157977,
2.65958448498073));
#236599=CARTESIAN_POINT('Ctrl Pts',(-39.519514147613,-43.8479386338065,
2.65928526260709));
#236600=CARTESIAN_POINT('Ctrl Pts',(-39.5168765098746,-43.850027157078,
2.65908463971271));
#236601=CARTESIAN_POINT('Ctrl Pts',(-39.5142388721361,-43.8521156803494,
2.65888401681833));
#236602=CARTESIAN_POINT('Ctrl Pts',(-39.5116566557594,-43.8542960677575,
2.6587819886023));
#236603=CARTESIAN_POINT('Ctrl Pts',(-39.5091373124618,-43.8565665267058,
2.6587819886023));
#236604=CARTESIAN_POINT('Origin',(-34.2342565846632,-47.1453396605409,2.83404198860228));
#236605=CARTESIAN_POINT('Ctrl Pts',(-36.6746059268174,-50.8023624960592,
2.83404198860226));
#236606=CARTESIAN_POINT('Ctrl Pts',(-36.6808425220334,-50.8109464329599,
2.82419652440042));
#236607=CARTESIAN_POINT('Ctrl Pts',(-36.6877379133663,-50.8190128116684,
2.81438790575641));
#236608=CARTESIAN_POINT('Ctrl Pts',(-36.6952462569237,-50.8265243508954,
2.8046678125691));
#236609=CARTESIAN_POINT('Ctrl Pts',(-36.7025106240248,-50.8337918098259,
2.795263564531));
#236610=CARTESIAN_POINT('Ctrl Pts',(-36.7103497152243,-50.8405407635276,
2.78594102496269));
#236611=CARTESIAN_POINT('Ctrl Pts',(-36.7187568768212,-50.8467071440068,
2.7767510908883));
#236612=CARTESIAN_POINT('Ctrl Pts',(-36.7267095340086,-50.8525401602362,
2.76805797913748));
#236613=CARTESIAN_POINT('Ctrl Pts',(-36.7351712462818,-50.8578524412743,
2.75948271210241));
#236614=CARTESIAN_POINT('Ctrl Pts',(-36.7441560526521,-50.8625525281331,
2.75108575573316));
#236615=CARTESIAN_POINT('Ctrl Pts',(-36.7524317091168,-50.8668816480489,
2.74335155163377));
#236616=CARTESIAN_POINT('Ctrl Pts',(-36.7611516658457,-50.8706916079189,
2.73576818686063));
#236617=CARTESIAN_POINT('Ctrl Pts',(-36.7703354510156,-50.8738736606201,
2.72840626160628));
#236618=CARTESIAN_POINT('Ctrl Pts',(-36.7729993179918,-50.8747966531499,
2.72627084693754));
#236619=CARTESIAN_POINT('Ctrl Pts',(-36.775702242457,-50.8756665488981,
2.72415424587541));
#236620=CARTESIAN_POINT('Ctrl Pts',(-36.7784447603815,-50.8764799968254,
2.72205867173221));
#236621=CARTESIAN_POINT('Ctrl Pts',(-36.7814178261389,-50.8773618266783,
2.71978693462824));
#236622=CARTESIAN_POINT('Ctrl Pts',(-36.7844329791243,-50.8781771258725,
2.71754411340724));
#236623=CARTESIAN_POINT('Ctrl Pts',(-36.7874899206171,-50.8789219044954,
2.71533341844221));
#236624=CARTESIAN_POINT('Ctrl Pts',(-36.7958797205313,-50.8809659552704,
2.70926614876368));
#236625=CARTESIAN_POINT('Ctrl Pts',(-36.80458376171,-50.8824343655144,2.70347381860386));
#236626=CARTESIAN_POINT('Ctrl Pts',(-36.8135226609474,-50.8832604021662,
2.69804914171372));
#236627=CARTESIAN_POINT('Ctrl Pts',(-36.8217012684456,-50.8840161808561,
2.69308585687176));
#236628=CARTESIAN_POINT('Ctrl Pts',(-36.8300699399856,-50.8842246658555,
2.68842799053152));
#236629=CARTESIAN_POINT('Ctrl Pts',(-36.8385876480148,-50.8838072802928,
2.68414767054181));
#236630=CARTESIAN_POINT('Ctrl Pts',(-36.8427715183743,-50.8836022618679,
2.6820451913452));
#236631=CARTESIAN_POINT('Ctrl Pts',(-36.8469911418446,-50.883245770697,
2.68003431778475));
#236632=CARTESIAN_POINT('Ctrl Pts',(-36.8512399286213,-50.8827256259725,
2.6781269394523));
#236633=CARTESIAN_POINT('Ctrl Pts',(-36.8520460945285,-50.8826269335773,
2.67776503299182));
#236634=CARTESIAN_POINT('Ctrl Pts',(-36.8528536453862,-50.8825219362259,
2.67740659639902));
#236635=CARTESIAN_POINT('Ctrl Pts',(-36.8536624499709,-50.8824105850807,
2.67705178968834));
#236636=CARTESIAN_POINT('Ctrl Pts',(-36.8544459794125,-50.8823027136588,
2.67670807068736));
#236637=CARTESIAN_POINT('Ctrl Pts',(-36.8552306854274,-50.8821888793658,
2.67636775825244));
#236638=CARTESIAN_POINT('Ctrl Pts',(-36.8560164456182,-50.8820690400776,
2.67603099699234));
#236639=CARTESIAN_POINT('Ctrl Pts',(-36.864579498267,-50.8807630562081,
2.67236104217116));
#236640=CARTESIAN_POINT('Ctrl Pts',(-36.8732733195866,-50.8787426509999,
2.66911440541469));
#236641=CARTESIAN_POINT('Ctrl Pts',(-36.8819119966099,-50.875966462067,
2.66646778189629));
#236642=CARTESIAN_POINT('Ctrl Pts',(-36.8855601635608,-50.8747940602413,
2.66535009634964));
#236643=CARTESIAN_POINT('Ctrl Pts',(-36.8891983713642,-50.8734872887379,
2.66433897912328));
#236644=CARTESIAN_POINT('Ctrl Pts',(-36.8928125648613,-50.8720449698705,
2.66344564884771));
#236645=CARTESIAN_POINT('Ctrl Pts',(-36.8988987764012,-50.8696161409375,
2.66194130298563));
#236646=CARTESIAN_POINT('Ctrl Pts',(-36.9049145742144,-50.8668019052537,
2.66077206705397));
#236647=CARTESIAN_POINT('Ctrl Pts',(-36.9107858666116,-50.8635979627952,
2.65998225155691));
#236648=CARTESIAN_POINT('Ctrl Pts',(-36.9122536897109,-50.8627969771806,
2.65978479768265));
#236649=CARTESIAN_POINT('Ctrl Pts',(-36.9137123559378,-50.8619714372919,
2.65961098966599));
#236650=CARTESIAN_POINT('Ctrl Pts',(-36.9151605322317,-50.8611210221659,
2.65946139030478));
#236651=CARTESIAN_POINT('Ctrl Pts',(-36.9173327966725,-50.8598453994769,
2.65923699126297));
#236652=CARTESIAN_POINT('Ctrl Pts',(-36.9194814382212,-50.8585138058058,
2.65906707562418));
#236653=CARTESIAN_POINT('Ctrl Pts',(-36.9216029292227,-50.857126526261,
2.65895332562896));
#236654=CARTESIAN_POINT('Ctrl Pts',(-36.9237244202241,-50.8557392467161,
2.65883957563374));
#236655=CARTESIAN_POINT('Ctrl Pts',(-36.9258187603126,-50.8542962928971,
2.65878198860226));
#236656=CARTESIAN_POINT('Ctrl Pts',(-36.9278827595322,-50.8527980281386,
2.65878198860226));
#236657=CARTESIAN_POINT('Ctrl Pts',(-34.6837837831342,-47.7640607692764,
2.65878198860228));
#236658=CARTESIAN_POINT('Ctrl Pts',(-34.6767997090226,-47.7691302463542,
2.65878198860228));
#236659=CARTESIAN_POINT('Ctrl Pts',(-34.6702946353243,-47.7747322888381,
2.65945335517822));
#236660=CARTESIAN_POINT('Ctrl Pts',(-34.6643211616154,-47.7807252357991,
2.66072561226571));
#236661=CARTESIAN_POINT('Ctrl Pts',(-34.6604629105134,-47.7845960646239,
2.66154735980309));
#236662=CARTESIAN_POINT('Ctrl Pts',(-34.656825764279,-47.7886293194336,
2.66261895766852));
#236663=CARTESIAN_POINT('Ctrl Pts',(-34.6534164822759,-47.792781989761,
2.66391429250994));
#236664=CARTESIAN_POINT('Ctrl Pts',(-34.6488976742765,-47.7982861164004,
2.66563118464091));
#236665=CARTESIAN_POINT('Ctrl Pts',(-34.6447843113771,-47.8040027249064,
2.66774105138666));
#236666=CARTESIAN_POINT('Ctrl Pts',(-34.6410949611629,-47.8098436832079,
2.67016894181716));
#236667=CARTESIAN_POINT('Ctrl Pts',(-34.6392502860558,-47.8127641623586,
2.67138288703241));
#236668=CARTESIAN_POINT('Ctrl Pts',(-34.6375114518663,-47.8157158446827,
2.67267613167517));
#236669=CARTESIAN_POINT('Ctrl Pts',(-34.635879631104,-47.8186885387638,
2.67403835432519));
#236670=CARTESIAN_POINT('Ctrl Pts',(-34.6350637207229,-47.8201748858043,
2.67471946565019));
#236671=CARTESIAN_POINT('Ctrl Pts',(-34.6342745503768,-47.8216664954025,
2.67541781389488));
#236672=CARTESIAN_POINT('Ctrl Pts',(-34.6335121829165,-47.8231621539166,
2.67613207244134));
#236673=CARTESIAN_POINT('Ctrl Pts',(-34.6333215910514,-47.8235360685451,
2.67631063707796));
#236674=CARTESIAN_POINT('Ctrl Pts',(-34.6331326740828,-47.8239102364347,
2.67649019601811));
#236675=CARTESIAN_POINT('Ctrl Pts',(-34.6329454324197,-47.8242846390326,
2.67667072836622));
#236676=CARTESIAN_POINT('Ctrl Pts',(-34.6323837074303,-47.8254078468265,
2.67721232541055));
#236677=CARTESIAN_POINT('Ctrl Pts',(-34.6318370616125,-47.8265331659851,
2.67776268340012));
#236678=CARTESIAN_POINT('Ctrl Pts',(-34.6313054933181,-47.8276601046326,
2.67832123541481));
#236679=CARTESIAN_POINT('Ctrl Pts',(-34.6275611948901,-47.8355981149513,
2.68225560368403));
#236680=CARTESIAN_POINT('Ctrl Pts',(-34.6245119115564,-47.8436253243396,
2.68661792998839));
#236681=CARTESIAN_POINT('Ctrl Pts',(-34.6220808005808,-47.8516500154446,
2.6913098662252));
#236682=CARTESIAN_POINT('Ctrl Pts',(-34.6209017143846,-47.8555419819592,
2.69358545023004));
#236683=CARTESIAN_POINT('Ctrl Pts',(-34.619868341351,-47.859433847954,2.69593918853427));
#236684=CARTESIAN_POINT('Ctrl Pts',(-34.6189736992136,-47.8633173872849,
2.69836306235441));
#236685=CARTESIAN_POINT('Ctrl Pts',(-34.6176040646081,-47.8692628146652,
2.70207384382174));
#236686=CARTESIAN_POINT('Ctrl Pts',(-34.6165592825242,-47.8751852090114,
2.70594760814175));
#236687=CARTESIAN_POINT('Ctrl Pts',(-34.6158190596249,-47.8810431641657,
2.70995196345655));
#236688=CARTESIAN_POINT('Ctrl Pts',(-34.615475296281,-47.8837636288444,
2.71181160678053));
#236689=CARTESIAN_POINT('Ctrl Pts',(-34.6151969889844,-47.8864700832047,
2.71369962772046));
#236690=CARTESIAN_POINT('Ctrl Pts',(-34.6149833323959,-47.8891582656052,
2.71561183138608));
#236691=CARTESIAN_POINT('Ctrl Pts',(-34.6149669564602,-47.8893643041943,
2.71575839426258));
#236692=CARTESIAN_POINT('Ctrl Pts',(-34.6149509280614,-47.8895702459311,
2.71590508903155));
#236693=CARTESIAN_POINT('Ctrl Pts',(-34.6149352461542,-47.8897760897956,
2.71605191409858));
#236694=CARTESIAN_POINT('Ctrl Pts',(-34.6147149626374,-47.8926675754933,
2.71811436362699));
#236695=CARTESIAN_POINT('Ctrl Pts',(-34.6145651177081,-47.8955400426775,
2.72020091026905));
#236696=CARTESIAN_POINT('Ctrl Pts',(-34.6144819591399,-47.8983891927624,
2.72230624862128));
#236697=CARTESIAN_POINT('Ctrl Pts',(-34.6141837673036,-47.9086057382627,
2.72985561753056));
#236698=CARTESIAN_POINT('Ctrl Pts',(-34.6147387685077,-47.9186013937337,
2.73770089914291));
#236699=CARTESIAN_POINT('Ctrl Pts',(-34.6160223355358,-47.9283423801887,
2.74574823347042));
#236700=CARTESIAN_POINT('Ctrl Pts',(-34.617432846754,-47.9390467457338,
2.75459144546981));
#236701=CARTESIAN_POINT('Ctrl Pts',(-34.6197230854582,-47.9494442419751,
2.76367911754214));
#236702=CARTESIAN_POINT('Ctrl Pts',(-34.6227799581214,-47.9594984812842,
2.77292162564658));
#236703=CARTESIAN_POINT('Ctrl Pts',(-34.6260806134271,-47.9703545364682,
2.78290121484624));
#236704=CARTESIAN_POINT('Ctrl Pts',(-34.6302752334093,-47.9808115517362,
2.79306229500042));
#236705=CARTESIAN_POINT('Ctrl Pts',(-34.6352786409533,-47.990818417994,
2.80331916685067));
#236706=CARTESIAN_POINT('Ctrl Pts',(-34.6402400750493,-48.0007413369266,
2.81348999408557));
#236707=CARTESIAN_POINT('Ctrl Pts',(-34.6459976651001,-48.0102227609131,
2.8237563596679));
#236708=CARTESIAN_POINT('Ctrl Pts',(-34.6525130919793,-48.0191904766737,
2.83404198860227));
#236709=CARTESIAN_POINT('Origin',(-0.0123294189942654,0.0089578472451312,
2.83404198860262));
#236710=CARTESIAN_POINT('Ctrl Pts',(-36.9525415975208,-50.8348823336487,
2.65878198860226));
#236711=CARTESIAN_POINT('Ctrl Pts',(-36.9594880792482,-50.829830979246,
2.65878198860226));
#236712=CARTESIAN_POINT('Ctrl Pts',(-36.9659508653429,-50.8242442388882,
2.65944603041811));
#236713=CARTESIAN_POINT('Ctrl Pts',(-36.9718804702594,-50.8182646381296,
2.66070439264023));
#236714=CARTESIAN_POINT('Ctrl Pts',(-36.9756692055205,-50.8144439579054,
2.66150842619549));
#236715=CARTESIAN_POINT('Ctrl Pts',(-36.9792409429412,-50.8104635307791,
2.66255428265325));
#236716=CARTESIAN_POINT('Ctrl Pts',(-36.9825899931424,-50.8063652005965,
2.66381699700618));
#236717=CARTESIAN_POINT('Ctrl Pts',(-36.9871607746746,-50.800771802234,
2.66554034873217));
#236718=CARTESIAN_POINT('Ctrl Pts',(-36.9913113073906,-50.7949560887231,
2.66766759643921));
#236719=CARTESIAN_POINT('Ctrl Pts',(-36.995023627142,-50.7890120203239,
2.67012012783097));
#236720=CARTESIAN_POINT('Ctrl Pts',(-36.9968797870177,-50.7860399861243,
2.67134639352685));
#236721=CARTESIAN_POINT('Ctrl Pts',(-36.9986265637267,-50.7830357420055,
2.6726537558496));
#236722=CARTESIAN_POINT('Ctrl Pts',(-37.0002629240967,-50.7800101622085,
2.67403135126888));
#236723=CARTESIAN_POINT('Ctrl Pts',(-37.0010811042817,-50.7784973723101,
2.67472014897852));
#236724=CARTESIAN_POINT('Ctrl Pts',(-37.0018716944997,-50.7769792382975,
2.67542649668581));
#236725=CARTESIAN_POINT('Ctrl Pts',(-37.0026346543981,-50.7754570554919,
2.6761489965605));
#236726=CARTESIAN_POINT('Ctrl Pts',(-37.0028253943726,-50.7750765097906,
2.67632962152917));
#236727=CARTESIAN_POINT('Ctrl Pts',(-37.0030144077536,-50.7746957108233,
2.67651125590898));
#236728=CARTESIAN_POINT('Ctrl Pts',(-37.0032016945186,-50.7743146783936,
2.67669387767471));
#236729=CARTESIAN_POINT('Ctrl Pts',(-37.0037635548135,-50.7731715811045,
2.67724174297192));
#236730=CARTESIAN_POINT('Ctrl Pts',(-37.0043098740552,-50.7720263837271,
2.67779849504695));
#236731=CARTESIAN_POINT('Ctrl Pts',(-37.0048406651179,-50.7708796113517,
2.67836353617956));
#236732=CARTESIAN_POINT('Ctrl Pts',(-37.008508760693,-50.7629547027164,
2.68226832098861));
#236733=CARTESIAN_POINT('Ctrl Pts',(-37.0114900453057,-50.7549442896465,
2.68659153751352));
#236734=CARTESIAN_POINT('Ctrl Pts',(-37.0138628466708,-50.7469376805976,
2.69123699486147));
#236735=CARTESIAN_POINT('Ctrl Pts',(-37.015042122436,-50.7429584178781,
2.69354577441179));
#236736=CARTESIAN_POINT('Ctrl Pts',(-37.0160707669655,-50.7389795822778,
2.69593478828072));
#236737=CARTESIAN_POINT('Ctrl Pts',(-37.0169563748086,-50.7350097117578,
2.69839565261167));
#236738=CARTESIAN_POINT('Ctrl Pts',(-37.0189101579882,-50.7262515844357,
2.70382468688992));
#236739=CARTESIAN_POINT('Ctrl Pts',(-37.0201796788541,-50.7175407334809,
2.70961155815034));
#236740=CARTESIAN_POINT('Ctrl Pts',(-37.0208019128471,-50.7090177292133,
2.71562701361713));
#236741=CARTESIAN_POINT('Ctrl Pts',(-37.0210292227715,-50.7059041682736,
2.71782453535804));
#236742=CARTESIAN_POINT('Ctrl Pts',(-37.0211776528888,-50.7028130194415,
2.72005051502349));
#236743=CARTESIAN_POINT('Ctrl Pts',(-37.0212513646532,-50.6997475881154,
2.72229986760063));
#236744=CARTESIAN_POINT('Ctrl Pts',(-37.02149895467,-50.6894511286646,2.72985520488837));
#236745=CARTESIAN_POINT('Ctrl Pts',(-37.0208967002923,-50.6793793407319,
2.73770845534507));
#236746=CARTESIAN_POINT('Ctrl Pts',(-37.0195682679083,-50.6695664063388,
2.74576706701705));
#236747=CARTESIAN_POINT('Ctrl Pts',(-37.0181081633552,-50.6587808290222,
2.75462443584983));
#236748=CARTESIAN_POINT('Ctrl Pts',(-37.0157708601097,-50.6483072759145,
2.76373036323138));
#236749=CARTESIAN_POINT('Ctrl Pts',(-37.0126680948709,-50.6381830571054,
2.77299664636776));
#236750=CARTESIAN_POINT('Ctrl Pts',(-37.0093262837658,-50.6272788396598,
2.78297683033423));
#236751=CARTESIAN_POINT('Ctrl Pts',(-37.0050963107884,-50.6167786802283,
2.79314401478829));
#236752=CARTESIAN_POINT('Ctrl Pts',(-37.0000610231249,-50.6067353452108,
2.80341452427853));
#236753=CARTESIAN_POINT('Ctrl Pts',(-36.9950937288462,-50.5968276291265,
2.813546347213));
#236754=CARTESIAN_POINT('Ctrl Pts',(-36.9893418170235,-50.5873633690981,
2.82378004209157));
#236755=CARTESIAN_POINT('Ctrl Pts',(-36.9828414016742,-50.5784163149358,
2.83404198860226));
#236756=CARTESIAN_POINT('Ctrl Pts',(-34.9607485668361,-47.7952442955503,
2.83404198860228));
#236757=CARTESIAN_POINT('Ctrl Pts',(-34.9545276336627,-47.7866819156019,
2.82422126442951));
#236758=CARTESIAN_POINT('Ctrl Pts',(-34.9476537221152,-47.7786409912508,
2.81442815028424));
#236759=CARTESIAN_POINT('Ctrl Pts',(-34.9401706643544,-47.7711595893163,
2.8047161816622));
#236760=CARTESIAN_POINT('Ctrl Pts',(-34.9329451136981,-47.7639356375059,
2.79533842146112));
#236761=CARTESIAN_POINT('Ctrl Pts',(-34.9251506707949,-47.7572325247348,
2.78603515650104));
#236762=CARTESIAN_POINT('Ctrl Pts',(-34.9167928415129,-47.7511153344865,
2.77685887346602));
#236763=CARTESIAN_POINT('Ctrl Pts',(-34.9088920753313,-47.7453326739165,
2.768184412164));
#236764=CARTESIAN_POINT('Ctrl Pts',(-34.9004871280264,-47.7400730704108,
2.75962261521426));
#236765=CARTESIAN_POINT('Ctrl Pts',(-34.8915635921214,-47.7354288821269,
2.75123537701441));
#236766=CARTESIAN_POINT('Ctrl Pts',(-34.8833451652563,-47.7311516626296,
2.74351087133876));
#236767=CARTESIAN_POINT('Ctrl Pts',(-34.8746863576787,-47.7273962447069,
2.73593399449582));
#236768=CARTESIAN_POINT('Ctrl Pts',(-34.8655676881406,-47.7242720089008,
2.72857657812293));
#236769=CARTESIAN_POINT('Ctrl Pts',(-34.8628486849585,-47.7233404248509,
2.7263827450812));
#236770=CARTESIAN_POINT('Ctrl Pts',(-34.8600887620236,-47.7224652397583,
2.72420861709476));
#236771=CARTESIAN_POINT('Ctrl Pts',(-34.8572873423617,-47.721650113202,
2.72205663736674));
#236772=CARTESIAN_POINT('Ctrl Pts',(-34.8545145463035,-47.7208433152299,
2.71992664556713));
#236773=CARTESIAN_POINT('Ctrl Pts',(-34.8517040509264,-47.7200959288449,
2.71782089927832));
#236774=CARTESIAN_POINT('Ctrl Pts',(-34.8488585612797,-47.7194121231166,
2.71574387311193));
#236775=CARTESIAN_POINT('Ctrl Pts',(-34.8486606914946,-47.7193645726036,
2.71559944077434));
#236776=CARTESIAN_POINT('Ctrl Pts',(-34.8484626496807,-47.719317317907,
2.71545515216016));
#236777=CARTESIAN_POINT('Ctrl Pts',(-34.8482644357605,-47.7192703603291,
2.71531100781677));
#236778=CARTESIAN_POINT('Ctrl Pts',(-34.8395740113843,-47.7172115680923,
2.70899119176037));
#236779=CARTESIAN_POINT('Ctrl Pts',(-34.8305531107004,-47.7157691359129,
2.70298296066798));
#236780=CARTESIAN_POINT('Ctrl Pts',(-34.8212734513098,-47.7150344641794,
2.69736727774102));
#236781=CARTESIAN_POINT('Ctrl Pts',(-34.8126231959641,-47.7143496224387,
2.69213248525406));
#236782=CARTESIAN_POINT('Ctrl Pts',(-34.8037473009127,-47.7142799923072,
2.68723866185455));
#236783=CARTESIAN_POINT('Ctrl Pts',(-34.7947186932886,-47.7149249376575,
2.68278595829557));
#236784=CARTESIAN_POINT('Ctrl Pts',(-34.791415911814,-47.7151608670104,
2.68115710172783));
#236785=CARTESIAN_POINT('Ctrl Pts',(-34.788092901115,-47.715492664483,2.67958763637771));
#236786=CARTESIAN_POINT('Ctrl Pts',(-34.7847540840176,-47.7159260651933,
2.67808378645311));
#236787=CARTESIAN_POINT('Ctrl Pts',(-34.7839512100458,-47.7160302835855,
2.67772216078546));
#236788=CARTESIAN_POINT('Ctrl Pts',(-34.7831469919154,-47.7161407719862,
2.6773640360351));
#236789=CARTESIAN_POINT('Ctrl Pts',(-34.78234155776,-47.7162575750188,2.67700956934426));
#236790=CARTESIAN_POINT('Ctrl Pts',(-34.781561293422,-47.7163707279567,
2.67666617973751));
#236791=CARTESIAN_POINT('Ctrl Pts',(-34.7807798878928,-47.7164898070135,
2.67632622314065));
#236792=CARTESIAN_POINT('Ctrl Pts',(-34.7799974607185,-47.7166148505127,
2.6759898415872));
#236793=CARTESIAN_POINT('Ctrl Pts',(-34.7714250667934,-47.717984846556,
2.6723043929217));
#236794=CARTESIAN_POINT('Ctrl Pts',(-34.7627244668153,-47.7200720995233,
2.66904964539926));
#236795=CARTESIAN_POINT('Ctrl Pts',(-34.7540804826577,-47.7229136891077,
2.66640203566677));
#236796=CARTESIAN_POINT('Ctrl Pts',(-34.750495564778,-47.7240921810072,
2.66530399299389));
#236797=CARTESIAN_POINT('Ctrl Pts',(-34.7469205018085,-47.7254000086987,
2.66430995142206));
#236798=CARTESIAN_POINT('Ctrl Pts',(-34.7433685265017,-47.7268379886353,
2.66343053473306));
#236799=CARTESIAN_POINT('Ctrl Pts',(-34.7373102624742,-47.7292906132653,
2.66193059792829));
#236800=CARTESIAN_POINT('Ctrl Pts',(-34.7313214412506,-47.732122868262,
2.66076519817072));
#236801=CARTESIAN_POINT('Ctrl Pts',(-34.72547478788,-47.7353375827197,2.65997805604404));
#236802=CARTESIAN_POINT('Ctrl Pts',(-34.7225514611947,-47.7369449399485,
2.65958448498071));
#236803=CARTESIAN_POINT('Ctrl Pts',(-34.7196644712712,-47.7386491210193,
2.65928526260706));
#236804=CARTESIAN_POINT('Ctrl Pts',(-34.7168229726602,-47.7404504949223,
2.65908463971268));
#236805=CARTESIAN_POINT('Ctrl Pts',(-34.7139814740492,-47.7422518688253,
2.6588840168183));
#236806=CARTESIAN_POINT('Ctrl Pts',(-34.7111854907789,-47.7441503967333,
2.65878198860228));
#236807=CARTESIAN_POINT('Ctrl Pts',(-34.7084426211227,-47.7461450747865,
2.65878198860228));
#236808=CARTESIAN_POINT('Origin',(-29.1186878401551,-50.4655267888876,2.83404198860226));
#236809=CARTESIAN_POINT('Ctrl Pts',(-31.1634057161435,-54.3576020372439,
2.83404198860223));
#236810=CARTESIAN_POINT('Ctrl Pts',(-31.1687108809055,-54.3667908521543,
2.8241965244008));
#236811=CARTESIAN_POINT('Ctrl Pts',(-31.1747253323927,-54.375533807056,
2.81438790575706));
#236812=CARTESIAN_POINT('Ctrl Pts',(-31.1814073748063,-54.3837890328989,
2.80466781256992));
#236813=CARTESIAN_POINT('Ctrl Pts',(-31.1878722906305,-54.3917760130587,
2.79526356453192));
#236814=CARTESIAN_POINT('Ctrl Pts',(-31.194962980709,-54.3993074034423,
2.78594102496363));
#236815=CARTESIAN_POINT('Ctrl Pts',(-31.2026795247195,-54.4063187915261,
2.77675109088922));
#236816=CARTESIAN_POINT('Ctrl Pts',(-31.209978900196,-54.4129511329169,
2.76805797913831));
#236817=CARTESIAN_POINT('Ctrl Pts',(-31.2178389737506,-54.4191188025041,
2.75948271210313));
#236818=CARTESIAN_POINT('Ctrl Pts',(-31.2262832675548,-54.4247323097978,
2.75108575573377));
#236819=CARTESIAN_POINT('Ctrl Pts',(-31.2340610728554,-54.4299027559945,
2.74335155163424));
#236820=CARTESIAN_POINT('Ctrl Pts',(-31.2423350114986,-54.4346033281822,
2.73576818686097));
#236821=CARTESIAN_POINT('Ctrl Pts',(-31.2511358718536,-54.4387279162167,
2.72840626160653));
#236822=CARTESIAN_POINT('Ctrl Pts',(-31.2536886668971,-54.4399243024183,
2.72627084693769));
#236823=CARTESIAN_POINT('Ctrl Pts',(-31.2562858555936,-54.4410719653272,
2.72415424587548));
#236824=CARTESIAN_POINT('Ctrl Pts',(-31.2589283212562,-54.4421676282858,
2.7220586717322));
#236825=CARTESIAN_POINT('Ctrl Pts',(-31.261792923929,-54.4433553973773,
2.71978693462822));
#236826=CARTESIAN_POINT('Ctrl Pts',(-31.264706337619,-54.4444813995853,
2.71754411340722));
#236827=CARTESIAN_POINT('Ctrl Pts',(-31.2676686823014,-54.4455416356296,
2.71533341844219));
#236828=CARTESIAN_POINT('Ctrl Pts',(-31.2757988605275,-54.4484514617727,
2.70926614876367));
#236829=CARTESIAN_POINT('Ctrl Pts',(-31.2843017293917,-54.4508216479603,
2.70347381860383));
#236830=CARTESIAN_POINT('Ctrl Pts',(-31.293105316062,-54.4525775288975,
2.69804914171369));
#236831=CARTESIAN_POINT('Ctrl Pts',(-31.3011601199073,-54.454184064626,
2.69308585687188));
#236832=CARTESIAN_POINT('Ctrl Pts',(-31.3094611543721,-54.4552661718985,
2.68842799053176));
#236833=CARTESIAN_POINT('Ctrl Pts',(-31.3179758301767,-54.4557414157485,
2.68414767054214));
#236834=CARTESIAN_POINT('Ctrl Pts',(-31.3221582111178,-54.4559748539752,
2.68204519134541));
#236835=CARTESIAN_POINT('Ctrl Pts',(-31.3263919825236,-54.4560613864571,
2.68003431778483));
#236836=CARTESIAN_POINT('Ctrl Pts',(-31.3306718639309,-54.4559882102924,
2.67812693945226));
#236837=CARTESIAN_POINT('Ctrl Pts',(-31.3314839297413,-54.4559743258279,
2.67776503299178));
#236838=CARTESIAN_POINT('Ctrl Pts',(-31.3322980319626,-54.4559543157131,
2.67740659639898));
#236839=CARTESIAN_POINT('Ctrl Pts',(-31.3331140451953,-54.4559281176615,
2.6770517896883));
#236840=CARTESIAN_POINT('Ctrl Pts',(-31.3339045580146,-54.4559027382989,
2.67670807068732));
#236841=CARTESIAN_POINT('Ctrl Pts',(-31.3346968642516,-54.455871551716,
2.6763677582524));
#236842=CARTESIAN_POINT('Ctrl Pts',(-31.3354908465824,-54.4558345032251,
2.6760309969923));
#236843=CARTESIAN_POINT('Ctrl Pts',(-31.3441435024202,-54.4554307564062,
2.67236104217099));
#236844=CARTESIAN_POINT('Ctrl Pts',(-31.3530008879288,-54.4543301709715,
2.66911440541442));
#236845=CARTESIAN_POINT('Ctrl Pts',(-31.3618824321387,-54.4524721779259,
2.66646778189597));
#236846=CARTESIAN_POINT('Ctrl Pts',(-31.3656331634102,-54.4516875359252,
2.66535009634944));
#236847=CARTESIAN_POINT('Ctrl Pts',(-31.3693880355474,-54.4507682193236,
2.66433897912317));
#236848=CARTESIAN_POINT('Ctrl Pts',(-31.3731331934888,-54.4497115877221,
2.66344564884767));
#236849=CARTESIAN_POINT('Ctrl Pts',(-31.3794399458809,-54.4479322465076,
2.6619413029856));
#236850=CARTESIAN_POINT('Ctrl Pts',(-31.3857169562555,-54.4457622496021,
2.66077206705395));
#236851=CARTESIAN_POINT('Ctrl Pts',(-31.3918909882804,-54.4431895758478,
2.65998225155689));
#236852=CARTESIAN_POINT('Ctrl Pts',(-31.3934344962867,-54.4425464074092,
2.65978479768263));
#236853=CARTESIAN_POINT('Ctrl Pts',(-31.3949714642034,-54.4418778620535,
2.65961098966597));
#236854=CARTESIAN_POINT('Ctrl Pts',(-31.3965005998222,-54.441183481233,
2.65946139030476));
#236855=CARTESIAN_POINT('Ctrl Pts',(-31.3987943032505,-54.4401419100023,
2.65923699126295));
#236856=CARTESIAN_POINT('Ctrl Pts',(-31.4010703637561,-54.4390422051398,
2.65906707562416));
#236857=CARTESIAN_POINT('Ctrl Pts',(-31.4033252432067,-54.4378842814516,
2.65895332562894));
#236858=CARTESIAN_POINT('Ctrl Pts',(-31.4055801226574,-54.4367263577633,
2.65883957563371));
#236859=CARTESIAN_POINT('Ctrl Pts',(-31.4078138194778,-54.4355102267487,
2.65878198860223));
#236860=CARTESIAN_POINT('Ctrl Pts',(-31.4100231232065,-54.4342359163079,
2.65878198860223));
#236861=CARTESIAN_POINT('Ctrl Pts',(-29.5010785149107,-51.1278468659048,
2.65878198860225));
#236862=CARTESIAN_POINT('Ctrl Pts',(-29.4936027956394,-51.1321585373224,
2.65878198860225));
#236863=CARTESIAN_POINT('Ctrl Pts',(-29.4865477845236,-51.1370499258742,
2.65945335517818));
#236864=CARTESIAN_POINT('Ctrl Pts',(-29.4799806005925,-51.1423856448174,
2.66072561226564));
#236865=CARTESIAN_POINT('Ctrl Pts',(-29.475738873605,-51.1458319717784,
2.66154735980303));
#236866=CARTESIAN_POINT('Ctrl Pts',(-29.4717000621109,-51.1494629466898,
2.66261895766849));
#236867=CARTESIAN_POINT('Ctrl Pts',(-29.4678753842635,-51.1532365012461,
2.66391429250995));
#236868=CARTESIAN_POINT('Ctrl Pts',(-29.4628059928679,-51.1582381316478,
2.66563118464092));
#236869=CARTESIAN_POINT('Ctrl Pts',(-29.4581176150985,-51.1634934604716,
2.66774105138667));
#236870=CARTESIAN_POINT('Ctrl Pts',(-29.4538379291356,-51.168916779284,
2.67016894181718));
#236871=CARTESIAN_POINT('Ctrl Pts',(-29.4516980861541,-51.1716284386902,
2.67138288703243));
#236872=CARTESIAN_POINT('Ctrl Pts',(-29.4496602426628,-51.174382193724,
2.6726761316752));
#236873=CARTESIAN_POINT('Ctrl Pts',(-29.4477266300414,-51.1771680313592,
2.67403835432521));
#236874=CARTESIAN_POINT('Ctrl Pts',(-29.4467598237306,-51.1785609501768,
2.67471946565022));
#236875=CARTESIAN_POINT('Ctrl Pts',(-29.4458190608833,-51.179961897818,
2.6754178138949));
#236876=CARTESIAN_POINT('Ctrl Pts',(-29.4449045308656,-51.1813696738592,
2.67613207244136));
#236877=CARTESIAN_POINT('Ctrl Pts',(-29.4446758983612,-51.1817216178695,
2.67631063707798));
#236878=CARTESIAN_POINT('Ctrl Pts',(-29.4444489051049,-51.1820739888278,
2.67649019601813));
#236879=CARTESIAN_POINT('Ctrl Pts',(-29.444223553443,-51.1824267683259,
2.67667072836624));
#236880=CARTESIAN_POINT('Ctrl Pts',(-29.4435474984573,-51.1834851068199,
2.67721232541058));
#236881=CARTESIAN_POINT('Ctrl Pts',(-29.4428862193402,-51.1845471213153,
2.67776268340015));
#236882=CARTESIAN_POINT('Ctrl Pts',(-29.4422397658675,-51.185612322458,
2.67832123541484));
#236883=CARTESIAN_POINT('Ctrl Pts',(-29.437686231078,-51.1931154617649,
2.68225560368405));
#236884=CARTESIAN_POINT('Ctrl Pts',(-29.4338145801759,-51.2007799603593,
2.6866179299884));
#236885=CARTESIAN_POINT('Ctrl Pts',(-29.4305579784511,-51.2085065710724,
2.69130986622519));
#236886=CARTESIAN_POINT('Ctrl Pts',(-29.4289785301336,-51.2122539689191,
2.69358545023003));
#236887=CARTESIAN_POINT('Ctrl Pts',(-29.4275440072539,-51.2160164979697,
2.69593918853426));
#236888=CARTESIAN_POINT('Ctrl Pts',(-29.4262483256615,-51.219785247298,
2.6983630623544));
#236889=CARTESIAN_POINT('Ctrl Pts',(-29.4242647276701,-51.2255549392044,
2.70207384382173));
#236890=CARTESIAN_POINT('Ctrl Pts',(-29.4226066102319,-51.231335680589,
2.70594760814172));
#236891=CARTESIAN_POINT('Ctrl Pts',(-29.4212581193009,-51.2370841708899,
2.70995196345652));
#236892=CARTESIAN_POINT('Ctrl Pts',(-29.4206318731364,-51.2397537995244,
2.71181160678049));
#236893=CARTESIAN_POINT('Ctrl Pts',(-29.4200721889211,-51.2424163366105,
2.71369962772043));
#236894=CARTESIAN_POINT('Ctrl Pts',(-29.4195787111903,-51.2450674596717,
2.71561183138605));
#236895=CARTESIAN_POINT('Ctrl Pts',(-29.4195408880667,-51.2452706578084,
2.71575839426256));
#236896=CARTESIAN_POINT('Ctrl Pts',(-29.4195034206998,-51.245473795951,
2.71590508903153));
#236897=CARTESIAN_POINT('Ctrl Pts',(-29.4194663081569,-51.2456768729756,
2.71605191409856));
#236898=CARTESIAN_POINT('Ctrl Pts',(-29.4189449888197,-51.2485294929146,
2.71811436362697));
#236899=CARTESIAN_POINT('Ctrl Pts',(-29.4184957101761,-51.2513705613628,
2.72020091026903));
#236900=CARTESIAN_POINT('Ctrl Pts',(-29.4181151898793,-51.2541954110681,
2.72230624862126));
#236901=CARTESIAN_POINT('Ctrl Pts',(-29.4167507117681,-51.264324819728,
2.72985561752999));
#236902=CARTESIAN_POINT('Ctrl Pts',(-29.4162578421117,-51.2743237313747,
2.73770089914175));
#236903=CARTESIAN_POINT('Ctrl Pts',(-29.4165161672804,-51.2841455249749,
2.74574823346864));
#236904=CARTESIAN_POINT('Ctrl Pts',(-29.4168000406897,-51.2949386894546,
2.75459144546713));
#236905=CARTESIAN_POINT('Ctrl Pts',(-29.4179908989225,-51.3055186222547,
2.7636791175385));
#236906=CARTESIAN_POINT('Ctrl Pts',(-29.4199800715326,-51.3158373135899,
2.77292162564196));
#236907=CARTESIAN_POINT('Ctrl Pts',(-29.4221278787371,-51.3269789105929,
2.78290121483999));
#236908=CARTESIAN_POINT('Ctrl Pts',(-29.4252064644148,-51.3378170984163,
2.79306229499247));
#236909=CARTESIAN_POINT('Ctrl Pts',(-29.4291364604156,-51.348292144514,
2.80331916684103));
#236910=CARTESIAN_POINT('Ctrl Pts',(-29.43303348779,-51.3586793157436,2.81348999407907));
#236911=CARTESIAN_POINT('Ctrl Pts',(-29.4377684584824,-51.3687106315409,
2.82375635966462));
#236912=CARTESIAN_POINT('Ctrl Pts',(-29.4433108116256,-51.3783102687786,
2.83404198860225));
#236913=CARTESIAN_POINT('Origin',(-0.0131982271536665,0.00762000000019421,
2.83404198860262));
#236914=CARTESIAN_POINT('Ctrl Pts',(-31.436419577513,-54.4189959163064,
2.65878198860223));
#236915=CARTESIAN_POINT('Ctrl Pts',(-31.4438560159997,-54.4146983388118,
2.65878198860223));
#236916=CARTESIAN_POINT('Ctrl Pts',(-31.45086737166,-54.4098177483013,2.65944603041804));
#236917=CARTESIAN_POINT('Ctrl Pts',(-31.4573895320584,-54.4044907169111,
2.66070439264011));
#236918=CARTESIAN_POINT('Ctrl Pts',(-31.461556882064,-54.4010869974475,
2.66150842619537));
#236919=CARTESIAN_POINT('Ctrl Pts',(-31.4655251210642,-54.3975017237412,
2.66255428265315));
#236920=CARTESIAN_POINT('Ctrl Pts',(-31.4692842169741,-54.3937759157109,
2.6638169970061));
#236921=CARTESIAN_POINT('Ctrl Pts',(-31.4744146286221,-54.3886909353394,
2.6655403487321));
#236922=CARTESIAN_POINT('Ctrl Pts',(-31.4791503318816,-54.3833409297222,
2.66766759643914));
#236923=CARTESIAN_POINT('Ctrl Pts',(-31.4834636394924,-54.3778174666303,
2.6701201278309));
#236924=CARTESIAN_POINT('Ctrl Pts',(-31.4856202932977,-54.3750557350844,
2.67134639352678));
#236925=CARTESIAN_POINT('Ctrl Pts',(-31.4876715300022,-54.3722505364143,
2.67265375584955));
#236926=CARTESIAN_POINT('Ctrl Pts',(-31.4896151854255,-54.3694125772948,
2.67403135126882));
#236927=CARTESIAN_POINT('Ctrl Pts',(-31.4905870131372,-54.3679935977351,
2.67472014897846));
#236928=CARTESIAN_POINT('Ctrl Pts',(-31.4915319606347,-54.3665664194,2.67542649668576));
#236929=CARTESIAN_POINT('Ctrl Pts',(-31.4924498523884,-54.3651323262969,
2.67614899656045));
#236930=CARTESIAN_POINT('Ctrl Pts',(-31.4926793253268,-54.3647738030211,
2.67632962152913));
#236931=CARTESIAN_POINT('Ctrl Pts',(-31.4929071076035,-54.3644148473886,
2.67651125590894));
#236932=CARTESIAN_POINT('Ctrl Pts',(-31.4931331971263,-54.3640554790922,
2.67669387767467));
#236933=CARTESIAN_POINT('Ctrl Pts',(-31.4938114656948,-54.3629773742029,
2.67724174297187));
#236934=CARTESIAN_POINT('Ctrl Pts',(-31.4944744978645,-54.3618955562473,
2.67779849504691));
#236935=CARTESIAN_POINT('Ctrl Pts',(-31.4951222515523,-54.360810548785,
2.67836353617953));
#236936=CARTESIAN_POINT('Ctrl Pts',(-31.4995986314372,-54.3533124740222,
2.68226832098851));
#236937=CARTESIAN_POINT('Ctrl Pts',(-31.5034009004291,-54.3456575719325,
2.68659153751332));
#236938=CARTESIAN_POINT('Ctrl Pts',(-31.5065976218799,-54.3379428492062,
2.69123699486118));
#236939=CARTESIAN_POINT('Ctrl Pts',(-31.5081863836661,-54.3341086531876,
2.69354577441158));
#236940=CARTESIAN_POINT('Ctrl Pts',(-31.5096252947442,-54.3302591366968,
2.6959347882806));
#236941=CARTESIAN_POINT('Ctrl Pts',(-31.5109210155997,-54.3264035847697,
2.69839565261164));
#236942=CARTESIAN_POINT('Ctrl Pts',(-31.5137795693408,-54.3178976613387,
2.7038246868899));
#236943=CARTESIAN_POINT('Ctrl Pts',(-31.5159526675026,-54.3093672304021,
2.70961155815031));
#236944=CARTESIAN_POINT('Ctrl Pts',(-31.5174623893712,-54.3009559572067,
2.71562701361712));
#236945=CARTESIAN_POINT('Ctrl Pts',(-31.5180139098084,-54.2978832130367,
2.71782453535803));
#236946=CARTESIAN_POINT('Ctrl Pts',(-31.5184846398471,-54.2948245130135,
2.72005051502347));
#236947=CARTESIAN_POINT('Ctrl Pts',(-31.5188783726365,-54.2917835794184,
2.72229986760061));
#236948=CARTESIAN_POINT('Ctrl Pts',(-31.5202008794128,-54.2815694052538,
2.72985520488829));
#236949=CARTESIAN_POINT('Ctrl Pts',(-31.5206547127626,-54.2714898389048,
2.73770845534488));
#236950=CARTESIAN_POINT('Ctrl Pts',(-31.5203592886225,-54.2615918017974,
2.74576706701677));
#236951=CARTESIAN_POINT('Ctrl Pts',(-31.5200345824971,-54.2507126865167,
2.75462443584947));
#236952=CARTESIAN_POINT('Ctrl Pts',(-31.5188048676548,-54.2400521939124,
2.76373036323094));
#236953=CARTESIAN_POINT('Ctrl Pts',(-31.5167773687225,-54.229659109351,
2.77299664636724));
#236954=CARTESIAN_POINT('Ctrl Pts',(-31.514593665501,-54.21846531197,2.7829768303337));
#236955=CARTESIAN_POINT('Ctrl Pts',(-31.5114844302875,-54.2075805209355,
2.79314401478776));
#236956=CARTESIAN_POINT('Ctrl Pts',(-31.5075265408322,-54.1970658734764,
2.80341452427803));
#236957=CARTESIAN_POINT('Ctrl Pts',(-31.5036220962481,-54.1866932092599,
2.81354634721262));
#236958=CARTESIAN_POINT('Ctrl Pts',(-31.4988909785568,-54.1766795569344,
2.82378004209134));
#236959=CARTESIAN_POINT('Ctrl Pts',(-31.4933613949854,-54.1671020372439,
2.83404198860223));
#236960=CARTESIAN_POINT('Ctrl Pts',(-29.7732664904675,-51.1878102687786,
2.83404198860225));
#236961=CARTESIAN_POINT('Ctrl Pts',(-29.7679746486351,-51.1786445298593,
2.82422126443012));
#236962=CARTESIAN_POINT('Ctrl Pts',(-29.7619788985604,-51.169929135123,
2.81442815028548));
#236963=CARTESIAN_POINT('Ctrl Pts',(-29.7553188532208,-51.1617065245633,
2.80471618166407));
#236964=CARTESIAN_POINT('Ctrl Pts',(-29.7488879934689,-51.1537668706107,
2.79533842146347));
#236965=CARTESIAN_POINT('Ctrl Pts',(-29.741836915417,-51.1462857370543,
2.78603515650385));
#236966=CARTESIAN_POINT('Ctrl Pts',(-29.734164291695,-51.1393284263634,
2.77685887346928));
#236967=CARTESIAN_POINT('Ctrl Pts',(-29.7269112593607,-51.1327515888657,
2.76818441216769));
#236968=CARTESIAN_POINT('Ctrl Pts',(-29.7191021335091,-51.1266422417928,
2.75962261521835));
#236969=CARTESIAN_POINT('Ctrl Pts',(-29.7107129315325,-51.1210907313634,
2.75123537701888));
#236970=CARTESIAN_POINT('Ctrl Pts',(-29.7029866172514,-51.1159778833914,
2.74351087134362));
#236971=CARTESIAN_POINT('Ctrl Pts',(-29.6947677915928,-51.1113379461912,
2.73593399450103));
#236972=CARTESIAN_POINT('Ctrl Pts',(-29.686025646649,-51.1072776647618,
2.72857657812844));
#236973=CARTESIAN_POINT('Ctrl Pts',(-29.6834189154979,-51.1060669708015,
2.72638274508483));
#236974=CARTESIAN_POINT('Ctrl Pts',(-29.6807655934602,-51.1049080895602,
2.72420861709655));
#236975=CARTESIAN_POINT('Ctrl Pts',(-29.6780647241923,-51.1038046002594,
2.72205663736672));
#236976=CARTESIAN_POINT('Ctrl Pts',(-29.6753914511533,-51.1027123859001,
2.71992664556711));
#236977=CARTESIAN_POINT('Ctrl Pts',(-29.6726744751142,-51.1016753170131,
2.71782089927829));
#236978=CARTESIAN_POINT('Ctrl Pts',(-29.6699160505195,-51.1006978225841,
2.7157438731119));
#236979=CARTESIAN_POINT('Ctrl Pts',(-29.6697242350678,-51.1006298495332,
2.71559944077431));
#236980=CARTESIAN_POINT('Ctrl Pts',(-29.6695322176085,-51.1005621526963,
2.71545515216013));
#236981=CARTESIAN_POINT('Ctrl Pts',(-29.6693399979284,-51.1004947333604,
2.71531100781675));
#236982=CARTESIAN_POINT('Ctrl Pts',(-29.6609123829947,-51.0975388226977,
2.70899119176026));
#236983=CARTESIAN_POINT('Ctrl Pts',(-29.6520916749676,-51.0951613514268,
2.70298296066779));
#236984=CARTESIAN_POINT('Ctrl Pts',(-29.6429396446294,-51.0934607157662,
2.69736727774075));
#236985=CARTESIAN_POINT('Ctrl Pts',(-29.6344083617419,-51.091875427762,
2.69213248525359));
#236986=CARTESIAN_POINT('Ctrl Pts',(-29.6255883681025,-51.0908783954019,
2.68723866185391));
#236987=CARTESIAN_POINT('Ctrl Pts',(-29.6165418049888,-51.0905760611937,
2.68278595829479));
#236988=CARTESIAN_POINT('Ctrl Pts',(-29.6132324551646,-51.090465463429,
2.68115710172733));
#236989=CARTESIAN_POINT('Ctrl Pts',(-29.6098929659864,-51.0904480940785,
2.67958763637747));
#236990=CARTESIAN_POINT('Ctrl Pts',(-29.6065271365688,-51.0905301191541,
2.6780837864531));
#236991=CARTESIAN_POINT('Ctrl Pts',(-29.6057177670362,-51.0905498434445,
2.67772216078545));
#236992=CARTESIAN_POINT('Ctrl Pts',(-29.6049064053142,-51.0905756628929,
2.67736403603509));
#236993=CARTESIAN_POINT('Ctrl Pts',(-29.6040931741699,-51.0906076352718,
2.67700956934425));
#236994=CARTESIAN_POINT('Ctrl Pts',(-29.6033053564988,-51.0906386085138,
2.67666617973749));
#236995=CARTESIAN_POINT('Ctrl Pts',(-29.60251578444,-51.0906753561239,2.67632622314064));
#236996=CARTESIAN_POINT('Ctrl Pts',(-29.6017245728789,-51.0907179287116,
2.67598984158719));
#236997=CARTESIAN_POINT('Ctrl Pts',(-29.5930559358434,-51.0911843606097,
2.67230439292164));
#236998=CARTESIAN_POINT('Ctrl Pts',(-29.5841848213171,-51.0923507190417,
2.66904964539915));
#236999=CARTESIAN_POINT('Ctrl Pts',(-29.5752911628165,-51.0942731997206,
2.66640203566664));
#237000=CARTESIAN_POINT('Ctrl Pts',(-29.5716026975449,-51.0950705097612,
2.66530399299381));
#237001=CARTESIAN_POINT('Ctrl Pts',(-29.5679105139258,-51.0959974771975,
2.66430995142202));
#237002=CARTESIAN_POINT('Ctrl Pts',(-29.5642276868785,-51.0970562972091,
2.66343053473304));
#237003=CARTESIAN_POINT('Ctrl Pts',(-29.5579462415717,-51.0988622250758,
2.66193059792828));
#237004=CARTESIAN_POINT('Ctrl Pts',(-29.551694176475,-51.1010529624041,
2.6607651981707));
#237005=CARTESIAN_POINT('Ctrl Pts',(-29.5455435225214,-51.1036389246279,
2.65997805604402));
#237006=CARTESIAN_POINT('Ctrl Pts',(-29.5424681955446,-51.1049319057398,
2.65958448498068));
#237007=CARTESIAN_POINT('Ctrl Pts',(-29.5394188854255,-51.1063249785082,
2.65928526260704));
#237008=CARTESIAN_POINT('Ctrl Pts',(-29.5364046579953,-51.1078194668131,
2.65908463971266));
#237009=CARTESIAN_POINT('Ctrl Pts',(-29.5333904305651,-51.109313955118,
2.65888401681828));
#237010=CARTESIAN_POINT('Ctrl Pts',(-29.5304113137788,-51.1109098228567,
2.65878198860225));
#237011=CARTESIAN_POINT('Ctrl Pts',(-29.527474969218,-51.1126068659048,
2.65878198860225));
#237012=CARTESIAN_POINT('Origin',(-23.6840886581931,-53.2328030451448,2.83404198860224));
#237013=CARTESIAN_POINT('Ctrl Pts',(-25.3107727110817,-57.317288315449,
2.83404198860221));
#237014=CARTESIAN_POINT('Ctrl Pts',(-25.3150883208942,-57.3269813337895,
2.82419652440052));
#237015=CARTESIAN_POINT('Ctrl Pts',(-25.3201559369465,-57.3363050752407,
2.81438790575664));
#237016=CARTESIAN_POINT('Ctrl Pts',(-25.3259384683613,-57.3452135417177,
2.80466781256942));
#237017=CARTESIAN_POINT('Ctrl Pts',(-25.3315331019378,-57.3538325360807,
2.7952635645314));
#237018=CARTESIAN_POINT('Ctrl Pts',(-25.3377977038111,-57.3620638476571,
2.78594102496314));
#237019=CARTESIAN_POINT('Ctrl Pts',(-25.3447390861644,-57.3698434251106,
2.77675109088879));
#237020=CARTESIAN_POINT('Ctrl Pts',(-25.3513052064448,-57.3772024263427,
2.76805797913801));
#237021=CARTESIAN_POINT('Ctrl Pts',(-25.3584775246701,-57.3841579102004,
2.75948271210298));
#237022=CARTESIAN_POINT('Ctrl Pts',(-25.3662887884584,-57.3906233351686,
2.75108575573376));
#237023=CARTESIAN_POINT('Ctrl Pts',(-25.3734835273323,-57.3965784591558,
2.74335155163439));
#237024=CARTESIAN_POINT('Ctrl Pts',(-25.3812207968865,-57.4021181432088,
2.73576818686127));
#237025=CARTESIAN_POINT('Ctrl Pts',(-25.3895423083587,-57.4071400767267,
2.72840626160694));
#237026=CARTESIAN_POINT('Ctrl Pts',(-25.3919560625129,-57.4085967487426,
2.72627084693796));
#237027=CARTESIAN_POINT('Ctrl Pts',(-25.3944190600979,-57.4100096047774,
2.72415424587559));
#237028=CARTESIAN_POINT('Ctrl Pts',(-25.396932522092,-57.4113754784547,
2.72205867173217));
#237029=CARTESIAN_POINT('Ctrl Pts',(-25.3996572764938,-57.4128561733381,
2.7197869346282));
#237030=CARTESIAN_POINT('Ctrl Pts',(-25.4024370309183,-57.414280541844,
2.7175441134072));
#237031=CARTESIAN_POINT('Ctrl Pts',(-25.4052723227222,-57.4156446191417,
2.71533341844218));
#237032=CARTESIAN_POINT('Ctrl Pts',(-25.4130538033262,-57.4193883399888,
2.70926614876365));
#237033=CARTESIAN_POINT('Ctrl Pts',(-25.4212623406652,-57.4226343338643,
2.70347381860382));
#237034=CARTESIAN_POINT('Ctrl Pts',(-25.4298341608305,-57.4253008212879,
2.69804914171368));
#237035=CARTESIAN_POINT('Ctrl Pts',(-25.4376769109069,-57.4277405125135,
2.69308585687178));
#237036=CARTESIAN_POINT('Ctrl Pts',(-25.4458193604262,-57.4296843862652,
2.6884279905316));
#237037=CARTESIAN_POINT('Ctrl Pts',(-25.4542377154367,-57.4310470526568,
2.68414767054192));
#237038=CARTESIAN_POINT('Ctrl Pts',(-25.4583727839181,-57.4317163899369,
2.68204519134526));
#237039=CARTESIAN_POINT('Ctrl Pts',(-25.4625743171737,-57.4322449980037,
2.68003431778476));
#237040=CARTESIAN_POINT('Ctrl Pts',(-25.4668384019346,-57.4326195921322,
2.67812693945226));
#237041=CARTESIAN_POINT('Ctrl Pts',(-25.4676474704853,-57.4326906677194,
2.67776503299178));
#237042=CARTESIAN_POINT('Ctrl Pts',(-25.4684592045961,-57.4327558640764,
2.67740659639898));
#237043=CARTESIAN_POINT('Ctrl Pts',(-25.469273486065,-57.4328151061496,
2.67705178968829));
#237044=CARTESIAN_POINT('Ctrl Pts',(-25.470062321238,-57.432872496908,2.67670807068732));
#237045=CARTESIAN_POINT('Ctrl Pts',(-25.4708535470242,-57.4329242997218,
2.67636775825239));
#237046=CARTESIAN_POINT('Ctrl Pts',(-25.4716470524585,-57.4329704479393,
2.67603099699229));
#237047=CARTESIAN_POINT('Ctrl Pts',(-25.4802945111768,-57.4334733617056,
2.67236104217099));
#237048=CARTESIAN_POINT('Ctrl Pts',(-25.489218417505,-57.4333046542889,
2.66911440541443));
#237049=CARTESIAN_POINT('Ctrl Pts',(-25.4982455208442,-57.4323852136913,
2.66646778189599));
#237050=CARTESIAN_POINT('Ctrl Pts',(-25.5020577226399,-57.4319969282175,
2.66535009634944));
#237051=CARTESIAN_POINT('Ctrl Pts',(-25.5058881199463,-57.4314751387427,
2.66433897912316));
#237052=CARTESIAN_POINT('Ctrl Pts',(-25.5097232095982,-57.430815771084,
2.66344564884766));
#237053=CARTESIAN_POINT('Ctrl Pts',(-25.5161814047437,-57.4297054124226,
2.66194130298559));
#237054=CARTESIAN_POINT('Ctrl Pts',(-25.5226508554405,-57.4282034292356,
2.66077206705393));
#237055=CARTESIAN_POINT('Ctrl Pts',(-25.5290599831059,-57.4262902109366,
2.65998225155687));
#237056=CARTESIAN_POINT('Ctrl Pts',(-25.5306622650222,-57.4258119063619,
2.6597847976826));
#237057=CARTESIAN_POINT('Ctrl Pts',(-25.5322606952865,-57.4253076802621,
2.65961098966595));
#237058=CARTESIAN_POINT('Ctrl Pts',(-25.5338540367005,-57.4247769415288,
2.65946139030474));
#237059=CARTESIAN_POINT('Ctrl Pts',(-25.5362440488216,-57.4239808334288,
2.65923699126293));
#237060=CARTESIAN_POINT('Ctrl Pts',(-25.5386225912889,-57.4231250659717,
2.65906707562414));
#237061=CARTESIAN_POINT('Ctrl Pts',(-25.5409861542577,-57.4222091845944,
2.65895332562892));
#237062=CARTESIAN_POINT('Ctrl Pts',(-25.5433497172266,-57.4212933032172,
2.65883957563369));
#237063=CARTESIAN_POINT('Ctrl Pts',(-25.5456982979275,-57.4203173191901,
2.65878198860221));
#237064=CARTESIAN_POINT('Ctrl Pts',(-25.5480287005713,-57.4192809246789,
2.65878198860221));
#237065=CARTESIAN_POINT('Ctrl Pts',(-23.9951532569802,-53.9314655730804,
2.65878198860223));
#237066=CARTESIAN_POINT('Ctrl Pts',(-23.9872677980937,-53.9349721992637,
2.65878198860223));
#237067=CARTESIAN_POINT('Ctrl Pts',(-23.9797401457382,-53.9390993428072,
2.6594533551782));
#237068=CARTESIAN_POINT('Ctrl Pts',(-23.9726512030262,-53.9437193744796,
2.66072561226572));
#237069=CARTESIAN_POINT('Ctrl Pts',(-23.968072473402,-53.9467034408971,
2.66154735980308));
#237070=CARTESIAN_POINT('Ctrl Pts',(-23.9636762467124,-53.949892354189,
2.6626189576685));
#237071=CARTESIAN_POINT('Ctrl Pts',(-23.9594780769918,-53.9532454491205,
2.66391429250989));
#237072=CARTESIAN_POINT('Ctrl Pts',(-23.9539136435129,-53.9576897843753,
2.66563118464085));
#237073=CARTESIAN_POINT('Ctrl Pts',(-23.9487016177216,-53.9624262550345,
2.66774105138661));
#237074=CARTESIAN_POINT('Ctrl Pts',(-23.9438784851449,-53.967372515342,
2.67016894181712));
#237075=CARTESIAN_POINT('Ctrl Pts',(-23.9414669188565,-53.9698456454958,
2.67138288703237));
#237076=CARTESIAN_POINT('Ctrl Pts',(-23.9391523931032,-53.9723713025228,
2.67267613167513));
#237077=CARTESIAN_POINT('Ctrl Pts',(-23.9369381736871,-53.9749397614921,
2.67403835432515));
#237078=CARTESIAN_POINT('Ctrl Pts',(-23.935831063979,-53.9762239909768,
2.67471946565016));
#237079=CARTESIAN_POINT('Ctrl Pts',(-23.9347490158249,-53.9775189275855,
2.67541781389485));
#237080=CARTESIAN_POINT('Ctrl Pts',(-23.9336923430321,-53.9788233972649,
2.67613207244132));
#237081=CARTESIAN_POINT('Ctrl Pts',(-23.9334281748339,-53.9791495146848,
2.67631063707793));
#237082=CARTESIAN_POINT('Ctrl Pts',(-23.9331655922757,-53.9794762280618,
2.67649019601808));
#237083=CARTESIAN_POINT('Ctrl Pts',(-23.932904599615,-53.9798035193339,
2.67667072836619));
#237084=CARTESIAN_POINT('Ctrl Pts',(-23.9321216216328,-53.9807853931503,
2.67721232541053));
#237085=CARTESIAN_POINT('Ctrl Pts',(-23.9313529543287,-53.9817724673291,
2.67776268340009));
#237086=CARTESIAN_POINT('Ctrl Pts',(-23.9305986983573,-53.9827642604005,
2.67832123541478));
#237087=CARTESIAN_POINT('Ctrl Pts',(-23.9252858166862,-53.9897503227314,
2.6822556036841));
#237088=CARTESIAN_POINT('Ctrl Pts',(-23.9206342168329,-53.9969681366816,
2.68661792998857));
#237089=CARTESIAN_POINT('Ctrl Pts',(-23.916587804369,-54.0043120126392,
2.69130986622551));
#237090=CARTESIAN_POINT('Ctrl Pts',(-23.9146252986966,-54.0078737845428,
2.69358545023024));
#237091=CARTESIAN_POINT('Ctrl Pts',(-23.9128053429038,-54.0114657535932,
2.69593918853435));
#237092=CARTESIAN_POINT('Ctrl Pts',(-23.911122817615,-54.0150784217124,
2.69836306235437));
#237093=CARTESIAN_POINT('Ctrl Pts',(-23.9085469889525,-54.0206091641931,
2.7020738438217));
#237094=CARTESIAN_POINT('Ctrl Pts',(-23.9062937028416,-54.0261849176039,
2.7059476081417));
#237095=CARTESIAN_POINT('Ctrl Pts',(-23.9043517182278,-54.0317609613886,
2.7099519634565));
#237096=CARTESIAN_POINT('Ctrl Pts',(-23.9034498505266,-54.0343505049689,
2.71181160678048));
#237097=CARTESIAN_POINT('Ctrl Pts',(-23.90261492141,-54.0369399534674,2.71369962772041));
#237098=CARTESIAN_POINT('Ctrl Pts',(-23.9018470291824,-54.0395249709302,
2.71561183138603));
#237099=CARTESIAN_POINT('Ctrl Pts',(-23.9017881732688,-54.0397231023333,
2.71575839426254));
#237100=CARTESIAN_POINT('Ctrl Pts',(-23.9017296774342,-54.0399212112575,
2.71590508903151));
#237101=CARTESIAN_POINT('Ctrl Pts',(-23.9016715408684,-54.0401192964879,
2.71605191409853));
#237102=CARTESIAN_POINT('Ctrl Pts',(-23.9008548973945,-54.0429017967672,
2.71811436362695));
#237103=CARTESIAN_POINT('Ctrl Pts',(-23.9001111074275,-54.045680339139,
2.72020091026901));
#237104=CARTESIAN_POINT('Ctrl Pts',(-23.899437394462,-54.0484499388202,
2.72230624862123));
#237105=CARTESIAN_POINT('Ctrl Pts',(-23.8970215795834,-54.0583812307203,
2.72985561753059));
#237106=CARTESIAN_POINT('Ctrl Pts',(-23.8954862390497,-54.0682738483759,
2.73770089914301));
#237107=CARTESIAN_POINT('Ctrl Pts',(-23.8947164920946,-54.0780688394969,
2.7457482334706));
#237108=CARTESIAN_POINT('Ctrl Pts',(-23.8938706175188,-54.0888325507449,
2.75459144547029));
#237109=CARTESIAN_POINT('Ctrl Pts',(-23.8939490479887,-54.0994790041486,
2.76367911754294));
#237110=CARTESIAN_POINT('Ctrl Pts',(-23.8948487267554,-54.1099490937704,
2.77292162564771));
#237111=CARTESIAN_POINT('Ctrl Pts',(-23.8958201540348,-54.1212541629284,
2.78290121484815));
#237112=CARTESIAN_POINT('Ctrl Pts',(-23.8977489757814,-54.1323547778572,
2.79306229500313));
#237113=CARTESIAN_POINT('Ctrl Pts',(-23.900562502383,-54.1431832370012,
2.8033191668542));
#237114=CARTESIAN_POINT('Ctrl Pts',(-23.903352426387,-54.1539208564978,
2.81348999408793));
#237115=CARTESIAN_POINT('Ctrl Pts',(-23.9070129003885,-54.164392158903,
2.82375635966906));
#237116=CARTESIAN_POINT('Ctrl Pts',(-23.911521456611,-54.174518541976,2.83404198860223));
#237117=CARTESIAN_POINT('Origin',(-0.0139224327744654,0.00619866644066967,
2.83404198860262));
#237118=CARTESIAN_POINT('Ctrl Pts',(-25.5758735661203,-57.406883591798,
2.65878198860221));
#237119=CARTESIAN_POINT('Ctrl Pts',(-25.58371848619,-57.4033868763698,2.65878198860221));
#237120=CARTESIAN_POINT('Ctrl Pts',(-25.5912015935362,-57.3992659084774,
2.65944603041801));
#237121=CARTESIAN_POINT('Ctrl Pts',(-25.5982448512625,-57.3946498105263,
2.66070439264004));
#237122=CARTESIAN_POINT('Ctrl Pts',(-25.6027451576538,-57.3917003436859,
2.66150842619531));
#237123=CARTESIAN_POINT('Ctrl Pts',(-25.6070664213765,-57.3885495044087,
2.66255428265311));
#237124=CARTESIAN_POINT('Ctrl Pts',(-25.6111943775536,-57.3852370392633,
2.66381699700609));
#237125=CARTESIAN_POINT('Ctrl Pts',(-25.6168282094538,-57.3807161889918,
2.66554034873209));
#237126=CARTESIAN_POINT('Ctrl Pts',(-25.622097197901,-57.3758905070493,
2.66766759643913));
#237127=CARTESIAN_POINT('Ctrl Pts',(-25.6269642358703,-57.3708481654824,
2.67012012783089));
#237128=CARTESIAN_POINT('Ctrl Pts',(-25.6293977548549,-57.3683269946989,
2.67134639352677));
#237129=CARTESIAN_POINT('Ctrl Pts',(-25.6317309777762,-57.3657515758211,
2.67265375584953));
#237130=CARTESIAN_POINT('Ctrl Pts',(-25.6339606331573,-57.3631323306532,
2.67403135126881));
#237131=CARTESIAN_POINT('Ctrl Pts',(-25.6350754608479,-57.3618227080692,
2.67472014897845));
#237132=CARTESIAN_POINT('Ctrl Pts',(-25.6361644125823,-57.3605021218762,
2.67542649668574));
#237133=CARTESIAN_POINT('Ctrl Pts',(-25.6372271795771,-57.3591718306996,
2.67614899656043));
#237134=CARTESIAN_POINT('Ctrl Pts',(-25.6374928713258,-57.3588392579054,
2.67632962152911));
#237135=CARTESIAN_POINT('Ctrl Pts',(-25.6377569268681,-57.3585060784008,
2.67651125590892));
#237136=CARTESIAN_POINT('Ctrl Pts',(-25.6380193420646,-57.3581723115519,
2.67669387767465));
#237137=CARTESIAN_POINT('Ctrl Pts',(-25.6388065876542,-57.3571710110051,
2.67724174297186));
#237138=CARTESIAN_POINT('Ctrl Pts',(-25.6395790684328,-57.3561644250953,
2.67779849504689));
#237139=CARTESIAN_POINT('Ctrl Pts',(-25.6403366878208,-57.355153070115,
2.67836353617951));
#237140=CARTESIAN_POINT('Ctrl Pts',(-25.6455723078605,-57.3481639797008,
2.68226832098838));
#237141=CARTESIAN_POINT('Ctrl Pts',(-25.6501539027769,-57.3409484573005,
2.68659153751308));
#237142=CARTESIAN_POINT('Ctrl Pts',(-25.6541395203641,-57.3336101450134,
2.6912369948608));
#237143=CARTESIAN_POINT('Ctrl Pts',(-25.6561203613648,-57.3299630239497,
2.69354577441131));
#237144=CARTESIAN_POINT('Ctrl Pts',(-25.6579537739807,-57.3262850026765,
2.69593478828045));
#237145=CARTESIAN_POINT('Ctrl Pts',(-25.6596454116599,-57.3225860115759,
2.69839565261162));
#237146=CARTESIAN_POINT('Ctrl Pts',(-25.6633774170493,-57.3144254847132,
2.70382468688988));
#237147=CARTESIAN_POINT('Ctrl Pts',(-25.6664302835889,-57.3061689349812,
2.70961155815029));
#237148=CARTESIAN_POINT('Ctrl Pts',(-25.6688109525044,-57.2979615485274,
2.7156270136171));
#237149=CARTESIAN_POINT('Ctrl Pts',(-25.669680640881,-57.2949632867553,
2.717824535358));
#237150=CARTESIAN_POINT('Ctrl Pts',(-25.6704685134243,-57.2919705472983,
2.72005051502344));
#237151=CARTESIAN_POINT('Ctrl Pts',(-25.67117795342,-57.2889874285391,2.72229986760058));
#237152=CARTESIAN_POINT('Ctrl Pts',(-25.6735608872947,-57.2789674482905,
2.72985520488809));
#237153=CARTESIAN_POINT('Ctrl Pts',(-25.6750658360787,-57.2689905373633,
2.73770845534447));
#237154=CARTESIAN_POINT('Ctrl Pts',(-25.6758066569111,-57.2591158425076,
2.74576706701612));
#237155=CARTESIAN_POINT('Ctrl Pts',(-25.6766209067619,-57.2482623831265,
2.75462443584862));
#237156=CARTESIAN_POINT('Ctrl Pts',(-25.6765122533357,-57.2375317496134,
2.76373036322987));
#237157=CARTESIAN_POINT('Ctrl Pts',(-25.6755822344126,-57.226983668109,
2.77299664636597));
#237158=CARTESIAN_POINT('Ctrl Pts',(-25.6745805641842,-57.2156229323793,
2.78297683033233));
#237159=CARTESIAN_POINT('Ctrl Pts',(-25.6726261321664,-57.2044727657902,
2.79314401478631));
#237160=CARTESIAN_POINT('Ctrl Pts',(-25.6697890043845,-57.1936020065676,
2.80341452427657));
#237161=CARTESIAN_POINT('Ctrl Pts',(-25.6669901874068,-57.1828780392983,
2.81354634721156));
#237162=CARTESIAN_POINT('Ctrl Pts',(-25.6633316989625,-57.1724247063459,
2.82378004209075));
#237163=CARTESIAN_POINT('Ctrl Pts',(-25.6588335304436,-57.1623216544371,
2.83404198860221));
#237164=CARTESIAN_POINT('Ctrl Pts',(-24.2595822759728,-54.0195518809641,
2.83404198860223));
#237165=CARTESIAN_POINT('Ctrl Pts',(-24.2552775040074,-54.0098832048265,
2.82422126442958));
#237166=CARTESIAN_POINT('Ctrl Pts',(-24.2502256060972,-54.0005888273926,
2.81442815028443));
#237167=CARTESIAN_POINT('Ctrl Pts',(-24.2444615420283,-53.9917150968488,
2.8047161816625));
#237168=CARTESIAN_POINT('Ctrl Pts',(-24.2388958310253,-53.9831467292637,
2.79533842146156));
#237169=CARTESIAN_POINT('Ctrl Pts',(-24.2326653709106,-53.9749695397864,
2.78603515650162));
#237170=CARTESIAN_POINT('Ctrl Pts',(-24.2257620156187,-53.9672483344043,
2.77685887346673));
#237171=CARTESIAN_POINT('Ctrl Pts',(-24.219236182871,-53.9599493771864,
2.76818441216492));
#237172=CARTESIAN_POINT('Ctrl Pts',(-24.2121084368886,-53.9530572218312,
2.75962261521538));
#237173=CARTESIAN_POINT('Ctrl Pts',(-24.2043454826918,-53.9466592127661,
2.75123537701573));
#237174=CARTESIAN_POINT('Ctrl Pts',(-24.1971959321099,-53.9407667537517,
2.74351087134032));
#237175=CARTESIAN_POINT('Ctrl Pts',(-24.189507135543,-53.935293133397,2.73593399449761));
#237176=CARTESIAN_POINT('Ctrl Pts',(-24.1812372959618,-53.9303412916376,
2.72857657812491));
#237177=CARTESIAN_POINT('Ctrl Pts',(-24.1787713967371,-53.9288647523849,
2.72638274508249));
#237178=CARTESIAN_POINT('Ctrl Pts',(-24.1762537459517,-53.9274348719419,
2.72420861709538));
#237179=CARTESIAN_POINT('Ctrl Pts',(-24.1736830183705,-53.9260551099576,
2.72205663736669));
#237180=CARTESIAN_POINT('Ctrl Pts',(-24.1711385572894,-53.9246894457401,
2.71992664556708));
#237181=CARTESIAN_POINT('Ctrl Pts',(-24.1685448683464,-53.9233740566949,
2.71782089927827));
#237182=CARTESIAN_POINT('Ctrl Pts',(-24.1659037306808,-53.9221135831988,
2.71574387311189));
#237183=CARTESIAN_POINT('Ctrl Pts',(-24.1657200711327,-53.922025932337,
2.71559944077429));
#237184=CARTESIAN_POINT('Ctrl Pts',(-24.1655361818115,-53.9219385350606,
2.71545515216012));
#237185=CARTESIAN_POINT('Ctrl Pts',(-24.1653520623704,-53.921851392627,
2.71531100781673));
#237186=CARTESIAN_POINT('Ctrl Pts',(-24.1572795915924,-53.9180307491142,
2.70899119176026));
#237187=CARTESIAN_POINT('Ctrl Pts',(-24.1487557177452,-53.9147442868247,
2.70298296066782));
#237188=CARTESIAN_POINT('Ctrl Pts',(-24.139831588019,-53.9120963197572,
2.6973672777408));
#237189=CARTESIAN_POINT('Ctrl Pts',(-24.1315127481107,-53.9096279542366,
2.69213248525367));
#237190=CARTESIAN_POINT('Ctrl Pts',(-24.1228452895799,-53.9077144433429,
2.68723866185402));
#237191=CARTESIAN_POINT('Ctrl Pts',(-24.1138798870158,-53.906468142013,
2.68278595829492));
#237192=CARTESIAN_POINT('Ctrl Pts',(-24.1106002267704,-53.9060122288629,
2.68115710172739));
#237193=CARTESIAN_POINT('Ctrl Pts',(-24.1072808472548,-53.9056458829916,
2.67958763637748));
#237194=CARTESIAN_POINT('Ctrl Pts',(-24.1039248822477,-53.9053756337486,
2.67808378645307));
#237195=CARTESIAN_POINT('Ctrl Pts',(-24.1031178847763,-53.9053106478339,
2.67772216078542));
#237196=CARTESIAN_POINT('Ctrl Pts',(-24.1023082689114,-53.9052515154466,
2.67736403603505));
#237197=CARTESIAN_POINT('Ctrl Pts',(-24.1014961507088,-53.9051983068757,
2.67700956934421));
#237198=CARTESIAN_POINT('Ctrl Pts',(-24.1007094112,-53.9051467610726,2.67666617973746));
#237199=CARTESIAN_POINT('Ctrl Pts',(-24.0999203233284,-53.9051007746215,
2.67632622314061));
#237200=CARTESIAN_POINT('Ctrl Pts',(-24.0991289960597,-53.9050604098634,
2.67598984158715));
#237201=CARTESIAN_POINT('Ctrl Pts',(-24.0904590913153,-53.9046181672909,
2.67230439292157));
#237202=CARTESIAN_POINT('Ctrl Pts',(-24.081514656028,-53.9048508523204,
2.66904964539907));
#237203=CARTESIAN_POINT('Ctrl Pts',(-24.0724687639682,-53.9058331609931,
2.66640203566655));
#237204=CARTESIAN_POINT('Ctrl Pts',(-24.0687171629021,-53.9062405536792,
2.66530399299374));
#237205=CARTESIAN_POINT('Ctrl Pts',(-24.0649483109695,-53.9067765048111,
2.66430995142197));
#237206=CARTESIAN_POINT('Ctrl Pts',(-24.0611749820056,-53.9074445642442,
2.66343053473301));
#237207=CARTESIAN_POINT('Ctrl Pts',(-24.0547391762487,-53.9085840092241,
2.66193059792825));
#237208=CARTESIAN_POINT('Ctrl Pts',(-24.0482923662124,-53.9101092267073,
2.66076519817067));
#237209=CARTESIAN_POINT('Ctrl Pts',(-24.0419050995274,-53.9120381043535,
2.65997805604399));
#237210=CARTESIAN_POINT('Ctrl Pts',(-24.0387114661849,-53.9130025431766,
2.65958448498065));
#237211=CARTESIAN_POINT('Ctrl Pts',(-24.0355332447499,-53.9140692448458,
2.65928526260701));
#237212=CARTESIAN_POINT('Ctrl Pts',(-24.0323793130071,-53.9152404736262,
2.65908463971264));
#237213=CARTESIAN_POINT('Ctrl Pts',(-24.0292253812643,-53.9164117024067,
2.65888401681826));
#237214=CARTESIAN_POINT('Ctrl Pts',(-24.0260957707892,-53.9176874253153,
2.65878198860223));
#237215=CARTESIAN_POINT('Ctrl Pts',(-24.0229981225292,-53.9190682401995,
2.65878198860223));
#237216=CARTESIAN_POINT('Origin',(-17.9900016446778,-55.4168495715592,2.83404198860222));
#237217=CARTESIAN_POINT('Ctrl Pts',(-19.1808295835776,-59.6489943884564,
2.83404198860219));
#237218=CARTESIAN_POINT('Ctrl Pts',(-19.1841083557165,-59.6590854114903,
2.82419652440032));
#237219=CARTESIAN_POINT('Ctrl Pts',(-19.1881736144721,-59.6688877866289,
2.81438790575622));
#237220=CARTESIAN_POINT('Ctrl Pts',(-19.1929932802641,-59.6783518907172,
2.80466781256879));
#237221=CARTESIAN_POINT('Ctrl Pts',(-19.197656335617,-59.6875084677777,
2.7952635645306));
#237222=CARTESIAN_POINT('Ctrl Pts',(-19.2030262129961,-59.6963495165751,
2.78594102496216));
#237223=CARTESIAN_POINT('Ctrl Pts',(-19.2091163824546,-59.7048120487197,
2.77675109088764));
#237224=CARTESIAN_POINT('Ctrl Pts',(-19.2148773077513,-59.7128170830358,
2.76805797913666));
#237225=CARTESIAN_POINT('Ctrl Pts',(-19.2212832892283,-59.7204841754274,
2.75948271210142));
#237226=CARTESIAN_POINT('Ctrl Pts',(-19.2283759411601,-59.7277306815212,
2.75108575573202));
#237227=CARTESIAN_POINT('Ctrl Pts',(-19.234908786543,-59.7344052377143,
2.74335155163246));
#237228=CARTESIAN_POINT('Ctrl Pts',(-19.2420246158643,-59.7407233396949,
2.73576818685916));
#237229=CARTESIAN_POINT('Ctrl Pts',(-19.249775606233,-59.7465875973418,
2.72840626160468));
#237230=CARTESIAN_POINT('Ctrl Pts',(-19.2520238739014,-59.7482885955678,
2.72627084693646));
#237231=CARTESIAN_POINT('Ctrl Pts',(-19.2543256952569,-59.7499511651814,
2.72415424587484));
#237232=CARTESIAN_POINT('Ctrl Pts',(-19.2566826155659,-59.7515722847789,
2.72205867173216));
#237233=CARTESIAN_POINT('Ctrl Pts',(-19.2592376687173,-59.7533296826512,
2.71978693462818));
#237234=CARTESIAN_POINT('Ctrl Pts',(-19.2618533083051,-59.7550368117758,
2.71754411340719));
#237235=CARTESIAN_POINT('Ctrl Pts',(-19.2645304831802,-59.7566897852104,
2.71533341844216));
#237236=CARTESIAN_POINT('Ctrl Pts',(-19.2718780106322,-59.7612263837724,
2.70926614876362));
#237237=CARTESIAN_POINT('Ctrl Pts',(-19.2797022819932,-59.7653126215476,
2.7034738186038));
#237238=CARTESIAN_POINT('Ctrl Pts',(-19.2879484209981,-59.7688605008634,
2.69804914171365));
#237239=CARTESIAN_POINT('Ctrl Pts',(-19.2954931904944,-59.7721066178185,
2.69308585687161));
#237240=CARTESIAN_POINT('Ctrl Pts',(-19.3033878446875,-59.774890960562,
2.6884279905313));
#237241=CARTESIAN_POINT('Ctrl Pts',(-19.3116176456448,-59.777126119837,
2.68414767054152));
#237242=CARTESIAN_POINT('Ctrl Pts',(-19.3156600969909,-59.7782240227713,
2.68204519134499));
#237243=CARTESIAN_POINT('Ctrl Pts',(-19.3197833592186,-59.7791889148824,
2.68003431778461));
#237244=CARTESIAN_POINT('Ctrl Pts',(-19.3239849291282,-59.7800071751722,
2.67812693945221));
#237245=CARTESIAN_POINT('Ctrl Pts',(-19.3247821360948,-59.7801624320923,
2.67776503299173));
#237246=CARTESIAN_POINT('Ctrl Pts',(-19.3255826085661,-59.7803121206159,
2.67740659639893));
#237247=CARTESIAN_POINT('Ctrl Pts',(-19.3263862368331,-59.7804561537454,
2.67705178968825));
#237248=CARTESIAN_POINT('Ctrl Pts',(-19.3271647517167,-59.7805956858397,
2.67670807068727));
#237249=CARTESIAN_POINT('Ctrl Pts',(-19.3279462282167,-59.7807299104878,
2.67636775825235));
#237250=CARTESIAN_POINT('Ctrl Pts',(-19.328730562943,-59.7808587498042,
2.67603099699224));
#237251=CARTESIAN_POINT('Ctrl Pts',(-19.3372780811741,-59.7822628141272,
2.6723610421711));
#237252=CARTESIAN_POINT('Ctrl Pts',(-19.3461707361363,-59.7830278331222,
2.66911440541466));
#237253=CARTESIAN_POINT('Ctrl Pts',(-19.3552444957713,-59.7830570185563,
2.66646778189628));
#237254=CARTESIAN_POINT('Ctrl Pts',(-19.3590764008109,-59.7830693437463,
2.6653500963496));
#237255=CARTESIAN_POINT('Ctrl Pts',(-19.3629403566525,-59.782950798233,
2.66433897912321));
#237256=CARTESIAN_POINT('Ctrl Pts',(-19.3668233599705,-59.7826959186871,
2.66344564884762));
#237257=CARTESIAN_POINT('Ctrl Pts',(-19.3733622405317,-59.7822667079006,
2.66194130298555));
#237258=CARTESIAN_POINT('Ctrl Pts',(-19.3799532508951,-59.7814491944742,
2.6607720670539));
#237259=CARTESIAN_POINT('Ctrl Pts',(-19.3865272544572,-59.7802163932508,
2.65998225155684));
#237260=CARTESIAN_POINT('Ctrl Pts',(-19.3881707553477,-59.779908192945,
2.65978479768258));
#237261=CARTESIAN_POINT('Ctrl Pts',(-19.3898131352231,-59.7795738105077,
2.65961098966592));
#237262=CARTESIAN_POINT('Ctrl Pts',(-19.3914532254503,-59.7792125287462,
2.65946139030472));
#237263=CARTESIAN_POINT('Ctrl Pts',(-19.3939133607912,-59.7786706061039,
2.6592369912629));
#237264=CARTESIAN_POINT('Ctrl Pts',(-19.3963683254113,-59.7780681520194,
2.65906707562412));
#237265=CARTESIAN_POINT('Ctrl Pts',(-19.3988146762077,-59.7774043475412,
2.6589533256289));
#237266=CARTESIAN_POINT('Ctrl Pts',(-19.4012610270042,-59.776740543063,
2.65883957563368));
#237267=CARTESIAN_POINT('Ctrl Pts',(-19.4036987600449,-59.7760153991101,
2.65878198860219));
#237268=CARTESIAN_POINT('Ctrl Pts',(-19.4061247292248,-59.7752282754837,
2.65878198860219));
#237269=CARTESIAN_POINT('Ctrl Pts',(-18.2263320786577,-56.1441998575527,
2.65878198860222));
#237270=CARTESIAN_POINT('Ctrl Pts',(-18.2181232748941,-56.1468630191712,
2.65878198860222));
#237271=CARTESIAN_POINT('Ctrl Pts',(-18.2102054558338,-56.1501806998576,
2.65945335517814));
#237272=CARTESIAN_POINT('Ctrl Pts',(-18.2026724222809,-56.1540344262251,
2.66072561226558));
#237273=CARTESIAN_POINT('Ctrl Pts',(-18.1978068555395,-56.1565235380433,
2.66154735980296));
#237274=CARTESIAN_POINT('Ctrl Pts',(-18.1931013796336,-56.1592354513146,
2.6626189576684));
#237275=CARTESIAN_POINT('Ctrl Pts',(-18.1885757140654,-56.1621313494119,
2.66391429250985));
#237276=CARTESIAN_POINT('Ctrl Pts',(-18.1825772036009,-56.1659696964527,
2.66563118464081));
#237277=CARTESIAN_POINT('Ctrl Pts',(-18.1768986338329,-56.1701354151835,
2.66774105138657));
#237278=CARTESIAN_POINT('Ctrl Pts',(-18.1715848978922,-56.1745504247232,
2.67016894181708));
#237279=CARTESIAN_POINT('Ctrl Pts',(-18.1689280299219,-56.1767579294931,
2.67138288703234));
#237280=CARTESIAN_POINT('Ctrl Pts',(-18.166362180335,-56.1790278168864,
2.6726761316751));
#237281=CARTESIAN_POINT('Ctrl Pts',(-18.1638916135754,-56.1813507566159,
2.67403835432512));
#237282=CARTESIAN_POINT('Ctrl Pts',(-18.1626563301957,-56.1825122264806,
2.67471946565013));
#237283=CARTESIAN_POINT('Ctrl Pts',(-18.1614448518808,-56.1836869644603,
2.67541781389482));
#237284=CARTESIAN_POINT('Ctrl Pts',(-18.1602576134412,-56.1848738357352,
2.67613207244129));
#237285=CARTESIAN_POINT('Ctrl Pts',(-18.1599608038313,-56.1851705535539,
2.6763106370779));
#237286=CARTESIAN_POINT('Ctrl Pts',(-18.1596655088806,-56.1854680298096,
2.67649019601805));
#237287=CARTESIAN_POINT('Ctrl Pts',(-18.1593717347113,-56.1857662469841,
2.67667072836617));
#237288=CARTESIAN_POINT('Ctrl Pts',(-18.1584904122033,-56.1866608985077,
2.6772123254105));
#237289=CARTESIAN_POINT('Ctrl Pts',(-18.157622778392,-56.1875622177789,
2.67776268340007));
#237290=CARTESIAN_POINT('Ctrl Pts',(-18.1567689837081,-56.1884697364864,
2.67832123541476));
#237291=CARTESIAN_POINT('Ctrl Pts',(-18.1507549641991,-56.1948621810802,
2.68225560368402));
#237292=CARTESIAN_POINT('Ctrl Pts',(-18.1453743792962,-56.2015542305059,
2.68661792998842));
#237293=CARTESIAN_POINT('Ctrl Pts',(-18.1405824894349,-56.2084349106659,
2.69130986622527));
#237294=CARTESIAN_POINT('Ctrl Pts',(-18.1382584280302,-56.2117720331083,
2.69358545023007));
#237295=CARTESIAN_POINT('Ctrl Pts',(-18.1360729791407,-56.2151540877943,
2.69593918853426));
#237296=CARTESIAN_POINT('Ctrl Pts',(-18.1340220442546,-56.2185710935568,
2.69836306235436));
#237297=CARTESIAN_POINT('Ctrl Pts',(-18.1308822062388,-56.2238022906398,
2.70207384382169));
#237298=CARTESIAN_POINT('Ctrl Pts',(-18.1280584389294,-56.2291119669555,
2.70594760814169));
#237299=CARTESIAN_POINT('Ctrl Pts',(-18.1255442374225,-56.2344544719216,
2.70995196345649));
#237300=CARTESIAN_POINT('Ctrl Pts',(-18.124376629236,-56.2369355588663,
2.71181160678047));
#237301=CARTESIAN_POINT('Ctrl Pts',(-18.1232756028762,-56.2394235482375,
2.7136996277204));
#237302=CARTESIAN_POINT('Ctrl Pts',(-18.1222417093396,-56.2419141381097,
2.71561183138601));
#237303=CARTESIAN_POINT('Ctrl Pts',(-18.1221624654738,-56.2421050320099,
2.71575839426252));
#237304=CARTESIAN_POINT('Ctrl Pts',(-18.1220835820641,-56.2422959411931,
2.7159050890315));
#237305=CARTESIAN_POINT('Ctrl Pts',(-18.1220050584317,-56.242486864366,
2.71605191409852));
#237306=CARTESIAN_POINT('Ctrl Pts',(-18.1209020381381,-56.2451687593303,
2.71811436362694));
#237307=CARTESIAN_POINT('Ctrl Pts',(-18.119871885966,-56.2478543333339,
2.720200910269));
#237308=CARTESIAN_POINT('Ctrl Pts',(-18.1189123616721,-56.2505383386773,
2.72230624862123));
#237309=CARTESIAN_POINT('Ctrl Pts',(-18.1154716781999,-56.2601627045038,
2.72985561753003));
#237310=CARTESIAN_POINT('Ctrl Pts',(-18.1129106883012,-56.2698406425774,
2.73770089914187));
#237311=CARTESIAN_POINT('Ctrl Pts',(-18.1111213027308,-56.2795015152452,
2.74574823346885));
#237312=CARTESIAN_POINT('Ctrl Pts',(-18.1091549477488,-56.2901178437861,
2.75459144546766));
#237313=CARTESIAN_POINT('Ctrl Pts',(-18.1081200911548,-56.3007141730196,
2.76367911753939));
#237314=CARTESIAN_POINT('Ctrl Pts',(-18.1079204190083,-56.3112209484329,
2.77292162564321));
#237315=CARTESIAN_POINT('Ctrl Pts',(-18.107704823201,-56.3225656290382,
2.78290121484209));
#237316=CARTESIAN_POINT('Ctrl Pts',(-18.1084627484398,-56.3338070504084,
2.79306229499546));
#237317=CARTESIAN_POINT('Ctrl Pts',(-18.1101289800536,-56.3448702837308,
2.80331916684491));
#237318=CARTESIAN_POINT('Ctrl Pts',(-18.1117812336968,-56.3558407078965,
2.81348999408167));
#237319=CARTESIAN_POINT('Ctrl Pts',(-18.1143271060903,-56.3666372711371,
2.82375635966592));
#237320=CARTESIAN_POINT('Ctrl Pts',(-18.1177524687101,-56.3771794532807,
2.83404198860222));
#237321=CARTESIAN_POINT('Origin',(-0.0144941013083308,0.00470941899446887,
2.83404198860262));
#237322=CARTESIAN_POINT('Ctrl Pts',(-19.4351129318415,-59.7658094374951,
2.65878198860219));
#237323=CARTESIAN_POINT('Ctrl Pts',(-19.4432803829093,-59.763151894879,
2.65878198860219));
#237324=CARTESIAN_POINT('Ctrl Pts',(-19.4511532554522,-59.7598356997909,
2.65944603041813));
#237325=CARTESIAN_POINT('Ctrl Pts',(-19.4586404431015,-59.7559811102133,
2.66070439264041));
#237326=CARTESIAN_POINT('Ctrl Pts',(-19.463424399579,-59.7535182109725,
2.66150842619564));
#237327=CARTESIAN_POINT('Ctrl Pts',(-19.4680513433539,-59.7508363273792,
2.66255428265332));
#237328=CARTESIAN_POINT('Ctrl Pts',(-19.4725029330457,-59.7479734971805,
2.66381699700611));
#237329=CARTESIAN_POINT('Ctrl Pts',(-19.4785784597568,-59.7440663083906,
2.66554034873211));
#237330=CARTESIAN_POINT('Ctrl Pts',(-19.4843230052517,-59.7398178213042,
2.66766759643915));
#237331=CARTESIAN_POINT('Ctrl Pts',(-19.4896904492929,-59.7353118462116,
2.67012012783091));
#237332=CARTESIAN_POINT('Ctrl Pts',(-19.4923741713135,-59.7330588586653,
2.67134639352678));
#237333=CARTESIAN_POINT('Ctrl Pts',(-19.4949638171731,-59.730741436408,
2.67265375584954));
#237334=CARTESIAN_POINT('Ctrl Pts',(-19.4974550439411,-59.7283696021898,
2.67403135126882));
#237335=CARTESIAN_POINT('Ctrl Pts',(-19.4987006573251,-59.7271836850806,
2.67472014897845));
#237336=CARTESIAN_POINT('Ctrl Pts',(-19.4999216825133,-59.7259841596483,
2.67542649668574));
#237337=CARTESIAN_POINT('Ctrl Pts',(-19.5011176808517,-59.7247722453467,
2.67614899656043));
#237338=CARTESIAN_POINT('Ctrl Pts',(-19.5014166804363,-59.7244692667714,
2.6763296215291));
#237339=CARTESIAN_POINT('Ctrl Pts',(-19.5017141161963,-59.724165513779,
2.67651125590891));
#237340=CARTESIAN_POINT('Ctrl Pts',(-19.5020099819907,-59.723861005197,
2.67669387767465));
#237341=CARTESIAN_POINT('Ctrl Pts',(-19.502897579374,-59.7229474794511,
2.67724174297185));
#237342=CARTESIAN_POINT('Ctrl Pts',(-19.5037710453003,-59.7220271539529,
2.67779849504688));
#237343=CARTESIAN_POINT('Ctrl Pts',(-19.504630229752,-59.7211005320714,
2.6783635361795));
#237344=CARTESIAN_POINT('Ctrl Pts',(-19.5105677273983,-59.7146969999424,
2.68226832098858));
#237345=CARTESIAN_POINT('Ctrl Pts',(-19.5158784513268,-59.7079999120044,
2.68659153751352));
#237346=CARTESIAN_POINT('Ctrl Pts',(-19.5206092977903,-59.701118410241,
2.69123699486152));
#237347=CARTESIAN_POINT('Ctrl Pts',(-19.5229605154966,-59.6976983227542,
2.6935457744118));
#237348=CARTESIAN_POINT('Ctrl Pts',(-19.5251683423977,-59.69423209387,2.6959347882807));
#237349=CARTESIAN_POINT('Ctrl Pts',(-19.5272373629638,-59.6907301905171,
2.69839565261161));
#237350=CARTESIAN_POINT('Ctrl Pts',(-19.5318019313697,-59.6830044686626,
2.70382468688987));
#237351=CARTESIAN_POINT('Ctrl Pts',(-19.5357011184423,-59.6751122606219,
2.70961155815028));
#237352=CARTESIAN_POINT('Ctrl Pts',(-19.5389266512978,-59.6671986827531,
2.71562701361709));
#237353=CARTESIAN_POINT('Ctrl Pts',(-19.540104979126,-59.6643077529622,
2.71782453535799));
#237354=CARTESIAN_POINT('Ctrl Pts',(-19.5412013620775,-59.6614137631514,
2.72005051502344));
#237355=CARTESIAN_POINT('Ctrl Pts',(-19.5422187365063,-59.6585211429013,
2.72229986760057));
#237356=CARTESIAN_POINT('Ctrl Pts',(-19.5456359895573,-59.6488051375689,
2.72985520488817));
#237357=CARTESIAN_POINT('Ctrl Pts',(-19.5481755652418,-59.6390401911872,
2.73770845534464));
#237358=CARTESIAN_POINT('Ctrl Pts',(-19.5499445144587,-59.6292970278062,
2.74576706701639));
#237359=CARTESIAN_POINT('Ctrl Pts',(-19.5518887991939,-59.6185881370968,
2.75462443584899));
#237360=CARTESIAN_POINT('Ctrl Pts',(-19.5529023976135,-59.6079049297411,
2.76373036323034));
#237361=CARTESIAN_POINT('Ctrl Pts',(-19.5530800481814,-59.597317418282,
2.77299664636654));
#237362=CARTESIAN_POINT('Ctrl Pts',(-19.5532713854547,-59.5859142148015,
2.782976830333));
#237363=CARTESIAN_POINT('Ctrl Pts',(-19.5524931697988,-59.5746208362162,
2.79314401478706));
#237364=CARTESIAN_POINT('Ctrl Pts',(-19.5508078878557,-59.5635130675428,
2.8034145242774));
#237365=CARTESIAN_POINT('Ctrl Pts',(-19.549145362909,-59.5525552912509,
2.81354634721213));
#237366=CARTESIAN_POINT('Ctrl Pts',(-19.5465995868768,-59.5417768065755,
2.82378004209104));
#237367=CARTESIAN_POINT('Ctrl Pts',(-19.5431821162861,-59.5312589135995,
2.8340419886022));
#237368=CARTESIAN_POINT('Ctrl Pts',(-18.4801050014185,-56.2594439784239,
2.83404198860221));
#237369=CARTESIAN_POINT('Ctrl Pts',(-18.476834463303,-56.2493782971079,
2.82422126442993));
#237370=CARTESIAN_POINT('Ctrl Pts',(-18.4727817672085,-56.2396067681213,
2.81442815028515));
#237371=CARTESIAN_POINT('Ctrl Pts',(-18.4679768367031,-56.2301791400429,
2.80471618166358));
#237372=CARTESIAN_POINT('Ctrl Pts',(-18.4633372535438,-56.2210759356541,
2.79533842146289));
#237373=CARTESIAN_POINT('Ctrl Pts',(-18.4579956735917,-56.2122922812552,
2.78603515650318));
#237374=CARTESIAN_POINT('Ctrl Pts',(-18.4519372213358,-56.2038917763242,
2.77685887346852));
#237375=CARTESIAN_POINT('Ctrl Pts',(-18.4462100865643,-56.1959506682892,
2.76818441216688));
#237376=CARTESIAN_POINT('Ctrl Pts',(-18.4398418135283,-56.1883512165481,
2.7596226152175));
#237377=CARTESIAN_POINT('Ctrl Pts',(-18.4327901596627,-56.1811768067735,
2.75123537701798));
#237378=CARTESIAN_POINT('Ctrl Pts',(-18.4262957047529,-56.1745692957308,
2.74351087134269));
#237379=CARTESIAN_POINT('Ctrl Pts',(-18.4192211773425,-56.1683219623517,
2.73593399450007));
#237380=CARTESIAN_POINT('Ctrl Pts',(-18.4115142492175,-56.1625328136766,
2.72857657812745));
#237381=CARTESIAN_POINT('Ctrl Pts',(-18.409216198825,-56.1608066064032,
2.72638274508417));
#237382=CARTESIAN_POINT('Ctrl Pts',(-18.4068618031985,-56.1591213928266,
2.72420861709621));
#237383=CARTESIAN_POINT('Ctrl Pts',(-18.4044493827309,-56.1574804751186,
2.72205663736669));
#237384=CARTESIAN_POINT('Ctrl Pts',(-18.4020616112558,-56.155856323546,
2.71992664556708));
#237385=CARTESIAN_POINT('Ctrl Pts',(-18.3996196264078,-56.1542770260202,
2.71782089927826));
#237386=CARTESIAN_POINT('Ctrl Pts',(-18.3971247125282,-56.1527473834683,
2.71574387311188));
#237387=CARTESIAN_POINT('Ctrl Pts',(-18.3969512210963,-56.1526410151168,
2.71559944077428));
#237388=CARTESIAN_POINT('Ctrl Pts',(-18.3967774746429,-56.1525348749436,
2.71545515216011));
#237389=CARTESIAN_POINT('Ctrl Pts',(-18.3966034726921,-56.1524289641632,
2.71531100781672));
#237390=CARTESIAN_POINT('Ctrl Pts',(-18.3889745897488,-56.1477854475701,
2.70899119176033));
#237391=CARTESIAN_POINT('Ctrl Pts',(-18.3808409394273,-56.1436260014307,
2.70298296066796));
#237392=CARTESIAN_POINT('Ctrl Pts',(-18.3722424849459,-56.1400597146376,
2.697367277741));
#237393=CARTESIAN_POINT('Ctrl Pts',(-18.364227230968,-56.1367353155299,
2.69213248525405));
#237394=CARTESIAN_POINT('Ctrl Pts',(-18.3558072700354,-56.1339262909285,
2.68723866185456));
#237395=CARTESIAN_POINT('Ctrl Pts',(-18.3470212548478,-56.1317496772151,
2.68278595829558));
#237396=CARTESIAN_POINT('Ctrl Pts',(-18.3438072168249,-56.1309534437593,
2.68115710172781));
#237397=CARTESIAN_POINT('Ctrl Pts',(-18.3405443147881,-56.1302421351291,
2.67958763637767));
#237398=CARTESIAN_POINT('Ctrl Pts',(-18.337234982846,-56.1296225724747,
2.67808378645305));
#237399=CARTESIAN_POINT('Ctrl Pts',(-18.3364391990691,-56.1294735883541,
2.6777221607854));
#237400=CARTESIAN_POINT('Ctrl Pts',(-18.3356401993822,-56.129330151998,
2.67736403603504));
#237401=CARTESIAN_POINT('Ctrl Pts',(-18.3348380918581,-56.1291923454415,
2.6770095693442));
#237402=CARTESIAN_POINT('Ctrl Pts',(-18.3340610501942,-56.1290588453398,
2.67666617973744));
#237403=CARTESIAN_POINT('Ctrl Pts',(-18.3332810919216,-56.1289306286647,
2.67632622314059));
#237404=CARTESIAN_POINT('Ctrl Pts',(-18.3324983188927,-56.1288077688057,
2.67598984158714));
#237405=CARTESIAN_POINT('Ctrl Pts',(-18.3239221357301,-56.1274616970647,
2.67230439292152));
#237406=CARTESIAN_POINT('Ctrl Pts',(-18.3150023767865,-56.1267581593458,
2.66904964539899));
#237407=CARTESIAN_POINT('Ctrl Pts',(-18.3059033598538,-56.126789533633,
2.66640203566646));
#237408=CARTESIAN_POINT('Ctrl Pts',(-18.3021297263195,-56.1268025454851,
2.66530399299368));
#237409=CARTESIAN_POINT('Ctrl Pts',(-18.2983254984041,-56.1269416083198,
2.66430995142194));
#237410=CARTESIAN_POINT('Ctrl Pts',(-18.2945030089052,-56.1272115877754,
2.663430534733));
#237411=CARTESIAN_POINT('Ctrl Pts',(-18.2879833547329,-56.1276720658709,
2.66193059792823));
#237412=CARTESIAN_POINT('Ctrl Pts',(-18.2814124323568,-56.128515052907,
2.66076519817066));
#237413=CARTESIAN_POINT('Ctrl Pts',(-18.2748585331707,-56.1297657127883,
2.65997805604398));
#237414=CARTESIAN_POINT('Ctrl Pts',(-18.2715815835777,-56.1303910427289,
2.65958448498064));
#237415=CARTESIAN_POINT('Ctrl Pts',(-18.2683092720861,-56.1311196862923,
2.659285262607));
#237416=CARTESIAN_POINT('Ctrl Pts',(-18.2650501911668,-56.1319548233207,
2.65908463971262));
#237417=CARTESIAN_POINT('Ctrl Pts',(-18.2617911102476,-56.1327899603491,
2.65888401681824));
#237418=CARTESIAN_POINT('Ctrl Pts',(-18.258545294751,-56.1337315613408,
2.65878198860222));
#237419=CARTESIAN_POINT('Ctrl Pts',(-18.2553202812744,-56.1347810195642,
2.65878198860222));
#237420=CARTESIAN_POINT('Origin',(-12.0988124084934,-56.9937374973463,2.83404198860222));
#237421=CARTESIAN_POINT('Ctrl Pts',(-12.8407372733092,-61.3271735965893,
2.83404198860219));
#237422=CARTESIAN_POINT('Ctrl Pts',(-12.8429432848606,-61.337552064956,
2.82419652440055));
#237423=CARTESIAN_POINT('Ctrl Pts',(-12.8459616464937,-61.3477256769082,
2.8143879057567));
#237424=CARTESIAN_POINT('Ctrl Pts',(-12.8497656413955,-61.3576417279025,
2.80466781256951));
#237425=CARTESIAN_POINT('Ctrl Pts',(-12.8534460291142,-61.3672355662858,
2.79526356453151));
#237426=CARTESIAN_POINT('Ctrl Pts',(-12.8578623484986,-61.376589487923,
2.78594102496326));
#237427=CARTESIAN_POINT('Ctrl Pts',(-12.863034579891,-61.3856422574855,
2.77675109088891));
#237428=CARTESIAN_POINT('Ctrl Pts',(-12.8679271923005,-61.3942056200541,
2.76805797913813));
#237429=CARTESIAN_POINT('Ctrl Pts',(-12.873496651755,-61.4025003187107,
2.75948271210308));
#237430=CARTESIAN_POINT('Ctrl Pts',(-12.8797929832512,-61.4104485116927,
2.75108575573384));
#237431=CARTESIAN_POINT('Ctrl Pts',(-12.8855923599214,-61.4177693722571,
2.74335155163446));
#237432=CARTESIAN_POINT('Ctrl Pts',(-12.8920087864941,-61.4247966697177,
2.73576818686133));
#237433=CARTESIAN_POINT('Ctrl Pts',(-12.8991043342861,-61.4314390014596,
2.72840626160699));
#237434=CARTESIAN_POINT('Ctrl Pts',(-12.9011624829791,-61.4333656894044,
2.72627084693799));
#237435=CARTESIAN_POINT('Ctrl Pts',(-12.9032779088704,-61.4352597571375,
2.7241542458756));
#237436=CARTESIAN_POINT('Ctrl Pts',(-12.9054524645838,-61.4371183613308,
2.72205867173216));
#237437=CARTESIAN_POINT('Ctrl Pts',(-12.9078098227877,-61.4391332077732,
2.71978693462818));
#237438=CARTESIAN_POINT('Ctrl Pts',(-12.9102326900442,-61.4411043938523,
2.71754411340719));
#237439=CARTESIAN_POINT('Ctrl Pts',(-12.9127224163023,-61.4430281531011,
2.71533341844216));
#237440=CARTESIAN_POINT('Ctrl Pts',(-12.9195554895539,-61.4483079254549,
2.70926614876362));
#237441=CARTESIAN_POINT('Ctrl Pts',(-12.9269097705826,-61.4531896374535,
2.70347381860379));
#237442=CARTESIAN_POINT('Ctrl Pts',(-12.9347398820024,-61.4575800373532,
2.69804914171365));
#237443=CARTESIAN_POINT('Ctrl Pts',(-12.9419040088448,-61.4615970149011,
2.69308585687183));
#237444=CARTESIAN_POINT('Ctrl Pts',(-12.9494643722276,-61.4651913207944,
2.68842799053171));
#237445=CARTESIAN_POINT('Ctrl Pts',(-12.9574154517097,-61.46827448408,2.68414767054209));
#237446=CARTESIAN_POINT('Ctrl Pts',(-12.9613209959781,-61.4697889238144,
2.68204519134536));
#237447=CARTESIAN_POINT('Ctrl Pts',(-12.9653208118547,-61.4711795284099,
2.68003431778479));
#237448=CARTESIAN_POINT('Ctrl Pts',(-12.9694138336344,-61.4724324898303,
2.67812693945222));
#237449=CARTESIAN_POINT('Ctrl Pts',(-12.9701904446506,-61.4726702270558,
2.67776503299174));
#237450=CARTESIAN_POINT('Ctrl Pts',(-12.9709708853386,-61.4729027677274,
2.67740659639895));
#237451=CARTESIAN_POINT('Ctrl Pts',(-12.9717550556842,-61.4731300138562,
2.67705178968826));
#237452=CARTESIAN_POINT('Ctrl Pts',(-12.9725147207064,-61.4733501585434,
2.67670807068729));
#237453=CARTESIAN_POINT('Ctrl Pts',(-12.9732778859002,-61.4735653344324,
2.67636775825236));
#237454=CARTESIAN_POINT('Ctrl Pts',(-12.974044456583,-61.4737754532573,
2.67603099699226));
#237455=CARTESIAN_POINT('Ctrl Pts',(-12.9823983859293,-61.4760652849145,
2.67236104217095));
#237456=CARTESIAN_POINT('Ctrl Pts',(-12.9911623597377,-61.477755648613,
2.66911440541437));
#237457=CARTESIAN_POINT('Ctrl Pts',(-13.0001833616598,-61.4787331403169,
2.66646778189593));
#237458=CARTESIAN_POINT('Ctrl Pts',(-13.0039929867891,-61.4791459411334,
2.6653500963494));
#237459=CARTESIAN_POINT('Ctrl Pts',(-13.0078481668562,-61.4794319383911,
2.66433897912312));
#237460=CARTESIAN_POINT('Ctrl Pts',(-13.0117365408425,-61.4795843394717,
2.66344564884763));
#237461=CARTESIAN_POINT('Ctrl Pts',(-13.0182844654758,-61.4798409790834,
2.66194130298556));
#237462=CARTESIAN_POINT('Ctrl Pts',(-13.024924823017,-61.4797168922657,
2.66077206705391));
#237463=CARTESIAN_POINT('Ctrl Pts',(-13.0315916763171,-61.4791780149466,
2.65998225155685));
#237464=CARTESIAN_POINT('Ctrl Pts',(-13.0332583896422,-61.4790432956168,
2.65978479768259));
#237465=CARTESIAN_POINT('Ctrl Pts',(-13.0349267248711,-61.478882420406,
2.65961098966593));
#237466=CARTESIAN_POINT('Ctrl Pts',(-13.0365955947398,-61.4786945538948,
2.65946139030472));
#237467=CARTESIAN_POINT('Ctrl Pts',(-13.0390988995429,-61.478412754128,
2.65923699126291));
#237468=CARTESIAN_POINT('Ctrl Pts',(-13.0416033892095,-61.4780702140291,
2.65906707562412));
#237469=CARTESIAN_POINT('Ctrl Pts',(-13.0441057251024,-61.4776657592306,
2.6589533256289));
#237470=CARTESIAN_POINT('Ctrl Pts',(-13.0466080609952,-61.477261304432,
2.65883957563368));
#237471=CARTESIAN_POINT('Ctrl Pts',(-13.0491082380622,-61.4767949453821,
2.65878198860219));
#237472=CARTESIAN_POINT('Ctrl Pts',(-13.0516031943522,-61.4762657165315,
2.65878198860219));
#237473=CARTESIAN_POINT('Ctrl Pts',(-12.2578193919762,-57.7418065394565,
2.65878198860222));
#237474=CARTESIAN_POINT('Ctrl Pts',(-12.249377180707,-57.7435970583544,
2.65878198860222));
#237475=CARTESIAN_POINT('Ctrl Pts',(-12.2411559442242,-57.74606892698,2.65945335517815));
#237476=CARTESIAN_POINT('Ctrl Pts',(-12.2332613533223,-57.7491141258102,
2.66072561226559));
#237477=CARTESIAN_POINT('Ctrl Pts',(-12.2281622576313,-57.7510810117991,
2.66154735980298));
#237478=CARTESIAN_POINT('Ctrl Pts',(-12.2231990866879,-57.7532862127603,
2.66261895766844));
#237479=CARTESIAN_POINT('Ctrl Pts',(-12.2183955094113,-57.7556931859578,
2.6639142925099));
#237480=CARTESIAN_POINT('Ctrl Pts',(-12.2120286428971,-57.7588834910511,
2.66563118464086));
#237481=CARTESIAN_POINT('Ctrl Pts',(-12.2059457447512,-57.7624328173674,
2.66774105138662));
#237482=CARTESIAN_POINT('Ctrl Pts',(-12.2001996238495,-57.7662682043708,
2.67016894181712));
#237483=CARTESIAN_POINT('Ctrl Pts',(-12.1973265633986,-57.7681858978725,
2.67138288703237));
#237484=CARTESIAN_POINT('Ctrl Pts',(-12.1945375019632,-57.7701751462709,
2.67267613167513));
#237485=CARTESIAN_POINT('Ctrl Pts',(-12.1918376559068,-57.7722271161467,
2.67403835432515));
#237486=CARTESIAN_POINT('Ctrl Pts',(-12.1904877328785,-57.7732531010846,
2.67471946565016));
#237487=CARTESIAN_POINT('Ctrl Pts',(-12.1891600976129,-57.7742947697602,
2.67541781389485));
#237488=CARTESIAN_POINT('Ctrl Pts',(-12.1878553011592,-57.7753510390204,
2.67613207244131));
#237489=CARTESIAN_POINT('Ctrl Pts',(-12.1875291020458,-57.7756151063354,
2.67631063707792));
#237490=CARTESIAN_POINT('Ctrl Pts',(-12.1872043300158,-57.7758800862576,
2.67649019601807));
#237491=CARTESIAN_POINT('Ctrl Pts',(-12.1868809929892,-57.7761459620048,
2.67667072836618));
#237492=CARTESIAN_POINT('Ctrl Pts',(-12.1859109819092,-57.7769435892464,
2.67721232541052));
#237493=CARTESIAN_POINT('Ctrl Pts',(-12.1849538875684,-57.7777492785673,
2.67776268340008));
#237494=CARTESIAN_POINT('Ctrl Pts',(-12.1840099085252,-57.7785625799461,
2.67832123541477));
#237495=CARTESIAN_POINT('Ctrl Pts',(-12.1773606420344,-57.7842913698423,
2.68225560368405));
#237496=CARTESIAN_POINT('Ctrl Pts',(-12.1713100228959,-57.7903843352496,
2.68661792998849));
#237497=CARTESIAN_POINT('Ctrl Pts',(-12.1658251565853,-57.7967264334405,
2.69130986622539));
#237498=CARTESIAN_POINT('Ctrl Pts',(-12.1631650023516,-57.7998023442098,
2.69358545023015));
#237499=CARTESIAN_POINT('Ctrl Pts',(-12.1606380046007,-57.8029374300324,
2.6959391885343));
#237500=CARTESIAN_POINT('Ctrl Pts',(-12.1582411305893,-57.8061213360078,
2.69836306235436));
#237501=CARTESIAN_POINT('Ctrl Pts',(-12.1545716839425,-57.8109956736032,
2.70207384382169));
#237502=CARTESIAN_POINT('Ctrl Pts',(-12.1512083732202,-57.8159810988989,
2.70594760814169));
#237503=CARTESIAN_POINT('Ctrl Pts',(-12.1481495009381,-57.821031531444,
2.70995196345648));
#237504=CARTESIAN_POINT('Ctrl Pts',(-12.1467289448258,-57.8233769784454,
2.71181160678046));
#237505=CARTESIAN_POINT('Ctrl Pts',(-12.145373884298,-57.8257362497571,
2.71369962772039));
#237506=CARTESIAN_POINT('Ctrl Pts',(-12.1440853170064,-57.8281051246148,
2.71561183138601));
#237507=CARTESIAN_POINT('Ctrl Pts',(-12.1439865534007,-57.8282866895388,
2.71575839426252));
#237508=CARTESIAN_POINT('Ctrl Pts',(-12.1438881466791,-57.8284683073398,
2.7159050890315));
#237509=CARTESIAN_POINT('Ctrl Pts',(-12.1437900963015,-57.828649976661,
2.71605191409852));
#237510=CARTESIAN_POINT('Ctrl Pts',(-12.1424127841092,-57.8312018829078,
2.71811436362694));
#237511=CARTESIAN_POINT('Ctrl Pts',(-12.1411075562949,-57.8337650648326,
2.720200910269));
#237512=CARTESIAN_POINT('Ctrl Pts',(-12.1398727334215,-57.836334069314,
2.72230624862123));
#237513=CARTESIAN_POINT('Ctrl Pts',(-12.1354448782036,-57.8455460625015,
2.72985561753008));
#237514=CARTESIAN_POINT('Ctrl Pts',(-12.1318862976811,-57.8549032874793,
2.73770089914196));
#237515=CARTESIAN_POINT('Ctrl Pts',(-12.1290968783783,-57.8643241951519,
2.74574823346899));
#237516=CARTESIAN_POINT('Ctrl Pts',(-12.1260315867866,-57.8746768262699,
2.75459144546788));
#237517=CARTESIAN_POINT('Ctrl Pts',(-12.1238947812343,-57.8851069357338,
2.76367911753968));
#237518=CARTESIAN_POINT('Ctrl Pts',(-12.1225979458249,-57.8955352825095,
2.77292162564359));
#237519=CARTESIAN_POINT('Ctrl Pts',(-12.121197689044,-57.9067952798691,
2.78290121484263));
#237520=CARTESIAN_POINT('Ctrl Pts',(-12.1207764137884,-57.9180543443175,
2.79306229499618));
#237521=CARTESIAN_POINT('Ctrl Pts',(-12.1212770948332,-57.9292311407204,
2.80331916684581));
#237522=CARTESIAN_POINT('Ctrl Pts',(-12.1217735756786,-57.9403141752886,
2.81348999408227));
#237523=CARTESIAN_POINT('Ctrl Pts',(-12.1231769533527,-57.9513177099548,
2.82375635966622));
#237524=CARTESIAN_POINT('Ctrl Pts',(-12.1254815933786,-57.962160188812,
2.83404198860222));
#237525=CARTESIAN_POINT('Origin',(-0.0149069694351764,0.00316857416825746,
2.83404198860263));
#237526=CARTESIAN_POINT('Ctrl Pts',(-13.0814171332226,-61.4699285681954,
2.65878198860219));
#237527=CARTESIAN_POINT('Ctrl Pts',(-13.0898176309841,-61.4681393149848,
2.65878198860219));
#237528=CARTESIAN_POINT('Ctrl Pts',(-13.0979940118835,-61.465664225629,
2.65944603041805));
#237529=CARTESIAN_POINT('Ctrl Pts',(-13.1058430982601,-61.4626133761159,
2.6607043926402));
#237530=CARTESIAN_POINT('Ctrl Pts',(-13.1108582907967,-61.4606640285136,
2.66150842619545));
#237531=CARTESIAN_POINT('Ctrl Pts',(-13.1157402208605,-61.4584804838815,
2.66255428265318));
#237532=CARTESIAN_POINT('Ctrl Pts',(-13.1204666715199,-61.4560986543956,
2.66381699700607));
#237533=CARTESIAN_POINT('Ctrl Pts',(-13.1269173282999,-61.4528479350654,
2.66554034873207));
#237534=CARTESIAN_POINT('Ctrl Pts',(-13.1330744923998,-61.4492231901484,
2.66766759643912));
#237535=CARTESIAN_POINT('Ctrl Pts',(-13.138883535673,-61.4453029499361,
2.67012012783089));
#237536=CARTESIAN_POINT('Ctrl Pts',(-13.1417880573096,-61.4433428298299,
2.67134639352677));
#237537=CARTESIAN_POINT('Ctrl Pts',(-13.1446057534055,-61.4413087943563,
2.67265375584954));
#237538=CARTESIAN_POINT('Ctrl Pts',(-13.1473312571585,-61.4392103573998,
2.67403135126882));
#237539=CARTESIAN_POINT('Ctrl Pts',(-13.1486940090351,-61.4381611389216,
2.67472014897846));
#237540=CARTESIAN_POINT('Ctrl Pts',(-13.1500337298696,-61.4370958165016,
2.67542649668575));
#237541=CARTESIAN_POINT('Ctrl Pts',(-13.1513498559436,-61.4360155570618,
2.67614899656044));
#237542=CARTESIAN_POINT('Ctrl Pts',(-13.1516788874621,-61.4357454922018,
2.67632962152912));
#237543=CARTESIAN_POINT('Ctrl Pts',(-13.1520064446714,-61.435474493703,
2.67651125590893));
#237544=CARTESIAN_POINT('Ctrl Pts',(-13.1523325194961,-61.4352025796478,
2.67669387767466));
#237545=CARTESIAN_POINT('Ctrl Pts',(-13.1533107439705,-61.434386837482,
2.67724174297187));
#237546=CARTESIAN_POINT('Ctrl Pts',(-13.1542756251691,-61.4335628556741,
2.6777984950469));
#237547=CARTESIAN_POINT('Ctrl Pts',(-13.1552269612797,-61.4327311191546,
2.67836353617952));
#237548=CARTESIAN_POINT('Ctrl Pts',(-13.1618012840654,-61.4269833037495,
2.68226832098846));
#237549=CARTESIAN_POINT('Ctrl Pts',(-13.1677829516028,-61.4208780249712,
2.68659153751323));
#237550=CARTESIAN_POINT('Ctrl Pts',(-13.1732071947986,-61.4145287289055,
2.69123699486104));
#237551=CARTESIAN_POINT('Ctrl Pts',(-13.1759030287778,-61.4113731461892,
2.69354577441147));
#237552=CARTESIAN_POINT('Ctrl Pts',(-13.1784610805508,-61.4081566864225,
2.69593478828053));
#237553=CARTESIAN_POINT('Ctrl Pts',(-13.180884815382,-61.4048902384026,
2.69839565261161));
#237554=CARTESIAN_POINT('Ctrl Pts',(-13.1862319364376,-61.3976839661817,
2.70382468688986));
#237555=CARTESIAN_POINT('Ctrl Pts',(-13.1909347237338,-61.3902425685151,
2.70961155815028));
#237556=CARTESIAN_POINT('Ctrl Pts',(-13.1949697809164,-61.3827095020465,
2.71562701361708));
#237557=CARTESIAN_POINT('Ctrl Pts',(-13.1964438381899,-61.3799575778686,
2.71782453535798));
#237558=CARTESIAN_POINT('Ctrl Pts',(-13.1978367193485,-61.3771940448618,
2.72005051502342));
#237559=CARTESIAN_POINT('Ctrl Pts',(-13.1991508816433,-61.3744236152738,
2.72229986760056));
#237560=CARTESIAN_POINT('Ctrl Pts',(-13.2035650137308,-61.3651180354455,
2.72985520488783));
#237561=CARTESIAN_POINT('Ctrl Pts',(-13.207111392193,-61.3556720404061,
2.73770845534397));
#237562=CARTESIAN_POINT('Ctrl Pts',(-13.2098890888166,-61.3461671566372,
2.74576706701538));
#237563=CARTESIAN_POINT('Ctrl Pts',(-13.2129421064456,-61.3357201634476,
2.75462443584761));
#237564=CARTESIAN_POINT('Ctrl Pts',(-13.2150668515147,-61.3252014297053,
2.76373036322859));
#237565=CARTESIAN_POINT('Ctrl Pts',(-13.216350225197,-61.3146904872831,
2.77299664636439));
#237566=CARTESIAN_POINT('Ctrl Pts',(-13.2177324736409,-61.3033697519362,
2.78297683033034));
#237567=CARTESIAN_POINT('Ctrl Pts',(-13.2181390006406,-61.2920568939744,
2.79314401478388));
#237568=CARTESIAN_POINT('Ctrl Pts',(-13.2176240288383,-61.2808338148888,
2.80341452427365));
#237569=CARTESIAN_POINT('Ctrl Pts',(-13.2171160108941,-61.2697622852627,
2.81354634720964));
#237570=CARTESIAN_POINT('Ctrl Pts',(-13.2157108393288,-61.2587767401961,
2.82378004208981));
#237571=CARTESIAN_POINT('Ctrl Pts',(-13.2134115091888,-61.2479592423877,
2.83404198860219));
#237572=CARTESIAN_POINT('Ctrl Pts',(-12.4981558292581,-57.8829458346105,
2.83404198860221));
#237573=CARTESIAN_POINT('Ctrl Pts',(-12.4959553576925,-57.8725934298276,
2.82422126443078));
#237574=CARTESIAN_POINT('Ctrl Pts',(-12.4929462656003,-57.8624518082052,
2.81442815028684));
#237575=CARTESIAN_POINT('Ctrl Pts',(-12.4891531124827,-57.8525735736588,
2.80471618166611));
#237576=CARTESIAN_POINT('Ctrl Pts',(-12.4854904894113,-57.8430352690787,
2.79533842146592));
#237577=CARTESIAN_POINT('Ctrl Pts',(-12.4810963130896,-57.8337413853143,
2.78603515650671));
#237578=CARTESIAN_POINT('Ctrl Pts',(-12.4759491415407,-57.8247536185246,
2.77685887347252));
#237579=CARTESIAN_POINT('Ctrl Pts',(-12.4710834524327,-57.8162573641139,
2.76818441217116));
#237580=CARTESIAN_POINT('Ctrl Pts',(-12.4655444244753,-57.8080338771707,
2.75962261522203));
#237581=CARTESIAN_POINT('Ctrl Pts',(-12.4592813303365,-57.8001616710216,
2.75123537702274));
#237582=CARTESIAN_POINT('Ctrl Pts',(-12.4535131257059,-57.7929115012243,
2.74351087134758));
#237583=CARTESIAN_POINT('Ctrl Pts',(-12.447130377455,-57.7859589019126,
2.73593399450508));
#237584=CARTESIAN_POINT('Ctrl Pts',(-12.4400707995038,-57.7793958734463,
2.72857657813254));
#237585=CARTESIAN_POINT('Ctrl Pts',(-12.4379657758639,-57.7774389108393,
2.72638274508753));
#237586=CARTESIAN_POINT('Ctrl Pts',(-12.4358004306468,-57.7755168276808,
2.72420861709787));
#237587=CARTESIAN_POINT('Ctrl Pts',(-12.4335727482756,-57.773632732486,
2.72205663736669));
#237588=CARTESIAN_POINT('Ctrl Pts',(-12.4313678273305,-57.7717678881027,
2.71992664556707));
#237589=CARTESIAN_POINT('Ctrl Pts',(-12.4291043014743,-57.7699419852105,
2.71782089927826));
#237590=CARTESIAN_POINT('Ctrl Pts',(-12.4267829461793,-57.7681599326867,
2.71574387311187));
#237591=CARTESIAN_POINT('Ctrl Pts',(-12.4266215236719,-57.7680360122394,
2.71559944077428));
#237592=CARTESIAN_POINT('Ctrl Pts',(-12.426459823689,-57.7679122920634,
2.7154551521601));
#237593=CARTESIAN_POINT('Ctrl Pts',(-12.4262978456302,-57.7677887733168,
2.71531100781672));
#237594=CARTESIAN_POINT('Ctrl Pts',(-12.4191961341595,-57.7623732589829,
2.70899119176029));
#237595=CARTESIAN_POINT('Ctrl Pts',(-12.4115418213384,-57.7573864007558,
2.70298296066787));
#237596=CARTESIAN_POINT('Ctrl Pts',(-12.4033632485683,-57.7529408672214,
2.69736727774088));
#237597=CARTESIAN_POINT('Ctrl Pts',(-12.3957393973204,-57.7487968573389,
2.69213248525393));
#237598=CARTESIAN_POINT('Ctrl Pts',(-12.3876591848397,-57.7451230952911,
2.68723866185445));
#237599=CARTESIAN_POINT('Ctrl Pts',(-12.3791488184491,-57.7420400166296,
2.68278595829548));
#237600=CARTESIAN_POINT('Ctrl Pts',(-12.3760356163224,-57.7409121865686,
2.68115710172774));
#237601=CARTESIAN_POINT('Ctrl Pts',(-12.3728649408024,-57.7398637084258,
2.67958763637763));
#237602=CARTESIAN_POINT('Ctrl Pts',(-12.3696384996592,-57.7389016204181,
2.67808378645303));
#237603=CARTESIAN_POINT('Ctrl Pts',(-12.3688626483502,-57.7386702703928,
2.67772216078539));
#237604=CARTESIAN_POINT('Ctrl Pts',(-12.3680830188491,-57.7384441015867,
2.67736403603501));
#237605=CARTESIAN_POINT('Ctrl Pts',(-12.3672997100616,-57.738223206882,
2.67700956934417));
#237606=CARTESIAN_POINT('Ctrl Pts',(-12.3665408796737,-57.7380092151369,
2.67666617973742));
#237607=CARTESIAN_POINT('Ctrl Pts',(-12.3657785963861,-57.7378001730064,
2.67632622314057));
#237608=CARTESIAN_POINT('Ctrl Pts',(-12.365012953822,-57.7375961641248,
2.67598984158712));
#237609=CARTESIAN_POINT('Ctrl Pts',(-12.3566244546988,-57.7353610110589,
2.67230439292157));
#237610=CARTESIAN_POINT('Ctrl Pts',(-12.3478270988448,-57.7337289586983,
2.66904964539909));
#237611=CARTESIAN_POINT('Ctrl Pts',(-12.338774647773,-57.7328090548566,
2.66640203566658));
#237612=CARTESIAN_POINT('Ctrl Pts',(-12.335020326489,-57.7324275433141,
2.66530399299375));
#237613=CARTESIAN_POINT('Ctrl Pts',(-12.3312224025075,-57.7321681942501,
2.66430995142196));
#237614=CARTESIAN_POINT('Ctrl Pts',(-12.3273926324683,-57.7320371357768,
2.66343053473299));
#237615=CARTESIAN_POINT('Ctrl Pts',(-12.320860560576,-57.7318136018934,
2.66193059792822));
#237616=CARTESIAN_POINT('Ctrl Pts',(-12.3142375182609,-57.7319651225402,
2.66076519817066));
#237617=CARTESIAN_POINT('Ctrl Pts',(-12.3075887924648,-57.7325238621654,
2.65997805604398));
#237618=CARTESIAN_POINT('Ctrl Pts',(-12.3042644295668,-57.732803231978,
2.65958448498064));
#237619=CARTESIAN_POINT('Ctrl Pts',(-12.300933880148,-57.7331858342642,
2.659285262607));
#237620=CARTESIAN_POINT('Ctrl Pts',(-12.2976053572248,-57.7336757296044,
2.65908463971263));
#237621=CARTESIAN_POINT('Ctrl Pts',(-12.2942768343016,-57.7341656249446,
2.65888401681825));
#237622=CARTESIAN_POINT('Ctrl Pts',(-12.2909503756172,-57.7347627876417,
2.65878198860222));
#237623=CARTESIAN_POINT('Ctrl Pts',(-12.2876333308465,-57.7354693911204,
2.65878198860222));
#237624=CARTESIAN_POINT('Origin',(-6.07506605172241,-57.9461901084061,2.83404198860221));
#237625=CARTESIAN_POINT('Ctrl Pts',(-6.35995915837739,-62.3334394572618,
2.83404198860218));
#237626=CARTESIAN_POINT('Ctrl Pts',(-6.36106823981726,-62.3439916622901,
2.82419652440029));
#237627=CARTESIAN_POINT('Ctrl Pts',(-6.36300663452631,-62.3544250468347,
2.81438790575626));
#237628=CARTESIAN_POINT('Ctrl Pts',(-6.36575328117388,-62.3646844024056,
2.80466781256893));
#237629=CARTESIAN_POINT('Ctrl Pts',(-6.3684106781606,-62.3746103900109,
2.79526356453085));
#237630=CARTESIAN_POINT('Ctrl Pts',(-6.3718250534311,-62.3843747009652,
2.78594102496257));
#237631=CARTESIAN_POINT('Ctrl Pts',(-6.37602267870808,-62.393918523908,
2.77675109088821));
#237632=CARTESIAN_POINT('Ctrl Pts',(-6.37999337374521,-62.4029463927371,
2.76805797913744));
#237633=CARTESIAN_POINT('Ctrl Pts',(-6.38466529101432,-62.4117778192047,
2.75948271210242));
#237634=CARTESIAN_POINT('Ctrl Pts',(-6.39009631814961,-62.4203406170095,
2.75108575573322));
#237635=CARTESIAN_POINT('Ctrl Pts',(-6.39509868692306,-62.428227573065,
2.74335155163389));
#237636=CARTESIAN_POINT('Ctrl Pts',(-6.40074541103519,-62.4358870734642,
2.73576818686081));
#237637=CARTESIAN_POINT('Ctrl Pts',(-6.40710777594456,-62.4432347045246,
2.7284062616065));
#237638=CARTESIAN_POINT('Ctrl Pts',(-6.40895325615343,-62.4453659729911,
2.72627084693766));
#237639=CARTESIAN_POINT('Ctrl Pts',(-6.41085910953077,-62.4474707870404,
2.72415424587543));
#237640=CARTESIAN_POINT('Ctrl Pts',(-6.41282747576019,-62.4495465125723,
2.72205867173214));
#237641=CARTESIAN_POINT('Ctrl Pts',(-6.41496131130683,-62.4517967325055,
2.71978693462817));
#237642=CARTESIAN_POINT('Ctrl Pts',(-6.41716486079139,-62.454010378812,
2.71754411340717));
#237643=CARTESIAN_POINT('Ctrl Pts',(-6.41943986047049,-62.4561838467661,
2.71533341844213));
#237644=CARTESIAN_POINT('Ctrl Pts',(-6.42568361494137,-62.4621489466209,
2.7092661487636));
#237645=CARTESIAN_POINT('Ctrl Pts',(-6.43248733059572,-62.4677726477848,
2.70347381860378));
#237646=CARTESIAN_POINT('Ctrl Pts',(-6.4398156260913,-62.4729574661285,
2.69804914171364));
#237647=CARTESIAN_POINT('Ctrl Pts',(-6.4465206186072,-62.4777012934225,
2.69308585687183));
#237648=CARTESIAN_POINT('Ctrl Pts',(-6.4536638582568,-62.4820661824982,
2.68842799053171));
#237649=CARTESIAN_POINT('Ctrl Pts',(-6.46124910257323,-62.4859635700123,
2.68414767054209));
#237650=CARTESIAN_POINT('Ctrl Pts',(-6.46497494980339,-62.4878779540279,
2.68204519134535));
#237651=CARTESIAN_POINT('Ctrl Pts',(-6.46880749650867,-62.4896790353529,
2.68003431778478));
#237652=CARTESIAN_POINT('Ctrl Pts',(-6.47274712615509,-62.4913529701964,
2.67812693945221));
#237653=CARTESIAN_POINT('Ctrl Pts',(-6.47349463250796,-62.4916705830285,
2.67776503299173));
#237654=CARTESIAN_POINT('Ctrl Pts',(-6.47424649074124,-62.4919834280837,
2.67740659639893));
#237655=CARTESIAN_POINT('Ctrl Pts',(-6.47500261163096,-62.4922913974556,
2.67705178968824));
#237656=CARTESIAN_POINT('Ctrl Pts',(-6.47573510374288,-62.4925897427846,
2.67670807068727));
#237657=CARTESIAN_POINT('Ctrl Pts',(-6.47647159623283,-62.4928835124025,
2.67636775825234));
#237658=CARTESIAN_POINT('Ctrl Pts',(-6.47721200416342,-62.49317260863,2.67603099699224));
#237659=CARTESIAN_POINT('Ctrl Pts',(-6.48528081722642,-62.4963231197466,
2.6723610421709));
#237660=CARTESIAN_POINT('Ctrl Pts',(-6.4938200899496,-62.4989203081702,
2.6691144054143));
#237661=CARTESIAN_POINT('Ctrl Pts',(-6.50268949817377,-62.5008353965404,
2.66646778189584));
#237662=CARTESIAN_POINT('Ctrl Pts',(-6.50643510434294,-62.5016441502511,
2.66535009634934));
#237663=CARTESIAN_POINT('Ctrl Pts',(-6.51023927047629,-62.5023315568339,
2.66433897912309));
#237664=CARTESIAN_POINT('Ctrl Pts',(-6.51409041329226,-62.5028895688028,
2.66344564884762));
#237665=CARTESIAN_POINT('Ctrl Pts',(-6.52057564156509,-62.5038292470154,
2.66194130298555));
#237666=CARTESIAN_POINT('Ctrl Pts',(-6.52719259313717,-62.5043999463276,
2.66077206705389));
#237667=CARTESIAN_POINT('Ctrl Pts',(-6.53387925273547,-62.5045608969653,
2.65998225155684));
#237668=CARTESIAN_POINT('Ctrl Pts',(-6.53555091763504,-62.5046011346247,
2.65978479768257));
#237669=CARTESIAN_POINT('Ctrl Pts',(-6.53722692958757,-62.5046155292228,
2.65961098966592));
#237670=CARTESIAN_POINT('Ctrl Pts',(-6.53890629461024,-62.5046031362668,
2.65946139030471));
#237671=CARTESIAN_POINT('Ctrl Pts',(-6.54142534214424,-62.5045845468328,
2.65923699126289));
#237672=CARTESIAN_POINT('Ctrl Pts',(-6.54395191714457,-62.5045056736604,
2.65906707562411));
#237673=CARTESIAN_POINT('Ctrl Pts',(-6.54648282201814,-62.504364999833,
2.65895332562888));
#237674=CARTESIAN_POINT('Ctrl Pts',(-6.54901372689171,-62.5042243260056,
2.65883957563366));
#237675=CARTESIAN_POINT('Ctrl Pts',(-6.55154895552196,-62.504021861386,
2.65878198860218));
#237676=CARTESIAN_POINT('Ctrl Pts',(-6.55408556365882,-62.5037563256533,
2.65878198860218));
#237677=CARTESIAN_POINT('Ctrl Pts',(-6.15500747092256,-58.7067819056642,
2.65878198860221));
#237678=CARTESIAN_POINT('Ctrl Pts',(-6.14642434678128,-58.7076801645416,
2.65878198860221));
#237679=CARTESIAN_POINT('Ctrl Pts',(-6.13798976646331,-58.7092791387966,
2.65945335517813));
#237680=CARTESIAN_POINT('Ctrl Pts',(-6.12982011300226,-58.7114824462538,
2.66072561226557));
#237681=CARTESIAN_POINT('Ctrl Pts',(-6.12454335512117,-58.7129055567988,
2.66154735980295));
#237682=CARTESIAN_POINT('Ctrl Pts',(-6.11937686667988,-58.7145798848068,
2.66261895766841));
#237683=CARTESIAN_POINT('Ctrl Pts',(-6.1143480066927,-58.7164715618023,
2.66391429250987));
#237684=CARTESIAN_POINT('Ctrl Pts',(-6.1076825408507,-58.718978871298,2.66563118464083));
#237685=CARTESIAN_POINT('Ctrl Pts',(-6.10126195983177,-58.721872918038,
2.66774105138658));
#237686=CARTESIAN_POINT('Ctrl Pts',(-6.09514640967211,-58.7250866612025,
2.67016894181709));
#237687=CARTESIAN_POINT('Ctrl Pts',(-6.09208863459227,-58.7266935327847,
2.67138288703234));
#237688=CARTESIAN_POINT('Ctrl Pts',(-6.08910691884909,-58.7283803475664,
2.6726761316751));
#237689=CARTESIAN_POINT('Ctrl Pts',(-6.08620737357403,-58.7301388657772,
2.67403835432512));
#237690=CARTESIAN_POINT('Ctrl Pts',(-6.08475760093649,-58.7310181248826,
2.67471946565013));
#237691=CARTESIAN_POINT('Ctrl Pts',(-6.08332835456981,-58.7319153115141,
2.67541781389482));
#237692=CARTESIAN_POINT('Ctrl Pts',(-6.08192029572508,-58.7328294060526,
2.67613207244128));
#237693=CARTESIAN_POINT('Ctrl Pts',(-6.0815682810139,-58.7330579296872,
2.6763106370779));
#237694=CARTESIAN_POINT('Ctrl Pts',(-6.08121759017506,-58.7332875101005,
2.67649019601804));
#237695=CARTESIAN_POINT('Ctrl Pts',(-6.08086823283919,-58.73351813143,2.67667072836616));
#237696=CARTESIAN_POINT('Ctrl Pts',(-6.07982016083158,-58.7342099954185,
2.67721232541049));
#237697=CARTESIAN_POINT('Ctrl Pts',(-6.07878409208716,-58.7349112274884,
2.67776268340006));
#237698=CARTESIAN_POINT('Ctrl Pts',(-6.07776027111658,-58.7356214008384,
2.67832123541475));
#237699=CARTESIAN_POINT('Ctrl Pts',(-6.07054860839913,-58.7406237702159,
2.68225560368402));
#237700=CARTESIAN_POINT('Ctrl Pts',(-6.06389424687466,-58.7460508958009,
2.68661792998844));
#237701=CARTESIAN_POINT('Ctrl Pts',(-6.05777649745776,-58.7517849266676,
2.69130986622532));
#237702=CARTESIAN_POINT('Ctrl Pts',(-6.0548093956014,-58.7545659254418,
2.6935854502301));
#237703=CARTESIAN_POINT('Ctrl Pts',(-6.05196853530536,-58.7574196937446,
2.69593918853427));
#237704=CARTESIAN_POINT('Ctrl Pts',(-6.04925198282171,-58.7603356163929,
2.69836306235434));
#237705=CARTESIAN_POINT('Ctrl Pts',(-6.04509313076931,-58.7647996902379,
2.70207384382167));
#237706=CARTESIAN_POINT('Ctrl Pts',(-6.04122712577015,-58.769406243151,
2.70594760814168));
#237707=CARTESIAN_POINT('Ctrl Pts',(-6.03765709635773,-58.7741092696791,
2.70995196345648));
#237708=CARTESIAN_POINT('Ctrl Pts',(-6.03599915622971,-58.776293379529,
2.71181160678046));
#237709=CARTESIAN_POINT('Ctrl Pts',(-6.03440490786061,-58.778498084111,
2.71369962772039));
#237710=CARTESIAN_POINT('Ctrl Pts',(-6.03287578462695,-58.7807192900656,
2.71561183138601));
#237711=CARTESIAN_POINT('Ctrl Pts',(-6.03275858335614,-58.78088953675,2.71575839426252));
#237712=CARTESIAN_POINT('Ctrl Pts',(-6.03264173148717,-58.7810598733264,
2.71590508903149));
#237713=CARTESIAN_POINT('Ctrl Pts',(-6.03252522862488,-58.7812302983887,
2.71605191409851));
#237714=CARTESIAN_POINT('Ctrl Pts',(-6.03088871465443,-58.7836242566992,
2.71811436362693));
#237715=CARTESIAN_POINT('Ctrl Pts',(-6.02932271154701,-58.7860369637875,
2.72020091026899));
#237716=CARTESIAN_POINT('Ctrl Pts',(-6.02782611907196,-58.7884628208562,
2.72230624862122));
#237717=CARTESIAN_POINT('Ctrl Pts',(-6.02245960461621,-58.7971615128805,
2.72985561753076));
#237718=CARTESIAN_POINT('Ctrl Pts',(-6.01794242202239,-58.8060955050482,
2.7377008991434));
#237719=CARTESIAN_POINT('Ctrl Pts',(-6.01418353044859,-58.8151732302906,
2.74574823347121));
#237720=CARTESIAN_POINT('Ctrl Pts',(-6.01005288622323,-58.8251487383934,
2.75459144547085));
#237721=CARTESIAN_POINT('Ctrl Pts',(-6.00683754300126,-58.8352983536265,
2.76367911754344));
#237722=CARTESIAN_POINT('Ctrl Pts',(-6.00445775272911,-58.8455340166158,
2.77292162564815));
#237723=CARTESIAN_POINT('Ctrl Pts',(-6.00188817648111,-58.8565859638431,
2.78290121484799));
#237724=CARTESIAN_POINT('Ctrl Pts',(-6.00029231631103,-58.8677393147042,
2.79306229500235));
#237725=CARTESIAN_POINT('Ctrl Pts',(-5.99962196122081,-58.878907218868,
2.80331916685278));
#237726=CARTESIAN_POINT('Ctrl Pts',(-5.99895722972104,-58.8899814357904,
2.81348999408696));
#237727=CARTESIAN_POINT('Ctrl Pts',(-5.99920273697641,-58.9010713848515,
2.82375635966856));
#237728=CARTESIAN_POINT('Ctrl Pts',(-6.00036140428986,-58.9120953679529,
2.8340419886022));
#237729=CARTESIAN_POINT('Origin',(-0.0151565136854063,0.00159301378039395,
2.83404198860262));
#237730=CARTESIAN_POINT('Ctrl Pts',(-6.58439859102965,-62.500570298093,
2.65878198860218));
#237731=CARTESIAN_POINT('Ctrl Pts',(-6.59294009787386,-62.4996689377204,
2.65878198860218));
#237732=CARTESIAN_POINT('Ctrl Pts',(-6.60133040498984,-62.4980620716936,
2.65944603041802));
#237733=CARTESIAN_POINT('Ctrl Pts',(-6.60945539386119,-62.4958483879904,
2.66070439264013));
#237734=CARTESIAN_POINT('Ctrl Pts',(-6.61464687495772,-62.494433949487,
2.6615084261954));
#237735=CARTESIAN_POINT('Ctrl Pts',(-6.61973030386286,-62.4927726671881,
2.66255428265316));
#237736=CARTESIAN_POINT('Ctrl Pts',(-6.62467983150704,-62.4908979342375,
2.66381699700609));
#237737=CARTESIAN_POINT('Ctrl Pts',(-6.63143494361032,-62.4883392999282,
2.66554034873209));
#237738=CARTESIAN_POINT('Ctrl Pts',(-6.63793726713702,-62.4853780106446,
2.66766759643914));
#237739=CARTESIAN_POINT('Ctrl Pts',(-6.64412426454832,-62.4820864562847,
2.6701201278309));
#237740=CARTESIAN_POINT('Ctrl Pts',(-6.64721776325397,-62.4804406791048,
2.67134639352678));
#237741=CARTESIAN_POINT('Ctrl Pts',(-6.65023263831811,-62.4787123157332,
2.67265375584954));
#237742=CARTESIAN_POINT('Ctrl Pts',(-6.65316255786678,-62.4769102669529,
2.67403135126882));
#237743=CARTESIAN_POINT('Ctrl Pts',(-6.65462751764111,-62.4760092425627,
2.67472014897846));
#237744=CARTESIAN_POINT('Ctrl Pts',(-6.65607125586019,-62.4750897950505,
2.67542649668575));
#237745=CARTESIAN_POINT('Ctrl Pts',(-6.65749308991699,-62.4741530260209,
2.67614899656044));
#237746=CARTESIAN_POINT('Ctrl Pts',(-6.65784854843119,-62.4739188337634,
2.67632962152911));
#237747=CARTESIAN_POINT('Ctrl Pts',(-6.65820263830441,-62.4736835588745,
2.67651125590892));
#237748=CARTESIAN_POINT('Ctrl Pts',(-6.65855534961552,-62.4734472184932,
2.67669387767466));
#237749=CARTESIAN_POINT('Ctrl Pts',(-6.65961348354886,-62.4727381973494,
2.67724174297186));
#237750=CARTESIAN_POINT('Ctrl Pts',(-6.66065920857944,-62.4720195869491,
2.6777984950469));
#237751=CARTESIAN_POINT('Ctrl Pts',(-6.66169227331155,-62.4712918484709,
2.67836353617951));
#237752=CARTESIAN_POINT('Ctrl Pts',(-6.66883139158055,-62.4662627240578,
2.68226832098846));
#237753=CARTESIAN_POINT('Ctrl Pts',(-6.67541846632588,-62.4608161451509,
2.68659153751324));
#237754=CARTESIAN_POINT('Ctrl Pts',(-6.68147667711047,-62.4550686189991,
2.69123699486105));
#237755=CARTESIAN_POINT('Ctrl Pts',(-6.68448759124107,-62.4522121142781,
2.69354577441148));
#237756=CARTESIAN_POINT('Ctrl Pts',(-6.68736784133544,-62.4492806638354,
2.69593478828053));
#237757=CARTESIAN_POINT('Ctrl Pts',(-6.69011973548545,-62.4462854590367,
2.6983956526116));
#237758=CARTESIAN_POINT('Ctrl Pts',(-6.69619082501359,-62.439677589876,
2.70382468688985));
#237759=CARTESIAN_POINT('Ctrl Pts',(-6.70164568781153,-62.4327685320935,
2.70961155815027));
#237760=CARTESIAN_POINT('Ctrl Pts',(-6.7064460603903,-62.4256985108777,
2.71562701361706));
#237761=CARTESIAN_POINT('Ctrl Pts',(-6.70819969702921,-62.4231157429699,
2.71782453535797));
#237762=CARTESIAN_POINT('Ctrl Pts',(-6.70987381569752,-62.4205129446132,
2.72005051502341));
#237763=CARTESIAN_POINT('Ctrl Pts',(-6.71147036762112,-62.4178950590934,
2.72229986760055));
#237764=CARTESIAN_POINT('Ctrl Pts',(-6.71683301659051,-62.4091018586488,
2.72985520488792));
#237765=CARTESIAN_POINT('Ctrl Pts',(-6.72134734296604,-62.4000783072493,
2.73770845534421));
#237766=CARTESIAN_POINT('Ctrl Pts',(-6.72510335397076,-62.3909158405876,
2.74576706701578));
#237767=CARTESIAN_POINT('Ctrl Pts',(-6.7292316549937,-62.3808452043609,
2.75462443584815));
#237768=CARTESIAN_POINT('Ctrl Pts',(-6.73244426756063,-62.3706061896796,
2.76373036322926));
#237769=CARTESIAN_POINT('Ctrl Pts',(-6.73481930344644,-62.3602869763785,
2.77299664636518));
#237770=CARTESIAN_POINT('Ctrl Pts',(-6.73737731885764,-62.3491727415103,
2.78297683033115));
#237771=CARTESIAN_POINT('Ctrl Pts',(-6.73896413451773,-62.3379643502107,
2.79314401478467));
#237772=CARTESIAN_POINT('Ctrl Pts',(-6.73962511499484,-62.3267489231156,
2.80341452427437));
#237773=CARTESIAN_POINT('Ctrl Pts',(-6.74027717000387,-62.3156849421522,
2.81354634721019));
#237774=CARTESIAN_POINT('Ctrl Pts',(-6.74002799825934,-62.3046126966266,
2.82378004209014));
#237775=CARTESIAN_POINT('Ctrl Pts',(-6.7388720005127,-62.2936141127568,
2.83404198860218));
#237776=CARTESIAN_POINT('Ctrl Pts',(-6.37927424642518,-58.8722700234479,
2.8340419886022));
#237777=CARTESIAN_POINT('Ctrl Pts',(-6.37816795023606,-58.8617443183103,
2.82422126443067));
#237778=CARTESIAN_POINT('Ctrl Pts',(-6.37623543038838,-58.8513437177799,
2.81442815028664));
#237779=CARTESIAN_POINT('Ctrl Pts',(-6.37349561323738,-58.8411231047696,
2.80471618166581));
#237780=CARTESIAN_POINT('Ctrl Pts',(-6.37085007871829,-58.8312542036587,
2.79533842146557));
#237781=CARTESIAN_POINT('Ctrl Pts',(-6.36745144954188,-58.8215519162637,
2.7860351565063));
#237782=CARTESIAN_POINT('Ctrl Pts',(-6.36327195218801,-58.8120753594687,
2.77685887347205));
#237783=CARTESIAN_POINT('Ctrl Pts',(-6.35932101825102,-58.8031170454234,
2.76818441217064));
#237784=CARTESIAN_POINT('Ctrl Pts',(-6.35467192212117,-58.7943596215217,
2.75962261522147));
#237785=CARTESIAN_POINT('Ctrl Pts',(-6.34926600747862,-58.7858758685359,
2.75123537702214));
#237786=CARTESIAN_POINT('Ctrl Pts',(-6.34428725078379,-58.7780624743614,
2.74351087134693));
#237787=CARTESIAN_POINT('Ctrl Pts',(-6.33866621241734,-58.7704807832501,
2.73593399450439));
#237788=CARTESIAN_POINT('Ctrl Pts',(-6.33233133085271,-58.7632157809058,
2.72857657813182));
#237789=CARTESIAN_POINT('Ctrl Pts',(-6.33044239704668,-58.7610495038588,
2.72638274508705));
#237790=CARTESIAN_POINT('Ctrl Pts',(-6.32848982621625,-58.7589116098652,
2.72420861709762));
#237791=CARTESIAN_POINT('Ctrl Pts',(-6.32647128889777,-58.7568049797263,
2.72205663736667));
#237792=CARTESIAN_POINT('Ctrl Pts',(-6.32447337605792,-58.7547198741576,
2.71992664556706));
#237793=CARTESIAN_POINT('Ctrl Pts',(-6.32241310885664,-58.7526673708732,
2.71782089927824));
#237794=CARTESIAN_POINT('Ctrl Pts',(-6.32029074540058,-58.7506524329179,
2.71574387311186));
#237795=CARTESIAN_POINT('Ctrl Pts',(-6.32014316039653,-58.7505123180731,
2.71559944077427));
#237796=CARTESIAN_POINT('Ctrl Pts',(-6.31999527850295,-58.7503723733985,
2.71545515216009));
#237797=CARTESIAN_POINT('Ctrl Pts',(-6.31984709900165,-58.750232599983,
2.7153110078167));
#237798=CARTESIAN_POINT('Ctrl Pts',(-6.31335036684049,-58.7441044214166,
2.70899119176023));
#237799=CARTESIAN_POINT('Ctrl Pts',(-6.30625925377286,-58.738344788164,
2.70298296066777));
#237800=CARTESIAN_POINT('Ctrl Pts',(-6.29859016886885,-58.733068714084,
2.69736727774074));
#237801=CARTESIAN_POINT('Ctrl Pts',(-6.29144124886036,-58.728150496066,
2.69213248525365));
#237802=CARTESIAN_POINT('Ctrl Pts',(-6.28378931333002,-58.7236522470775,
2.68723866185404));
#237803=CARTESIAN_POINT('Ctrl Pts',(-6.27564783709133,-58.7196964823228,
2.68278595829497));
#237804=CARTESIAN_POINT('Ctrl Pts',(-6.27266957975507,-58.7182494123989,
2.68115710172741));
#237805=CARTESIAN_POINT('Ctrl Pts',(-6.26962586933668,-58.7168752520896,
2.67958763637747));
#237806=CARTESIAN_POINT('Ctrl Pts',(-6.26651766855692,-58.7155811795663,
2.67808378645303));
#237807=CARTESIAN_POINT('Ctrl Pts',(-6.26577025010519,-58.7152699983555,
2.67772216078538));
#237808=CARTESIAN_POINT('Ctrl Pts',(-6.26501853257379,-58.7149635750522,
2.67736403603501));
#237809=CARTESIAN_POINT('Ctrl Pts',(-6.26426260461781,-58.714662012368,
2.67700956934417));
#237810=CARTESIAN_POINT('Ctrl Pts',(-6.26353029941046,-58.7143698735177,
2.67666617973742));
#237811=CARTESIAN_POINT('Ctrl Pts',(-6.26279404284316,-58.7140822962413,
2.67632622314057));
#237812=CARTESIAN_POINT('Ctrl Pts',(-6.262053919284,-58.713799373501,2.67598984158711));
#237813=CARTESIAN_POINT('Ctrl Pts',(-6.25394501035187,-58.7106996279151,
2.6723043929216));
#237814=CARTESIAN_POINT('Ctrl Pts',(-6.24536644325901,-58.7081569420198,
2.66904964539914));
#237815=CARTESIAN_POINT('Ctrl Pts',(-6.23645973859638,-58.7062958387083,
2.66640203566664));
#237816=CARTESIAN_POINT('Ctrl Pts',(-6.23276586269236,-58.7055239836914,
2.66530399299379));
#237817=CARTESIAN_POINT('Ctrl Pts',(-6.22901585349491,-58.7048690642114,
2.66430995142197));
#237818=CARTESIAN_POINT('Ctrl Pts',(-6.2252207626774,-58.7043384037132,
2.66343053473298));
#237819=CARTESIAN_POINT('Ctrl Pts',(-6.21874783981175,-58.703433306935,
2.66193059792822));
#237820=CARTESIAN_POINT('Ctrl Pts',(-6.21214524099502,-58.7028917011004,
2.66076519817064));
#237821=CARTESIAN_POINT('Ctrl Pts',(-6.20547453342013,-58.7027523988016,
2.65997805604397));
#237822=CARTESIAN_POINT('Ctrl Pts',(-6.20213917963269,-58.7026827476522,
2.65958448498063));
#237823=CARTESIAN_POINT('Ctrl Pts',(-6.19878688248308,-58.7027151167904,
2.65928526260699));
#237824=CARTESIAN_POINT('Ctrl Pts',(-6.19542538554965,-58.7028544030465,
2.65908463971261));
#237825=CARTESIAN_POINT('Ctrl Pts',(-6.19206388861623,-58.7029936893026,
2.65888401681823));
#237826=CARTESIAN_POINT('Ctrl Pts',(-6.18869323212156,-58.7032398710653,
2.65878198860221));
#237827=CARTESIAN_POINT('Ctrl Pts',(-6.18532049829339,-58.7035958781038,
2.65878198860221));
#237828=CARTESIAN_POINT('Origin',(0.0152400000006159,-58.2637721346183,
2.83404198860221));
#237829=CARTESIAN_POINT('Ctrl Pts',(0.190500000000662,-62.6567671111298,
2.83404198860218));
#237830=CARTESIAN_POINT('Ctrl Pts',(0.190500000000662,-62.6673774406536,
2.82419652440023));
#237831=CARTESIAN_POINT('Ctrl Pts',(0.189662809673738,-62.6779562874463,
2.81438790575611));
#237832=CARTESIAN_POINT('Ctrl Pts',(0.188003604115792,-62.6884465439472,
2.80466781256867));
#237833=CARTESIAN_POINT('Ctrl Pts',(0.186398312858558,-62.6985959295773,
2.79526356453047));
#237834=CARTESIAN_POINT('Ctrl Pts',(0.184023290311906,-62.7086636500147,
2.78594102496205));
#237835=CARTESIAN_POINT('Ctrl Pts',(0.180846261211217,-62.7185939622165,
2.77675109088756));
#237836=CARTESIAN_POINT('Ctrl Pts',(0.177840987312148,-62.727987426086,
2.76805797913663));
#237837=CARTESIAN_POINT('Ctrl Pts',(0.174117798731669,-62.7372588214081,
2.75948271210146));
#237838=CARTESIAN_POINT('Ctrl Pts',(0.169611579426945,-62.7463424082311,
2.75108575573212));
#237839=CARTESIAN_POINT('Ctrl Pts',(0.165461025549218,-62.7547090486368,
2.74335155163261));
#237840=CARTESIAN_POINT('Ctrl Pts',(0.160645870588547,-62.7629168328855,
2.73576818685937));
#237841=CARTESIAN_POINT('Ctrl Pts',(0.155086395963031,-62.770889261081,
2.72840626160493));
#237842=CARTESIAN_POINT('Ctrl Pts',(0.153473803705819,-62.7732017594456,
2.72627084693661));
#237843=CARTESIAN_POINT('Ctrl Pts',(0.151798403771124,-62.7754942590275,
2.7241542458749));
#237844=CARTESIAN_POINT('Ctrl Pts',(0.150057792858307,-62.7777643638144,
2.72205867173211));
#237845=CARTESIAN_POINT('Ctrl Pts',(0.148170858717691,-62.7802253033579,
2.71978693462815));
#237846=CARTESIAN_POINT('Ctrl Pts',(0.146210769554423,-62.7826571567197,
2.71754411340716));
#237847=CARTESIAN_POINT('Ctrl Pts',(0.144175421826809,-62.7850565204093,
2.71533341844214));
#237848=CARTESIAN_POINT('Ctrl Pts',(0.138589394017279,-62.7916415928828,
2.70926614876361));
#237849=CARTESIAN_POINT('Ctrl Pts',(0.132410786669697,-62.7979456687652,
2.70347381860378));
#237850=CARTESIAN_POINT('Ctrl Pts',(0.125664597437387,-62.803868099598,
2.69804914171364));
#237851=CARTESIAN_POINT('Ctrl Pts',(0.119492200549002,-62.8092868022737,
2.69308585687176));
#237852=CARTESIAN_POINT('Ctrl Pts',(0.112844347460919,-62.8143744518937,
2.68842799053158));
#237853=CARTESIAN_POINT('Ctrl Pts',(0.105708043833992,-62.8190433630432,
2.68414767054191));
#237854=CARTESIAN_POINT('Ctrl Pts',(0.102202714804165,-62.8213367169481,
2.68204519134525));
#237855=CARTESIAN_POINT('Ctrl Pts',(0.0985794274539604,-62.8235285419786,
2.68003431778474));
#237856=CARTESIAN_POINT('Ctrl Pts',(0.0948363533478736,-62.8256051102646,
2.67812693945223));
#237857=CARTESIAN_POINT('Ctrl Pts',(0.0941261414942743,-62.8259991188708,
2.67776503299174));
#237858=CARTESIAN_POINT('Ctrl Pts',(0.0934111032319262,-62.8263888407137,
2.67740659639895));
#237859=CARTESIAN_POINT('Ctrl Pts',(0.0926913160167301,-62.8267741591518,
2.67705178968826));
#237860=CARTESIAN_POINT('Ctrl Pts',(0.091994022152009,-62.8271474363887,
2.67670807068729));
#237861=CARTESIAN_POINT('Ctrl Pts',(0.0912922715316926,-62.8275165811341,
2.67636775825236));
#237862=CARTESIAN_POINT('Ctrl Pts',(0.0905861384176031,-62.8278814873653,
2.67603099699226));
#237863=CARTESIAN_POINT('Ctrl Pts',(0.0828908452424436,-62.8318581602823,
2.67236104217096));
#237864=CARTESIAN_POINT('Ctrl Pts',(0.0746698316635625,-62.8353337180911,
2.66911440541439));
#237865=CARTESIAN_POINT('Ctrl Pts',(0.0660491922301222,-62.8381654210185,
2.66646778189595));
#237866=CARTESIAN_POINT('Ctrl Pts',(0.0624086426659131,-62.8393612667487,
2.66535009634941));
#237867=CARTESIAN_POINT('Ctrl Pts',(0.0586971697063133,-62.8404425512863,
2.66433897912313));
#237868=CARTESIAN_POINT('Ctrl Pts',(0.054925451987136,-62.8414000604477,
2.66344564884763));
#237869=CARTESIAN_POINT('Ctrl Pts',(0.0485739735928758,-62.8430124819499,
2.66194130298556));
#237870=CARTESIAN_POINT('Ctrl Pts',(0.0420529246959322,-62.844271714691,
2.6607720670539));
#237871=CARTESIAN_POINT('Ctrl Pts',(0.0354197192413684,-62.8451307298762,
2.65998225155684));
#237872=CARTESIAN_POINT('Ctrl Pts',(0.0337614178777275,-62.8453454836725,
2.65978479768257));
#237873=CARTESIAN_POINT('Ctrl Pts',(0.032096091939252,-62.8455349903693,
2.65961098966591));
#237874=CARTESIAN_POINT('Ctrl Pts',(0.0304246312372505,-62.8456982067483,
2.65946139030471));
#237875=CARTESIAN_POINT('Ctrl Pts',(0.0279174401842483,-62.8459430313168,
2.65923699126289));
#237876=CARTESIAN_POINT('Ctrl Pts',(0.0253964615346301,-62.8461286892221,
2.65906707562411));
#237877=CARTESIAN_POINT('Ctrl Pts',(0.0228647168037737,-62.8462533376178,
2.65895332562888));
#237878=CARTESIAN_POINT('Ctrl Pts',(0.0203329720729172,-62.8463779860135,
2.65883957563366));
#237879=CARTESIAN_POINT('Ctrl Pts',(0.0177904683748175,-62.8464416340691,
2.65878198860218));
#237880=CARTESIAN_POINT('Ctrl Pts',(0.0152400000006639,-62.8464427007194,
2.65878198860218));
#237881=CARTESIAN_POINT('Ctrl Pts',(0.0152400000006241,-59.0285534841294,
2.6587819886022));
#237882=CARTESIAN_POINT('Ctrl Pts',(0.0238699985099668,-59.0285496414742,
2.6587819886022));
#237883=CARTESIAN_POINT('Ctrl Pts',(0.0324255116361993,-59.029258202662,
2.65945335517814));
#237884=CARTESIAN_POINT('Ctrl Pts',(0.0407807192234809,-59.0305954788488,
2.66072561226561));
#237885=CARTESIAN_POINT('Ctrl Pts',(0.0461773260310371,-59.031459222053,
2.66154735980299));
#237886=CARTESIAN_POINT('Ctrl Pts',(0.0514905268416817,-59.0325843328197,
2.66261895766844));
#237887=CARTESIAN_POINT('Ctrl Pts',(0.0566895722969428,-59.0339399880042,
2.66391429250988));
#237888=CARTESIAN_POINT('Ctrl Pts',(0.0635806092281412,-59.0357368312947,
2.66563118464085));
#237889=CARTESIAN_POINT('Ctrl Pts',(0.0702685278908046,-59.0379438906766,
2.6677410513866));
#237890=CARTESIAN_POINT('Ctrl Pts',(0.0766865040611197,-59.0405007795596,
2.67016894181711));
#237891=CARTESIAN_POINT('Ctrl Pts',(0.0798954921462772,-59.041779224001,
2.67138288703236));
#237892=CARTESIAN_POINT('Ctrl Pts',(0.0830371938955821,-59.0431451240704,
2.67267613167512));
#237893=CARTESIAN_POINT('Ctrl Pts',(0.0861046703644424,-59.0445909239226,
2.67403835432513));
#237894=CARTESIAN_POINT('Ctrl Pts',(0.0876384085988726,-59.0453138238487,
2.67471946565014));
#237895=CARTESIAN_POINT('Ctrl Pts',(0.0891536069442672,-59.0460566986717,
2.67541781389483));
#237896=CARTESIAN_POINT('Ctrl Pts',(0.090649501192699,-59.0468186034774,
2.67613207244129));
#237897=CARTESIAN_POINT('Ctrl Pts',(0.091023474754807,-59.0470090796788,
2.6763106370779));
#237898=CARTESIAN_POINT('Ctrl Pts',(0.0913962421603352,-59.0472007452521,
2.67649019601805));
#237899=CARTESIAN_POINT('Ctrl Pts',(0.0917677921733363,-59.0473935854284,
2.67667072836616));
#237900=CARTESIAN_POINT('Ctrl Pts',(0.0928824422123397,-59.0479721059572,
2.6772123254105));
#237901=CARTESIAN_POINT('Ctrl Pts',(0.0939861339744225,-59.0485611979308,
2.67776268340007));
#237902=CARTESIAN_POINT('Ctrl Pts',(0.0950785796755408,-59.0491604624442,
2.67832123541475));
#237903=CARTESIAN_POINT('Ctrl Pts',(0.102773626133754,-59.0533816042974,
2.68225560368401));
#237904=CARTESIAN_POINT('Ctrl Pts',(0.109958823466863,-59.0580834293363,
2.68661792998841));
#237905=CARTESIAN_POINT('Ctrl Pts',(0.116642428647153,-59.0631465696368,
2.69130986622527));
#237906=CARTESIAN_POINT('Ctrl Pts',(0.11988396993733,-59.0656021872113,
2.69358545023007));
#237907=CARTESIAN_POINT('Ctrl Pts',(0.123007567718671,-59.0681433715117,
2.69593918853425));
#237908=CARTESIAN_POINT('Ctrl Pts',(0.126014035557039,-59.0707593633742,
2.69836306235434));
#237909=CARTESIAN_POINT('Ctrl Pts',(0.130616727761666,-59.0747642641415,
2.70207384382167));
#237910=CARTESIAN_POINT('Ctrl Pts',(0.134943070277899,-59.0789414743142,
2.70594760814168));
#237911=CARTESIAN_POINT('Ctrl Pts',(0.138985142831362,-59.0832455674826,
2.70995196345647));
#237912=CARTESIAN_POINT('Ctrl Pts',(0.1408623022361,-59.0852444106165,2.71181160678045));
#237913=CARTESIAN_POINT('Ctrl Pts',(0.14267827152774,-59.087270393264,2.71369962772038));
#237914=CARTESIAN_POINT('Ctrl Pts',(0.14443119730936,-59.0893195943181,
2.715611831386));
#237915=CARTESIAN_POINT('Ctrl Pts',(0.144565552163647,-59.0894766575047,
2.71575839426251));
#237916=CARTESIAN_POINT('Ctrl Pts',(0.144699568926416,-59.0896338466132,
2.71590508903148));
#237917=CARTESIAN_POINT('Ctrl Pts',(0.144833247843708,-59.089791160204,
2.71605191409851));
#237918=CARTESIAN_POINT('Ctrl Pts',(0.146711033602715,-59.09200094187,2.71811436362692));
#237919=CARTESIAN_POINT('Ctrl Pts',(0.14852065454552,-59.0942367399981,
2.72020091026899));
#237920=CARTESIAN_POINT('Ctrl Pts',(0.150262619641901,-59.0964928714564,
2.72230624862121));
#237921=CARTESIAN_POINT('Ctrl Pts',(0.156508996679337,-59.104582957626,
2.72985561753033));
#237922=CARTESIAN_POINT('Ctrl Pts',(0.161935290146135,-59.1129958342945,
2.73770089914249));
#237923=CARTESIAN_POINT('Ctrl Pts',(0.166622470787953,-59.1216309196479,
2.74574823346981));
#237924=CARTESIAN_POINT('Ctrl Pts',(0.171773211444284,-59.1311200109801,
2.75459144546915));
#237925=CARTESIAN_POINT('Ctrl Pts',(0.176031864362722,-59.1408779306728,
2.76367911754144));
#237926=CARTESIAN_POINT('Ctrl Pts',(0.179468536017587,-59.1508087658088,
2.77292162564584));
#237927=CARTESIAN_POINT('Ctrl Pts',(0.183179278918004,-59.1615315754565,
2.78290121484572));
#237928=CARTESIAN_POINT('Ctrl Pts',(0.185932239425051,-59.1724570142834,
2.79306229500014));
#237929=CARTESIAN_POINT('Ctrl Pts',(0.187766286100246,-59.1834936683123,
2.80331916685064));
#237930=CARTESIAN_POINT('Ctrl Pts',(0.18958494700837,-59.1944377361543,
2.81348999408552));
#237931=CARTESIAN_POINT('Ctrl Pts',(0.190500000000626,-59.2054925958109,
2.82375635966784));
#237932=CARTESIAN_POINT('Ctrl Pts',(0.190500000000626,-59.2165773020939,
2.8340419886022));
#237933=CARTESIAN_POINT('Origin',(-0.0152399999999944,1.94929247519246E-13,
2.83404198860262));
#237934=CARTESIAN_POINT('Ctrl Pts',(-0.0152399999993361,-62.8464427007194,
2.65878198860218));
#237935=CARTESIAN_POINT('Ctrl Pts',(-0.023828933389605,-62.8464391086777,
2.65878198860218));
#237936=CARTESIAN_POINT('Ctrl Pts',(-0.0323412407614512,-62.8457180711403,
2.65944603041796));
#237937=CARTESIAN_POINT('Ctrl Pts',(-0.0406531130489861,-62.8443658068289,
2.66070439263997));
#237938=CARTESIAN_POINT('Ctrl Pts',(-0.0459640037523977,-62.8435017743088,
2.66150842619525));
#237939=CARTESIAN_POINT('Ctrl Pts',(-0.0511932363882295,-62.8423809556997,
2.66255428265307));
#237940=CARTESIAN_POINT('Ctrl Pts',(-0.0563116129568179,-62.8410338592508,
2.66381699700609));
#237941=CARTESIAN_POINT('Ctrl Pts',(-0.0632971699615973,-62.8391953428953,
2.66554034873208));
#237942=CARTESIAN_POINT('Ctrl Pts',(-0.070073412097744,-62.8369299537502,
2.66766759643912));
#237943=CARTESIAN_POINT('Ctrl Pts',(-0.0765705776088438,-62.8343031482012,
2.67012012783087));
#237944=CARTESIAN_POINT('Ctrl Pts',(-0.0798191603643938,-62.8329897454267,
2.67134639352674));
#237945=CARTESIAN_POINT('Ctrl Pts',(-0.08299818279468,-62.8315859904679,
2.6726537558495));
#237946=CARTESIAN_POINT('Ctrl Pts',(-0.0861004173272267,-62.8301000734872,
2.67403135126878));
#237947=CARTESIAN_POINT('Ctrl Pts',(-0.0876515345935001,-62.8293571149969,
2.67472014897841));
#237948=CARTESIAN_POINT('Ctrl Pts',(-0.0891834722990619,-62.8285936160518,
2.6754264966857));
#237949=CARTESIAN_POINT('Ctrl Pts',(-0.0906954364272254,-62.8278106008699,
2.67614899656039));
#237950=CARTESIAN_POINT('Ctrl Pts',(-0.0910734274592663,-62.8276148470744,
2.67632962152906));
#237951=CARTESIAN_POINT('Ctrl Pts',(-0.0914501705136929,-62.8274178735162,
2.67651125590887));
#237952=CARTESIAN_POINT('Ctrl Pts',(-0.0918256539322006,-62.8272196962036,
2.67669387767461));
#237953=CARTESIAN_POINT('Ctrl Pts',(-0.0929521041877236,-62.8266251642657,
2.67724174297181));
#237954=CARTESIAN_POINT('Ctrl Pts',(-0.0940672158680064,-62.8260197985188,
2.67779849504684));
#237955=CARTESIAN_POINT('Ctrl Pts',(-0.0951706907481964,-62.8254040313371,
2.67836353617946));
#237956=CARTESIAN_POINT('Ctrl Pts',(-0.10279638682687,-62.8211486980554,
2.68226832098843));
#237957=CARTESIAN_POINT('Ctrl Pts',(-0.109916699410765,-62.8164204928783,
2.68659153751325));
#237958=CARTESIAN_POINT('Ctrl Pts',(-0.116542502759065,-62.8113377077395,
2.6912369948611));
#237959=CARTESIAN_POINT('Ctrl Pts',(-0.119835508835773,-62.8088115774774,
2.6935457744115));
#237960=CARTESIAN_POINT('Ctrl Pts',(-0.123006400628657,-62.8061972539431,
2.69593478828053));
#237961=CARTESIAN_POINT('Ctrl Pts',(-0.126056303769311,-62.8035061084564,
2.69839565261158));
#237962=CARTESIAN_POINT('Ctrl Pts',(-0.132784845642624,-62.797569039553,
2.70382468688984));
#237963=CARTESIAN_POINT('Ctrl Pts',(-0.138932019324019,-62.7912680187376,
2.70961155815025));
#237964=CARTESIAN_POINT('Ctrl Pts',(-0.144445113412511,-62.7847385034066,
2.71562701361707));
#237965=CARTESIAN_POINT('Ctrl Pts',(-0.146459116206809,-62.7823531891146,
2.71782453535798));
#237966=CARTESIAN_POINT('Ctrl Pts',(-0.148396130390324,-62.7799396422113,
2.72005051502342));
#237967=CARTESIAN_POINT('Ctrl Pts',(-0.150257579785834,-62.7775029828614,
2.72229986760055));
#237968=CARTESIAN_POINT('Ctrl Pts',(-0.156509991333105,-62.7693185019443,
2.7298552048883));
#237969=CARTESIAN_POINT('Ctrl Pts',(-0.161942805717696,-62.7608162581016,
2.73770845534492));
#237970=CARTESIAN_POINT('Ctrl Pts',(-0.1666359794612,-62.7520965944487,
2.74576706701681));
#237971=CARTESIAN_POINT('Ctrl Pts',(-0.171794333348312,-62.742512651182,
2.75462443584957));
#237972=CARTESIAN_POINT('Ctrl Pts',(-0.176059615357581,-62.7326655363484,
2.76373036323109));
#237973=CARTESIAN_POINT('Ctrl Pts',(-0.179500292056813,-62.7226511116281,
2.77299664636747));
#237974=CARTESIAN_POINT('Ctrl Pts',(-0.183206048283218,-62.7118651471201,
2.78297683033417));
#237975=CARTESIAN_POINT('Ctrl Pts',(-0.185955767119278,-62.7008840239623,
2.7931440147885));
#237976=CARTESIAN_POINT('Ctrl Pts',(-0.187785458035107,-62.6897991274229,
2.80341452427914));
#237977=CARTESIAN_POINT('Ctrl Pts',(-0.189590441945618,-62.6788639144151,
2.81354634721326));
#237978=CARTESIAN_POINT('Ctrl Pts',(-0.190499999999338,-62.6678262782717,
2.82378004209157));
#237979=CARTESIAN_POINT('Ctrl Pts',(-0.190499999999338,-62.6567671111297,
2.83404198860218));
#237980=CARTESIAN_POINT('Ctrl Pts',(-0.190499999999374,-59.2165773020939,
2.8340419886022));
#237981=CARTESIAN_POINT('Ctrl Pts',(-0.190499999999374,-59.2059936184288,
2.82422126442975));
#237982=CARTESIAN_POINT('Ctrl Pts',(-0.189665225487999,-59.1954479901455,
2.8144281502848));
#237983=CARTESIAN_POINT('Ctrl Pts',(-0.188008762313356,-59.1849969778452,
2.80471618166307));
#237984=CARTESIAN_POINT('Ctrl Pts',(-0.186409301376204,-59.1749056059489,
2.79533842146223));
#237985=CARTESIAN_POINT('Ctrl Pts',(-0.184043455437269,-59.1649012152137,
2.78603515650239));
#237986=CARTESIAN_POINT('Ctrl Pts',(-0.180877423725614,-59.1550396955521,
2.77685887346759));
#237987=CARTESIAN_POINT('Ctrl Pts',(-0.177884532218364,-59.1457174710352,
2.76818441216581));
#237988=CARTESIAN_POINT('Ctrl Pts',(-0.174176304385712,-59.1365220583436,
2.75962261521629));
#237989=CARTESIAN_POINT('Ctrl Pts',(-0.169686797570988,-59.1275197082938,
2.75123537701665));
#237990=CARTESIAN_POINT('Ctrl Pts',(-0.165552037111723,-59.1192286949236,
2.7435108713412));
#237991=CARTESIAN_POINT('Ctrl Pts',(-0.16075429390185,-59.1111009786068,
2.73593399449844));
#237992=CARTESIAN_POINT('Ctrl Pts',(-0.15521351501129,-59.1032135992704,
2.7285765781257));
#237993=CARTESIAN_POINT('Ctrl Pts',(-0.153561366594434,-59.10086174197,
2.726382745083));
#237994=CARTESIAN_POINT('Ctrl Pts',(-0.151842962926626,-59.0985314603572,
2.72420861709562));
#237995=CARTESIAN_POINT('Ctrl Pts',(-0.150055686179522,-59.0962253759568,
2.72205663736666));
#237996=CARTESIAN_POINT('Ctrl Pts',(-0.148286670996087,-59.0939428540557,
2.71992664556705));
#237997=CARTESIAN_POINT('Ctrl Pts',(-0.146452235168283,-59.0916862380346,
2.71782089927824));
#237998=CARTESIAN_POINT('Ctrl Pts',(-0.144552116609346,-59.0894604907297,
2.71574387311185));
#237999=CARTESIAN_POINT('Ctrl Pts',(-0.1444199860808,-59.089305716615,2.71559944077426));
#238000=CARTESIAN_POINT('Ctrl Pts',(-0.144287542501481,-59.0891510807049,
2.71545515216009));
#238001=CARTESIAN_POINT('Ctrl Pts',(-0.144154785043327,-59.0889965840072,
2.7153110078167));
#238002=CARTESIAN_POINT('Ctrl Pts',(-0.138334211748957,-59.0822228828152,
2.7089911917603));
#238003=CARTESIAN_POINT('Ctrl Pts',(-0.131883990153634,-59.0757535782844,
2.70298296066791));
#238004=CARTESIAN_POINT('Ctrl Pts',(-0.124808417214922,-59.0697047694307,
2.69736727774094));
#238005=CARTESIAN_POINT('Ctrl Pts',(-0.118212753509866,-59.0640662283032,
2.69213248525398));
#238006=CARTESIAN_POINT('Ctrl Pts',(-0.111072931137383,-59.0587927761315,
2.68723866185448));
#238007=CARTESIAN_POINT('Ctrl Pts',(-0.103389544768496,-59.0540076654701,
2.68278595829549));
#238008=CARTESIAN_POINT('Ctrl Pts',(-0.100578862632642,-59.0522572100838,
2.68115710172775));
#238009=CARTESIAN_POINT('Ctrl Pts',(-0.0976954648434998,-59.0505724231957,
2.67958763637763));
#238010=CARTESIAN_POINT('Ctrl Pts',(-0.09473955852473,-59.0489605442858,
2.67808378645302));
#238011=CARTESIAN_POINT('Ctrl Pts',(-0.0940287618032339,-59.0485729412561,
2.67772216078538));
#238012=CARTESIAN_POINT('Ctrl Pts',(-0.0933131922161383,-59.0481896206933,
2.67736403603501));
#238013=CARTESIAN_POINT('Ctrl Pts',(-0.092592927196552,-59.0478106940135,
2.67700956934417));
#238014=CARTESIAN_POINT('Ctrl Pts',(-0.0918951704588278,-59.0474436087924,
2.67666617973741));
#238015=CARTESIAN_POINT('Ctrl Pts',(-0.0911930071928101,-59.0470806471269,
2.67632622314056));
#238016=CARTESIAN_POINT('Ctrl Pts',(-0.0904865115872116,-59.0467219102887,
2.67598984158711));
#238017=CARTESIAN_POINT('Ctrl Pts',(-0.0827460357491968,-59.0427915336439,
2.67230439292155));
#238018=CARTESIAN_POINT('Ctrl Pts',(-0.0744802459935639,-59.0393660724127,
2.66904964539906));
#238019=CARTESIAN_POINT('Ctrl Pts',(-0.0658168714600205,-59.0365841602687,
2.66640203566654));
#238020=CARTESIAN_POINT('Ctrl Pts',(-0.0622239118135767,-59.0354304183827,
2.66530399299372));
#238021=CARTESIAN_POINT('Ctrl Pts',(-0.0585629032857959,-59.0343871039215,
2.66430995142194));
#238022=CARTESIAN_POINT('Ctrl Pts',(-0.0548440714993542,-59.033462655426,
2.66343053473297));
#238023=CARTESIAN_POINT('Ctrl Pts',(-0.0485012163577858,-59.0318859121825,
2.66193059792821));
#238024=CARTESIAN_POINT('Ctrl Pts',(-0.0419914004938017,-59.0306571138135,
2.66076519817064));
#238025=CARTESIAN_POINT('Ctrl Pts',(-0.0353717968082149,-59.0298212958154,
2.65997805604397));
#238026=CARTESIAN_POINT('Ctrl Pts',(-0.0320619949654215,-59.0294033868163,
2.65958448498063));
#238027=CARTESIAN_POINT('Ctrl Pts',(-0.0287246785540649,-59.0290851681635,
2.65928526260699));
#238028=CARTESIAN_POINT('Ctrl Pts',(-0.0253670368742519,-59.0288723192862,
2.65908463971261));
#238029=CARTESIAN_POINT('Ctrl Pts',(-0.0220093951944389,-59.028659470409,
2.65888401681823));
#238030=CARTESIAN_POINT('Ctrl Pts',(-0.0186314705073835,-59.0285519740189,
2.6587819886022));
#238031=CARTESIAN_POINT('Ctrl Pts',(-0.0152399999993761,-59.0285534841294,
2.6587819886022));
#238032=CARTESIAN_POINT('Origin',(6.10537907909441,-57.9430040808455,2.83404198860222));
#238033=CARTESIAN_POINT('Ctrl Pts',(6.73887200051396,-62.2936141127567,
2.83404198860219));
#238034=CARTESIAN_POINT('Ctrl Pts',(6.73998108195386,-62.3041663177854,
2.82419652440036));
#238035=CARTESIAN_POINT('Ctrl Pts',(6.74025426844153,-62.3147747227668,
2.81438790575631));
#238036=CARTESIAN_POINT('Ctrl Pts',(6.73970068257657,-62.3253809467523,
2.80466781256892));
#238037=CARTESIAN_POINT('Ctrl Pts',(6.73916508495583,-62.3356425316141,
2.79526356453073));
#238038=CARTESIAN_POINT('Ctrl Pts',(6.73785543637712,-62.3459033574826,
2.7859410249623));
#238039=CARTESIAN_POINT('Ctrl Pts',(6.73573381164848,-62.3561113603647,
2.77675109088778));
#238040=CARTESIAN_POINT('Ctrl Pts',(6.7337268852973,-62.3657675025187,2.76805797913679));
#238041=CARTESIAN_POINT('Ctrl Pts',(6.73099321743878,-62.3753772873479,
2.75948271210155));
#238042=CARTESIAN_POINT('Ctrl Pts',(6.72746117704644,-62.3848821415109,
2.75108575573215));
#238043=CARTESIAN_POINT('Ctrl Pts',(6.72420791240144,-62.3936367996036,
2.74335155163256));
#238044=CARTESIAN_POINT('Ctrl Pts',(6.72027708243777,-62.4023029414998,
2.73576818685925));
#238045=CARTESIAN_POINT('Ctrl Pts',(6.71558140886371,-62.4108128192388,
2.72840626160476));
#238046=CARTESIAN_POINT('Ctrl Pts',(6.714219372456,-62.4132812112858,2.7262708469365));
#238047=CARTESIAN_POINT('Ctrl Pts',(6.71279278199583,-62.4157362792955,
2.72415424587485));
#238048=CARTESIAN_POINT('Ctrl Pts',(6.7112989968966,-62.4181758915947,2.72205867173213));
#238049=CARTESIAN_POINT('Ctrl Pts',(6.70967963780731,-62.4208205881799,
2.71978693462816));
#238050=CARTESIAN_POINT('Ctrl Pts',(6.70798448411237,-62.4234440047026,
2.71754411340717));
#238051=CARTESIAN_POINT('Ctrl Pts',(6.70621108803186,-62.4260429761971,
2.71533341844214));
#238052=CARTESIAN_POINT('Ctrl Pts',(6.70134398857332,-62.4331758738573,
2.70926614876362));
#238053=CARTESIAN_POINT('Ctrl Pts',(6.69585818364757,-62.4400912556835,
2.70347381860379));
#238054=CARTESIAN_POINT('Ctrl Pts',(6.68976801333951,-62.4466864116139,
2.69804914171366));
#238055=CARTESIAN_POINT('Ctrl Pts',(6.68419583815074,-62.4527206212308,
2.6930858568718));
#238056=CARTESIAN_POINT('Ctrl Pts',(6.67811620689392,-62.4584752900412,
2.68842799053166));
#238057=CARTESIAN_POINT('Ctrl Pts',(6.67150703079258,-62.4638645712583,
2.68414767054201));
#238058=CARTESIAN_POINT('Ctrl Pts',(6.66826062508132,-62.4665117685874,
2.68204519134531));
#238059=CARTESIAN_POINT('Ctrl Pts',(6.66488629458047,-62.4690703232298,
2.68003431778478));
#238060=CARTESIAN_POINT('Ctrl Pts',(6.66138078591774,-62.4715267736416,
2.67812693945224));
#238061=CARTESIAN_POINT('Ctrl Pts',(6.66071564979311,-62.4719928611811,
2.67776503299176));
#238062=CARTESIAN_POINT('Ctrl Pts',(6.66004526561052,-62.4724551899378,
2.67740659639896));
#238063=CARTESIAN_POINT('Ctrl Pts',(6.6593696982092,-62.4729136358126,2.67705178968828));
#238064=CARTESIAN_POINT('Ctrl Pts',(6.65871524228918,-62.4733577552539,
2.6767080706873));
#238065=CARTESIAN_POINT('Ctrl Pts',(6.65805592206515,-62.4737982306997,
2.67636775825238));
#238066=CARTESIAN_POINT('Ctrl Pts',(6.65739180030972,-62.4742349489457,
2.67603099699228));
#238067=CARTESIAN_POINT('Ctrl Pts',(6.65015433826464,-62.4789942144023,
2.67236104217096));
#238068=CARTESIAN_POINT('Ctrl Pts',(6.64234165497504,-62.4833100626577,
2.66911440541437));
#238069=CARTESIAN_POINT('Ctrl Pts',(6.63406423386179,-62.4870273554126,
2.66646778189592));
#238070=CARTESIAN_POINT('Ctrl Pts',(6.63056862752553,-62.4885971912262,
2.66535009634939));
#238071=CARTESIAN_POINT('Ctrl Pts',(6.62699051141425,-62.4900605069388,
2.66433897912313));
#238072=CARTESIAN_POINT('Ctrl Pts',(6.62333954252063,-62.4914070226218,
2.66344564884764));
#238073=CARTESIAN_POINT('Ctrl Pts',(6.61719140213135,-62.4936745213864,
2.66194130298556));
#238074=CARTESIAN_POINT('Ctrl Pts',(6.61083770188589,-62.4956084911388,
2.6607720670539));
#238075=CARTESIAN_POINT('Ctrl Pts',(6.60433062536211,-62.4971561593219,
2.65998225155684));
#238076=CARTESIAN_POINT('Ctrl Pts',(6.60270385623117,-62.4975430763676,
2.65978479768258));
#238077=CARTESIAN_POINT('Ctrl Pts',(6.60106746196622,-62.4979056188881,
2.65961098966592));
#238078=CARTESIAN_POINT('Ctrl Pts',(6.5994222184581,-62.4982426563693,2.65946139030471));
#238079=CARTESIAN_POINT('Ctrl Pts',(6.59695435319593,-62.498748212591,2.6592369912629));
#238080=CARTESIAN_POINT('Ctrl Pts',(6.59446659126666,-62.4991963674671,
2.65906707562411));
#238081=CARTESIAN_POINT('Ctrl Pts',(6.59196174500359,-62.4995849724119,
2.65895332562889));
#238082=CARTESIAN_POINT('Ctrl Pts',(6.58945689874051,-62.4999735773567,
2.65883957563366));
#238083=CARTESIAN_POINT('Ctrl Pts',(6.58693497617713,-62.5003026407459,
2.65878198860218));
#238084=CARTESIAN_POINT('Ctrl Pts',(6.58439859103091,-62.5005702980928,
2.65878198860218));
#238085=CARTESIAN_POINT('Ctrl Pts',(6.18532049829458,-58.7035958781036,
2.65878198860221));
#238086=CARTESIAN_POINT('Ctrl Pts',(6.19390281910186,-58.7026899760168,
2.65878198860221));
#238087=CARTESIAN_POINT('Ctrl Pts',(6.20248552904368,-58.7025003609926,
2.65945335517809));
#238088=CARTESIAN_POINT('Ctrl Pts',(6.21093474935395,-58.7029569544311,
2.66072561226544));
#238089=CARTESIAN_POINT('Ctrl Pts',(6.21639207873494,-58.7032518669431,
2.66154735980284));
#238090=CARTESIAN_POINT('Ctrl Pts',(6.22179377937545,-58.7038154335196,
2.66261895766835));
#238091=CARTESIAN_POINT('Ctrl Pts',(6.22710604846926,-58.7046202140514,
2.66391429250988));
#238092=CARTESIAN_POINT('Ctrl Pts',(6.23414715684702,-58.7056869045455,
2.66563118464085));
#238093=CARTESIAN_POINT('Ctrl Pts',(6.24102913891703,-58.707182795565,2.66774105138661));
#238094=CARTESIAN_POINT('Ctrl Pts',(6.24767922440805,-58.7090548163567,
2.67016894181711));
#238095=CARTESIAN_POINT('Ctrl Pts',(6.25100426715356,-58.7099908267526,
2.67138288703237));
#238096=CARTESIAN_POINT('Ctrl Pts',(6.2542715337672,-58.7110208470225,2.67267613167513));
#238097=CARTESIAN_POINT('Ctrl Pts',(6.25747333351575,-58.7121380880305,
2.67403835432515));
#238098=CARTESIAN_POINT('Ctrl Pts',(6.25907423339003,-58.7126967085345,
2.67471946565015));
#238099=CARTESIAN_POINT('Ctrl Pts',(6.260658782884,-58.7132771324568,2.67541781389484));
#238100=CARTESIAN_POINT('Ctrl Pts',(6.26222612320572,-58.7138784999413,
2.6761320724413));
#238101=CARTESIAN_POINT('Ctrl Pts',(6.26261795828615,-58.7140288418124,
2.67631063707792));
#238102=CARTESIAN_POINT('Ctrl Pts',(6.26300871814067,-58.7141804926176,
2.67649019601807));
#238103=CARTESIAN_POINT('Ctrl Pts',(6.26339839005111,-58.7143334388433,
2.67667072836618));
#238104=CARTESIAN_POINT('Ctrl Pts',(6.26456740578242,-58.7147922775205,
2.67721232541052));
#238105=CARTESIAN_POINT('Ctrl Pts',(6.26572662828427,-58.7152627751828,
2.67776268340008));
#238106=CARTESIAN_POINT('Ctrl Pts',(6.26687572965221,-58.7157445651921,
2.67832123541477));
#238107=CARTESIAN_POINT('Ctrl Pts',(6.27496985131181,-58.7191382318075,
2.68225560368397));
#238108=CARTESIAN_POINT('Ctrl Pts',(6.2826071619279,-58.7230632421214,2.6866179299883));
#238109=CARTESIAN_POINT('Ctrl Pts',(6.28978339589452,-58.7274000190308,
2.69130986622508));
#238110=CARTESIAN_POINT('Ctrl Pts',(6.29326386161389,-58.7295033511457,
2.69358545022994));
#238111=CARTESIAN_POINT('Ctrl Pts',(6.29663597408966,-58.7317041096967,
2.69593918853419));
#238112=CARTESIAN_POINT('Ctrl Pts',(6.29989941779204,-58.7339915094191,
2.69836306235435));
#238113=CARTESIAN_POINT('Ctrl Pts',(6.30489552208993,-58.737493358578,2.70207384382168));
#238114=CARTESIAN_POINT('Ctrl Pts',(6.30963480180928,-58.7411954596214,
2.70594760814168));
#238115=CARTESIAN_POINT('Ctrl Pts',(6.31410463171103,-58.7450534628847,
2.70995196345648));
#238116=CARTESIAN_POINT('Ctrl Pts',(6.31618044384124,-58.7468451395589,
2.71181160678046));
#238117=CARTESIAN_POINT('Ctrl Pts',(6.31819823791584,-58.7486702031821,
2.71369962772039));
#238118=CARTESIAN_POINT('Ctrl Pts',(6.32015576082374,-58.7505249478603,
2.71561183138601));
#238119=CARTESIAN_POINT('Ctrl Pts',(6.3203057972416,-58.7506671067318,2.71575839426252));
#238120=CARTESIAN_POINT('Ctrl Pts',(6.32045551058247,-58.7508094261756,
2.71590508903149));
#238121=CARTESIAN_POINT('Ctrl Pts',(6.32060490094057,-58.7509519047343,
2.71605191409852));
#238122=CARTESIAN_POINT('Ctrl Pts',(6.32270338507441,-58.7529532989254,
2.71811436362693));
#238123=CARTESIAN_POINT('Ctrl Pts',(6.32473679726686,-58.7549876922213,
2.72020091026899));
#238124=CARTESIAN_POINT('Ctrl Pts',(6.32670504965044,-58.7570493794207,
2.72230624862122));
#238125=CARTESIAN_POINT('Ctrl Pts',(6.3337628526565,-58.7644422230597,2.72985561753095));
#238126=CARTESIAN_POINT('Ctrl Pts',(6.34003880539021,-58.7722418109929,
2.73770089914377));
#238127=CARTESIAN_POINT('Ctrl Pts',(6.34560292136856,-58.7803396486564,
2.74574823347179));
#238128=CARTESIAN_POINT('Ctrl Pts',(6.35171732586367,-58.7892383587485,
2.75459144547171));
#238129=CARTESIAN_POINT('Ctrl Pts',(6.35697262978615,-58.7984976730916,
2.7636791175446));
#238130=CARTESIAN_POINT('Ctrl Pts',(6.3614285299299,-58.8080148760675,2.77292162564961));
#238131=CARTESIAN_POINT('Ctrl Pts',(6.36623978380681,-58.8182910667895,
2.78290121485001));
#238132=CARTESIAN_POINT('Ctrl Pts',(6.37011968263915,-58.8288688921888,
2.79306229500494));
#238133=CARTESIAN_POINT('Ctrl Pts',(6.37309732669983,-58.8396533761922,
2.80331916685595));
#238134=CARTESIAN_POINT('Ctrl Pts',(6.3760499913858,-58.8503473894538,2.8134899940891));
#238135=CARTESIAN_POINT('Ctrl Pts',(6.37811557911303,-58.8612460403475,
2.82375635966963));
#238136=CARTESIAN_POINT('Ctrl Pts',(6.37927424642637,-58.8722700234478,
2.83404198860221));
#238137=CARTESIAN_POINT('Origin',(-0.0151565136854075,-0.00159301378000414,
2.83404198860263));
#238138=CARTESIAN_POINT('Ctrl Pts',(6.55408556366009,-62.5037563256532,
2.65878198860219));
#238139=CARTESIAN_POINT('Ctrl Pts',(6.54554330587499,-62.5046505412975,
2.65878198860219));
#238140=CARTESIAN_POINT('Ctrl Pts',(6.53700226086782,-62.5048232320876,
2.65944603041798));
#238141=CARTESIAN_POINT('Ctrl Pts',(6.52859457177595,-62.5043472028587,
2.66070439264));
#238142=CARTESIAN_POINT('Ctrl Pts',(6.52322245869602,-62.5040430428429,
2.66150842619527));
#238143=CARTESIAN_POINT('Ctrl Pts',(6.51790471489697,-62.5034749678469,
2.66255428265308));
#238144=CARTESIAN_POINT('Ctrl Pts',(6.51267356740915,-62.5026702669704,
2.66381699700608));
#238145=CARTESIAN_POINT('Ctrl Pts',(6.50553410072719,-62.5015720117387,
2.66554034873208));
#238146=CARTESIAN_POINT('Ctrl Pts',(6.49855818190841,-62.5000273428096,
2.66766759643912));
#238147=CARTESIAN_POINT('Ctrl Pts',(6.49182203260243,-62.4980940659027,
2.67012012783088));
#238148=CARTESIAN_POINT('Ctrl Pts',(6.48845395794944,-62.4971274274492,
2.67134639352676));
#238149=CARTESIAN_POINT('Ctrl Pts',(6.48514561818799,-62.4960636607363,
2.67265375584952));
#238150=CARTESIAN_POINT('Ctrl Pts',(6.48190505740227,-62.4949101555727,
2.6740313512688));
#238151=CARTESIAN_POINT('Ctrl Pts',(6.4802847770094,-62.4943334029909,2.67472014897844));
#238152=CARTESIAN_POINT('Ctrl Pts',(6.47868142404743,-62.4937342176671,
2.67542649668573));
#238153=CARTESIAN_POINT('Ctrl Pts',(6.47709589524328,-62.4931135352111,
2.67614899656042));
#238154=CARTESIAN_POINT('Ctrl Pts',(6.47669951304224,-62.4929583645971,
2.6763296215291));
#238155=CARTESIAN_POINT('Ctrl Pts',(6.47630424448235,-62.4928018504532,
2.67651125590891));
#238156=CARTESIAN_POINT('Ctrl Pts',(6.47591010283135,-62.4926440074814,
2.67669387767464));
#238157=CARTESIAN_POINT('Ctrl Pts',(6.47472767787836,-62.4921704785658,
2.67724174297184));
#238158=CARTESIAN_POINT('Ctrl Pts',(6.47355539694529,-62.4916849899862,
2.67779849504688));
#238159=CARTESIAN_POINT('Ctrl Pts',(6.47239360181871,-62.491187940575,2.67836353617949));
#238160=CARTESIAN_POINT('Ctrl Pts',(6.46436487665244,-62.4877530207467,
2.68226832098846));
#238161=CARTESIAN_POINT('Ctrl Pts',(6.45678933786472,-62.4837949925046,
2.68659153751326));
#238162=CARTESIAN_POINT('Ctrl Pts',(6.44966853564076,-62.4794326364365,
2.6912369948611));
#238163=CARTESIAN_POINT('Ctrl Pts',(6.44612951648157,-62.4772645574451,
2.69354577441151));
#238164=CARTESIAN_POINT('Ctrl Pts',(6.44270272394416,-62.4749960038949,
2.69593478828055));
#238165=CARTESIAN_POINT('Ctrl Pts',(6.43938822718985,-62.4726384024731,
2.6983956526116));
#238166=CARTESIAN_POINT('Ctrl Pts',(6.43207595228416,-62.4674371815965,
2.70382468688986));
#238167=CARTESIAN_POINT('Ctrl Pts',(6.42530381744052,-62.4618132330507,
2.70961155815027));
#238168=CARTESIAN_POINT('Ctrl Pts',(6.41913840445487,-62.4558957623408,
2.71562701361707));
#238169=CARTESIAN_POINT('Ctrl Pts',(6.41688610134126,-62.4537340356672,
2.71782453535798));
#238170=CARTESIAN_POINT('Ctrl Pts',(6.41470741397529,-62.4515361835423,
2.72005051502342));
#238171=CARTESIAN_POINT('Ctrl Pts',(6.41260146153699,-62.449307446912,2.72229986760055));
#238172=CARTESIAN_POINT('Ctrl Pts',(6.40552779014133,-62.4418213564083,
2.72985520488845));
#238173=CARTESIAN_POINT('Ctrl Pts',(6.39923601079907,-62.4339335724856,
2.73770845534527));
#238174=CARTESIAN_POINT('Ctrl Pts',(6.39365709371045,-62.4257522463017,
2.74576706701739));
#238175=CARTESIAN_POINT('Ctrl Pts',(6.3875252029639,-62.4167599996838,2.75462443585034));
#238176=CARTESIAN_POINT('Ctrl Pts',(6.38225398283455,-62.4074126717492,
2.76373036323206));
#238177=CARTESIAN_POINT('Ctrl Pts',(6.37778536209574,-62.3978127557432,
2.77299664636864));
#238178=CARTESIAN_POINT('Ctrl Pts',(6.37297246609485,-62.387473234881,2.78297683033545));
#238179=CARTESIAN_POINT('Ctrl Pts',(6.36908997057768,-62.3768396913491,
2.79314401478987));
#238180=CARTESIAN_POINT('Ctrl Pts',(6.36611161569944,-62.3660067738125,
2.80341452428055));
#238181=CARTESIAN_POINT('Ctrl Pts',(6.3631734786686,-62.3553201372404,2.81354634721426));
#238182=CARTESIAN_POINT('Ctrl Pts',(6.36111515612499,-62.3444380411286,
2.82378004209212));
#238183=CARTESIAN_POINT('Ctrl Pts',(6.35995915837865,-62.3334394572617,
2.83404198860219));
#238184=CARTESIAN_POINT('Ctrl Pts',(6.00036140429106,-58.9120953679528,
2.83404198860221));
#238185=CARTESIAN_POINT('Ctrl Pts',(5.99925510810183,-58.9015696628141,
2.82422126442971));
#238186=CARTESIAN_POINT('Ctrl Pts',(5.99898299131244,-58.8909945468891,
2.8144281502847));
#238187=CARTESIAN_POINT('Ctrl Pts',(5.99953795195317,-58.8804276387775,
2.80471618166292));
#238188=CARTESIAN_POINT('Ctrl Pts',(6.00007381527937,-58.8702243592784,
2.79533842146204));
#238189=CARTESIAN_POINT('Ctrl Pts',(6.00138095727725,-58.8600274754021,
2.78603515650214));
#238190=CARTESIAN_POINT('Ctrl Pts',(6.00349883564024,-58.8498890377475,
2.7768588734673));
#238191=CARTESIAN_POINT('Ctrl Pts',(6.00550089397171,-58.8403050390018,
2.76818441216545));
#238192=CARTESIAN_POINT('Ctrl Pts',(6.00822762538657,-58.8307723843861,
2.75962261521585));
#238193=CARTESIAN_POINT('Ctrl Pts',(6.01175153639678,-58.8213500689036,
2.75123537701615));
#238194=CARTESIAN_POINT('Ctrl Pts',(6.01499699931917,-58.8126722744153,
2.74351087134063));
#238195=CARTESIAN_POINT('Ctrl Pts',(6.01891888229335,-58.804087581854,2.7359339944978));
#238196=CARTESIAN_POINT('Ctrl Pts',(6.02360485257626,-58.795664241304,2.728576578125));
#238197=CARTESIAN_POINT('Ctrl Pts',(6.02500211432165,-58.7931525711891,
2.72638274508255));
#238198=CARTESIAN_POINT('Ctrl Pts',(6.02646752363825,-58.7906554330084,
2.7242086170954));
#238199=CARTESIAN_POINT('Ctrl Pts',(6.02800395803762,-58.7881751602881,
2.72205663736668));
#238200=CARTESIAN_POINT('Ctrl Pts',(6.0295246938641,-58.7857202298422,2.71992664556707));
#238201=CARTESIAN_POINT('Ctrl Pts',(6.03111319985562,-58.7832842250417,
2.71782089927825));
#238202=CARTESIAN_POINT('Ctrl Pts',(6.03277025542088,-58.7808720541405,
2.71574387311186));
#238203=CARTESIAN_POINT('Ctrl Pts',(6.0328854838242,-58.7807043164934,2.71559944077427));
#238204=CARTESIAN_POINT('Ctrl Pts',(6.03300103800968,-58.7805366835712,
2.7154551521601));
#238205=CARTESIAN_POINT('Ctrl Pts',(6.0331169189062,-58.7803691562895,2.71531100781671));
#238206=CARTESIAN_POINT('Ctrl Pts',(6.03819756191484,-58.7730241465596,
2.70899119176029));
#238207=CARTESIAN_POINT('Ctrl Pts',(6.04393622206038,-58.7659160498048,
2.70298296066787));
#238208=CARTESIAN_POINT('Ctrl Pts',(6.05034076157616,-58.7591607781928,
2.69736727774089));
#238209=CARTESIAN_POINT('Ctrl Pts',(6.05631090550625,-58.7528636909923,
2.69213248525389));
#238210=CARTESIAN_POINT('Ctrl Pts',(6.06286038933315,-58.7468728126826,
2.68723866185436));
#238211=CARTESIAN_POINT('Ctrl Pts',(6.07000150504366,-58.7413107827882,
2.68278595829535));
#238212=CARTESIAN_POINT('Ctrl Pts',(6.07261381755706,-58.7392761202954,
2.68115710172766));
#238213=CARTESIAN_POINT('Ctrl Pts',(6.07530531160698,-58.7372991657063,
2.6795876363776));
#238214=CARTESIAN_POINT('Ctrl Pts',(6.07807653793614,-58.7353871404928,
2.67808378645304));
#238215=CARTESIAN_POINT('Ctrl Pts',(6.07874292528977,-58.734927362304,2.6777221607854));
#238216=CARTESIAN_POINT('Ctrl Pts',(6.07941450700242,-58.734471344222,2.67736403603502));
#238217=CARTESIAN_POINT('Ctrl Pts',(6.08009121771134,-58.7340192051466,
2.67700956934418));
#238218=CARTESIAN_POINT('Ctrl Pts',(6.0807467812106,-58.7335811954172,2.67666617973743));
#238219=CARTESIAN_POINT('Ctrl Pts',(6.08140715812765,-58.7331468260465,
2.67632622314058));
#238220=CARTESIAN_POINT('Ctrl Pts',(6.08207228526599,-58.7327162055063,
2.67598984158713));
#238221=CARTESIAN_POINT('Ctrl Pts',(6.08935952173666,-58.7279982598318,
2.6723043929216));
#238222=CARTESIAN_POINT('Ctrl Pts',(6.0972219724326,-58.7237275533348,2.66904964539913));
#238223=CARTESIAN_POINT('Ctrl Pts',(6.10554709909255,-58.7200553115699,
2.66640203566663));
#238224=CARTESIAN_POINT('Ctrl Pts',(6.10899977726383,-58.7185323234522,
2.66530399299378));
#238225=CARTESIAN_POINT('Ctrl Pts',(6.11253167434656,-58.7171120447813,
2.66430995142198));
#238226=CARTESIAN_POINT('Ctrl Pts',(6.11613350280284,-58.7158039367396,
2.66343053473299));
#238227=CARTESIAN_POINT('Ctrl Pts',(6.12227679657208,-58.7135728221599,
2.66193059792823));
#238228=CARTESIAN_POINT('Ctrl Pts',(6.12862250657844,-58.7116702942285,
2.66076519817065));
#238229=CARTESIAN_POINT('Ctrl Pts',(6.13511848061151,-58.7101471179282,
2.65997805604398));
#238230=CARTESIAN_POINT('Ctrl Pts',(6.13836646762804,-58.709385529778,2.65958448498064));
#238231=CARTESIAN_POINT('Ctrl Pts',(6.14165223896415,-58.7087202098044,
2.659285262607));
#238232=CARTESIAN_POINT('Ctrl Pts',(6.14496923836547,-58.7081575578105,
2.65908463971262));
#238233=CARTESIAN_POINT('Ctrl Pts',(6.14828623776679,-58.7075949058167,
2.65888401681824));
#238234=CARTESIAN_POINT('Ctrl Pts',(6.15163442139651,-58.7071349090265,
2.65878198860221));
#238235=CARTESIAN_POINT('Ctrl Pts',(6.15500747092375,-58.706781905664,2.65878198860221));
#238236=CARTESIAN_POINT('Origin',(12.128626347365,-56.9874003490099,2.83404198860222));
#238237=CARTESIAN_POINT('Ctrl Pts',(13.21341150919,-61.2479592423874,2.8340419886022));
#238238=CARTESIAN_POINT('Ctrl Pts',(13.2156175207415,-61.2583377107542,
2.82419652440026));
#238239=CARTESIAN_POINT('Ctrl Pts',(13.2169980909554,-61.2688594460194,
2.81438790575614));
#238240=CARTESIAN_POINT('Ctrl Pts',(13.217556189986,-61.2794654334799,2.80466781256871));
#238241=CARTESIAN_POINT('Ctrl Pts',(13.2180961541214,-61.2897267895024,
2.7952635645305));
#238242=CARTESIAN_POINT('Ctrl Pts',(13.2178662282945,-61.3000683010466,
2.78594102496207));
#238243=CARTESIAN_POINT('Ctrl Pts',(13.2168232529024,-61.3104421535934,
2.77675109088757));
#238244=CARTESIAN_POINT('Ctrl Pts',(13.2158366624042,-61.3202551793176,
2.76805797913662));
#238245=CARTESIAN_POINT('Ctrl Pts',(13.2141224659048,-61.3300980668404,
2.75948271210143));
#238246=CARTESIAN_POINT('Ctrl Pts',(13.2116033021986,-61.3399200511723,
2.75108575573207));
#238247=CARTESIAN_POINT('Ctrl Pts',(13.2092829702346,-61.3489668090859,
2.74335155163254));
#238248=CARTESIAN_POINT('Ctrl Pts',(13.2062795322636,-61.3579963605655,
2.73576818685928));
#238249=CARTESIAN_POINT('Ctrl Pts',(13.2024991065234,-61.3669504518464,
2.72840626160483));
#238250=CARTESIAN_POINT('Ctrl Pts',(13.201402548721,-61.3695476933562,2.72627084693655));
#238251=CARTESIAN_POINT('Ctrl Pts',(13.2002403977589,-61.372138431555,2.72415424587488));
#238252=CARTESIAN_POINT('Ctrl Pts',(13.1990098046953,-61.3747208224636,
2.72205867173214));
#238253=CARTESIAN_POINT('Ctrl Pts',(13.1976757626944,-61.3775203002413,
2.71978693462817));
#238254=CARTESIAN_POINT('Ctrl Pts',(13.1962641169264,-61.3803065372246,
2.71754411340718));
#238255=CARTESIAN_POINT('Ctrl Pts',(13.1947721021916,-61.3830766416483,
2.71533341844215));
#238256=CARTESIAN_POINT('Ctrl Pts',(13.1906772560442,-61.3906792149758,
2.70926614876363));
#238257=CARTESIAN_POINT('Ctrl Pts',(13.1859443571671,-61.3981301363755,
2.7034738186038));
#238258=CARTESIAN_POINT('Ctrl Pts',(13.1805769309636,-61.405325759495,2.69804914171366));
#238259=CARTESIAN_POINT('Ctrl Pts',(13.1756660273918,-61.4119093639898,
2.69308585687178));
#238260=CARTESIAN_POINT('Ctrl Pts',(13.1702212276784,-61.4182680026348,
2.6884279905316));
#238261=CARTESIAN_POINT('Ctrl Pts',(13.164211590619,-61.424318607827,2.68414767054194));
#238262=CARTESIAN_POINT('Ctrl Pts',(13.1612596765267,-61.4272906453322,
2.68204519134527));
#238263=CARTESIAN_POINT('Ctrl Pts',(13.1581712727464,-61.4301878975263,
2.68003431778476));
#238264=CARTESIAN_POINT('Ctrl Pts',(13.1549417366136,-61.4329973166792,
2.67812693945224));
#238265=CARTESIAN_POINT('Ctrl Pts',(13.1543289635885,-61.4335303765994,
2.67776503299176));
#238266=CARTESIAN_POINT('Ctrl Pts',(13.1537105783551,-61.4340602468992,
2.67740659639897));
#238267=CARTESIAN_POINT('Ctrl Pts',(13.1530866324255,-61.4345867973818,
2.67705178968828));
#238268=CARTESIAN_POINT('Ctrl Pts',(13.1524821848061,-61.4350968931619,
2.6767080706873));
#238269=CARTESIAN_POINT('Ctrl Pts',(13.1518725186287,-61.435603873367,2.67636775825238));
#238270=CARTESIAN_POINT('Ctrl Pts',(13.1512576844889,-61.4361076188512,
2.67603099699228));
#238271=CARTESIAN_POINT('Ctrl Pts',(13.1445573487226,-61.4415973333393,
2.67236104217094));
#238272=CARTESIAN_POINT('Ctrl Pts',(13.1372385931153,-61.4467061867047,
2.66911440541433));
#238273=CARTESIAN_POINT('Ctrl Pts',(13.1293950794801,-61.4512683418497,
2.66646778189587));
#238274=CARTESIAN_POINT('Ctrl Pts',(13.1260827149663,-61.4531949682969,
2.66535009634936));
#238275=CARTESIAN_POINT('Ctrl Pts',(13.1226771582923,-61.4550242827914,
2.66433897912312));
#238276=CARTESIAN_POINT('Ctrl Pts',(13.1191869390034,-61.4567450522886,
2.66344564884764));
#238277=CARTESIAN_POINT('Ctrl Pts',(13.1133094969318,-61.4596427851245,
2.66194130298557));
#238278=CARTESIAN_POINT('Ctrl Pts',(13.1071927578073,-61.462230302911,2.66077206705391));
#238279=CARTESIAN_POINT('Ctrl Pts',(13.1008831031064,-61.4644496675151,
2.65998225155685));
#238280=CARTESIAN_POINT('Ctrl Pts',(13.0993056894312,-61.4650045086662,
2.65978479768258));
#238281=CARTESIAN_POINT('Ctrl Pts',(13.0977161555177,-61.4655361149186,
2.65961098966593));
#238282=CARTESIAN_POINT('Ctrl Pts',(13.0961151548357,-61.4660432808488,
2.65946139030472));
#238283=CARTESIAN_POINT('Ctrl Pts',(13.0937136538126,-61.4668040297441,
2.6592369912629));
#238284=CARTESIAN_POINT('Ctrl Pts',(13.091286365044,-61.4675097715122,2.65906707562412));
#238285=CARTESIAN_POINT('Ctrl Pts',(13.0888358608685,-61.4681580753691,
2.65895332562889));
#238286=CARTESIAN_POINT('Ctrl Pts',(13.0863853566931,-61.468806379226,2.65883957563367));
#238287=CARTESIAN_POINT('Ctrl Pts',(13.0839116459757,-61.4693972526616,
2.65878198860219));
#238288=CARTESIAN_POINT('Ctrl Pts',(13.0814171332239,-61.4699285681951,
2.65878198860219));
#238289=CARTESIAN_POINT('Ctrl Pts',(12.2876333308477,-57.7354693911201,
2.65878198860222));
#238290=CARTESIAN_POINT('Ctrl Pts',(12.296073944251,-57.7336713548543,2.65878198860222));
#238291=CARTESIAN_POINT('Ctrl Pts',(12.3045898170431,-57.7325856410802,
2.65945335517815));
#238292=CARTESIAN_POINT('Ctrl Pts',(12.3130404786512,-57.7321565492372,
2.66072561226561));
#238293=CARTESIAN_POINT('Ctrl Pts',(12.3184987389622,-57.731879399934,2.66154735980299));
#238294=CARTESIAN_POINT('Ctrl Pts',(12.3239297572692,-57.7318752477668,
2.66261895766843));
#238295=CARTESIAN_POINT('Ctrl Pts',(12.3292970476689,-57.7321203363018,
2.66391429250987));
#238296=CARTESIAN_POINT('Ctrl Pts',(12.3364110836364,-57.7324451871154,
2.66563118464083));
#238297=CARTESIAN_POINT('Ctrl Pts',(12.343411728678,-57.7332135204773,2.66774105138659));
#238298=CARTESIAN_POINT('Ctrl Pts',(12.3502210637615,-57.7343801629263,
2.6701689418171));
#238299=CARTESIAN_POINT('Ctrl Pts',(12.3536257313032,-57.7349634841508,
2.67138288703235));
#238300=CARTESIAN_POINT('Ctrl Pts',(12.3569827659245,-57.7356463395037,
2.67267613167511));
#238301=CARTESIAN_POINT('Ctrl Pts',(12.3602838093647,-57.7364227809411,
2.67403835432513));
#238302=CARTESIAN_POINT('Ctrl Pts',(12.3619343310848,-57.7368110016598,
2.67471946565014));
#238303=CARTESIAN_POINT('Ctrl Pts',(12.3635708710714,-57.7372226154356,
2.67541781389483));
#238304=CARTESIAN_POINT('Ctrl Pts',(12.3651924853579,-57.7376568568908,
2.67613207244129));
#238305=CARTESIAN_POINT('Ctrl Pts',(12.3655978889295,-57.7377654172546,
2.67631063707791));
#238306=CARTESIAN_POINT('Ctrl Pts',(12.3660023599863,-57.7378753917738,
2.67649019601806));
#238307=CARTESIAN_POINT('Ctrl Pts',(12.3664058844672,-57.7379867683381,
2.67667072836617));
#238308=CARTESIAN_POINT('Ctrl Pts',(12.3676164579098,-57.7383208980311,
2.67721232541051));
#238309=CARTESIAN_POINT('Ctrl Pts',(12.3688185104671,-57.7386676465112,
2.67776268340007));
#238310=CARTESIAN_POINT('Ctrl Pts',(12.3700116777068,-57.7390266834243,
2.67832123541476));
#238311=CARTESIAN_POINT('Ctrl Pts',(12.3784161936774,-57.7415556930804,
2.68225560368407));
#238312=CARTESIAN_POINT('Ctrl Pts',(12.3864219416035,-57.744660885435,2.68661792998854));
#238313=CARTESIAN_POINT('Ctrl Pts',(12.3940121800357,-57.7482237843183,
2.69130986622547));
#238314=CARTESIAN_POINT('Ctrl Pts',(12.3976934374731,-57.7499517864266,
2.69358545023021));
#238315=CARTESIAN_POINT('Ctrl Pts',(12.4012771190731,-57.7517880072568,
2.69593918853433));
#238316=CARTESIAN_POINT('Ctrl Pts',(12.4047617836671,-57.7537217536089,
2.69836306235435));
#238317=CARTESIAN_POINT('Ctrl Pts',(12.410096561694,-57.7566821841671,2.70207384382168));
#238318=CARTESIAN_POINT('Ctrl Pts',(12.4151968540761,-57.7598686150877,
2.70594760814168));
#238319=CARTESIAN_POINT('Ctrl Pts',(12.4200454689344,-57.7632382593548,
2.70995196345648));
#238320=CARTESIAN_POINT('Ctrl Pts',(12.422297190758,-57.7648031395846,2.71181160678046));
#238321=CARTESIAN_POINT('Ctrl Pts',(12.4244947022414,-57.7664072884045,
2.7136996277204));
#238322=CARTESIAN_POINT('Ctrl Pts',(12.426635375245,-57.7680472557359,2.71561183138603));
#238323=CARTESIAN_POINT('Ctrl Pts',(12.426799449396,-57.76817295277,2.71575839426253));
#238324=CARTESIAN_POINT('Ctrl Pts',(12.4269632190243,-57.7682988432676,
2.7159050890315));
#238325=CARTESIAN_POINT('Ctrl Pts',(12.4271266840712,-57.7684249257693,
2.71605191409852));
#238326=CARTESIAN_POINT('Ctrl Pts',(12.4294228751485,-57.7701960047918,
2.71811436362694));
#238327=CARTESIAN_POINT('Ctrl Pts',(12.4316578001011,-57.7720067040167,
2.720200910269));
#238328=CARTESIAN_POINT('Ctrl Pts',(12.4338307751869,-57.773851358681,2.72230624862123));
#238329=CARTESIAN_POINT('Ctrl Pts',(12.4416226773939,-57.7804659622463,
2.72985561753044));
#238330=CARTESIAN_POINT('Ctrl Pts',(12.4486795287422,-57.7875668075255,
2.73770089914271));
#238331=CARTESIAN_POINT('Ctrl Pts',(12.4550596184374,-57.7950386758937,
2.74574823347014));
#238332=CARTESIAN_POINT('Ctrl Pts',(12.4620706960757,-57.8032495086148,
2.75459144546965));
#238333=CARTESIAN_POINT('Ctrl Pts',(12.4682650727925,-57.8119087706216,
2.7636791175421));
#238334=CARTESIAN_POINT('Ctrl Pts',(12.4736913816506,-57.8209080689689,
2.77292162564668));
#238335=CARTESIAN_POINT('Ctrl Pts',(12.4795504333999,-57.8306250526684,
2.78290121484682));
#238336=CARTESIAN_POINT('Ctrl Pts',(12.4845147615742,-57.8407393717705,
2.7930622950015));
#238337=CARTESIAN_POINT('Ctrl Pts',(12.4886033793293,-57.851153528684,2.80331916685226));
#238338=CARTESIAN_POINT('Ctrl Pts',(12.4926576977823,-57.861480321521,2.81348999408662));
#238339=CARTESIAN_POINT('Ctrl Pts',(12.495851189234,-57.8721033557552,2.8237563596684));
#238340=CARTESIAN_POINT('Ctrl Pts',(12.4981558292594,-57.8829458346102,
2.83404198860222));
#238341=CARTESIAN_POINT('Origin',(-0.0149069694351787,-0.00316857416786783,
2.83404198860263));
#238342=CARTESIAN_POINT('Ctrl Pts',(13.0516031943535,-61.4762657165312,
2.65878198860219));
#238343=CARTESIAN_POINT('Ctrl Pts',(13.0432012029372,-61.4780479426478,
2.65878198860219));
#238344=CARTESIAN_POINT('Ctrl Pts',(13.0347249977709,-61.479112469729,2.65944603041803));
#238345=CARTESIAN_POINT('Ctrl Pts',(13.0263136082755,-61.4795178910584,
2.66070439264014));
#238346=CARTESIAN_POINT('Ctrl Pts',(13.0209391308144,-61.4797769359878,
2.6615084261954));
#238347=CARTESIAN_POINT('Ctrl Pts',(13.0155911381662,-61.4797678285534,
2.66255428265317));
#238348=CARTESIAN_POINT('Ctrl Pts',(13.0103045333059,-61.4795143397205,
2.66381699700611));
#238349=CARTESIAN_POINT('Ctrl Pts',(13.0030893784378,-61.4791683783267,
2.66554034873211));
#238350=CARTESIAN_POINT('Ctrl Pts',(12.9959902125628,-61.4783613533296,
2.66766759643915));
#238351=CARTESIAN_POINT('Ctrl Pts',(12.9890888821234,-61.4771427864511,
2.67012012783091));
#238352=CARTESIAN_POINT('Ctrl Pts',(12.9856382169037,-61.4765335030119,
2.67134639352679));
#238353=CARTESIAN_POINT('Ctrl Pts',(12.9822368066739,-61.4758213793956,
2.67265375584955));
#238354=CARTESIAN_POINT('Ctrl Pts',(12.9788934238971,-61.4750129240931,
2.67403135126883));
#238355=CARTESIAN_POINT('Ctrl Pts',(12.9772217325087,-61.4746086964418,
2.67472014897847));
#238356=CARTESIAN_POINT('Ctrl Pts',(12.9755645309609,-61.474180389539,2.67542649668576));
#238357=CARTESIAN_POINT('Ctrl Pts',(12.9739228088661,-61.4737288401358,
2.67614899656045));
#238358=CARTESIAN_POINT('Ctrl Pts',(12.9735123783424,-61.473615952785,2.67632962152912));
#238359=CARTESIAN_POINT('Ctrl Pts',(12.9731029149221,-61.4735016128572,
2.67651125590894));
#238360=CARTESIAN_POINT('Ctrl Pts',(12.972694433337,-61.4733858335867,2.67669387767467));
#238361=CARTESIAN_POINT('Ctrl Pts',(12.9714689885818,-61.4730384957754,
2.67724174297187));
#238362=CARTESIAN_POINT('Ctrl Pts',(12.9702523821512,-61.4726782034774,
2.67779849504691));
#238363=CARTESIAN_POINT('Ctrl Pts',(12.9690449956487,-61.4723053176141,
2.67836353617952));
#238364=CARTESIAN_POINT('Ctrl Pts',(12.9607012057879,-61.4697284449397,
2.68226832098848));
#238365=CARTESIAN_POINT('Ctrl Pts',(12.9527534399846,-61.4665839586183,
2.68659153751326));
#238366=CARTESIAN_POINT('Ctrl Pts',(12.9452156558843,-61.462989826507,2.69123699486108));
#238367=CARTESIAN_POINT('Ctrl Pts',(12.9414693978771,-61.4612035527133,
2.6935457744115));
#238368=CARTESIAN_POINT('Ctrl Pts',(12.9378242492513,-61.4593056238946,
2.69593478828055));
#238369=CARTESIAN_POINT('Ctrl Pts',(12.9342814732034,-61.4573073969123,
2.69839565261162));
#238370=CARTESIAN_POINT('Ctrl Pts',(12.9264655800793,-61.4528990097267,
2.70382468688987));
#238371=CARTESIAN_POINT('Ctrl Pts',(12.919142681,-61.4480137506079,2.70961155815028));
#238372=CARTESIAN_POINT('Ctrl Pts',(12.912392498672,-61.4427731575664,2.71562701361708));
#238373=CARTESIAN_POINT('Ctrl Pts',(12.9099265719433,-61.4408587028411,
2.71782453535799));
#238374=CARTESIAN_POINT('Ctrl Pts',(12.9075300815496,-61.4389006256223,
2.72005051502344));
#238375=CARTESIAN_POINT('Ctrl Pts',(12.9052026993241,-61.4369042302167,
2.72229986760058));
#238376=CARTESIAN_POINT('Ctrl Pts',(12.8973852687049,-61.4301985493012,
2.72985520488788));
#238377=CARTESIAN_POINT('Ctrl Pts',(12.8903034584567,-61.4230116455107,
2.73770845534406));
#238378=CARTESIAN_POINT('Ctrl Pts',(12.8838999218066,-61.4154582931183,
2.74576706701549));
#238379=CARTESIAN_POINT('Ctrl Pts',(12.8768616764793,-61.4071562640856,
2.75462443584776));
#238380=CARTESIAN_POINT('Ctrl Pts',(12.870642270821,-61.398411134332,2.76373036322875));
#238381=CARTESIAN_POINT('Ctrl Pts',(12.8651946651867,-61.3893309057298,
2.77299664636458));
#238382=CARTESIAN_POINT('Ctrl Pts',(12.8593273605072,-61.3795511104685,
2.78297683033057));
#238383=CARTESIAN_POINT('Ctrl Pts',(12.8543546257423,-61.3693816498916,
2.79314401478415));
#238384=CARTESIAN_POINT('Ctrl Pts',(12.8502602383809,-61.3589193990701,
2.80341452427397));
#238385=CARTESIAN_POINT('Ctrl Pts',(12.8462211390724,-61.3485984239579,
2.81354634720985));
#238386=CARTESIAN_POINT('Ctrl Pts',(12.8430366034505,-61.3379910943972,
2.82378004208991));
#238387=CARTESIAN_POINT('Ctrl Pts',(12.8407372733105,-61.327173596589,2.8340419886022));
#238388=CARTESIAN_POINT('Ctrl Pts',(12.1254815933798,-57.9621601888118,
2.83404198860222));
#238389=CARTESIAN_POINT('Ctrl Pts',(12.123281121814,-57.9518077840283,2.82422126443027));
#238390=CARTESIAN_POINT('Ctrl Pts',(12.1219050950924,-57.9413190436452,
2.81442815028583));
#238391=CARTESIAN_POINT('Ctrl Pts',(12.1213524729342,-57.9307520129796,
2.8047161816646));
#238392=CARTESIAN_POINT('Ctrl Pts',(12.1208188676186,-57.9205486151435,
2.79533842146407));
#238393=CARTESIAN_POINT('Ctrl Pts',(12.1210529843541,-57.9102709573202,
2.78603515650452));
#238394=CARTESIAN_POINT('Ctrl Pts',(12.1220995054496,-57.8999666805176,
2.77685887347001));
#238395=CARTESIAN_POINT('Ctrl Pts',(12.123088795635,-57.8902259118393,2.76818441216839));
#238396=CARTESIAN_POINT('Ctrl Pts',(12.1248041559918,-57.8804604570588,
2.75962261521902));
#238397=CARTESIAN_POINT('Ctrl Pts',(12.1273238624907,-57.870721409004,2.7512353770195));
#238398=CARTESIAN_POINT('Ctrl Pts',(12.129644469905,-57.8617519091303,2.74351087134412));
#238399=CARTESIAN_POINT('Ctrl Pts',(12.1326475236725,-57.8528042960128,
2.73593399450142));
#238400=CARTESIAN_POINT('Ctrl Pts',(12.1364273448763,-57.8439372821313,
2.72857657812872));
#238401=CARTESIAN_POINT('Ctrl Pts',(12.1375544112588,-57.8412933175836,
2.726382745085));
#238402=CARTESIAN_POINT('Ctrl Pts',(12.1387507708939,-57.8386566820017,
2.72420861709662));
#238403=CARTESIAN_POINT('Ctrl Pts',(12.1400195294497,-57.8360293953468,
2.72205663736668));
#238404=CARTESIAN_POINT('Ctrl Pts',(12.1412753244192,-57.8334289530878,
2.71992664556707));
#238405=CARTESIAN_POINT('Ctrl Pts',(12.1426004965704,-57.8308402488863,
2.71782089927826));
#238406=CARTESIAN_POINT('Ctrl Pts',(12.1439963340944,-57.8282680826378,
2.71574387311187));
#238407=CARTESIAN_POINT('Ctrl Pts',(12.144093397906,-57.8280892192272,2.71559944077428));
#238408=CARTESIAN_POINT('Ctrl Pts',(12.1441907966618,-57.8279104259143,
2.7154551521601));
#238409=CARTESIAN_POINT('Ctrl Pts',(12.1442885313814,-57.8277317035125,
2.71531100781671));
#238410=CARTESIAN_POINT('Ctrl Pts',(12.1485735795163,-57.8198958587082,
2.70899119176024));
#238411=CARTESIAN_POINT('Ctrl Pts',(12.1535378042506,-57.8122268475249,
2.70298296066779));
#238412=CARTESIAN_POINT('Ctrl Pts',(12.1592011408683,-57.8048391253241,
2.69736727774077));
#238413=CARTESIAN_POINT('Ctrl Pts',(12.1644803548772,-57.7979524842555,
2.69213248525369));
#238414=CARTESIAN_POINT('Ctrl Pts',(12.1703677426432,-57.7913098171243,
2.68723866185408));
#238415=CARTESIAN_POINT('Ctrl Pts',(12.1768883481373,-57.7850318067603,
2.68278595829502));
#238416=CARTESIAN_POINT('Ctrl Pts',(12.1792736699857,-57.7827352293491,
2.68115710172745));
#238417=CARTESIAN_POINT('Ctrl Pts',(12.1817437717242,-57.7804877669873,
2.6795876363775));
#238418=CARTESIAN_POINT('Ctrl Pts',(12.1842999559281,-57.7782965440185,
2.67808378645305));
#238419=CARTESIAN_POINT('Ctrl Pts',(12.1849146328346,-57.7777696280968,
2.6777221607854));
#238420=CARTESIAN_POINT('Ctrl Pts',(12.185534868683,-57.7772459087252,2.67736403603503));
#238421=CARTESIAN_POINT('Ctrl Pts',(12.1861606108971,-57.7767255109844,
2.67700956934419));
#238422=CARTESIAN_POINT('Ctrl Pts',(12.1867667986671,-57.776221375673,2.67666617973744));
#238423=CARTESIAN_POINT('Ctrl Pts',(12.1873781540075,-57.7757203576389,
2.67632622314058));
#238424=CARTESIAN_POINT('Ctrl Pts',(12.1879946254064,-57.7752225713654,
2.67598984158713));
#238425=CARTESIAN_POINT('Ctrl Pts',(12.194748782022,-57.7697687474612,2.67230439292162));
#238426=CARTESIAN_POINT('Ctrl Pts',(12.2021217510032,-57.7646995864525,
2.66904964539918));
#238427=CARTESIAN_POINT('Ctrl Pts',(12.2100174179597,-57.760177248916,2.66640203566668));
#238428=CARTESIAN_POINT('Ctrl Pts',(12.2132919863912,-57.7583017007431,
2.66530399299382));
#238429=CARTESIAN_POINT('Ctrl Pts',(12.2166560758254,-57.7565200187329,
2.66430995142199));
#238430=CARTESIAN_POINT('Ctrl Pts',(12.2201014385652,-57.7548425830504,
2.663430534733));
#238431=CARTESIAN_POINT('Ctrl Pts',(12.22597786375,-57.7519815416927,2.66193059792823));
#238432=CARTESIAN_POINT('Ctrl Pts',(12.232089942972,-57.7494261286931,2.66076519817066));
#238433=CARTESIAN_POINT('Ctrl Pts',(12.2383911161017,-57.7472322823289,
2.65997805604398));
#238434=CARTESIAN_POINT('Ctrl Pts',(12.2415417026665,-57.7461353591468,
2.65958448498064));
#238435=CARTESIAN_POINT('Ctrl Pts',(12.244739929329,-57.7451302272372,2.659285262607));
#238436=CARTESIAN_POINT('Ctrl Pts',(12.2479799447123,-57.7442239366597,
2.65908463971263));
#238437=CARTESIAN_POINT('Ctrl Pts',(12.2512199600955,-57.7433176460823,
2.65888401681825));
#238438=CARTESIAN_POINT('Ctrl Pts',(12.2545017192674,-57.7425101887129,
2.65878198860222));
#238439=CARTESIAN_POINT('Ctrl Pts',(12.2578193919774,-57.7418065394563,
2.65878198860222));
#238440=CARTESIAN_POINT('Origin',(18.0189898472955,-55.4074307335703,2.83404198860224));
#238441=CARTESIAN_POINT('Ctrl Pts',(19.5431821162873,-59.5312589135992,
2.83404198860221));
#238442=CARTESIAN_POINT('Ctrl Pts',(19.5464608884259,-59.5413499366323,
2.82419652440104));
#238443=CARTESIAN_POINT('Ctrl Pts',(19.5489337165498,-59.5516697238472,
2.81438790575766));
#238444=CARTESIAN_POINT('Ctrl Pts',(19.5505973858262,-59.5621592733639,
2.80466781257095));
#238445=CARTESIAN_POINT('Ctrl Pts',(19.5522069957576,-59.5723079749825,
2.79526356453334));
#238446=CARTESIAN_POINT('Ctrl Pts',(19.5530593117982,-59.5826168684371,
2.78594102496549));
#238447=CARTESIAN_POINT('Ctrl Pts',(19.5531064127995,-59.5930429125485,
2.77675109089153));
#238448=CARTESIAN_POINT('Ctrl Pts',(19.5531509674465,-59.6029053082791,
2.76805797914111));
#238449=CARTESIAN_POINT('Ctrl Pts',(19.5524750234021,-59.6128734577593,
2.75948271210642));
#238450=CARTESIAN_POINT('Ctrl Pts',(19.5509963368671,-59.6229049605435,
2.7510857557375));
#238451=CARTESIAN_POINT('Ctrl Pts',(19.549634359627,-59.6321447001044,2.7433515516385));
#238452=CARTESIAN_POINT('Ctrl Pts',(19.5475912199442,-59.641438731511,2.73576818686571));
#238453=CARTESIAN_POINT('Ctrl Pts',(19.544767461174,-59.6507389334354,2.72840626161167));
#238454=CARTESIAN_POINT('Ctrl Pts',(19.543948396093,-59.6534365684892,2.72627084694109));
#238455=CARTESIAN_POINT('Ctrl Pts',(19.5430634173973,-59.6561345922101,
2.72415424587715));
#238456=CARTESIAN_POINT('Ctrl Pts',(19.5421094990035,-59.6588314685158,
2.72205867173219));
#238457=CARTESIAN_POINT('Ctrl Pts',(19.5410753901343,-59.6617550558215,
2.71978693462821));
#238458=CARTESIAN_POINT('Ctrl Pts',(19.5399627185796,-59.6646735866698,
2.7175441134072));
#238459=CARTESIAN_POINT('Ctrl Pts',(19.5387684320161,-59.6675844741791,
2.71533341844217));
#238460=CARTESIAN_POINT('Ctrl Pts',(19.5354907031712,-59.6755734277895,
2.70926614876364));
#238461=CARTESIAN_POINT('Ctrl Pts',(19.5315625649731,-59.6834782549086,
2.70347381860381));
#238462=CARTESIAN_POINT('Ctrl Pts',(19.5269766895189,-59.6911955084645,
2.69804914171367));
#238463=CARTESIAN_POINT('Ctrl Pts',(19.5227808624514,-59.6982563764886,
2.69308585687186));
#238464=CARTESIAN_POINT('Ctrl Pts',(19.5180305486467,-59.7051493183925,
2.68842799053174));
#238465=CARTESIAN_POINT('Ctrl Pts',(19.5126862934705,-59.7117949558629,
2.68414767054212));
#238466=CARTESIAN_POINT('Ctrl Pts',(19.5100612127856,-59.7150592712796,
2.68204519134539));
#238467=CARTESIAN_POINT('Ctrl Pts',(19.5072925729238,-59.7182634781242,
2.68003431778482));
#238468=CARTESIAN_POINT('Ctrl Pts',(19.5043743927945,-59.7213950854342,
2.67812693945226));
#238469=CARTESIAN_POINT('Ctrl Pts',(19.5038206965385,-59.7219892774189,
2.67776503299178));
#238470=CARTESIAN_POINT('Ctrl Pts',(19.5032610854122,-59.7225808838919,
2.67740659639898));
#238471=CARTESIAN_POINT('Ctrl Pts',(19.5026955970365,-59.7231697699851,
2.6770517896883));
#238472=CARTESIAN_POINT('Ctrl Pts',(19.5021477801725,-59.7237402533879,
2.67670807068732));
#238473=CARTESIAN_POINT('Ctrl Pts',(19.5015944476719,-59.724308183771,2.6763677582524));
#238474=CARTESIAN_POINT('Ctrl Pts',(19.5010356373992,-59.7248734373526,
2.67603099699229));
#238475=CARTESIAN_POINT('Ctrl Pts',(19.4949458381923,-59.7310334544116,
2.67236104217082));
#238476=CARTESIAN_POINT('Ctrl Pts',(19.488201196085,-59.7368793392205,2.66911440541411));
#238477=CARTESIAN_POINT('Ctrl Pts',(19.4808775251044,-59.7422363728294,
2.66646778189559));
#238478=CARTESIAN_POINT('Ctrl Pts',(19.4777846933721,-59.7444986813875,
2.6653500963492));
#238479=CARTESIAN_POINT('Ctrl Pts',(19.474589008127,-59.7466739523113,2.66433897912305));
#238480=CARTESIAN_POINT('Ctrl Pts',(19.4712977780161,-59.7487501225116,
2.66344564884766));
#238481=CARTESIAN_POINT('Ctrl Pts',(19.4657554287474,-59.7522463412516,
2.66194130298558));
#238482=CARTESIAN_POINT('Ctrl Pts',(19.4599426670177,-59.7554590576858,
2.66077206705392));
#238483=CARTESIAN_POINT('Ctrl Pts',(19.4538995640369,-59.758325802888,2.65998225155686));
#238484=CARTESIAN_POINT('Ctrl Pts',(19.4523887882917,-59.7590424891886,
2.6597847976826));
#238485=CARTESIAN_POINT('Ctrl Pts',(19.450863529996,-59.7597373347836,2.65961098966594));
#238486=CARTESIAN_POINT('Ctrl Pts',(19.4493243130385,-59.7604090725468,
2.65946139030473));
#238487=CARTESIAN_POINT('Ctrl Pts',(19.4470154876023,-59.7614166791915,
2.65923699126292));
#238488=CARTESIAN_POINT('Ctrl Pts',(19.444675265878,-59.7623722755973,2.65906707562413));
#238489=CARTESIAN_POINT('Ctrl Pts',(19.4423059520267,-59.7632731754136,
2.65895332562891));
#238490=CARTESIAN_POINT('Ctrl Pts',(19.4399366381754,-59.7641740752298,
2.65883957563368));
#238491=CARTESIAN_POINT('Ctrl Pts',(19.4375382417965,-59.7650202849787,
2.6587819886022));
#238492=CARTESIAN_POINT('Ctrl Pts',(19.4351129318427,-59.7658094374947,
2.6587819886022));
#238493=CARTESIAN_POINT('Ctrl Pts',(18.2553202812755,-56.1347810195638,
2.65878198860223));
#238494=CARTESIAN_POINT('Ctrl Pts',(18.2635267101475,-56.1321105487808,
2.65878198860223));
#238495=CARTESIAN_POINT('Ctrl Pts',(18.2718824441049,-56.130140631564,2.65945335517815));
#238496=CARTESIAN_POINT('Ctrl Pts',(18.2802419597936,-56.1288305556595,
2.66072561226558));
#238497=CARTESIAN_POINT('Ctrl Pts',(18.2856413491927,-56.1279843810467,
2.66154735980296));
#238498=CARTESIAN_POINT('Ctrl Pts',(18.2910421817936,-56.1274125556279,
2.6626189576684));
#238499=CARTESIAN_POINT('Ctrl Pts',(18.2964056883429,-56.1270952669248,
2.66391429250985));
#238500=CARTESIAN_POINT('Ctrl Pts',(18.3035147090334,-56.1266747189243,
2.66563118464082));
#238501=CARTESIAN_POINT('Ctrl Pts',(18.3105573165146,-56.1267070766077,
2.66774105138658));
#238502=CARTESIAN_POINT('Ctrl Pts',(18.3174512966904,-56.1271555587351,
2.67016894181709));
#238503=CARTESIAN_POINT('Ctrl Pts',(18.3208982867783,-56.1273797997988,
2.67138288703234));
#238504=CARTESIAN_POINT('Ctrl Pts',(18.3243083090333,-56.1277080087286,
2.67267613167511));
#238505=CARTESIAN_POINT('Ctrl Pts',(18.3276724292424,-56.1281351437406,
2.67403835432513));
#238506=CARTESIAN_POINT('Ctrl Pts',(18.329354489347,-56.1283487112466,2.67471946565014));
#238507=CARTESIAN_POINT('Ctrl Pts',(18.3310250895518,-56.1285870051492,
2.67541781389483));
#238508=CARTESIAN_POINT('Ctrl Pts',(18.3326832110576,-56.1288493629349,
2.6761320724413));
#238509=CARTESIAN_POINT('Ctrl Pts',(18.333097741434,-56.1289149523813,2.67631063707791));
#238510=CARTESIAN_POINT('Ctrl Pts',(18.3335114922235,-56.1289820457105,
2.67649019601806));
#238511=CARTESIAN_POINT('Ctrl Pts',(18.3339244481761,-56.1290506323485,
2.67667072836617));
#238512=CARTESIAN_POINT('Ctrl Pts',(18.3351633160341,-56.1292563922624,
2.67721232541051));
#238513=CARTESIAN_POINT('Ctrl Pts',(18.3363950287075,-56.1294755925115,
2.67776268340008));
#238514=CARTESIAN_POINT('Ctrl Pts',(18.337619189229,-56.1297079426449,2.67832123541478));
#238515=CARTESIAN_POINT('Ctrl Pts',(18.3462420178745,-56.1313445869825,
2.68225560368399));
#238516=CARTESIAN_POINT('Ctrl Pts',(18.3545284904606,-56.1335959402404,
2.68661792998835));
#238517=CARTESIAN_POINT('Ctrl Pts',(18.3624495731173,-56.1363459252316,
2.69130986622515));
#238518=CARTESIAN_POINT('Ctrl Pts',(18.3662912896465,-56.1376796649807,
2.69358545022999));
#238519=CARTESIAN_POINT('Ctrl Pts',(18.3700472768054,-56.1391312300707,
2.69593918853423));
#238520=CARTESIAN_POINT('Ctrl Pts',(18.3737149835769,-56.140690136523,2.69836306235437));
#238521=CARTESIAN_POINT('Ctrl Pts',(18.3793299863885,-56.1430767133838,
2.7020738438217));
#238522=CARTESIAN_POINT('Ctrl Pts',(18.3847354115627,-56.1457125629775,
2.7059476081417));
#238523=CARTESIAN_POINT('Ctrl Pts',(18.3899096889384,-56.1485569297206,
2.7099519634565));
#238524=CARTESIAN_POINT('Ctrl Pts',(18.3923126501199,-56.1498778683509,
2.71181160678048));
#238525=CARTESIAN_POINT('Ctrl Pts',(18.3946658026165,-56.1512435269773,
2.71369962772041));
#238526=CARTESIAN_POINT('Ctrl Pts',(18.3969661720543,-56.1526507491366,
2.71561183138603));
#238527=CARTESIAN_POINT('Ctrl Pts',(18.3971424863078,-56.1527586071704,
2.71575839426254));
#238528=CARTESIAN_POINT('Ctrl Pts',(18.3973185179292,-56.1528666894391,
2.71590508903151));
#238529=CARTESIAN_POINT('Ctrl Pts',(18.3974942667076,-56.1529749944975,
2.71605191409853));
#238530=CARTESIAN_POINT('Ctrl Pts',(18.3999630071785,-56.1544963540392,
2.71811436362695));
#238531=CARTESIAN_POINT('Ctrl Pts',(18.4023749585858,-56.1560635207934,
2.72020091026901));
#238532=CARTESIAN_POINT('Ctrl Pts',(18.404728848804,-56.1576709325,2.72230624862124));
#238533=CARTESIAN_POINT('Ctrl Pts',(18.4131694805012,-56.1634348250113,
2.72985561753041));
#238534=CARTESIAN_POINT('Ctrl Pts',(18.4209299141243,-56.16975912929,2.73770089914263));
#238535=CARTESIAN_POINT('Ctrl Pts',(18.4280560759389,-56.1765231650101,
2.74574823347001));
#238536=CARTESIAN_POINT('Ctrl Pts',(18.4358870118867,-56.183956160759,2.75459144546945));
#238537=CARTESIAN_POINT('Ctrl Pts',(18.4429525945103,-56.1919204977433,
2.76367911754183));
#238538=CARTESIAN_POINT('Ctrl Pts',(18.4492898603074,-56.2003032932664,
2.77292162564633));
#238539=CARTESIAN_POINT('Ctrl Pts',(18.4561325169318,-56.2093546086369,
2.78290121484639));
#238540=CARTESIAN_POINT('Ctrl Pts',(18.4621268842297,-56.2188946068453,
2.79306229500099));
#238541=CARTESIAN_POINT('Ctrl Pts',(18.4672816799273,-56.2288243369867,
2.80331916685167));
#238542=CARTESIAN_POINT('Ctrl Pts',(18.4723932321855,-56.2386707668947,
2.81348999408623));
#238543=CARTESIAN_POINT('Ctrl Pts',(18.4766796388007,-56.2489017962822,
2.82375635966821));
#238544=CARTESIAN_POINT('Ctrl Pts',(18.4801050014197,-56.2594439784235,
2.83404198860223));
#238545=CARTESIAN_POINT('Origin',(-0.0144941013083342,-0.00470941899407953,
2.83404198860263));
#238546=CARTESIAN_POINT('Ctrl Pts',(19.406124729226,-59.7752282754833,2.65878198860221));
#238547=CARTESIAN_POINT('Ctrl Pts',(19.3979550581551,-59.7778789856298,
2.65878198860221));
#238548=CARTESIAN_POINT('Ctrl Pts',(19.3896365599077,-59.7798236858206,
2.65944603041802));
#238549=CARTESIAN_POINT('Ctrl Pts',(19.3813136269528,-59.7811061158275,
2.66070439264007));
#238550=CARTESIAN_POINT('Ctrl Pts',(19.3759956690097,-59.7819255275515,
2.66150842619534));
#238551=CARTESIAN_POINT('Ctrl Pts',(19.3706760212385,-59.7824754874617,
2.66255428265314));
#238552=CARTESIAN_POINT('Ctrl Pts',(19.3653918801545,-59.7827759879491,
2.66381699700612));
#238553=CARTESIAN_POINT('Ctrl Pts',(19.3581800878468,-59.7831861108186,
2.66554034873212));
#238554=CARTESIAN_POINT('Ctrl Pts',(19.3510354548625,-59.7831255716882,
2.66766759643916));
#238555=CARTESIAN_POINT('Ctrl Pts',(19.3440445557102,-59.782635065712,2.67012012783092));
#238556=CARTESIAN_POINT('Ctrl Pts',(19.340549106134,-59.7823898127239,2.6713463935268));
#238557=CARTESIAN_POINT('Ctrl Pts',(19.337091891998,-59.7820371343795,2.67265375584956));
#238558=CARTESIAN_POINT('Ctrl Pts',(19.3336823180315,-59.7815825865435,
2.67403135126883));
#238559=CARTESIAN_POINT('Ctrl Pts',(19.3319775310482,-59.7813553126255,
2.67472014897847));
#238560=CARTESIAN_POINT('Ctrl Pts',(19.3302846375616,-59.7811025767638,
2.67542649668576));
#238561=CARTESIAN_POINT('Ctrl Pts',(19.328604709227,-59.7808251076832,2.67614899656045));
#238562=CARTESIAN_POINT('Ctrl Pts',(19.3281847271434,-59.7807557404131,
2.67632962152913));
#238563=CARTESIAN_POINT('Ctrl Pts',(19.3277655550296,-59.7806848274334,
2.67651125590894));
#238564=CARTESIAN_POINT('Ctrl Pts',(19.3273472089201,-59.7806123803663,
2.67669387767467));
#238565=CARTESIAN_POINT('Ctrl Pts',(19.3260921705918,-59.7803950391649,
2.67724174297187));
#238566=CARTESIAN_POINT('Ctrl Pts',(19.3248445680583,-59.7801638905864,
2.67779849504691));
#238567=CARTESIAN_POINT('Ctrl Pts',(19.3236048185592,-59.7799192536865,
2.67836353617952));
#238568=CARTESIAN_POINT('Ctrl Pts',(19.3150373803116,-59.7782286609223,
2.68226832098846));
#238569=CARTESIAN_POINT('Ctrl Pts',(19.306804464878,-59.7759321681718,2.68659153751323));
#238570=CARTESIAN_POINT('Ctrl Pts',(19.2989322844414,-59.7731456380807,
2.69123699486104));
#238571=CARTESIAN_POINT('Ctrl Pts',(19.2950198323729,-59.7717607402742,
2.69354577441147));
#238572=CARTESIAN_POINT('Ctrl Pts',(19.2911962646698,-59.7702542302925,
2.69593478828054));
#238573=CARTESIAN_POINT('Ctrl Pts',(19.287464024724,-59.7686372707427,2.69839565261162));
#238574=CARTESIAN_POINT('Ctrl Pts',(19.2792301459423,-59.7650700164607,
2.70382468688988));
#238575=CARTESIAN_POINT('Ctrl Pts',(19.271436713842,-59.7609769706898,2.70961155815029));
#238576=CARTESIAN_POINT('Ctrl Pts',(19.2641757185818,-59.7564706723509,
2.71562701361709));
#238577=CARTESIAN_POINT('Ctrl Pts',(19.2615231854473,-59.7548244647403,
2.717824535358));
#238578=CARTESIAN_POINT('Ctrl Pts',(19.2589351484761,-59.7531276155315,
2.72005051502344));
#238579=CARTESIAN_POINT('Ctrl Pts',(19.2564118357501,-59.7513854342762,
2.72229986760057));
#238580=CARTESIAN_POINT('Ctrl Pts',(19.247936295312,-59.7455336317913,2.72985520488834));
#238581=CARTESIAN_POINT('Ctrl Pts',(19.2401420439519,-59.7391263493537,
2.737708455345));
#238582=CARTESIAN_POINT('Ctrl Pts',(19.2329840462271,-59.732283726861,2.74576706701695));
#238583=CARTESIAN_POINT('Ctrl Pts',(19.2251165588069,-59.7247628741795,
2.75462443584974));
#238584=CARTESIAN_POINT('Ctrl Pts',(19.2180171087289,-59.7167157560769,
2.76373036323129));
#238585=CARTESIAN_POINT('Ctrl Pts',(19.2116502033062,-59.7082546997619,
2.77299664636771));
#238586=CARTESIAN_POINT('Ctrl Pts',(19.2047927733656,-59.6991417795832,
2.78297683033439));
#238587=CARTESIAN_POINT('Ctrl Pts',(19.1987842816755,-59.6895478206978,
2.79314401478871));
#238588=CARTESIAN_POINT('Ctrl Pts',(19.1936187207957,-59.6795708631991,
2.80341452427932));
#238589=CARTESIAN_POINT('Ctrl Pts',(19.1885229124293,-59.6697286283138,
2.8135463472134));
#238590=CARTESIAN_POINT('Ctrl Pts',(19.1842470541693,-59.6595122814311,
2.82378004209167));
#238591=CARTESIAN_POINT('Ctrl Pts',(19.1808295835788,-59.648994388456,2.83404198860221));
#238592=CARTESIAN_POINT('Ctrl Pts',(18.1177524687112,-56.3771794532803,
2.83404198860223));
#238593=CARTESIAN_POINT('Ctrl Pts',(18.1144819305957,-56.3671137719644,
2.82422126442995));
#238594=CARTESIAN_POINT('Ctrl Pts',(18.1120170699785,-56.3568263239569,
2.81442815028516));
#238595=CARTESIAN_POINT('Ctrl Pts',(18.1103629196655,-56.3463749453355,
2.8047161816636));
#238596=CARTESIAN_POINT('Ctrl Pts',(18.1087656919998,-56.3362832197238,
2.79533842146289));
#238597=CARTESIAN_POINT('Ctrl Pts',(18.1079242184411,-56.3260373921225,
2.78603515650317));
#238598=CARTESIAN_POINT('Ctrl Pts',(18.1078879163654,-56.3156801719843,
2.77685887346849));
#238599=CARTESIAN_POINT('Ctrl Pts',(18.1078535995348,-56.3058893552732,
2.76818441216681));
#238600=CARTESIAN_POINT('Ctrl Pts',(18.1085387949868,-56.2959980926936,
2.75962261521739));
#238601=CARTESIAN_POINT('Ctrl Pts',(18.1100266905431,-56.2860490151148,
2.75123537701784));
#238602=CARTESIAN_POINT('Ctrl Pts',(18.1113970173892,-56.276886081573,2.7435108713425));
#238603=CARTESIAN_POINT('Ctrl Pts',(18.113448339865,-56.2676735798209,2.73593399449985));
#238604=CARTESIAN_POINT('Ctrl Pts',(18.116280599478,-56.2584600414674,2.7285765781272));
#238605=CARTESIAN_POINT('Ctrl Pts',(18.1171251221217,-56.2557127503178,
2.726382745084));
#238606=CARTESIAN_POINT('Ctrl Pts',(18.1180393245077,-56.252965504868,2.72420861709613));
#238607=CARTESIAN_POINT('Ctrl Pts',(18.1190265064346,-56.2502199893828,
2.72205663736669));
#238608=CARTESIAN_POINT('Ctrl Pts',(18.1200036017947,-56.2475025263002,
2.71992664556708));
#238609=CARTESIAN_POINT('Ctrl Pts',(18.1210509212422,-56.2447894850826,
2.71782089927827));
#238610=CARTESIAN_POINT('Ctrl Pts',(18.122170247637,-56.2420855046787,2.71574387311188));
#238611=CARTESIAN_POINT('Ctrl Pts',(18.1222480834054,-56.2418974751695,
2.71559944077429));
#238612=CARTESIAN_POINT('Ctrl Pts',(18.1223262596104,-56.2417094803627,
2.71545515216011));
#238613=CARTESIAN_POINT('Ctrl Pts',(18.1224047773509,-56.241521520961,2.71531100781673));
#238614=CARTESIAN_POINT('Ctrl Pts',(18.1258472827279,-56.233280692238,2.70899119176036));
#238615=CARTESIAN_POINT('Ctrl Pts',(18.1299826829659,-56.2251347899177,
2.70298296066801));
#238616=CARTESIAN_POINT('Ctrl Pts',(18.1348427679842,-56.2171955585586,
2.69736727774107));
#238617=CARTESIAN_POINT('Ctrl Pts',(18.1393732118983,-56.209794815103,2.69213248525417));
#238618=CARTESIAN_POINT('Ctrl Pts',(18.1445340001506,-56.2025731376018,
2.68723866185472));
#238619=CARTESIAN_POINT('Ctrl Pts',(18.1503626543095,-56.1956479299638,
2.68278595829577));
#238620=CARTESIAN_POINT('Ctrl Pts',(18.1524948514079,-56.1931145994164,
2.68115710172794));
#238621=CARTESIAN_POINT('Ctrl Pts',(18.1547164978841,-56.1906212529493,
2.67958763637774));
#238622=CARTESIAN_POINT('Ctrl Pts',(18.1570296338743,-56.1881748397222,
2.67808378645306));
#238623=CARTESIAN_POINT('Ctrl Pts',(18.1575858658048,-56.1875865590686,
2.67772216078541));
#238624=CARTESIAN_POINT('Ctrl Pts',(18.1581479603552,-56.1870008763864,
2.67736403603504));
#238625=CARTESIAN_POINT('Ctrl Pts',(18.1587158783119,-56.1864179215668,
2.6770095693442));
#238626=CARTESIAN_POINT('Ctrl Pts',(18.1592660488324,-56.1858531840854,
2.67666617973745));
#238627=CARTESIAN_POINT('Ctrl Pts',(18.1598216844591,-56.1852910066462,
2.6763262231406));
#238628=CARTESIAN_POINT('Ctrl Pts',(18.160382745929,-56.1847315084901,2.67598984158714));
#238629=CARTESIAN_POINT('Ctrl Pts',(18.1665298227365,-56.178601559592,2.67230439292156));
#238630=CARTESIAN_POINT('Ctrl Pts',(18.1733325302119,-56.1727894828603,
2.66904964539906));
#238631=CARTESIAN_POINT('Ctrl Pts',(18.1807122308858,-56.1674665972284,
2.66640203566653));
#238632=CARTESIAN_POINT('Ctrl Pts',(18.1837728127204,-56.1652590378988,
2.66530399299373));
#238633=CARTESIAN_POINT('Ctrl Pts',(18.1869322368379,-56.1631354730303,
2.66430995142196));
#238634=CARTESIAN_POINT('Ctrl Pts',(18.1901833857459,-56.1611070880435,
2.663430534733));
#238635=CARTESIAN_POINT('Ctrl Pts',(18.1957285590022,-56.1576474660757,
2.66193059792824));
#238636=CARTESIAN_POINT('Ctrl Pts',(18.2015400422208,-56.1544671656474,
2.66076519817067));
#238637=CARTESIAN_POINT('Ctrl Pts',(18.2075773774756,-56.1516266854589,
2.659978056044));
#238638=CARTESIAN_POINT('Ctrl Pts',(18.210596045103,-56.1502064453646,2.65958448498066));
#238639=CARTESIAN_POINT('Ctrl Pts',(18.2136716866514,-56.1488725139546,
2.65928526260701));
#238640=CARTESIAN_POINT('Ctrl Pts',(18.21679921973,-56.1476325143028,2.65908463971264));
#238641=CARTESIAN_POINT('Ctrl Pts',(18.2199267528087,-56.146392514651,2.65888401681826));
#238642=CARTESIAN_POINT('Ctrl Pts',(18.2231061318825,-56.1452464433748,
2.65878198860223));
#238643=CARTESIAN_POINT('Ctrl Pts',(18.2263320786588,-56.1441998575524,
2.65878198860223));
#238644=CARTESIAN_POINT('Origin',(23.7119335237431,-53.2204057122634,2.83404198860225));
#238645=CARTESIAN_POINT('Ctrl Pts',(25.6588335304447,-57.1623216544366,
2.83404198860222));
#238646=CARTESIAN_POINT('Ctrl Pts',(25.6631491402573,-57.1720146727775,
2.82419652440011));
#238647=CARTESIAN_POINT('Ctrl Pts',(25.6666871334691,-57.1820194461955,
2.8143879057558));
#238648=CARTESIAN_POINT('Ctrl Pts',(25.6694381454826,-57.1922776320705,
2.80466781256816));
#238649=CARTESIAN_POINT('Ctrl Pts',(25.6720997659868,-57.202202487988,2.79526356452979));
#238650=CARTESIAN_POINT('Ctrl Pts',(25.6740249857416,-57.2123658169605,
2.78594102496119));
#238651=CARTESIAN_POINT('Ctrl Pts',(25.6751616470875,-57.222729822717,2.77675109088652));
#238652=CARTESIAN_POINT('Ctrl Pts',(25.6762368587291,-57.2325335339839,
2.76805797913539));
#238653=CARTESIAN_POINT('Ctrl Pts',(25.6766065729233,-57.2425177322914,
2.75948271210003));
#238654=CARTESIAN_POINT('Ctrl Pts',(25.6761845643577,-57.2526488462859,
2.75108575573051));
#238655=CARTESIAN_POINT('Ctrl Pts',(25.6757958639483,-57.2619803349756,
2.7433515516308));
#238656=CARTESIAN_POINT('Ctrl Pts',(25.6747354076184,-57.2714370189582,
2.73576818685737));
#238657=CARTESIAN_POINT('Ctrl Pts',(25.6728992535086,-57.2809814365693,
2.72840626160277));
#238658=CARTESIAN_POINT('Ctrl Pts',(25.6723666549991,-57.2837499093065,
2.7262708469352));
#238659=CARTESIAN_POINT('Ctrl Pts',(25.6717685445834,-57.2865256584304,
2.72415424587422));
#238660=CARTESIAN_POINT('Ctrl Pts',(25.6711017521911,-57.2893074725855,
2.72205867173215));
#238661=CARTESIAN_POINT('Ctrl Pts',(25.6703789063668,-57.2923231379851,
2.71978693462819));
#238662=CARTESIAN_POINT('Ctrl Pts',(25.669577399688,-57.2953419866638,2.7175441134072));
#238663=CARTESIAN_POINT('Ctrl Pts',(25.6686939261493,-57.2983617649659,
2.71533341844218));
#238664=CARTESIAN_POINT('Ctrl Pts',(25.66626922609,-57.3066495702118,2.70926614876366));
#238665=CARTESIAN_POINT('Ctrl Pts',(25.6631888860751,-57.3149216961102,
2.70347381860383));
#238666=CARTESIAN_POINT('Ctrl Pts',(25.6594348051813,-57.3230760282576,
2.69804914171369));
#238667=CARTESIAN_POINT('Ctrl Pts',(25.6560000249773,-57.3305367994634,
2.69308585687179));
#238668=CARTESIAN_POINT('Ctrl Pts',(25.6519962425132,-57.3378885241126,
2.68842799053161));
#238669=CARTESIAN_POINT('Ctrl Pts',(25.6473759219982,-57.3450563828665,
2.68414767054193));
#238670=CARTESIAN_POINT('Ctrl Pts',(25.6451064356542,-57.3485772116716,
2.68204519134528));
#238671=CARTESIAN_POINT('Ctrl Pts',(25.6426878935088,-57.3520532672058,
2.68003431778478));
#238672=CARTESIAN_POINT('Ctrl Pts',(25.6401130415753,-57.3554727521276,
2.67812693945227));
#238673=CARTESIAN_POINT('Ctrl Pts',(25.6396244885003,-57.3561215660853,
2.67776503299179));
#238674=CARTESIAN_POINT('Ctrl Pts',(25.6391297826978,-57.3567684269672,
2.677406596399));
#238675=CARTESIAN_POINT('Ctrl Pts',(25.6386289474849,-57.3574131967117,
2.67705178968831));
#238676=CARTESIAN_POINT('Ctrl Pts',(25.6381437633725,-57.3580378174017,
2.67670807068733));
#238677=CARTESIAN_POINT('Ctrl Pts',(25.6376528269754,-57.3586604755986,
2.67636775825241));
#238678=CARTESIAN_POINT('Ctrl Pts',(25.6371561630121,-57.359281044241,2.67603099699231));
#238679=CARTESIAN_POINT('Ctrl Pts',(25.6317436214796,-57.3660438734343,
2.67236104217107));
#238680=CARTESIAN_POINT('Ctrl Pts',(25.6256469885835,-57.372562740949,2.66911440541455));
#238681=CARTESIAN_POINT('Ctrl Pts',(25.6189233999302,-57.3786559602399,
2.66646778189613));
#238682=CARTESIAN_POINT('Ctrl Pts',(25.6160839866903,-57.3812291645836,
2.66535009634953));
#238683=CARTESIAN_POINT('Ctrl Pts',(25.6131331854698,-57.3837265592139,
2.66433897912321));
#238684=CARTESIAN_POINT('Ctrl Pts',(25.6100770039418,-57.3861353831627,
2.66344564884768));
#238685=CARTESIAN_POINT('Ctrl Pts',(25.6049304706145,-57.3901917825026,
2.6619413029856));
#238686=CARTESIAN_POINT('Ctrl Pts',(25.5994853721135,-57.3939944983909,
2.66077206705394));
#238687=CARTESIAN_POINT('Ctrl Pts',(25.5937750303537,-57.3974772155308,
2.65998225155688));
#238688=CARTESIAN_POINT('Ctrl Pts',(25.5923474449137,-57.3983478948158,
2.65978479768261));
#238689=CARTESIAN_POINT('Ctrl Pts',(25.5909031732848,-57.3991983668797,
2.65961098966596));
#238690=CARTESIAN_POINT('Ctrl Pts',(25.589442604035,-57.4000273167763,2.65946139030475));
#238691=CARTESIAN_POINT('Ctrl Pts',(25.5872517501602,-57.4012707416212,
2.65923699126293));
#238692=CARTESIAN_POINT('Ctrl Pts',(25.5850242354392,-57.4024657229505,
2.65906707562415));
#238693=CARTESIAN_POINT('Ctrl Pts',(25.5827620706104,-57.4036093482792,
2.65895332562892));
#238694=CARTESIAN_POINT('Ctrl Pts',(25.5804999057817,-57.4047529736078,
2.6588395756337));
#238695=CARTESIAN_POINT('Ctrl Pts',(25.5782031010737,-57.4058452484191,
2.65878198860222));
#238696=CARTESIAN_POINT('Ctrl Pts',(25.5758735661215,-57.4068835917975,
2.65878198860222));
#238697=CARTESIAN_POINT('Ctrl Pts',(24.0229981225303,-53.919068240199,2.65878198860225));
#238698=CARTESIAN_POINT('Ctrl Pts',(24.0308804555195,-53.9155545931353,
2.65878198860225));
#238699=CARTESIAN_POINT('Ctrl Pts',(24.0389845034728,-53.912722055301,2.65945335517821));
#238700=CARTESIAN_POINT('Ctrl Pts',(24.0471612846391,-53.9105453488008,
2.66072561226574));
#238701=CARTESIAN_POINT('Ctrl Pts',(24.052442646286,-53.9091394197447,2.66154735980311));
#238702=CARTESIAN_POINT('Ctrl Pts',(24.0577541205282,-53.9080061861133,
2.66261895766853));
#238703=CARTESIAN_POINT('Ctrl Pts',(24.0630550795267,-53.9071299964537,
2.66391429250993));
#238704=CARTESIAN_POINT('Ctrl Pts',(24.0700811970218,-53.9059686572511,
2.66563118464089));
#238705=CARTESIAN_POINT('Ctrl Pts',(24.0770886066612,-53.9052646847382,
2.66774105138665));
#238706=CARTESIAN_POINT('Ctrl Pts',(24.0839917000398,-53.90499009288,2.67016894181716));
#238707=CARTESIAN_POINT('Ctrl Pts',(24.0874432467291,-53.9048527969509,
2.67138288703242));
#238708=CARTESIAN_POINT('Ctrl Pts',(24.0908688957005,-53.9048227635318,
2.67267613167517));
#238709=CARTESIAN_POINT('Ctrl Pts',(24.0942592346735,-53.9048959123378,
2.67403835432519));
#238710=CARTESIAN_POINT('Ctrl Pts',(24.09595440416,-53.9049324867408,2.6747194656502));
#238711=CARTESIAN_POINT('Ctrl Pts',(24.0976407611376,-53.9049948499723,
2.67541781389489));
#238712=CARTESIAN_POINT('Ctrl Pts',(24.0993172231363,-53.9050824496417,
2.67613207244135));
#238713=CARTESIAN_POINT('Ctrl Pts',(24.099736338636,-53.9051043495591,2.67631063707797));
#238714=CARTESIAN_POINT('Ctrl Pts',(24.100154836018,-53.9051278266098,2.67649019601811));
#238715=CARTESIAN_POINT('Ctrl Pts',(24.1005726990106,-53.9051528718718,
2.67667072836623));
#238716=CARTESIAN_POINT('Ctrl Pts',(24.1018262879885,-53.9052280076581,
2.67721232541056));
#238717=CARTESIAN_POINT('Ctrl Pts',(24.1030741658761,-53.9053172580723,
2.67776268340013));
#238718=CARTESIAN_POINT('Ctrl Pts',(24.1043159075206,-53.9054203757492,
2.67832123541482));
#238719=CARTESIAN_POINT('Ctrl Pts',(24.1130625753261,-53.9061467233506,
2.68225560368406));
#238720=CARTESIAN_POINT('Ctrl Pts',(24.1215389842447,-53.9075195712144,
2.68661792998844));
#238721=CARTESIAN_POINT('Ctrl Pts',(24.129704126087,-53.9094265129026,2.69130986622527));
#238722=CARTESIAN_POINT('Ctrl Pts',(24.1336642110574,-53.9103513775608,
2.69358545023008));
#238723=CARTESIAN_POINT('Ctrl Pts',(24.1375513523939,-53.9114023832595,
2.69593918853428));
#238724=CARTESIAN_POINT('Ctrl Pts',(24.1413619171796,-53.9125693701067,
2.69836306235439));
#238725=CARTESIAN_POINT('Ctrl Pts',(24.1471956256301,-53.9143559454345,
2.70207384382172));
#238726=CARTESIAN_POINT('Ctrl Pts',(24.152846960627,-53.9164123347816,2.70594760814172));
#238727=CARTESIAN_POINT('Ctrl Pts',(24.1582902100545,-53.9187002605234,
2.70995196345652));
#238728=CARTESIAN_POINT('Ctrl Pts',(24.1608180832483,-53.9197627850741,
2.71181160678049));
#238729=CARTESIAN_POINT('Ctrl Pts',(24.1633010951269,-53.9208749910653,
2.71369962772043));
#238730=CARTESIAN_POINT('Ctrl Pts',(24.16573595767,-53.9220340502322,2.71561183138605));
#238731=CARTESIAN_POINT('Ctrl Pts',(24.1659225802901,-53.9221228875504,
2.71575839426256));
#238732=CARTESIAN_POINT('Ctrl Pts',(24.1661089452653,-53.9222119774183,
2.71590508903153));
#238733=CARTESIAN_POINT('Ctrl Pts',(24.1662950522348,-53.9223013184205,
2.71605191409855));
#238734=CARTESIAN_POINT('Ctrl Pts',(24.1689092940621,-53.9235562901478,
2.71811436362697));
#238735=CARTESIAN_POINT('Ctrl Pts',(24.1714718460797,-53.9248627542245,
2.72020091026904));
#238736=CARTESIAN_POINT('Ctrl Pts',(24.1739808617166,-53.9262153118344,
2.72230624862126));
#238737=CARTESIAN_POINT('Ctrl Pts',(24.182977745577,-53.9310653428792,2.72985561753067));
#238738=CARTESIAN_POINT('Ctrl Pts',(24.1913567365405,-53.9365438157566,
2.73770089914315));
#238739=CARTESIAN_POINT('Ctrl Pts',(24.1991508947546,-53.9425259106381,
2.7457482334708));
#238740=CARTESIAN_POINT('Ctrl Pts',(24.2077158916392,-53.9490996319581,
2.75459144547045));
#238741=CARTESIAN_POINT('Ctrl Pts',(24.2155752681679,-53.9562817849776,
2.76367911754305));
#238742=CARTESIAN_POINT('Ctrl Pts',(24.2227540584939,-53.9639562340148,
2.77292162564776));
#238743=CARTESIAN_POINT('Ctrl Pts',(24.2305053504156,-53.9722427129512,
2.78290121484794));
#238744=CARTESIAN_POINT('Ctrl Pts',(24.2374640812946,-53.9811038680495,
2.79306229500265));
#238745=CARTESIAN_POINT('Ctrl Pts',(24.2436285779143,-53.9904403792176,
2.80331916685344));
#238746=CARTESIAN_POINT('Ctrl Pts',(24.2497413607409,-53.9996985666494,
2.81348999408742));
#238747=CARTESIAN_POINT('Ctrl Pts',(24.2550737197513,-54.0094254978904,
2.82375635966881));
#238748=CARTESIAN_POINT('Ctrl Pts',(24.2595822759739,-54.0195518809636,
2.83404198860224));
#238749=CARTESIAN_POINT('Origin',(-0.0139224327744698,-0.00619866644028074,
2.83404198860263));
#238750=CARTESIAN_POINT('Ctrl Pts',(25.5480287005725,-57.4192809246784,
2.65878198860223));
#238751=CARTESIAN_POINT('Ctrl Pts',(25.5401808584723,-57.42277107712,2.65878198860223));
#238752=CARTESIAN_POINT('Ctrl Pts',(25.5321112063506,-57.4255746438783,
2.65944603041811));
#238753=CARTESIAN_POINT('Ctrl Pts',(25.5239679177307,-57.4277200319911,
2.6607043926403));
#238754=CARTESIAN_POINT('Ctrl Pts',(25.5187647439664,-57.4290908328633,
2.66150842619555));
#238755=CARTESIAN_POINT('Ctrl Pts',(25.513531724247,-57.4301938346421,2.66255428265327));
#238756=CARTESIAN_POINT('Ctrl Pts',(25.5083079410953,-57.4310450321036,
2.66381699700614));
#238757=CARTESIAN_POINT('Ctrl Pts',(25.5011785252538,-57.4322067458444,
2.66554034873214));
#238758=CARTESIAN_POINT('Ctrl Pts',(25.4940667032543,-57.4328933558602,
2.66766759643918));
#238759=CARTESIAN_POINT('Ctrl Pts',(25.4870628291431,-57.4331362848723,
2.67012012783094));
#238760=CARTESIAN_POINT('Ctrl Pts',(25.4835608920874,-57.4332577493783,
2.67134639352682));
#238761=CARTESIAN_POINT('Ctrl Pts',(25.4800857520069,-57.4332683803236,
2.67265375584958));
#238762=CARTESIAN_POINT('Ctrl Pts',(25.4766473428565,-57.4331727200753,
2.67403135126885));
#238763=CARTESIAN_POINT('Ctrl Pts',(25.4749281382813,-57.4331248899512,
2.67472014897849));
#238764=CARTESIAN_POINT('Ctrl Pts',(25.4732181005511,-57.4330504941577,
2.67542649668578));
#238765=CARTESIAN_POINT('Ctrl Pts',(25.4715183716231,-57.432950145409,2.67614899656047));
#238766=CARTESIAN_POINT('Ctrl Pts',(25.4710934393911,-57.4329250582218,
2.67632962152915));
#238767=CARTESIAN_POINT('Ctrl Pts',(25.4706691511212,-57.4328983491277,
2.67651125590896));
#238768=CARTESIAN_POINT('Ctrl Pts',(25.470245523975,-57.4328700280091,2.67669387767469));
#238769=CARTESIAN_POINT('Ctrl Pts',(25.4689746425362,-57.4327850646534,
2.6772417429719));
#238770=CARTESIAN_POINT('Ctrl Pts',(25.4677097128941,-57.4326855923066,
2.67779849504693));
#238771=CARTESIAN_POINT('Ctrl Pts',(25.4664511833533,-57.4325718846632,
2.67836353617954));
#238772=CARTESIAN_POINT('Ctrl Pts',(25.4577539633651,-57.4317860942972,
2.68226832098854));
#238773=CARTESIAN_POINT('Ctrl Pts',(25.4493260998455,-57.4303627559728,
2.68659153751337));
#238774=CARTESIAN_POINT('Ctrl Pts',(25.4412057723285,-57.4284143577086,
2.69123699486124));
#238775=CARTESIAN_POINT('Ctrl Pts',(25.4371699918424,-57.4274460091196,
2.69354577441162));
#238776=CARTESIAN_POINT('Ctrl Pts',(25.4332098968701,-57.4263474236134,
2.69593478828062));
#238777=CARTESIAN_POINT('Ctrl Pts',(25.4293290842285,-57.4251294472433,
2.69839565261164));
#238778=CARTESIAN_POINT('Ctrl Pts',(25.4207674318881,-57.4224424094492,
2.7038246868899));
#238779=CARTESIAN_POINT('Ctrl Pts',(25.4125888532397,-57.4191864212924,
2.70961155815031));
#238780=CARTESIAN_POINT('Ctrl Pts',(25.404896598031,-57.4154637896036,2.71562701361711));
#238781=CARTESIAN_POINT('Ctrl Pts',(25.4020865201988,-57.4141038653028,
2.71782453535801));
#238782=CARTESIAN_POINT('Ctrl Pts',(25.3993352917247,-57.4126868351391,
2.72005051502345));
#238783=CARTESIAN_POINT('Ctrl Pts',(25.3966436944405,-57.4112179557366,
2.72229986760058));
#238784=CARTESIAN_POINT('Ctrl Pts',(25.3876029039784,-57.4062841452553,
2.72985520488844));
#238785=CARTESIAN_POINT('Ctrl Pts',(25.3791816069559,-57.4007266836981,
2.73770845534522));
#238786=CARTESIAN_POINT('Ctrl Pts',(25.3713475726775,-57.3946697603096,
2.74576706701729));
#238787=CARTESIAN_POINT('Ctrl Pts',(25.3627370410033,-57.3880124840158,
2.7546244358502));
#238788=CARTESIAN_POINT('Ctrl Pts',(25.3548353295667,-57.3807515434748,
2.76373036323187));
#238789=CARTESIAN_POINT('Ctrl Pts',(25.3476188815037,-57.3730023605511,
2.7729966463684));
#238790=CARTESIAN_POINT('Ctrl Pts',(25.3398464577397,-57.3646561585162,
2.78297683033518));
#238791=CARTESIAN_POINT('Ctrl Pts',(25.3328680394168,-57.3557428147443,
2.79314401478959));
#238792=CARTESIAN_POINT('Ctrl Pts',(25.3266878999846,-57.3463604602032,
2.80341452428026));
#238793=CARTESIAN_POINT('Ctrl Pts',(25.3205912133021,-57.3371047991284,
2.81354634721407));
#238794=CARTESIAN_POINT('Ctrl Pts',(25.3152708796014,-57.3273913673561,
2.82378004209203));
#238795=CARTESIAN_POINT('Ctrl Pts',(25.3107727110829,-57.3172883154485,
2.83404198860222));
#238796=CARTESIAN_POINT('Ctrl Pts',(23.9115214566121,-54.1745185419755,
2.83404198860224));
#238797=CARTESIAN_POINT('Ctrl Pts',(23.9072166846467,-54.164849865838,2.82422126442961));
#238798=CARTESIAN_POINT('Ctrl Pts',(23.9036899956626,-54.1548764216391,
2.81442815028448));
#238799=CARTESIAN_POINT('Ctrl Pts',(23.9009524404117,-54.1446552025532,
2.80471618166257));
#238800=CARTESIAN_POINT('Ctrl Pts',(23.8983090899564,-54.1347857162234,
2.79533842146166));
#238801=CARTESIAN_POINT('Ctrl Pts',(23.8964012454638,-54.1246839742756,
2.78603515650173));
#238802=CARTESIAN_POINT('Ctrl Pts',(23.89528251795,-54.1143872866729,2.77685887346686));
#238803=CARTESIAN_POINT('Ctrl Pts',(23.8942249700856,-54.1046536921655,
2.76818441216505));
#238804=CARTESIAN_POINT('Ctrl Pts',(23.8938724934882,-54.0947449925294,
2.7596226152155));
#238805=CARTESIAN_POINT('Ctrl Pts',(23.8943122764069,-54.0846948896024,
2.75123537701584));
#238806=CARTESIAN_POINT('Ctrl Pts',(23.8947173090971,-54.0754389134097,
2.74351087134042));
#238807=CARTESIAN_POINT('Ctrl Pts',(23.8957944255629,-54.06606245712,2.7359339944977));
#238808=CARTESIAN_POINT('Ctrl Pts',(23.8976480927562,-54.0566033397486,
2.72857657812499));
#238809=CARTESIAN_POINT('Ctrl Pts',(23.8982008188944,-54.0537828218941,
2.72638274508255));
#238810=CARTESIAN_POINT('Ctrl Pts',(23.8988228478388,-54.0509550659728,
2.72420861709542));
#238811=CARTESIAN_POINT('Ctrl Pts',(23.899517637365,-54.0481214020998,2.72205663736671));
#238812=CARTESIAN_POINT('Ctrl Pts',(23.9002053278545,-54.0453166912879,
2.7199266455671));
#238813=CARTESIAN_POINT('Ctrl Pts',(23.9009633199472,-54.0425090377016,
2.71782089927828));
#238814=CARTESIAN_POINT('Ctrl Pts',(23.9017938716385,-54.0397028685172,
2.7157438731119));
#238815=CARTESIAN_POINT('Ctrl Pts',(23.9018516265789,-54.0395077330001,
2.71559944077431));
#238816=CARTESIAN_POINT('Ctrl Pts',(23.9019097237182,-54.03931259641,2.71545515216013));
#238817=CARTESIAN_POINT('Ctrl Pts',(23.9019681642229,-54.0391174593308,
2.71531100781674));
#238818=CARTESIAN_POINT('Ctrl Pts',(23.9045304100328,-54.0305619349328,
2.70899119176028));
#238819=CARTESIAN_POINT('Ctrl Pts',(23.9077916774642,-54.0220283896857,
2.70298296066784));
#238820=CARTESIAN_POINT('Ctrl Pts',(23.9117952627748,-54.0136246330482,
2.69736727774082));
#238821=CARTESIAN_POINT('Ctrl Pts',(23.9155273001028,-54.005790871299,2.69213248525371));
#238822=CARTESIAN_POINT('Ctrl Pts',(23.919904946166,-53.9980693056372,2.68723866185408));
#238823=CARTESIAN_POINT('Ctrl Pts',(23.9249777890357,-53.9905727747488,
2.682785958295));
#238824=CARTESIAN_POINT('Ctrl Pts',(23.9268335005859,-53.9878304467655,
2.68115710172746));
#238825=CARTESIAN_POINT('Ctrl Pts',(23.9287823509753,-53.9851185338197,
2.67958763637753));
#238826=CARTESIAN_POINT('Ctrl Pts',(23.930827095549,-53.9824437337503,2.67808378645311));
#238827=CARTESIAN_POINT('Ctrl Pts',(23.9313187883101,-53.9818005336907,
2.67772216078546));
#238828=CARTESIAN_POINT('Ctrl Pts',(23.931816583137,-53.98115930456,2.67736403603509));
#238829=CARTESIAN_POINT('Ctrl Pts',(23.9323204546083,-53.9805201796367,
2.67700956934425));
#238830=CARTESIAN_POINT('Ctrl Pts',(23.932808580096,-53.9799010273672,2.6766661797375));
#238831=CARTESIAN_POINT('Ctrl Pts',(23.9333024083488,-53.9792838498566,
2.67632622314065));
#238832=CARTESIAN_POINT('Ctrl Pts',(23.9338019127828,-53.9786687697967,
2.67598984158719));
#238833=CARTESIAN_POINT('Ctrl Pts',(23.939274561122,-53.971929856908,2.6723043929217));
#238834=CARTESIAN_POINT('Ctrl Pts',(23.9454324752048,-53.9654385427824,
2.66904964539926));
#238835=CARTESIAN_POINT('Ctrl Pts',(23.9522153560509,-53.9593734277043,
2.66640203566676));
#238836=CARTESIAN_POINT('Ctrl Pts',(23.9550284189138,-53.9568580436996,
2.66530399299388));
#238837=CARTESIAN_POINT('Ctrl Pts',(23.9579485624032,-53.9544158621937,
2.66430995142205));
#238838=CARTESIAN_POINT('Ctrl Pts',(23.9609698772118,-53.9520587513127,
2.66343053473304));
#238839=CARTESIAN_POINT('Ctrl Pts',(23.9661230444611,-53.948038453077,2.66193059792827));
#238840=CARTESIAN_POINT('Ctrl Pts',(23.9715702598501,-53.9442681092571,
2.6607651981707));
#238841=CARTESIAN_POINT('Ctrl Pts',(23.9772776109218,-53.9408121161402,
2.65997805604402));
#238842=CARTESIAN_POINT('Ctrl Pts',(23.9801312864576,-53.9390841195817,
2.65958448498067));
#238843=CARTESIAN_POINT('Ctrl Pts',(23.9830506455193,-53.9374360035028,
2.65928526260703));
#238844=CARTESIAN_POINT('Ctrl Pts',(23.9860314303864,-53.9358758804722,
2.65908463971265));
#238845=CARTESIAN_POINT('Ctrl Pts',(23.9890122152535,-53.9343157574417,
2.65888401681827));
#238846=CARTESIAN_POINT('Ctrl Pts',(23.9920543802867,-53.9328436288549,
2.65878198860225));
#238847=CARTESIAN_POINT('Ctrl Pts',(23.9951532569813,-53.93146557308,2.65878198860225));
#238848=CARTESIAN_POINT('Origin',(29.1450842944635,-50.450286788887,2.83404198860226));
#238849=CARTESIAN_POINT('Ctrl Pts',(31.4933613949865,-54.1671020372433,
2.83404198860224));
#238850=CARTESIAN_POINT('Ctrl Pts',(31.4986665597481,-54.1762908521529,
2.8241965244016));
#238851=CARTESIAN_POINT('Ctrl Pts',(31.5032309550532,-54.1858709973807,
2.81438790575866));
#238852=CARTESIAN_POINT('Ctrl Pts',(31.5070391691402,-54.1957854287807,
2.80466781257231));
#238853=CARTESIAN_POINT('Ctrl Pts',(31.5107236389459,-54.2053777001969,
2.79526356453497));
#238854=CARTESIAN_POINT('Ctrl Pts',(31.5137006693046,-54.2152841131264,
2.78594102496732));
#238855=CARTESIAN_POINT('Ctrl Pts',(31.5159144374958,-54.2254725303099,
2.77675109089352));
#238856=CARTESIAN_POINT('Ctrl Pts',(31.5180085258887,-54.235110145599,2.76805797914324));
#238857=CARTESIAN_POINT('Ctrl Pts',(31.5194198476562,-54.2450010037657,
2.75948271210865));
#238858=CARTESIAN_POINT('Ctrl Pts',(31.5200591406751,-54.2551207303631,
2.75108575573982));
#238859=CARTESIAN_POINT('Ctrl Pts',(31.5206479757804,-54.2644417304365,
2.7433515516409));
#238860=CARTESIAN_POINT('Ctrl Pts',(31.5205818213861,-54.2739574575838,
2.73576818686817));
#238861=CARTESIAN_POINT('Ctrl Pts',(31.5197533892272,-54.2836415202426,
2.7284062616142));
#238862=CARTESIAN_POINT('Ctrl Pts',(31.5195130925486,-54.286450498705,2.72627084694278));
#238863=CARTESIAN_POINT('Ctrl Pts',(31.5192084034342,-54.2892735615524,
2.72415424587802));
#238864=CARTESIAN_POINT('Ctrl Pts',(31.5188360425585,-54.2921098354275,
2.72205867173224));
#238865=CARTESIAN_POINT('Ctrl Pts',(31.5184323794292,-54.2951845386597,
2.71978693462826));
#238866=CARTESIAN_POINT('Ctrl Pts',(31.517950819101,-54.2982706300309,2.71754411340725));
#238867=CARTESIAN_POINT('Ctrl Pts',(31.5173878381082,-54.3013662138028,
2.71533341844222));
#238868=CARTESIAN_POINT('Ctrl Pts',(31.5158427323556,-54.3098620677554,
2.70926614876369));
#238869=CARTESIAN_POINT('Ctrl Pts',(31.5136439393738,-54.3184108612907,
2.70347381860385));
#238870=CARTESIAN_POINT('Ctrl Pts',(31.5107627835363,-54.3269129314602,
2.69804914171372));
#238871=CARTESIAN_POINT('Ctrl Pts',(31.5081266823665,-54.3346918640773,
2.69308585687172));
#238872=CARTESIAN_POINT('Ctrl Pts',(31.5049132975215,-54.342421824438,2.68842799053145));
#238873=CARTESIAN_POINT('Ctrl Pts',(31.5010675328661,-54.3500333719151,
2.6841476705417));
#238874=CARTESIAN_POINT('Ctrl Pts',(31.4991785058302,-54.3537721391714,
2.68204519134514));
#238875=CARTESIAN_POINT('Ctrl Pts',(31.497136559455,-54.3574819590034,2.68003431778473));
#238876=CARTESIAN_POINT('Ctrl Pts',(31.494933246334,-54.3611518569446,2.67812693945231));
#238877=CARTESIAN_POINT('Ctrl Pts',(31.4945151891298,-54.3618481843337,
2.67776503299183));
#238878=CARTESIAN_POINT('Ctrl Pts',(31.4940908087514,-54.3625432124812,
2.67740659639903));
#238879=CARTESIAN_POINT('Ctrl Pts',(31.4936601139568,-54.3632368016448,
2.67705178968835));
#238880=CARTESIAN_POINT('Ctrl Pts',(31.4932428783745,-54.363908716147,2.67670807068737));
#238881=CARTESIAN_POINT('Ctrl Pts',(31.4928197168828,-54.3645792801843,
2.67636775825245));
#238882=CARTESIAN_POINT('Ctrl Pts',(31.4923906407832,-54.3652483648075,
2.67603099699235));
#238883=CARTESIAN_POINT('Ctrl Pts',(31.4877146578622,-54.3725399111641,
2.67236104217089));
#238884=CARTESIAN_POINT('Ctrl Pts',(31.4823328301622,-54.3796603393086,
2.6691144054142));
#238885=CARTESIAN_POINT('Ctrl Pts',(31.4762829888794,-54.3864229856966,
2.66646778189569));
#238886=CARTESIAN_POINT('Ctrl Pts',(31.4737281033384,-54.3892788932598,
2.66535009634929));
#238887=CARTESIAN_POINT('Ctrl Pts',(31.4710545157389,-54.3920710496176,
2.66433897912312));
#238888=CARTESIAN_POINT('Ctrl Pts',(31.4682668669592,-54.394786135735,2.66344564884771));
#238889=CARTESIAN_POINT('Ctrl Pts',(31.4635725360693,-54.3993582729147,
2.66194130298563));
#238890=CARTESIAN_POINT('Ctrl Pts',(31.4585547584358,-54.4037093249062,
2.66077206705397));
#238891=CARTESIAN_POINT('Ctrl Pts',(31.4532397415961,-54.4077698566059,
2.6599822515569));
#238892=CARTESIAN_POINT('Ctrl Pts',(31.4519109873861,-54.4087849895309,
2.65978479768264));
#238893=CARTESIAN_POINT('Ctrl Pts',(31.4505635261662,-54.4097817701137,
2.65961098966598));
#238894=CARTESIAN_POINT('Ctrl Pts',(31.4491976069264,-54.4107588499952,
2.65946139030477));
#238895=CARTESIAN_POINT('Ctrl Pts',(31.4471487280666,-54.4122244698176,
2.65923699126296));
#238896=CARTESIAN_POINT('Ctrl Pts',(31.4450583254663,-54.4136457436048,
2.65906707562417));
#238897=CARTESIAN_POINT('Ctrl Pts',(31.4429280944114,-54.4150195646475,
2.65895332562895));
#238898=CARTESIAN_POINT('Ctrl Pts',(31.4407978633565,-54.4163933856902,
2.65883957563372));
#238899=CARTESIAN_POINT('Ctrl Pts',(31.4386278145925,-54.4177197583724,
2.65878198860224));
#238900=CARTESIAN_POINT('Ctrl Pts',(31.4364195775141,-54.4189959163058,
2.65878198860224));
#238901=CARTESIAN_POINT('Ctrl Pts',(29.5274749692191,-51.1126068659042,
2.65878198860226));
#238902=CARTESIAN_POINT('Ctrl Pts',(29.5349468458347,-51.1082885388127,
2.65878198860226));
#238903=CARTESIAN_POINT('Ctrl Pts',(29.5427104181378,-51.1046244142385,
2.65945335517811));
#238904=CARTESIAN_POINT('Ctrl Pts',(29.5506148782552,-51.1016049255946,
2.66072561226542));
#238905=CARTESIAN_POINT('Ctrl Pts',(29.5557203484474,-51.0996546457478,
2.66154735980284));
#238906=CARTESIAN_POINT('Ctrl Pts',(29.5608842707086,-51.0979724198483,
2.66261895766837));
#238907=CARTESIAN_POINT('Ctrl Pts',(29.5660646037411,-51.0965469289492,
2.66391429250994));
#238908=CARTESIAN_POINT('Ctrl Pts',(29.5729308384272,-51.0946575224197,
2.6656311846409));
#238909=CARTESIAN_POINT('Ctrl Pts',(29.5798262755784,-51.0932249325808,
2.66774105138665));
#238910=CARTESIAN_POINT('Ctrl Pts',(29.5866628504243,-51.0922302752229,
2.67016894181715));
#238911=CARTESIAN_POINT('Ctrl Pts',(29.5900811378472,-51.091732946544,2.6713828870324));
#238912=CARTESIAN_POINT('Ctrl Pts',(29.5934848814079,-51.0913449998284,
2.67267613167516));
#238913=CARTESIAN_POINT('Ctrl Pts',(29.5968642938815,-51.0910633609948,
2.67403835432518));
#238914=CARTESIAN_POINT('Ctrl Pts',(29.5985540001184,-51.090922541578,2.67471946565019));
#238915=CARTESIAN_POINT('Ctrl Pts',(29.6002376377887,-51.0908082908738,
2.67541781389487));
#238916=CARTESIAN_POINT('Ctrl Pts',(29.6019140726121,-51.0907201726666,
2.67613207244134));
#238917=CARTESIAN_POINT('Ctrl Pts',(29.6023331813179,-51.0906981431148,
2.67631063707795));
#238918=CARTESIAN_POINT('Ctrl Pts',(29.6027518401475,-51.0906777466675,
2.6764901960181));
#238919=CARTESIAN_POINT('Ctrl Pts',(29.6031700319857,-51.0906589761525,
2.67667072836621));
#238920=CARTESIAN_POINT('Ctrl Pts',(29.6044246075002,-51.0906026646076,
2.67721232541055));
#238921=CARTESIAN_POINT('Ctrl Pts',(29.6056749785909,-51.0905609873408,
2.67776268340011));
#238922=CARTESIAN_POINT('Ctrl Pts',(29.606920696577,-51.0905337427825,2.6783212354148));
#238923=CARTESIAN_POINT('Ctrl Pts',(29.6156953732195,-51.0903418356312,
2.68225560368394));
#238924=CARTESIAN_POINT('Ctrl Pts',(29.6242688491604,-51.0908211368925,
2.68661792998821));
#238925=CARTESIAN_POINT('Ctrl Pts',(29.6325885911854,-51.0918641424254,
2.69130986622492));
#238926=CARTESIAN_POINT('Ctrl Pts',(29.6366236570776,-51.0923699989819,
2.69358545022984));
#238927=CARTESIAN_POINT('Ctrl Pts',(29.6405993642579,-51.0930089302511,
2.69593918853416));
#238928=CARTESIAN_POINT('Ctrl Pts',(29.644511037713,-51.0937712117409,2.6983630623544));
#238929=CARTESIAN_POINT('Ctrl Pts',(29.6504995364717,-51.0949382114428,
2.70207384382173));
#238930=CARTESIAN_POINT('Ctrl Pts',(29.6563348640826,-51.0963926103111,
2.70594760814173));
#238931=CARTESIAN_POINT('Ctrl Pts',(29.661987448182,-51.0980990280585,2.70995196345653));
#238932=CARTESIAN_POINT('Ctrl Pts',(29.6646125374804,-51.0988914972883,
2.7118116067805));
#238933=CARTESIAN_POINT('Ctrl Pts',(29.6671982043432,-51.0997380650828,
2.71369962772044));
#238934=CARTESIAN_POINT('Ctrl Pts',(29.6697408831281,-51.1006362623624,
2.71561183138606));
#238935=CARTESIAN_POINT('Ctrl Pts',(29.6699357694383,-51.1007051056447,
2.71575839426257));
#238936=CARTESIAN_POINT('Ctrl Pts',(29.6701304259137,-51.1007742270245,
2.71590508903154));
#238937=CARTESIAN_POINT('Ctrl Pts',(29.6703248520474,-51.1008436251319,
2.71605191409856));
#238938=CARTESIAN_POINT('Ctrl Pts',(29.6730559530505,-51.1018184593119,
2.71811436362698));
#238939=CARTESIAN_POINT('Ctrl Pts',(29.6757410298223,-51.1028499068173,
2.72020091026904));
#238940=CARTESIAN_POINT('Ctrl Pts',(29.6783776815774,-51.1039327914262,
2.72230624862126));
#238941=CARTESIAN_POINT('Ctrl Pts',(29.6878322458588,-51.1078158230494,
2.72985561753074));
#238942=CARTESIAN_POINT('Ctrl Pts',(29.6967379921841,-51.1123884412301,
2.7377008991433));
#238943=CARTESIAN_POINT('Ctrl Pts',(29.7051147523691,-51.1175230541893,
2.74574823347104));
#238944=CARTESIAN_POINT('Ctrl Pts',(29.7143199702922,-51.123165478014,2.75459144547081));
#238945=CARTESIAN_POINT('Ctrl Pts',(29.7228870317522,-51.1294867578971,
2.76367911754355));
#238946=CARTESIAN_POINT('Ctrl Pts',(29.730828694278,-51.1363687775787,2.7729216256484));
#238947=CARTESIAN_POINT('Ctrl Pts',(29.7394036967208,-51.1437996316838,
2.78290121484885));
#238948=CARTESIAN_POINT('Ctrl Pts',(29.7472505498693,-51.1518848590025,
2.79306229500385));
#238949=CARTESIAN_POINT('Ctrl Pts',(29.7543572078963,-51.1605258584273,
2.80331916685492));
#238950=CARTESIAN_POINT('Ctrl Pts',(29.7614042483635,-51.1690943687441,
2.81348999408842));
#238951=CARTESIAN_POINT('Ctrl Pts',(29.7677241373279,-51.1782106315447,
2.82375635966932));
#238952=CARTESIAN_POINT('Ctrl Pts',(29.7732664904686,-51.1878102687779,
2.83404198860226));
#238953=CARTESIAN_POINT('Origin',(-0.0131982271536719,-0.00761999999980581,
2.83404198860262));
#238954=CARTESIAN_POINT('Ctrl Pts',(31.4100231232068,-54.4342359163058,
2.65878198860224));
#238955=CARTESIAN_POINT('Ctrl Pts',(31.4025830926779,-54.4385272722019,
2.65878198860224));
#238956=CARTESIAN_POINT('Ctrl Pts',(31.3948506994796,-54.4421589890636,
2.65944603041815));
#238957=CARTESIAN_POINT('Ctrl Pts',(31.3869762747692,-54.4451438299613,
2.66070439264038));
#238958=CARTESIAN_POINT('Ctrl Pts',(31.381944892244,-54.4470510012005,2.66150842619562));
#238959=CARTESIAN_POINT('Ctrl Pts',(31.3768558346353,-54.4486949601296,
2.66255428265332));
#238960=CARTESIAN_POINT('Ctrl Pts',(31.371749642277,-54.4500875286676,2.66381699700615));
#238961=CARTESIAN_POINT('Ctrl Pts',(31.3647807142735,-54.4519881053008,
2.66554034873215));
#238962=CARTESIAN_POINT('Ctrl Pts',(31.3577796218689,-54.4534143418198,
2.66766759643919));
#238963=CARTESIAN_POINT('Ctrl Pts',(31.3508395087091,-54.4543880442391,
2.67012012783095));
#238964=CARTESIAN_POINT('Ctrl Pts',(31.3473694521293,-54.4548748954487,
2.67134639352683));
#238965=CARTESIAN_POINT('Ctrl Pts',(31.343914460466,-54.4552487192089,2.67265375584959));
#238966=CARTESIAN_POINT('Ctrl Pts',(31.340484888062,-54.455512994622,2.67403135126887));
#238967=CARTESIAN_POINT('Ctrl Pts',(31.33877010186,-54.4556451323286,2.67472014897851));
#238968=CARTESIAN_POINT('Ctrl Pts',(31.3370616554174,-54.4557498916991,
2.6754264966858));
#238969=CARTESIAN_POINT('Ctrl Pts',(31.3353607484818,-54.4558277627241,
2.67614899656049));
#238970=CARTESIAN_POINT('Ctrl Pts',(31.3349355217479,-54.4558472304803,
2.67632962152916));
#238971=CARTESIAN_POINT('Ctrl Pts',(31.334510765913,-54.4558650179023,2.67651125590897));
#238972=CARTESIAN_POINT('Ctrl Pts',(31.3340864990776,-54.4558811330244,
2.67669387767471));
#238973=CARTESIAN_POINT('Ctrl Pts',(31.3328136985713,-54.4559294783906,
2.67724174297191));
#238974=CARTESIAN_POINT('Ctrl Pts',(31.3315453006546,-54.4559627721153,
2.67779849504695));
#238975=CARTESIAN_POINT('Ctrl Pts',(31.3302817797851,-54.4559812395332,
2.67836353617956));
#238976=CARTESIAN_POINT('Ctrl Pts',(31.3215500666185,-54.4561088608491,
2.68226832098858));
#238977=CARTESIAN_POINT('Ctrl Pts',(31.3130195924492,-54.4555742713433,
2.68659153751344));
#238978=CARTESIAN_POINT('Ctrl Pts',(31.3047400858596,-54.4544853519652,
2.69123699486134));
#238979=CARTESIAN_POINT('Ctrl Pts',(31.3006251938115,-54.4539441620234,
2.69354577441169));
#238980=CARTESIAN_POINT('Ctrl Pts',(31.2965719591991,-54.4532655373254,
2.69593478828066));
#238981=CARTESIAN_POINT('Ctrl Pts',(31.292585092857,-54.4524598885389,2.69839565261165));
#238982=CARTESIAN_POINT('Ctrl Pts',(31.2837894702125,-54.4506825069813,
2.7038246868899));
#238983=CARTESIAN_POINT('Ctrl Pts',(31.2753153512353,-54.4482992497261,
2.70961155815032));
#238984=CARTESIAN_POINT('Ctrl Pts',(31.2672761140357,-54.4454010706192,
2.71562701361713));
#238985=CARTESIAN_POINT('Ctrl Pts',(31.2643392793065,-54.4443423292436,
2.71782453535804));
#238986=CARTESIAN_POINT('Ctrl Pts',(31.2614550023645,-54.4432206434038,
2.72005051502348));
#238987=CARTESIAN_POINT('Ctrl Pts',(31.2586246102252,-54.4420411592042,
2.72229986760062));
#238988=CARTESIAN_POINT('Ctrl Pts',(31.2491176225324,-54.4380793965871,
2.72985520488787));
#238989=CARTESIAN_POINT('Ctrl Pts',(31.2401615453406,-54.4334326446229,
2.73770845534399));
#238990=CARTESIAN_POINT('Ctrl Pts',(31.2317373058284,-54.4282277812593,
2.74576706701537));
#238991=CARTESIAN_POINT('Ctrl Pts',(31.2224780686878,-54.422507019866,2.75462443584758));
#238992=CARTESIAN_POINT('Ctrl Pts',(31.2138606686971,-54.4161118092713,
2.76373036322853));
#238993=CARTESIAN_POINT('Ctrl Pts',(31.2058737429096,-54.4091594014095,
2.77299664636431));
#238994=CARTESIAN_POINT('Ctrl Pts',(31.1972714816238,-54.4016713602553,
2.78297683033026));
#238995=CARTESIAN_POINT('Ctrl Pts',(31.1893995936799,-54.3935362880573,
2.79314401478381));
#238996=CARTESIAN_POINT('Ctrl Pts',(31.1822725865963,-54.3848513315147,
2.8034145242736));
#238997=CARTESIAN_POINT('Ctrl Pts',(31.1752418181707,-54.3762836512078,
2.81354634720961));
#238998=CARTESIAN_POINT('Ctrl Pts',(31.1689352997168,-54.367179556935,2.82378004208982));
#238999=CARTESIAN_POINT('Ctrl Pts',(31.1634057161447,-54.3576020372433,
2.83404198860224));
#239000=CARTESIAN_POINT('Ctrl Pts',(29.4433108116267,-51.3783102687779,
2.83404198860226));
#239001=CARTESIAN_POINT('Ctrl Pts',(29.4380189697936,-51.3691445298574,
2.82422126442883));
#239002=CARTESIAN_POINT('Ctrl Pts',(29.4334690915849,-51.3595943606086,
2.8144281502829));
#239003=CARTESIAN_POINT('Ctrl Pts',(29.4296781246242,-51.3497152868729,
2.8047161816602));
#239004=CARTESIAN_POINT('Ctrl Pts',(29.4260176124798,-51.3401761719824,
2.79533842145879));
#239005=CARTESIAN_POINT('Ctrl Pts',(29.4230642997968,-51.3303291924862,
2.78603515649837));
#239006=CARTESIAN_POINT('Ctrl Pts',(29.4208754038576,-51.3202058500828,
2.77685887346304));
#239007=CARTESIAN_POINT('Ctrl Pts',(29.4188062116754,-51.3106361210773,
2.76818441216095));
#239008=CARTESIAN_POINT('Ctrl Pts',(29.4174199248358,-51.3008185461712,
2.75962261521114));
#239009=CARTESIAN_POINT('Ctrl Pts',(29.4168067767633,-51.2907775289265,
2.75123537701125));
#239010=CARTESIAN_POINT('Ctrl Pts',(29.4162420776748,-51.2815299204948,
2.74351087133569));
#239011=CARTESIAN_POINT('Ctrl Pts',(29.4163331870173,-51.2720922400845,
2.73593399449284));
#239012=CARTESIAN_POINT('Ctrl Pts',(29.4171879526255,-51.2624911797642,
2.72857657812005));
#239013=CARTESIAN_POINT('Ctrl Pts',(29.417442826475,-51.25962833739,2.72638274507929));
#239014=CARTESIAN_POINT('Ctrl Pts',(29.4177658668987,-51.2567510524839,
2.72420861709381));
#239015=CARTESIAN_POINT('Ctrl Pts',(29.4181606517648,-51.2538602864389,
2.72205663736673));
#239016=CARTESIAN_POINT('Ctrl Pts',(29.4185514029028,-51.2509990568961,
2.71992664556712));
#239017=CARTESIAN_POINT('Ctrl Pts',(29.4190117629207,-51.2481275521813,
2.71782089927831));
#239018=CARTESIAN_POINT('Ctrl Pts',(29.4195444402105,-51.2452499391934,
2.71574387311192));
#239019=CARTESIAN_POINT('Ctrl Pts',(29.4195814815475,-51.245049835614,2.71559944077433));
#239020=CARTESIAN_POINT('Ctrl Pts',(29.4196188630967,-51.2448496951978,
2.71545515216015));
#239021=CARTESIAN_POINT('Ctrl Pts',(29.4196565860791,-51.2446495184037,
2.71531100781677));
#239022=CARTESIAN_POINT('Ctrl Pts',(29.4213104998207,-51.2358730344466,
2.70899119176035));
#239023=CARTESIAN_POINT('Ctrl Pts',(29.4236619033169,-51.2270453415805,
2.70298296066795));
#239024=CARTESIAN_POINT('Ctrl Pts',(29.4267651248013,-51.2182691329812,
2.69736727774097));
#239025=CARTESIAN_POINT('Ctrl Pts',(29.4296578665609,-51.210088181272,2.692132485254));
#239026=CARTESIAN_POINT('Ctrl Pts',(29.4332044080281,-51.2019513265393,
2.6872386618545));
#239027=CARTESIAN_POINT('Ctrl Pts',(29.43746586048,-51.1939656059622,2.68278595829551));
#239028=CARTESIAN_POINT('Ctrl Pts',(29.4390247549185,-51.1910443260616,
2.68115710172778));
#239029=CARTESIAN_POINT('Ctrl Pts',(29.440679457209,-51.1881435589219,2.67958763637767));
#239030=CARTESIAN_POINT('Ctrl Pts',(29.4424334077173,-51.1852696776788,
2.67808378645308));
#239031=CARTESIAN_POINT('Ctrl Pts',(29.4428551742202,-51.1845786052478,
2.67772216078543));
#239032=CARTESIAN_POINT('Ctrl Pts',(29.4432832153794,-51.183888855109,2.67736403603506));
#239033=CARTESIAN_POINT('Ctrl Pts',(29.4437175198439,-51.1832005624683,
2.67700956934422));
#239034=CARTESIAN_POINT('Ctrl Pts',(29.4441382522939,-51.1825337789726,
2.67666617973747));
#239035=CARTESIAN_POINT('Ctrl Pts',(29.4445648626871,-51.1818683633167,
2.67632622314062));
#239036=CARTESIAN_POINT('Ctrl Pts',(29.4449973374101,-51.1812044402988,
2.67598984158716));
#239037=CARTESIAN_POINT('Ctrl Pts',(29.4497355978008,-51.173930396359,2.67230439292164));
#239038=CARTESIAN_POINT('Ctrl Pts',(29.4551812510958,-51.1668309650354,
2.66904964539918));
#239039=CARTESIAN_POINT('Ctrl Pts',(29.4612929974523,-51.1600900711809,
2.66640203566668));
#239040=CARTESIAN_POINT('Ctrl Pts',(29.463827720838,-51.1572944215749,2.66530399299383));
#239041=CARTESIAN_POINT('Ctrl Pts',(29.4664765899959,-51.1545603804833,
2.66430995142202));
#239042=CARTESIAN_POINT('Ctrl Pts',(29.4692349685477,-51.1519003687084,
2.66343053473303));
#239043=CARTESIAN_POINT('Ctrl Pts',(29.4739396706111,-51.1473634414336,
2.66193059792826));
#239044=CARTESIAN_POINT('Ctrl Pts',(29.4789629373388,-51.1430443628979,
2.6607651981707));
#239045=CARTESIAN_POINT('Ctrl Pts',(29.4842777732944,-51.1390107214358,
2.65997805604402));
#239046=CARTESIAN_POINT('Ctrl Pts',(29.4869351912722,-51.1369939007047,
2.65958448498068));
#239047=CARTESIAN_POINT('Ctrl Pts',(29.4896662827385,-51.1350496570618,
2.65928526260704));
#239048=CARTESIAN_POINT('Ctrl Pts',(29.4924676612914,-51.133186503687,2.65908463971266));
#239049=CARTESIAN_POINT('Ctrl Pts',(29.4952690398443,-51.1313233503122,
2.65888401681829));
#239050=CARTESIAN_POINT('Ctrl Pts',(29.4981406602403,-51.1295412933641,
2.65878198860226));
#239051=CARTESIAN_POINT('Ctrl Pts',(29.5010785149117,-51.1278468659042,
2.65878198860226));
#239052=CARTESIAN_POINT('Origin',(34.2589154226527,-47.1274239660504,2.83404198860229));
#239053=CARTESIAN_POINT('Ctrl Pts',(36.9828414016752,-50.5784163149351,
2.83404198860226));
#239054=CARTESIAN_POINT('Ctrl Pts',(36.9890779968915,-50.587000251836,2.82419652440071));
#239055=CARTESIAN_POINT('Ctrl Pts',(36.9946187858205,-50.5960508067997,
2.81438790575687));
#239056=CARTESIAN_POINT('Ctrl Pts',(36.999442478391,-50.6055128591417,2.80466781256964));
#239057=CARTESIAN_POINT('Ctrl Pts',(37.0041094296761,-50.6146674511255,
2.79526356453155));
#239058=CARTESIAN_POINT('Ctrl Pts',(37.0081056536712,-50.6242084112807,
2.78594102496317));
#239059=CARTESIAN_POINT('Ctrl Pts',(37.0113722741999,-50.6341096134627,
2.77675109088868));
#239060=CARTESIAN_POINT('Ctrl Pts',(37.0144622960732,-50.6434755410461,
2.7680579791377));
#239061=CARTESIAN_POINT('Ctrl Pts',(37.0168997626768,-50.6531646927622,
2.75948271210245));
#239062=CARTESIAN_POINT('Ctrl Pts',(37.0185933530513,-50.6631621581227,
2.75108575573304));
#239063=CARTESIAN_POINT('Ctrl Pts',(37.0201532722699,-50.6723705467548,
2.74335155163341));
#239064=CARTESIAN_POINT('Ctrl Pts',(37.0210821446115,-50.6818410607715,
2.73576818686005));
#239065=CARTESIAN_POINT('Ctrl Pts',(37.021270510878,-50.6915586678635,2.72840626160554));
#239066=CARTESIAN_POINT('Ctrl Pts',(37.0213251487715,-50.6943773762868,
2.72627084693704));
#239067=CARTESIAN_POINT('Ctrl Pts',(37.0213172191971,-50.6972168227817,
2.72415424587516));
#239068=CARTESIAN_POINT('Ctrl Pts',(37.021243369503,-50.700076481558,2.72205867173221));
#239069=CARTESIAN_POINT('Ctrl Pts',(37.0211633116864,-50.7031765355308,
2.71978693462824));
#239070=CARTESIAN_POINT('Ctrl Pts',(37.0210069737846,-50.7062960577316,
2.71754411340725));
#239071=CARTESIAN_POINT('Ctrl Pts',(37.0207706534752,-50.7094335311098,
2.71533341844222));
#239072=CARTESIAN_POINT('Ctrl Pts',(37.0201220705315,-50.7180443514155,
2.7092661487637));
#239073=CARTESIAN_POINT('Ctrl Pts',(37.0188289150186,-50.7267761502167,
2.70347381860387));
#239074=CARTESIAN_POINT('Ctrl Pts',(37.0168522507837,-50.7355328079483,
2.69804914171373));
#239075=CARTESIAN_POINT('Ctrl Pts',(37.0150437103243,-50.7435446743629,
2.69308585687179));
#239076=CARTESIAN_POINT('Ctrl Pts',(37.0126559296154,-50.7515681793716,
2.68842799053157));
#239077=CARTESIAN_POINT('Ctrl Pts',(37.009626855822,-50.7595400218646,2.68414767054186));
#239078=CARTESIAN_POINT('Ctrl Pts',(37.0081389846697,-50.7634557648559,
2.68204519134525));
#239079=CARTESIAN_POINT('Ctrl Pts',(37.0064960060564,-50.7673587034234,
2.68003431778479));
#239080=CARTESIAN_POINT('Ctrl Pts',(37.0046883717073,-50.7712388062144,
2.67812693945232));
#239081=CARTESIAN_POINT('Ctrl Pts',(37.0043453906961,-50.7719750179263,
2.67776503299184));
#239082=CARTESIAN_POINT('Ctrl Pts',(37.003995985342,-50.7727105984658,2.67740659639905));
#239083=CARTESIAN_POINT('Ctrl Pts',(37.003640149748,-50.7734454079403,2.67705178968836));
#239084=CARTESIAN_POINT('Ctrl Pts',(37.0032954340162,-50.7741572546188,
2.67670807068738));
#239085=CARTESIAN_POINT('Ctrl Pts',(37.0029446836758,-50.7748683776566,
2.67636775825246));
#239086=CARTESIAN_POINT('Ctrl Pts',(37.0025878964874,-50.7755786476296,
2.67603099699236));
#239087=CARTESIAN_POINT('Ctrl Pts',(36.9986997032259,-50.7833190234408,
2.67236104217115));
#239088=CARTESIAN_POINT('Ctrl Pts',(36.9940916451532,-50.7909629993134,
2.66911440541465));
#239089=CARTESIAN_POINT('Ctrl Pts',(36.988781834569,-50.7983209798289,2.66646778189624));
#239090=CARTESIAN_POINT('Ctrl Pts',(36.9865394685868,-50.8014283006915,
2.66535009634962));
#239091=CARTESIAN_POINT('Ctrl Pts',(36.9841723869929,-50.8044846273283,
2.66433897912328));
#239092=CARTESIAN_POINT('Ctrl Pts',(36.9816838130239,-50.8074762285634,
2.66344564884773));
#239093=CARTESIAN_POINT('Ctrl Pts',(36.9774931166431,-50.8125140102912,
2.66194130298565));
#239094=CARTESIAN_POINT('Ctrl Pts',(36.9729576356987,-50.8173657273497,
2.66077206705399));
#239095=CARTESIAN_POINT('Ctrl Pts',(36.9680961762161,-50.8219595855745,
2.65998225155693));
#239096=CARTESIAN_POINT('Ctrl Pts',(36.9668808113454,-50.8231080501307,
2.65978479768266));
#239097=CARTESIAN_POINT('Ctrl Pts',(36.9656449236016,-50.8242402182959,
2.65961098966601));
#239098=CARTESIAN_POINT('Ctrl Pts',(36.9643886196688,-50.8253547230707,
2.6594613903048));
#239099=CARTESIAN_POINT('Ctrl Pts',(36.9625041637695,-50.8270264802329,
2.65923699126298));
#239100=CARTESIAN_POINT('Ctrl Pts',(36.9605737761783,-50.828658474705,2.6590670756242));
#239101=CARTESIAN_POINT('Ctrl Pts',(36.9585988181543,-50.8302474395909,
2.65895332562898));
#239102=CARTESIAN_POINT('Ctrl Pts',(36.9566238601303,-50.8318364044767,
2.65883957563375));
#239103=CARTESIAN_POINT('Ctrl Pts',(36.9546043428198,-50.8333823430144,
2.65878198860227));
#239104=CARTESIAN_POINT('Ctrl Pts',(36.9525415975228,-50.8348823336494,
2.65878198860227));
#239105=CARTESIAN_POINT('Ctrl Pts',(34.7084426211237,-47.7461450747859,
2.65878198860229));
#239106=CARTESIAN_POINT('Ctrl Pts',(34.7154221779231,-47.7410693801614,
2.65878198860229));
#239107=CARTESIAN_POINT('Ctrl Pts',(34.7227602152543,-47.7366138137625,
2.65945335517822));
#239108=CARTESIAN_POINT('Ctrl Pts',(34.7303057514047,-47.7327846251242,
2.66072561226567));
#239109=CARTESIAN_POINT('Ctrl Pts',(34.7351793935412,-47.7303113621612,
2.66154735980305));
#239110=CARTESIAN_POINT('Ctrl Pts',(34.7401391868074,-47.7280985748131,
2.6626189576685));
#239111=CARTESIAN_POINT('Ctrl Pts',(34.7451421370599,-47.7261394006513,
2.66391429250994));
#239112=CARTESIAN_POINT('Ctrl Pts',(34.7517732610329,-47.7235426275283,
2.6656311846409));
#239113=CARTESIAN_POINT('Ctrl Pts',(34.7584811778437,-47.7213971161174,
2.66774105138666));
#239114=CARTESIAN_POINT('Ctrl Pts',(34.7651763312121,-47.719693290934,2.67016894181717));
#239115=CARTESIAN_POINT('Ctrl Pts',(34.7685239078963,-47.7188413783422,
2.67138288703242));
#239116=CARTESIAN_POINT('Ctrl Pts',(34.7718684539197,-47.7180997687556,
2.67267613167518));
#239117=CARTESIAN_POINT('Ctrl Pts',(34.7751999143437,-47.7174664279764,
2.6740383543252));
#239118=CARTESIAN_POINT('Ctrl Pts',(34.7768656445558,-47.7171497575867,
2.67471946565021));
#239119=CARTESIAN_POINT('Ctrl Pts',(34.7785281166323,-47.7168601447015,
2.6754178138949));
#239120=CARTESIAN_POINT('Ctrl Pts',(34.7801861569095,-47.7165972740592,
2.67613207244136));
#239121=CARTESIAN_POINT('Ctrl Pts',(34.7806006669788,-47.7165315563986,
2.67631063707798));
#239122=CARTESIAN_POINT('Ctrl Pts',(34.7810149003422,-47.7164675099211,
2.67649019601813));
#239123=CARTESIAN_POINT('Ctrl Pts',(34.7814288392286,-47.7164051292828,
2.67667072836624));
#239124=CARTESIAN_POINT('Ctrl Pts',(34.7826706558879,-47.7162179873678,
2.67721232541058));
#239125=CARTESIAN_POINT('Ctrl Pts',(34.7839098208543,-47.7160458390449,
2.67776268340014));
#239126=CARTESIAN_POINT('Ctrl Pts',(34.7851458668352,-47.7158885307483,
2.67832123541483));
#239127=CARTESIAN_POINT('Ctrl Pts',(34.7938524151216,-47.7147804714194,
2.68225560368412));
#239128=CARTESIAN_POINT('Ctrl Pts',(34.8024290252888,-47.7143609747532,
2.68661792998856));
#239129=CARTESIAN_POINT('Ctrl Pts',(34.8108122146623,-47.7145286167441,
2.69130986622546));
#239130=CARTESIAN_POINT('Ctrl Pts',(34.8148780524495,-47.7146099229285,
2.69358545023023));
#239131=CARTESIAN_POINT('Ctrl Pts',(34.8188987667933,-47.7148297795034,
2.69593918853438));
#239132=CARTESIAN_POINT('Ctrl Pts',(34.8228686918044,-47.7151790039204,
2.69836306235443));
#239133=CARTESIAN_POINT('Ctrl Pts',(34.8289463696258,-47.7157136421032,
2.70207384382176));
#239134=CARTESIAN_POINT('Ctrl Pts',(34.8349017567801,-47.7165501157946,
2.70594760814176));
#239135=CARTESIAN_POINT('Ctrl Pts',(34.8407017446573,-47.7176563296776,
2.70995196345656));
#239136=CARTESIAN_POINT('Ctrl Pts',(34.8433952890326,-47.7181700611277,
2.71181160678054));
#239137=CARTESIAN_POINT('Ctrl Pts',(34.8460552817724,-47.7187417155516,
2.71369962772047));
#239138=CARTESIAN_POINT('Ctrl Pts',(34.8486779186782,-47.7193692101065,
2.7156118313861));
#239139=CARTESIAN_POINT('Ctrl Pts',(34.8488789334633,-47.7194173050917,
2.7157583942626));
#239140=CARTESIAN_POINT('Ctrl Pts',(34.8490797487417,-47.719465700675,2.71590508903158));
#239141=CARTESIAN_POINT('Ctrl Pts',(34.8492803638663,-47.7195143955473,
2.7160519140986));
#239142=CARTESIAN_POINT('Ctrl Pts',(34.8520984015311,-47.7201984116928,
2.71811436362702));
#239143=CARTESIAN_POINT('Ctrl Pts',(34.8548765847941,-47.7209435418721,
2.72020091026908));
#239144=CARTESIAN_POINT('Ctrl Pts',(34.8576119849591,-47.7217448891697,
2.72230624862131));
#239145=CARTESIAN_POINT('Ctrl Pts',(34.8674206434762,-47.7246183780641,
2.7298556175306));
#239146=CARTESIAN_POINT('Ctrl Pts',(34.8767555719426,-47.7282350429863,
2.73770089914297));
#239147=CARTESIAN_POINT('Ctrl Pts',(34.8856231565607,-47.7324659181291,
2.7457482334705));
#239148=CARTESIAN_POINT('Ctrl Pts',(34.895367741228,-47.7371152248818,2.75459144546986));
#239149=CARTESIAN_POINT('Ctrl Pts',(34.9045486251005,-47.7425063743629,
2.76367911754215));
#239150=CARTESIAN_POINT('Ctrl Pts',(34.9131661493093,-47.7485205638406,
2.77292162564655));
#239151=CARTESIAN_POINT('Ctrl Pts',(34.9224709127511,-47.7550143791208,
2.78290121484603));
#239152=CARTESIAN_POINT('Ctrl Pts',(34.9311199164031,-47.7622350952164,
2.79306229500001));
#239153=CARTESIAN_POINT('Ctrl Pts',(34.9390908738043,-47.7700859102987,
2.80331916685007));
#239154=CARTESIAN_POINT('Ctrl Pts',(34.9469949630638,-47.7778708651099,
2.81348999408516));
#239155=CARTESIAN_POINT('Ctrl Pts',(34.9542331399578,-47.7862765797888,
2.8237563596677));
#239156=CARTESIAN_POINT('Ctrl Pts',(34.9607485668371,-47.7952442955496,
2.83404198860229));
#239157=CARTESIAN_POINT('Origin',(-0.0123294189942718,-0.00895784724474341,
2.83404198860262));
#239158=CARTESIAN_POINT('Ctrl Pts',(36.9278827595333,-50.8527980281379,
2.65878198860226));
#239159=CARTESIAN_POINT('Ctrl Pts',(36.9209320551072,-50.8578435704953,
2.65878198860226));
#239160=CARTESIAN_POINT('Ctrl Pts',(36.9136216385505,-50.8622636476104,
2.65944603041817));
#239161=CARTESIAN_POINT('Ctrl Pts',(36.9061023515947,-50.8660552387514,
2.6607043926404));
#239162=CARTESIAN_POINT('Ctrl Pts',(36.9012978851882,-50.8684778849905,
2.66150842619563));
#239163=CARTESIAN_POINT('Ctrl Pts',(36.8964085464701,-50.8706447895119,
2.66255428265333));
#239164=CARTESIAN_POINT('Ctrl Pts',(36.8914758894172,-50.8725634718541,
2.66381699700615));
#239165=CARTESIAN_POINT('Ctrl Pts',(36.8847438022852,-50.8751820882645,
2.66554034873215));
#239166=CARTESIAN_POINT('Ctrl Pts',(36.8779301449089,-50.8773323251408,
2.66766759643919));
#239167=CARTESIAN_POINT('Ctrl Pts',(36.8711298300327,-50.8790261328799,
2.67012012783095));
#239168=CARTESIAN_POINT('Ctrl Pts',(36.8677296725947,-50.8798730367495,
2.67134639352683));
#239169=CARTESIAN_POINT('Ctrl Pts',(36.8643326829605,-50.8806059576331,
2.6726537558496));
#239170=CARTESIAN_POINT('Ctrl Pts',(36.8609495224157,-50.8812272732509,
2.67403135126888));
#239171=CARTESIAN_POINT('Ctrl Pts',(36.8592579421434,-50.8815379310598,
2.67472014897852));
#239172=CARTESIAN_POINT('Ctrl Pts',(36.8575698050851,-50.8818206978287,
2.6754264966858));
#239173=CARTESIAN_POINT('Ctrl Pts',(36.8558863556343,-50.8820759354563,
2.6761489965605));
#239174=CARTESIAN_POINT('Ctrl Pts',(36.8554654932716,-50.8821397448631,
2.67632962152917));
#239175=CARTESIAN_POINT('Ctrl Pts',(36.8550449235855,-50.8822018339184,
2.67651125590898));
#239176=CARTESIAN_POINT('Ctrl Pts',(36.8546246654171,-50.8822622087205,
2.67669387767471));
#239177=CARTESIAN_POINT('Ctrl Pts',(36.853363890912,-50.8824433331267,2.67724174297192));
#239178=CARTESIAN_POINT('Ctrl Pts',(36.8521059215537,-50.88260902815,2.67779849504695));
#239179=CARTESIAN_POINT('Ctrl Pts',(36.8508512527545,-50.8827594682963,
2.67836353617957));
#239180=CARTESIAN_POINT('Ctrl Pts',(36.8421807128861,-50.8837991030482,
2.68226832098865));
#239181=CARTESIAN_POINT('Ctrl Pts',(36.8336410897273,-50.8841591194355,
2.68659153751359));
#239182=CARTESIAN_POINT('Ctrl Pts',(36.8252931160718,-50.8839416093721,
2.69123699486159));
#239183=CARTESIAN_POINT('Ctrl Pts',(36.8211441960799,-50.8838335074677,
2.69354577441187));
#239184=CARTESIAN_POINT('Ctrl Pts',(36.8170422299142,-50.8835822787321,
2.69593478828077));
#239185=CARTESIAN_POINT('Ctrl Pts',(36.8129929908136,-50.883197784386,2.69839565261167));
#239186=CARTESIAN_POINT('Ctrl Pts',(36.8040597645474,-50.882349532429,2.70382468688993));
#239187=CARTESIAN_POINT('Ctrl Pts',(36.7953829494622,-50.8808651175407,
2.70961155815034));
#239188=CARTESIAN_POINT('Ctrl Pts',(36.7870848098368,-50.8788231440725,
2.71562701361715));
#239189=CARTESIAN_POINT('Ctrl Pts',(36.7840533947866,-50.878077185414,2.71782453535805));
#239190=CARTESIAN_POINT('Ctrl Pts',(36.7810676701183,-50.877263133323,2.72005051502349));
#239191=CARTESIAN_POINT('Ctrl Pts',(36.7781294934924,-50.876385967002,2.72229986760062));
#239192=CARTESIAN_POINT('Ctrl Pts',(36.7682604691141,-50.8734396581486,
2.72985520488837));
#239193=CARTESIAN_POINT('Ctrl Pts',(36.7588677364076,-50.8697545265633,
2.73770845534504));
#239194=CARTESIAN_POINT('Ctrl Pts',(36.7499455893915,-50.8654587487958,
2.745767067017));
#239195=CARTESIAN_POINT('Ctrl Pts',(36.740139092923,-50.860737180161,2.75462443584979));
#239196=CARTESIAN_POINT('Ctrl Pts',(36.730900418415,-50.8552777667771,2.76373036323134));
#239197=CARTESIAN_POINT('Ctrl Pts',(36.7222305213324,-50.8491983060113,
2.77299664636773));
#239198=CARTESIAN_POINT('Ctrl Pts',(36.712892670699,-50.8426504662824,2.78297683033429));
#239199=CARTESIAN_POINT('Ctrl Pts',(36.7042135591852,-50.8353827952104,
2.79314401478846));
#239200=CARTESIAN_POINT('Ctrl Pts',(36.696217769431,-50.8274903908659,2.80341452427885));
#239201=CARTESIAN_POINT('Ctrl Pts',(36.6883299498358,-50.8197045606284,
2.81354634721317));
#239202=CARTESIAN_POINT('Ctrl Pts',(36.6811063421674,-50.8113095502205,
2.82378004209163));
#239203=CARTESIAN_POINT('Ctrl Pts',(36.6746059268184,-50.8023624960585,
2.83404198860227));
#239204=CARTESIAN_POINT('Ctrl Pts',(34.6525130919802,-48.0191904766731,
2.83404198860228));
#239205=CARTESIAN_POINT('Ctrl Pts',(34.646292158807,-48.0106280967249,2.82422126442986));
#239206=CARTESIAN_POINT('Ctrl Pts',(34.6407689407921,-48.0016058360806,
2.81442815028493));
#239207=CARTESIAN_POINT('Ctrl Pts',(34.6359660967493,-47.9921771448963,
2.80471618166322));
#239208=CARTESIAN_POINT('Ctrl Pts',(34.6313285282533,-47.9830729139852,
2.79533842146252));
#239209=CARTESIAN_POINT('Ctrl Pts',(34.6273621044917,-47.9735885825102,
2.78603515650279));
#239210=CARTESIAN_POINT('Ctrl Pts',(34.6241270221289,-47.9637494987653,
2.77685887346812));
#239211=CARTESIAN_POINT('Ctrl Pts',(34.6210688561311,-47.9544484832163,
2.76818441216655));
#239212=CARTESIAN_POINT('Ctrl Pts',(34.6186639474978,-47.9448295964466,
2.75962261521724));
#239213=CARTESIAN_POINT('Ctrl Pts',(34.617004586212,-47.9349076763715,2.7512353770178));
#239214=CARTESIAN_POINT('Ctrl Pts',(34.6154763423057,-47.9257697544352,
2.74351087134269));
#239215=CARTESIAN_POINT('Ctrl Pts',(34.6145804463112,-47.9163742511068,
2.73593399450026));
#239216=CARTESIAN_POINT('Ctrl Pts',(34.6144269453425,-47.906736439065,2.72857657812782));
#239217=CARTESIAN_POINT('Ctrl Pts',(34.6143811744522,-47.9038626380657,
2.72638274508443));
#239218=CARTESIAN_POINT('Ctrl Pts',(34.6144016870569,-47.9009673483049,
2.72420861709637));
#239219=CARTESIAN_POINT('Ctrl Pts',(34.6144921419179,-47.89805115192,2.72205663736675));
#239220=CARTESIAN_POINT('Ctrl Pts',(34.6145816725532,-47.8951647518761,
2.71992664556714));
#239221=CARTESIAN_POINT('Ctrl Pts',(34.6147393566956,-47.8922608568393,
2.71782089927832));
#239222=CARTESIAN_POINT('Ctrl Pts',(34.61496832346,-47.8893433277779,2.71574387311194));
#239223=CARTESIAN_POINT('Ctrl Pts',(34.614984245361,-47.8891404485128,2.71559944077434));
#239224=CARTESIAN_POINT('Ctrl Pts',(34.61500050176,-47.8889374970509,2.71545515216017));
#239225=CARTESIAN_POINT('Ctrl Pts',(34.6150170939194,-47.8887344737208,
2.71531100781678));
#239226=CARTESIAN_POINT('Ctrl Pts',(34.6157445549674,-47.8798331871994,
2.70899119176039));
#239227=CARTESIAN_POINT('Ctrl Pts',(34.6171603320598,-47.8708080647645,
2.70298296066801));
#239228=CARTESIAN_POINT('Ctrl Pts',(34.619329190174,-47.8617555581812,2.69736727774105));
#239229=CARTESIAN_POINT('Ctrl Pts',(34.6213509428814,-47.8533170487307,
2.69213248525409));
#239230=CARTESIAN_POINT('Ctrl Pts',(34.6240275231023,-47.8448540540101,
2.68723866185458));
#239231=CARTESIAN_POINT('Ctrl Pts',(34.6274308957717,-47.8364666369698,
2.68278595829559));
#239232=CARTESIAN_POINT('Ctrl Pts',(34.6286758935246,-47.8333984113061,
2.68115710172785));
#239233=CARTESIAN_POINT('Ctrl Pts',(34.6300183184514,-47.8303405713847,
2.67958763637774));
#239234=CARTESIAN_POINT('Ctrl Pts',(34.6314622582454,-47.8272990958124,
2.67808378645315));
#239235=CARTESIAN_POINT('Ctrl Pts',(34.631809477528,-47.8265677225441,2.6777221607855));
#239236=CARTESIAN_POINT('Ctrl Pts',(34.6321630753109,-47.8258370084441,
2.67736403603513));
#239237=CARTESIAN_POINT('Ctrl Pts',(34.6325230544381,-47.8251070891643,
2.67700956934429));
#239238=CARTESIAN_POINT('Ctrl Pts',(34.6328717842176,-47.824399979862,2.67666617973753));
#239239=CARTESIAN_POINT('Ctrl Pts',(34.6332265027185,-47.8236936164938,
2.67632622314069));
#239240=CARTESIAN_POINT('Ctrl Pts',(34.6335872094469,-47.8229881245974,
2.67598984158723));
#239241=CARTESIAN_POINT('Ctrl Pts',(34.6375391685168,-47.815258645554,2.67230439292157));
#239242=CARTESIAN_POINT('Ctrl Pts',(34.6422128973072,-47.8076288798872,
2.66904964539901));
#239243=CARTESIAN_POINT('Ctrl Pts',(34.6475865476022,-47.8002860618998,
2.66640203566645));
#239244=CARTESIAN_POINT('Ctrl Pts',(34.6498151605506,-47.7972407764148,
2.66530399299372));
#239245=CARTESIAN_POINT('Ctrl Pts',(34.6521637338121,-47.7942448304643,
2.664309951422));
#239246=CARTESIAN_POINT('Ctrl Pts',(34.6546289547343,-47.7913110614413,
2.66343053473309));
#239247=CARTESIAN_POINT('Ctrl Pts',(34.6588336459115,-47.786307212652,2.66193059792832));
#239248=CARTESIAN_POINT('Ctrl Pts',(34.6633779280164,-47.7814867201288,
2.66076519817074));
#239249=CARTESIAN_POINT('Ctrl Pts',(34.6682420184012,-47.7769196237418,
2.65997805604406));
#239250=CARTESIAN_POINT('Ctrl Pts',(34.6706740635937,-47.7746360755483,
2.65958448498072));
#239251=CARTESIAN_POINT('Ctrl Pts',(34.6731869650549,-47.7724170058814,
2.65928526260708));
#239252=CARTESIAN_POINT('Ctrl Pts',(34.6757782448039,-47.7702712352606,
2.6590846397127));
#239253=CARTESIAN_POINT('Ctrl Pts',(34.6783695245528,-47.7681254646397,
2.65888401681832));
#239254=CARTESIAN_POINT('Ctrl Pts',(34.6810391382375,-47.7660530039188,
2.65878198860229));
#239255=CARTESIAN_POINT('Ctrl Pts',(34.6837837831351,-47.7640607692758,
2.65878198860229));
#239256=CARTESIAN_POINT('Origin',(38.9973987043324,-43.2882232241942,2.83404198860232));
#239257=CARTESIAN_POINT('Ctrl Pts',(42.0671296588101,-46.4355828792663,
2.8340419886023));
#239258=CARTESIAN_POINT('Ctrl Pts',(42.0742293550387,-46.4434678907493,
2.82419652439974));
#239259=CARTESIAN_POINT('Ctrl Pts',(42.0806858315488,-46.4518896956746,
2.81438790575495));
#239260=CARTESIAN_POINT('Ctrl Pts',(42.0864721532177,-46.460795700733,2.80466781256683));
#239261=CARTESIAN_POINT('Ctrl Pts',(42.0920704538876,-46.4694123136587,
2.79526356452807));
#239262=CARTESIAN_POINT('Ctrl Pts',(42.0970420880529,-46.4784832882836,
2.78594102495908));
#239263=CARTESIAN_POINT('Ctrl Pts',(42.1013257711413,-46.487988795821,2.77675109088403));
#239264=CARTESIAN_POINT('Ctrl Pts',(42.1053778715689,-46.4969804206359,
2.76805797913257));
#239265=CARTESIAN_POINT('Ctrl Pts',(42.1088147776147,-46.5063617095277,
2.75948271209687));
#239266=CARTESIAN_POINT('Ctrl Pts',(42.1115441100145,-46.5161273793285,
2.75108575572704));
#239267=CARTESIAN_POINT('Ctrl Pts',(42.1140580225452,-46.5251222674863,
2.74335155162698));
#239268=CARTESIAN_POINT('Ctrl Pts',(42.1159717447032,-46.5344438074388,
2.73576818685323));
#239269=CARTESIAN_POINT('Ctrl Pts',(42.1171748456151,-46.5440884908269,
2.72840626159835));
#239270=CARTESIAN_POINT('Ctrl Pts',(42.1175238194559,-46.5468860468524,
2.72627084693231));
#239271=CARTESIAN_POINT('Ctrl Pts',(42.1178127362988,-46.5497107674253,
2.72415424587285));
#239272=CARTESIAN_POINT('Ctrl Pts',(42.1180382068981,-46.5525624800835,
2.72205867173227));
#239273=CARTESIAN_POINT('Ctrl Pts',(42.1182826315244,-46.5556539199568,
2.7197869346283));
#239274=CARTESIAN_POINT('Ctrl Pts',(42.1184532289198,-46.5587726948493,
2.7175441134073));
#239275=CARTESIAN_POINT('Ctrl Pts',(42.1185461584685,-46.5619176830188,
2.71533341844227));
#239276=CARTESIAN_POINT('Ctrl Pts',(42.118801204344,-46.5705491277282,2.70926614876372));
#239277=CARTESIAN_POINT('Ctrl Pts',(42.1184278543827,-46.5793682643805,
2.70347381860389));
#239278=CARTESIAN_POINT('Ctrl Pts',(42.1173773384973,-46.5882835698998,
2.69804914171374));
#239279=CARTESIAN_POINT('Ctrl Pts',(42.1164161734959,-46.5964405904273,
2.69308585687143));
#239280=CARTESIAN_POINT('Ctrl Pts',(42.114880157948,-46.6046697328847,2.68842799053089));
#239281=CARTESIAN_POINT('Ctrl Pts',(42.1127009621828,-46.6129145292198,
2.68414767054092));
#239282=CARTESIAN_POINT('Ctrl Pts',(42.1116305483418,-46.6169643462458,
2.68204519134462));
#239283=CARTESIAN_POINT('Ctrl Pts',(42.1104045383081,-46.6210176421365,
2.68003431778445));
#239284=CARTESIAN_POINT('Ctrl Pts',(42.1090123875514,-46.6250654385586,
2.67812693945225));
#239285=CARTESIAN_POINT('Ctrl Pts',(42.108748240505,-46.6258334685037,2.67776503299177));
#239286=CARTESIAN_POINT('Ctrl Pts',(42.1084776383334,-46.6266015422607,
2.67740659639897));
#239287=CARTESIAN_POINT('Ctrl Pts',(42.1082005605491,-46.6273695213199,
2.67705178968829));
#239288=CARTESIAN_POINT('Ctrl Pts',(42.1079321414455,-46.6281135010335,
2.67670807068731));
#239289=CARTESIAN_POINT('Ctrl Pts',(42.1076576451506,-46.628857391859,2.67636775825239));
#239290=CARTESIAN_POINT('Ctrl Pts',(42.1073770559085,-46.6296010653153,
2.67603099699229));
#239291=CARTESIAN_POINT('Ctrl Pts',(42.1043192521654,-46.6377054654036,
2.67236104217142));
#239292=CARTESIAN_POINT('Ctrl Pts',(42.1005354505687,-46.6457892400048,
2.6691144054152));
#239293=CARTESIAN_POINT('Ctrl Pts',(42.096023846079,-46.653661939073,2.66646778189694));
#239294=CARTESIAN_POINT('Ctrl Pts',(42.0941185674866,-46.6569866287779,
2.66535009635002));
#239295=CARTESIAN_POINT('Ctrl Pts',(42.0920839261394,-46.6602736399397,
2.66433897912343));
#239296=CARTESIAN_POINT('Ctrl Pts',(42.0899216923184,-46.6635089796837,
2.66344564884769));
#239297=CARTESIAN_POINT('Ctrl Pts',(42.0862805445931,-46.6689572109688,
2.66194130298562));
#239298=CARTESIAN_POINT('Ctrl Pts',(42.0822770520162,-46.6742564366669,
2.66077206705398));
#239299=CARTESIAN_POINT('Ctrl Pts',(42.0779224130576,-46.6793332901443,
2.65998225155693));
#239300=CARTESIAN_POINT('Ctrl Pts',(42.076833753318,-46.6806025035137,2.65978479768267));
#239301=CARTESIAN_POINT('Ctrl Pts',(42.0757229796951,-46.6818576549898,
2.65961098966601));
#239302=CARTESIAN_POINT('Ctrl Pts',(42.0745900553981,-46.6830973739104,
2.65946139030481));
#239303=CARTESIAN_POINT('Ctrl Pts',(42.0728906689526,-46.6849569522912,
2.659236991263));
#239304=CARTESIAN_POINT('Ctrl Pts',(42.0711414461008,-46.6867817869753,
2.65906707562422));
#239305=CARTESIAN_POINT('Ctrl Pts',(42.0693433991613,-46.6885684866726,
2.658953325629));
#239306=CARTESIAN_POINT('Ctrl Pts',(42.0675453522218,-46.6903551863698,
2.65883957563378));
#239307=CARTESIAN_POINT('Ctrl Pts',(42.065698492617,-46.6921037531344,2.6587819886023));
#239308=CARTESIAN_POINT('Ctrl Pts',(42.0638038389706,-46.6938111422597,
2.6587819886023));
#239309=CARTESIAN_POINT('Ctrl Pts',(39.5091373124628,-43.856566526705,2.65878198860232));
#239310=CARTESIAN_POINT('Ctrl Pts',(39.5155480799608,-43.8507890749201,
2.65878198860232));
#239311=CARTESIAN_POINT('Ctrl Pts',(39.5223801852471,-43.8455908828144,
2.65945335517828));
#239312=CARTESIAN_POINT('Ctrl Pts',(39.5294841269573,-43.8409939475736,
2.66072561226578));
#239313=CARTESIAN_POINT('Ctrl Pts',(39.5340725443953,-43.838024799081,2.66154735980316));
#239314=CARTESIAN_POINT('Ctrl Pts',(39.5387738681338,-43.8353056940454,
2.66261895766858));
#239315=CARTESIAN_POINT('Ctrl Pts',(39.5435446222369,-43.832834301743,2.66391429250998));
#239316=CARTESIAN_POINT('Ctrl Pts',(39.5498679835149,-43.8295586128163,
2.66563118464095));
#239317=CARTESIAN_POINT('Ctrl Pts',(39.5563148866448,-43.8267236865055,
2.6677410513867));
#239318=CARTESIAN_POINT('Ctrl Pts',(39.5627952650345,-43.8243293609617,
2.6701689418172));
#239319=CARTESIAN_POINT('Ctrl Pts',(39.5660354542293,-43.8231321981898,
2.67138288703246));
#239320=CARTESIAN_POINT('Ctrl Pts',(39.5692841591691,-43.8220450509619,
2.67267613167522));
#239321=CARTESIAN_POINT('Ctrl Pts',(39.572531167366,-43.8210669472512,2.67403835432524));
#239322=CARTESIAN_POINT('Ctrl Pts',(39.5741546714645,-43.8205778953958,
2.67471946565025));
#239323=CARTESIAN_POINT('Ctrl Pts',(39.5757777635552,-43.8201160933889,
2.67541781389493));
#239324=CARTESIAN_POINT('Ctrl Pts',(39.57739924345,-43.8196813503772,2.6761320724414));
#239325=CARTESIAN_POINT('Ctrl Pts',(39.5778046134237,-43.8195726646243,
2.67631063707801));
#239326=CARTESIAN_POINT('Ctrl Pts',(39.5782098828935,-43.8194656698232,
2.67649019601816));
#239327=CARTESIAN_POINT('Ctrl Pts',(39.5786150336271,-43.8193603625169,
2.67667072836627));
#239328=CARTESIAN_POINT('Ctrl Pts',(39.5798304858281,-43.8190444405979,
2.67721232541061));
#239329=CARTESIAN_POINT('Ctrl Pts',(39.5810448681194,-43.8187437073117,
2.67776268340017));
#239330=CARTESIAN_POINT('Ctrl Pts',(39.5822576997166,-43.8184580587796,
2.67832123541486));
#239331=CARTESIAN_POINT('Ctrl Pts',(39.5908007288818,-43.8164459874028,
2.6822556036842));
#239332=CARTESIAN_POINT('Ctrl Pts',(39.5992865061394,-43.8151322889025,
2.68661792998872));
#239333=CARTESIAN_POINT('Ctrl Pts',(39.6076412948842,-43.8144227306305,
2.69130986622569));
#239334=CARTESIAN_POINT('Ctrl Pts',(39.611693358397,-43.8140785956353,2.69358545023039));
#239335=CARTESIAN_POINT('Ctrl Pts',(39.6157150281166,-43.8138769687213,
2.69593918853448));
#239336=CARTESIAN_POINT('Ctrl Pts',(39.6196997093547,-43.8138093098897,
2.69836306235446));
#239337=CARTESIAN_POINT('Ctrl Pts',(39.6257999779287,-43.8137057289457,
2.70207384382179));
#239338=CARTESIAN_POINT('Ctrl Pts',(39.6318101761586,-43.8139151128793,
2.70594760814179));
#239339=CARTESIAN_POINT('Ctrl Pts',(39.6376940219325,-43.8144090029872,
2.70995196345659));
#239340=CARTESIAN_POINT('Ctrl Pts',(39.6404265103489,-43.8146383681083,
2.71181160678057));
#239341=CARTESIAN_POINT('Ctrl Pts',(39.6431316855286,-43.8149288459961,
2.7136996277205));
#239342=CARTESIAN_POINT('Ctrl Pts',(39.6458055463966,-43.8152787628647,
2.71561183138612));
#239343=CARTESIAN_POINT('Ctrl Pts',(39.6460104872966,-43.8153055826139,
2.71575839426263));
#239344=CARTESIAN_POINT('Ctrl Pts',(39.6462152612038,-43.8153327221687,
2.7159050890316));
#239345=CARTESIAN_POINT('Ctrl Pts',(39.6464198673379,-43.8153601802948,
2.71605191409863));
#239346=CARTESIAN_POINT('Ctrl Pts',(39.6492939666541,-43.8157458841817,
2.71811436362704));
#239347=CARTESIAN_POINT('Ctrl Pts',(39.6521348180511,-43.8161965332328,
2.7202009102691));
#239348=CARTESIAN_POINT('Ctrl Pts',(39.6549389970093,-43.8167075634904,
2.72230624862133));
#239349=CARTESIAN_POINT('Ctrl Pts',(39.6649942840471,-43.8185400271104,
2.72985561753061));
#239350=CARTESIAN_POINT('Ctrl Pts',(39.6746561192251,-43.8211611138364,
2.73770089914295));
#239351=CARTESIAN_POINT('Ctrl Pts',(39.6839173731638,-43.8244418968094,
2.74574823347047));
#239352=CARTESIAN_POINT('Ctrl Pts',(39.6940945608671,-43.828047147713,2.75459144547006));
#239353=CARTESIAN_POINT('Ctrl Pts',(39.7037886794679,-43.8324491002306,
2.76367911754261));
#239354=CARTESIAN_POINT('Ctrl Pts',(39.7129876499616,-43.8375295667866,
2.77292162564728));
#239355=CARTESIAN_POINT('Ctrl Pts',(39.7229202294684,-43.8430151956441,
2.78290121484759));
#239356=CARTESIAN_POINT('Ctrl Pts',(39.7322766233313,-43.8492922888414,
2.79306229500245));
#239357=CARTESIAN_POINT('Ctrl Pts',(39.7410245486304,-43.8562669044101,
2.80331916685339));
#239358=CARTESIAN_POINT('Ctrl Pts',(39.7496990878239,-43.8631830101199,
2.81348999408741));
#239359=CARTESIAN_POINT('Ctrl Pts',(39.7577762496646,-43.8707860819059,
2.82375635966885));
#239360=CARTESIAN_POINT('Ctrl Pts',(39.7651933659004,-43.8790236240213,
2.83404198860232));
#239361=CARTESIAN_POINT('Origin',(-0.0113255271402735,-0.0101975504407155,
2.83404198860262));
#239362=CARTESIAN_POINT('Ctrl Pts',(42.0411527846901,-46.7142062431416,
2.6587819886023));
#239363=CARTESIAN_POINT('Ctrl Pts',(42.0347675597393,-46.7199506919421,
2.6587819886023));
#239364=CARTESIAN_POINT('Ctrl Pts',(42.0279592142781,-46.7251107020207,
2.65944603041816));
#239365=CARTESIAN_POINT('Ctrl Pts',(42.0208774479585,-46.7296675019389,
2.66070439264032));
#239366=CARTESIAN_POINT('Ctrl Pts',(42.0163525364099,-46.7325790801589,
2.66150842619558));
#239367=CARTESIAN_POINT('Ctrl Pts',(42.0117164852002,-46.7352451892134,
2.66255428265334));
#239368=CARTESIAN_POINT('Ctrl Pts',(42.0070114066752,-46.7376689638746,
2.66381699700625));
#239369=CARTESIAN_POINT('Ctrl Pts',(42.0005899185702,-46.7409769299529,
2.66554034873225));
#239370=CARTESIAN_POINT('Ctrl Pts',(41.9940383480783,-46.7438276087414,
2.6676675964393));
#239371=CARTESIAN_POINT('Ctrl Pts',(41.9874523371586,-46.7462229640882,
2.67012012783106));
#239372=CARTESIAN_POINT('Ctrl Pts',(41.9841593316988,-46.7474206417616,
2.67134639352694));
#239373=CARTESIAN_POINT('Ctrl Pts',(41.9808575622229,-46.7485046297341,
2.6726537558497));
#239374=CARTESIAN_POINT('Ctrl Pts',(41.9775578801523,-46.7494761782927,
2.67403135126898));
#239375=CARTESIAN_POINT('Ctrl Pts',(41.9759080391171,-46.749961952572,2.67472014897862));
#239376=CARTESIAN_POINT('Ctrl Pts',(41.9742587070261,-46.7504196286874,
2.6754264966859));
#239377=CARTESIAN_POINT('Ctrl Pts',(41.9726111592845,-46.7508494364806,
2.67614899656059));
#239378=CARTESIAN_POINT('Ctrl Pts',(41.9721992723491,-46.7509568884289,
2.67632962152926));
#239379=CARTESIAN_POINT('Ctrl Pts',(41.9717874966612,-46.7510625988569,
2.67651125590908));
#239380=CARTESIAN_POINT('Ctrl Pts',(41.9713758515963,-46.75116657186,2.67669387767482));
#239381=CARTESIAN_POINT('Ctrl Pts',(41.9701409164017,-46.7514784908693,
2.67724174297202));
#239382=CARTESIAN_POINT('Ctrl Pts',(41.9689071581774,-46.7517747718017,
2.67779849504705));
#239383=CARTESIAN_POINT('Ctrl Pts',(41.9676750878625,-46.7520555364226,
2.67836353617967));
#239384=CARTESIAN_POINT('Ctrl Pts',(41.9591607175419,-46.7539957941547,
2.68226832098866));
#239385=CARTESIAN_POINT('Ctrl Pts',(41.9507055072921,-46.7552464720202,
2.6865915375135));
#239386=CARTESIAN_POINT('Ctrl Pts',(41.9423805287172,-46.7559027543574,
2.69123699486138));
#239387=CARTESIAN_POINT('Ctrl Pts',(41.9382430372171,-46.7562289248775,
2.69354577441174));
#239388=CARTESIAN_POINT('Ctrl Pts',(41.9341372814973,-46.7564078446189,
2.69593478828073));
#239389=CARTESIAN_POINT('Ctrl Pts',(41.9300700339489,-46.7564487173136,
2.69839565261173));
#239390=CARTESIAN_POINT('Ctrl Pts',(41.9210970783574,-46.7565388885832,
2.70382468688997));
#239391=CARTESIAN_POINT('Ctrl Pts',(41.9123126321659,-46.7559695796219,
2.70961155815039));
#239392=CARTESIAN_POINT('Ctrl Pts',(41.903846506269,-46.7548061840811,2.71562701361718));
#239393=CARTESIAN_POINT('Ctrl Pts',(41.9007537237153,-46.7543811810188,
2.71782453535808));
#239394=CARTESIAN_POINT('Ctrl Pts',(41.8976992635451,-46.7538836816017,
2.72005051502352));
#239395=CARTESIAN_POINT('Ctrl Pts',(41.8946854937106,-46.7533184435771,
2.72229986760064));
#239396=CARTESIAN_POINT('Ctrl Pts',(41.8845625597436,-46.751419868864,2.72985520488842));
#239397=CARTESIAN_POINT('Ctrl Pts',(41.8748360802679,-46.7487367327307,
2.73770845534509));
#239398=CARTESIAN_POINT('Ctrl Pts',(41.865513778658,-46.7453971059998,2.74576706701706));
#239399=CARTESIAN_POINT('Ctrl Pts',(41.8552674648894,-46.7417264606178,
2.75462443584986));
#239400=CARTESIAN_POINT('Ctrl Pts',(41.8455087367155,-46.7372626589204,
2.76373036323144));
#239401=CARTESIAN_POINT('Ctrl Pts',(41.8362508575448,-46.7321227530954,
2.77299664636788));
#239402=CARTESIAN_POINT('Ctrl Pts',(41.8262797250094,-46.7265868542943,
2.78297683033457));
#239403=CARTESIAN_POINT('Ctrl Pts',(41.8168884800878,-46.7202662104738,
2.7931440147889));
#239404=CARTESIAN_POINT('Ctrl Pts',(41.8081115112088,-46.7132528291616,
2.80341452427952));
#239405=CARTESIAN_POINT('Ctrl Pts',(41.7994530610451,-46.706334152178,2.81354634721356));
#239406=CARTESIAN_POINT('Ctrl Pts',(41.7913915075187,-46.6987402031246,
2.82378004209179));
#239407=CARTESIAN_POINT('Ctrl Pts',(41.7839914803032,-46.690521640289,2.8340419886023));
#239408=CARTESIAN_POINT('Ctrl Pts',(39.4820551873935,-44.1339623850441,
2.83404198860232));
#239409=CARTESIAN_POINT('Ctrl Pts',(39.4749733207249,-44.1260971752936,
2.82422126442949));
#239410=CARTESIAN_POINT('Ctrl Pts',(39.4685372764356,-44.1177016730281,
2.81442815028416));
#239411=CARTESIAN_POINT('Ctrl Pts',(39.4627751762747,-44.1088266671073,
2.80471618166206));
#239412=CARTESIAN_POINT('Ctrl Pts',(39.4572113615976,-44.1002570680336,
2.79533842146101));
#239413=CARTESIAN_POINT('Ctrl Pts',(39.4522752837261,-44.0912392968988,
2.78603515650095));
#239414=CARTESIAN_POINT('Ctrl Pts',(39.4480294591791,-44.0817922708717,
2.77685887346595));
#239415=CARTESIAN_POINT('Ctrl Pts',(39.4440158252724,-44.0728618726508,
2.76818441216407));
#239416=CARTESIAN_POINT('Ctrl Pts',(39.4406186435279,-44.0635470605525,
2.75962261521446));
#239417=CARTESIAN_POINT('Ctrl Pts',(39.4379312493388,-44.0538529442785,
2.75123537701474));
#239418=CARTESIAN_POINT('Ctrl Pts',(39.4354562043751,-44.0449248258212,
2.74351087133926));
#239419=CARTESIAN_POINT('Ctrl Pts',(39.4335831186682,-44.0356744386741,
2.73593399449648));
#239420=CARTESIAN_POINT('Ctrl Pts',(39.432423032912,-44.0261054687947,2.72857657812373));
#239421=CARTESIAN_POINT('Ctrl Pts',(39.4320771187575,-44.0232521951406,
2.72638274508174));
#239422=CARTESIAN_POINT('Ctrl Pts',(39.4317948788029,-44.0203706219308,
2.72420861709505));
#239423=CARTESIAN_POINT('Ctrl Pts',(39.4315800126161,-44.017460945669,2.72205663736677));
#239424=CARTESIAN_POINT('Ctrl Pts',(39.4313673418322,-44.0145809991268,
2.71992664556716));
#239425=CARTESIAN_POINT('Ctrl Pts',(39.4312206224788,-44.0116765294498,
2.71782089927835));
#239426=CARTESIAN_POINT('Ctrl Pts',(39.4311433701099,-44.0087510493739,
2.71574387311197));
#239427=CARTESIAN_POINT('Ctrl Pts',(39.4311379981313,-44.0085476172107,
2.71559944077438));
#239428=CARTESIAN_POINT('Ctrl Pts',(39.4311329512716,-44.0083440782818,
2.7154551521602));
#239429=CARTESIAN_POINT('Ctrl Pts',(39.4311282308207,-44.0081404327819,
2.71531100781681));
#239430=CARTESIAN_POINT('Ctrl Pts',(39.4309212689598,-43.9992118680539,
2.70899119176044));
#239431=CARTESIAN_POINT('Ctrl Pts',(39.4313859080982,-43.9900881971803,
2.70298296066808));
#239432=CARTESIAN_POINT('Ctrl Pts',(39.4325966403788,-43.9808585737695,
2.69736727774114));
#239433=CARTESIAN_POINT('Ctrl Pts',(39.4337252532882,-43.9722549606532,
2.69213248525424));
#239434=CARTESIAN_POINT('Ctrl Pts',(39.4355025470898,-43.9635585482861,
2.6872386618548));
#239435=CARTESIAN_POINT('Ctrl Pts',(39.4380105519135,-43.954861329079,2.68278595829586));
#239436=CARTESIAN_POINT('Ctrl Pts',(39.4389280125249,-43.9516797737744,
2.68115710172802));
#239437=CARTESIAN_POINT('Ctrl Pts',(39.4399434521997,-43.9484983634053,
2.67958763637782));
#239438=CARTESIAN_POINT('Ctrl Pts',(39.4410615611728,-43.9453226165465,
2.67808378645314));
#239439=CARTESIAN_POINT('Ctrl Pts',(39.4413304290281,-43.9445589555194,
2.67772216078549));
#239440=CARTESIAN_POINT('Ctrl Pts',(39.4416057093433,-43.9437952833149,
2.67736403603512));
#239441=CARTESIAN_POINT('Ctrl Pts',(39.4418874191266,-43.9430317345443,
2.67700956934428));
#239442=CARTESIAN_POINT('Ctrl Pts',(39.4421603254791,-43.9422920466728,
2.67666617973753));
#239443=CARTESIAN_POINT('Ctrl Pts',(39.4424392657175,-43.9415524746572,
2.67632622314068));
#239444=CARTESIAN_POINT('Ctrl Pts',(39.442724252473,-43.9408131433993,2.67598984158722));
#239445=CARTESIAN_POINT('Ctrl Pts',(39.4458466117312,-43.9327129150425,
2.67230439292165));
#239446=CARTESIAN_POINT('Ctrl Pts',(39.4496972096659,-43.9246364083424,
2.66904964539915));
#239447=CARTESIAN_POINT('Ctrl Pts',(39.454273889062,-43.9167721156729,2.66640203566663));
#239448=CARTESIAN_POINT('Ctrl Pts',(39.4561719744236,-43.9135105590935,
2.66530399299382));
#239449=CARTESIAN_POINT('Ctrl Pts',(39.458194520329,-43.9102855324943,2.66430995142205));
#239450=CARTESIAN_POINT('Ctrl Pts',(39.4603395741455,-43.9071101492102,
2.66343053473309));
#239451=CARTESIAN_POINT('Ctrl Pts',(39.4639981869602,-43.9016942021209,
2.66193059792833));
#239452=CARTESIAN_POINT('Ctrl Pts',(39.4680136963365,-43.896425109935,2.66076519817076));
#239453=CARTESIAN_POINT('Ctrl Pts',(39.4723737491582,-43.8913745966866,
2.65997805604408));
#239454=CARTESIAN_POINT('Ctrl Pts',(39.4745537755691,-43.8888493400624,
2.65958448498074));
#239455=CARTESIAN_POINT('Ctrl Pts',(39.4768209551511,-43.8863797569633,
2.6592852626071));
#239456=CARTESIAN_POINT('Ctrl Pts',(39.479173745493,-43.8839748786084,2.65908463971272));
#239457=CARTESIAN_POINT('Ctrl Pts',(39.4815265358348,-43.8815700002535,
2.65888401681834));
#239458=CARTESIAN_POINT('Ctrl Pts',(39.4839648939622,-43.8792298420734,
2.65878198860232));
#239459=CARTESIAN_POINT('Ctrl Pts',(39.4864862581822,-43.8769616275868,
2.65878198860232));
#239460=CARTESIAN_POINT('Origin',(43.3086183250771,-38.9747476500507,2.83404198860235));
#239461=CARTESIAN_POINT('Ctrl Pts',(46.6905216402902,-41.7839914803019,
2.83404198860233));
#239462=CARTESIAN_POINT('Ctrl Pts',(46.6984066517725,-41.7910911765299,
2.82419652440033));
#239463=CARTESIAN_POINT('Ctrl Pts',(46.7057080773549,-41.7987919603583,
2.81438790575617));
#239464=CARTESIAN_POINT('Ctrl Pts',(46.7123936319704,-41.8070443420764,
2.8046678125687));
#239465=CARTESIAN_POINT('Ctrl Pts',(46.7188619458709,-41.8150285705284,
2.79526356453048));
#239466=CARTESIAN_POINT('Ctrl Pts',(46.7247545199416,-41.8235301761253,
2.78594102496204));
#239467=CARTESIAN_POINT('Ctrl Pts',(46.7300083326611,-41.8325358446869,
2.77675109088754));
#239468=CARTESIAN_POINT('Ctrl Pts',(46.7349781159827,-41.8410546526089,
2.76805797913662));
#239469=CARTESIAN_POINT('Ctrl Pts',(46.7393768060089,-41.8500252953105,
2.75948271210145));
#239470=CARTESIAN_POINT('Ctrl Pts',(46.7431119772974,-41.8594521748281,
2.75108575573212));
#239471=CARTESIAN_POINT('Ctrl Pts',(46.7465523401886,-41.868135012633,2.74335155163261));
#239472=CARTESIAN_POINT('Ctrl Pts',(46.7494299450231,-41.8772054497771,
2.73576818685938));
#239473=CARTESIAN_POINT('Ctrl Pts',(46.7516345991559,-41.8866715402901,
2.72840626160495));
#239474=CARTESIAN_POINT('Ctrl Pts',(46.7522740855145,-41.8894172933145,
2.72627084693667));
#239475=CARTESIAN_POINT('Ctrl Pts',(46.752856683342,-41.8921963397418,2.72415424587501));
#239476=CARTESIAN_POINT('Ctrl Pts',(46.7533790039321,-41.8950088623273,
2.72205867173227));
#239477=CARTESIAN_POINT('Ctrl Pts',(46.753945233034,-41.8980578176389,2.7197869346283));
#239478=CARTESIAN_POINT('Ctrl Pts',(46.7544408966258,-41.9011416752726,
2.71754411340731));
#239479=CARTESIAN_POINT('Ctrl Pts',(46.7548620578771,-41.9042597210849,
2.71533341844229));
#239480=CARTESIAN_POINT('Ctrl Pts',(46.7560179382359,-41.9128172222837,
2.70926614876376));
#239481=CARTESIAN_POINT('Ctrl Pts',(46.7565684843263,-41.9216270724804,
2.70347381860393));
#239482=CARTESIAN_POINT('Ctrl Pts',(46.7564556264623,-41.9306033478343,
2.69804914171379));
#239483=CARTESIAN_POINT('Ctrl Pts',(46.756352367644,-41.9388161524498,2.69308585687191));
#239484=CARTESIAN_POINT('Ctrl Pts',(46.7556849461651,-41.9471607721479,
2.68842799053174));
#239485=CARTESIAN_POINT('Ctrl Pts',(46.7543795041534,-41.9555881906098,
2.68414767054208));
#239486=CARTESIAN_POINT('Ctrl Pts',(46.7537382753017,-41.9597277110289,
2.68204519134541));
#239487=CARTESIAN_POINT('Ctrl Pts',(46.7529426662698,-41.9638869554861,
2.6800343177849));
#239488=CARTESIAN_POINT('Ctrl Pts',(46.7519812518,-41.9680580970358,2.67812693945238));
#239489=CARTESIAN_POINT('Ctrl Pts',(46.7517988327686,-41.9688495305174,
2.6777650329919));
#239490=CARTESIAN_POINT('Ctrl Pts',(46.7516099985535,-41.9696416823151,
2.6774065963991));
#239491=CARTESIAN_POINT('Ctrl Pts',(46.7514147143012,-41.9704344168197,
2.67705178968841));
#239492=CARTESIAN_POINT('Ctrl Pts',(46.7512255326818,-41.9712023783709,
2.67670807068744));
#239493=CARTESIAN_POINT('Ctrl Pts',(46.7510302978711,-41.9719708867605,
2.67636775825252));
#239494=CARTESIAN_POINT('Ctrl Pts',(46.7508289807698,-41.9727398158581,
2.67603099699241));
#239495=CARTESIAN_POINT('Ctrl Pts',(46.7486350684823,-41.9811194467219,
2.67236104217115));
#239496=CARTESIAN_POINT('Ctrl Pts',(46.7457169794826,-41.9895544525272,
2.6691144054146));
#239497=CARTESIAN_POINT('Ctrl Pts',(46.7420530111692,-41.9978556152113,
2.66646778189617));
#239498=CARTESIAN_POINT('Ctrl Pts',(46.7405056945983,-42.0013612477604,
2.6653500963496));
#239499=CARTESIAN_POINT('Ctrl Pts',(46.7388257854552,-42.0048429302636,
2.6643389791233));
#239500=CARTESIAN_POINT('Ctrl Pts',(46.7370135816694,-42.0082865614556,
2.66344564884778));
#239501=CARTESIAN_POINT('Ctrl Pts',(46.733961875776,-42.0140855503359,2.66194130298571));
#239502=CARTESIAN_POINT('Ctrl Pts',(46.7305342346691,-42.0197742252479,
2.66077206705405));
#239503=CARTESIAN_POINT('Ctrl Pts',(46.7267341265709,-42.0252784509094,
2.65998225155699));
#239504=CARTESIAN_POINT('Ctrl Pts',(46.7257840995464,-42.0266545073248,
2.65978479768272));
#239505=CARTESIAN_POINT('Ctrl Pts',(46.7248106099125,-42.0280188904096,
2.65961098966606));
#239506=CARTESIAN_POINT('Ctrl Pts',(46.7238134778069,-42.029370240856,2.65946139030486));
#239507=CARTESIAN_POINT('Ctrl Pts',(46.7223177796487,-42.0313972665255,
2.65923699126304));
#239508=CARTESIAN_POINT('Ctrl Pts',(46.7207688863879,-42.0333949481509,
2.65906707562426));
#239509=CARTESIAN_POINT('Ctrl Pts',(46.7191674503113,-42.0353598072037,
2.65895332562904));
#239510=CARTESIAN_POINT('Ctrl Pts',(46.7175660142347,-42.0373246662565,
2.65883957563381));
#239511=CARTESIAN_POINT('Ctrl Pts',(46.7159120469168,-42.0392567035856,
2.65878198860233));
#239512=CARTESIAN_POINT('Ctrl Pts',(46.7142062431428,-42.0411527846888,
2.65878198860233));
#239513=CARTESIAN_POINT('Ctrl Pts',(43.8769616275879,-39.486486258181,2.65878198860235));
#239514=CARTESIAN_POINT('Ctrl Pts',(43.8827333680736,-39.4800703482071,
2.65878198860235));
#239515=CARTESIAN_POINT('Ctrl Pts',(43.8889846873393,-39.4741864828756,
2.65945335517819));
#239516=CARTESIAN_POINT('Ctrl Pts',(43.8955692023364,-39.4688721660173,
2.66072561226549));
#239517=CARTESIAN_POINT('Ctrl Pts',(43.8998221234149,-39.4654396626067,
2.6615473598029));
#239518=CARTESIAN_POINT('Ctrl Pts',(43.9042134689398,-39.4622440309668,
2.66261895766843));
#239519=CARTESIAN_POINT('Ctrl Pts',(43.9086997575137,-39.4592874976147,
2.66391429250999));
#239520=CARTESIAN_POINT('Ctrl Pts',(43.9146460760274,-39.4553687820175,
2.66563118464095));
#239521=CARTESIAN_POINT('Ctrl Pts',(43.9207613318567,-39.4518755008527,
2.6677410513867));
#239522=CARTESIAN_POINT('Ctrl Pts',(43.9269559348858,-39.4488169076803,
2.67016894181721));
#239523=CARTESIAN_POINT('Ctrl Pts',(43.9300532364004,-39.4472876110941,
2.67138288703246));
#239524=CARTESIAN_POINT('Ctrl Pts',(43.9331705067656,-39.4458668372375,
2.67267613167523));
#239525=CARTESIAN_POINT('Ctrl Pts',(43.936297487834,-39.4445546869042,2.67403835432524));
#239526=CARTESIAN_POINT('Ctrl Pts',(43.9378609783683,-39.4438986117375,
2.67471946565025));
#239527=CARTESIAN_POINT('Ctrl Pts',(43.9394269075365,-39.4432696802083,
2.67541781389495));
#239528=CARTESIAN_POINT('Ctrl Pts',(43.9409940617759,-39.4426678279627,
2.67613207244141));
#239529=CARTESIAN_POINT('Ctrl Pts',(43.9413858503357,-39.4425173649013,
2.67631063707802));
#239530=CARTESIAN_POINT('Ctrl Pts',(43.9417777156949,-39.4423685940341,
2.67649019601817));
#239531=CARTESIAN_POINT('Ctrl Pts',(43.9421696393595,-39.4422215138286,
2.67667072836629));
#239532=CARTESIAN_POINT('Ctrl Pts',(43.9433454103534,-39.4417802732122,
2.67721232541063));
#239533=CARTESIAN_POINT('Ctrl Pts',(43.9445217049433,-39.4413542498597,
2.67776268340019));
#239534=CARTESIAN_POINT('Ctrl Pts',(43.9456980341199,-39.440943390717,2.67832123541488));
#239535=CARTESIAN_POINT('Ctrl Pts',(43.9539839449481,-39.4380493519676,
2.68225560368406));
#239536=CARTESIAN_POINT('Ctrl Pts',(43.9622859173443,-39.4358558447888,
2.68661792998838));
#239537=CARTESIAN_POINT('Ctrl Pts',(43.970520768646,-39.4342768603229,2.69130986622514));
#239538=CARTESIAN_POINT('Ctrl Pts',(43.9745146626291,-39.4335110545631,
2.69358545023002));
#239539=CARTESIAN_POINT('Ctrl Pts',(43.9784932254701,-39.4328901532268,
2.69593918853429));
#239540=CARTESIAN_POINT('Ctrl Pts',(43.982449005934,-39.4324063524309,2.69836306235448));
#239541=CARTESIAN_POINT('Ctrl Pts',(43.9885050294416,-39.4316656872146,
2.70207384382181));
#239542=CARTESIAN_POINT('Ctrl Pts',(43.9945041897575,-39.4312456873362,
2.70594760814182));
#239543=CARTESIAN_POINT('Ctrl Pts',(44.0004074287827,-39.4311218425055,
2.70995196345661));
#239544=CARTESIAN_POINT('Ctrl Pts',(44.0031489235253,-39.4310643283254,
2.71181160678059));
#239545=CARTESIAN_POINT('Ctrl Pts',(44.0058696426795,-39.4310704471405,
2.71369962772052));
#239546=CARTESIAN_POINT('Ctrl Pts',(44.0085654321305,-39.4311389525604,
2.71561183138614));
#239547=CARTESIAN_POINT('Ctrl Pts',(44.0087720537699,-39.4311442032309,
2.71575839426265));
#239548=CARTESIAN_POINT('Ctrl Pts',(44.0089785427603,-39.4311497894106,
2.71590508903162));
#239549=CARTESIAN_POINT('Ctrl Pts',(44.0091848981962,-39.4311557099534,
2.71605191409865));
#239550=CARTESIAN_POINT('Ctrl Pts',(44.0120835699303,-39.4312388757292,
2.71811436362706));
#239551=CARTESIAN_POINT('Ctrl Pts',(44.0149559644988,-39.4313901062468,
2.72020091026913));
#239552=CARTESIAN_POINT('Ctrl Pts',(44.0177981990788,-39.4316052205099,
2.72230624862136));
#239553=CARTESIAN_POINT('Ctrl Pts',(44.0279899468077,-39.4323765820007,
2.72985561753024));
#239554=CARTESIAN_POINT('Ctrl Pts',(44.0378728316087,-39.4339733733557,
2.73770089914215));
#239555=CARTESIAN_POINT('Ctrl Pts',(44.0474262866313,-39.436268119214,2.7457482334692));
#239556=CARTESIAN_POINT('Ctrl Pts',(44.0579245739712,-39.4387898143846,
2.75459144546802));
#239557=CARTESIAN_POINT('Ctrl Pts',(44.0680257165073,-39.4421543412252,
2.76367911753975));
#239558=CARTESIAN_POINT('Ctrl Pts',(44.0777053474391,-39.4462454222039,
2.77292162564357));
#239559=CARTESIAN_POINT('Ctrl Pts',(44.0881569195892,-39.4506627629395,
2.78290121484227));
#239560=CARTESIAN_POINT('Ctrl Pts',(44.0981181930518,-39.4559274600901,
2.79306229499547));
#239561=CARTESIAN_POINT('Ctrl Pts',(44.107547242147,-39.4619494607953,2.80331916684474));
#239562=CARTESIAN_POINT('Ctrl Pts',(44.1168971912118,-39.4679209431042,
2.81348999408159));
#239563=CARTESIAN_POINT('Ctrl Pts',(44.1257248429274,-39.4746380711544,
2.82375635966594));
#239564=CARTESIAN_POINT('Ctrl Pts',(44.1339623850452,-39.4820551873923,
2.83404198860235));
#239565=CARTESIAN_POINT('Origin',(-0.0101975504409074,-0.0113255271400824,
2.83404198860262));
#239566=CARTESIAN_POINT('Ctrl Pts',(46.6938111422609,-42.0638038389693,
2.65878198860233));
#239567=CARTESIAN_POINT('Ctrl Pts',(46.6880613546461,-42.0701842568298,
2.65878198860233));
#239568=CARTESIAN_POINT('Ctrl Pts',(46.6818296739378,-42.0760276657216,
2.65944603041817));
#239569=CARTESIAN_POINT('Ctrl Pts',(46.6752630175681,-42.0812997491637,
2.66070439264027));
#239570=CARTESIAN_POINT('Ctrl Pts',(46.6710672367553,-42.0846683595042,
2.66150842619554));
#239571=CARTESIAN_POINT('Ctrl Pts',(46.6667352666015,-42.0878044626431,
2.66255428265332));
#239572=CARTESIAN_POINT('Ctrl Pts',(46.6623093164294,-42.090706774241,2.66381699700627));
#239573=CARTESIAN_POINT('Ctrl Pts',(46.6562687825188,-42.0946678472184,
2.66554034873227));
#239574=CARTESIAN_POINT('Ctrl Pts',(46.6500510792886,-42.0981877352858,
2.66766759643931));
#239575=CARTESIAN_POINT('Ctrl Pts',(46.6437515300392,-42.1012583942258,
2.67012012783107));
#239576=CARTESIAN_POINT('Ctrl Pts',(46.6406017554146,-42.1027937236959,
2.67134639352695));
#239577=CARTESIAN_POINT('Ctrl Pts',(46.6374313809743,-42.1042169023582,
2.67265375584971));
#239578=CARTESIAN_POINT('Ctrl Pts',(46.6342513293852,-42.1055280393683,
2.67403135126899));
#239579=CARTESIAN_POINT('Ctrl Pts',(46.6326613035906,-42.1061836078733,
2.67472014897863));
#239580=CARTESIAN_POINT('Ctrl Pts',(46.6310688468945,-42.10681117894,2.67542649668591));
#239581=CARTESIAN_POINT('Ctrl Pts',(46.6294752517399,-42.1074108478347,
2.6761489965606));
#239582=CARTESIAN_POINT('Ctrl Pts',(46.6290768529512,-42.1075607650584,
2.67632962152927));
#239583=CARTESIAN_POINT('Ctrl Pts',(46.6286783827623,-42.1077089386734,
2.67651125590908));
#239584=CARTESIAN_POINT('Ctrl Pts',(46.6282798608704,-42.1078553707275,
2.67669387767482));
#239585=CARTESIAN_POINT('Ctrl Pts',(46.6270842951947,-42.10829466689,2.67724174297202));
#239586=CARTESIAN_POINT('Ctrl Pts',(46.6258882654176,-42.1087182876158,
2.67779849504706));
#239587=CARTESIAN_POINT('Ctrl Pts',(46.6246922924071,-42.1091263005953,
2.67836353617967));
#239588=CARTESIAN_POINT('Ctrl Pts',(46.6164273768573,-42.1119459234378,
2.68226832098857));
#239589=CARTESIAN_POINT('Ctrl Pts',(46.6081492165695,-42.1140735600931,
2.68659153751328));
#239590=CARTESIAN_POINT('Ctrl Pts',(46.5999384432826,-42.1155964444641,
2.69123699486103));
#239591=CARTESIAN_POINT('Ctrl Pts',(46.5958577114969,-42.1163533138163,
2.69354577441151));
#239592=CARTESIAN_POINT('Ctrl Pts',(46.591793149742,-42.1169604217526,2.69593478828062));
#239593=CARTESIAN_POINT('Ctrl Pts',(46.5877524553609,-42.1174262136785,
2.69839565261175));
#239594=CARTESIAN_POINT('Ctrl Pts',(46.5788380800233,-42.1184538202393,
2.70382468689001));
#239595=CARTESIAN_POINT('Ctrl Pts',(46.5700422469563,-42.1188058546731,
2.70961155815042));
#239596=CARTESIAN_POINT('Ctrl Pts',(46.5615008914348,-42.1185337834646,
2.71562701361721));
#239597=CARTESIAN_POINT('Ctrl Pts',(46.5583806265506,-42.1184343924212,
2.71782453535811));
#239598=CARTESIAN_POINT('Ctrl Pts',(46.5552908961832,-42.1182588963856,
2.72005051502355));
#239599=CARTESIAN_POINT('Ctrl Pts',(46.5522345526332,-42.1180117795235,
2.72229986760067));
#239600=CARTESIAN_POINT('Ctrl Pts',(46.5419686180604,-42.1171817401327,
2.7298552048885));
#239601=CARTESIAN_POINT('Ctrl Pts',(46.5320149571602,-42.1155299964524,
2.73770845534523));
#239602=CARTESIAN_POINT('Ctrl Pts',(46.5223946380437,-42.1131831104076,
2.74576706701726));
#239603=CARTESIAN_POINT('Ctrl Pts',(46.5118207677331,-42.1106036046374,
2.75462443585012));
#239604=CARTESIAN_POINT('Ctrl Pts',(46.5016489045613,-42.1071843209722,
2.76373036323175));
#239605=CARTESIAN_POINT('Ctrl Pts',(46.4919044745642,-42.1030402839719,
2.77299664636825));
#239606=CARTESIAN_POINT('Ctrl Pts',(46.4814093059416,-42.0985769785647,
2.782976830335));
#239607=CARTESIAN_POINT('Ctrl Pts',(46.4714088200568,-42.0932726122921,
2.79314401478939));
#239608=CARTESIAN_POINT('Ctrl Pts',(46.4619468343607,-42.0872150940856,
2.80341452428007));
#239609=CARTESIAN_POINT('Ctrl Pts',(46.4526126174202,-42.0812393728283,
2.81354634721395));
#239610=CARTESIAN_POINT('Ctrl Pts',(46.4438014421029,-42.0745296860242,
2.823780042092));
#239611=CARTESIAN_POINT('Ctrl Pts',(46.4355828792675,-42.0671296588088,
2.83404198860233));
#239612=CARTESIAN_POINT('Ctrl Pts',(43.8790236240225,-39.7651933658992,
2.83404198860234));
#239613=CARTESIAN_POINT('Ctrl Pts',(43.8711584142724,-39.758111499231,2.82422126443014));
#239614=CARTESIAN_POINT('Ctrl Pts',(43.8638800583574,-39.750434738225,2.81442815028543));
#239615=CARTESIAN_POINT('Ctrl Pts',(43.8572218328541,-39.7422106539909,
2.80471618166395));
#239616=CARTESIAN_POINT('Ctrl Pts',(43.8507927303141,-39.734269577076,2.79533842146328));
#239617=CARTESIAN_POINT('Ctrl Pts',(43.844941079035,-39.72581716687,2.7860351565036));
#239618=CARTESIAN_POINT('Ctrl Pts',(43.8397310304462,-39.7168657021556,
2.77685887346896));
#239619=CARTESIAN_POINT('Ctrl Pts',(43.8348059028435,-39.7084037645753,
2.76818441216728));
#239620=CARTESIAN_POINT('Ctrl Pts',(43.8304536682217,-39.6994950821798,
2.75962261521785));
#239621=CARTESIAN_POINT('Ctrl Pts',(43.8267676847823,-39.6901349804742,
2.75123537701829));
#239622=CARTESIAN_POINT('Ctrl Pts',(43.8233729558715,-39.6815144838308,
2.74351087134292));
#239623=CARTESIAN_POINT('Ctrl Pts',(43.8205432023708,-39.6725105620432,
2.73593399450023));
#239624=CARTESIAN_POINT('Ctrl Pts',(43.818389241969,-39.6631152739638,2.72857657812754));
#239625=CARTESIAN_POINT('Ctrl Pts',(43.8177469744577,-39.6603137887146,
2.72638274508427));
#239626=CARTESIAN_POINT('Ctrl Pts',(43.8171650742233,-39.6574775031716,
2.72420861709632));
#239627=CARTESIAN_POINT('Ctrl Pts',(43.8166472411075,-39.6546062260514,
2.72205663736681));
#239628=CARTESIAN_POINT('Ctrl Pts',(43.81613469897,-39.6517642863079,2.71992664556719));
#239629=CARTESIAN_POINT('Ctrl Pts',(43.8156851836086,-39.6488910639683,
2.71782089927838));
#239630=CARTESIAN_POINT('Ctrl Pts',(43.8153025584996,-39.6459896850497,
2.71574387311199));
#239631=CARTESIAN_POINT('Ctrl Pts',(43.8152759514979,-39.6457879288339,
2.7155994407744));
#239632=CARTESIAN_POINT('Ctrl Pts',(43.815249656674,-39.6455860324529,2.71545515216022));
#239633=CARTESIAN_POINT('Ctrl Pts',(43.815223675331,-39.6453839959659,2.71531100781683));
#239634=CARTESIAN_POINT('Ctrl Pts',(43.8140845580787,-39.636525976255,2.70899119176047));
#239635=CARTESIAN_POINT('Ctrl Pts',(43.8135929685794,-39.6274037177899,
2.70298296066812));
#239636=CARTESIAN_POINT('Ctrl Pts',(43.8138323099903,-39.6180980992372,
2.69736727774118));
#239637=CARTESIAN_POINT('Ctrl Pts',(43.8140554177825,-39.6094236454406,
2.69213248525422));
#239638=CARTESIAN_POINT('Ctrl Pts',(43.814913952762,-39.6005890951404,2.68723866185471));
#239639=CARTESIAN_POINT('Ctrl Pts',(43.8164991115146,-39.5916773623198,
2.68278595829573));
#239640=CARTESIAN_POINT('Ctrl Pts',(43.8170789830939,-39.5884173351605,
2.68115710172796));
#239641=CARTESIAN_POINT('Ctrl Pts',(43.8177563121469,-39.5851472105415,
2.67958763637782));
#239642=CARTESIAN_POINT('Ctrl Pts',(43.8185363400632,-39.5818719865438,
2.6780837864532));
#239643=CARTESIAN_POINT('Ctrl Pts',(43.8187239107186,-39.581084404588,2.67772216078556));
#239644=CARTESIAN_POINT('Ctrl Pts',(43.8189178575375,-39.5802961412314,
2.67736403603519));
#239645=CARTESIAN_POINT('Ctrl Pts',(43.8191182115055,-39.5795073285701,
2.67700956934434));
#239646=CARTESIAN_POINT('Ctrl Pts',(43.819312304412,-39.5787431663045,2.67666617973759));
#239647=CARTESIAN_POINT('Ctrl Pts',(43.8195124102603,-39.5779784885473,
2.67632622314074));
#239648=CARTESIAN_POINT('Ctrl Pts',(43.8197185546683,-39.5772134181958,
2.67598984158729));
#239649=CARTESIAN_POINT('Ctrl Pts',(43.8219771048936,-39.5688311883222,
2.67230439292161));
#239650=CARTESIAN_POINT('Ctrl Pts',(43.8249623840161,-39.5603964284858,
2.66904964539902));
#239651=CARTESIAN_POINT('Ctrl Pts',(43.8286919494563,-39.55209682397,2.66640203566646));
#239652=CARTESIAN_POINT('Ctrl Pts',(43.8302387114105,-39.5486547305931,
2.66530399299374));
#239653=CARTESIAN_POINT('Ctrl Pts',(43.8319130705232,-39.5452359574119,
2.66430995142204));
#239654=CARTESIAN_POINT('Ctrl Pts',(43.8337144555754,-39.5418537500309,
2.66343053473314));
#239655=CARTESIAN_POINT('Ctrl Pts',(43.8367869054999,-39.5360850428912,
2.66193059792838));
#239656=CARTESIAN_POINT('Ctrl Pts',(43.8402296473868,-39.5304250803193,
2.6607651981708));
#239657=CARTESIAN_POINT('Ctrl Pts',(43.8440378929944,-39.5249464846897,
2.65997805604412));
#239658=CARTESIAN_POINT('Ctrl Pts',(43.8459420157982,-39.522207186875,2.65958448498078));
#239659=CARTESIAN_POINT('Ctrl Pts',(43.847938633807,-39.5195141476128,2.65928526260714));
#239660=CARTESIAN_POINT('Ctrl Pts',(43.8500271570784,-39.5168765098743,
2.65908463971276));
#239661=CARTESIAN_POINT('Ctrl Pts',(43.8521156803498,-39.5142388721359,
2.65888401681838));
#239662=CARTESIAN_POINT('Ctrl Pts',(43.8542960677578,-39.5116566557591,
2.65878198860235));
#239663=CARTESIAN_POINT('Ctrl Pts',(43.8565665267061,-39.5091373124615,
2.65878198860235));
#239664=CARTESIAN_POINT('Origin',(47.1453396605412,-34.2342565846629,2.83404198860238));
#239665=CARTESIAN_POINT('Ctrl Pts',(50.8023624960595,-36.674605926817,2.83404198860237));
#239666=CARTESIAN_POINT('Ctrl Pts',(50.8109464329605,-36.6808425220333,
2.82419652440019));
#239667=CARTESIAN_POINT('Ctrl Pts',(50.8190128116693,-36.6877379133664,
2.81438790575583));
#239668=CARTESIAN_POINT('Ctrl Pts',(50.8265243508966,-36.6952462569242,
2.80466781256817));
#239669=CARTESIAN_POINT('Ctrl Pts',(50.8337918098273,-36.7025106240256,
2.7952635645298));
#239670=CARTESIAN_POINT('Ctrl Pts',(50.8405407635291,-36.7103497152253,
2.78594102496122));
#239671=CARTESIAN_POINT('Ctrl Pts',(50.8467071440084,-36.7187568768225,
2.77675109088657));
#239672=CARTESIAN_POINT('Ctrl Pts',(50.8525401602379,-36.7267095340102,
2.7680579791355));
#239673=CARTESIAN_POINT('Ctrl Pts',(50.857852441276,-36.7351712462838,2.7594827121002));
#239674=CARTESIAN_POINT('Ctrl Pts',(50.8625525281348,-36.7441560526544,
2.75108575573074));
#239675=CARTESIAN_POINT('Ctrl Pts',(50.8668816480507,-36.7524317091195,
2.7433515516311));
#239676=CARTESIAN_POINT('Ctrl Pts',(50.8706916079206,-36.7611516658488,
2.73576818685773));
#239677=CARTESIAN_POINT('Ctrl Pts',(50.8738736606218,-36.7703354510192,
2.72840626160318));
#239678=CARTESIAN_POINT('Ctrl Pts',(50.8747966531511,-36.7729993179942,
2.72627084693553));
#239679=CARTESIAN_POINT('Ctrl Pts',(50.8756665488988,-36.775702242458,2.72415424587447));
#239680=CARTESIAN_POINT('Ctrl Pts',(50.8764799968257,-36.7784447603811,
2.72205867173233));
#239681=CARTESIAN_POINT('Ctrl Pts',(50.8773618266786,-36.7814178261386,
2.71978693462836));
#239682=CARTESIAN_POINT('Ctrl Pts',(50.8781771258728,-36.784432979124,2.71754411340736));
#239683=CARTESIAN_POINT('Ctrl Pts',(50.8789219044957,-36.7874899206167,
2.71533341844232));
#239684=CARTESIAN_POINT('Ctrl Pts',(50.8809659552707,-36.7958797205309,
2.70926614876379));
#239685=CARTESIAN_POINT('Ctrl Pts',(50.8824343655147,-36.8045837617096,
2.70347381860397));
#239686=CARTESIAN_POINT('Ctrl Pts',(50.8832604021666,-36.8135226609471,
2.69804914171382));
#239687=CARTESIAN_POINT('Ctrl Pts',(50.8840161808564,-36.8217012684451,
2.69308585687198));
#239688=CARTESIAN_POINT('Ctrl Pts',(50.8842246658558,-36.8300699399848,
2.68842799053184));
#239689=CARTESIAN_POINT('Ctrl Pts',(50.8838072802932,-36.8385876480139,
2.6841476705422));
#239690=CARTESIAN_POINT('Ctrl Pts',(50.8836022618683,-36.8427715183736,
2.68204519134548));
#239691=CARTESIAN_POINT('Ctrl Pts',(50.8832457706973,-36.846991141844,2.68003431778493));
#239692=CARTESIAN_POINT('Ctrl Pts',(50.8827256259729,-36.851239928621,2.67812693945238));
#239693=CARTESIAN_POINT('Ctrl Pts',(50.8826269335777,-36.8520460945281,
2.67776503299189));
#239694=CARTESIAN_POINT('Ctrl Pts',(50.8825219362263,-36.8528536453858,
2.6774065963991));
#239695=CARTESIAN_POINT('Ctrl Pts',(50.8824105850811,-36.8536624499706,
2.67705178968841));
#239696=CARTESIAN_POINT('Ctrl Pts',(50.8823027136591,-36.8544459794121,
2.67670807068744));
#239697=CARTESIAN_POINT('Ctrl Pts',(50.8821888793661,-36.855230685427,2.67636775825251));
#239698=CARTESIAN_POINT('Ctrl Pts',(50.8820690400779,-36.8560164456178,
2.67603099699241));
#239699=CARTESIAN_POINT('Ctrl Pts',(50.8807630562084,-36.8645794982668,
2.6723610421712));
#239700=CARTESIAN_POINT('Ctrl Pts',(50.8787426510002,-36.8732733195864,
2.6691144054147));
#239701=CARTESIAN_POINT('Ctrl Pts',(50.8759664620673,-36.8819119966098,
2.6664677818963));
#239702=CARTESIAN_POINT('Ctrl Pts',(50.8747940602416,-36.8855601635606,
2.66535009634968));
#239703=CARTESIAN_POINT('Ctrl Pts',(50.8734872887382,-36.889198371364,2.66433897912334));
#239704=CARTESIAN_POINT('Ctrl Pts',(50.8720449698708,-36.892812564861,2.66344564884779));
#239705=CARTESIAN_POINT('Ctrl Pts',(50.8696161409378,-36.8988987764009,
2.66194130298573));
#239706=CARTESIAN_POINT('Ctrl Pts',(50.8668019052541,-36.904914574214,2.66077206705407));
#239707=CARTESIAN_POINT('Ctrl Pts',(50.8635979627959,-36.9107858666114,
2.65998225155702));
#239708=CARTESIAN_POINT('Ctrl Pts',(50.8627969771814,-36.9122536897108,
2.65978479768276));
#239709=CARTESIAN_POINT('Ctrl Pts',(50.8619714372927,-36.9137123559378,
2.6596109896661));
#239710=CARTESIAN_POINT('Ctrl Pts',(50.8611210221666,-36.9151605322316,
2.65946139030489));
#239711=CARTESIAN_POINT('Ctrl Pts',(50.8598453994776,-36.9173327966724,
2.65923699126308));
#239712=CARTESIAN_POINT('Ctrl Pts',(50.8585138058065,-36.9194814382211,
2.65906707562429));
#239713=CARTESIAN_POINT('Ctrl Pts',(50.8571265262615,-36.9216029292225,
2.65895332562907));
#239714=CARTESIAN_POINT('Ctrl Pts',(50.8557392467166,-36.9237244202238,
2.65883957563385));
#239715=CARTESIAN_POINT('Ctrl Pts',(50.8542962928974,-36.9258187603122,
2.65878198860237));
#239716=CARTESIAN_POINT('Ctrl Pts',(50.8527980281389,-36.9278827595319,
2.65878198860237));
#239717=CARTESIAN_POINT('Ctrl Pts',(47.7640607692767,-34.6837837831338,
2.65878198860238));
#239718=CARTESIAN_POINT('Ctrl Pts',(47.7691302463544,-34.6767997090224,
2.65878198860238));
#239719=CARTESIAN_POINT('Ctrl Pts',(47.7747322888382,-34.6702946353242,
2.6594533551783));
#239720=CARTESIAN_POINT('Ctrl Pts',(47.7807252357991,-34.6643211616154,
2.66072561226574));
#239721=CARTESIAN_POINT('Ctrl Pts',(47.784596064624,-34.6604629105133,2.66154735980313));
#239722=CARTESIAN_POINT('Ctrl Pts',(47.7886293194338,-34.6568257642788,
2.66261895766859));
#239723=CARTESIAN_POINT('Ctrl Pts',(47.7927819897613,-34.6534164822756,
2.66391429251005));
#239724=CARTESIAN_POINT('Ctrl Pts',(47.7982861164007,-34.6488976742762,
2.66563118464101));
#239725=CARTESIAN_POINT('Ctrl Pts',(47.8040027249067,-34.6447843113767,
2.66774105138676));
#239726=CARTESIAN_POINT('Ctrl Pts',(47.8098436832082,-34.6410949611626,
2.67016894181727));
#239727=CARTESIAN_POINT('Ctrl Pts',(47.812764162359,-34.6392502860555,2.67138288703252));
#239728=CARTESIAN_POINT('Ctrl Pts',(47.815715844683,-34.6375114518659,2.67267613167528));
#239729=CARTESIAN_POINT('Ctrl Pts',(47.8186885387641,-34.6358796311037,
2.6740383543253));
#239730=CARTESIAN_POINT('Ctrl Pts',(47.8201748858046,-34.6350637207225,
2.67471946565031));
#239731=CARTESIAN_POINT('Ctrl Pts',(47.8216664954028,-34.6342745503765,
2.67541781389499));
#239732=CARTESIAN_POINT('Ctrl Pts',(47.8231621539169,-34.6335121829162,
2.67613207244145));
#239733=CARTESIAN_POINT('Ctrl Pts',(47.8235360685455,-34.6333215910511,
2.67631063707807));
#239734=CARTESIAN_POINT('Ctrl Pts',(47.823910236435,-34.6331326740824,2.67649019601822));
#239735=CARTESIAN_POINT('Ctrl Pts',(47.824284639033,-34.6329454324193,2.67667072836633));
#239736=CARTESIAN_POINT('Ctrl Pts',(47.8254078468268,-34.63238370743,2.67721232541067));
#239737=CARTESIAN_POINT('Ctrl Pts',(47.8265331659855,-34.6318370616122,
2.67776268340023));
#239738=CARTESIAN_POINT('Ctrl Pts',(47.827660104633,-34.6313054933178,2.67832123541492));
#239739=CARTESIAN_POINT('Ctrl Pts',(47.8355981149517,-34.6275611948897,
2.68225560368415));
#239740=CARTESIAN_POINT('Ctrl Pts',(47.8436253243399,-34.6245119115561,
2.68661792998852));
#239741=CARTESIAN_POINT('Ctrl Pts',(47.8516500154449,-34.6220808005804,
2.69130986622533));
#239742=CARTESIAN_POINT('Ctrl Pts',(47.8555419819595,-34.6209017143843,
2.69358545023017));
#239743=CARTESIAN_POINT('Ctrl Pts',(47.8594338479544,-34.6198683413507,
2.69593918853438));
#239744=CARTESIAN_POINT('Ctrl Pts',(47.8633173872852,-34.6189736992133,
2.69836306235451));
#239745=CARTESIAN_POINT('Ctrl Pts',(47.8692628146655,-34.6176040646078,
2.70207384382184));
#239746=CARTESIAN_POINT('Ctrl Pts',(47.8751852090117,-34.6165592825239,
2.70594760814184));
#239747=CARTESIAN_POINT('Ctrl Pts',(47.881043164166,-34.6158190596246,2.70995196345663));
#239748=CARTESIAN_POINT('Ctrl Pts',(47.8837636288447,-34.6154752962807,
2.71181160678061));
#239749=CARTESIAN_POINT('Ctrl Pts',(47.886470083205,-34.6151969889841,2.71369962772056));
#239750=CARTESIAN_POINT('Ctrl Pts',(47.8891582656056,-34.6149833323955,
2.71561183138618));
#239751=CARTESIAN_POINT('Ctrl Pts',(47.8893643041946,-34.6149669564598,
2.71575839426269));
#239752=CARTESIAN_POINT('Ctrl Pts',(47.8895702459314,-34.614950928061,2.71590508903166));
#239753=CARTESIAN_POINT('Ctrl Pts',(47.8897760897959,-34.6149352461538,
2.71605191409868));
#239754=CARTESIAN_POINT('Ctrl Pts',(47.8926675754936,-34.614714962637,2.7181143636271));
#239755=CARTESIAN_POINT('Ctrl Pts',(47.8955400426778,-34.6145651177078,
2.72020091026915));
#239756=CARTESIAN_POINT('Ctrl Pts',(47.8983891927627,-34.6144819591396,
2.72230624862138));
#239757=CARTESIAN_POINT('Ctrl Pts',(47.9086057382625,-34.6141837673033,
2.72985561753034));
#239758=CARTESIAN_POINT('Ctrl Pts',(47.9186013937331,-34.6147387685073,
2.73770089914233));
#239759=CARTESIAN_POINT('Ctrl Pts',(47.9283423801878,-34.6160223355353,
2.74574823346948));
#239760=CARTESIAN_POINT('Ctrl Pts',(47.9390467457327,-34.6174328467534,
2.75459144546866));
#239761=CARTESIAN_POINT('Ctrl Pts',(47.9494442419738,-34.6197230854575,
2.76367911754079));
#239762=CARTESIAN_POINT('Ctrl Pts',(47.9594984812827,-34.6227799581205,
2.77292162564502));
#239763=CARTESIAN_POINT('Ctrl Pts',(47.9703545364669,-34.6260806134262,
2.78290121484476));
#239764=CARTESIAN_POINT('Ctrl Pts',(47.980811551735,-34.6302752334083,2.79306229499904));
#239765=CARTESIAN_POINT('Ctrl Pts',(47.990818417993,-34.6352786409523,2.8033191668494));
#239766=CARTESIAN_POINT('Ctrl Pts',(48.000741336926,-34.6402400750484,2.81348999408475));
#239767=CARTESIAN_POINT('Ctrl Pts',(48.010222760913,-34.6459976650995,2.82375635966754));
#239768=CARTESIAN_POINT('Ctrl Pts',(48.019190476674,-34.6525130919789,2.83404198860238));
#239769=CARTESIAN_POINT('Origin',(-0.00895784724493606,-0.0123294189940815,
2.83404198860262));
#239770=CARTESIAN_POINT('Ctrl Pts',(50.8348823336491,-36.9525415975204,
2.65878198860237));
#239771=CARTESIAN_POINT('Ctrl Pts',(50.8298309792463,-36.9594880792479,
2.65878198860237));
#239772=CARTESIAN_POINT('Ctrl Pts',(50.8242442388885,-36.9659508653425,
2.65944603041822));
#239773=CARTESIAN_POINT('Ctrl Pts',(50.8182646381299,-36.971880470259,2.66070439264035));
#239774=CARTESIAN_POINT('Ctrl Pts',(50.8144439579057,-36.9756692055201,
2.66150842619561));
#239775=CARTESIAN_POINT('Ctrl Pts',(50.8104635307794,-36.9792409429409,
2.66255428265338));
#239776=CARTESIAN_POINT('Ctrl Pts',(50.8063652005968,-36.9825899931421,
2.66381699700631));
#239777=CARTESIAN_POINT('Ctrl Pts',(50.8007718022343,-36.9871607746743,
2.66554034873231));
#239778=CARTESIAN_POINT('Ctrl Pts',(50.7949560887234,-36.9913113073903,
2.66766759643936));
#239779=CARTESIAN_POINT('Ctrl Pts',(50.7890120203242,-36.9950236271417,
2.67012012783111));
#239780=CARTESIAN_POINT('Ctrl Pts',(50.7860399861246,-36.9968797870174,
2.67134639352699));
#239781=CARTESIAN_POINT('Ctrl Pts',(50.7830357420058,-36.9986265637263,
2.67265375584973));
#239782=CARTESIAN_POINT('Ctrl Pts',(50.7800101622088,-37.0002629240964,
2.67403135126901));
#239783=CARTESIAN_POINT('Ctrl Pts',(50.7784973723104,-37.0010811042814,
2.67472014897864));
#239784=CARTESIAN_POINT('Ctrl Pts',(50.7769792382978,-37.0018716944994,
2.67542649668593));
#239785=CARTESIAN_POINT('Ctrl Pts',(50.7754570554922,-37.0026346543977,
2.67614899656062));
#239786=CARTESIAN_POINT('Ctrl Pts',(50.7750765097909,-37.0028253943723,
2.67632962152929));
#239787=CARTESIAN_POINT('Ctrl Pts',(50.7746957108236,-37.0030144077533,
2.6765112559091));
#239788=CARTESIAN_POINT('Ctrl Pts',(50.7743146783939,-37.0032016945182,
2.67669387767484));
#239789=CARTESIAN_POINT('Ctrl Pts',(50.7731715811048,-37.0037635548132,
2.67724174297204));
#239790=CARTESIAN_POINT('Ctrl Pts',(50.7720263837274,-37.0043098740549,
2.67779849504707));
#239791=CARTESIAN_POINT('Ctrl Pts',(50.770879611352,-37.0048406651175,2.67836353617968));
#239792=CARTESIAN_POINT('Ctrl Pts',(50.7629547027166,-37.0085087606927,
2.68226832098876));
#239793=CARTESIAN_POINT('Ctrl Pts',(50.7549442896467,-37.0114900453054,
2.6865915375137));
#239794=CARTESIAN_POINT('Ctrl Pts',(50.7469376805977,-37.0138628466705,
2.6912369948617));
#239795=CARTESIAN_POINT('Ctrl Pts',(50.7429584178783,-37.0150421224356,
2.69354577441198));
#239796=CARTESIAN_POINT('Ctrl Pts',(50.738979582278,-37.0160707669651,2.69593478828088));
#239797=CARTESIAN_POINT('Ctrl Pts',(50.7350097117581,-37.0169563748082,
2.69839565261178));
#239798=CARTESIAN_POINT('Ctrl Pts',(50.7262515844359,-37.0189101579878,
2.70382468689004));
#239799=CARTESIAN_POINT('Ctrl Pts',(50.7175407334812,-37.0201796788538,
2.70961155815045));
#239800=CARTESIAN_POINT('Ctrl Pts',(50.7090177292136,-37.0208019128467,
2.71562701361724));
#239801=CARTESIAN_POINT('Ctrl Pts',(50.7059041682739,-37.0210292227711,
2.71782453535815));
#239802=CARTESIAN_POINT('Ctrl Pts',(50.7028130194419,-37.0211776528884,
2.72005051502358));
#239803=CARTESIAN_POINT('Ctrl Pts',(50.6997475881157,-37.0212513646528,
2.7222998676007));
#239804=CARTESIAN_POINT('Ctrl Pts',(50.6894511286644,-37.0214989546696,
2.72985520488877));
#239805=CARTESIAN_POINT('Ctrl Pts',(50.6793793407311,-37.0208967002918,
2.73770845534576));
#239806=CARTESIAN_POINT('Ctrl Pts',(50.6695664063374,-37.0195682679076,
2.74576706701804));
#239807=CARTESIAN_POINT('Ctrl Pts',(50.6587808290202,-37.0181081633542,
2.75462443585118));
#239808=CARTESIAN_POINT('Ctrl Pts',(50.6483072759119,-37.0157708601084,
2.76373036323309));
#239809=CARTESIAN_POINT('Ctrl Pts',(50.6381830571022,-37.0126680948693,
2.77299664636988));
#239810=CARTESIAN_POINT('Ctrl Pts',(50.6272788396558,-37.0093262837637,
2.78297683033696));
#239811=CARTESIAN_POINT('Ctrl Pts',(50.6167786802238,-37.0050963107858,
2.79314401479169));
#239812=CARTESIAN_POINT('Ctrl Pts',(50.6067353452058,-37.0000610231218,
2.80341452428271));
#239813=CARTESIAN_POINT('Ctrl Pts',(50.5968276291233,-36.9950937288437,
2.81354634721573));
#239814=CARTESIAN_POINT('Ctrl Pts',(50.5873633690966,-36.9893418170218,
2.82378004209291));
#239815=CARTESIAN_POINT('Ctrl Pts',(50.5784163149361,-36.9828414016739,
2.83404198860236));
#239816=CARTESIAN_POINT('Ctrl Pts',(47.7952442955506,-34.9607485668358,
2.83404198860238));
#239817=CARTESIAN_POINT('Ctrl Pts',(47.7866819156027,-34.9545276336627,
2.82422126443021));
#239818=CARTESIAN_POINT('Ctrl Pts',(47.7786409912522,-34.9476537221156,
2.81442815028553));
#239819=CARTESIAN_POINT('Ctrl Pts',(47.771159589318,-34.9401706643554,2.80471618166407));
#239820=CARTESIAN_POINT('Ctrl Pts',(47.7639356375079,-34.9329451136995,
2.79533842146349));
#239821=CARTESIAN_POINT('Ctrl Pts',(47.7572325247371,-34.9251506707969,
2.7860351565039));
#239822=CARTESIAN_POINT('Ctrl Pts',(47.751115334489,-34.9167928415154,2.77685887346935));
#239823=CARTESIAN_POINT('Ctrl Pts',(47.7453326739193,-34.9088920753345,
2.76818441216786));
#239824=CARTESIAN_POINT('Ctrl Pts',(47.7400730704137,-34.9004871280303,
2.75962261521862));
#239825=CARTESIAN_POINT('Ctrl Pts',(47.7354288821299,-34.891563592126,2.75123537701924));
#239826=CARTESIAN_POINT('Ctrl Pts',(47.7311516626327,-34.8833451652618,
2.74351087134415));
#239827=CARTESIAN_POINT('Ctrl Pts',(47.72739624471,-34.874686357685,2.73593399450172));
#239828=CARTESIAN_POINT('Ctrl Pts',(47.7242720089038,-34.8655676881479,
2.72857657812927));
#239829=CARTESIAN_POINT('Ctrl Pts',(47.7233404248529,-34.8628486849634,
2.72638274508542));
#239830=CARTESIAN_POINT('Ctrl Pts',(47.7224652397594,-34.8600887620259,
2.72420861709691));
#239831=CARTESIAN_POINT('Ctrl Pts',(47.7216501132023,-34.8572873423613,
2.72205663736684));
#239832=CARTESIAN_POINT('Ctrl Pts',(47.7208433152302,-34.8545145463031,
2.71992664556723));
#239833=CARTESIAN_POINT('Ctrl Pts',(47.7200959288452,-34.851704050926,2.71782089927842));
#239834=CARTESIAN_POINT('Ctrl Pts',(47.7194121231169,-34.8488585612793,
2.71574387311204));
#239835=CARTESIAN_POINT('Ctrl Pts',(47.7193645726039,-34.8486606914942,
2.71559944077444));
#239836=CARTESIAN_POINT('Ctrl Pts',(47.7193173179073,-34.8484626496803,
2.71545515216027));
#239837=CARTESIAN_POINT('Ctrl Pts',(47.7192703603294,-34.8482644357601,
2.71531100781688));
#239838=CARTESIAN_POINT('Ctrl Pts',(47.7172115680926,-34.8395740113841,
2.70899119176062));
#239839=CARTESIAN_POINT('Ctrl Pts',(47.7157691359132,-34.8305531107004,
2.70298296066836));
#239840=CARTESIAN_POINT('Ctrl Pts',(47.7150344641797,-34.8212734513101,
2.6973672777415));
#239841=CARTESIAN_POINT('Ctrl Pts',(47.714349622439,-34.8126231959648,2.69213248525475));
#239842=CARTESIAN_POINT('Ctrl Pts',(47.7142799923075,-34.8037473009138,
2.68723866185542));
#239843=CARTESIAN_POINT('Ctrl Pts',(47.7149249376576,-34.7947186932901,
2.68278595829657));
#239844=CARTESIAN_POINT('Ctrl Pts',(47.7151608670106,-34.7914159118149,
2.6811571017285));
#239845=CARTESIAN_POINT('Ctrl Pts',(47.7154926644832,-34.7880929011152,
2.67958763637807));
#239846=CARTESIAN_POINT('Ctrl Pts',(47.7159260651936,-34.7847540840173,
2.67808378645319));
#239847=CARTESIAN_POINT('Ctrl Pts',(47.7160302835858,-34.7839512100454,
2.67772216078554));
#239848=CARTESIAN_POINT('Ctrl Pts',(47.7161407719865,-34.7831469919151,
2.67736403603517));
#239849=CARTESIAN_POINT('Ctrl Pts',(47.7162575750191,-34.7823415577597,
2.67700956934433));
#239850=CARTESIAN_POINT('Ctrl Pts',(47.716370727957,-34.7815612934216,2.67666617973758));
#239851=CARTESIAN_POINT('Ctrl Pts',(47.7164898070138,-34.7807798878925,
2.67632622314073));
#239852=CARTESIAN_POINT('Ctrl Pts',(47.716614850513,-34.7799974607182,2.67598984158727));
#239853=CARTESIAN_POINT('Ctrl Pts',(47.7179848465564,-34.7714250667927,
2.67230439292165));
#239854=CARTESIAN_POINT('Ctrl Pts',(47.7200720995237,-34.7627244668144,
2.66904964539912));
#239855=CARTESIAN_POINT('Ctrl Pts',(47.7229136891083,-34.7540804826565,
2.66640203566659));
#239856=CARTESIAN_POINT('Ctrl Pts',(47.7240921810077,-34.7504955647771,
2.66530399299382));
#239857=CARTESIAN_POINT('Ctrl Pts',(47.7254000086991,-34.7469205018078,
2.66430995142208));
#239858=CARTESIAN_POINT('Ctrl Pts',(47.7268379886356,-34.7433685265014,
2.66343053473314));
#239859=CARTESIAN_POINT('Ctrl Pts',(47.7292906132656,-34.7373102624738,
2.66193059792838));
#239860=CARTESIAN_POINT('Ctrl Pts',(47.7321228682623,-34.7313214412503,
2.66076519817082));
#239861=CARTESIAN_POINT('Ctrl Pts',(47.7353375827199,-34.7254747878796,
2.65997805604414));
#239862=CARTESIAN_POINT('Ctrl Pts',(47.7369449399486,-34.7225514611942,
2.65958448498081));
#239863=CARTESIAN_POINT('Ctrl Pts',(47.7386491210195,-34.7196644712708,
2.65928526260716));
#239864=CARTESIAN_POINT('Ctrl Pts',(47.7404504949225,-34.7168229726598,
2.65908463971278));
#239865=CARTESIAN_POINT('Ctrl Pts',(47.7422518688255,-34.7139814740488,
2.65888401681841));
#239866=CARTESIAN_POINT('Ctrl Pts',(47.7441503967336,-34.7111854907786,
2.65878198860238));
#239867=CARTESIAN_POINT('Ctrl Pts',(47.7461450747869,-34.7084426211224,
2.65878198860238));
#239868=CARTESIAN_POINT('Origin',(50.4655267888879,-29.1186878401547,2.83404198860242));
#239869=CARTESIAN_POINT('Ctrl Pts',(54.3576020372442,-31.1634057161431,
2.8340419886024));
#239870=CARTESIAN_POINT('Ctrl Pts',(54.3667908521544,-31.1687108809051,
2.82419652440104));
#239871=CARTESIAN_POINT('Ctrl Pts',(54.3755338070561,-31.1747253323922,
2.81438790575739));
#239872=CARTESIAN_POINT('Ctrl Pts',(54.383789032899,-31.1814073748058,2.80466781257036));
#239873=CARTESIAN_POINT('Ctrl Pts',(54.3917760130587,-31.1878722906299,
2.79526356453248));
#239874=CARTESIAN_POINT('Ctrl Pts',(54.3993074034423,-31.1949629807083,
2.78594102496432));
#239875=CARTESIAN_POINT('Ctrl Pts',(54.406318791526,-31.2026795247186,2.77675109089004));
#239876=CARTESIAN_POINT('Ctrl Pts',(54.4129511329169,-31.209978900195,2.7680579791393));
#239877=CARTESIAN_POINT('Ctrl Pts',(54.4191188025039,-31.2178389737494,
2.75948271210427));
#239878=CARTESIAN_POINT('Ctrl Pts',(54.4247323097976,-31.2262832675534,
2.75108575573505));
#239879=CARTESIAN_POINT('Ctrl Pts',(54.4299027559943,-31.2340610728538,
2.74335155163568));
#239880=CARTESIAN_POINT('Ctrl Pts',(54.434603328182,-31.2423350114968,2.73576818686256));
#239881=CARTESIAN_POINT('Ctrl Pts',(54.4387279162163,-31.2511358718515,
2.72840626160824));
#239882=CARTESIAN_POINT('Ctrl Pts',(54.4399243024182,-31.2536886668956,
2.72627084693889));
#239883=CARTESIAN_POINT('Ctrl Pts',(54.4410719653274,-31.2562858555926,
2.72415424587617));
#239884=CARTESIAN_POINT('Ctrl Pts',(54.4421676282862,-31.2589283212559,
2.7220586717324));
#239885=CARTESIAN_POINT('Ctrl Pts',(54.4433553973777,-31.2617929239286,
2.71978693462842));
#239886=CARTESIAN_POINT('Ctrl Pts',(54.4444813995856,-31.2647063376186,
2.71754411340741));
#239887=CARTESIAN_POINT('Ctrl Pts',(54.4455416356299,-31.2676686823011,
2.71533341844237));
#239888=CARTESIAN_POINT('Ctrl Pts',(54.448451461773,-31.2757988605271,2.70926614876383));
#239889=CARTESIAN_POINT('Ctrl Pts',(54.4508216479607,-31.2843017293913,
2.703473818604));
#239890=CARTESIAN_POINT('Ctrl Pts',(54.4525775288979,-31.2931053160616,
2.69804914171385));
#239891=CARTESIAN_POINT('Ctrl Pts',(54.4541840646265,-31.3011601199073,
2.69308585687181));
#239892=CARTESIAN_POINT('Ctrl Pts',(54.455266171899,-31.3094611543724,2.6884279905315));
#239893=CARTESIAN_POINT('Ctrl Pts',(54.4557414157489,-31.3179758301775,
2.68414767054173));
#239894=CARTESIAN_POINT('Ctrl Pts',(54.4559748539755,-31.3221582111182,
2.68204519134519));
#239895=CARTESIAN_POINT('Ctrl Pts',(54.4560613864574,-31.3263919825236,
2.6800343177848));
#239896=CARTESIAN_POINT('Ctrl Pts',(54.4559882102927,-31.3306718639305,
2.67812693945239));
#239897=CARTESIAN_POINT('Ctrl Pts',(54.4559743258282,-31.3314839297409,
2.67776503299191));
#239898=CARTESIAN_POINT('Ctrl Pts',(54.4559543157135,-31.3322980319622,
2.67740659639912));
#239899=CARTESIAN_POINT('Ctrl Pts',(54.4559281176618,-31.333114045195,2.67705178968843));
#239900=CARTESIAN_POINT('Ctrl Pts',(54.4559027382993,-31.3339045580142,
2.67670807068745));
#239901=CARTESIAN_POINT('Ctrl Pts',(54.4558715517163,-31.3346968642512,
2.67636775825253));
#239902=CARTESIAN_POINT('Ctrl Pts',(54.4558345032255,-31.335490846582,2.67603099699243));
#239903=CARTESIAN_POINT('Ctrl Pts',(54.4554307564065,-31.3441435024193,
2.67236104217133));
#239904=CARTESIAN_POINT('Ctrl Pts',(54.454330170972,-31.3530008879274,2.66911440541493));
#239905=CARTESIAN_POINT('Ctrl Pts',(54.4524721779265,-31.3618824321368,
2.66646778189657));
#239906=CARTESIAN_POINT('Ctrl Pts',(54.4516875359257,-31.3656331634087,
2.66535009634985));
#239907=CARTESIAN_POINT('Ctrl Pts',(54.4507682193241,-31.3693880355465,
2.66433897912343));
#239908=CARTESIAN_POINT('Ctrl Pts',(54.4497115877225,-31.3731331934884,
2.66344564884782));
#239909=CARTESIAN_POINT('Ctrl Pts',(54.4479322465079,-31.3794399458806,
2.66194130298575));
#239910=CARTESIAN_POINT('Ctrl Pts',(54.4457622496024,-31.3857169562551,
2.6607720670541));
#239911=CARTESIAN_POINT('Ctrl Pts',(54.4431895758475,-31.3918909882798,
2.65998225155705));
#239912=CARTESIAN_POINT('Ctrl Pts',(54.4425464074088,-31.393434496286,2.65978479768278));
#239913=CARTESIAN_POINT('Ctrl Pts',(54.4418778620531,-31.3949714642027,
2.65961098966613));
#239914=CARTESIAN_POINT('Ctrl Pts',(54.4411834812327,-31.3965005998215,
2.65946139030492));
#239915=CARTESIAN_POINT('Ctrl Pts',(54.4401419100021,-31.3987943032499,
2.65923699126311));
#239916=CARTESIAN_POINT('Ctrl Pts',(54.4390422051397,-31.4010703637555,
2.65906707562433));
#239917=CARTESIAN_POINT('Ctrl Pts',(54.4378842814515,-31.4033252432062,
2.65895332562911));
#239918=CARTESIAN_POINT('Ctrl Pts',(54.4367263577634,-31.4055801226569,
2.65883957563389));
#239919=CARTESIAN_POINT('Ctrl Pts',(54.435510226749,-31.4078138194774,2.65878198860241));
#239920=CARTESIAN_POINT('Ctrl Pts',(54.4342359163082,-31.4100231232061,
2.65878198860241));
#239921=CARTESIAN_POINT('Ctrl Pts',(51.1278468659051,-29.5010785149103,
2.65878198860242));
#239922=CARTESIAN_POINT('Ctrl Pts',(51.1321585373228,-29.4936027956388,
2.65878198860242));
#239923=CARTESIAN_POINT('Ctrl Pts',(51.1370499258748,-29.4865477845228,
2.65945335517838));
#239924=CARTESIAN_POINT('Ctrl Pts',(51.1423856448182,-29.4799806005916,
2.6607256122659));
#239925=CARTESIAN_POINT('Ctrl Pts',(51.145831971779,-29.4757388736043,2.66154735980328));
#239926=CARTESIAN_POINT('Ctrl Pts',(51.1494629466903,-29.4717000621104,
2.66261895766869));
#239927=CARTESIAN_POINT('Ctrl Pts',(51.1532365012464,-29.4678753842631,
2.66391429251009));
#239928=CARTESIAN_POINT('Ctrl Pts',(51.1582381316481,-29.4628059928675,
2.66563118464105));
#239929=CARTESIAN_POINT('Ctrl Pts',(51.1634934604719,-29.4581176150981,
2.6677410513868));
#239930=CARTESIAN_POINT('Ctrl Pts',(51.1689167792843,-29.4538379291352,
2.6701689418173));
#239931=CARTESIAN_POINT('Ctrl Pts',(51.1716284386905,-29.4516980861538,
2.67138288703256));
#239932=CARTESIAN_POINT('Ctrl Pts',(51.1743821937243,-29.4496602426625,
2.67267613167532));
#239933=CARTESIAN_POINT('Ctrl Pts',(51.1771680313595,-29.447726630041,2.67403835432533));
#239934=CARTESIAN_POINT('Ctrl Pts',(51.1785609501771,-29.4467598237303,
2.67471946565034));
#239935=CARTESIAN_POINT('Ctrl Pts',(51.1799618978184,-29.4458190608829,
2.67541781389503));
#239936=CARTESIAN_POINT('Ctrl Pts',(51.1813696738596,-29.4449045308652,
2.67613207244149));
#239937=CARTESIAN_POINT('Ctrl Pts',(51.1817216178699,-29.4446758983608,
2.67631063707811));
#239938=CARTESIAN_POINT('Ctrl Pts',(51.1820739888281,-29.4444489051046,
2.67649019601825));
#239939=CARTESIAN_POINT('Ctrl Pts',(51.1824267683262,-29.4442235534427,
2.67667072836637));
#239940=CARTESIAN_POINT('Ctrl Pts',(51.1834851068202,-29.443547498457,2.6772123254107));
#239941=CARTESIAN_POINT('Ctrl Pts',(51.1845471213156,-29.4428862193398,
2.67776268340027));
#239942=CARTESIAN_POINT('Ctrl Pts',(51.1856123224583,-29.4422397658671,
2.67832123541496));
#239943=CARTESIAN_POINT('Ctrl Pts',(51.1931154617654,-29.4376862310775,
2.68225560368428));
#239944=CARTESIAN_POINT('Ctrl Pts',(51.20077996036,-29.4338145801753,2.68661792998877));
#239945=CARTESIAN_POINT('Ctrl Pts',(51.2085065710734,-29.4305579784505,
2.69130986622573));
#239946=CARTESIAN_POINT('Ctrl Pts',(51.2122539689199,-29.4289785301331,
2.69358545023045));
#239947=CARTESIAN_POINT('Ctrl Pts',(51.2160164979702,-29.4275440072535,
2.69593918853455));
#239948=CARTESIAN_POINT('Ctrl Pts',(51.2197852472983,-29.4262483256611,
2.69836306235455));
#239949=CARTESIAN_POINT('Ctrl Pts',(51.2255549392047,-29.4242647276697,
2.70207384382188));
#239950=CARTESIAN_POINT('Ctrl Pts',(51.2313356805893,-29.4226066102315,
2.70594760814189));
#239951=CARTESIAN_POINT('Ctrl Pts',(51.2370841708902,-29.4212581193005,
2.70995196345668));
#239952=CARTESIAN_POINT('Ctrl Pts',(51.2397537995246,-29.420631873136,2.71181160678066));
#239953=CARTESIAN_POINT('Ctrl Pts',(51.2424163366108,-29.4200721889207,
2.71369962772059));
#239954=CARTESIAN_POINT('Ctrl Pts',(51.245067459672,-29.4195787111899,2.71561183138621));
#239955=CARTESIAN_POINT('Ctrl Pts',(51.2452706578087,-29.4195408880663,
2.71575839426272));
#239956=CARTESIAN_POINT('Ctrl Pts',(51.2454737959512,-29.4195034206994,
2.7159050890317));
#239957=CARTESIAN_POINT('Ctrl Pts',(51.2456768729759,-29.4194663081565,
2.71605191409872));
#239958=CARTESIAN_POINT('Ctrl Pts',(51.2485294929149,-29.4189449888193,
2.71811436362714));
#239959=CARTESIAN_POINT('Ctrl Pts',(51.2513705613631,-29.4184957101758,
2.7202009102692));
#239960=CARTESIAN_POINT('Ctrl Pts',(51.2541954110684,-29.4181151898789,
2.72230624862143));
#239961=CARTESIAN_POINT('Ctrl Pts',(51.2643248197287,-29.4167507117677,
2.72985561753046));
#239962=CARTESIAN_POINT('Ctrl Pts',(51.2743237313758,-29.4162578421113,
2.73770089914254));
#239963=CARTESIAN_POINT('Ctrl Pts',(51.2841455249765,-29.4165161672801,
2.74574823346978));
#239964=CARTESIAN_POINT('Ctrl Pts',(51.2949386894568,-29.4168000406894,
2.75459144546882));
#239965=CARTESIAN_POINT('Ctrl Pts',(51.3055186222576,-29.4179908989224,
2.7636791175408));
#239966=CARTESIAN_POINT('Ctrl Pts',(51.3158373135934,-29.4199800715328,
2.77292162564486));
#239967=CARTESIAN_POINT('Ctrl Pts',(51.3269789105976,-29.4221278787377,
2.78290121484403));
#239968=CARTESIAN_POINT('Ctrl Pts',(51.337817098422,-29.4252064644161,2.79306229499769));
#239969=CARTESIAN_POINT('Ctrl Pts',(51.3482921445208,-29.4291364604176,
2.80331916684744));
#239970=CARTESIAN_POINT('Ctrl Pts',(51.358679315748,-29.4330334877915,2.81348999408344));
#239971=CARTESIAN_POINT('Ctrl Pts',(51.3687106315432,-29.4377684584832,
2.8237563596669));
#239972=CARTESIAN_POINT('Ctrl Pts',(51.3783102687789,-29.4433108116253,
2.83404198860242));
#239973=CARTESIAN_POINT('Origin',(-0.00761999999999908,-0.0131982271534827,
2.83404198860262));
#239974=CARTESIAN_POINT('Ctrl Pts',(54.4189959163067,-31.4364195775126,
2.65878198860241));
#239975=CARTESIAN_POINT('Ctrl Pts',(54.4146983388121,-31.4438560159993,
2.65878198860241));
#239976=CARTESIAN_POINT('Ctrl Pts',(54.4098177483016,-31.4508673716596,
2.65944603041822));
#239977=CARTESIAN_POINT('Ctrl Pts',(54.4044907169114,-31.457389532058,2.66070439264029));
#239978=CARTESIAN_POINT('Ctrl Pts',(54.4010869974477,-31.4615568820637,
2.66150842619556));
#239979=CARTESIAN_POINT('Ctrl Pts',(54.3975017237414,-31.4655251210639,
2.66255428265336));
#239980=CARTESIAN_POINT('Ctrl Pts',(54.3937759157111,-31.4692842169739,
2.66381699700634));
#239981=CARTESIAN_POINT('Ctrl Pts',(54.3886909353395,-31.4744146286218,
2.66554034873233));
#239982=CARTESIAN_POINT('Ctrl Pts',(54.3833409297224,-31.4791503318814,
2.66766759643937));
#239983=CARTESIAN_POINT('Ctrl Pts',(54.3778174666306,-31.4834636394921,
2.67012012783112));
#239984=CARTESIAN_POINT('Ctrl Pts',(54.3750557350847,-31.4856202932974,
2.671346393527));
#239985=CARTESIAN_POINT('Ctrl Pts',(54.3722505364145,-31.4876715300018,
2.67265375584976));
#239986=CARTESIAN_POINT('Ctrl Pts',(54.3694125772951,-31.4896151854252,
2.67403135126903));
#239987=CARTESIAN_POINT('Ctrl Pts',(54.3679935977354,-31.4905870131369,
2.67472014897867));
#239988=CARTESIAN_POINT('Ctrl Pts',(54.3665664194003,-31.4915319606344,
2.67542649668595));
#239989=CARTESIAN_POINT('Ctrl Pts',(54.3651323262972,-31.492449852388,2.67614899656064));
#239990=CARTESIAN_POINT('Ctrl Pts',(54.3647738030214,-31.4926793253264,
2.67632962152931));
#239991=CARTESIAN_POINT('Ctrl Pts',(54.3644148473889,-31.4929071076032,
2.67651125590913));
#239992=CARTESIAN_POINT('Ctrl Pts',(54.3640554790925,-31.493133197126,2.67669387767486));
#239993=CARTESIAN_POINT('Ctrl Pts',(54.3629773742032,-31.4938114656944,
2.67724174297206));
#239994=CARTESIAN_POINT('Ctrl Pts',(54.3618955562477,-31.4944744978642,
2.67779849504709));
#239995=CARTESIAN_POINT('Ctrl Pts',(54.3608105487854,-31.495122251552,2.67836353617971));
#239996=CARTESIAN_POINT('Ctrl Pts',(54.3533124740225,-31.4995986314368,
2.68226832098868));
#239997=CARTESIAN_POINT('Ctrl Pts',(54.3456575719328,-31.5034009004288,
2.6865915375135));
#239998=CARTESIAN_POINT('Ctrl Pts',(54.3379428492065,-31.5065976218795,
2.69123699486135));
#239999=CARTESIAN_POINT('Ctrl Pts',(54.3341086531879,-31.5081863836657,
2.69354577441175));
#240000=CARTESIAN_POINT('Ctrl Pts',(54.330259136697,-31.5096252947438,2.69593478828078));
#240001=CARTESIAN_POINT('Ctrl Pts',(54.3264035847699,-31.5109210155993,
2.69839565261182));
#240002=CARTESIAN_POINT('Ctrl Pts',(54.3178976613389,-31.5137795693404,
2.70382468689008));
#240003=CARTESIAN_POINT('Ctrl Pts',(54.3093672304023,-31.5159526675022,
2.70961155815049));
#240004=CARTESIAN_POINT('Ctrl Pts',(54.300955957207,-31.5174623893708,2.71562701361729));
#240005=CARTESIAN_POINT('Ctrl Pts',(54.2978832130371,-31.518013909808,2.7178245353582));
#240006=CARTESIAN_POINT('Ctrl Pts',(54.2948245130138,-31.5184846398467,
2.72005051502364));
#240007=CARTESIAN_POINT('Ctrl Pts',(54.2917835794187,-31.5188783726362,
2.72229986760077));
#240008=CARTESIAN_POINT('Ctrl Pts',(54.2815694052538,-31.5202008794124,
2.72985520488861));
#240009=CARTESIAN_POINT('Ctrl Pts',(54.2714898389045,-31.5206547127622,
2.73770845534536));
#240010=CARTESIAN_POINT('Ctrl Pts',(54.2615918017967,-31.520359288622,2.74576706701739));
#240011=CARTESIAN_POINT('Ctrl Pts',(54.2507126865157,-31.5200345824966,
2.75462443585027));
#240012=CARTESIAN_POINT('Ctrl Pts',(54.2400521939111,-31.518804867654,2.76373036323191));
#240013=CARTESIAN_POINT('Ctrl Pts',(54.2296591093493,-31.5167773687216,
2.77299664636842));
#240014=CARTESIAN_POINT('Ctrl Pts',(54.2184653119679,-31.5145936654999,
2.78297683033519));
#240015=CARTESIAN_POINT('Ctrl Pts',(54.2075805209331,-31.5114844302862,
2.7931440147896));
#240016=CARTESIAN_POINT('Ctrl Pts',(54.1970658734737,-31.5075265408307,
2.80341452428028));
#240017=CARTESIAN_POINT('Ctrl Pts',(54.1866932092582,-31.5036220962467,
2.81354634721413));
#240018=CARTESIAN_POINT('Ctrl Pts',(54.1766795569337,-31.4988909785559,
2.82378004209214));
#240019=CARTESIAN_POINT('Ctrl Pts',(54.1671020372442,-31.493361394985,2.83404198860241));
#240020=CARTESIAN_POINT('Ctrl Pts',(51.1878102687789,-29.7732664904671,
2.83404198860241));
#240021=CARTESIAN_POINT('Ctrl Pts',(51.1786445298598,-29.7679746486349,
2.82422126443058));
#240022=CARTESIAN_POINT('Ctrl Pts',(51.1699291351239,-29.7619788985604,
2.81442815028624));
#240023=CARTESIAN_POINT('Ctrl Pts',(51.1617065245643,-29.7553188532211,
2.80471618166512));
#240024=CARTESIAN_POINT('Ctrl Pts',(51.1537668706119,-29.7488879934693,
2.79533842146471));
#240025=CARTESIAN_POINT('Ctrl Pts',(51.1462857370556,-29.7418369154176,
2.78603515650528));
#240026=CARTESIAN_POINT('Ctrl Pts',(51.1393284263648,-29.7341642916958,
2.77685887347088));
#240027=CARTESIAN_POINT('Ctrl Pts',(51.1327515888671,-29.7269112593617,
2.76818441216939));
#240028=CARTESIAN_POINT('Ctrl Pts',(51.1266422417943,-29.7191021335102,
2.75962261522015));
#240029=CARTESIAN_POINT('Ctrl Pts',(51.1210907313648,-29.7107129315338,
2.75123537702076));
#240030=CARTESIAN_POINT('Ctrl Pts',(51.1159778833928,-29.7029866172529,
2.74351087134555));
#240031=CARTESIAN_POINT('Ctrl Pts',(51.1113379461926,-29.6947677915945,
2.73593399450301));
#240032=CARTESIAN_POINT('Ctrl Pts',(51.1072776647632,-29.6860256466508,
2.72857657813045));
#240033=CARTESIAN_POINT('Ctrl Pts',(51.1060669708024,-29.6834189154991,
2.72638274508621));
#240034=CARTESIAN_POINT('Ctrl Pts',(51.1049080895609,-29.6807655934606,
2.72420861709731));
#240035=CARTESIAN_POINT('Ctrl Pts',(51.1038046002597,-29.678064724192,2.72205663736687));
#240036=CARTESIAN_POINT('Ctrl Pts',(51.1027123859004,-29.6753914511529,
2.71992664556726));
#240037=CARTESIAN_POINT('Ctrl Pts',(51.1016753170134,-29.6726744751138,
2.71782089927846));
#240038=CARTESIAN_POINT('Ctrl Pts',(51.1006978225844,-29.6699160505192,
2.71574387311207));
#240039=CARTESIAN_POINT('Ctrl Pts',(51.1006298495335,-29.6697242350675,
2.71559944077448));
#240040=CARTESIAN_POINT('Ctrl Pts',(51.1005621526966,-29.6695322176081,
2.7154551521603));
#240041=CARTESIAN_POINT('Ctrl Pts',(51.1004947333607,-29.669339997928,2.71531100781691));
#240042=CARTESIAN_POINT('Ctrl Pts',(51.097538822698,-29.6609123829944,2.70899119176043));
#240043=CARTESIAN_POINT('Ctrl Pts',(51.0951613514272,-29.6520916749673,
2.70298296066797));
#240044=CARTESIAN_POINT('Ctrl Pts',(51.0934607157665,-29.642939644629,2.69736727774094));
#240045=CARTESIAN_POINT('Ctrl Pts',(51.0918754277624,-29.6344083617416,
2.69213248525382));
#240046=CARTESIAN_POINT('Ctrl Pts',(51.0908783954022,-29.6255883681023,
2.68723866185417));
#240047=CARTESIAN_POINT('Ctrl Pts',(51.090576061194,-29.6165418049887,2.68278595829508));
#240048=CARTESIAN_POINT('Ctrl Pts',(51.0904654634293,-29.6132324551644,
2.68115710172757));
#240049=CARTESIAN_POINT('Ctrl Pts',(51.0904480940788,-29.6098929659862,
2.67958763637767));
#240050=CARTESIAN_POINT('Ctrl Pts',(51.0905301191544,-29.6065271365684,
2.67808378645327));
#240051=CARTESIAN_POINT('Ctrl Pts',(51.0905498434448,-29.6057177670358,
2.67772216078562));
#240052=CARTESIAN_POINT('Ctrl Pts',(51.0905756628932,-29.6049064053138,
2.67736403603526));
#240053=CARTESIAN_POINT('Ctrl Pts',(51.0906076352721,-29.6040931741695,
2.67700956934442));
#240054=CARTESIAN_POINT('Ctrl Pts',(51.0906386085141,-29.6033053564984,
2.67666617973766));
#240055=CARTESIAN_POINT('Ctrl Pts',(51.0906753561242,-29.6025157844397,
2.67632622314081));
#240056=CARTESIAN_POINT('Ctrl Pts',(51.0907179287119,-29.6017245728785,
2.67598984158736));
#240057=CARTESIAN_POINT('Ctrl Pts',(51.09118436061,-29.5930559358433,2.67230439292193));
#240058=CARTESIAN_POINT('Ctrl Pts',(51.0923507190419,-29.5841848213173,
2.66904964539953));
#240059=CARTESIAN_POINT('Ctrl Pts',(51.0942731997207,-29.575291162817,2.66640203566706));
#240060=CARTESIAN_POINT('Ctrl Pts',(51.0950705097613,-29.5716026975451,
2.66530399299413));
#240061=CARTESIAN_POINT('Ctrl Pts',(51.0959974771977,-29.5679105139257,
2.66430995142226));
#240062=CARTESIAN_POINT('Ctrl Pts',(51.0970562972094,-29.5642276868782,
2.66343053473321));
#240063=CARTESIAN_POINT('Ctrl Pts',(51.0988622250761,-29.5579462415713,
2.66193059792844));
#240064=CARTESIAN_POINT('Ctrl Pts',(51.1010529624044,-29.5516941764747,
2.66076519817087));
#240065=CARTESIAN_POINT('Ctrl Pts',(51.1036389246282,-29.545543522521,2.65997805604419));
#240066=CARTESIAN_POINT('Ctrl Pts',(51.1049319057401,-29.5424681955442,
2.65958448498084));
#240067=CARTESIAN_POINT('Ctrl Pts',(51.1063249785084,-29.5394188854251,
2.6592852626072));
#240068=CARTESIAN_POINT('Ctrl Pts',(51.1078194668134,-29.5364046579949,
2.65908463971282));
#240069=CARTESIAN_POINT('Ctrl Pts',(51.1093139551183,-29.5333904305647,
2.65888401681845));
#240070=CARTESIAN_POINT('Ctrl Pts',(51.110909822857,-29.5304113137785,2.65878198860242));
#240071=CARTESIAN_POINT('Ctrl Pts',(51.1126068659051,-29.5274749692176,
2.65878198860242));
#240072=CARTESIAN_POINT('Origin',(53.2328030451451,-23.6840886581928,2.83404198860246));
#240073=CARTESIAN_POINT('Ctrl Pts',(57.3172883154493,-25.3107727110814,
2.83404198860245));
#240074=CARTESIAN_POINT('Ctrl Pts',(57.3269813337899,-25.3150883208938,
2.8241965244006));
#240075=CARTESIAN_POINT('Ctrl Pts',(57.3363050752412,-25.3201559369462,
2.81438790575656));
#240076=CARTESIAN_POINT('Ctrl Pts',(57.3452135417183,-25.3259384683611,
2.8046678125692));
#240077=CARTESIAN_POINT('Ctrl Pts',(57.3538325360813,-25.3315331019378,
2.79526356453103));
#240078=CARTESIAN_POINT('Ctrl Pts',(57.3620638476579,-25.3377977038112,
2.78594102496265));
#240079=CARTESIAN_POINT('Ctrl Pts',(57.3698434251114,-25.3447390861645,
2.77675109088818));
#240080=CARTESIAN_POINT('Ctrl Pts',(57.3772024263436,-25.3513052064451,
2.76805797913728));
#240081=CARTESIAN_POINT('Ctrl Pts',(57.3841579102014,-25.3584775246706,
2.75948271210214));
#240082=CARTESIAN_POINT('Ctrl Pts',(57.3906233351696,-25.366288788459,2.75108575573282));
#240083=CARTESIAN_POINT('Ctrl Pts',(57.3965784591568,-25.3734835273331,
2.74335155163333));
#240084=CARTESIAN_POINT('Ctrl Pts',(57.4021181432099,-25.3812207968876,
2.73576818686011));
#240085=CARTESIAN_POINT('Ctrl Pts',(57.4071400767279,-25.3895423083599,
2.72840626160569));
#240086=CARTESIAN_POINT('Ctrl Pts',(57.4085967487434,-25.3919560625136,
2.72627084693721));
#240087=CARTESIAN_POINT('Ctrl Pts',(57.4100096047779,-25.3944190600981,
2.72415424587533));
#240088=CARTESIAN_POINT('Ctrl Pts',(57.4113754784549,-25.3969325220916,
2.72205867173239));
#240089=CARTESIAN_POINT('Ctrl Pts',(57.4128561733383,-25.3996572764934,
2.71978693462842));
#240090=CARTESIAN_POINT('Ctrl Pts',(57.4142805418443,-25.4024370309179,
2.71754411340743));
#240091=CARTESIAN_POINT('Ctrl Pts',(57.4156446191419,-25.4052723227218,
2.71533341844241));
#240092=CARTESIAN_POINT('Ctrl Pts',(57.419388339989,-25.4130538033258,2.70926614876388));
#240093=CARTESIAN_POINT('Ctrl Pts',(57.4226343338645,-25.4212623406648,
2.70347381860405));
#240094=CARTESIAN_POINT('Ctrl Pts',(57.4253008212881,-25.4298341608302,
2.69804914171392));
#240095=CARTESIAN_POINT('Ctrl Pts',(57.4277405125136,-25.4376769109061,
2.69308585687228));
#240096=CARTESIAN_POINT('Ctrl Pts',(57.4296843862653,-25.445819360425,2.68842799053232));
#240097=CARTESIAN_POINT('Ctrl Pts',(57.4310470526568,-25.454237715435,2.68414767054283));
#240098=CARTESIAN_POINT('Ctrl Pts',(57.4317163899371,-25.4583727839168,
2.68204519134593));
#240099=CARTESIAN_POINT('Ctrl Pts',(57.432244998004,-25.4625743171729,2.68003431778521));
#240100=CARTESIAN_POINT('Ctrl Pts',(57.4326195921325,-25.4668384019343,
2.67812693945251));
#240101=CARTESIAN_POINT('Ctrl Pts',(57.4326906677197,-25.4676474704849,
2.67776503299203));
#240102=CARTESIAN_POINT('Ctrl Pts',(57.4327558640766,-25.4684592045957,
2.67740659639923));
#240103=CARTESIAN_POINT('Ctrl Pts',(57.4328151061498,-25.4692734860646,
2.67705178968855));
#240104=CARTESIAN_POINT('Ctrl Pts',(57.4328724969083,-25.4700623212376,
2.67670807068757));
#240105=CARTESIAN_POINT('Ctrl Pts',(57.4329242997221,-25.4708535470238,
2.67636775825265));
#240106=CARTESIAN_POINT('Ctrl Pts',(57.4329704479397,-25.4716470524582,
2.67603099699254));
#240107=CARTESIAN_POINT('Ctrl Pts',(57.433473361706,-25.4802945111768,2.6723610421711));
#240108=CARTESIAN_POINT('Ctrl Pts',(57.4333046542892,-25.4892184175053,
2.66911440541443));
#240109=CARTESIAN_POINT('Ctrl Pts',(57.4323852136915,-25.4982455208449,
2.66646778189593));
#240110=CARTESIAN_POINT('Ctrl Pts',(57.4319969282177,-25.5020577226402,
2.6653500963495));
#240111=CARTESIAN_POINT('Ctrl Pts',(57.431475138743,-25.5058881199463,2.66433897912333));
#240112=CARTESIAN_POINT('Ctrl Pts',(57.4308157710843,-25.5097232095978,
2.66344564884791));
#240113=CARTESIAN_POINT('Ctrl Pts',(57.4297054124229,-25.5161814047433,
2.66194130298583));
#240114=CARTESIAN_POINT('Ctrl Pts',(57.4282034292359,-25.5226508554401,
2.66077206705417));
#240115=CARTESIAN_POINT('Ctrl Pts',(57.4262902109374,-25.5290599831057,
2.65998225155711));
#240116=CARTESIAN_POINT('Ctrl Pts',(57.4258119063628,-25.5306622650221,
2.65978479768285));
#240117=CARTESIAN_POINT('Ctrl Pts',(57.425307680263,-25.5322606952863,2.65961098966619));
#240118=CARTESIAN_POINT('Ctrl Pts',(57.4247769415296,-25.5338540367004,
2.65946139030498));
#240119=CARTESIAN_POINT('Ctrl Pts',(57.4239808334296,-25.5362440488214,
2.65923699126317));
#240120=CARTESIAN_POINT('Ctrl Pts',(57.4231250659724,-25.5386225912887,
2.65906707562438));
#240121=CARTESIAN_POINT('Ctrl Pts',(57.422209184595,-25.5409861542575,2.65895332562915));
#240122=CARTESIAN_POINT('Ctrl Pts',(57.4212933032177,-25.5433497172263,
2.65883957563393));
#240123=CARTESIAN_POINT('Ctrl Pts',(57.4203173191904,-25.5456982979271,
2.65878198860245));
#240124=CARTESIAN_POINT('Ctrl Pts',(57.4192809246792,-25.548028700571,2.65878198860245));
#240125=CARTESIAN_POINT('Ctrl Pts',(53.9314655730807,-23.9951532569799,
2.65878198860246));
#240126=CARTESIAN_POINT('Ctrl Pts',(53.9349721992641,-23.9872677980933,
2.65878198860246));
#240127=CARTESIAN_POINT('Ctrl Pts',(53.9390993428075,-23.9797401457377,
2.65945335517843));
#240128=CARTESIAN_POINT('Ctrl Pts',(53.9437193744799,-23.9726512030256,
2.66072561226598));
#240129=CARTESIAN_POINT('Ctrl Pts',(53.9467034408975,-23.9680724734015,
2.66154735980335));
#240130=CARTESIAN_POINT('Ctrl Pts',(53.9498923541893,-23.9636762467119,
2.66261895766876));
#240131=CARTESIAN_POINT('Ctrl Pts',(53.9532454491209,-23.9594780769913,
2.66391429251014));
#240132=CARTESIAN_POINT('Ctrl Pts',(53.9576897843756,-23.9539136435124,
2.66563118464111));
#240133=CARTESIAN_POINT('Ctrl Pts',(53.9624262550348,-23.9487016177212,
2.66774105138686));
#240134=CARTESIAN_POINT('Ctrl Pts',(53.9673725153423,-23.9438784851445,
2.67016894181736));
#240135=CARTESIAN_POINT('Ctrl Pts',(53.9698456454961,-23.9414669188561,
2.67138288703262));
#240136=CARTESIAN_POINT('Ctrl Pts',(53.9723713025231,-23.9391523931028,
2.67267613167538));
#240137=CARTESIAN_POINT('Ctrl Pts',(53.9749397614924,-23.9369381736867,
2.67403835432539));
#240138=CARTESIAN_POINT('Ctrl Pts',(53.9762239909771,-23.9358310639786,
2.6747194656504));
#240139=CARTESIAN_POINT('Ctrl Pts',(53.9775189275858,-23.9347490158245,
2.67541781389509));
#240140=CARTESIAN_POINT('Ctrl Pts',(53.9788233972652,-23.9336923430317,
2.67613207244155));
#240141=CARTESIAN_POINT('Ctrl Pts',(53.979149514685,-23.9334281748335,2.67631063707816));
#240142=CARTESIAN_POINT('Ctrl Pts',(53.9794762280621,-23.9331655922753,
2.67649019601831));
#240143=CARTESIAN_POINT('Ctrl Pts',(53.9798035193342,-23.9329045996146,
2.67667072836642));
#240144=CARTESIAN_POINT('Ctrl Pts',(53.9807853931505,-23.9321216216325,
2.67721232541076));
#240145=CARTESIAN_POINT('Ctrl Pts',(53.9817724673294,-23.9313529543284,
2.67776268340033));
#240146=CARTESIAN_POINT('Ctrl Pts',(53.9827642604008,-23.9305986983569,
2.67832123541502));
#240147=CARTESIAN_POINT('Ctrl Pts',(53.9897503227318,-23.9252858166858,
2.68225560368437));
#240148=CARTESIAN_POINT('Ctrl Pts',(53.996968136682,-23.9206342168325,2.6866179299889));
#240149=CARTESIAN_POINT('Ctrl Pts',(54.0043120126398,-23.9165878043685,
2.6913098662259));
#240150=CARTESIAN_POINT('Ctrl Pts',(54.0078737845432,-23.9146252986961,
2.69358545023058));
#240151=CARTESIAN_POINT('Ctrl Pts',(54.0114657535936,-23.9128053429034,
2.69593918853464));
#240152=CARTESIAN_POINT('Ctrl Pts',(54.0150784217127,-23.9111228176146,
2.6983630623546));
#240153=CARTESIAN_POINT('Ctrl Pts',(54.0206091641934,-23.9085469889521,
2.70207384382192));
#240154=CARTESIAN_POINT('Ctrl Pts',(54.0261849176042,-23.9062937028413,
2.70594760814192));
#240155=CARTESIAN_POINT('Ctrl Pts',(54.0317609613889,-23.9043517182274,
2.70995196345672));
#240156=CARTESIAN_POINT('Ctrl Pts',(54.0343505049692,-23.9034498505262,
2.7118116067807));
#240157=CARTESIAN_POINT('Ctrl Pts',(54.0369399534677,-23.9026149214096,
2.71369962772063));
#240158=CARTESIAN_POINT('Ctrl Pts',(54.0395249709305,-23.901847029182,2.71561183138625));
#240159=CARTESIAN_POINT('Ctrl Pts',(54.0397231023336,-23.9017881732684,
2.71575839426276));
#240160=CARTESIAN_POINT('Ctrl Pts',(54.0399212112578,-23.9017296774338,
2.71590508903173));
#240161=CARTESIAN_POINT('Ctrl Pts',(54.0401192964882,-23.901671540868,2.71605191409876));
#240162=CARTESIAN_POINT('Ctrl Pts',(54.0429017967675,-23.9008548973942,
2.71811436362717));
#240163=CARTESIAN_POINT('Ctrl Pts',(54.0456803391393,-23.9001111074271,
2.72020091026924));
#240164=CARTESIAN_POINT('Ctrl Pts',(54.0484499388205,-23.8994373944616,
2.72230624862147));
#240165=CARTESIAN_POINT('Ctrl Pts',(54.0583812307202,-23.8970215795832,
2.72985561753049));
#240166=CARTESIAN_POINT('Ctrl Pts',(54.0682738483753,-23.8954862390495,
2.73770089914257));
#240167=CARTESIAN_POINT('Ctrl Pts',(54.0780688394959,-23.8947164920943,
2.74574823346979));
#240168=CARTESIAN_POINT('Ctrl Pts',(54.0888325507431,-23.8938706175186,
2.75459144546888));
#240169=CARTESIAN_POINT('Ctrl Pts',(54.0994790041462,-23.8939490479884,
2.7636791175409));
#240170=CARTESIAN_POINT('Ctrl Pts',(54.1099490937673,-23.8948487267548,
2.77292162564502));
#240171=CARTESIAN_POINT('Ctrl Pts',(54.121254162924,-23.8958201540339,2.78290121484429));
#240172=CARTESIAN_POINT('Ctrl Pts',(54.1323547778516,-23.89774897578,2.79306229499807));
#240173=CARTESIAN_POINT('Ctrl Pts',(54.1431832369946,-23.9005625023809,
2.80331916684792));
#240174=CARTESIAN_POINT('Ctrl Pts',(54.1539208564936,-23.903352426385,2.81348999408378));
#240175=CARTESIAN_POINT('Ctrl Pts',(54.1643921589012,-23.9070129003871,
2.82375635966709));
#240176=CARTESIAN_POINT('Ctrl Pts',(54.1745185419763,-23.9115214566106,
2.83404198860246));
#240177=CARTESIAN_POINT('Origin',(-0.00619866644047451,-0.0139224327742815,
2.83404198860262));
#240178=CARTESIAN_POINT('Ctrl Pts',(57.4068835917983,-25.5758735661199,
2.65878198860245));
#240179=CARTESIAN_POINT('Ctrl Pts',(57.4033868763699,-25.5837184861902,
2.65878198860245));
#240180=CARTESIAN_POINT('Ctrl Pts',(57.3992659084772,-25.5912015935368,
2.65944603041834));
#240181=CARTESIAN_POINT('Ctrl Pts',(57.3946498105256,-25.5982448512635,
2.66070439264055));
#240182=CARTESIAN_POINT('Ctrl Pts',(57.3917003436855,-25.6027451576543,
2.66150842619579));
#240183=CARTESIAN_POINT('Ctrl Pts',(57.3885495044085,-25.6070664213766,
2.66255428265351));
#240184=CARTESIAN_POINT('Ctrl Pts',(57.3852370392635,-25.6111943775533,
2.66381699700637));
#240185=CARTESIAN_POINT('Ctrl Pts',(57.380716188992,-25.6168282094534,2.66554034873237));
#240186=CARTESIAN_POINT('Ctrl Pts',(57.3758905070496,-25.6220971979007,
2.66766759643942));
#240187=CARTESIAN_POINT('Ctrl Pts',(57.3708481654826,-25.6269642358699,
2.67012012783117));
#240188=CARTESIAN_POINT('Ctrl Pts',(57.3683269946992,-25.6293977548545,
2.67134639352705));
#240189=CARTESIAN_POINT('Ctrl Pts',(57.3657515758214,-25.6317309777758,
2.67265375584981));
#240190=CARTESIAN_POINT('Ctrl Pts',(57.3631323306535,-25.6339606331569,
2.67403135126909));
#240191=CARTESIAN_POINT('Ctrl Pts',(57.3618227080695,-25.6350754608475,
2.67472014897872));
#240192=CARTESIAN_POINT('Ctrl Pts',(57.3605021218765,-25.6361644125819,
2.67542649668601));
#240193=CARTESIAN_POINT('Ctrl Pts',(57.3591718306998,-25.6372271795767,
2.67614899656071));
#240194=CARTESIAN_POINT('Ctrl Pts',(57.3588392579057,-25.6374928713254,
2.67632962152938));
#240195=CARTESIAN_POINT('Ctrl Pts',(57.3585060784011,-25.6377569268677,
2.67651125590919));
#240196=CARTESIAN_POINT('Ctrl Pts',(57.3581723115521,-25.6380193420642,
2.67669387767493));
#240197=CARTESIAN_POINT('Ctrl Pts',(57.3571710110054,-25.6388065876538,
2.67724174297213));
#240198=CARTESIAN_POINT('Ctrl Pts',(57.3561644250956,-25.6395790684324,
2.67779849504716));
#240199=CARTESIAN_POINT('Ctrl Pts',(57.3551530701153,-25.6403366878204,
2.67836353617978));
#240200=CARTESIAN_POINT('Ctrl Pts',(57.3481639797008,-25.6455723078603,
2.68226832098882));
#240201=CARTESIAN_POINT('Ctrl Pts',(57.3409484573002,-25.6501539027769,
2.68659153751371));
#240202=CARTESIAN_POINT('Ctrl Pts',(57.3336101450128,-25.6541395203642,
2.69123699486164));
#240203=CARTESIAN_POINT('Ctrl Pts',(57.3299630239493,-25.6561203613647,
2.69354577441197));
#240204=CARTESIAN_POINT('Ctrl Pts',(57.3262850026764,-25.6579537739804,
2.69593478828091));
#240205=CARTESIAN_POINT('Ctrl Pts',(57.3225860115762,-25.6596454116595,
2.69839565261187));
#240206=CARTESIAN_POINT('Ctrl Pts',(57.3144254847134,-25.6633774170489,
2.70382468689012));
#240207=CARTESIAN_POINT('Ctrl Pts',(57.3061689349815,-25.6664302835885,
2.70961155815053));
#240208=CARTESIAN_POINT('Ctrl Pts',(57.2979615485277,-25.668810952504,2.71562701361733));
#240209=CARTESIAN_POINT('Ctrl Pts',(57.2949632867555,-25.6696806408806,
2.71782453535824));
#240210=CARTESIAN_POINT('Ctrl Pts',(57.2919705472986,-25.6704685134239,
2.72005051502368));
#240211=CARTESIAN_POINT('Ctrl Pts',(57.2889874285393,-25.6711779534196,
2.72229986760081));
#240212=CARTESIAN_POINT('Ctrl Pts',(57.2789674482908,-25.6735608872942,
2.72985520488827));
#240213=CARTESIAN_POINT('Ctrl Pts',(57.2689905373637,-25.6750658360783,
2.7377084553446));
#240214=CARTESIAN_POINT('Ctrl Pts',(57.259115842508,-25.6758066569107,2.7457670670162));
#240215=CARTESIAN_POINT('Ctrl Pts',(57.248262383127,-25.6766209067615,2.75462443584864));
#240216=CARTESIAN_POINT('Ctrl Pts',(57.237531749614,-25.6765122533353,2.76373036322983));
#240217=CARTESIAN_POINT('Ctrl Pts',(57.2269836681097,-25.6755822344122,
2.77299664636587));
#240218=CARTESIAN_POINT('Ctrl Pts',(57.2156229323801,-25.6745805641838,
2.78297683033213));
#240219=CARTESIAN_POINT('Ctrl Pts',(57.2044727657911,-25.6726261321662,
2.79314401478602));
#240220=CARTESIAN_POINT('Ctrl Pts',(57.1936020065686,-25.6697890043843,
2.80341452427617));
#240221=CARTESIAN_POINT('Ctrl Pts',(57.1828780392991,-25.6669901874066,
2.81354634721137));
#240222=CARTESIAN_POINT('Ctrl Pts',(57.1724247063465,-25.6633316989623,
2.82378004209078));
#240223=CARTESIAN_POINT('Ctrl Pts',(57.1623216544374,-25.6588335304432,
2.83404198860244));
#240224=CARTESIAN_POINT('Ctrl Pts',(54.0195518809644,-24.2595822759724,
2.83404198860245));
#240225=CARTESIAN_POINT('Ctrl Pts',(54.0098832048281,-24.2552775040076,
2.82422126443109));
#240226=CARTESIAN_POINT('Ctrl Pts',(54.0005888273954,-24.2502256060981,
2.81442815028723));
#240227=CARTESIAN_POINT('Ctrl Pts',(53.9917150968526,-24.2444615420302,
2.80471618166656));
#240228=CARTESIAN_POINT('Ctrl Pts',(53.9831467292681,-24.2388958310277,
2.79533842146638));
#240229=CARTESIAN_POINT('Ctrl Pts',(53.9749695397912,-24.2326653709137,
2.78603515650717));
#240230=CARTESIAN_POINT('Ctrl Pts',(53.9672483344096,-24.2257620156227,
2.77685887347298));
#240231=CARTESIAN_POINT('Ctrl Pts',(53.9599493771919,-24.2192361828756,
2.76818441217154));
#240232=CARTESIAN_POINT('Ctrl Pts',(53.9530572218368,-24.2121084368938,
2.75962261522233));
#240233=CARTESIAN_POINT('Ctrl Pts',(53.9466592127717,-24.2043454826978,
2.75123537702297));
#240234=CARTESIAN_POINT('Ctrl Pts',(53.9407667537572,-24.1971959321165,
2.74351087134767));
#240235=CARTESIAN_POINT('Ctrl Pts',(53.9352931334024,-24.1895071355501,
2.73593399450503));
#240236=CARTESIAN_POINT('Ctrl Pts',(53.9303412916427,-24.1812372959695,
2.72857657813237));
#240237=CARTESIAN_POINT('Ctrl Pts',(53.9288647523883,-24.1787713967423,
2.72638274508749));
#240238=CARTESIAN_POINT('Ctrl Pts',(53.9274348719438,-24.1762537459541,
2.72420861709797));
#240239=CARTESIAN_POINT('Ctrl Pts',(53.9260551099579,-24.1736830183701,
2.72205663736691));
#240240=CARTESIAN_POINT('Ctrl Pts',(53.9246894457405,-24.171138557289,2.7199266455673));
#240241=CARTESIAN_POINT('Ctrl Pts',(53.9233740566952,-24.168544868346,2.71782089927849));
#240242=CARTESIAN_POINT('Ctrl Pts',(53.9221135831991,-24.1659037306804,
2.7157438731121));
#240243=CARTESIAN_POINT('Ctrl Pts',(53.9220259323373,-24.1657200711324,
2.71559944077451));
#240244=CARTESIAN_POINT('Ctrl Pts',(53.9219385350609,-24.1655361818111,
2.71545515216033));
#240245=CARTESIAN_POINT('Ctrl Pts',(53.9218513926274,-24.1653520623701,
2.71531100781694));
#240246=CARTESIAN_POINT('Ctrl Pts',(53.9180307491145,-24.1572795915921,
2.70899119176053));
#240247=CARTESIAN_POINT('Ctrl Pts',(53.9147442868251,-24.148755717745,2.70298296066814));
#240248=CARTESIAN_POINT('Ctrl Pts',(53.9120963197576,-24.1398315880188,
2.69736727774116));
#240249=CARTESIAN_POINT('Ctrl Pts',(53.9096279542371,-24.1315127481109,
2.6921324852542));
#240250=CARTESIAN_POINT('Ctrl Pts',(53.9077144433434,-24.1228452895803,
2.68723866185469));
#240251=CARTESIAN_POINT('Ctrl Pts',(53.9064681420135,-24.1138798870165,
2.6827859582957));
#240252=CARTESIAN_POINT('Ctrl Pts',(53.9060122288633,-24.1106002267708,
2.68115710172797));
#240253=CARTESIAN_POINT('Ctrl Pts',(53.9056458829919,-24.1072808472548,
2.67958763637787));
#240254=CARTESIAN_POINT('Ctrl Pts',(53.9053756337489,-24.1039248822473,
2.67808378645328));
#240255=CARTESIAN_POINT('Ctrl Pts',(53.9053106478341,-24.1031178847759,
2.67772216078563));
#240256=CARTESIAN_POINT('Ctrl Pts',(53.9052515154469,-24.102308268911,2.67736403603527));
#240257=CARTESIAN_POINT('Ctrl Pts',(53.9051983068759,-24.1014961507084,
2.67700956934443));
#240258=CARTESIAN_POINT('Ctrl Pts',(53.9051467610728,-24.1007094111996,
2.67666617973767));
#240259=CARTESIAN_POINT('Ctrl Pts',(53.9051007746217,-24.099920323328,2.67632622314082));
#240260=CARTESIAN_POINT('Ctrl Pts',(53.9050604098637,-24.0991289960593,
2.67598984158737));
#240261=CARTESIAN_POINT('Ctrl Pts',(53.9046181672912,-24.0904590913151,
2.67230439292184));
#240262=CARTESIAN_POINT('Ctrl Pts',(53.9048508523207,-24.0815146560279,
2.66904964539938));
#240263=CARTESIAN_POINT('Ctrl Pts',(53.9058331609934,-24.0724687639682,
2.66640203566687));
#240264=CARTESIAN_POINT('Ctrl Pts',(53.9062405536795,-24.0687171629019,
2.66530399299402));
#240265=CARTESIAN_POINT('Ctrl Pts',(53.9067765048114,-24.0649483109693,
2.66430995142222));
#240266=CARTESIAN_POINT('Ctrl Pts',(53.9074445642445,-24.0611749820052,
2.66343053473323));
#240267=CARTESIAN_POINT('Ctrl Pts',(53.9085840092244,-24.0547391762483,
2.66193059792847));
#240268=CARTESIAN_POINT('Ctrl Pts',(53.9101092267075,-24.0482923662121,
2.6607651981709));
#240269=CARTESIAN_POINT('Ctrl Pts',(53.9120381043535,-24.0419050995269,
2.65997805604422));
#240270=CARTESIAN_POINT('Ctrl Pts',(53.9130025431765,-24.0387114661843,
2.65958448498088));
#240271=CARTESIAN_POINT('Ctrl Pts',(53.9140692448457,-24.0355332447494,
2.65928526260724));
#240272=CARTESIAN_POINT('Ctrl Pts',(53.9152404736262,-24.0323793130066,
2.65908463971286));
#240273=CARTESIAN_POINT('Ctrl Pts',(53.9164117024067,-24.0292253812638,
2.65888401681848));
#240274=CARTESIAN_POINT('Ctrl Pts',(53.9176874253156,-24.0260957707889,
2.65878198860246));
#240275=CARTESIAN_POINT('Ctrl Pts',(53.9190682401998,-24.0229981225288,
2.65878198860246));
#240276=CARTESIAN_POINT('Origin',(55.4168495715594,-17.9900016446774,2.8340419886025));
#240277=CARTESIAN_POINT('Ctrl Pts',(59.6489943884567,-19.1808295835772,
2.83404198860249));
#240278=CARTESIAN_POINT('Ctrl Pts',(59.6590854114903,-19.184108355716,2.82419652440052));
#240279=CARTESIAN_POINT('Ctrl Pts',(59.6688877866288,-19.1881736144716,
2.81438790575639));
#240280=CARTESIAN_POINT('Ctrl Pts',(59.678351890717,-19.1929932802635,2.80466781256897));
#240281=CARTESIAN_POINT('Ctrl Pts',(59.6875084677774,-19.1976563356163,
2.79526356453078));
#240282=CARTESIAN_POINT('Ctrl Pts',(59.6963495165747,-19.2030262129955,
2.78594102496239));
#240283=CARTESIAN_POINT('Ctrl Pts',(59.7048120487193,-19.2091163824539,
2.77675109088793));
#240284=CARTESIAN_POINT('Ctrl Pts',(59.7128170830354,-19.2148773077506,
2.76805797913705));
#240285=CARTESIAN_POINT('Ctrl Pts',(59.720484175427,-19.2212832892275,2.75948271210193));
#240286=CARTESIAN_POINT('Ctrl Pts',(59.7277306815208,-19.2283759411593,
2.75108575573264));
#240287=CARTESIAN_POINT('Ctrl Pts',(59.7344052377139,-19.2349087865421,
2.74335155163319));
#240288=CARTESIAN_POINT('Ctrl Pts',(59.7407233396945,-19.2420246158633,
2.73576818686));
#240289=CARTESIAN_POINT('Ctrl Pts',(59.7465875973415,-19.2497756062319,
2.72840626160561));
#240290=CARTESIAN_POINT('Ctrl Pts',(59.7482885955677,-19.2520238739005,
2.72627084693717));
#240291=CARTESIAN_POINT('Ctrl Pts',(59.7499511651815,-19.2543256952563,
2.72415424587534));
#240292=CARTESIAN_POINT('Ctrl Pts',(59.7515722847792,-19.2566826155655,
2.72205867173244));
#240293=CARTESIAN_POINT('Ctrl Pts',(59.7533296826515,-19.2592376687169,
2.71978693462847));
#240294=CARTESIAN_POINT('Ctrl Pts',(59.755036811776,-19.2618533083047,2.71754411340748));
#240295=CARTESIAN_POINT('Ctrl Pts',(59.7566897852107,-19.2645304831798,
2.71533341844245));
#240296=CARTESIAN_POINT('Ctrl Pts',(59.7612263837727,-19.2718780106318,
2.70926614876392));
#240297=CARTESIAN_POINT('Ctrl Pts',(59.7653126215479,-19.2797022819928,
2.7034738186041));
#240298=CARTESIAN_POINT('Ctrl Pts',(59.7688605008636,-19.2879484209977,
2.69804914171396));
#240299=CARTESIAN_POINT('Ctrl Pts',(59.7721066178187,-19.2954931904938,
2.69308585687204));
#240300=CARTESIAN_POINT('Ctrl Pts',(59.7748909605622,-19.3033878446867,
2.68842799053184));
#240301=CARTESIAN_POINT('Ctrl Pts',(59.7771261198371,-19.3116176456438,
2.68414767054215));
#240302=CARTESIAN_POINT('Ctrl Pts',(59.7782240227715,-19.3156600969901,
2.68204519134551));
#240303=CARTESIAN_POINT('Ctrl Pts',(59.7791889148826,-19.319783359218,2.68003431778503));
#240304=CARTESIAN_POINT('Ctrl Pts',(59.7800071751725,-19.3239849291278,
2.67812693945254));
#240305=CARTESIAN_POINT('Ctrl Pts',(59.7801624320925,-19.3247821360944,
2.67776503299206));
#240306=CARTESIAN_POINT('Ctrl Pts',(59.7803121206161,-19.3255826085658,
2.67740659639927));
#240307=CARTESIAN_POINT('Ctrl Pts',(59.7804561537457,-19.3263862368327,
2.67705178968858));
#240308=CARTESIAN_POINT('Ctrl Pts',(59.78059568584,-19.3271647517164,2.6767080706876));
#240309=CARTESIAN_POINT('Ctrl Pts',(59.780729910488,-19.3279462282163,2.67636775825268));
#240310=CARTESIAN_POINT('Ctrl Pts',(59.7808587498045,-19.3287305629427,
2.67603099699257));
#240311=CARTESIAN_POINT('Ctrl Pts',(59.7822628141275,-19.337278081174,2.67236104217133));
#240312=CARTESIAN_POINT('Ctrl Pts',(59.7830278331225,-19.3461707361365,
2.6691144054148));
#240313=CARTESIAN_POINT('Ctrl Pts',(59.7830570185565,-19.3552444957717,
2.66646778189637));
#240314=CARTESIAN_POINT('Ctrl Pts',(59.7830693437465,-19.3590764008111,
2.66535009634979));
#240315=CARTESIAN_POINT('Ctrl Pts',(59.7829507982333,-19.3629403566523,
2.66433897912347));
#240316=CARTESIAN_POINT('Ctrl Pts',(59.7826959186874,-19.3668233599701,
2.66344564884794));
#240317=CARTESIAN_POINT('Ctrl Pts',(59.7822667079009,-19.3733622405313,
2.66194130298587));
#240318=CARTESIAN_POINT('Ctrl Pts',(59.7814491944745,-19.3799532508947,
2.66077206705421));
#240319=CARTESIAN_POINT('Ctrl Pts',(59.7802163932513,-19.3865272544568,
2.65998225155715));
#240320=CARTESIAN_POINT('Ctrl Pts',(59.7799081929455,-19.3881707553474,
2.65978479768288));
#240321=CARTESIAN_POINT('Ctrl Pts',(59.7795738105081,-19.3898131352228,
2.65961098966623));
#240322=CARTESIAN_POINT('Ctrl Pts',(59.7792125287466,-19.39145322545,2.65946139030502));
#240323=CARTESIAN_POINT('Ctrl Pts',(59.7786706061044,-19.3939133607909,
2.6592369912632));
#240324=CARTESIAN_POINT('Ctrl Pts',(59.7780681520198,-19.3963683254109,
2.65906707562442));
#240325=CARTESIAN_POINT('Ctrl Pts',(59.7774043475416,-19.3988146762074,
2.65895332562919));
#240326=CARTESIAN_POINT('Ctrl Pts',(59.7767405430633,-19.4012610270039,
2.65883957563397));
#240327=CARTESIAN_POINT('Ctrl Pts',(59.7760153991104,-19.4036987600445,
2.65878198860249));
#240328=CARTESIAN_POINT('Ctrl Pts',(59.7752282754839,-19.4061247292244,
2.65878198860249));
#240329=CARTESIAN_POINT('Ctrl Pts',(56.144199857553,-18.2263320786573,2.6587819886025));
#240330=CARTESIAN_POINT('Ctrl Pts',(56.1468630191715,-18.2181232748938,
2.6587819886025));
#240331=CARTESIAN_POINT('Ctrl Pts',(56.1501806998578,-18.2102054558336,
2.6594533551784));
#240332=CARTESIAN_POINT('Ctrl Pts',(56.1540344262252,-18.2026724222807,
2.66072561226582));
#240333=CARTESIAN_POINT('Ctrl Pts',(56.1565235380435,-18.1978068555392,
2.66154735980322));
#240334=CARTESIAN_POINT('Ctrl Pts',(56.1592354513148,-18.1931013796332,
2.66261895766869));
#240335=CARTESIAN_POINT('Ctrl Pts',(56.1621313494123,-18.1885757140648,
2.66391429251018));
#240336=CARTESIAN_POINT('Ctrl Pts',(56.165969696453,-18.1825772036004,2.66563118464114));
#240337=CARTESIAN_POINT('Ctrl Pts',(56.1701354151839,-18.1768986338324,
2.6677410513869));
#240338=CARTESIAN_POINT('Ctrl Pts',(56.1745504247235,-18.1715848978918,
2.6701689418174));
#240339=CARTESIAN_POINT('Ctrl Pts',(56.1767579294934,-18.1689280299214,
2.67138288703266));
#240340=CARTESIAN_POINT('Ctrl Pts',(56.1790278168867,-18.1663621803345,
2.67267613167542));
#240341=CARTESIAN_POINT('Ctrl Pts',(56.1813507566161,-18.163891613575,2.67403835432543));
#240342=CARTESIAN_POINT('Ctrl Pts',(56.1825122264809,-18.1626563301953,
2.67471946565044));
#240343=CARTESIAN_POINT('Ctrl Pts',(56.1836869644606,-18.1614448518804,
2.67541781389513));
#240344=CARTESIAN_POINT('Ctrl Pts',(56.1848738357354,-18.1602576134408,
2.67613207244159));
#240345=CARTESIAN_POINT('Ctrl Pts',(56.1851705535541,-18.1599608038309,
2.6763106370782));
#240346=CARTESIAN_POINT('Ctrl Pts',(56.1854680298098,-18.1596655088802,
2.67649019601836));
#240347=CARTESIAN_POINT('Ctrl Pts',(56.1857662469844,-18.1593717347109,
2.67667072836647));
#240348=CARTESIAN_POINT('Ctrl Pts',(56.186660898508,-18.1584904122029,2.6772123254108));
#240349=CARTESIAN_POINT('Ctrl Pts',(56.1875622177791,-18.1576227783917,
2.67776268340037));
#240350=CARTESIAN_POINT('Ctrl Pts',(56.1884697364867,-18.1567689837077,
2.67832123541506));
#240351=CARTESIAN_POINT('Ctrl Pts',(56.1948621810804,-18.1507549641988,
2.68225560368426));
#240352=CARTESIAN_POINT('Ctrl Pts',(56.2015542305059,-18.1453743792959,
2.68661792998861));
#240353=CARTESIAN_POINT('Ctrl Pts',(56.2084349106659,-18.1405824894347,
2.6913098662254));
#240354=CARTESIAN_POINT('Ctrl Pts',(56.2117720331084,-18.1382584280299,
2.69358545023025));
#240355=CARTESIAN_POINT('Ctrl Pts',(56.2151540877945,-18.1360729791403,
2.69593918853449));
#240356=CARTESIAN_POINT('Ctrl Pts',(56.2185710935571,-18.1340220442542,
2.69836306235464));
#240357=CARTESIAN_POINT('Ctrl Pts',(56.2238022906401,-18.1308822062384,
2.70207384382197));
#240358=CARTESIAN_POINT('Ctrl Pts',(56.2291119669557,-18.128058438929,2.70594760814197));
#240359=CARTESIAN_POINT('Ctrl Pts',(56.2344544719218,-18.1255442374222,
2.70995196345676));
#240360=CARTESIAN_POINT('Ctrl Pts',(56.2369355588666,-18.1243766292356,
2.71181160678074));
#240361=CARTESIAN_POINT('Ctrl Pts',(56.2394235482377,-18.1232756028758,
2.71369962772068));
#240362=CARTESIAN_POINT('Ctrl Pts',(56.2419141381099,-18.1222417093392,
2.7156118313863));
#240363=CARTESIAN_POINT('Ctrl Pts',(56.2421050320102,-18.1221624654734,
2.71575839426281));
#240364=CARTESIAN_POINT('Ctrl Pts',(56.2422959411933,-18.1220835820637,
2.71590508903178));
#240365=CARTESIAN_POINT('Ctrl Pts',(56.2424868643662,-18.1220050584313,
2.7160519140988));
#240366=CARTESIAN_POINT('Ctrl Pts',(56.2451687593305,-18.1209020381377,
2.71811436362722));
#240367=CARTESIAN_POINT('Ctrl Pts',(56.2478543333342,-18.1198718859656,
2.72020091026928));
#240368=CARTESIAN_POINT('Ctrl Pts',(56.2505383386776,-18.1189123616717,
2.72230624862151));
#240369=CARTESIAN_POINT('Ctrl Pts',(56.2601627045038,-18.1154716781996,
2.72985561753017));
#240370=CARTESIAN_POINT('Ctrl Pts',(56.2698406425773,-18.1129106883009,
2.73770089914185));
#240371=CARTESIAN_POINT('Ctrl Pts',(56.2795015152448,-18.1111213027306,
2.74574823346867));
#240372=CARTESIAN_POINT('Ctrl Pts',(56.2901178437854,-18.1091549477486,
2.75459144546718));
#240373=CARTESIAN_POINT('Ctrl Pts',(56.3007141730186,-18.1081200911546,
2.76367911753858));
#240374=CARTESIAN_POINT('Ctrl Pts',(56.3112209484315,-18.107920419008,2.77292162564207));
#240375=CARTESIAN_POINT('Ctrl Pts',(56.3225656290361,-18.1077048232006,
2.78290121484032));
#240376=CARTESIAN_POINT('Ctrl Pts',(56.3338070504056,-18.1084627484392,
2.79306229499306));
#240377=CARTESIAN_POINT('Ctrl Pts',(56.3448702837274,-18.1101289800527,
2.80331916684187));
#240378=CARTESIAN_POINT('Ctrl Pts',(56.3558407078943,-18.1117812336958,
2.81348999407971));
#240379=CARTESIAN_POINT('Ctrl Pts',(56.3666372711362,-18.1143271060896,
2.82375635966507));
#240380=CARTESIAN_POINT('Ctrl Pts',(56.377179453281,-18.1177524687097,2.8340419886025));
#240381=CARTESIAN_POINT('Origin',(-0.00470941899427373,-0.014494101308147,
2.83404198860262));
#240382=CARTESIAN_POINT('Ctrl Pts',(59.7658094374954,-19.4351129318411,
2.65878198860249));
#240383=CARTESIAN_POINT('Ctrl Pts',(59.7631518948793,-19.4432803829088,
2.65878198860249));
#240384=CARTESIAN_POINT('Ctrl Pts',(59.7598356997912,-19.4511532554516,
2.6594460304184));
#240385=CARTESIAN_POINT('Ctrl Pts',(59.7559811102138,-19.4586404431008,
2.66070439264065));
#240386=CARTESIAN_POINT('Ctrl Pts',(59.7535182109729,-19.4634243995784,
2.66150842619589));
#240387=CARTESIAN_POINT('Ctrl Pts',(59.7508363273795,-19.4680513433534,
2.66255428265358));
#240388=CARTESIAN_POINT('Ctrl Pts',(59.7479734971808,-19.4725029330453,
2.66381699700641));
#240389=CARTESIAN_POINT('Ctrl Pts',(59.7440663083909,-19.4785784597564,
2.6655403487324));
#240390=CARTESIAN_POINT('Ctrl Pts',(59.7398178213044,-19.4843230052513,
2.66766759643944));
#240391=CARTESIAN_POINT('Ctrl Pts',(59.7353118462118,-19.4896904492925,
2.6701201278312));
#240392=CARTESIAN_POINT('Ctrl Pts',(59.7330588586655,-19.4923741713131,
2.67134639352707));
#240393=CARTESIAN_POINT('Ctrl Pts',(59.7307414364082,-19.4949638171727,
2.67265375584983));
#240394=CARTESIAN_POINT('Ctrl Pts',(59.72836960219,-19.4974550439407,2.67403135126911));
#240395=CARTESIAN_POINT('Ctrl Pts',(59.7271836850809,-19.4987006573247,
2.67472014897875));
#240396=CARTESIAN_POINT('Ctrl Pts',(59.7259841596486,-19.4999216825129,
2.67542649668603));
#240397=CARTESIAN_POINT('Ctrl Pts',(59.724772245347,-19.5011176808513,2.67614899656072));
#240398=CARTESIAN_POINT('Ctrl Pts',(59.7244692667716,-19.5014166804359,
2.67632962152939));
#240399=CARTESIAN_POINT('Ctrl Pts',(59.7241655137792,-19.5017141161959,
2.67651125590921));
#240400=CARTESIAN_POINT('Ctrl Pts',(59.7238610051972,-19.5020099819903,
2.67669387767494));
#240401=CARTESIAN_POINT('Ctrl Pts',(59.7229474794513,-19.5028975793736,
2.67724174297214));
#240402=CARTESIAN_POINT('Ctrl Pts',(59.7220271539532,-19.5037710453,2.67779849504718));
#240403=CARTESIAN_POINT('Ctrl Pts',(59.7211005320716,-19.5046302297516,
2.67836353617979));
#240404=CARTESIAN_POINT('Ctrl Pts',(59.7146969999426,-19.510567727398,2.68226832098892));
#240405=CARTESIAN_POINT('Ctrl Pts',(59.7079999120045,-19.5158784513265,
2.68659153751391));
#240406=CARTESIAN_POINT('Ctrl Pts',(59.701118410241,-19.5206092977901,2.69123699486197));
#240407=CARTESIAN_POINT('Ctrl Pts',(59.6976983227542,-19.5229605154963,
2.6935457744122));
#240408=CARTESIAN_POINT('Ctrl Pts',(59.6942320938701,-19.5251683423973,
2.69593478828105));
#240409=CARTESIAN_POINT('Ctrl Pts',(59.6907301905173,-19.5272373629634,
2.6983956526119));
#240410=CARTESIAN_POINT('Ctrl Pts',(59.6830044686628,-19.5318019313693,
2.70382468689016));
#240411=CARTESIAN_POINT('Ctrl Pts',(59.6751122606221,-19.5357011184419,
2.70961155815057));
#240412=CARTESIAN_POINT('Ctrl Pts',(59.6671986827534,-19.5389266512974,
2.71562701361738));
#240413=CARTESIAN_POINT('Ctrl Pts',(59.6643077529624,-19.5401049791256,
2.71782453535829));
#240414=CARTESIAN_POINT('Ctrl Pts',(59.6614137631516,-19.5412013620772,
2.72005051502373));
#240415=CARTESIAN_POINT('Ctrl Pts',(59.6585211429015,-19.5422187365059,
2.72229986760086));
#240416=CARTESIAN_POINT('Ctrl Pts',(59.6488051375687,-19.545635989557,2.7298552048887));
#240417=CARTESIAN_POINT('Ctrl Pts',(59.6390401911867,-19.5481755652416,
2.73770845534541));
#240418=CARTESIAN_POINT('Ctrl Pts',(59.6292970278052,-19.5499445144585,
2.7457670670174));
#240419=CARTESIAN_POINT('Ctrl Pts',(59.6185881370953,-19.5518887991936,
2.75462443585027));
#240420=CARTESIAN_POINT('Ctrl Pts',(59.6079049297392,-19.5529023976132,
2.76373036323189));
#240421=CARTESIAN_POINT('Ctrl Pts',(59.5973174182796,-19.5530800481809,
2.7729966463684));
#240422=CARTESIAN_POINT('Ctrl Pts',(59.5859142147986,-19.5532713854541,
2.78297683033527));
#240423=CARTESIAN_POINT('Ctrl Pts',(59.5746208362127,-19.5524931697979,
2.7931440147898));
#240424=CARTESIAN_POINT('Ctrl Pts',(59.5635130675389,-19.5508078878546,
2.80341452428065));
#240425=CARTESIAN_POINT('Ctrl Pts',(59.5525552912484,-19.549145362908,2.81354634721434));
#240426=CARTESIAN_POINT('Ctrl Pts',(59.5417768065743,-19.546599586876,2.82378004209225));
#240427=CARTESIAN_POINT('Ctrl Pts',(59.5312589135998,-19.5431821162857,
2.83404198860249));
#240428=CARTESIAN_POINT('Ctrl Pts',(56.2594439784241,-18.4801050014181,
2.83404198860249));
#240429=CARTESIAN_POINT('Ctrl Pts',(56.2493782971089,-18.4768344633028,
2.8242212644309));
#240430=CARTESIAN_POINT('Ctrl Pts',(56.239606768123,-18.4727817672086,2.8144281502868));
#240431=CARTESIAN_POINT('Ctrl Pts',(56.2301791400452,-18.4679768367037,
2.80471618166591));
#240432=CARTESIAN_POINT('Ctrl Pts',(56.2210759356566,-18.4633372535447,
2.7953384214656));
#240433=CARTESIAN_POINT('Ctrl Pts',(56.212292281258,-18.4579956735929,2.78603515650626));
#240434=CARTESIAN_POINT('Ctrl Pts',(56.2038917763273,-18.4519372213374,
2.77685887347194));
#240435=CARTESIAN_POINT('Ctrl Pts',(56.1959506682923,-18.4462100865662,
2.76818441217041));
#240436=CARTESIAN_POINT('Ctrl Pts',(56.1883512165513,-18.4398418135305,
2.75962261522113));
#240437=CARTESIAN_POINT('Ctrl Pts',(56.1811768067767,-18.4327901596652,
2.75123537702169));
#240438=CARTESIAN_POINT('Ctrl Pts',(56.1745692957339,-18.4262957047555,
2.74351087134639));
#240439=CARTESIAN_POINT('Ctrl Pts',(56.1683219623547,-18.4192211773454,
2.73593399450374));
#240440=CARTESIAN_POINT('Ctrl Pts',(56.1625328136795,-18.4115142492207,
2.72857657813109));
#240441=CARTESIAN_POINT('Ctrl Pts',(56.1608066064052,-18.4092161988271,
2.72638274508666));
#240442=CARTESIAN_POINT('Ctrl Pts',(56.1591213928277,-18.4068618031994,
2.72420861709758));
#240443=CARTESIAN_POINT('Ctrl Pts',(56.1574804751189,-18.4044493827306,
2.72205663736696));
#240444=CARTESIAN_POINT('Ctrl Pts',(56.1558563235463,-18.4020616112555,
2.71992664556735));
#240445=CARTESIAN_POINT('Ctrl Pts',(56.1542770260205,-18.3996196264074,
2.71782089927853));
#240446=CARTESIAN_POINT('Ctrl Pts',(56.1527473834686,-18.3971247125278,
2.71574387311215));
#240447=CARTESIAN_POINT('Ctrl Pts',(56.152641015117,-18.3969512210959,2.71559944077456));
#240448=CARTESIAN_POINT('Ctrl Pts',(56.1525348749439,-18.3967774746426,
2.71545515216038));
#240449=CARTESIAN_POINT('Ctrl Pts',(56.1524289641635,-18.3966034726917,
2.71531100781699));
#240450=CARTESIAN_POINT('Ctrl Pts',(56.1477854475703,-18.3889745897483,
2.70899119176047));
#240451=CARTESIAN_POINT('Ctrl Pts',(56.1436260014308,-18.3808409394265,
2.70298296066796));
#240452=CARTESIAN_POINT('Ctrl Pts',(56.1400597146376,-18.3722424849449,
2.69736727774089));
#240453=CARTESIAN_POINT('Ctrl Pts',(56.1367353155298,-18.3642272309667,
2.6921324852537));
#240454=CARTESIAN_POINT('Ctrl Pts',(56.1339262909283,-18.3558072700336,
2.68723866185399));
#240455=CARTESIAN_POINT('Ctrl Pts',(56.1317496772149,-18.3470212548454,
2.68278595829485));
#240456=CARTESIAN_POINT('Ctrl Pts',(56.1309534437593,-18.3438072168233,
2.68115710172744));
#240457=CARTESIAN_POINT('Ctrl Pts',(56.1302421351292,-18.3405443147871,
2.67958763637763));
#240458=CARTESIAN_POINT('Ctrl Pts',(56.1296225724749,-18.3372349828457,
2.67808378645331));
#240459=CARTESIAN_POINT('Ctrl Pts',(56.1294735883543,-18.3364391990687,
2.67772216078566));
#240460=CARTESIAN_POINT('Ctrl Pts',(56.1293301519983,-18.3356401993818,
2.67736403603529));
#240461=CARTESIAN_POINT('Ctrl Pts',(56.1291923454417,-18.3348380918578,
2.67700956934445));
#240462=CARTESIAN_POINT('Ctrl Pts',(56.1290588453401,-18.3340610501939,
2.6766661797377));
#240463=CARTESIAN_POINT('Ctrl Pts',(56.128930628665,-18.3332810919213,2.67632622314085));
#240464=CARTESIAN_POINT('Ctrl Pts',(56.128807768806,-18.3324983188923,2.67598984158739));
#240465=CARTESIAN_POINT('Ctrl Pts',(56.127461697065,-18.3239221357301,2.67230439292194));
#240466=CARTESIAN_POINT('Ctrl Pts',(56.1267581593462,-18.3150023767869,
2.66904964539953));
#240467=CARTESIAN_POINT('Ctrl Pts',(56.1267895336333,-18.3059033598546,
2.66640203566706));
#240468=CARTESIAN_POINT('Ctrl Pts',(56.1268025454853,-18.3021297263199,
2.66530399299415));
#240469=CARTESIAN_POINT('Ctrl Pts',(56.12694160832,-18.2983254984041,2.66430995142229));
#240470=CARTESIAN_POINT('Ctrl Pts',(56.1272115877757,-18.2945030089048,
2.66343053473326));
#240471=CARTESIAN_POINT('Ctrl Pts',(56.1276720658711,-18.2879833547325,
2.6619305979285));
#240472=CARTESIAN_POINT('Ctrl Pts',(56.1285150529072,-18.2814124323565,
2.66076519817093));
#240473=CARTESIAN_POINT('Ctrl Pts',(56.1297657127889,-18.2748585331705,
2.65997805604425));
#240474=CARTESIAN_POINT('Ctrl Pts',(56.1303910427297,-18.2715815835775,
2.65958448498091));
#240475=CARTESIAN_POINT('Ctrl Pts',(56.131119686293,-18.2683092720859,2.65928526260727));
#240476=CARTESIAN_POINT('Ctrl Pts',(56.1319548233213,-18.2650501911666,
2.6590846397129));
#240477=CARTESIAN_POINT('Ctrl Pts',(56.1327899603496,-18.2617911102473,
2.65888401681852));
#240478=CARTESIAN_POINT('Ctrl Pts',(56.1337315613411,-18.2585452947506,
2.6587819886025));
#240479=CARTESIAN_POINT('Ctrl Pts',(56.1347810195644,-18.255320281274,2.6587819886025));
#240480=CARTESIAN_POINT('Origin',(56.9937374973465,-12.0988124084931,2.83404198860254));
#240481=CARTESIAN_POINT('Ctrl Pts',(61.3271735965895,-12.8407372733088,
2.83404198860254));
#240482=CARTESIAN_POINT('Ctrl Pts',(61.3375520649561,-12.8429432848602,
2.82419652440068));
#240483=CARTESIAN_POINT('Ctrl Pts',(61.3477256769083,-12.8459616464934,
2.81438790575667));
#240484=CARTESIAN_POINT('Ctrl Pts',(61.3576417279027,-12.8497656413952,
2.80466781256936));
#240485=CARTESIAN_POINT('Ctrl Pts',(61.367235566286,-12.853446029114,2.79526356453127));
#240486=CARTESIAN_POINT('Ctrl Pts',(61.3765894879233,-12.8578623484984,
2.78594102496298));
#240487=CARTESIAN_POINT('Ctrl Pts',(61.3856422574858,-12.8630345798908,
2.7767510908886));
#240488=CARTESIAN_POINT('Ctrl Pts',(61.3942056200545,-12.8679271923004,
2.7680579791378));
#240489=CARTESIAN_POINT('Ctrl Pts',(61.4025003187112,-12.873496651755,2.75948271210275));
#240490=CARTESIAN_POINT('Ctrl Pts',(61.4104485116933,-12.8797929832512,
2.75108575573353));
#240491=CARTESIAN_POINT('Ctrl Pts',(61.4177693722577,-12.8855923599215,
2.74335155163415));
#240492=CARTESIAN_POINT('Ctrl Pts',(61.4247966697184,-12.8920087864942,
2.73576818686103));
#240493=CARTESIAN_POINT('Ctrl Pts',(61.4314390014603,-12.8991043342864,
2.7284062616067));
#240494=CARTESIAN_POINT('Ctrl Pts',(61.4333656894049,-12.9011624829791,
2.7262708469379));
#240495=CARTESIAN_POINT('Ctrl Pts',(61.4352597571378,-12.9032779088702,
2.72415424587572));
#240496=CARTESIAN_POINT('Ctrl Pts',(61.437118361331,-12.9054524645835,2.72205867173248));
#240497=CARTESIAN_POINT('Ctrl Pts',(61.4391332077734,-12.9078098227873,
2.71978693462851));
#240498=CARTESIAN_POINT('Ctrl Pts',(61.4411043938525,-12.9102326900439,
2.71754411340752));
#240499=CARTESIAN_POINT('Ctrl Pts',(61.4430281531013,-12.9127224163019,
2.71533341844249));
#240500=CARTESIAN_POINT('Ctrl Pts',(61.4483079254551,-12.9195554895536,
2.70926614876396));
#240501=CARTESIAN_POINT('Ctrl Pts',(61.4531896374537,-12.9269097705822,
2.70347381860413));
#240502=CARTESIAN_POINT('Ctrl Pts',(61.4575800373535,-12.9347398820021,
2.698049141714));
#240503=CARTESIAN_POINT('Ctrl Pts',(61.4615970149013,-12.9419040088445,
2.69308585687216));
#240504=CARTESIAN_POINT('Ctrl Pts',(61.4651913207947,-12.9494643722274,
2.68842799053203));
#240505=CARTESIAN_POINT('Ctrl Pts',(61.4682744840803,-12.9574154517094,
2.68414767054239));
#240506=CARTESIAN_POINT('Ctrl Pts',(61.4697889238146,-12.9613209959778,
2.68204519134568));
#240507=CARTESIAN_POINT('Ctrl Pts',(61.4711795284101,-12.9653208118544,
2.68003431778513));
#240508=CARTESIAN_POINT('Ctrl Pts',(61.4724324898306,-12.9694138336341,
2.67812693945258));
#240509=CARTESIAN_POINT('Ctrl Pts',(61.4726702270561,-12.9701904446502,
2.6777650329921));
#240510=CARTESIAN_POINT('Ctrl Pts',(61.4729027677276,-12.9709708853383,
2.6774065963993));
#240511=CARTESIAN_POINT('Ctrl Pts',(61.4731300138564,-12.9717550556838,
2.67705178968862));
#240512=CARTESIAN_POINT('Ctrl Pts',(61.4733501585437,-12.9725147207061,
2.67670807068764));
#240513=CARTESIAN_POINT('Ctrl Pts',(61.4735653344327,-12.9732778858998,
2.67636775825272));
#240514=CARTESIAN_POINT('Ctrl Pts',(61.4737754532575,-12.9740444565827,
2.67603099699262));
#240515=CARTESIAN_POINT('Ctrl Pts',(61.4760652849148,-12.982398385929,2.67236104217127));
#240516=CARTESIAN_POINT('Ctrl Pts',(61.4777556486133,-12.9911623597375,
2.66911440541467));
#240517=CARTESIAN_POINT('Ctrl Pts',(61.4787331403172,-13.0001833616597,
2.66646778189621));
#240518=CARTESIAN_POINT('Ctrl Pts',(61.4791459411336,-13.0039929867889,
2.66535009634971));
#240519=CARTESIAN_POINT('Ctrl Pts',(61.4794319383913,-13.0078481668559,
2.66433897912346));
#240520=CARTESIAN_POINT('Ctrl Pts',(61.4795843394719,-13.0117365408422,
2.66344564884798));
#240521=CARTESIAN_POINT('Ctrl Pts',(61.4798409790836,-13.0182844654755,
2.66194130298591));
#240522=CARTESIAN_POINT('Ctrl Pts',(61.4797168922659,-13.0249248230166,
2.66077206705425));
#240523=CARTESIAN_POINT('Ctrl Pts',(61.4791780149469,-13.0315916763168,
2.65998225155719));
#240524=CARTESIAN_POINT('Ctrl Pts',(61.4790432956172,-13.0332583896419,
2.65978479768293));
#240525=CARTESIAN_POINT('Ctrl Pts',(61.4788824204063,-13.0349267248708,
2.65961098966627));
#240526=CARTESIAN_POINT('Ctrl Pts',(61.4786945538951,-13.0365955947395,
2.65946139030506));
#240527=CARTESIAN_POINT('Ctrl Pts',(61.4784127541283,-13.0390988995425,
2.65923699126325));
#240528=CARTESIAN_POINT('Ctrl Pts',(61.4780702140294,-13.0416033892092,
2.65906707562446));
#240529=CARTESIAN_POINT('Ctrl Pts',(61.4776657592308,-13.044105725102,2.65895332562924));
#240530=CARTESIAN_POINT('Ctrl Pts',(61.4772613044323,-13.0466080609949,
2.65883957563402));
#240531=CARTESIAN_POINT('Ctrl Pts',(61.4767949453823,-13.0491082380619,
2.65878198860253));
#240532=CARTESIAN_POINT('Ctrl Pts',(61.4762657165317,-13.0516031943519,
2.65878198860253));
#240533=CARTESIAN_POINT('Ctrl Pts',(57.7418065394567,-12.2578193919758,
2.65878198860254));
#240534=CARTESIAN_POINT('Ctrl Pts',(57.7435970583545,-12.2493771807069,
2.65878198860254));
#240535=CARTESIAN_POINT('Ctrl Pts',(57.7460689269801,-12.2411559442244,
2.65945335517842));
#240536=CARTESIAN_POINT('Ctrl Pts',(57.7491141258102,-12.2332613533226,
2.6607256122658));
#240537=CARTESIAN_POINT('Ctrl Pts',(57.7510810117991,-12.2281622576314,
2.6615473598032));
#240538=CARTESIAN_POINT('Ctrl Pts',(57.7532862127604,-12.2231990866879,
2.66261895766868));
#240539=CARTESIAN_POINT('Ctrl Pts',(57.755693185958,-12.2183955094111,2.66391429251019));
#240540=CARTESIAN_POINT('Ctrl Pts',(57.7588834910513,-12.2120286428969,
2.66563118464116));
#240541=CARTESIAN_POINT('Ctrl Pts',(57.7624328173676,-12.2059457447509,
2.66774105138691));
#240542=CARTESIAN_POINT('Ctrl Pts',(57.766268204371,-12.2001996238492,2.67016894181742));
#240543=CARTESIAN_POINT('Ctrl Pts',(57.7681858978727,-12.1973265633984,
2.67138288703268));
#240544=CARTESIAN_POINT('Ctrl Pts',(57.7701751462711,-12.1945375019629,
2.67267613167544));
#240545=CARTESIAN_POINT('Ctrl Pts',(57.7722271161469,-12.1918376559065,
2.67403835432546));
#240546=CARTESIAN_POINT('Ctrl Pts',(57.7732531010848,-12.1904877328782,
2.67471946565047));
#240547=CARTESIAN_POINT('Ctrl Pts',(57.7742947697605,-12.1891600976126,
2.67541781389516));
#240548=CARTESIAN_POINT('Ctrl Pts',(57.7753510390206,-12.1878553011589,
2.67613207244162));
#240549=CARTESIAN_POINT('Ctrl Pts',(57.7756151063356,-12.1875291020455,
2.67631063707824));
#240550=CARTESIAN_POINT('Ctrl Pts',(57.7758800862579,-12.1872043300155,
2.67649019601839));
#240551=CARTESIAN_POINT('Ctrl Pts',(57.7761459620051,-12.1868809929889,
2.6766707283665));
#240552=CARTESIAN_POINT('Ctrl Pts',(57.7769435892466,-12.1859109819089,
2.67721232541084));
#240553=CARTESIAN_POINT('Ctrl Pts',(57.7777492785675,-12.1849538875681,
2.6777626834004));
#240554=CARTESIAN_POINT('Ctrl Pts',(57.7785625799464,-12.1840099085249,
2.67832123541509));
#240555=CARTESIAN_POINT('Ctrl Pts',(57.7842913698424,-12.1773606420342,
2.68225560368432));
#240556=CARTESIAN_POINT('Ctrl Pts',(57.7903843352497,-12.1713100228958,
2.68661792998868));
#240557=CARTESIAN_POINT('Ctrl Pts',(57.7967264334405,-12.1658251565852,
2.69130986622549));
#240558=CARTESIAN_POINT('Ctrl Pts',(57.7998023442099,-12.1631650023514,
2.69358545023032));
#240559=CARTESIAN_POINT('Ctrl Pts',(57.8029374300325,-12.1606380046005,
2.69593918853454));
#240560=CARTESIAN_POINT('Ctrl Pts',(57.806121336008,-12.1582411305889,2.69836306235468));
#240561=CARTESIAN_POINT('Ctrl Pts',(57.8109956736034,-12.1545716839421,
2.70207384382201));
#240562=CARTESIAN_POINT('Ctrl Pts',(57.8159810988991,-12.1512083732199,
2.705947608142));
#240563=CARTESIAN_POINT('Ctrl Pts',(57.8210315314442,-12.1481495009378,
2.7099519634568));
#240564=CARTESIAN_POINT('Ctrl Pts',(57.8233769784456,-12.1467289448255,
2.71181160678078));
#240565=CARTESIAN_POINT('Ctrl Pts',(57.8257362497573,-12.1453738842977,
2.71369962772071));
#240566=CARTESIAN_POINT('Ctrl Pts',(57.828105124615,-12.1440853170061,2.71561183138634));
#240567=CARTESIAN_POINT('Ctrl Pts',(57.828286689539,-12.1439865534004,2.71575839426285));
#240568=CARTESIAN_POINT('Ctrl Pts',(57.82846830734,-12.1438881466788,2.71590508903182));
#240569=CARTESIAN_POINT('Ctrl Pts',(57.8286499766612,-12.1437900963012,
2.71605191409884));
#240570=CARTESIAN_POINT('Ctrl Pts',(57.831201882908,-12.1424127841089,2.71811436362725));
#240571=CARTESIAN_POINT('Ctrl Pts',(57.8337650648328,-12.1411075562946,
2.72020091026932));
#240572=CARTESIAN_POINT('Ctrl Pts',(57.8363340693142,-12.1398727334212,
2.72230624862154));
#240573=CARTESIAN_POINT('Ctrl Pts',(57.845546062502,-12.1354448782032,2.72985561753057));
#240574=CARTESIAN_POINT('Ctrl Pts',(57.85490328748,-12.1318862976806,2.73770089914263));
#240575=CARTESIAN_POINT('Ctrl Pts',(57.8643241951528,-12.1290968783778,
2.74574823346985));
#240576=CARTESIAN_POINT('Ctrl Pts',(57.8746768262713,-12.126031586786,2.75459144546915));
#240577=CARTESIAN_POINT('Ctrl Pts',(57.8851069357357,-12.1238947812336,
2.7636791175414));
#240578=CARTESIAN_POINT('Ctrl Pts',(57.8955352825119,-12.1225979458242,
2.77292162564575));
#240579=CARTESIAN_POINT('Ctrl Pts',(57.9067952798725,-12.1211976890434,
2.78290121484571));
#240580=CARTESIAN_POINT('Ctrl Pts',(57.9180543443219,-12.1207764137879,
2.7930622950002));
#240581=CARTESIAN_POINT('Ctrl Pts',(57.9292311407257,-12.121277094833,2.80331916685078));
#240582=CARTESIAN_POINT('Ctrl Pts',(57.9403141752922,-12.1217735756786,
2.81348999408573));
#240583=CARTESIAN_POINT('Ctrl Pts',(57.9513177099566,-12.1231769533527,
2.82375635966811));
#240584=CARTESIAN_POINT('Ctrl Pts',(57.9621601888122,-12.1254815933782,
2.83404198860254));
#240585=CARTESIAN_POINT('Origin',(-0.00316857416806234,-0.0149069694349926,
2.83404198860262));
#240586=CARTESIAN_POINT('Ctrl Pts',(61.4699285681956,-13.0814171332223,
2.65878198860253));
#240587=CARTESIAN_POINT('Ctrl Pts',(61.468139314985,-13.089817630984,2.65878198860253));
#240588=CARTESIAN_POINT('Ctrl Pts',(61.4656642256291,-13.0979940118835,
2.65944603041842));
#240589=CARTESIAN_POINT('Ctrl Pts',(61.4626133761159,-13.1058430982603,
2.66070439264062));
#240590=CARTESIAN_POINT('Ctrl Pts',(61.4606640285136,-13.1108582907967,
2.66150842619587));
#240591=CARTESIAN_POINT('Ctrl Pts',(61.4584804838816,-13.1157402208604,
2.66255428265359));
#240592=CARTESIAN_POINT('Ctrl Pts',(61.4560986543958,-13.1204666715196,
2.66381699700645));
#240593=CARTESIAN_POINT('Ctrl Pts',(61.4528479350655,-13.1269173282996,
2.66554034873245));
#240594=CARTESIAN_POINT('Ctrl Pts',(61.4492231901486,-13.1330744923996,
2.66766759643949));
#240595=CARTESIAN_POINT('Ctrl Pts',(61.4453029499363,-13.1388835356727,
2.67012012783125));
#240596=CARTESIAN_POINT('Ctrl Pts',(61.4433428298301,-13.1417880573093,
2.67134639352713));
#240597=CARTESIAN_POINT('Ctrl Pts',(61.4413087943566,-13.1446057534052,
2.67265375584989));
#240598=CARTESIAN_POINT('Ctrl Pts',(61.4392103574001,-13.1473312571582,
2.67403135126917));
#240599=CARTESIAN_POINT('Ctrl Pts',(61.4381611389218,-13.1486940090348,
2.67472014897881));
#240600=CARTESIAN_POINT('Ctrl Pts',(61.4370958165018,-13.1500337298693,
2.6754264966861));
#240601=CARTESIAN_POINT('Ctrl Pts',(61.436015557062,-13.1513498559433,2.67614899656079));
#240602=CARTESIAN_POINT('Ctrl Pts',(61.435745492202,-13.1516788874618,2.67632962152946));
#240603=CARTESIAN_POINT('Ctrl Pts',(61.4354744937032,-13.152006444671,2.67651125590927));
#240604=CARTESIAN_POINT('Ctrl Pts',(61.435202579648,-13.1523325194958,2.67669387767501));
#240605=CARTESIAN_POINT('Ctrl Pts',(61.4343868374822,-13.1533107439701,
2.67724174297221));
#240606=CARTESIAN_POINT('Ctrl Pts',(61.4335628556744,-13.1542756251688,
2.67779849504725));
#240607=CARTESIAN_POINT('Ctrl Pts',(61.4327311191548,-13.1552269612794,
2.67836353617986));
#240608=CARTESIAN_POINT('Ctrl Pts',(61.4269833037496,-13.1618012840651,
2.68226832098887));
#240609=CARTESIAN_POINT('Ctrl Pts',(61.4208780249712,-13.1677829516027,
2.68659153751371));
#240610=CARTESIAN_POINT('Ctrl Pts',(61.4145287289055,-13.1732071947985,
2.6912369948616));
#240611=CARTESIAN_POINT('Ctrl Pts',(61.4113731461892,-13.1759030287776,
2.69354577441197));
#240612=CARTESIAN_POINT('Ctrl Pts',(61.4081566864226,-13.1784610805506,
2.69593478828095));
#240613=CARTESIAN_POINT('Ctrl Pts',(61.4048902384028,-13.1808848153817,
2.69839565261195));
#240614=CARTESIAN_POINT('Ctrl Pts',(61.3976839661819,-13.1862319364373,
2.7038246868902));
#240615=CARTESIAN_POINT('Ctrl Pts',(61.3902425685154,-13.1909347237334,
2.70961155815062));
#240616=CARTESIAN_POINT('Ctrl Pts',(61.3827095020468,-13.194969780916,2.71562701361742));
#240617=CARTESIAN_POINT('Ctrl Pts',(61.3799575778688,-13.1964438381895,
2.71782453535832));
#240618=CARTESIAN_POINT('Ctrl Pts',(61.377194044862,-13.1978367193482,2.72005051502376));
#240619=CARTESIAN_POINT('Ctrl Pts',(61.374423615274,-13.1991508816429,2.7222998676009));
#240620=CARTESIAN_POINT('Ctrl Pts',(61.3651180354455,-13.2035650137305,
2.72985520488838));
#240621=CARTESIAN_POINT('Ctrl Pts',(61.3556720404057,-13.2071113921929,
2.73770845534476));
#240622=CARTESIAN_POINT('Ctrl Pts',(61.3461671566366,-13.2098890888164,
2.74576706701642));
#240623=CARTESIAN_POINT('Ctrl Pts',(61.3357201634468,-13.2129421064455,
2.75462443584889));
#240624=CARTESIAN_POINT('Ctrl Pts',(61.3252014297043,-13.2150668515146,
2.76373036323012));
#240625=CARTESIAN_POINT('Ctrl Pts',(61.3146904872818,-13.2163502251968,
2.77299664636617));
#240626=CARTESIAN_POINT('Ctrl Pts',(61.3033697519348,-13.2177324736407,
2.78297683033235));
#240627=CARTESIAN_POINT('Ctrl Pts',(61.2920568939728,-13.2181390006403,
2.7931440147861));
#240628=CARTESIAN_POINT('Ctrl Pts',(61.280833814887,-13.2176240288379,2.80341452427607));
#240629=CARTESIAN_POINT('Ctrl Pts',(61.2697622852616,-13.2171160108936,
2.8135463472114));
#240630=CARTESIAN_POINT('Ctrl Pts',(61.2587767401957,-13.2157108393283,
2.82378004209088));
#240631=CARTESIAN_POINT('Ctrl Pts',(61.2479592423879,-13.2134115091884,
2.83404198860253));
#240632=CARTESIAN_POINT('Ctrl Pts',(57.8829458346107,-12.4981558292578,
2.83404198860253));
#240633=CARTESIAN_POINT('Ctrl Pts',(57.8725934298275,-12.4959553576921,
2.82422126443084));
#240634=CARTESIAN_POINT('Ctrl Pts',(57.8624518082049,-12.4929462655998,
2.81442815028665));
#240635=CARTESIAN_POINT('Ctrl Pts',(57.8525735736582,-12.4891531124821,
2.80471618166567));
#240636=CARTESIAN_POINT('Ctrl Pts',(57.8430352690779,-12.4854904894106,
2.79533842146522));
#240637=CARTESIAN_POINT('Ctrl Pts',(57.8337413853132,-12.4810963130887,
2.78603515650575));
#240638=CARTESIAN_POINT('Ctrl Pts',(57.8247536185233,-12.4759491415396,
2.77685887347131));
#240639=CARTESIAN_POINT('Ctrl Pts',(57.8162573641123,-12.4710834524312,
2.76818441216959));
#240640=CARTESIAN_POINT('Ctrl Pts',(57.8080338771688,-12.4655444244735,
2.75962261522012));
#240641=CARTESIAN_POINT('Ctrl Pts',(57.8001616710194,-12.4592813303343,
2.7512353770205));
#240642=CARTESIAN_POINT('Ctrl Pts',(57.7929115012218,-12.4535131257032,
2.74351087134493));
#240643=CARTESIAN_POINT('Ctrl Pts',(57.7859589019098,-12.4471303774518,
2.73593399450203));
#240644=CARTESIAN_POINT('Ctrl Pts',(57.7793958734432,-12.4400707994999,
2.72857657812914));
#240645=CARTESIAN_POINT('Ctrl Pts',(57.7774389108374,-12.4379657758611,
2.72638274508539));
#240646=CARTESIAN_POINT('Ctrl Pts',(57.7755168276799,-12.4358004306452,
2.72420861709697));
#240647=CARTESIAN_POINT('Ctrl Pts',(57.7736327324862,-12.4335727482752,
2.722056637367));
#240648=CARTESIAN_POINT('Ctrl Pts',(57.7717678881029,-12.4313678273301,
2.71992664556739));
#240649=CARTESIAN_POINT('Ctrl Pts',(57.7699419852107,-12.429104301474,2.71782089927857));
#240650=CARTESIAN_POINT('Ctrl Pts',(57.7681599326869,-12.4267829461789,
2.71574387311219));
#240651=CARTESIAN_POINT('Ctrl Pts',(57.7680360122396,-12.4266215236716,
2.7155994407746));
#240652=CARTESIAN_POINT('Ctrl Pts',(57.7679122920636,-12.4264598236887,
2.71545515216042));
#240653=CARTESIAN_POINT('Ctrl Pts',(57.7677887733171,-12.4262978456299,
2.71531100781703));
#240654=CARTESIAN_POINT('Ctrl Pts',(57.7623732589831,-12.419196134159,2.70899119176049));
#240655=CARTESIAN_POINT('Ctrl Pts',(57.7573864007558,-12.4115418213378,
2.70298296066798));
#240656=CARTESIAN_POINT('Ctrl Pts',(57.7529408672214,-12.4033632485675,
2.6973672777409));
#240657=CARTESIAN_POINT('Ctrl Pts',(57.7487968573387,-12.3957393973193,
2.69213248525374));
#240658=CARTESIAN_POINT('Ctrl Pts',(57.7451230952908,-12.3876591848381,
2.68723866185406));
#240659=CARTESIAN_POINT('Ctrl Pts',(57.7420400166292,-12.3791488184471,
2.68278595829494));
#240660=CARTESIAN_POINT('Ctrl Pts',(57.7409121865684,-12.376035616321,2.68115710172751));
#240661=CARTESIAN_POINT('Ctrl Pts',(57.7398637084259,-12.3728649408015,
2.67958763637769));
#240662=CARTESIAN_POINT('Ctrl Pts',(57.7389016204183,-12.3696384996589,
2.67808378645336));
#240663=CARTESIAN_POINT('Ctrl Pts',(57.738670270393,-12.3688626483499,2.67772216078571));
#240664=CARTESIAN_POINT('Ctrl Pts',(57.7384441015869,-12.3680830188488,
2.67736403603534));
#240665=CARTESIAN_POINT('Ctrl Pts',(57.7382232068822,-12.3672997100613,
2.6770095693445));
#240666=CARTESIAN_POINT('Ctrl Pts',(57.7380092151371,-12.3665408796734,
2.67666617973775));
#240667=CARTESIAN_POINT('Ctrl Pts',(57.7378001730067,-12.3657785963858,
2.6763262231409));
#240668=CARTESIAN_POINT('Ctrl Pts',(57.737596164125,-12.3650129538217,2.67598984158744));
#240669=CARTESIAN_POINT('Ctrl Pts',(57.7353610110592,-12.3566244546987,
2.67230439292203));
#240670=CARTESIAN_POINT('Ctrl Pts',(57.7337289586986,-12.3478270988451,
2.66904964539965));
#240671=CARTESIAN_POINT('Ctrl Pts',(57.732809054857,-12.3387746477736,2.66640203566719));
#240672=CARTESIAN_POINT('Ctrl Pts',(57.7324275433144,-12.3350203264893,
2.66530399299425));
#240673=CARTESIAN_POINT('Ctrl Pts',(57.7321681942504,-12.3312224025075,
2.66430995142236));
#240674=CARTESIAN_POINT('Ctrl Pts',(57.7320371357771,-12.327392632468,2.66343053473331));
#240675=CARTESIAN_POINT('Ctrl Pts',(57.7318136018937,-12.3208605605757,
2.66193059792855));
#240676=CARTESIAN_POINT('Ctrl Pts',(57.7319651225404,-12.3142375182605,
2.66076519817097));
#240677=CARTESIAN_POINT('Ctrl Pts',(57.7325238621659,-12.3075887924645,
2.6599780560443));
#240678=CARTESIAN_POINT('Ctrl Pts',(57.7328032319787,-12.3042644295665,
2.65958448498096));
#240679=CARTESIAN_POINT('Ctrl Pts',(57.7331858342648,-12.3009338801477,
2.65928526260732));
#240680=CARTESIAN_POINT('Ctrl Pts',(57.7336757296049,-12.2976053572245,
2.65908463971294));
#240681=CARTESIAN_POINT('Ctrl Pts',(57.7341656249451,-12.2942768343013,
2.65888401681856));
#240682=CARTESIAN_POINT('Ctrl Pts',(57.7347627876419,-12.2909503756169,
2.65878198860254));
#240683=CARTESIAN_POINT('Ctrl Pts',(57.7354693911206,-12.2876333308462,
2.65878198860254));
#240684=CARTESIAN_POINT('Origin',(57.9461901084063,-6.07506605172202,2.83404198860258));
#240685=CARTESIAN_POINT('Ctrl Pts',(62.333439457262,-6.35995915837698,2.83404198860258));
#240686=CARTESIAN_POINT('Ctrl Pts',(62.3439916622904,-6.36106823981685,
2.82419652440068));
#240687=CARTESIAN_POINT('Ctrl Pts',(62.354425046835,-6.36300663452592,2.81438790575664));
#240688=CARTESIAN_POINT('Ctrl Pts',(62.3646844024059,-6.36575328117349,
2.8046678125693));
#240689=CARTESIAN_POINT('Ctrl Pts',(62.3746103900112,-6.36841067816022,
2.7952635645312));
#240690=CARTESIAN_POINT('Ctrl Pts',(62.3843747009655,-6.37182505343072,
2.7859410249629));
#240691=CARTESIAN_POINT('Ctrl Pts',(62.3939185239083,-6.37602267870771,
2.77675109088853));
#240692=CARTESIAN_POINT('Ctrl Pts',(62.4029463927375,-6.37999337374486,
2.76805797913774));
#240693=CARTESIAN_POINT('Ctrl Pts',(62.4117778192051,-6.38466529101398,
2.75948271210271));
#240694=CARTESIAN_POINT('Ctrl Pts',(62.4203406170099,-6.39009631814929,
2.7510857557335));
#240695=CARTESIAN_POINT('Ctrl Pts',(62.4282275730653,-6.39509868692276,
2.74335155163415));
#240696=CARTESIAN_POINT('Ctrl Pts',(62.4358870734646,-6.4007454110349,2.73576818686106));
#240697=CARTESIAN_POINT('Ctrl Pts',(62.443234704525,-6.4071077759443,2.72840626160674));
#240698=CARTESIAN_POINT('Ctrl Pts',(62.4453659729915,-6.40895325615313,
2.72627084693796));
#240699=CARTESIAN_POINT('Ctrl Pts',(62.4474707870407,-6.41085910953041,
2.72415424587578));
#240700=CARTESIAN_POINT('Ctrl Pts',(62.4495465125726,-6.41282747575978,
2.72205867173254));
#240701=CARTESIAN_POINT('Ctrl Pts',(62.4517967325057,-6.41496131130642,
2.71978693462857));
#240702=CARTESIAN_POINT('Ctrl Pts',(62.4540103788123,-6.41716486079098,
2.71754411340758));
#240703=CARTESIAN_POINT('Ctrl Pts',(62.4561838467663,-6.41943986047008,
2.71533341844254));
#240704=CARTESIAN_POINT('Ctrl Pts',(62.4621489466212,-6.42568361494097,
2.70926614876401));
#240705=CARTESIAN_POINT('Ctrl Pts',(62.467772647785,-6.43248733059531,2.70347381860418));
#240706=CARTESIAN_POINT('Ctrl Pts',(62.4729574661287,-6.43981562609089,
2.69804914171404));
#240707=CARTESIAN_POINT('Ctrl Pts',(62.4777012934231,-6.44652061860733,
2.69308585687183));
#240708=CARTESIAN_POINT('Ctrl Pts',(62.4820661824991,-6.45366385825755,
2.68842799053136));
#240709=CARTESIAN_POINT('Ctrl Pts',(62.4859635700134,-6.46124910257467,
2.68414767054146));
#240710=CARTESIAN_POINT('Ctrl Pts',(62.4878779540287,-6.46497494980425,
2.6820451913451));
#240711=CARTESIAN_POINT('Ctrl Pts',(62.4896790353534,-6.46880749650892,
2.68003431778487));
#240712=CARTESIAN_POINT('Ctrl Pts',(62.4913529701965,-6.47274712615468,
2.67812693945262));
#240713=CARTESIAN_POINT('Ctrl Pts',(62.4916705830287,-6.47349463250756,
2.67776503299213));
#240714=CARTESIAN_POINT('Ctrl Pts',(62.491983428084,-6.47424649074084,2.67740659639934));
#240715=CARTESIAN_POINT('Ctrl Pts',(62.4922913974558,-6.47500261163056,
2.67705178968865));
#240716=CARTESIAN_POINT('Ctrl Pts',(62.4925897427849,-6.47573510374248,
2.67670807068768));
#240717=CARTESIAN_POINT('Ctrl Pts',(62.4928835124027,-6.47647159623243,
2.67636775825275));
#240718=CARTESIAN_POINT('Ctrl Pts',(62.4931726086302,-6.47721200416302,
2.67603099699265));
#240719=CARTESIAN_POINT('Ctrl Pts',(62.4963231197466,-6.4852808172255,2.67236104217154));
#240720=CARTESIAN_POINT('Ctrl Pts',(62.4989203081701,-6.4938200899481,2.66911440541513));
#240721=CARTESIAN_POINT('Ctrl Pts',(62.5008353965402,-6.50268949817166,
2.66646778189676));
#240722=CARTESIAN_POINT('Ctrl Pts',(62.5016441502512,-6.50643510434138,
2.66535009635005));
#240723=CARTESIAN_POINT('Ctrl Pts',(62.502331556834,-6.5102392704753,2.66433897912363));
#240724=CARTESIAN_POINT('Ctrl Pts',(62.5028895688031,-6.51409041329186,
2.66344564884803));
#240725=CARTESIAN_POINT('Ctrl Pts',(62.5038292470156,-6.52057564156468,
2.66194130298595));
#240726=CARTESIAN_POINT('Ctrl Pts',(62.5043999463278,-6.5271925931368,2.66077206705429));
#240727=CARTESIAN_POINT('Ctrl Pts',(62.5045608969644,-6.53387925273503,
2.65998225155723));
#240728=CARTESIAN_POINT('Ctrl Pts',(62.5046011346236,-6.53555091763458,
2.65978479768296));
#240729=CARTESIAN_POINT('Ctrl Pts',(62.5046155292217,-6.53722692958711,
2.65961098966631));
#240730=CARTESIAN_POINT('Ctrl Pts',(62.5046031362658,-6.53890629460977,
2.6594613903051));
#240731=CARTESIAN_POINT('Ctrl Pts',(62.5045845468319,-6.54142534214377,
2.65923699126329));
#240732=CARTESIAN_POINT('Ctrl Pts',(62.5045056736598,-6.54395191714411,
2.6590670756245));
#240733=CARTESIAN_POINT('Ctrl Pts',(62.5043649998326,-6.54648282201769,
2.65895332562928));
#240734=CARTESIAN_POINT('Ctrl Pts',(62.5042243260054,-6.54901372689127,
2.65883957563406));
#240735=CARTESIAN_POINT('Ctrl Pts',(62.5040218613862,-6.55154895552156,
2.65878198860258));
#240736=CARTESIAN_POINT('Ctrl Pts',(62.5037563256536,-6.55408556365842,
2.65878198860258));
#240737=CARTESIAN_POINT('Ctrl Pts',(58.7067819056644,-6.15500747092217,
2.65878198860258));
#240738=CARTESIAN_POINT('Ctrl Pts',(58.7076801645418,-6.14642434678064,
2.65878198860258));
#240739=CARTESIAN_POINT('Ctrl Pts',(58.7092791387969,-6.13798976646243,
2.65945335517854));
#240740=CARTESIAN_POINT('Ctrl Pts',(58.7114824462542,-6.12982011300116,
2.66072561226605));
#240741=CARTESIAN_POINT('Ctrl Pts',(58.7129055567992,-6.12454335512034,
2.66154735980342));
#240742=CARTESIAN_POINT('Ctrl Pts',(58.7145798848071,-6.1193768666793,2.66261895766884));
#240743=CARTESIAN_POINT('Ctrl Pts',(58.7164715618025,-6.11434800669237,
2.66391429251023));
#240744=CARTESIAN_POINT('Ctrl Pts',(58.7189788712982,-6.10768254085036,
2.6656311846412));
#240745=CARTESIAN_POINT('Ctrl Pts',(58.7218729180382,-6.10126195983141,
2.66774105138695));
#240746=CARTESIAN_POINT('Ctrl Pts',(58.7250866612027,-6.09514640967174,
2.67016894181746));
#240747=CARTESIAN_POINT('Ctrl Pts',(58.7266935327849,-6.09208863459191,
2.67138288703272));
#240748=CARTESIAN_POINT('Ctrl Pts',(58.7283803475667,-6.08910691884873,
2.67267613167548));
#240749=CARTESIAN_POINT('Ctrl Pts',(58.7301388657774,-6.08620737357365,
2.6740383543255));
#240750=CARTESIAN_POINT('Ctrl Pts',(58.7310181248828,-6.08475760093612,
2.67471946565051));
#240751=CARTESIAN_POINT('Ctrl Pts',(58.7319153115143,-6.08332835456944,
2.6754178138952));
#240752=CARTESIAN_POINT('Ctrl Pts',(58.7328294060528,-6.08192029572471,
2.67613207244166));
#240753=CARTESIAN_POINT('Ctrl Pts',(58.7330579296874,-6.08156828101352,
2.67631063707827));
#240754=CARTESIAN_POINT('Ctrl Pts',(58.7332875101007,-6.08121759017468,
2.67649019601842));
#240755=CARTESIAN_POINT('Ctrl Pts',(58.7335181314302,-6.08086823283881,
2.67667072836654));
#240756=CARTESIAN_POINT('Ctrl Pts',(58.7342099954187,-6.0798201608312,2.67721232541088));
#240757=CARTESIAN_POINT('Ctrl Pts',(58.7349112274886,-6.07878409208678,
2.67776268340044));
#240758=CARTESIAN_POINT('Ctrl Pts',(58.7356214008386,-6.07776027111619,
2.67832123541513));
#240759=CARTESIAN_POINT('Ctrl Pts',(58.7406237702162,-6.07054860839873,
2.68225560368441));
#240760=CARTESIAN_POINT('Ctrl Pts',(58.7460508958012,-6.06389424687424,
2.68661792998885));
#240761=CARTESIAN_POINT('Ctrl Pts',(58.7517849266679,-6.05777649745733,
2.69130986622574));
#240762=CARTESIAN_POINT('Ctrl Pts',(58.7545659254421,-6.05480939560099,
2.69358545023051));
#240763=CARTESIAN_POINT('Ctrl Pts',(58.7574196937449,-6.05196853530496,
2.69593918853466));
#240764=CARTESIAN_POINT('Ctrl Pts',(58.7603356163932,-6.04925198282133,
2.69836306235472));
#240765=CARTESIAN_POINT('Ctrl Pts',(58.7647996902381,-6.04509313076893,
2.70207384382205));
#240766=CARTESIAN_POINT('Ctrl Pts',(58.7694062431512,-6.04122712576978,
2.70594760814205));
#240767=CARTESIAN_POINT('Ctrl Pts',(58.7741092696794,-6.03765709635735,
2.70995196345684));
#240768=CARTESIAN_POINT('Ctrl Pts',(58.7762933795293,-6.03599915622934,
2.71181160678082));
#240769=CARTESIAN_POINT('Ctrl Pts',(58.7784980841112,-6.03440490786023,
2.71369962772075));
#240770=CARTESIAN_POINT('Ctrl Pts',(58.7807192900658,-6.03287578462657,
2.71561183138637));
#240771=CARTESIAN_POINT('Ctrl Pts',(58.7808895367502,-6.03275858335576,
2.71575839426288));
#240772=CARTESIAN_POINT('Ctrl Pts',(58.7810598733266,-6.03264173148679,
2.71590508903186));
#240773=CARTESIAN_POINT('Ctrl Pts',(58.7812302983889,-6.0325252286245,2.71605191409888));
#240774=CARTESIAN_POINT('Ctrl Pts',(58.7836242566994,-6.03088871465405,
2.7181143636273));
#240775=CARTESIAN_POINT('Ctrl Pts',(58.7860369637878,-6.02932271154663,
2.72020091026936));
#240776=CARTESIAN_POINT('Ctrl Pts',(58.7884628208564,-6.02782611907157,
2.72230624862159));
#240777=CARTESIAN_POINT('Ctrl Pts',(58.7971615128805,-6.02245960461597,
2.72985561753093));
#240778=CARTESIAN_POINT('Ctrl Pts',(58.8060955050479,-6.01794242202224,
2.73770089914333));
#240779=CARTESIAN_POINT('Ctrl Pts',(58.8151732302901,-6.01418353044851,
2.74574823347091));
#240780=CARTESIAN_POINT('Ctrl Pts',(58.8251487383928,-6.01005288622314,
2.75459144547047));
#240781=CARTESIAN_POINT('Ctrl Pts',(58.8352983536258,-6.00683754300114,
2.76367911754297));
#240782=CARTESIAN_POINT('Ctrl Pts',(58.845534016615,-6.00445775272896,2.77292162564759));
#240783=CARTESIAN_POINT('Ctrl Pts',(58.8565859638426,-6.00188817648084,
2.78290121484763));
#240784=CARTESIAN_POINT('Ctrl Pts',(58.8677393147039,-6.00029231631069,
2.79306229500219));
#240785=CARTESIAN_POINT('Ctrl Pts',(58.8789072188679,-5.99962196122044,
2.80331916685283));
#240786=CARTESIAN_POINT('Ctrl Pts',(58.8899814357904,-5.99895722972064,
2.81348999408712));
#240787=CARTESIAN_POINT('Ctrl Pts',(58.9010713848516,-5.99920273697601,
2.82375635966883));
#240788=CARTESIAN_POINT('Ctrl Pts',(58.9120953679531,-6.00036140428947,
2.83404198860258));
#240789=CARTESIAN_POINT('Origin',(-0.00159301378019881,-0.0151565136852225,
2.83404198860262));
#240790=CARTESIAN_POINT('Ctrl Pts',(62.5005702980932,-6.58439859102925,
2.65878198860258));
#240791=CARTESIAN_POINT('Ctrl Pts',(62.4996689377206,-6.59294009787341,
2.65878198860258));
#240792=CARTESIAN_POINT('Ctrl Pts',(62.4980620716938,-6.60133040498934,
2.65944603041841));
#240793=CARTESIAN_POINT('Ctrl Pts',(62.4958483879906,-6.60945539386065,
2.6607043926405));
#240794=CARTESIAN_POINT('Ctrl Pts',(62.4944339494873,-6.61464687495722,
2.66150842619576));
#240795=CARTESIAN_POINT('Ctrl Pts',(62.4927726671884,-6.61973030386238,
2.66255428265352));
#240796=CARTESIAN_POINT('Ctrl Pts',(62.4908979342377,-6.62467983150659,
2.66381699700646));
#240797=CARTESIAN_POINT('Ctrl Pts',(62.4883392999284,-6.63143494360989,
2.66554034873245));
#240798=CARTESIAN_POINT('Ctrl Pts',(62.4853780106448,-6.63793726713659,
2.6676675964395));
#240799=CARTESIAN_POINT('Ctrl Pts',(62.482086456285,-6.6441242645479,2.67012012783126));
#240800=CARTESIAN_POINT('Ctrl Pts',(62.4804406791051,-6.64721776325356,
2.67134639352714));
#240801=CARTESIAN_POINT('Ctrl Pts',(62.4787123157335,-6.65023263831771,
2.6726537558499));
#240802=CARTESIAN_POINT('Ctrl Pts',(62.4769102669531,-6.65316255786638,
2.67403135126918));
#240803=CARTESIAN_POINT('Ctrl Pts',(62.476009242563,-6.65462751764071,2.67472014897882));
#240804=CARTESIAN_POINT('Ctrl Pts',(62.4750897950507,-6.65607125585979,
2.67542649668611));
#240805=CARTESIAN_POINT('Ctrl Pts',(62.474153026021,-6.65749308991659,2.6761489965608));
#240806=CARTESIAN_POINT('Ctrl Pts',(62.4739188337636,-6.65784854843079,
2.67632962152947));
#240807=CARTESIAN_POINT('Ctrl Pts',(62.4736835588747,-6.65820263830401,
2.67651125590929));
#240808=CARTESIAN_POINT('Ctrl Pts',(62.4734472184934,-6.65855534961512,
2.67669387767502));
#240809=CARTESIAN_POINT('Ctrl Pts',(62.4727381973496,-6.65961348354846,
2.67724174297222));
#240810=CARTESIAN_POINT('Ctrl Pts',(62.4720195869493,-6.66065920857905,
2.67779849504726));
#240811=CARTESIAN_POINT('Ctrl Pts',(62.4712918484711,-6.66169227331115,
2.67836353617988));
#240812=CARTESIAN_POINT('Ctrl Pts',(62.4662627240579,-6.66883139158019,
2.68226832098884));
#240813=CARTESIAN_POINT('Ctrl Pts',(62.4608161451511,-6.67541846632554,
2.68659153751365));
#240814=CARTESIAN_POINT('Ctrl Pts',(62.4550686189992,-6.68147667711015,
2.69123699486149));
#240815=CARTESIAN_POINT('Ctrl Pts',(62.4522121142783,-6.68448759124072,
2.6935457744119));
#240816=CARTESIAN_POINT('Ctrl Pts',(62.4492806638355,-6.68736784133507,
2.69593478828094));
#240817=CARTESIAN_POINT('Ctrl Pts',(62.4462854590369,-6.69011973548505,
2.69839565261199));
#240818=CARTESIAN_POINT('Ctrl Pts',(62.4396775898762,-6.69619082501318,
2.70382468689024));
#240819=CARTESIAN_POINT('Ctrl Pts',(62.4327685320937,-6.70164568781112,
2.70961155815066));
#240820=CARTESIAN_POINT('Ctrl Pts',(62.4256985108779,-6.7064460603899,2.71562701361746));
#240821=CARTESIAN_POINT('Ctrl Pts',(62.4231157429702,-6.70819969702881,
2.71782453535837));
#240822=CARTESIAN_POINT('Ctrl Pts',(62.4205129446134,-6.70987381569712,
2.72005051502381));
#240823=CARTESIAN_POINT('Ctrl Pts',(62.4178950590936,-6.71147036762072,
2.72229986760094));
#240824=CARTESIAN_POINT('Ctrl Pts',(62.4091018586485,-6.71683301659044,
2.72985520488873));
#240825=CARTESIAN_POINT('Ctrl Pts',(62.4000783072483,-6.7213473429662,2.73770845534544));
#240826=CARTESIAN_POINT('Ctrl Pts',(62.390915840586,-6.72510335397105,2.74576706701744));
#240827=CARTESIAN_POINT('Ctrl Pts',(62.3808452043586,-6.72923165499413,
2.75462443585026));
#240828=CARTESIAN_POINT('Ctrl Pts',(62.3706061896766,-6.7324442675611,2.76373036323186));
#240829=CARTESIAN_POINT('Ctrl Pts',(62.3602869763748,-6.73481930344685,
2.7729966463683));
#240830=CARTESIAN_POINT('Ctrl Pts',(62.3491727415056,-6.73737731885801,
2.78297683033495));
#240831=CARTESIAN_POINT('Ctrl Pts',(62.3379643502052,-6.73896413451793,
2.79314401478921));
#240832=CARTESIAN_POINT('Ctrl Pts',(62.3267489231093,-6.73962511499475,
2.80341452427971));
#240833=CARTESIAN_POINT('Ctrl Pts',(62.315684942148,-6.74027717000334,2.81354634721384));
#240834=CARTESIAN_POINT('Ctrl Pts',(62.3046126966245,-6.74002799825869,
2.82378004209211));
#240835=CARTESIAN_POINT('Ctrl Pts',(62.293614112757,-6.73887200051229,2.83404198860258));
#240836=CARTESIAN_POINT('Ctrl Pts',(58.8722700234481,-6.37927424642479,
2.83404198860258));
#240837=CARTESIAN_POINT('Ctrl Pts',(58.8617443183095,-6.37816795023556,
2.82422126443008));
#240838=CARTESIAN_POINT('Ctrl Pts',(58.8513437177781,-6.37623543038764,
2.81442815028507));
#240839=CARTESIAN_POINT('Ctrl Pts',(58.8411231047668,-6.37349561323622,
2.80471618166329));
#240840=CARTESIAN_POINT('Ctrl Pts',(58.8312542036553,-6.37085007871684,
2.79533842146247));
#240841=CARTESIAN_POINT('Ctrl Pts',(58.8215519162598,-6.36745144954003,
2.78603515650264));
#240842=CARTESIAN_POINT('Ctrl Pts',(58.8120753594642,-6.36327195218565,
2.77685887346786));
#240843=CARTESIAN_POINT('Ctrl Pts',(58.8031170454187,-6.35932101824826,
2.76818441216615));
#240844=CARTESIAN_POINT('Ctrl Pts',(58.7943596215167,-6.35467192211794,
2.7596226152167));
#240845=CARTESIAN_POINT('Ctrl Pts',(58.7858758685307,-6.34926600747485,
2.75123537701714));
#240846=CARTESIAN_POINT('Ctrl Pts',(58.7780624743562,-6.34428725077959,
2.74351087134184));
#240847=CARTESIAN_POINT('Ctrl Pts',(58.7704807832448,-6.33866621241268,
2.73593399449922));
#240848=CARTESIAN_POINT('Ctrl Pts',(58.7632157809005,-6.33233133084754,
2.72857657812661));
#240849=CARTESIAN_POINT('Ctrl Pts',(58.7610495038554,-6.33044239704299,
2.72638274508373));
#240850=CARTESIAN_POINT('Ctrl Pts',(58.7589116098636,-6.32848982621416,
2.72420861709617));
#240851=CARTESIAN_POINT('Ctrl Pts',(58.7568049797265,-6.32647128889738,
2.72205663736704));
#240852=CARTESIAN_POINT('Ctrl Pts',(58.7547198741578,-6.32447337605752,
2.71992664556743));
#240853=CARTESIAN_POINT('Ctrl Pts',(58.7526673708734,-6.32241310885625,
2.71782089927861));
#240854=CARTESIAN_POINT('Ctrl Pts',(58.7506524329181,-6.32029074540019,
2.71574387311223));
#240855=CARTESIAN_POINT('Ctrl Pts',(58.7505123180733,-6.32014316039614,
2.71559944077464));
#240856=CARTESIAN_POINT('Ctrl Pts',(58.7503723733987,-6.31999527850255,
2.71545515216046));
#240857=CARTESIAN_POINT('Ctrl Pts',(58.7502325999832,-6.31984709900125,
2.71531100781707));
#240858=CARTESIAN_POINT('Ctrl Pts',(58.7441044214169,-6.31335036684014,
2.70899119176064));
#240859=CARTESIAN_POINT('Ctrl Pts',(58.7383447881643,-6.30625925377255,
2.70298296066821));
#240860=CARTESIAN_POINT('Ctrl Pts',(58.7330687140844,-6.29859016886859,
2.69736727774122));
#240861=CARTESIAN_POINT('Ctrl Pts',(58.7281504960664,-6.29144124886016,
2.69213248525417));
#240862=CARTESIAN_POINT('Ctrl Pts',(58.7236522470779,-6.28378931332989,
2.68723866185458));
#240863=CARTESIAN_POINT('Ctrl Pts',(58.7196964823232,-6.27564783709128,
2.68278595829554));
#240864=CARTESIAN_POINT('Ctrl Pts',(58.7182494123992,-6.27266957975491,
2.68115710172791));
#240865=CARTESIAN_POINT('Ctrl Pts',(58.7168752520899,-6.2696258693364,2.67958763637791));
#240866=CARTESIAN_POINT('Ctrl Pts',(58.7155811795665,-6.26651766855652,
2.67808378645341));
#240867=CARTESIAN_POINT('Ctrl Pts',(58.7152699983558,-6.26577025010479,
2.67772216078576));
#240868=CARTESIAN_POINT('Ctrl Pts',(58.7149635750523,-6.26501853257339,
2.67736403603539));
#240869=CARTESIAN_POINT('Ctrl Pts',(58.7146620123682,-6.26426260461741,
2.67700956934455));
#240870=CARTESIAN_POINT('Ctrl Pts',(58.7143698735179,-6.26353029941006,
2.6766661797378));
#240871=CARTESIAN_POINT('Ctrl Pts',(58.7140822962415,-6.26279404284275,
2.67632622314095));
#240872=CARTESIAN_POINT('Ctrl Pts',(58.7137993735012,-6.26205391928359,
2.67598984158749));
#240873=CARTESIAN_POINT('Ctrl Pts',(58.7106996279153,-6.25394501035143,
2.67230439292196));
#240874=CARTESIAN_POINT('Ctrl Pts',(58.70815694202,-6.24536644325852,2.66904964539949));
#240875=CARTESIAN_POINT('Ctrl Pts',(58.7062958387084,-6.23645973859584,
2.66640203566698));
#240876=CARTESIAN_POINT('Ctrl Pts',(58.7055239836916,-6.23276586269187,
2.66530399299414));
#240877=CARTESIAN_POINT('Ctrl Pts',(58.7048690642116,-6.22901585349446,
2.66430995142234));
#240878=CARTESIAN_POINT('Ctrl Pts',(58.7043384037135,-6.225220762677,2.66343053473336));
#240879=CARTESIAN_POINT('Ctrl Pts',(58.7034333069352,-6.21874783981136,
2.66193059792859));
#240880=CARTESIAN_POINT('Ctrl Pts',(58.7028917011006,-6.21214524099463,
2.66076519817102));
#240881=CARTESIAN_POINT('Ctrl Pts',(58.7027523988018,-6.20547453341974,
2.65997805604434));
#240882=CARTESIAN_POINT('Ctrl Pts',(58.7026827476524,-6.2021391796323,2.659584484981));
#240883=CARTESIAN_POINT('Ctrl Pts',(58.7027151167905,-6.19878688248268,
2.65928526260736));
#240884=CARTESIAN_POINT('Ctrl Pts',(58.7028544030466,-6.19542538554926,
2.65908463971298));
#240885=CARTESIAN_POINT('Ctrl Pts',(58.7029936893027,-6.19206388861583,
2.6588840168186));
#240886=CARTESIAN_POINT('Ctrl Pts',(58.7032398710656,-6.18869323212117,
2.65878198860258));
#240887=CARTESIAN_POINT('Ctrl Pts',(58.703595878104,-6.185320498293,2.65878198860258));
#240888=CARTESIAN_POINT('Origin',(61.0544000815099,6.7363249086374,3.56647653909516));
#240889=CARTESIAN_POINT('Origin',(61.0983782637164,6.740999176878,3.64299466007777));
#240890=CARTESIAN_POINT('Origin',(60.9730100652054,6.72777047351143,3.42473028058489));
#240891=CARTESIAN_POINT('Ctrl Pts',(60.8636883187845,6.71570789669429,3.48823028058489));
#240892=CARTESIAN_POINT('Ctrl Pts',(60.8773920302461,6.59002106156485,3.48794691941605));
#240893=CARTESIAN_POINT('Ctrl Pts',(60.9862851800404,6.60146619279966,3.4247302805849));
#240894=CARTESIAN_POINT('Ctrl Pts',(60.818916972731,6.711118718498,3.4102800592509));
#240895=CARTESIAN_POINT('Ctrl Pts',(60.8324022194115,6.58529244190214,3.40982512230983));
#240896=CARTESIAN_POINT('Ctrl Pts',(60.9191469903166,6.59440968471161,3.30780486372849));
#240897=CARTESIAN_POINT('Ctrl Pts',(60.7340977611529,6.70242508976221,3.36123028058486));
#240898=CARTESIAN_POINT('Ctrl Pts',(60.7472645033903,6.57634410736716,3.36099721048503));
#240899=CARTESIAN_POINT('Ctrl Pts',(60.7919547682788,6.58104124348259,3.23423045308447));
#240900=CARTESIAN_POINT('Ctrl Pts',(60.6448574988554,6.69328024897474,3.36123028058487));
#240901=CARTESIAN_POINT('Ctrl Pts',(60.6581326136904,6.56697596826297,3.36123028058487));
#240902=CARTESIAN_POINT('Ctrl Pts',(60.6581326136904,6.56697596826297,3.23423028058486));
#240903=CARTESIAN_POINT('Origin',(60.6448574988554,6.69328024897474,3.23423028058487));
#240904=CARTESIAN_POINT('Origin',(-0.0331877870874745,0.315760701779611,
3.64303198860263));
#240905=CARTESIAN_POINT('Origin',(61.4975385923862,6.78290064323579,3.64303198860268));
#240906=CARTESIAN_POINT('Origin',(-0.0331877870874745,0.315760701779613,
3.23423028058482));
#240907=CARTESIAN_POINT('Origin',(60.4944777170594,6.67747469700965,3.23423028058487));
#240908=CARTESIAN_POINT('Ctrl Pts',(62.0330459552232,6.83973663030279,3.47153072139077));
#240909=CARTESIAN_POINT('Ctrl Pts',(62.0468640234019,6.71274550335245,3.47182327902667));
#240910=CARTESIAN_POINT('Ctrl Pts',(61.9391074687686,6.70161199370844,3.40413028959037));
#240911=CARTESIAN_POINT('Ctrl Pts',(61.9187065474465,6.82760205123589,3.65553807120964));
#240912=CARTESIAN_POINT('Ctrl Pts',(61.9323544653024,6.7007103254433,3.65586275496912));
#240913=CARTESIAN_POINT('Ctrl Pts',(61.847659827901,6.6920004592179,3.5512812683724));
#240914=CARTESIAN_POINT('Ctrl Pts',(61.7133000470646,6.80580199871493,3.77003198860268));
#240915=CARTESIAN_POINT('Ctrl Pts',(61.7268034525367,6.67910652125837,3.77025505748527));
#240916=CARTESIAN_POINT('Ctrl Pts',(61.683377859151,6.67473372828961,3.64284211731182));
#240917=CARTESIAN_POINT('Ctrl Pts',(61.4975385923862,6.78290064323579,3.77003198860269));
#240918=CARTESIAN_POINT('Ctrl Pts',(61.5108335396272,6.65640766978549,3.77003198860269));
#240919=CARTESIAN_POINT('Ctrl Pts',(61.510813692429,6.65659650326271,3.64284239821713));
#240920=CARTESIAN_POINT('Origin',(61.9259926140919,6.82793297553368,3.40423097483315));
#240921=CARTESIAN_POINT('Ctrl Pts',(60.4944777170594,6.67747469700965,3.36123028058487));
#240922=CARTESIAN_POINT('Ctrl Pts',(60.5077528318944,6.55117041629788,3.36123028058486));
#240923=CARTESIAN_POINT('Ctrl Pts',(60.5077528318944,6.55117041629788,3.23423028058486));
#240924=CARTESIAN_POINT('Ctrl Pts',(60.4049357747551,6.66829952659943,3.36123028058487));
#240925=CARTESIAN_POINT('Ctrl Pts',(60.4181493202572,6.54175270773023,3.36146538610217));
#240926=CARTESIAN_POINT('Ctrl Pts',(60.3734783767964,6.53705760237909,3.23423043688484));
#240927=CARTESIAN_POINT('Ctrl Pts',(60.3202668847283,6.65962554481729,3.41054258693106));
#240928=CARTESIAN_POINT('Ctrl Pts',(60.3338524728743,6.53289275205003,3.41100608859737));
#240929=CARTESIAN_POINT('Ctrl Pts',(60.2465123062132,6.52371293062576,3.30819866970803));
#240930=CARTESIAN_POINT('Ctrl Pts',(60.2756459899119,6.65505462397414,3.48823028058486));
#240931=CARTESIAN_POINT('Ctrl Pts',(60.2894805317162,6.52822907310797,3.48852004212264));
#240932=CARTESIAN_POINT('Ctrl Pts',(60.1796001951995,6.51668018436765,3.42473028058485));
#240933=CARTESIAN_POINT('Origin',(60.1663250803646,6.64298446507942,3.42473028058486));
#240934=CARTESIAN_POINT('Origin',(62.1031658061134,6.84655462836832,3.11913648178332));
#240935=CARTESIAN_POINT('Origin',(62.2803389979219,6.86517628122529,2.83404198860267));
#240936=CARTESIAN_POINT('Origin',(60.0854204576116,6.63448104656903,3.56563113460833));
#240937=CARTESIAN_POINT('Origin',(60.0409538388298,6.62985850077833,3.6429917172181));
#240938=CARTESIAN_POINT('Ctrl Pts',(62.6076796697354,6.59568250079905,2.59908173516028));
#240939=CARTESIAN_POINT('Ctrl Pts',(62.5705801176609,6.59177408464793,2.65878198860267));
#240940=CARTESIAN_POINT('Ctrl Pts',(62.5005702980931,6.58439859103048,2.65878198860267));
#240941=CARTESIAN_POINT('Ctrl Pts',(62.5984477290791,6.68331293653946,2.59908193475784));
#240942=CARTESIAN_POINT('Ctrl Pts',(62.5638523220891,6.65560500345248,2.65878715325336));
#240943=CARTESIAN_POINT('Ctrl Pts',(62.4952175264233,6.63512154272615,2.65878198860267));
#240944=CARTESIAN_POINT('Ctrl Pts',(62.5650504549418,6.76155265492292,2.63878778849877));
#240945=CARTESIAN_POINT('Ctrl Pts',(62.5346567608587,6.71196843232436,2.69564460180128));
#240946=CARTESIAN_POINT('Ctrl Pts',(62.4653998062676,6.67930776339589,2.68180481624896));
#240947=CARTESIAN_POINT('Ctrl Pts',(62.4816328770701,6.86003002196278,2.7544323887865));
#240948=CARTESIAN_POINT('Ctrl Pts',(62.4676069047243,6.76863258245059,2.79268340777084));
#240949=CARTESIAN_POINT('Ctrl Pts',(62.3866783619496,6.73311104631474,2.74885926835607));
#240950=CARTESIAN_POINT('Ctrl Pts',(62.4326191774618,6.88172985342194,2.82856655361678));
#240951=CARTESIAN_POINT('Ctrl Pts',(62.4292062449152,6.76853939445046,2.85384197230682));
#240952=CARTESIAN_POINT('Ctrl Pts',(62.3388388123819,6.74362530798272,2.79184624278386));
#240953=CARTESIAN_POINT('Ctrl Pts',(62.3873926810691,6.87697683366584,2.9013417351603));
#240954=CARTESIAN_POINT('Ctrl Pts',(62.4011871104969,6.75017837817621,2.90163218716397));
#240955=CARTESIAN_POINT('Ctrl Pts',(62.2936141127569,6.73887200051352,2.83404198860268));
#240956=CARTESIAN_POINT('Origin',(62.5005702980931,6.58439859103048,2.53178198860267));
#240957=CARTESIAN_POINT('Origin',(-0.0331877870874745,0.315760701779611,
3.64303198860263));
#240958=CARTESIAN_POINT('Origin',(59.6417962403143,6.58785426247114,3.64303198860268));
#240959=CARTESIAN_POINT('Origin',(5.50069060731754E-15,1.85865314505527E-13,
2.53178198860262));
#240960=CARTESIAN_POINT('Origin',(62.5037563256535,6.55408556365965,2.53178198860267));
#240961=CARTESIAN_POINT('Ctrl Pts',(59.6417962403143,6.58785426247114,3.77003198860268));
#240962=CARTESIAN_POINT('Ctrl Pts',(59.6550912418708,6.46136077224306,3.77003198860268));
#240963=CARTESIAN_POINT('Ctrl Pts',(59.655071340276,6.46155012326943,3.64284187937014));
#240964=CARTESIAN_POINT('Ctrl Pts',(59.4260321009469,6.56494565834894,3.77003198860269));
#240965=CARTESIAN_POINT('Ctrl Pts',(59.4394927947744,6.43870097938004,3.76980208963001));
#240966=CARTESIAN_POINT('Ctrl Pts',(59.4825041216653,6.44341257746694,3.64284193928327));
#240967=CARTESIAN_POINT('Ctrl Pts',(59.2206282517276,6.54313468201947,3.65553535416592));
#240968=CARTESIAN_POINT('Ctrl Pts',(59.2341955513569,6.41712387095898,3.6552005783454));
#240969=CARTESIAN_POINT('Ctrl Pts',(59.3182233753696,6.42614597500995,3.55127910964209));
#240970=CARTESIAN_POINT('Ctrl Pts',(59.1062911958296,6.53099325080074,3.47153072139077));
#240971=CARTESIAN_POINT('Ctrl Pts',(59.1200087130389,6.40512262640546,3.47122746281587));
#240972=CARTESIAN_POINT('Ctrl Pts',(59.2267768553867,6.41653455832048,3.40413045901259));
#240973=CARTESIAN_POINT('Origin',(59.2133417798936,6.54282188406246,3.40423097483315));
#240974=CARTESIAN_POINT('Ctrl Pts',(62.4538823482275,6.24436990788079,2.90134173516029));
#240975=CARTESIAN_POINT('Ctrl Pts',(62.4410124550018,6.3712655360409,2.90163218716396));
#240976=CARTESIAN_POINT('Ctrl Pts',(62.3334394572619,6.35995915837821,2.83404198860267));
#240977=CARTESIAN_POINT('Ctrl Pts',(62.4991292864731,6.24912604340928,2.82853349835366));
#240978=CARTESIAN_POINT('Ctrl Pts',(62.4722545055307,6.35912437831578,2.85381483162363));
#240979=CARTESIAN_POINT('Ctrl Pts',(62.3786847639679,6.3647146317389,2.79182701594255));
#240980=CARTESIAN_POINT('Ctrl Pts',(62.5423796567684,6.28053011789759,2.75468822073642));
#240981=CARTESIAN_POINT('Ctrl Pts',(62.509694696565,6.36708533499915,2.79286913083882));
#240982=CARTESIAN_POINT('Ctrl Pts',(62.4231124872028,6.38493060453726,2.74900763297914));
#240983=CARTESIAN_POINT('Ctrl Pts',(62.6032845425345,6.39322569848906,2.63954450640404));
#240984=CARTESIAN_POINT('Ctrl Pts',(62.5632890102007,6.43576006824464,2.69627684028838));
#240985=CARTESIAN_POINT('Ctrl Pts',(62.4886705126496,6.45334792019217,2.682243560365));
#240986=CARTESIAN_POINT('Ctrl Pts',(62.6200908675645,6.47739243510505,2.59908178706469));
#240987=CARTESIAN_POINT('Ctrl Pts',(62.5804859237117,6.49734694408369,2.65878704321546));
#240988=CARTESIAN_POINT('Ctrl Pts',(62.5090840872014,6.50319024212522,2.65878198860267));
#240989=CARTESIAN_POINT('Ctrl Pts',(62.6108711573006,6.56531752495321,2.59908173516028));
#240990=CARTESIAN_POINT('Ctrl Pts',(62.5737697140402,6.56142710223371,2.65878198860267));
#240991=CARTESIAN_POINT('Ctrl Pts',(62.5037563256535,6.55408556365965,2.65878198860267));
#240992=CARTESIAN_POINT('Origin',(62.3467145720969,6.23365487766644,2.83404198860265));
#240993=CARTESIAN_POINT('Origin',(59.0361683443304,6.52420020557803,3.11913648167145));
#240994=CARTESIAN_POINT('Origin',(58.858994908613,6.50557852713774,2.83404198860267));
#240995=CARTESIAN_POINT('Origin',(62.1695413802689,6.21503322485029,3.11913648177391));
#240996=CARTESIAN_POINT('Origin',(61.9923681882669,6.19641157197482,3.40423097483315));
#240997=CARTESIAN_POINT('Ctrl Pts',(58.7519447039088,6.49374646112759,2.90134173516028));
#240998=CARTESIAN_POINT('Ctrl Pts',(58.7656442740271,6.36806742857345,2.90103711553234));
#240999=CARTESIAN_POINT('Ctrl Pts',(58.872270023448,6.37927424642597,2.83404198860267));
#241000=CARTESIAN_POINT('Ctrl Pts',(58.7067576262547,6.48899657309085,2.82862991747966));
#241001=CARTESIAN_POINT('Ctrl Pts',(58.7342098038491,6.38004220452818,2.85314045886426));
#241002=CARTESIAN_POINT('Ctrl Pts',(58.8270810177598,6.37452469054069,2.79187960999899));
#241003=CARTESIAN_POINT('Ctrl Pts',(58.6637560248473,6.45774144355334,2.7547062579333));
#241004=CARTESIAN_POINT('Ctrl Pts',(58.6967899354326,6.3718711793815,2.79224250381907));
#241005=CARTESIAN_POINT('Ctrl Pts',(58.7829167175848,6.35435266912784,2.7490180910826));
#241006=CARTESIAN_POINT('Ctrl Pts',(58.6035914159081,6.3453990801634,2.63947868311704));
#241007=CARTESIAN_POINT('Ctrl Pts',(58.6436439608621,6.30313135363863,2.69595066767916));
#241008=CARTESIAN_POINT('Ctrl Pts',(58.7181337176191,6.28595874576536,2.6822053943607));
#241009=CARTESIAN_POINT('Ctrl Pts',(58.5872698677167,6.2615101002574,2.5990817858507));
#241010=CARTESIAN_POINT('Ctrl Pts',(58.626864594668,6.24170554357551,2.6587767094479));
#241011=CARTESIAN_POINT('Ctrl Pts',(58.6982323944353,6.23613328458279,2.65878198860267));
#241012=CARTESIAN_POINT('Ctrl Pts',(58.5964866834551,6.17403490859039,2.59908173516029));
#241013=CARTESIAN_POINT('Ctrl Pts',(58.6335861742242,6.17794390662191,2.65878198860267));
#241014=CARTESIAN_POINT('Ctrl Pts',(58.7035958781039,6.18532049829418,2.65878198860267));
#241015=CARTESIAN_POINT('Origin',(58.7035958781039,6.18532049829418,2.53178198860267));
#241016=CARTESIAN_POINT('Ctrl Pts',(61.5639141665612,6.15137923967694,3.77003198860268));
#241017=CARTESIAN_POINT('Ctrl Pts',(61.5506192181748,6.27787222402466,3.77003198860268));
#241018=CARTESIAN_POINT('Ctrl Pts',(61.5506390665201,6.27768337963378,3.64284238727605));
#241019=CARTESIAN_POINT('Ctrl Pts',(61.7797255331386,6.17383801205373,3.77003198860268));
#241020=CARTESIAN_POINT('Ctrl Pts',(61.7665923920123,6.30057242039952,3.77025506105794));
#241021=CARTESIAN_POINT('Ctrl Pts',(61.7232059145523,6.29582088597906,3.64284210641878));
#241022=CARTESIAN_POINT('Ctrl Pts',(61.9851742714891,6.19522058691261,3.65553527987838));
#241023=CARTESIAN_POINT('Ctrl Pts',(61.9721416759924,6.3221769985454,3.65585996533047));
#241024=CARTESIAN_POINT('Ctrl Pts',(61.8874865820178,6.31308747966704,3.55127902710209));
#241025=CARTESIAN_POINT('Ctrl Pts',(62.0995362748659,6.20712349654482,3.47153072139077));
#241026=CARTESIAN_POINT('Ctrl Pts',(62.086649444066,6.33421251157719,3.47182327905194));
#241027=CARTESIAN_POINT('Ctrl Pts',(61.9789328337399,6.32269886789189,3.40413028377994));
#241028=CARTESIAN_POINT('Origin',(61.5639141665612,6.15137923967694,3.64303198860268));
#241029=CARTESIAN_POINT('Origin',(5.72301283402738E-15,1.86330858203059E-13,
2.53178198860262));
#241030=CARTESIAN_POINT('Origin',(58.7067819056643,6.15500747092335,2.53178198860267));
#241031=CARTESIAN_POINT('Origin',(61.5757885448747,6.15262728712883,3.64303198860268));
#241032=CARTESIAN_POINT('Origin',(61.1647646440466,6.10937495962146,3.64299466007718));
#241033=CARTESIAN_POINT('Ctrl Pts',(58.5996668978648,6.14377718965341,2.59908173516029));
#241034=CARTESIAN_POINT('Ctrl Pts',(58.6367684021392,6.1476670304619,2.65878198860267));
#241035=CARTESIAN_POINT('Ctrl Pts',(58.7067819056643,6.15500747092335,2.65878198860267));
#241036=CARTESIAN_POINT('Ctrl Pts',(58.6088074259633,6.05659553606724,2.59908193199912));
#241037=CARTESIAN_POINT('Ctrl Pts',(58.6434243604386,6.08415140319833,2.65877685806568));
#241038=CARTESIAN_POINT('Ctrl Pts',(58.7120821529696,6.10436324506841,2.65878198860267));
#241039=CARTESIAN_POINT('Ctrl Pts',(58.6416817365139,5.97852000021532,2.63872492669802));
#241040=CARTESIAN_POINT('Ctrl Pts',(58.6721826510715,6.0278583913126,2.69532212015282));
#241041=CARTESIAN_POINT('Ctrl Pts',(58.7414038195495,6.06008468706708,2.68176836726643));
#241042=CARTESIAN_POINT('Ctrl Pts',(58.7242744516464,5.88025093392496,2.75442176402255));
#241043=CARTESIAN_POINT('Ctrl Pts',(58.738786069515,5.97104363802187,2.7920317992014));
#241044=CARTESIAN_POINT('Ctrl Pts',(58.8193360415244,6.00614981441045,2.74885310748176));
#241045=CARTESIAN_POINT('Ctrl Pts',(58.7730316211507,5.85862682030293,2.82866089558402));
#241046=CARTESIAN_POINT('Ctrl Pts',(58.7772266151797,5.97091547255876,2.85316563119283));
#241047=CARTESIAN_POINT('Ctrl Pts',(58.866925555678,5.99561386571439,2.79189751796684));
#241048=CARTESIAN_POINT('Ctrl Pts',(58.8181995570485,5.86337364149599,2.90134173516028));
#241049=CARTESIAN_POINT('Ctrl Pts',(58.805469618532,5.98915458643813,2.90103711553234));
#241050=CARTESIAN_POINT('Ctrl Pts',(58.912095367953,6.00036140429066,2.83404198860266));
#241051=CARTESIAN_POINT('Origin',(58.925370482788,5.87405712357889,2.83404198860266));
#241052=CARTESIAN_POINT('Origin',(61.1207756545816,6.10480350526345,3.56647653971745));
#241053=CARTESIAN_POINT('Origin',(61.0393856393804,6.09624906995258,3.4247302805849));
#241054=CARTESIAN_POINT('Origin',(59.1025439184834,5.89267880207675,3.11913648168135));
#241055=CARTESIAN_POINT('Origin',(59.2797173540686,5.91130048050361,3.40423097483316));
#241056=CARTESIAN_POINT('Ctrl Pts',(60.7112330730304,6.06175884541589,3.36123028058486));
#241057=CARTESIAN_POINT('Ctrl Pts',(60.6979579581954,6.18806312612766,3.36123028058486));
#241058=CARTESIAN_POINT('Ctrl Pts',(60.6979579581954,6.18806312612766,3.23423028058486));
#241059=CARTESIAN_POINT('Ctrl Pts',(60.8007259828526,6.07140041118264,3.36123028058486));
#241060=CARTESIAN_POINT('Ctrl Pts',(60.7873912833627,6.19746294737676,3.36099641108536));
#241061=CARTESIAN_POINT('Ctrl Pts',(60.8322324012627,6.20217593878197,3.23423043688433));
#241062=CARTESIAN_POINT('Ctrl Pts',(60.885348460727,6.0805154206754,3.4105425890529));
#241063=CARTESIAN_POINT('Ctrl Pts',(60.8723790316482,6.20639551966689,3.41008815825971));
#241064=CARTESIAN_POINT('Ctrl Pts',(60.9591984396287,6.21552060714914,3.30819867304265));
#241065=CARTESIAN_POINT('Ctrl Pts',(60.929944884669,6.08531878138339,3.48823028058488));
#241066=CARTESIAN_POINT('Ctrl Pts',(60.917217374751,6.21110821942954,3.48794691941605));
#241067=CARTESIAN_POINT('Ctrl Pts',(61.0261105245454,6.22255335066434,3.42473028058489));
#241068=CARTESIAN_POINT('Origin',(60.7112330730304,6.06175884541589,3.23423028058486));
#241069=CARTESIAN_POINT('Ctrl Pts',(59.1725467709677,5.90061356181275,3.47153072139077));
#241070=CARTESIAN_POINT('Ctrl Pts',(59.1597945546412,6.02658562874821,3.47122746285082));
#241071=CARTESIAN_POINT('Ctrl Pts',(59.2666022171587,6.0376214331677,3.40413046676795));
#241072=CARTESIAN_POINT('Ctrl Pts',(59.2869113614505,5.91250964036482,3.65553813457993));
#241073=CARTESIAN_POINT('Ctrl Pts',(59.2739830624778,6.03858760028864,3.65520336072117));
#241074=CARTESIAN_POINT('Ctrl Pts',(59.358050121575,6.04723299508908,3.55128134519901));
#241075=CARTESIAN_POINT('Ctrl Pts',(59.4923630227875,5.93388131656907,3.77003198860267));
#241076=CARTESIAN_POINT('Ctrl Pts',(59.4792818168371,6.06016587018187,3.76980209314199));
#241077=CARTESIAN_POINT('Ctrl Pts',(59.5223321697727,6.0644997338841,3.64284195387436));
#241078=CARTESIAN_POINT('Ctrl Pts',(59.7081718144892,5.95633285891229,3.77003198860268));
#241079=CARTESIAN_POINT('Ctrl Pts',(59.6948768144683,6.08282633453086,3.77003198860268));
#241080=CARTESIAN_POINT('Ctrl Pts',(59.6948967145252,6.08263699813584,3.64284189403812));
#241081=CARTESIAN_POINT('Origin',(59.7081718144892,5.95633285891229,3.64303198860268));
#241082=CARTESIAN_POINT('Origin',(60.0850508448141,5.99594444118226,3.23423028058486));
#241083=CARTESIAN_POINT('Origin',(60.5608532912343,6.0459532934508,3.23423028058486));
#241084=CARTESIAN_POINT('Origin',(59.851607889689,5.97140859790567,3.64303198860267));
#241085=CARTESIAN_POINT('Origin',(60.1073400339998,5.99823604520145,3.64299171721797));
#241086=CARTESIAN_POINT('Ctrl Pts',(60.3421421670675,6.02238575970294,3.48823028058486));
#241087=CARTESIAN_POINT('Ctrl Pts',(60.3293058762211,6.14931623097265,3.48852004212264));
#241088=CARTESIAN_POINT('Ctrl Pts',(60.2194255397045,6.13776734223234,3.42473028058486));
#241089=CARTESIAN_POINT('Ctrl Pts',(60.3868890390928,6.02720817145219,3.41028005848414));
#241090=CARTESIAN_POINT('Ctrl Pts',(60.373827809951,6.15399567476929,3.41074404220338));
#241091=CARTESIAN_POINT('Ctrl Pts',(60.2865637544299,6.14482385294816,3.30780486243867));
#241092=CARTESIAN_POINT('Ctrl Pts',(60.4716618705782,6.03634362557921,3.36123028058486));
#241093=CARTESIAN_POINT('Ctrl Pts',(60.4582762833197,6.16287156698257,3.36146460586438));
#241094=CARTESIAN_POINT('Ctrl Pts',(60.4137560077509,6.15819229746517,3.23423045308448));
#241095=CARTESIAN_POINT('Ctrl Pts',(60.5608532912343,6.04595329345079,3.36123028058486));
#241096=CARTESIAN_POINT('Ctrl Pts',(60.5475781763993,6.17225757416256,3.36123028058486));
#241097=CARTESIAN_POINT('Ctrl Pts',(60.5475781763993,6.17225757416256,3.23423028058486));
#241098=CARTESIAN_POINT('Origin',(60.2327006545395,6.01146306152057,3.42473028058486));
#241099=CARTESIAN_POINT('Origin',(60.1517960329189,6.00295964283199,3.56563113524772));
#241100=CARTESIAN_POINT('Origin',(60.0157999988651,13.0813452322047,3.56647653909476));
#241101=CARTESIAN_POINT('Origin',(60.0590486699122,13.0905908661185,3.64299466007602));
#241102=CARTESIAN_POINT('Origin',(59.9357500275433,13.0643300858384,3.42473028058494));
#241103=CARTESIAN_POINT('Ctrl Pts',(59.8282880397055,13.0409063549241,3.48823028058493));
#241104=CARTESIAN_POINT('Ctrl Pts',(59.8550545325309,12.9173404733284,3.48794691941609));
#241105=CARTESIAN_POINT('Ctrl Pts',(59.9621548122771,12.9401053405452,3.42473028058494));
#241106=CARTESIAN_POINT('Ctrl Pts',(59.7842416555147,13.0316624367245,3.41028005925099));
#241107=CARTESIAN_POINT('Ctrl Pts',(59.8108054559367,12.9079350417515,3.40982512230876));
#241108=CARTESIAN_POINT('Ctrl Pts',(59.896122018529,12.9260696369486,3.30780486372844));
#241109=CARTESIAN_POINT('Ctrl Pts',(59.7007958241042,13.014150410756,3.36123028058491));
#241110=CARTESIAN_POINT('Ctrl Pts',(59.7270694888849,12.8901364125065,3.36099721048557));
#241111=CARTESIAN_POINT('Ctrl Pts',(59.7710239514078,12.8994792219298,3.23423045308437));
#241112=CARTESIAN_POINT('Ctrl Pts',(59.6130003254555,12.9957275188826,3.36123028058491));
#241113=CARTESIAN_POINT('Ctrl Pts',(59.6394051101893,12.8715027735894,3.36123028058491));
#241114=CARTESIAN_POINT('Ctrl Pts',(59.6394051101893,12.8715027735894,3.23423028058491));
#241115=CARTESIAN_POINT('Origin',(59.6130003254555,12.9957275188826,3.23423028058491));
#241116=CARTESIAN_POINT('Origin',(-0.0660119618346332,0.310561863233167,
3.64303198860263));
#241117=CARTESIAN_POINT('Origin',(60.4516424606489,13.1739864076109,3.64303198860273));
#241118=CARTESIAN_POINT('Origin',(-0.0660119618346331,0.31056186323317,
3.23423028058482));
#241119=CARTESIAN_POINT('Origin',(59.4650964698966,12.9642895838873,3.23423028058491));
#241120=CARTESIAN_POINT('Ctrl Pts',(60.9782752797348,13.2864868028998,3.47153072139082));
#241121=CARTESIAN_POINT('Ctrl Pts',(61.0052918384389,13.1616357280627,3.47182327902673));
#241122=CARTESIAN_POINT('Ctrl Pts',(60.8992893541409,13.1392995818862,3.40413028959068));
#241123=CARTESIAN_POINT('Ctrl Pts',(60.8658306440996,13.262466975741,3.65553807120968));
#241124=CARTESIAN_POINT('Ctrl Pts',(60.8926675943301,13.1376969719809,3.65586275496942));
#241125=CARTESIAN_POINT('Ctrl Pts',(60.8093473519449,13.1201818190172,3.5512812683721));
#241126=CARTESIAN_POINT('Ctrl Pts',(60.6638281080081,13.2193155203585,3.77003198860273));
#241127=CARTESIAN_POINT('Ctrl Pts',(60.6905008239745,13.0947255842078,3.77025505748434));
#241128=CARTESIAN_POINT('Ctrl Pts',(60.6477702018641,13.0858375353128,3.64284211731209));
#241129=CARTESIAN_POINT('Ctrl Pts',(60.4516424606489,13.1739864076109,3.77003198860273));
#241130=CARTESIAN_POINT('Ctrl Pts',(60.4780866929066,13.0495760763091,3.77003198860273));
#241131=CARTESIAN_POINT('Ctrl Pts',(60.4780472159603,13.0497618007392,3.64284239821766));
#241132=CARTESIAN_POINT('Origin',(60.8730422059013,13.2635576885504,3.4042309748332));
#241133=CARTESIAN_POINT('Ctrl Pts',(59.4650964698966,12.9642895838873,3.36123028058491));
#241134=CARTESIAN_POINT('Ctrl Pts',(59.4915012546305,12.8400648385941,3.36123028058491));
#241135=CARTESIAN_POINT('Ctrl Pts',(59.4915012546305,12.8400648385941,3.23423028058491));
#241136=CARTESIAN_POINT('Ctrl Pts',(59.3770041141843,12.945804994394,3.36123028058491));
#241137=CARTESIAN_POINT('Ctrl Pts',(59.4033730190103,12.8213326038448,3.36146538610185));
#241138=CARTESIAN_POINT('Ctrl Pts',(59.3594375597985,12.8119938336991,3.23423043688462));
#241139=CARTESIAN_POINT('Ctrl Pts',(59.2937057271824,12.9283282206298,3.41054258693108));
#241140=CARTESIAN_POINT('Ctrl Pts',(59.3204640761277,12.8037097640123,3.41100608859742));
#241141=CARTESIAN_POINT('Ctrl Pts',(59.2345619206652,12.7854506972086,3.30819866970818));
#241142=CARTESIAN_POINT('Ctrl Pts',(59.2498070616279,12.9191181862048,3.48823028058491));
#241143=CARTESIAN_POINT('Ctrl Pts',(59.2768226962998,12.794433502371,3.48852004212269));
#241144=CARTESIAN_POINT('Ctrl Pts',(59.1687514833561,12.7714622569322,3.42473028058491));
#241145=CARTESIAN_POINT('Origin',(59.1423466986222,12.8956870022254,3.42473028058489));
#241146=CARTESIAN_POINT('Origin',(61.047298331885,13.3005969715169,3.11913648178364));
#241147=CARTESIAN_POINT('Origin',(61.2215544576539,13.3376362544828,2.83404198860272));
#241148=CARTESIAN_POINT('Origin',(59.062774129126,12.8787733304441,3.56563113460766));
#241149=CARTESIAN_POINT('Origin',(59.0190342907436,12.8695280801148,3.64299171721792));
#241150=CARTESIAN_POINT('Ctrl Pts',(61.5752716937451,13.103835206573,2.59908173516033));
#241151=CARTESIAN_POINT('Ctrl Pts',(61.5387839176328,13.0960702419682,2.65878198860271));
#241152=CARTESIAN_POINT('Ctrl Pts',(61.4699285681954,13.0814171332235,2.65878198860271));
#241153=CARTESIAN_POINT('Ctrl Pts',(61.5569304518428,13.1900205930481,2.59908193475691));
#241154=CARTESIAN_POINT('Ctrl Pts',(61.5254208297802,13.1588482421891,2.6587871532543));
#241155=CARTESIAN_POINT('Ctrl Pts',(61.4593031273756,13.1313027022857,2.65878198860271));
#241156=CARTESIAN_POINT('Ctrl Pts',(61.515537853938,13.2643407403243,2.63878778849882));
#241157=CARTESIAN_POINT('Ctrl Pts',(61.4904936222815,13.21185113915,2.69564460180118));
#241158=CARTESIAN_POINT('Ctrl Pts',(61.4250300340663,13.1721300657491,2.68180481624894));
#241159=CARTESIAN_POINT('Ctrl Pts',(61.4222835584426,13.3535591268198,2.75443238878654));
#241160=CARTESIAN_POINT('Ctrl Pts',(61.41788805574,13.261196258709,2.79268340777107));
#241161=CARTESIAN_POINT('Ctrl Pts',(61.3411158595757,13.2174099770541,2.74885926835619));
#241162=CARTESIAN_POINT('Ctrl Pts',(61.3712701109737,13.3700167576321,2.82856655361681));
#241163=CARTESIAN_POINT('Ctrl Pts',(61.3797074995622,13.257089619244,2.85384197230726));
#241164=CARTESIAN_POINT('Ctrl Pts',(61.2924393404513,13.2228660458967,2.79184624278457));
#241165=CARTESIAN_POINT('Ctrl Pts',(61.3267881959113,13.3605623192489,2.90134173516034));
#241166=CARTESIAN_POINT('Ctrl Pts',(61.3537611057083,13.2359003894753,2.90163218716401));
#241167=CARTESIAN_POINT('Ctrl Pts',(61.2479592423878,13.2134115091896,2.83404198860272));
#241168=CARTESIAN_POINT('Origin',(61.4699285681954,13.0814171332235,2.53178198860271));
#241169=CARTESIAN_POINT('Origin',(-0.0660119618346332,0.310561863233167,
3.64303198860263));
#241170=CARTESIAN_POINT('Origin',(58.6264539577984,12.7860306150453,3.64303198860272));
#241171=CARTESIAN_POINT('Origin',(5.5033905580924E-15,1.85848267687233E-13,
2.53178198860262));
#241172=CARTESIAN_POINT('Origin',(61.4762657165316,13.0516031943531,2.53178198860271));
#241173=CARTESIAN_POINT('Ctrl Pts',(58.6264539577984,12.7860306150453,3.77003198860273));
#241174=CARTESIAN_POINT('Ctrl Pts',(58.6528982980922,12.6616197754737,3.77003198860273));
#241175=CARTESIAN_POINT('Ctrl Pts',(58.6528587129485,12.6618060089323,3.64284187937009));
#241176=CARTESIAN_POINT('Ctrl Pts',(58.4142663981468,12.7406940127368,3.77003198860273));
#241177=CARTESIAN_POINT('Ctrl Pts',(58.4408495151723,12.6165479409686,3.76980208962847));
#241178=CARTESIAN_POINT('Ctrl Pts',(58.4831327254081,12.6257296363319,3.64284193928262));
#241179=CARTESIAN_POINT('Ctrl Pts',(58.2122676405433,12.6975319705099,3.65553535416594));
#241180=CARTESIAN_POINT('Ctrl Pts',(58.2389323335222,12.5736296288395,3.65520057834622));
#241181=CARTESIAN_POINT('Ctrl Pts',(58.3215567776491,12.5913856081747,3.55127910964279));
#241182=CARTESIAN_POINT('Ctrl Pts',(58.099826060148,12.6735055745743,3.4715307213908));
#241183=CARTESIAN_POINT('Ctrl Pts',(58.1266254943014,12.5497583536231,3.4712274628159));
#241184=CARTESIAN_POINT('Ctrl Pts',(58.2316158778881,12.5722680796267,3.40413045901257));
#241185=CARTESIAN_POINT('Origin',(58.2050537810542,12.6964592423895,3.4042309748332));
#241186=CARTESIAN_POINT('Ctrl Pts',(61.4590390555209,12.7383709431253,2.90134173516033));
#241187=CARTESIAN_POINT('Ctrl Pts',(61.4329754599099,12.8632261535957,2.901632187164));
#241188=CARTESIAN_POINT('Ctrl Pts',(61.3271735965893,12.84073727331,2.83404198860272));
#241189=CARTESIAN_POINT('Ctrl Pts',(61.5035409747666,12.7478306169684,2.82853349835365));
#241190=CARTESIAN_POINT('Ctrl Pts',(61.4653154597763,12.8544171899351,2.85381483162389));
#241191=CARTESIAN_POINT('Ctrl Pts',(61.3716739624483,12.8501961180701,2.79182701594252));
#241192=CARTESIAN_POINT('Ctrl Pts',(61.5432717953614,12.7835835513932,2.75468822073652));
#241193=CARTESIAN_POINT('Ctrl Pts',(61.501718402959,12.8662481012968,2.79286913083821));
#241194=CARTESIAN_POINT('Ctrl Pts',(61.4137451613974,12.8749453072905,2.74900763297923));
#241195=CARTESIAN_POINT('Ctrl Pts',(61.5920631419344,12.9020280679173,2.63954450640403));
#241196=CARTESIAN_POINT('Ctrl Pts',(61.5478406570046,12.9401487584128,2.69627684028883));
#241197=CARTESIAN_POINT('Ctrl Pts',(61.4717924962542,12.9498405053864,2.682243560365));
#241198=CARTESIAN_POINT('Ctrl Pts',(61.599979580521,12.9874904696722,2.5990817870642));
#241199=CARTESIAN_POINT('Ctrl Pts',(61.5585057825378,13.0031958218443,2.6587870432155));
#241200=CARTESIAN_POINT('Ctrl Pts',(61.4868843017925,13.0015435854426,2.65878198860271));
#241201=CARTESIAN_POINT('Ctrl Pts',(61.5816197022698,13.0739701745327,2.59908173516033));
#241202=CARTESIAN_POINT('Ctrl Pts',(61.5451281645059,13.0662229071069,2.65878198860271));
#241203=CARTESIAN_POINT('Ctrl Pts',(61.4762657165316,13.0516031943531,2.65878198860271));
#241204=CARTESIAN_POINT('Origin',(61.3535783813232,12.7165125280168,2.83404198860271));
#241205=CARTESIAN_POINT('Origin',(58.030797415544,12.6594199084572,3.11913648167168));
#241206=CARTESIAN_POINT('Origin',(57.8565410498767,12.6223805745521,2.83404198860271));
#241207=CARTESIAN_POINT('Origin',(61.1793222555328,12.6794732450928,3.11913648177592));
#241208=CARTESIAN_POINT('Origin',(61.0050661295706,12.6424339620844,3.4042309748332));
#241209=CARTESIAN_POINT('Ctrl Pts',(57.751314065072,12.5994235324474,2.90134173516033));
#241210=CARTESIAN_POINT('Ctrl Pts',(57.7780756236495,12.4758649777955,2.90103711553238));
#241211=CARTESIAN_POINT('Ctrl Pts',(57.8829458346105,12.4981558292589,2.83404198860271));
#241212=CARTESIAN_POINT('Ctrl Pts',(57.7068710254545,12.5899763290075,2.82862991747974));
#241213=CARTESIAN_POINT('Ctrl Pts',(57.7455616498589,12.4844883578131,2.85314045886506));
#241214=CARTESIAN_POINT('Ctrl Pts',(57.838500842801,12.4887087546165,2.79187961000003));
#241215=CARTESIAN_POINT('Ctrl Pts',(57.6673720419786,12.5543975270268,2.7547062579333));
#241216=CARTESIAN_POINT('Ctrl Pts',(57.709200876099,12.472450653056,2.79224250381909));
#241217=CARTESIAN_POINT('Ctrl Pts',(57.7966870296826,12.464030811219,2.74901809108272));
#241218=CARTESIAN_POINT('Ctrl Pts',(57.6192799956674,12.4363816727425,2.63947868311713));
#241219=CARTESIAN_POINT('Ctrl Pts',(57.6635313090893,12.3985321242202,2.69595066767919));
#241220=CARTESIAN_POINT('Ctrl Pts',(57.7394080294762,12.3892398894927,2.68220539436066));
#241221=CARTESIAN_POINT('Ctrl Pts',(57.6118166447795,12.3512461790954,2.59908178585092));
#241222=CARTESIAN_POINT('Ctrl Pts',(57.6532646075499,12.335688889809,2.65877670944976));
#241223=CARTESIAN_POINT('Ctrl Pts',(57.7248239067136,12.3376071226709,2.65878198860271));
#241224=CARTESIAN_POINT('Ctrl Pts',(57.6301266171957,12.2652136052663,2.59908173516033));
#241225=CARTESIAN_POINT('Ctrl Pts',(57.6666142715155,12.2729791421557,2.65878198860271));
#241226=CARTESIAN_POINT('Ctrl Pts',(57.7354693911205,12.2876333308473,2.65878198860271));
#241227=CARTESIAN_POINT('Origin',(57.7354693911204,12.2876333308473,2.53178198860271));
#241228=CARTESIAN_POINT('Ctrl Pts',(60.5836663843182,12.5528626811449,3.77003198860273));
#241229=CARTESIAN_POINT('Ctrl Pts',(60.5572221497821,12.6772730231653,3.77003198860273));
#241230=CARTESIAN_POINT('Ctrl Pts',(60.5572616290101,12.6770872880007,3.64284238727601));
#241231=CARTESIAN_POINT('Ctrl Pts',(60.7959479326852,12.5977568525213,3.77003198860273));
#241232=CARTESIAN_POINT('Ctrl Pts',(60.769639383333,12.7224242094582,3.77025506105854));
#241233=CARTESIAN_POINT('Ctrl Pts',(60.7269872521267,12.7131635826241,3.64284210641938));
#241234=CARTESIAN_POINT('Ctrl Pts',(60.9980361136598,12.6404975322979,3.65553527987845));
#241235=CARTESIAN_POINT('Ctrl Pts',(60.9718043534744,12.7653961862443,3.65585996532996));
#241236=CARTESIAN_POINT('Ctrl Pts',(60.8885631224033,12.7475075938201,3.55127902710167));
#241237=CARTESIAN_POINT('Ctrl Pts',(61.1105274371641,12.6642893210143,3.47153072139081));
#241238=CARTESIAN_POINT('Ctrl Pts',(61.0844267823321,12.789335088505,3.47182327905198));
#241239=CARTESIAN_POINT('Ctrl Pts',(60.978503758349,12.7666250660186,3.40413028377993));
#241240=CARTESIAN_POINT('Origin',(60.5836663843182,12.5528626811449,3.64303198860273));
#241241=CARTESIAN_POINT('Origin',(5.72205236298458E-15,1.8633692237856E-13,
2.53178198860262));
#241242=CARTESIAN_POINT('Origin',(57.7418065394566,12.257819391977,2.53178198860271));
#241243=CARTESIAN_POINT('Origin',(59.5987607253194,12.3435145206988,3.64303198860272));
#241244=CARTESIAN_POINT('Origin',(60.1910940874972,12.4693660187261,3.64299466007668));
#241245=CARTESIAN_POINT('Ctrl Pts',(57.6364522029207,12.2354540642047,2.59908173516033));
#241246=CARTESIAN_POINT('Ctrl Pts',(57.6729438621906,12.2432007592849,2.65878198860272));
#241247=CARTESIAN_POINT('Ctrl Pts',(57.7418065394566,12.257819391977,2.65878198860271));
#241248=CARTESIAN_POINT('Ctrl Pts',(57.6546556225249,12.1497054461945,2.59908193200013));
#241249=CARTESIAN_POINT('Ctrl Pts',(57.6862025493675,12.1807288143664,2.65877685806641));
#241250=CARTESIAN_POINT('Ctrl Pts',(57.7523715145553,12.2080066271961,2.65878198860271));
#241251=CARTESIAN_POINT('Ctrl Pts',(57.6955109599436,12.07549391746,2.63872492669823));
#241252=CARTESIAN_POINT('Ctrl Pts',(57.7206875210986,12.1277502414154,2.69532212015283));
#241253=CARTESIAN_POINT('Ctrl Pts',(57.786160923601,12.1670355805165,2.68176836726644));
#241254=CARTESIAN_POINT('Ctrl Pts',(57.7879231380266,11.9863964689866,2.75442176402243));
#241255=CARTESIAN_POINT('Ctrl Pts',(57.7928648378988,12.078208678266,2.79203179920148));
#241256=CARTESIAN_POINT('Ctrl Pts',(57.8693039540642,12.1215423041374,2.74885310748183));
#241257=CARTESIAN_POINT('Ctrl Pts',(57.8386735460214,11.9699873265231,2.8286608955842));
#241258=CARTESIAN_POINT('Ctrl Pts',(57.8311081991734,12.0820993460728,2.85316563119168));
#241259=CARTESIAN_POINT('Ctrl Pts',(57.9177340744074,12.1160385312531,2.79189751796631));
#241260=CARTESIAN_POINT('Ctrl Pts',(57.8830978693156,11.9794294790614,2.90134173516032));
#241261=CARTESIAN_POINT('Ctrl Pts',(57.8572899778511,12.1031907419159,2.90103711553238));
#241262=CARTESIAN_POINT('Ctrl Pts',(57.9621601888121,12.1254815933794,2.8340419886027));
#241263=CARTESIAN_POINT('Origin',(57.9885649735459,12.0012568480862,2.83404198860271));
#241264=CARTESIAN_POINT('Origin',(60.1478239214148,12.4602215058071,3.56647653971879));
#241265=CARTESIAN_POINT('Origin',(60.0677739512126,12.4432063593724,3.42473028058494));
#241266=CARTESIAN_POINT('Origin',(58.1628213391868,12.0382961820438,3.11913648168105));
#241267=CARTESIAN_POINT('Origin',(58.3370777047235,12.0753355159235,3.4042309748332));
#241268=CARTESIAN_POINT('Ctrl Pts',(59.7450242491248,12.3746037924166,3.36123028058491));
#241269=CARTESIAN_POINT('Ctrl Pts',(59.7186194643909,12.4988285377098,3.36123028058491));
#241270=CARTESIAN_POINT('Ctrl Pts',(59.7186194643909,12.4988285377098,3.23423028058491));
#241271=CARTESIAN_POINT('Ctrl Pts',(59.8330190893702,12.3935470970139,3.36123028058491));
#241272=CARTESIAN_POINT('Ctrl Pts',(59.8065803155747,12.5175251937986,3.360996411086));
#241273=CARTESIAN_POINT('Ctrl Pts',(59.850683147391,12.5268995400898,3.23423043688411));
#241274=CARTESIAN_POINT('Ctrl Pts',(59.9162252185215,12.4114576311017,3.41054258905295));
#241275=CARTESIAN_POINT('Ctrl Pts',(59.8901687840297,12.5352924712488,3.41008815825902));
#241276=CARTESIAN_POINT('Ctrl Pts',(59.975558754836,12.5534426698448,3.30819867304308));
#241277=CARTESIAN_POINT('Ctrl Pts',(59.9600752506737,12.4208962741589,3.48823028058493));
#241278=CARTESIAN_POINT('Ctrl Pts',(59.9342688867325,12.5446662374489,3.48794691941609));
#241279=CARTESIAN_POINT('Ctrl Pts',(60.0413691664787,12.5674311046656,3.42473028058495));
#241280=CARTESIAN_POINT('Origin',(59.7450242491248,12.3746037924166,3.23423028058491));
#241281=CARTESIAN_POINT('Ctrl Pts',(58.2316113004781,12.0535047649324,3.47153072139082));
#241282=CARTESIAN_POINT('Ctrl Pts',(58.2057612755555,12.1774537741287,3.47122746285087));
#241283=CARTESIAN_POINT('Ctrl Pts',(58.3108302788454,12.199593564085,3.40413046676797));
#241284=CARTESIAN_POINT('Ctrl Pts',(58.3441059109581,12.0772900304169,3.65553813457996));
#241285=CARTESIAN_POINT('Ctrl Pts',(58.3180696991549,12.2013259468569,3.65520336072245));
#241286=CARTESIAN_POINT('Ctrl Pts',(58.400772540275,12.218711381782,3.55128134519958));
#241287=CARTESIAN_POINT('Ctrl Pts',(58.5461981381264,12.1200201767777,3.77003198860273));
#241288=CARTESIAN_POINT('Ctrl Pts',(58.5199882620693,12.2442455720377,3.7698020931414));
#241289=CARTESIAN_POINT('Ctrl Pts',(58.562349768553,12.2530556816161,3.64284195387389));
#241290=CARTESIAN_POINT('Ctrl Pts',(58.7584778814676,12.1649068885794,3.77003198860273));
#241291=CARTESIAN_POINT('Ctrl Pts',(58.7320335442281,12.289317713782,3.77003198860273));
#241292=CARTESIAN_POINT('Ctrl Pts',(58.7320731263129,12.2891314947139,3.64284189403811));
#241293=CARTESIAN_POINT('Origin',(58.7584778814676,12.1649068885794,3.64303198860273));
#241294=CARTESIAN_POINT('Origin',(58.1567073854021,12.0369966210212,3.2342302805849));
#241295=CARTESIAN_POINT('Origin',(59.5971203935659,12.3431658574213,3.23423028058491));
#241296=CARTESIAN_POINT('Origin',(57.9308881865554,11.9889972685553,3.64303198860271));
#241297=CARTESIAN_POINT('Origin',(59.1510793400373,12.2483049654005,3.64299171721818));
#241298=CARTESIAN_POINT('Ctrl Pts',(59.3820708699071,12.2968658913805,3.4882302805849));
#241299=CARTESIAN_POINT('Ctrl Pts',(59.3560370505014,12.4217592664914,3.48852004212268));
#241300=CARTESIAN_POINT('Ctrl Pts',(59.2479658375576,12.3987880210526,3.4247302805849));
#241301=CARTESIAN_POINT('Ctrl Pts',(59.4260685345961,12.3063392072225,3.41028005848414));
#241302=CARTESIAN_POINT('Ctrl Pts',(59.3998259533503,12.4310668851196,3.41074404220356));
#241303=CARTESIAN_POINT('Ctrl Pts',(59.3139986558962,12.412823729876,3.30780486243865));
#241304=CARTESIAN_POINT('Ctrl Pts',(59.5094220566593,12.3242857901784,3.36123028058491));
#241305=CARTESIAN_POINT('Ctrl Pts',(59.4828840257734,12.4487214234142,3.36146460586404));
#241306=CARTESIAN_POINT('Ctrl Pts',(59.4390967537846,12.4394141514346,3.23423045308438));
#241307=CARTESIAN_POINT('Ctrl Pts',(59.5971203935659,12.3431658574213,3.36123028058491));
#241308=CARTESIAN_POINT('Ctrl Pts',(59.5707156088321,12.4673906027145,3.36123028058491));
#241309=CARTESIAN_POINT('Ctrl Pts',(59.5707156088321,12.4673906027145,3.23423028058491));
#241310=CARTESIAN_POINT('Origin',(59.2743706222915,12.2745632757594,3.4247302805849));
#241311=CARTESIAN_POINT('Origin',(59.194798053941,12.2576496039181,3.56563113524751));
#241312=CARTESIAN_POINT('Origin',(58.3196542523191,19.2830435999599,3.56647653909436));
#241313=CARTESIAN_POINT('Origin',(58.361699570716,19.2967593024467,3.6429946600746));
#241314=CARTESIAN_POINT('Origin',(58.2418213702174,19.2577541638581,3.42473028058498));
#241315=CARTESIAN_POINT('Ctrl Pts',(58.1373965169893,19.2232259141442,3.48823028058498));
#241316=CARTESIAN_POINT('Ctrl Pts',(58.1769325318819,19.103134799739,3.48794691941614));
#241317=CARTESIAN_POINT('Ctrl Pts',(58.281066528503,19.1369699862886,3.42473028058499));
#241318=CARTESIAN_POINT('Ctrl Pts',(58.0945576760632,19.2094285342456,3.410280059251));
#241319=CARTESIAN_POINT('Ctrl Pts',(58.1339089916607,19.089155604122,3.40982512231157));
#241320=CARTESIAN_POINT('Ctrl Pts',(58.2168625998345,19.1161088652887,3.30780486372925));
#241321=CARTESIAN_POINT('Ctrl Pts',(58.0133994748125,19.1832899764608,3.36123028058496));
#241322=CARTESIAN_POINT('Ctrl Pts',(58.0524922023746,19.0627016856749,3.36099721048456));
#241323=CARTESIAN_POINT('Ctrl Pts',(58.0952292882363,19.0765878066324,3.23423045308386));
#241324=CARTESIAN_POINT('Ctrl Pts',(57.9280106456676,19.1557908785627,3.36123028058496));
#241325=CARTESIAN_POINT('Ctrl Pts',(57.9672558039532,19.0350067009933,3.36123028058496));
#241326=CARTESIAN_POINT('Ctrl Pts',(57.9672558039532,19.0350067009933,3.23423028058496));
#241327=CARTESIAN_POINT('Origin',(57.9280106456676,19.1557908785627,3.23423028058496));
#241328=CARTESIAN_POINT('Origin',(-0.0981128957140405,0.301960443923895,
3.64303198860263));
#241329=CARTESIAN_POINT('Origin',(58.7434254837932,19.4207352200703,3.64303198860277));
#241330=CARTESIAN_POINT('Origin',(-0.0981128957140404,0.301960443923898,
3.23423028058482));
#241331=CARTESIAN_POINT('Origin',(57.7842031819383,19.1090650011318,3.23423028058496));
#241332=CARTESIAN_POINT('Ctrl Pts',(59.2554138597571,19.5876674457081,3.47153072139086));
#241333=CARTESIAN_POINT('Ctrl Pts',(59.2953329099159,19.4663243174863,3.47182327902676));
#241334=CARTESIAN_POINT('Ctrl Pts',(59.1922458813531,19.4330302542695,3.40413028959063));
#241335=CARTESIAN_POINT('Ctrl Pts',(59.1460959632229,19.5520255367076,3.6555380712097));
#241336=CARTESIAN_POINT('Ctrl Pts',(59.1858279145887,19.4307442612476,3.65586275496854));
#241337=CARTESIAN_POINT('Ctrl Pts',(59.1047949412317,19.4046157212337,3.55128126837225));
#241338=CARTESIAN_POINT('Ctrl Pts',(58.9497105734782,19.4879954548407,3.77003198860277));
#241339=CARTESIAN_POINT('Ctrl Pts',(58.9892603680798,19.3668760934059,3.77025505748615));
#241340=CARTESIAN_POINT('Ctrl Pts',(58.9476928828794,19.3535701679107,3.64284211731241));
#241341=CARTESIAN_POINT('Ctrl Pts',(58.7434254837932,19.4207352200703,3.77003198860277));
#241342=CARTESIAN_POINT('Ctrl Pts',(58.7827292725254,19.2997705965407,3.77003198860277));
#241343=CARTESIAN_POINT('Ctrl Pts',(58.7826705983486,19.2999511770886,3.64284239821754));
#241344=CARTESIAN_POINT('Origin',(59.1531540087999,19.5538640879535,3.40423097483324));
#241345=CARTESIAN_POINT('Ctrl Pts',(57.7842031819382,19.1090650011318,3.36123028058496));
#241346=CARTESIAN_POINT('Ctrl Pts',(57.8234483402239,18.9882808235623,3.36123028058496));
#241347=CARTESIAN_POINT('Ctrl Pts',(57.8234483402239,18.9882808235623,3.23423028058496));
#241348=CARTESIAN_POINT('Ctrl Pts',(57.6985255711019,19.0814735135848,3.36123028058496));
#241349=CARTESIAN_POINT('Ctrl Pts',(57.7377609320111,18.9604392969148,3.36146538610105));
#241350=CARTESIAN_POINT('Ctrl Pts',(57.6950423231338,18.9465591794949,3.23423043688411));
#241351=CARTESIAN_POINT('Ctrl Pts',(57.6175103216835,19.0553854270318,3.41054258693115));
#241352=CARTESIAN_POINT('Ctrl Pts',(57.6571482613586,18.9342466524541,3.41100608859817));
#241353=CARTESIAN_POINT('Ctrl Pts',(57.5736252790864,18.9071083904255,3.30819866970882));
#241354=CARTESIAN_POINT('Ctrl Pts',(57.5748148483576,19.041637186088,3.48823028058495));
#241355=CARTESIAN_POINT('Ctrl Pts',(57.6147155869502,18.9204594407748,3.48852004212273));
#241356=CARTESIAN_POINT('Ctrl Pts',(57.5096375484037,18.8863175164095,3.42473028058495));
#241357=CARTESIAN_POINT('Origin',(57.4703923901181,19.007101693979,3.42473028058494));
#241358=CARTESIAN_POINT('Origin',(59.3225838821626,19.6089151909161,3.11913648178297));
#241359=CARTESIAN_POINT('Origin',(59.4920137553139,19.6639662938564,2.83404198860276));
#241360=CARTESIAN_POINT('Origin',(57.3930236876037,18.9819630786539,3.56563113460818));
#241361=CARTESIAN_POINT('Origin',(57.3504898524409,18.9681964166835,3.64299171721781));
#241362=CARTESIAN_POINT('Ctrl Pts',(59.8682321556242,19.4684195516699,2.59908173516038));
#241363=CARTESIAN_POINT('Ctrl Pts',(59.8327559231846,19.4568831131886,2.65878198860276));
#241364=CARTESIAN_POINT('Ctrl Pts',(59.7658094374951,19.4351129318423,2.65878198860276));
#241365=CARTESIAN_POINT('Ctrl Pts',(59.8409825629599,19.5522156237496,2.5990819347567));
#241366=CARTESIAN_POINT('Ctrl Pts',(59.8129039518352,19.5179203859181,2.65878715325351));
#241367=CARTESIAN_POINT('Ctrl Pts',(59.7500277420787,19.4836145615372,2.65878198860276));
#241368=CARTESIAN_POINT('Ctrl Pts',(59.7920481472525,19.6218019328335,2.6387877884989));
#241369=CARTESIAN_POINT('Ctrl Pts',(59.7726277678661,19.5669820401374,2.6956446018013));
#241370=CARTESIAN_POINT('Ctrl Pts',(59.7116747787988,19.5206357546568,2.68180481624901));
#241371=CARTESIAN_POINT('Ctrl Pts',(59.6899788477097,19.700783843471,2.75443238878654));
#241372=CARTESIAN_POINT('Ctrl Pts',(59.6952619726971,19.6084674936732,2.79268340777105));
#241373=CARTESIAN_POINT('Ctrl Pts',(59.6234872553896,19.5568961981638,2.74885926835621));
#241374=CARTESIAN_POINT('Ctrl Pts',(59.6375245663856,19.7118189603904,2.82856655361687));
#241375=CARTESIAN_POINT('Ctrl Pts',(59.6577198343149,19.6003923959453,2.85384197230812));
#241376=CARTESIAN_POINT('Ctrl Pts',(59.5745070768392,19.5572342963493,2.79184624278451));
#241377=CARTESIAN_POINT('Ctrl Pts',(59.5942745858236,19.6977666881848,2.90134173516037));
#241378=CARTESIAN_POINT('Ctrl Pts',(59.6341304551457,19.5766071063171,2.90163218716404));
#241379=CARTESIAN_POINT('Ctrl Pts',(59.5312589135995,19.5431821162869,2.83404198860275));
#241380=CARTESIAN_POINT('Origin',(59.7658094374951,19.4351129318423,2.53178198860275));
#241381=CARTESIAN_POINT('Origin',(-0.0981128957140405,0.301960443923895,
3.64303198860263));
#241382=CARTESIAN_POINT('Origin',(56.9687879773466,18.8441205405522,3.64303198860276));
#241383=CARTESIAN_POINT('Origin',(5.50785759597432E-15,1.85831596474898E-13,
2.53178198860262));
#241384=CARTESIAN_POINT('Origin',(59.7752282754837,19.4061247292256,2.53178198860276));
#241385=CARTESIAN_POINT('Ctrl Pts',(56.9687879773466,18.8441205405522,3.77003198860277));
#241386=CARTESIAN_POINT('Ctrl Pts',(57.0080919266514,18.7231554228307,3.77003198860277));
#241387=CARTESIAN_POINT('Ctrl Pts',(57.0080330916623,18.7233364983081,3.64284187937081));
#241388=CARTESIAN_POINT('Ctrl Pts',(56.7625017687172,18.7768526573606,3.77003198860276));
#241389=CARTESIAN_POINT('Ctrl Pts',(56.801916058745,18.6561653631331,3.7698020896293));
#241390=CARTESIAN_POINT('Ctrl Pts',(56.8430078886249,18.6697165591961,3.64284193928345));
#241391=CARTESIAN_POINT('Ctrl Pts',(56.5661212433897,18.7128124416003,3.65553535416601));
#241392=CARTESIAN_POINT('Ctrl Pts',(56.6055911857651,18.5923760693057,3.65520057834411));
#241393=CARTESIAN_POINT('Ctrl Pts',(56.6859069993072,18.618671385701,3.55127910964192));
#241394=CARTESIAN_POINT('Ctrl Pts',(56.4568070719811,18.6771643191712,3.47153072139087));
#241395=CARTESIAN_POINT('Ctrl Pts',(56.4963948028695,18.5568963021135,3.47122746281597));
#241396=CARTESIAN_POINT('Ctrl Pts',(56.5984571310816,18.5902572009362,3.40413045901299));
#241397=CARTESIAN_POINT('Origin',(56.5590590327989,18.7109915363519,3.40423097483324));
#241398=CARTESIAN_POINT('Ctrl Pts',(59.7908376697911,19.0928077206414,2.90134173516038));
#241399=CARTESIAN_POINT('Ctrl Pts',(59.7518659300026,19.2142545736086,2.90163218716405));
#241400=CARTESIAN_POINT('Ctrl Pts',(59.6489943884564,19.1808295835784,2.83404198860276));
#241401=CARTESIAN_POINT('Ctrl Pts',(59.8341069976972,19.1068672906324,2.82853349835363));
#241402=CARTESIAN_POINT('Ctrl Pts',(59.7849495554008,19.2088743168611,2.85381483162395));
#241403=CARTESIAN_POINT('Ctrl Pts',(59.6922622581485,19.1948881666554,2.7918270159429));
#241404=CARTESIAN_POINT('Ctrl Pts',(59.8698829694068,19.1465773683628,2.75468822073666));
#241405=CARTESIAN_POINT('Ctrl Pts',(59.8199164124673,19.2244455609615,2.79286913083863));
#241406=CARTESIAN_POINT('Ctrl Pts',(59.7315159919505,19.2238994150015,2.74900763297922));
#241407=CARTESIAN_POINT('Ctrl Pts',(59.9060262085835,19.2694731179105,2.63954450640398));
#241408=CARTESIAN_POINT('Ctrl Pts',(59.8580612818573,19.3027624708831,2.69627684028865));
#241409=CARTESIAN_POINT('Ctrl Pts',(59.7814166574712,19.3044519280754,2.6822435603651));
#241410=CARTESIAN_POINT('Ctrl Pts',(59.9049660265691,19.3552948408466,2.59908178706338));
#241411=CARTESIAN_POINT('Ctrl Pts',(59.8620777700642,19.3665789650876,2.65878704321569));
#241412=CARTESIAN_POINT('Ctrl Pts',(59.7910213450144,19.35744929649,2.65878198860276));
#241413=CARTESIAN_POINT('Ctrl Pts',(59.8776671349985,19.4393816709759,2.59908173516038));
#241414=CARTESIAN_POINT('Ctrl Pts',(59.8421853116552,19.4278624395269,2.65878198860276));
#241415=CARTESIAN_POINT('Ctrl Pts',(59.7752282754837,19.4061247292256,2.65878198860276));
#241416=CARTESIAN_POINT('Origin',(59.688239546742,19.0600454060089,2.83404198860274));
#241417=CARTESIAN_POINT('Origin',(56.3896289265484,18.655940357665,3.1191364816716));
#241418=CARTESIAN_POINT('Origin',(56.2201988201383,18.6008891789888,2.83404198860276));
#241419=CARTESIAN_POINT('Origin',(59.5188096735651,19.004994303108,3.11913648177534));
#241420=CARTESIAN_POINT('Origin',(59.349379800228,18.949943200106,3.40423097483324));
#241421=CARTESIAN_POINT('Ctrl Pts',(56.1179479440988,18.5670586829468,2.90134173516037));
#241422=CARTESIAN_POINT('Ctrl Pts',(56.1574782858997,18.4469743395782,2.90103711553243));
#241423=CARTESIAN_POINT('Ctrl Pts',(56.2594439784239,18.4801050014193,2.83404198860275));
#241424=CARTESIAN_POINT('Ctrl Pts',(56.0747358697604,18.5530176696409,2.82862991747964));
#241425=CARTESIAN_POINT('Ctrl Pts',(56.124241038399,18.4521518441037,2.853140458864));
#241426=CARTESIAN_POINT('Ctrl Pts',(56.2162299491245,18.4660639121464,2.79187960999976));
#241427=CARTESIAN_POINT('Ctrl Pts',(56.0391722633447,18.5135050040177,2.75470625793355));
#241428=CARTESIAN_POINT('Ctrl Pts',(56.0893377355418,18.4363793473474,2.79224250381941));
#241429=CARTESIAN_POINT('Ctrl Pts',(56.17722474395,18.4371504234765,2.74901809108276));
#241430=CARTESIAN_POINT('Ctrl Pts',(56.0036796861845,18.3911086652348,2.63947868311697));
#241431=CARTESIAN_POINT('Ctrl Pts',(56.051644941423,18.3580919822894,2.69595066767905));
#241432=CARTESIAN_POINT('Ctrl Pts',(56.1280773042132,18.3567819283755,2.68220539436071));
#241433=CARTESIAN_POINT('Ctrl Pts',(56.0051563026341,18.3056594201307,2.59908178585071));
#241434=CARTESIAN_POINT('Ctrl Pts',(56.0480033886683,18.2945198471562,2.65877670944838));
#241435=CARTESIAN_POINT('Ctrl Pts',(56.1189701685708,18.3039075553121,2.65878198860275));
#241436=CARTESIAN_POINT('Ctrl Pts',(56.0323588238391,18.2220120550219,2.59908173516037));
#241437=CARTESIAN_POINT('Ctrl Pts',(56.0678348753332,18.233549049922,2.65878198860275));
#241438=CARTESIAN_POINT('Ctrl Pts',(56.1347810195642,18.2553202812751,2.65878198860275));
#241439=CARTESIAN_POINT('Origin',(56.1347810195642,18.2553202812751,2.53178198860275));
#241440=CARTESIAN_POINT('Ctrl Pts',(58.9396512752213,18.8168143322229,3.77003198860277));
#241441=CARTESIAN_POINT('Ctrl Pts',(58.9003474831029,18.9377789661741,3.77003198860277));
#241442=CARTESIAN_POINT('Ctrl Pts',(58.9004061606709,18.9375983751891,3.64284238727594));
#241443=CARTESIAN_POINT('Ctrl Pts',(59.1460772043121,18.8836520326596,3.77003198860278));
#241444=CARTESIAN_POINT('Ctrl Pts',(59.1068814887048,19.0048864565363,3.77025506105934));
#241445=CARTESIAN_POINT('Ctrl Pts',(59.0654310094281,18.9912181986574,3.64284210641901));
#241446=CARTESIAN_POINT('Ctrl Pts',(59.3425907075099,18.9472825415239,3.65553527987848));
#241447=CARTESIAN_POINT('Ctrl Pts',(59.3034471832918,19.0687550219942,3.65585996532983));
#241448=CARTESIAN_POINT('Ctrl Pts',(59.2225318234683,19.0422633471877,3.55127902710181));
#241449=CARTESIAN_POINT('Ctrl Pts',(59.4519788726607,18.9827025415099,3.47153072139086));
#241450=CARTESIAN_POINT('Ctrl Pts',(59.4129503580329,19.1043350338628,3.47182327905202));
#241451=CARTESIAN_POINT('Ctrl Pts',(59.3099814352093,19.070677448334,3.40413028377992));
#241452=CARTESIAN_POINT('Origin',(58.9396512752213,18.8168143322229,3.64303198860277));
#241453=CARTESIAN_POINT('Origin',(5.72046327455653E-15,1.86342852937311E-13,
2.53178198860262));
#241454=CARTESIAN_POINT('Origin',(56.1441998575527,18.2263320786585,2.53178198860275));
#241455=CARTESIAN_POINT('Origin',(56.3788528200606,17.9847604760584,3.64303198860276));
#241456=CARTESIAN_POINT('Origin',(58.557957308329,18.6927400943496,3.64299466007604));
#241457=CARTESIAN_POINT('Ctrl Pts',(56.0417604764383,18.1930767435951,2.59908173516037));
#241458=CARTESIAN_POINT('Ctrl Pts',(56.0772424804484,18.2045954185348,2.65878198860275));
#241459=CARTESIAN_POINT('Ctrl Pts',(56.1441998575527,18.2263320786585,2.65878198860275));
#241460=CARTESIAN_POINT('Ctrl Pts',(56.0688273470726,18.1097006409637,2.59908193199914));
#241461=CARTESIAN_POINT('Ctrl Pts',(56.0969586315475,18.143851611662,2.65877685806678));
#241462=CARTESIAN_POINT('Ctrl Pts',(56.1599138083653,18.1778965340264,2.65878198860275));
#241463=CARTESIAN_POINT('Ctrl Pts',(56.117216091734,18.0401661963853,2.63872492669811));
#241464=CARTESIAN_POINT('Ctrl Pts',(56.1367924598137,18.0947679219783,2.69532212015279));
#241465=CARTESIAN_POINT('Ctrl Pts',(56.1978007560413,18.1406818860298,2.68176836726648));
#241466=CARTESIAN_POINT('Ctrl Pts',(56.2184352456064,17.9612165360193,2.75442176402263));
#241467=CARTESIAN_POINT('Ctrl Pts',(56.2137528851844,18.0530423367035,2.79203179920163));
#241468=CARTESIAN_POINT('Ctrl Pts',(56.2852436625535,18.1041286397846,2.74885310748188));
#241469=CARTESIAN_POINT('Ctrl Pts',(56.2706228600014,17.9502021467128,2.82866089558414));
#241470=CARTESIAN_POINT('Ctrl Pts',(56.2513800597969,18.0609092108093,2.85316563119182));
#241471=CARTESIAN_POINT('Ctrl Pts',(56.3339837785515,18.1037173431993,2.79189751796638));
#241472=CARTESIAN_POINT('Ctrl Pts',(56.3138168485095,17.9642361803975,2.90134173516036));
#241473=CARTESIAN_POINT('Ctrl Pts',(56.2752137607566,18.0846218068697,2.90103711553242));
#241474=CARTESIAN_POINT('Ctrl Pts',(56.3771794532807,18.1177524687109,2.83404198860275));
#241475=CARTESIAN_POINT('Origin',(56.4164246115663,17.9969682911414,2.83404198860275));
#241476=CARTESIAN_POINT('Origin',(58.5158800426277,18.6791227120617,3.56647653971811));
#241477=CARTESIAN_POINT('Origin',(58.4380471616454,18.6538332760107,3.42473028058499));
#241478=CARTESIAN_POINT('Origin',(56.5858547179432,18.0520194698692,3.11913648168141));
#241479=CARTESIAN_POINT('Origin',(56.755284824227,18.1070706485045,3.40423097483324));
#241480=CARTESIAN_POINT('Ctrl Pts',(58.1242364370956,18.5518699907153,3.36123028058495));
#241481=CARTESIAN_POINT('Ctrl Pts',(58.08499127881,18.6726541682848,3.36123028058495));
#241482=CARTESIAN_POINT('Ctrl Pts',(58.08499127881,18.6726541682848,3.23423028058495));
#241483=CARTESIAN_POINT('Ctrl Pts',(58.2097691178803,18.5799074873345,3.36123028058495));
#241484=CARTESIAN_POINT('Ctrl Pts',(58.1705159385191,18.7004428147373,3.36099641108521));
#241485=CARTESIAN_POINT('Ctrl Pts',(58.2133972843954,18.7143758086141,3.23423043688441));
#241486=CARTESIAN_POINT('Ctrl Pts',(58.2906472745455,18.6064173144578,3.41054258905298));
#241487=CARTESIAN_POINT('Ctrl Pts',(58.2517893143876,18.726850135337,3.41008815826));
#241488=CARTESIAN_POINT('Ctrl Pts',(58.3348142976333,18.7538265876728,3.30819867304287));
#241489=CARTESIAN_POINT('Ctrl Pts',(58.3332704847796,18.620387828115,3.48823028058497));
#241490=CARTESIAN_POINT('Ctrl Pts',(58.2946680067388,18.7407822670305,3.48794691941613));
#241491=CARTESIAN_POINT('Ctrl Pts',(58.3988020033598,18.7746174535802,3.42473028058498));
#241492=CARTESIAN_POINT('Origin',(58.1242364370957,18.5518699907153,3.23423028058495));
#241493=CARTESIAN_POINT('Ctrl Pts',(56.6526781108323,18.0743352474894,3.47153072139085));
#241494=CARTESIAN_POINT('Ctrl Pts',(56.6140134955962,18.1949031876636,3.4712274628509));
#241495=CARTESIAN_POINT('Ctrl Pts',(56.7161926816712,18.227904394985,3.40413046676804));
#241496=CARTESIAN_POINT('Ctrl Pts',(56.7620702268163,18.1097491035594,3.65553813458));
#241497=CARTESIAN_POINT('Ctrl Pts',(56.7232113603703,18.2303840130651,3.65520336072255));
#241498=CARTESIAN_POINT('Ctrl Pts',(56.8036438738775,18.2563190096466,3.55128134519941));
#241499=CARTESIAN_POINT('Ctrl Pts',(56.9585888550845,18.1733695596525,3.77003198860277));
#241500=CARTESIAN_POINT('Ctrl Pts',(56.9195374698046,18.2941747571327,3.76980209314092));
#241501=CARTESIAN_POINT('Ctrl Pts',(56.9607460083083,18.3073645871834,3.64284195387411));
#241502=CARTESIAN_POINT('Ctrl Pts',(57.1650137687747,18.2401996527047,3.77003198860277));
#241503=CARTESIAN_POINT('Ctrl Pts',(57.1257098240091,18.3611647564558,3.77003198860277));
#241504=CARTESIAN_POINT('Ctrl Pts',(57.1257686544522,18.3609836949697,3.64284189403821));
#241505=CARTESIAN_POINT('Origin',(57.1650137687747,18.2401996527048,3.64303198860277));
#241506=CARTESIAN_POINT('Origin',(55.0155724295758,17.5418038257018,3.23423028058494));
#241507=CARTESIAN_POINT('Origin',(57.9804289733664,18.5051441132844,3.23423028058495));
#241508=CARTESIAN_POINT('Origin',(54.8020887275094,17.4724387660757,3.64303198860275));
#241509=CARTESIAN_POINT('Origin',(57.5467470426661,18.3641788932758,3.64299171721809));
#241510=CARTESIAN_POINT('Ctrl Pts',(57.7713971777987,18.4366189870675,3.48823028058495));
#241511=CARTESIAN_POINT('Ctrl Pts',(57.732451061807,18.5581069080663,3.48852004212273));
#241512=CARTESIAN_POINT('Ctrl Pts',(57.6273730232605,18.523964983701,3.42473028058495));
#241513=CARTESIAN_POINT('Ctrl Pts',(57.81416358753,18.4506394153714,3.41028005848421));
#241514=CARTESIAN_POINT('Ctrl Pts',(57.7750271733923,18.571940725309,3.4107440422031));
#241515=CARTESIAN_POINT('Ctrl Pts',(57.691576975838,18.5448261124695,3.30780486243884));
#241516=CARTESIAN_POINT('Ctrl Pts',(57.8951845615409,18.4772005006368,3.36123028058495));
#241517=CARTESIAN_POINT('Ctrl Pts',(57.8557848432471,18.5981804828671,3.36146460586464));
#241518=CARTESIAN_POINT('Ctrl Pts',(57.8132103173518,18.5843471808459,3.2342304530846));
#241519=CARTESIAN_POINT('Ctrl Pts',(57.9804289733664,18.5051441132844,3.36123028058495));
#241520=CARTESIAN_POINT('Ctrl Pts',(57.9411838150807,18.6259282908539,3.36123028058495));
#241521=CARTESIAN_POINT('Ctrl Pts',(57.9411838150807,18.6259282908539,3.23423028058495));
#241522=CARTESIAN_POINT('Origin',(57.6666181815461,18.4031808061315,3.42473028058494));
#241523=CARTESIAN_POINT('Origin',(57.5892494801763,18.378042190866,3.56563113524728));
#241524=CARTESIAN_POINT('Origin',(55.9845461696119,25.2734729067944,3.56647653909496));
#241525=CARTESIAN_POINT('Origin',(56.024927478051,25.291508405747,3.642994660078));
#241526=CARTESIAN_POINT('Origin',(55.9097831300746,25.2401862573144,3.42473028058502));
#241527=CARTESIAN_POINT('Ctrl Pts',(55.8095395120007,25.1949317875303,3.48823028058502));
#241528=CARTESIAN_POINT('Ctrl Pts',(55.8614118841079,25.0796311836956,3.48794691941618));
#241529=CARTESIAN_POINT('Ctrl Pts',(55.9614386837453,25.1241659841938,3.42473028058503));
#241530=CARTESIAN_POINT('Ctrl Pts',(55.768377565646,25.1767321129109,3.41028005925103));
#241531=CARTESIAN_POINT('Ctrl Pts',(55.8200852551805,25.0612313830313,3.40982512231043));
#241532=CARTESIAN_POINT('Ctrl Pts',(55.8997670518382,25.096708004599,3.30780486372873));
#241533=CARTESIAN_POINT('Ctrl Pts',(55.69039618079,25.142253402824,3.36123028058499));
#241534=CARTESIAN_POINT('Ctrl Pts',(55.7418796630224,25.0264120100475,3.36099721048512));
#241535=CARTESIAN_POINT('Ctrl Pts',(55.7829311357718,25.0446893032919,3.23423045308384));
#241536=CARTESIAN_POINT('Ctrl Pts',(55.6083495590301,25.1059793847704,3.361230280585));
#241537=CARTESIAN_POINT('Ctrl Pts',(55.6600051127008,24.9899591116498,3.36123028058499));
#241538=CARTESIAN_POINT('Ctrl Pts',(55.6600051127007,24.9899591116498,3.234230280585));
#241539=CARTESIAN_POINT('Origin',(55.6083495590301,25.1059793847704,3.234230280585));
#241540=CARTESIAN_POINT('Origin',(-0.129138884176561,0.29005068280171,3.64303198860263));
#241541=CARTESIAN_POINT('Origin',(56.391603244485,25.4547063934086,3.64303198860281));
#241542=CARTESIAN_POINT('Origin',(-0.129138884176561,0.290050682801712,
3.23423028058482));
#241543=CARTESIAN_POINT('Origin',(55.4702140717966,25.044477503395,3.234230280585));
#241544=CARTESIAN_POINT('Ctrl Pts',(56.8833377255394,25.6742415049982,3.47153072139089));
#241545=CARTESIAN_POINT('Ctrl Pts',(56.9357219056859,25.557735784097,3.4718232790268));
#241546=CARTESIAN_POINT('Ctrl Pts',(56.8366797759152,25.5138485805639,3.4041302895904));
#241547=CARTESIAN_POINT('Ctrl Pts',(56.7783442778561,25.6273680143726,3.65553807120976));
#241548=CARTESIAN_POINT('Ctrl Pts',(56.8305359187846,25.5109042502493,3.65586275496975));
#241549=CARTESIAN_POINT('Ctrl Pts',(56.75267802867,25.4764485929324,3.55128126837275));
#241550=CARTESIAN_POINT('Ctrl Pts',(56.589727673885,25.5431608329956,3.77003198860282));
#241551=CARTESIAN_POINT('Ctrl Pts',(56.6417212312943,25.4268390553474,3.77025505748559));
#241552=CARTESIAN_POINT('Ctrl Pts',(56.6017723050711,25.4092610357532,3.6428421173121));
#241553=CARTESIAN_POINT('Ctrl Pts',(56.391603244485,25.4547063934086,3.77003198860282));
#241554=CARTESIAN_POINT('Ctrl Pts',(56.4433359691576,25.3385127913797,3.77003198860282));
#241555=CARTESIAN_POINT('Ctrl Pts',(56.4432587405968,25.3386862495674,3.64284239821708));
#241556=CARTESIAN_POINT('Origin',(56.7851714777847,25.6299342604998,3.40423097483328));
#241557=CARTESIAN_POINT('Ctrl Pts',(55.4702140717966,25.044477503395,3.361230280585));
#241558=CARTESIAN_POINT('Ctrl Pts',(55.5218696254673,24.9284572302744,3.361230280585));
#241559=CARTESIAN_POINT('Ctrl Pts',(55.5218696254673,24.9284572302744,3.234230280585));
#241560=CARTESIAN_POINT('Ctrl Pts',(55.3878899076697,25.0080814159064,3.361230280585));
#241561=CARTESIAN_POINT('Ctrl Pts',(55.4395618538378,24.8918114493205,3.36146538610114));
#241562=CARTESIAN_POINT('Ctrl Pts',(55.3985281293136,24.8735420580979,3.23423043688406));
#241563=CARTESIAN_POINT('Ctrl Pts',(55.310045415862,24.9736678430967,3.41054258693119));
#241564=CARTESIAN_POINT('Ctrl Pts',(55.3621286647045,24.8573359723243,3.41100608859826));
#241565=CARTESIAN_POINT('Ctrl Pts',(55.2818999508935,24.82161584755,3.30819866970888));
#241566=CARTESIAN_POINT('Ctrl Pts',(55.269020915304,24.9555320242418,3.48823028058499));
#241567=CARTESIAN_POINT('Ctrl Pts',(55.3213695969755,24.8391888661847,3.48852004212277));
#241568=CARTESIAN_POINT('Ctrl Pts',(55.2204359898056,24.794250328961,3.42473028058498));
#241569=CARTESIAN_POINT('Origin',(55.168780436135,24.9102706020816,3.42473028058499));
#241570=CARTESIAN_POINT('Origin',(56.9479187893833,25.7023940320522,3.11913648178455));
#241571=CARTESIAN_POINT('Origin',(57.1106661007665,25.774853803565,2.8340419886028));
#241572=CARTESIAN_POINT('Origin',(55.0944632682972,24.8771824671427,3.56563113460844));
#241573=CARTESIAN_POINT('Origin',(55.0536014459541,24.8590452239602,3.64299171721836));
#241574=CARTESIAN_POINT('Ctrl Pts',(57.5052637377732,25.61970381813,2.59908173516042));
#241575=CARTESIAN_POINT('Ctrl Pts',(57.4711877340329,25.6045223014064,2.6587819886028));
#241576=CARTESIAN_POINT('Ctrl Pts',(57.4068835917979,25.5758735661211,2.6587819886028));
#241577=CARTESIAN_POINT('Ctrl Pts',(57.4694043465862,25.7001924885132,2.59908193475692));
#241578=CARTESIAN_POINT('Ctrl Pts',(57.4450643815391,25.6631501095112,2.65878715325466));
#241579=CARTESIAN_POINT('Ctrl Pts',(57.3861185493425,25.6224598624441,2.6587819886028));
#241580=CARTESIAN_POINT('Ctrl Pts',(57.4134642487754,25.7642825572403,2.63878778849882));
#241581=CARTESIAN_POINT('Ctrl Pts',(57.3998804953989,25.707732991239,2.69564460180121));
#241582=CARTESIAN_POINT('Ctrl Pts',(57.3441059191831,25.6552692732807,2.68180481624899));
#241583=CARTESIAN_POINT('Ctrl Pts',(57.3036982377901,25.8321626496793,2.75443238878672));
#241584=CARTESIAN_POINT('Ctrl Pts',(57.3186021074451,25.7409042554411,2.79268340777125));
#241585=CARTESIAN_POINT('Ctrl Pts',(57.252611247817,25.6821129719829,2.74885926835631));
#241586=CARTESIAN_POINT('Ctrl Pts',(57.2503778226942,25.8376543496547,2.8285665536168));
#241587=CARTESIAN_POINT('Ctrl Pts',(57.2821097063818,25.7289491719109,2.85384197230857));
#241588=CARTESIAN_POINT('Ctrl Pts',(57.2038640469265,25.677329395237,2.79184624278517));
#241589=CARTESIAN_POINT('Ctrl Pts',(57.2088336324698,25.8191582032623,2.90134173516043));
#241590=CARTESIAN_POINT('Ctrl Pts',(57.2611357920724,25.7028284190336,2.9016321871641));
#241591=CARTESIAN_POINT('Ctrl Pts',(57.1623216544371,25.6588335304443,2.83404198860281));
#241592=CARTESIAN_POINT('Origin',(57.4068835917979,25.5758735661211,2.53178198860279));
#241593=CARTESIAN_POINT('Origin',(-0.129138884176561,0.29005068280171,3.64303198860263));
#241594=CARTESIAN_POINT('Origin',(54.6869600343297,24.695750338031,3.64303198860281));
#241595=CARTESIAN_POINT('Origin',(5.51404277916147E-15,1.85815483521814E-13,
2.53178198860262));
#241596=CARTESIAN_POINT('Origin',(57.4192809246789,25.5480287005721,2.5317819886028));
#241597=CARTESIAN_POINT('Ctrl Pts',(54.6869600343297,24.695750338031,3.77003198860281));
#241598=CARTESIAN_POINT('Ctrl Pts',(54.7386929703524,24.579556261302,3.77003198860281));
#241599=CARTESIAN_POINT('Ctrl Pts',(54.738615530126,24.5797301948983,3.64284187937045));
#241600=CARTESIAN_POINT('Ctrl Pts',(54.4888352915928,24.6072881749597,3.77003198860281));
#241601=CARTESIAN_POINT('Ctrl Pts',(54.5406489234213,24.4913819335272,3.76980208962995));
#241602=CARTESIAN_POINT('Ctrl Pts',(54.5800991622565,24.5091541605505,3.64284193928275));
#241603=CARTESIAN_POINT('Ctrl Pts',(54.3002245846706,24.523071423676,3.65553535416607));
#241604=CARTESIAN_POINT('Ctrl Pts',(54.3520673354842,24.4074205468493,3.65520057834532));
#241605=CARTESIAN_POINT('Ctrl Pts',(54.4291945615844,24.4419671033155,3.55127910964304));
#241606=CARTESIAN_POINT('Ctrl Pts',(54.1952354911872,24.4761921430395,3.4715307213909));
#241607=CARTESIAN_POINT('Ctrl Pts',(54.2471777873471,24.3607210114366,3.471227462816));
#241608=CARTESIAN_POINT('Ctrl Pts',(54.3451938439593,24.404567574091,3.4041304590128));
#241609=CARTESIAN_POINT('Origin',(54.2933913980363,24.5205222915154,3.40423097483328));
#241610=CARTESIAN_POINT('Ctrl Pts',(57.467555354514,25.2380597013433,2.90134173516042));
#241611=CARTESIAN_POINT('Ctrl Pts',(57.4161024530843,25.3547675996718,2.9016321871641));
#241612=CARTESIAN_POINT('Ctrl Pts',(57.317288315449,25.3107727110825,2.8340419886028));
#241613=CARTESIAN_POINT('Ctrl Pts',(57.5091180232694,25.2565651278905,2.82853349835381));
#241614=CARTESIAN_POINT('Ctrl Pts',(57.4495672328897,25.3528749970544,2.85381483162391));
#241615=CARTESIAN_POINT('Ctrl Pts',(57.3588496371379,25.3292770036978,2.79182701594204));
#241616=CARTESIAN_POINT('Ctrl Pts',(57.5405471770611,25.2997972770058,2.7546882207365));
#241617=CARTESIAN_POINT('Ctrl Pts',(57.4827148996401,25.3720159720862,2.79286913083861));
#241618=CARTESIAN_POINT('Ctrl Pts',(57.3948558336735,25.3622324578623,2.74900763297944));
#241619=CARTESIAN_POINT('Ctrl Pts',(57.5636463159493,25.4257977880274,2.63954450640422));
#241620=CARTESIAN_POINT('Ctrl Pts',(57.5124644611998,25.4538910783599,2.6962768402887));
#241621=CARTESIAN_POINT('Ctrl Pts',(57.4360631077221,25.4475597357239,2.68224356036497));
#241622=CARTESIAN_POINT('Ctrl Pts',(57.5536211289093,25.5110385513886,2.59908178706382));
#241623=CARTESIAN_POINT('Ctrl Pts',(57.5097883065956,25.5177778164716,2.65878704321471));
#241624=CARTESIAN_POINT('Ctrl Pts',(57.4400754463057,25.5012707422385,2.6587819886028));
#241625=CARTESIAN_POINT('Ctrl Pts',(57.5176823163888,25.5918112338797,2.59908173516042));
#241626=CARTESIAN_POINT('Ctrl Pts',(57.4835989537477,25.5766462455179,2.6587819886028));
#241627=CARTESIAN_POINT('Ctrl Pts',(57.4192809246789,25.5480287005721,2.6587819886028));
#241628=CARTESIAN_POINT('Origin',(57.3689438691196,25.1947524379619,2.8340419886028));
#241629=CARTESIAN_POINT('Origin',(54.1306438627454,24.4480624203093,3.11913648167094));
#241630=CARTESIAN_POINT('Origin',(53.9678963272934,24.3756025490942,2.83404198860279));
#241631=CARTESIAN_POINT('Origin',(57.2061965577015,25.1222926664872,3.11913648177431));
#241632=CARTESIAN_POINT('Origin',(57.0434492461379,25.0498328948967,3.40423097483328));
#241633=CARTESIAN_POINT('Ctrl Pts',(53.8697418420145,24.3312692531091,2.90134173516041));
#241634=CARTESIAN_POINT('Ctrl Pts',(53.9216078643417,24.2159747902189,2.90103711553247));
#241635=CARTESIAN_POINT('Ctrl Pts',(54.0195518809641,24.2595822759735,2.83404198860279));
#241636=CARTESIAN_POINT('Ctrl Pts',(53.8282341734841,24.3127882662182,2.82862991747974));
#241637=CARTESIAN_POINT('Ctrl Pts',(53.8880114973698,24.2176496934292,2.85314045886379));
#241638=CARTESIAN_POINT('Ctrl Pts',(53.9780422761232,24.2411010091826,2.79187960999981));
#241639=CARTESIAN_POINT('Ctrl Pts',(53.7969955864427,24.2697746459844,2.75470625793349));
#241640=CARTESIAN_POINT('Ctrl Pts',(53.8549480733041,24.1983152114493,2.79224250381912));
#241641=CARTESIAN_POINT('Ctrl Pts',(53.9422730280819,24.2082687574725,2.7490180910828));
#241642=CARTESIAN_POINT('Ctrl Pts',(53.7744913425366,24.1443388226039,2.63947868311711));
#241643=CARTESIAN_POINT('Ctrl Pts',(53.825645022219,24.1165167429223,2.69595066767933));
#241644=CARTESIAN_POINT('Ctrl Pts',(53.9017956184508,24.1232032230476,2.68220539436075));
#241645=CARTESIAN_POINT('Ctrl Pts',(53.7848917482047,24.0595120258536,2.59908178585076));
#241646=CARTESIAN_POINT('Ctrl Pts',(53.8286685158637,24.0529122166846,2.65877670944865));
#241647=CARTESIAN_POINT('Ctrl Pts',(53.8982652496115,24.0696665464382,2.65878198860279));
#241648=CARTESIAN_POINT('Ctrl Pts',(53.8206887816836,23.9791663275016,2.59908173516041));
#241649=CARTESIAN_POINT('Ctrl Pts',(53.8547645473081,23.994348378682,2.65878198860279));
#241650=CARTESIAN_POINT('Ctrl Pts',(53.9190682401995,24.0229981225299,2.65878198860279));
#241651=CARTESIAN_POINT('Origin',(53.9190682401995,24.0229981225299,2.53178198860279));
#241652=CARTESIAN_POINT('Ctrl Pts',(56.6498810128382,24.8746050278055,3.77003198860281));
#241653=CARTESIAN_POINT('Ctrl Pts',(56.5981482837089,24.9907986398443,3.77003198860282));
#241654=CARTESIAN_POINT('Ctrl Pts',(56.5982255167331,24.9906251716318,3.64284238727617));
#241655=CARTESIAN_POINT('Ctrl Pts',(56.8481896769745,24.962653969475,3.77003198860281));
#241656=CARTESIAN_POINT('Ctrl Pts',(56.7965362315775,25.0791271905738,3.77025506105648));
#241657=CARTESIAN_POINT('Ctrl Pts',(56.7567415443552,25.0612010539389,3.64284210641936));
#241658=CARTESIAN_POINT('Ctrl Pts',(57.0369754593332,25.0464771582513,3.65553527987854));
#241659=CARTESIAN_POINT('Ctrl Pts',(56.9853490357203,25.1631925873308,3.65585996533124));
#241660=CARTESIAN_POINT('Ctrl Pts',(56.9076460727629,25.1283880784732,3.55127902710152));
#241661=CARTESIAN_POINT('Ctrl Pts',(57.1420619865021,25.0931373005748,3.4715307213909));
#241662=CARTESIAN_POINT('Ctrl Pts',(57.0905332166521,25.2100238867501,3.47182327905207));
#241663=CARTESIAN_POINT('Ctrl Pts',(56.9916465440541,25.1657874977297,3.40413028378006));
#241664=CARTESIAN_POINT('Origin',(56.6498810128382,24.8746050278055,3.64303198860281));
#241665=CARTESIAN_POINT('Origin',(5.71826297912856E-15,1.8634858490287E-13,
2.53178198860262));
#241666=CARTESIAN_POINT('Origin',(53.9314655730804,23.995153256981,2.53178198860279));
#241667=CARTESIAN_POINT('Origin',(52.0578415156894,22.8300973196051,3.64303198860279));
#241668=CARTESIAN_POINT('Origin',(56.2832472948513,24.7113125977908,3.64299466007434));
#241669=CARTESIAN_POINT('Ctrl Pts',(53.8330634946837,23.9513722670367,2.59908173516041));
#241670=CARTESIAN_POINT('Ctrl Pts',(53.867147095173,23.9665367208227,2.65878198860279));
#241671=CARTESIAN_POINT('Ctrl Pts',(53.9314655730804,23.995153256981,2.65878198860279));
#241672=CARTESIAN_POINT('Ctrl Pts',(53.8686972660497,23.871282165812,2.59908193199869));
#241673=CARTESIAN_POINT('Ctrl Pts',(53.8931046959184,23.9081865738553,2.65877685806683));
#241674=CARTESIAN_POINT('Ctrl Pts',(53.9521563342717,23.9486256024595,2.65878198860279));
#241675=CARTESIAN_POINT('Ctrl Pts',(53.9240892607412,23.8071866393156,2.63872492669835));
#241676=CARTESIAN_POINT('Ctrl Pts',(53.93785095296,23.8635355386145,2.69532212015295));
#241677=CARTESIAN_POINT('Ctrl Pts',(53.9937257232527,23.915575084618,2.68176836726654));
#241678=CARTESIAN_POINT('Ctrl Pts',(54.0330064121713,23.7392497560572,2.75442176402247));
#241679=CARTESIAN_POINT('Ctrl Pts',(54.018751292376,23.8300830854579,2.79203179920153));
#241680=CARTESIAN_POINT('Ctrl Pts',(54.0845104630313,23.8883623535218,2.7488531074819));
#241681=CARTESIAN_POINT('Ctrl Pts',(54.0860594545425,23.7337507958616,2.82866089558431));
#241682=CARTESIAN_POINT('Ctrl Pts',(54.0553500291274,23.8418399747432,2.85316563119239));
#241683=CARTESIAN_POINT('Ctrl Pts',(54.1330265677739,23.8930480394869,2.79189751796661));
#241684=CARTESIAN_POINT('Ctrl Pts',(54.1275498658873,23.752222950883,2.90134173516041));
#241685=CARTESIAN_POINT('Ctrl Pts',(54.0765745253536,23.8679139708571,2.90103711553246));
#241686=CARTESIAN_POINT('Ctrl Pts',(54.1745185419759,23.9115214566117,2.83404198860279));
#241687=CARTESIAN_POINT('Origin',(54.2261740956466,23.7955011834911,2.83404198860279));
#241688=CARTESIAN_POINT('Origin',(56.2428239368568,24.6933715410265,3.5664765397182));
#241689=CARTESIAN_POINT('Origin',(56.1680608984278,24.6600848917114,3.42473028058504));
#241690=CARTESIAN_POINT('Origin',(54.3889216310578,23.8679610547533,3.11913648168222));
#241691=CARTESIAN_POINT('Origin',(54.5516691663895,23.9404209259124,3.40423097483327));
#241692=CARTESIAN_POINT('Ctrl Pts',(55.8666273273833,24.5258780191674,3.36123028058499));
#241693=CARTESIAN_POINT('Ctrl Pts',(55.8149717737126,24.641898292288,3.36123028058499));
#241694=CARTESIAN_POINT('Ctrl Pts',(55.8149717737126,24.641898292288,3.23423028058499));
#241695=CARTESIAN_POINT('Ctrl Pts',(55.9487607347572,24.5627025231289,3.36123028058499));
#241696=CARTESIAN_POINT('Ctrl Pts',(55.897123215879,24.6784744708799,3.36099641108583));
#241697=CARTESIAN_POINT('Ctrl Pts',(55.9383132588164,24.6968134595447,3.23423043688445));
#241698=CARTESIAN_POINT('Ctrl Pts',(56.0264248009279,24.597521196072,3.41054258905304));
#241699=CARTESIAN_POINT('Ctrl Pts',(55.9751910510453,24.7132325104955,3.41008815826033));
#241700=CARTESIAN_POINT('Ctrl Pts',(56.0549414076397,24.7487396569153,3.3081986730433));
#241701=CARTESIAN_POINT('Ctrl Pts',(56.0673542004326,24.6158705164596,3.48823028058501));
#241702=CARTESIAN_POINT('Ctrl Pts',(56.0163785451197,24.7315703643338,3.48794691941618));
#241703=CARTESIAN_POINT('Ctrl Pts',(56.1164053447572,24.776105164832,3.42473028058503));
#241704=CARTESIAN_POINT('Origin',(55.8666273273833,24.5258780191674,3.23423028058499));
#241705=CARTESIAN_POINT('Ctrl Pts',(54.4530463244692,23.8971395307771,3.47153072139089));
#241706=CARTESIAN_POINT('Ctrl Pts',(54.4019907365351,24.0130054343465,3.47122746285094));
#241707=CARTESIAN_POINT('Ctrl Pts',(54.5001606088505,24.0565064908995,3.40413046676799));
#241708=CARTESIAN_POINT('Ctrl Pts',(54.5581374230425,23.9437939758158,3.65553813458006));
#241709=CARTESIAN_POINT('Ctrl Pts',(54.5068816478256,24.0597061770701,3.65520336072347));
#241710=CARTESIAN_POINT('Ctrl Pts',(54.5841625982694,24.0939065860605,3.55128134519988));
#241711=CARTESIAN_POINT('Ctrl Pts',(54.7469293531944,24.0276077026117,3.7700319886028));
#241712=CARTESIAN_POINT('Ctrl Pts',(54.6954643138422,24.1436691352881,3.76980209313998));
#241713=CARTESIAN_POINT('Ctrl Pts',(54.7350683949958,24.1610941752717,3.64284195387376));
#241714=CARTESIAN_POINT('Ctrl Pts',(54.9452378026828,24.1156489724279,3.77003198860281));
#241715=CARTESIAN_POINT('Ctrl Pts',(54.893504872635,24.2318430357372,3.77003198860282));
#241716=CARTESIAN_POINT('Ctrl Pts',(54.8935823068776,24.2316691155807,3.64284189403809));
#241717=CARTESIAN_POINT('Origin',(54.9452378026828,24.1156489724279,3.64303198860281));
#241718=CARTESIAN_POINT('Origin',(50.7999799080414,22.2700612497319,3.23423028058498));
#241719=CARTESIAN_POINT('Origin',(55.7284918401498,24.4643761377919,3.23423028058499));
#241720=CARTESIAN_POINT('Origin',(50.6030043228557,22.1823620689018,3.64303198860279));
#241721=CARTESIAN_POINT('Origin',(55.3119205422645,24.2788510342448,3.64299171721805));
#241722=CARTESIAN_POINT('Ctrl Pts',(55.5277679687683,24.3743766270217,3.48823028058498));
#241723=CARTESIAN_POINT('Ctrl Pts',(55.4763362579874,24.4911280468229,3.48852004212277));
#241724=CARTESIAN_POINT('Ctrl Pts',(55.3754026508175,24.4461895095991,3.42473028058498));
#241725=CARTESIAN_POINT('Ctrl Pts',(55.5688345658069,24.3927905570421,3.41028005848426));
#241726=CARTESIAN_POINT('Ctrl Pts',(55.517233105522,24.509336496484,3.41074404220322));
#241727=CARTESIAN_POINT('Ctrl Pts',(55.4370743056941,24.4736474994207,3.30780486243939));
#241728=CARTESIAN_POINT('Ctrl Pts',(55.6466353090193,24.4276751358089,3.36123028058499));
#241729=CARTESIAN_POINT('Ctrl Pts',(55.5948055748756,24.5438739850311,3.36146460586506));
#241730=CARTESIAN_POINT('Ctrl Pts',(55.55391025049,24.5256662135189,3.23423045308453));
#241731=CARTESIAN_POINT('Ctrl Pts',(55.7284918401498,24.464376137792,3.36123028058499));
#241732=CARTESIAN_POINT('Ctrl Pts',(55.6768362864792,24.5803964109126,3.36123028058499));
#241733=CARTESIAN_POINT('Ctrl Pts',(55.6768362864792,24.5803964109126,3.23423028058499));
#241734=CARTESIAN_POINT('Origin',(55.4270582044881,24.3301692364785,3.42473028058498));
#241735=CARTESIAN_POINT('Origin',(55.3527410377821,24.2970811017195,3.56563113524761));
#241736=CARTESIAN_POINT('Origin',(53.036059683551,30.9870007556513,3.56647653909479));
#241737=CARTESIAN_POINT('Origin',(53.0743345559679,31.0091584503691,3.64299466007737));
#241738=CARTESIAN_POINT('Origin',(52.9651856060845,30.9460815882871,3.42473028058506));
#241739=CARTESIAN_POINT('Ctrl Pts',(52.8702215132216,30.8905967158739,3.48823028058506));
#241740=CARTESIAN_POINT('Ctrl Pts',(52.9338619179795,30.7813498801535,3.48794691941622));
#241741=CARTESIAN_POINT('Ctrl Pts',(53.0286856060846,30.8360963620065,3.42473028058507));
#241742=CARTESIAN_POINT('Ctrl Pts',(52.8311874403365,30.8681941459775,3.41028005925108));
#241743=CARTESIAN_POINT('Ctrl Pts',(52.8946849835393,30.7587310665082,3.40982512231106));
#241744=CARTESIAN_POINT('Ctrl Pts',(52.9702219582397,30.8023423591854,3.30780486372904));
#241745=CARTESIAN_POINT('Ctrl Pts',(52.7572372522458,30.8257530395514,3.36123028058504));
#241746=CARTESIAN_POINT('Ctrl Pts',(52.820547425344,30.7159277273268,3.36099721048389));
#241747=CARTESIAN_POINT('Ctrl Pts',(52.8594635164579,30.7383959430077,3.23423045308414));
#241748=CARTESIAN_POINT('Ctrl Pts',(52.6794317578287,30.7811015270746,3.36123028058504));
#241749=CARTESIAN_POINT('Ctrl Pts',(52.7429317578287,30.671116300794,3.36123028058504));
#241750=CARTESIAN_POINT('Ctrl Pts',(52.7429317578287,30.671116300794,3.23423028058503));
#241751=CARTESIAN_POINT('Origin',(52.6794317578287,30.7811015270746,3.23423028058504));
#241752=CARTESIAN_POINT('Origin',(-0.158749999999995,0.274963065701743,
3.64303198860263));
#241753=CARTESIAN_POINT('Origin',(53.4219427993286,31.2097904767608,3.64303198860285));
#241754=CARTESIAN_POINT('Origin',(-0.158749999999995,0.274963065701746,
3.23423028058482));
#241755=CARTESIAN_POINT('Origin',(52.5484816883959,30.7054974692372,3.23423028058504));
#241756=CARTESIAN_POINT('Ctrl Pts',(53.888035839597,31.4795232016792,3.47153072139094));
#241757=CARTESIAN_POINT('Ctrl Pts',(53.9523112176912,31.3691313491577,3.47182327902685));
#241758=CARTESIAN_POINT('Ctrl Pts',(53.858399113013,31.3151318426937,3.40413028959057));
#241759=CARTESIAN_POINT('Ctrl Pts',(53.7885171709474,31.4219316852026,3.6555380712098));
#241760=CARTESIAN_POINT('Ctrl Pts',(53.8525966788902,31.3115614337853,3.65586275496962));
#241761=CARTESIAN_POINT('Ctrl Pts',(53.7787668993598,31.2691561625552,3.55128126837278));
#241762=CARTESIAN_POINT('Ctrl Pts',(53.6097358757352,31.3184699958133,3.77003198860286));
#241763=CARTESIAN_POINT('Ctrl Pts',(53.6736035436629,31.2082202476918,3.77025505748367));
#241764=CARTESIAN_POINT('Ctrl Pts',(53.6357108652104,31.1865627224602,3.64284211731176));
#241765=CARTESIAN_POINT('Ctrl Pts',(53.4219427993286,31.2097904767608,3.77003198860286));
#241766=CARTESIAN_POINT('Ctrl Pts',(53.485537665384,31.0996409376523,3.77003198860286));
#241767=CARTESIAN_POINT('Ctrl Pts',(53.4854427285717,31.0998053730349,3.64284239821734));
#241768=CARTESIAN_POINT('Origin',(53.7950387249979,31.4251975098795,3.40423097483333));
#241769=CARTESIAN_POINT('Ctrl Pts',(52.5484816883959,30.7054974692372,3.36123028058504));
#241770=CARTESIAN_POINT('Ctrl Pts',(52.6119816883959,30.5955122429565,3.36123028058503));
#241771=CARTESIAN_POINT('Ctrl Pts',(52.6119816883959,30.5955122429565,3.23423028058503));
#241772=CARTESIAN_POINT('Ctrl Pts',(52.4704129317475,30.6606955449586,3.36123028058504));
#241773=CARTESIAN_POINT('Ctrl Pts',(52.5339553345216,30.5504637065426,3.3614653861012));
#241774=CARTESIAN_POINT('Ctrl Pts',(52.4950560684217,30.5280052047893,3.23423043688428));
#241775=CARTESIAN_POINT('Ctrl Pts',(52.3965920780925,30.6183335281986,3.41054258693123));
#241776=CARTESIAN_POINT('Ctrl Pts',(52.4605500011269,30.5080831175481,3.41100608859759));
#241777=CARTESIAN_POINT('Ctrl Pts',(52.3844945583568,30.4641724871913,3.30819866970862));
#241778=CARTESIAN_POINT('Ctrl Pts',(52.3576880233162,30.5960088312571,3.48823028058503));
#241779=CARTESIAN_POINT('Ctrl Pts',(52.4219111049556,30.4857749404423,3.48852004212281));
#241780=CARTESIAN_POINT('Ctrl Pts',(52.3262277788841,30.4305321463779,3.42473028058503));
#241781=CARTESIAN_POINT('Origin',(52.2627277788841,30.5405173726585,3.42473028058503));
#241782=CARTESIAN_POINT('Origin',(53.9493203812233,31.5142720656054,3.11913648178361));
#241783=CARTESIAN_POINT('Origin',(54.1036020372438,31.6033466212668,2.83404198860284));
#241784=CARTESIAN_POINT('Origin',(52.1922763801647,30.4998422386367,3.5656311346083));
#241785=CARTESIAN_POINT('Origin',(52.1535342613179,30.4775331296741,3.64299171721819));
#241786=CARTESIAN_POINT('Ctrl Pts',(54.5122556166611,31.490293248291,2.59908173516046));
#241787=CARTESIAN_POINT('Ctrl Pts',(54.4799531854479,31.4716329851992,2.65878198860284));
#241788=CARTESIAN_POINT('Ctrl Pts',(54.4189959163063,31.4364195775137,2.65878198860284));
#241789=CARTESIAN_POINT('Ctrl Pts',(54.4681793099455,31.5665926662618,2.59908193475672));
#241790=CARTESIAN_POINT('Ctrl Pts',(54.4478446647267,31.5272089901455,2.65878715325372));
#241791=CARTESIAN_POINT('Ctrl Pts',(54.3934750329626,31.4805801312539,2.65878198860284));
#241792=CARTESIAN_POINT('Ctrl Pts',(54.4058464214486,31.6244843104271,2.6387877884991));
#241793=CARTESIAN_POINT('Ctrl Pts',(54.3982481205272,31.5668246399996,2.69564460180143));
#241794=CARTESIAN_POINT('Ctrl Pts',(54.3482630350908,31.5088182930362,2.68180481624906));
#241795=CARTESIAN_POINT('Ctrl Pts',(54.2895863184077,31.6805188761702,2.75443238878651));
#241796=CARTESIAN_POINT('Ctrl Pts',(54.3139476428151,31.5913182835557,2.7926834077711));
#241797=CARTESIAN_POINT('Ctrl Pts',(54.2544636505346,31.5259511417533,2.74885926835632));
#241798=CARTESIAN_POINT('Ctrl Pts',(54.2359839591651,31.680406990988,2.82856655361704));
#241799=CARTESIAN_POINT('Ctrl Pts',(54.2789047974504,31.5756141966208,2.85384197230815));
#241800=CARTESIAN_POINT('Ctrl Pts',(54.2064835118364,31.5160982999433,2.79184624278487));
#241801=CARTESIAN_POINT('Ctrl Pts',(54.1966007261207,31.6576696180587,2.90134173516047));
#241802=CARTESIAN_POINT('Ctrl Pts',(54.2607761425982,31.5474441649286,2.90163218716414));
#241803=CARTESIAN_POINT('Ctrl Pts',(54.1671020372438,31.4933613949861,2.83404198860285));
#241804=CARTESIAN_POINT('Origin',(54.4189959163063,31.4364195775137,2.53178198860284));
#241805=CARTESIAN_POINT('Origin',(-0.158749999999995,0.274963065701743,
3.64303198860263));
#241806=CARTESIAN_POINT('Origin',(51.8059703131946,30.2768083268883,3.64303198860284));
#241807=CARTESIAN_POINT('Origin',(5.52187834149254E-15,1.85800105364867E-13,
2.53178198860262));
#241808=CARTESIAN_POINT('Origin',(54.4342359163063,31.4100231232064,2.53178198860284));
#241809=CARTESIAN_POINT('Ctrl Pts',(51.8059703131946,30.2768083268883,3.77003198860285));
#241810=CARTESIAN_POINT('Ctrl Pts',(51.8695654390622,30.166658337772,3.77003198860285));
#241811=CARTESIAN_POINT('Ctrl Pts',(51.8694702420498,30.1668232238341,3.6428418793704));
#241812=CARTESIAN_POINT('Ctrl Pts',(51.6181777324915,30.1681210939092,3.77003198860285));
#241813=CARTESIAN_POINT('Ctrl Pts',(51.6818230251222,30.058265798306,3.76980208962999));
#241814=CARTESIAN_POINT('Ctrl Pts',(51.7191994478437,30.080064340051,3.64284193928282));
#241815=CARTESIAN_POINT('Ctrl Pts',(51.4394033023493,30.0646505034507,3.65553535416608));
#241816=CARTESIAN_POINT('Ctrl Pts',(51.5030508615805,29.955052217304,3.65520057834494));
#241817=CARTESIAN_POINT('Ctrl Pts',(51.5761444782068,29.9974715145366,3.55127910964311));
#241818=CARTESIAN_POINT('Ctrl Pts',(51.3398895692697,30.007053683816,3.47153072139095));
#241819=CARTESIAN_POINT('Ctrl Pts',(51.4036173400347,29.8976445635502,3.47122746281605));
#241820=CARTESIAN_POINT('Ctrl Pts',(51.4965132406194,29.95149639792,3.40413045901281));
#241821=CARTESIAN_POINT('Origin',(51.4328740054943,30.0614010732039,3.40423097483332));
#241822=CARTESIAN_POINT('Ctrl Pts',(54.5146464769138,31.1067982185537,2.90134173516046));
#241823=CARTESIAN_POINT('Ctrl Pts',(54.4512761425982,31.2174884860868,2.90163218716414));
#241824=CARTESIAN_POINT('Ctrl Pts',(54.3576020372438,31.1634057161443,2.83404198860284));
#241825=CARTESIAN_POINT('Ctrl Pts',(54.5540471172215,31.1295467523331,2.82853349835374));
#241826=CARTESIAN_POINT('Ctrl Pts',(54.4847554296818,31.2191042733499,2.85381483162335));
#241827=CARTESIAN_POINT('Ctrl Pts',(54.3970014563935,31.1861529813963,2.79182701594249));
#241828=CARTESIAN_POINT('Ctrl Pts',(54.5807851087096,31.1758273123592,2.75468822073668));
#241829=CARTESIAN_POINT('Ctrl Pts',(54.5157207333379,31.2416052667856,2.79286913083842));
#241830=CARTESIAN_POINT('Ctrl Pts',(54.4293656242358,31.2226915745262,2.74900763297926));
#241831=CARTESIAN_POINT('Ctrl Pts',(54.5905870683104,31.3035520968882,2.63954450640412));
#241832=CARTESIAN_POINT('Ctrl Pts',(54.5367490446513,31.3261415286127,2.69627684028892));
#241833=CARTESIAN_POINT('Ctrl Pts',(54.4614280312972,31.3118587536638,2.68224356036523));
#241834=CARTESIAN_POINT('Ctrl Pts',(54.5717067142914,31.3872779850337,2.59908178706453));
#241835=CARTESIAN_POINT('Ctrl Pts',(54.5274095677396,31.3893985541597,2.65878704321558));
#241836=CARTESIAN_POINT('Ctrl Pts',(54.4598040608963,31.3656949292502,2.65878198860284));
#241837=CARTESIAN_POINT('Ctrl Pts',(54.5275217339719,31.4638515574743,2.59908173516046));
#241838=CARTESIAN_POINT('Ctrl Pts',(54.4952102564865,31.4452069629856,2.65878198860284));
#241839=CARTESIAN_POINT('Ctrl Pts',(54.4342359163063,31.4100231232064,2.65878198860284));
#241840=CARTESIAN_POINT('Origin',(54.4211020372438,31.0534204898637,2.83404198860284));
#241841=CARTESIAN_POINT('Origin',(51.2785921372156,29.9723263949883,3.11913648167148));
#241842=CARTESIAN_POINT('Origin',(51.1243102687785,29.8832517167489,2.83404198860284));
#241843=CARTESIAN_POINT('Origin',(54.2668203811903,30.9643459342355,3.11913648177614));
#241844=CARTESIAN_POINT('Origin',(54.1125387249979,30.8752713784764,3.40423097483332));
#241845=CARTESIAN_POINT('Ctrl Pts',(51.0313275753408,29.8289013456888,2.90134173516045));
#241846=CARTESIAN_POINT('Ctrl Pts',(51.0949610232001,29.7196599535395,2.90103711553251));
#241847=CARTESIAN_POINT('Ctrl Pts',(51.1878102687784,29.7732664904682,2.83404198860283));
#241848=CARTESIAN_POINT('Ctrl Pts',(50.991979079321,29.8061828667727,2.82862991747972));
#241849=CARTESIAN_POINT('Ctrl Pts',(51.0613736255819,29.7178139048432,2.85314045886472));
#241850=CARTESIAN_POINT('Ctrl Pts',(51.148459876313,29.7505475307856,2.7918796099996));
#241851=CARTESIAN_POINT('Ctrl Pts',(50.9654077681508,29.7601395581527,2.75470625793362));
#241852=CARTESIAN_POINT('Ctrl Pts',(51.0305123301031,29.6951292702712,2.79224250381908));
#241853=CARTESIAN_POINT('Ctrl Pts',(51.1163184807723,29.7141562330558,2.74901809108276));
#241854=CARTESIAN_POINT('Ctrl Pts',(50.9561384187038,29.6330385513052,2.63947868311705));
#241855=CARTESIAN_POINT('Ctrl Pts',(51.009920072411,29.6107158994146,2.69595066767941));
#241856=CARTESIAN_POINT('Ctrl Pts',(51.0849545802162,29.6253256551031,2.68220539436086));
#241857=CARTESIAN_POINT('Ctrl Pts',(50.9753486645701,29.5497635830445,2.59908178585111));
#241858=CARTESIAN_POINT('Ctrl Pts',(51.0195754864254,29.5477758465711,2.65877670944928));
#241859=CARTESIAN_POINT('Ctrl Pts',(51.0870396576422,29.5717132339806,2.65878198860283));
#241860=CARTESIAN_POINT('Ctrl Pts',(51.0193480105327,29.473599835734,2.59908173516044));
#241861=CARTESIAN_POINT('Ctrl Pts',(51.0516501490686,29.4922606054649,2.65878198860283));
#241862=CARTESIAN_POINT('Ctrl Pts',(51.1126068659047,29.5274749692187,2.65878198860283));
#241863=CARTESIAN_POINT('Origin',(51.1126068659047,29.5274749692187,2.53178198860283));
#241864=CARTESIAN_POINT('Ctrl Pts',(53.7394427993286,30.6598643453577,3.77003198860285));
#241865=CARTESIAN_POINT('Ctrl Pts',(53.6758479277943,30.770013893956,3.77003198860286));
#241866=CARTESIAN_POINT('Ctrl Pts',(53.6759428700937,30.7698494490696,3.64284238727595));
#241867=CARTESIAN_POINT('Ctrl Pts',(53.927461487289,30.7681598456258,3.77003198860286));
#241868=CARTESIAN_POINT('Ctrl Pts',(53.8639162380539,30.8785957589617,3.77025506105754));
#241869=CARTESIAN_POINT('Ctrl Pts',(53.8262133418071,30.8566081460782,3.64284210641868));
#241870=CARTESIAN_POINT('Ctrl Pts',(54.1064511722693,30.8712573299213,3.65553527987854));
#241871=CARTESIAN_POINT('Ctrl Pts',(54.0429074791695,30.9819369489461,3.65585996533185));
#241872=CARTESIAN_POINT('Ctrl Pts',(53.9692682429978,30.9392009315198,3.5512790271026));
#241873=CARTESIAN_POINT('Ctrl Pts',(54.2060847114741,30.9286463962981,3.47153072139093));
#241874=CARTESIAN_POINT('Ctrl Pts',(54.1426202463872,31.039506442398,3.4718232790521));
#241875=CARTESIAN_POINT('Ctrl Pts',(54.0488992470932,30.9851759130204,3.40413028377995));
#241876=CARTESIAN_POINT('Origin',(53.7394427993286,30.6598643453577,3.64303198860285));
#241877=CARTESIAN_POINT('Origin',(5.71547558359784E-15,1.86354055474621E-13,
2.53178198860262));
#241878=CARTESIAN_POINT('Origin',(51.1278468659047,29.5010785149114,2.53178198860283));
#241879=CARTESIAN_POINT('Origin',(46.8255917980722,26.6681506086454,3.64303198860282));
#241880=CARTESIAN_POINT('Origin',(53.3918862459818,30.4591427892376,3.64299466007562));
#241881=CARTESIAN_POINT('Ctrl Pts',(51.0345602039887,29.4472515437738,2.59908173516044));
#241882=CARTESIAN_POINT('Ctrl Pts',(51.0668719738977,29.465895631477,2.65878198860283));
#241883=CARTESIAN_POINT('Ctrl Pts',(51.1278468659047,29.5010785149114,2.65878198860283));
#241884=CARTESIAN_POINT('Ctrl Pts',(51.0783704650305,29.371324927865,2.59908193199872));
#241885=CARTESIAN_POINT('Ctrl Pts',(51.0987866273845,29.4105784408362,2.65877685806679));
#241886=CARTESIAN_POINT('Ctrl Pts',(51.1532877451687,29.4569685172212,2.65878198860283));
#241887=CARTESIAN_POINT('Ctrl Pts',(51.1401588234664,29.3133705634513,2.63872492669832));
#241888=CARTESIAN_POINT('Ctrl Pts',(51.147955063845,29.3708492661237,2.6953221201529));
#241889=CARTESIAN_POINT('Ctrl Pts',(51.1980841325267,29.4284442379234,2.68176836726648));
#241890=CARTESIAN_POINT('Ctrl Pts',(51.255580653351,29.2571907880105,2.75442176402257));
#241891=CARTESIAN_POINT('Ctrl Pts',(51.2319089562575,29.3460364571626,2.79203179920163));
#241892=CARTESIAN_POINT('Ctrl Pts',(51.2912160489646,29.4108701703525,2.74885310748203));
#241893=CARTESIAN_POINT('Ctrl Pts',(51.3089178634639,29.2572675046847,2.8286608955843));
#241894=CARTESIAN_POINT('Ctrl Pts',(51.267078271731,29.3615545506877,2.85316563119254));
#241895=CARTESIAN_POINT('Ctrl Pts',(51.338976589856,29.4206015015123,2.79189751796631));
#241896=CARTESIAN_POINT('Ctrl Pts',(51.3482501200165,29.2799753962465,2.90134173516044));
#241897=CARTESIAN_POINT('Ctrl Pts',(51.2854610232001,29.3897042746976,2.9010371155325));
#241898=CARTESIAN_POINT('Ctrl Pts',(51.3783102687784,29.4433108116264,2.83404198860283));
#241899=CARTESIAN_POINT('Origin',(51.4418102687785,29.3333255853458,2.83404198860283));
#241900=CARTESIAN_POINT('Origin',(53.3535596824668,30.4370746239672,3.56647653971804));
#241901=CARTESIAN_POINT('Origin',(53.2826856060845,30.396155456884,3.42473028058507));
#241902=CARTESIAN_POINT('Origin',(51.5960921371718,29.4224002636282,3.11913648168176));
#241903=CARTESIAN_POINT('Origin',(51.7503740054943,29.5114749418008,3.40423097483332));
#241904=CARTESIAN_POINT('Ctrl Pts',(52.9969317578287,30.2311753956715,3.36123028058503));
#241905=CARTESIAN_POINT('Ctrl Pts',(52.9334317578287,30.3411606219521,3.36123028058504));
#241906=CARTESIAN_POINT('Ctrl Pts',(52.9334317578287,30.3411606219521,3.23423028058503));
#241907=CARTESIAN_POINT('Ctrl Pts',(53.0747660209942,30.2763834500021,3.36123028058503));
#241908=CARTESIAN_POINT('Ctrl Pts',(53.0113099140584,30.3861235964147,3.36099641108553));
#241909=CARTESIAN_POINT('Ctrl Pts',(53.0503573673275,30.4086676540714,3.23423043688406));
#241910=CARTESIAN_POINT('Ctrl Pts',(53.1483650929077,30.3191294881009,3.41054258905306));
#241911=CARTESIAN_POINT('Ctrl Pts',(53.0853168809886,30.4288515386958,3.41008815826037));
#241912=CARTESIAN_POINT('Ctrl Pts',(53.1609188493357,30.4725003554708,3.30819867304338));
#241913=CARTESIAN_POINT('Ctrl Pts',(53.1871522506175,30.3416565762239,3.48823028058505));
#241914=CARTESIAN_POINT('Ctrl Pts',(53.1243619179795,30.4513942013116,3.48794691941621));
#241915=CARTESIAN_POINT('Ctrl Pts',(53.2191856060846,30.5061406831646,3.42473028058506));
#241916=CARTESIAN_POINT('Origin',(52.9969317578287,30.2311753956715,3.23423028058503));
#241917=CARTESIAN_POINT('Ctrl Pts',(51.6568155675427,29.4581217525676,3.47153072139093));
#241918=CARTESIAN_POINT('Ctrl Pts',(51.5939283826162,29.5680161684459,3.47122746285098));
#241919=CARTESIAN_POINT('Ctrl Pts',(51.6870133715071,29.6215404675519,3.40413046676814));
#241920=CARTESIAN_POINT('Ctrl Pts',(51.7564542486376,29.515505630712,3.65553813458009));
#241921=CARTESIAN_POINT('Ctrl Pts',(51.6933631336487,29.6254251653805,3.65520336072143));
#241922=CARTESIAN_POINT('Ctrl Pts',(51.7666458147661,29.6675162799441,3.5512813451999));
#241923=CARTESIAN_POINT('Ctrl Pts',(51.9354510367811,29.6185943474767,3.77003198860285));
#241924=CARTESIAN_POINT('Ctrl Pts',(51.8721362050985,29.7286404220052,3.76980209314336));
#241925=CARTESIAN_POINT('Ctrl Pts',(51.9097019182966,29.7501097595411,3.64284195387409));
#241926=CARTESIAN_POINT('Ctrl Pts',(52.1234703131946,29.7268821954852,3.77003198860285));
#241927=CARTESIAN_POINT('Ctrl Pts',(52.059875194672,29.8370321718797,3.77003198860284));
#241928=CARTESIAN_POINT('Ctrl Pts',(52.0599703843284,29.8368672985585,3.64284189403835));
#241929=CARTESIAN_POINT('Origin',(52.1234703131946,29.7268821954852,3.64303198860285));
#241930=CARTESIAN_POINT('Origin',(45.6951875,26.0155113828602,3.234230280585));
#241931=CARTESIAN_POINT('Origin',(52.8659816883959,30.155571337834,3.23423028058503));
#241932=CARTESIAN_POINT('Origin',(45.518171167873,25.9133109558558,3.64303198860281));
#241933=CARTESIAN_POINT('Origin',(52.4710850656383,29.9275190026066,3.64299171721804));
#241934=CARTESIAN_POINT('Ctrl Pts',(52.6757649139395,30.0450834959839,3.48823028058502));
#241935=CARTESIAN_POINT('Ctrl Pts',(52.6124111049556,30.1558192616004,3.4885200421228));
#241936=CARTESIAN_POINT('Ctrl Pts',(52.5167277788841,30.100576467536,3.42473028058502));
#241937=CARTESIAN_POINT('Ctrl Pts',(52.7146817640555,30.0676891808481,3.41028005848428));
#241938=CARTESIAN_POINT('Ctrl Pts',(52.6511806140155,30.1782028480908,3.41074404220291));
#241939=CARTESIAN_POINT('Ctrl Pts',(52.5751914484999,30.1343304829265,3.30780486243907));
#241940=CARTESIAN_POINT('Ctrl Pts',(52.788409875246,30.1105150503714,3.36123028058503));
#241941=CARTESIAN_POINT('Ctrl Pts',(52.7247179826696,30.2206596676792,3.36146460586399));
#241942=CARTESIAN_POINT('Ctrl Pts',(52.6859499175234,30.1982769148323,3.23423045308413));
#241943=CARTESIAN_POINT('Ctrl Pts',(52.8659816883959,30.155571337834,3.36123028058503));
#241944=CARTESIAN_POINT('Ctrl Pts',(52.8024816883959,30.2655565641147,3.36123028058503));
#241945=CARTESIAN_POINT('Ctrl Pts',(52.8024816883959,30.2655565641147,3.23423028058503));
#241946=CARTESIAN_POINT('Origin',(52.5802277788841,29.9905912412554,3.42473028058502));
#241947=CARTESIAN_POINT('Origin',(52.5097763812721,29.9499161075317,3.56563113524805));
#241948=CARTESIAN_POINT('Origin',(49.5064990290884,36.3610285397823,3.56647653909451));
#241949=CARTESIAN_POINT('Origin',(49.5422481179706,36.3870656659281,3.64299466007424));
#241950=CARTESIAN_POINT('Origin',(49.4402904249165,36.3129251734945,3.4247302805851));
#241951=CARTESIAN_POINT('Ctrl Pts',(49.3516463037385,36.2478178023253,3.48823028058509));
#241952=CARTESIAN_POINT('Ctrl Pts',(49.4263574835551,36.1458216659128,3.48794691941626));
#241953=CARTESIAN_POINT('Ctrl Pts',(49.5149391519577,36.2101800152089,3.4247302805851));
#241954=CARTESIAN_POINT('Ctrl Pts',(49.3151677697919,36.2214577843991,3.41028005925111));
#241955=CARTESIAN_POINT('Ctrl Pts',(49.389759474291,36.1192316557425,3.40982512230885));
#241956=CARTESIAN_POINT('Ctrl Pts',(49.4603240281395,36.1704998050828,3.30780486372839));
#241957=CARTESIAN_POINT('Ctrl Pts',(49.2460589922039,36.1715192752743,3.36123028058507));
#241958=CARTESIAN_POINT('Ctrl Pts',(49.3205022166664,36.068913312703,3.36099721048721));
#241959=CARTESIAN_POINT('Ctrl Pts',(49.3568565533006,36.095326284347,3.23423045308392));
#241960=CARTESIAN_POINT('Ctrl Pts',(49.1733470784087,36.1189794796885,3.36123028058507));
#241961=CARTESIAN_POINT('Ctrl Pts',(49.2479958054498,36.0162343214029,3.36123028058507));
#241962=CARTESIAN_POINT('Ctrl Pts',(49.2479958054498,36.0162343214029,3.23423028058507));
#241963=CARTESIAN_POINT('Origin',(49.1733470784087,36.1189794796885,3.23423028058507));
#241964=CARTESIAN_POINT('Origin',(-0.186621817602855,0.256862895714229,
3.64303198860263));
#241965=CARTESIAN_POINT('Origin',(49.8669803696025,36.6229335645812,3.64303198860289));
#241966=CARTESIAN_POINT('Origin',(-0.186621817602855,0.256862895714232,
3.23423028058482));
#241967=CARTESIAN_POINT('Origin',(49.0510171431403,36.0301015792679,3.23423028058507));
#241968=CARTESIAN_POINT('Ctrl Pts',(50.3023253561995,36.9399086546489,3.47153072139097));
#241969=CARTESIAN_POINT('Ctrl Pts',(50.377787717749,36.8368401467435,3.47182327902688));
#241970=CARTESIAN_POINT('Ctrl Pts',(50.2900345588334,36.773319967242,3.40413028959026));
#241971=CARTESIAN_POINT('Ctrl Pts',(50.209371813944,36.8722300970252,3.65553807120984));
#241972=CARTESIAN_POINT('Ctrl Pts',(50.2846371204137,36.769162597888,3.65586275497155));
#241973=CARTESIAN_POINT('Ctrl Pts',(50.2156443459751,36.7192723137729,3.55128126837369));
#241974=CARTESIAN_POINT('Ctrl Pts',(50.0423845927715,36.7506474475471,3.7700319886029));
#241975=CARTESIAN_POINT('Ctrl Pts',(50.1174266236742,36.6476776482614,3.77025505748318));
#241976=CARTESIAN_POINT('Ctrl Pts',(50.0820053531117,36.6221779017691,3.64284211731108));
#241977=CARTESIAN_POINT('Ctrl Pts',(49.8669803696025,36.6229335645812,3.7700319886029));
#241978=CARTESIAN_POINT('Ctrl Pts',(49.9417406183807,36.520034909793,3.7700319886029));
#241979=CARTESIAN_POINT('Ctrl Pts',(49.9416290134639,36.5201885207827,3.64284239821673));
#241980=CARTESIAN_POINT('Origin',(50.2155162706044,36.8761597191957,3.40423097483336));
#241981=CARTESIAN_POINT('Ctrl Pts',(49.0510171431403,36.0301015792679,3.36123028058507));
#241982=CARTESIAN_POINT('Ctrl Pts',(49.1256658701815,35.9273564209823,3.36123028058507));
#241983=CARTESIAN_POINT('Ctrl Pts',(49.1256658701815,35.9273564209823,3.23423028058507));
#241984=CARTESIAN_POINT('Ctrl Pts',(48.9780591316061,35.9773846774559,3.36123028058507));
#241985=CARTESIAN_POINT('Ctrl Pts',(49.0527758071189,35.8743986902987,3.36146538610131));
#241986=CARTESIAN_POINT('Ctrl Pts',(49.0164371879466,35.8479971380607,3.23423043688408));
#241987=CARTESIAN_POINT('Ctrl Pts',(48.9090707128234,35.9275383438676,3.41054258693127));
#241988=CARTESIAN_POINT('Ctrl Pts',(48.9842025736675,35.8245773199113,3.41100608859846));
#241989=CARTESIAN_POINT('Ctrl Pts',(48.9131536812798,35.7729572780257,3.30819866970899));
#241990=CARTESIAN_POINT('Ctrl Pts',(48.8727133447943,35.9012693628907,3.48823028058506));
#241991=CARTESIAN_POINT('Ctrl Pts',(48.9481071848796,35.7983524848938,3.48852004212283));
#241992=CARTESIAN_POINT('Ctrl Pts',(48.85872246645,35.7334106856009,3.42473028058505));
#241993=CARTESIAN_POINT('Origin',(48.7840737394089,35.8361558438865,3.42473028058506));
#241994=CARTESIAN_POINT('Origin',(50.3596419293496,36.9808731396203,3.11913648178429));
#241995=CARTESIAN_POINT('Origin',(50.5037675878945,37.0855865599605,2.83404198860288));
#241996=CARTESIAN_POINT('Origin',(48.7182599900761,35.7883393560613,3.56563113460849));
#241997=CARTESIAN_POINT('Origin',(48.6820620414867,35.7621028045851,3.64299171721869));
#241998=CARTESIAN_POINT('Ctrl Pts',(50.9219998155899,37.0158684358562,2.5990817351605));
#241999=CARTESIAN_POINT('Ctrl Pts',(50.8918248691,36.9939338721436,2.65878198860288));
#242000=CARTESIAN_POINT('Ctrl Pts',(50.8348823336486,36.9525415975215,2.65878198860288));
#242001=CARTESIAN_POINT('Ctrl Pts',(50.8701895025858,37.0871426490245,2.59908193475663));
#242002=CARTESIAN_POINT('Ctrl Pts',(50.8540829678233,37.0458491715908,2.65878715325424));
#242003=CARTESIAN_POINT('Ctrl Pts',(50.8048852215549,36.9937925764104,2.65878198860288));
#242004=CARTESIAN_POINT('Ctrl Pts',(50.8021467555733,37.1382015956602,2.63878778849918));
#242005=CARTESIAN_POINT('Ctrl Pts',(50.8006171556815,37.0800635522215,2.69564460180147));
#242006=CARTESIAN_POINT('Ctrl Pts',(50.7569692080811,37.0171501059292,2.6818048162493));
#242007=CARTESIAN_POINT('Ctrl Pts',(50.6806663304944,37.181776708279,2.75443238878649));
#242008=CARTESIAN_POINT('Ctrl Pts',(50.7142182018865,37.0956112176475,2.7926834077711));
#242009=CARTESIAN_POINT('Ctrl Pts',(50.6618927960203,37.0243843935852,2.74885926835615));
#242010=CARTESIAN_POINT('Ctrl Pts',(50.6273693057705,37.1760624637761,2.8285665536171));
#242011=CARTESIAN_POINT('Ctrl Pts',(50.6810088489707,37.076330184568,2.85384197230783));
#242012=CARTESIAN_POINT('Ctrl Pts',(50.6152053999547,37.0095702365076,2.79184624278437));
#242013=CARTESIAN_POINT('Ctrl Pts',(50.5905785208484,37.1493329797263,2.9013417351605));
#242014=CARTESIAN_POINT('Ctrl Pts',(50.6659240749083,37.0464195108255,2.90163218716417));
#242015=CARTESIAN_POINT('Ctrl Pts',(50.5784163149356,36.9828414016749,2.83404198860288));
#242016=CARTESIAN_POINT('Origin',(50.8348823336486,36.9525415975215,2.53178198860288));
#242017=CARTESIAN_POINT('Origin',(-0.186621817602855,0.256862895714229,
3.64303198860263));
#242018=CARTESIAN_POINT('Origin',(48.3573835402119,35.5261472678868,3.64303198860288));
#242019=CARTESIAN_POINT('Origin',(5.53127843490691E-15,1.85785630490362E-13,
2.53178198860262));
#242020=CARTESIAN_POINT('Origin',(50.8527980281384,36.9278827595329,2.53178198860288));
#242021=CARTESIAN_POINT('Ctrl Pts',(48.3573835402119,35.5261472678868,3.77003198860288));
#242022=CARTESIAN_POINT('Ctrl Pts',(48.4321440944169,35.4232481927146,3.77003198860289));
#242023=CARTESIAN_POINT('Ctrl Pts',(48.4320321836173,35.4234022247158,3.64284187937085));
#242024=CARTESIAN_POINT('Ctrl Pts',(48.1819806163552,35.3984257650681,3.77003198860288));
#242025=CARTESIAN_POINT('Ctrl Pts',(48.2567602586451,35.2958250128978,3.76980208962949));
#242026=CARTESIAN_POINT('Ctrl Pts',(48.2916533613389,35.3214110399815,3.64284193928375));
#242027=CARTESIAN_POINT('Ctrl Pts',(48.0150011530601,35.2768349808768,3.65553535416611));
#242028=CARTESIAN_POINT('Ctrl Pts',(48.0897561847312,35.1744900671688,3.65520057834472));
#242029=CARTESIAN_POINT('Ctrl Pts',(48.1580153629278,35.2243173504725,3.55127910964188));
#242030=CARTESIAN_POINT('Ctrl Pts',(47.9220530736687,35.209151665053,3.47153072139098));
#242031=CARTESIAN_POINT('Ctrl Pts',(47.9968681042461,35.1070032653416,3.47122746281608));
#242032=CARTESIAN_POINT('Ctrl Pts',(48.0836260618766,35.1702703594595,3.40413045901306));
#242033=CARTESIAN_POINT('Origin',(48.0088472823272,35.2729208539817,3.40423097483335));
#242034=CARTESIAN_POINT('Ctrl Pts',(50.9644637245892,36.6347241449657,2.90134173516049));
#242035=CARTESIAN_POINT('Ctrl Pts',(50.8898702560317,36.7381840359687,2.90163218716417));
#242036=CARTESIAN_POINT('Ctrl Pts',(50.8023624960591,36.6746059268181,2.83404198860288));
#242037=CARTESIAN_POINT('Ctrl Pts',(51.0012706547893,36.6614665482799,2.82853349835375));
#242038=CARTESIAN_POINT('Ctrl Pts',(50.9229972443171,36.7432905102108,2.85381483162291));
#242039=CARTESIAN_POINT('Ctrl Pts',(50.8391683443882,36.7013469409085,2.79182701594282));
#242040=CARTESIAN_POINT('Ctrl Pts',(51.0230245369437,36.7102884597168,2.75468822073677));
#242041=CARTESIAN_POINT('Ctrl Pts',(50.9514409225353,36.768904996455,2.79286913083859));
#242042=CARTESIAN_POINT('Ctrl Pts',(50.8675358949426,36.7410683485314,2.74900763297934));
#242043=CARTESIAN_POINT('Ctrl Pts',(51.0194219249361,36.8383381382864,2.63954450640411));
#242044=CARTESIAN_POINT('Ctrl Pts',(50.9635175930192,36.8551762168621,2.6962768402889));
#242045=CARTESIAN_POINT('Ctrl Pts',(50.8901021525742,36.8330984946708,2.68224356036522));
#242046=CARTESIAN_POINT('Ctrl Pts',(50.9918932610486,36.9196318328646,2.59908178706433));
#242047=CARTESIAN_POINT('Ctrl Pts',(50.9476171190683,36.9171104726343,2.65878704321594));
#242048=CARTESIAN_POINT('Ctrl Pts',(50.8828596657515,36.8864699989243,2.65878198860288));
#242049=CARTESIAN_POINT('Ctrl Pts',(50.9399462128201,36.991167339171,2.5990817351605));
#242050=CARTESIAN_POINT('Ctrl Pts',(50.9097606317994,36.9692474126343,2.65878198860288));
#242051=CARTESIAN_POINT('Ctrl Pts',(50.8527980281385,36.9278827595329,2.65878198860288));
#242052=CARTESIAN_POINT('Origin',(50.8770112231002,36.5718607685324,2.83404198860286));
#242053=CARTESIAN_POINT('Origin',(47.8647214254968,35.1682072895727,3.11913648167076));
#242054=CARTESIAN_POINT('Origin',(47.720595568509,35.0634937251224,2.83404198860287));
#242055=CARTESIAN_POINT('Origin',(50.732885564516,36.4671473482239,3.11913648177603));
#242056=CARTESIAN_POINT('Origin',(50.5887599058101,36.3624339277676,3.40423097483335));
#242057=CARTESIAN_POINT('Ctrl Pts',(47.6338034047599,34.9997217530263,2.90134173516048));
#242058=CARTESIAN_POINT('Ctrl Pts',(47.7085070967803,34.8977303031705,2.90103711553254));
#242059=CARTESIAN_POINT('Ctrl Pts',(47.7952442955502,34.9607485668368,2.83404198860287));
#242060=CARTESIAN_POINT('Ctrl Pts',(47.5970451916064,34.9730146904951,2.82862991747981));
#242061=CARTESIAN_POINT('Ctrl Pts',(47.6752966590732,34.8923835282627,2.85314045886538));
#242062=CARTESIAN_POINT('Ctrl Pts',(47.7584842465947,34.9340408279391,2.79187960999998));
#242063=CARTESIAN_POINT('Ctrl Pts',(47.5754322771535,34.9244461536127,2.75470625793358));
#242064=CARTESIAN_POINT('Ctrl Pts',(47.6469756149923,34.8665972787025,2.7922425038192));
#242065=CARTESIAN_POINT('Ctrl Pts',(47.7303228514092,34.8944891948625,2.74901809108285));
#242066=CARTESIAN_POINT('Ctrl Pts',(47.5794993790985,34.7970725085259,2.63947868311716));
#242067=CARTESIAN_POINT('Ctrl Pts',(47.6353197637775,34.7804938560724,2.69595066767937));
#242068=CARTESIAN_POINT('Ctrl Pts',(47.7084160893875,34.8028668197836,2.68220539436084));
#242069=CARTESIAN_POINT('Ctrl Pts',(47.6073089936889,34.7162617467346,2.59908178585162));
#242070=CARTESIAN_POINT('Ctrl Pts',(47.6515013114269,34.7189078610138,2.65877670944829));
#242071=CARTESIAN_POINT('Ctrl Pts',(47.7160937685338,34.7497660430532,2.65878198860287));
#242072=CARTESIAN_POINT('Ctrl Pts',(47.6590285860935,34.6451144164188,2.59908173516048));
#242073=CARTESIAN_POINT('Ctrl Pts',(47.6892031885513,34.667049453402,2.65878198860287));
#242074=CARTESIAN_POINT('Ctrl Pts',(47.7461450747864,34.7084426211234,2.65878198860287));
#242075=CARTESIAN_POINT('Origin',(47.7461450747864,34.7084426211234,2.53178198860287));
#242076=CARTESIAN_POINT('Ctrl Pts',(50.2402240048083,36.1092077731531,3.77003198860289));
#242077=CARTESIAN_POINT('Ctrl Pts',(50.1654637495898,36.2121064368056,3.77003198860289));
#242078=CARTESIAN_POINT('Ctrl Pts',(50.1655753609565,36.2119528169383,3.64284238727618));
#242079=CARTESIAN_POINT('Ctrl Pts',(50.4158927445022,36.2365633238567,3.77003198860289));
#242080=CARTESIAN_POINT('Ctrl Pts',(50.341151906482,36.3397519704545,3.77025506105886));
#242081=CARTESIAN_POINT('Ctrl Pts',(50.3059538820309,36.3139437822109,3.64284210641865));
#242082=CARTESIAN_POINT('Ctrl Pts',(50.5831252836564,36.3578055460627,3.6555352798786));
#242083=CARTESIAN_POINT('Ctrl Pts',(50.5083605190613,36.4612367259645,3.65585996533031));
#242084=CARTESIAN_POINT('Ctrl Pts',(50.4395918165622,36.4110374247138,3.55127902710232));
#242085=CARTESIAN_POINT('Ctrl Pts',(50.6762142289948,36.4252947698681,3.47153072139098));
#242086=CARTESIAN_POINT('Ctrl Pts',(50.6015093986315,36.5289136700282,3.47182327905215));
#242087=CARTESIAN_POINT('Ctrl Pts',(50.5139808995222,36.4650842569434,3.4041302837801));
#242088=CARTESIAN_POINT('Origin',(50.2402240048083,36.1092077731531,3.64303198860289));
#242089=CARTESIAN_POINT('Origin',(5.7121316272531E-15,1.86359204715837E-13,
2.53178198860262));
#242090=CARTESIAN_POINT('Origin',(47.7640607692763,34.6837837831348,2.53178198860287));
#242091=CARTESIAN_POINT('Origin',(40.9117478092586,29.3316730956006,3.64303198860284));
#242092=CARTESIAN_POINT('Origin',(49.915552518433,35.8732562382983,3.64299466007548));
#242093=CARTESIAN_POINT('Ctrl Pts',(47.6769115920304,34.6205005703637,2.59908173516048));
#242094=CARTESIAN_POINT('Ctrl Pts',(47.7070975168463,34.6424200234577,2.65878198860287));
#242095=CARTESIAN_POINT('Ctrl Pts',(47.7640607692763,34.6837837831348,2.65878198860287));
#242096=CARTESIAN_POINT('Ctrl Pts',(47.7284183483602,34.549569307663,2.59908193199826));
#242097=CARTESIAN_POINT('Ctrl Pts',(47.744619559451,34.590741855859,2.65877685806643));
#242098=CARTESIAN_POINT('Ctrl Pts',(47.7939730310146,34.6425747206405,2.65878198860287));
#242099=CARTESIAN_POINT('Ctrl Pts',(47.7959261043553,34.4983910654768,2.63872492669804));
#242100=CARTESIAN_POINT('Ctrl Pts',(47.7976714756521,34.5563698228279,2.69532212015263));
#242101=CARTESIAN_POINT('Ctrl Pts',(47.8415056181567,34.6188891978603,2.68176836726639));
#242102=CARTESIAN_POINT('Ctrl Pts',(47.9165880269729,34.4545839152295,2.75442176402293));
#242103=CARTESIAN_POINT('Ctrl Pts',(47.8837591046489,34.5404685123899,2.79203179920204));
#242104=CARTESIAN_POINT('Ctrl Pts',(47.9359643384885,34.6111463389766,2.7488531074822));
#242105=CARTESIAN_POINT('Ctrl Pts',(47.9696250311907,34.4602354682512,2.8286608955841));
#242106=CARTESIAN_POINT('Ctrl Pts',(47.9171136764626,34.5595777906759,2.85316563119194));
#242107=CARTESIAN_POINT('Ctrl Pts',(47.9824460410473,34.6258166968299,2.79189751796707));
#242108=CARTESIAN_POINT('Ctrl Pts',(48.0063682005187,34.4869303039399,2.90134173516047));
#242109=CARTESIAN_POINT('Ctrl Pts',(47.9324532779037,34.5894948283136,2.90103711553254));
#242110=CARTESIAN_POINT('Ctrl Pts',(48.0191904766736,34.6525130919799,2.83404198860286));
#242111=CARTESIAN_POINT('Origin',(48.0938392037147,34.5497679336943,2.83404198860286));
#242112=CARTESIAN_POINT('Origin',(49.8797426632439,35.8473027479614,3.56647653971835));
#242113=CARTESIAN_POINT('Origin',(49.8135340601223,35.7991993820665,3.42473028058511));
#242114=CARTESIAN_POINT('Origin',(48.2379650606502,34.6544814981832,3.11913648168303));
#242115=CARTESIAN_POINT('Origin',(48.3820909175329,34.7591950625537,3.40423097483335));
#242116=CARTESIAN_POINT('Ctrl Pts',(49.5465907136144,35.6052536882605,3.36123028058507));
#242117=CARTESIAN_POINT('Ctrl Pts',(49.4719419865733,35.7079988465461,3.36123028058507));
#242118=CARTESIAN_POINT('Ctrl Pts',(49.4719419865733,35.7079988465461,3.23423028058507));
#242119=CARTESIAN_POINT('Ctrl Pts',(49.6192730640952,35.6583499840585,3.36123028058507));
#242120=CARTESIAN_POINT('Ctrl Pts',(49.5446936074896,35.7608559931228,3.36099641108551));
#242121=CARTESIAN_POINT('Ctrl Pts',(49.5811706590218,35.7873581223575,3.23423043688383));
#242122=CARTESIAN_POINT('Ctrl Pts',(49.6880007749183,35.7085550527735,3.41054258905307));
#242123=CARTESIAN_POINT('Ctrl Pts',(49.613828870366,35.8110857017915,3.41008815826029));
#242124=CARTESIAN_POINT('Ctrl Pts',(49.6844541394801,35.8623979633508,3.30819867304359));
#242125=CARTESIAN_POINT('Ctrl Pts',(49.7242207306175,35.7350130971392,3.48823028058509));
#242126=CARTESIAN_POINT('Ctrl Pts',(49.6503036646785,35.8375861910559,3.48794691941625));
#242127=CARTESIAN_POINT('Ctrl Pts',(49.7388853330811,35.9019445403521,3.4247302805851));
#242128=CARTESIAN_POINT('Origin',(49.5465907136144,35.6052536882604,3.23423028058507));
#242129=CARTESIAN_POINT('Ctrl Pts',(48.2946219293746,34.6963546279288,3.47153072139098));
#242130=CARTESIAN_POINT('Ctrl Pts',(48.2205921526138,34.7990735298986,3.47122746285102));
#242131=CARTESIAN_POINT('Ctrl Pts',(48.3075723994626,34.8620346481359,3.40413046676832));
#242132=CARTESIAN_POINT('Ctrl Pts',(48.3877165307493,34.7638392294026,3.65553813458009));
#242133=CARTESIAN_POINT('Ctrl Pts',(48.3134813154532,34.8665617960676,3.65520336072165));
#242134=CARTESIAN_POINT('Ctrl Pts',(48.3819628268506,34.916082457139,3.55128134519971));
#242135=CARTESIAN_POINT('Ctrl Pts',(48.554957050614,34.8850734745865,3.77003198860289));
#242136=CARTESIAN_POINT('Ctrl Pts',(48.4804861171424,34.9878985031416,3.76980209314062));
#242137=CARTESIAN_POINT('Ctrl Pts',(48.5156018845759,35.0131769156733,3.64284195387393));
#242138=CARTESIAN_POINT('Ctrl Pts',(48.7306271754176,35.0124214764587,3.77003198860288));
#242139=CARTESIAN_POINT('Ctrl Pts',(48.655866629847,35.1153205397466,3.77003198860288));
#242140=CARTESIAN_POINT('Ctrl Pts',(48.6559785319992,35.1151665196475,3.64284189403863));
#242141=CARTESIAN_POINT('Origin',(48.7306271754176,35.0124214764587,3.64303198860288));
#242142=CARTESIAN_POINT('Origin',(39.9252688514646,28.6149541797808,3.23423028058502));
#242143=CARTESIAN_POINT('Origin',(49.424260778346,35.5163757878398,3.23423028058507));
#242144=CARTESIAN_POINT('Origin',(39.7707905934405,28.5027191556742,3.64303198860283));
#242145=CARTESIAN_POINT('Origin',(49.0553654007526,35.2482948100398,3.64299171721812));
#242146=CARTESIAN_POINT('Ctrl Pts',(49.2466351556012,35.3866101428262,3.48823028058506));
#242147=CARTESIAN_POINT('Ctrl Pts',(49.1720533660031,35.4901170100369,3.48852004212285));
#242148=CARTESIAN_POINT('Ctrl Pts',(49.0826686475734,35.425175210744,3.42473028058506));
#242149=CARTESIAN_POINT('Ctrl Pts',(49.2829758776385,35.4131599099239,3.41028005848434));
#242150=CARTESIAN_POINT('Ctrl Pts',(49.2082707697383,35.5164304941074,3.41074404220394));
#242151=CARTESIAN_POINT('Ctrl Pts',(49.1372837917345,35.4648554356502,3.30780486243961));
#242152=CARTESIAN_POINT('Ctrl Pts',(49.3518235761936,35.4634578610135,3.36123028058507));
#242153=CARTESIAN_POINT('Ctrl Pts',(49.2769673468815,35.5663414789286,3.36146460586394));
#242154=CARTESIAN_POINT('Ctrl Pts',(49.2407512920129,35.5400289748689,3.2342304530846));
#242155=CARTESIAN_POINT('Ctrl Pts',(49.424260778346,35.5163757878398,3.36123028058507));
#242156=CARTESIAN_POINT('Ctrl Pts',(49.3496120513049,35.6191209461254,3.36123028058507));
#242157=CARTESIAN_POINT('Ctrl Pts',(49.3496120513049,35.6191209461254,3.23423028058507));
#242158=CARTESIAN_POINT('Origin',(49.1573173746146,35.3224300524584,3.42473028058506));
#242159=CARTESIAN_POINT('Origin',(49.0915036263521,35.2746135650472,3.56563113524886));
#242160=CARTESIAN_POINT('Origin',(45.434534811362,41.3366772861974,3.56647653909408));
#242161=CARTESIAN_POINT('Origin',(45.467366442211,41.3663085755643,3.64299466007437));
#242162=CARTESIAN_POINT('Origin',(45.3737170758072,41.2819167515331,3.42473028058513));
#242163=CARTESIAN_POINT('Ctrl Pts',(45.2923641298557,41.207900211591,3.48823028058513));
#242164=CARTESIAN_POINT('Ctrl Pts',(45.3773275334105,41.1142722655009,3.48794691941629));
#242165=CARTESIAN_POINT('Ctrl Pts',(45.4586966628148,41.1875373586975,3.42473028058514));
#242166=CARTESIAN_POINT('Ctrl Pts',(45.2588408013013,41.1778715515044,3.41028005925115));
#242167=CARTESIAN_POINT('Ctrl Pts',(45.3437094247747,41.0840023845244,3.40982512230998));
#242168=CARTESIAN_POINT('Ctrl Pts',(45.4085284377455,41.1423656859498,3.30780486372877));
#242169=CARTESIAN_POINT('Ctrl Pts',(45.1953306044445,41.1209827764382,3.36123028058511));
#242170=CARTESIAN_POINT('Ctrl Pts',(45.2800912647191,41.0267203359203,3.3609972104844));
#242171=CARTESIAN_POINT('Ctrl Pts',(45.3134855411616,41.0567886774839,3.23423045308378));
#242172=CARTESIAN_POINT('Ctrl Pts',(45.1285089182132,41.0611303347406,3.36123028058511));
#242173=CARTESIAN_POINT('Ctrl Pts',(45.2134885052208,40.966750941905,3.36123028058511));
#242174=CARTESIAN_POINT('Ctrl Pts',(45.2134885052208,40.966750941905,3.23423028058511));
#242175=CARTESIAN_POINT('Origin',(45.1285089182132,41.0611303347407,3.23423028058511));
#242176=CARTESIAN_POINT('Origin',(-0.212448967518932,0.235948482089256,
3.64303198860263));
#242177=CARTESIAN_POINT('Origin',(45.7656648676106,41.6348281284264,3.64303198860292));
#242178=CARTESIAN_POINT('Origin',(-0.212448967518932,0.235948482089259,
3.23423028058482));
#242179=CARTESIAN_POINT('Origin',(45.0161393894793,40.9599523566127,3.23423028058511));
#242180=CARTESIAN_POINT('Ctrl Pts',(46.1654920697611,41.9955727382253,3.47153072139101));
#242181=CARTESIAN_POINT('Ctrl Pts',(46.2513146333407,41.9009568150781,3.47182327902692));
#242182=CARTESIAN_POINT('Ctrl Pts',(46.1706818621617,41.8286119029178,3.4041302895905));
#242183=CARTESIAN_POINT('Ctrl Pts',(46.0801220723609,41.918548639894,3.65553807120987));
#242184=CARTESIAN_POINT('Ctrl Pts',(46.1657485549047,41.823913122127,3.65586275497073));
#242185=CARTESIAN_POINT('Ctrl Pts',(46.1023486848312,41.7670844335153,3.55128126837336));
#242186=CARTESIAN_POINT('Ctrl Pts',(45.9267584721668,41.7801771152782,3.77003198860294));
#242187=CARTESIAN_POINT('Ctrl Pts',(46.0121526898534,41.6856154234963,3.77025505748536));
#242188=CARTESIAN_POINT('Ctrl Pts',(45.9795909100358,41.6565528363061,3.64284211731136));
#242189=CARTESIAN_POINT('Ctrl Pts',(45.7656648676106,41.6348281284264,3.77003198860293));
#242190=CARTESIAN_POINT('Ctrl Pts',(45.8507714101807,41.5403077371542,3.77003198860292));
#242191=CARTESIAN_POINT('Ctrl Pts',(45.8506443599268,41.5404488407561,3.64284239821717));
#242192=CARTESIAN_POINT('Origin',(46.0858221116777,41.9230990057958,3.4042309748334));
#242193=CARTESIAN_POINT('Ctrl Pts',(45.0161393894793,40.9599523566127,3.36123028058511));
#242194=CARTESIAN_POINT('Ctrl Pts',(45.1011189764868,40.8655729637771,3.36123028058511));
#242195=CARTESIAN_POINT('Ctrl Pts',(45.1011189764868,40.8655729637771,3.23423028058511));
#242196=CARTESIAN_POINT('Ctrl Pts',(44.9490914662984,40.8998980546784,3.36123028058511));
#242197=CARTESIAN_POINT('Ctrl Pts',(45.0341638030238,40.8052862548076,3.36146538609985));
#242198=CARTESIAN_POINT('Ctrl Pts',(45.0007839642919,40.7752309130122,3.23423043688394));
#242199=CARTESIAN_POINT('Ctrl Pts',(44.885691333943,40.843113531121,3.41054258693128));
#242200=CARTESIAN_POINT('Ctrl Pts',(44.9711739721975,40.7485699563826,3.41100608859847));
#242201=CARTESIAN_POINT('Ctrl Pts',(44.9059100567345,40.6898060629491,3.3081986697091));
#242202=CARTESIAN_POINT('Ctrl Pts',(44.8522789915941,40.8131880745609,3.4882302805851));
#242203=CARTESIAN_POINT('Ctrl Pts',(44.9380175594362,40.718715788234,3.48852004212289));
#242204=CARTESIAN_POINT('Ctrl Pts',(44.8559107663285,40.6447864996555,3.4247302805851));
#242205=CARTESIAN_POINT('Origin',(44.7709311793209,40.7391658924911,3.4247302805851));
#242206=CARTESIAN_POINT('Origin',(46.2182127020614,42.0423040287743,3.11913648178372));
#242207=CARTESIAN_POINT('Origin',(46.3506032922594,42.1615090516455,2.83404198860292));
#242208=CARTESIAN_POINT('Origin',(44.7104761485842,40.6847319383097,3.5656311346084));
#242209=CARTESIAN_POINT('Origin',(44.6772189625508,40.6548553974686,3.64299171721753));
#242210=CARTESIAN_POINT('Ctrl Pts',(46.7738319284257,42.1358900227698,2.59908173516054));
#242211=CARTESIAN_POINT('Ctrl Pts',(46.7461150696872,42.1109214781064,2.65878198860292));
#242212=CARTESIAN_POINT('Ctrl Pts',(46.6938111422604,42.0638038389703,2.65878198860292));
#242213=CARTESIAN_POINT('Ctrl Pts',(46.7148552537637,42.2013581359408,2.59908193475748));
#242214=CARTESIAN_POINT('Ctrl Pts',(46.7031532960233,42.1586072771698,2.65878715325374));
#242215=CARTESIAN_POINT('Ctrl Pts',(46.6596664560525,42.1016932886501,2.65878198860292));
#242216=CARTESIAN_POINT('Ctrl Pts',(46.6418481388115,42.245024972543,2.63878778849886));
#242217=CARTESIAN_POINT('Ctrl Pts',(46.646403998566,42.1870455286636,2.69564460180144));
#242218=CARTESIAN_POINT('Ctrl Pts',(46.6095714048494,42.1199142759252,2.68180481624926));
#242219=CARTESIAN_POINT('Ctrl Pts',(46.5164783566527,42.2756632139847,2.75443238878691));
#242220=CARTESIAN_POINT('Ctrl Pts',(46.558853173705,42.1934768724826,2.79268340777122));
#242221=CARTESIAN_POINT('Ctrl Pts',(46.5142596423497,42.1171707421502,2.74885926835627));
#242222=CARTESIAN_POINT('Ctrl Pts',(46.4640705998045,42.2644092166193,2.82856655361689));
#242223=CARTESIAN_POINT('Ctrl Pts',(46.527841161857,42.1708301402926,2.85384197230662));
#242224=CARTESIAN_POINT('Ctrl Pts',(46.4693765057995,42.0975575768112,2.79184624278484));
#242225=CARTESIAN_POINT('Ctrl Pts',(46.4302753505424,42.2339804752704,2.90134173516054));
#242226=CARTESIAN_POINT('Ctrl Pts',(46.5159655405274,42.1395065321002,2.90163218716422));
#242227=CARTESIAN_POINT('Ctrl Pts',(46.435582879267,42.0671296588098,2.83404198860292));
#242228=CARTESIAN_POINT('Origin',(46.6938111422604,42.0638038389703,2.53178198860292));
#242229=CARTESIAN_POINT('Origin',(-0.212448967518932,0.235948482089256,
3.64303198860263));
#242230=CARTESIAN_POINT('Origin',(44.3789831537295,40.3862543050941,3.64303198860291));
#242231=CARTESIAN_POINT('Origin',(5.54214007001405E-15,1.85772217488052E-13,
2.53178198860262));
#242232=CARTESIAN_POINT('Origin',(46.7142062431422,42.0411527846897,2.53178198860292));
#242233=CARTESIAN_POINT('Ctrl Pts',(44.3789831537295,40.3862543050941,3.77003198860292));
#242234=CARTESIAN_POINT('Ctrl Pts',(44.4640900439956,40.2917335276664,3.77003198860292));
#242235=CARTESIAN_POINT('Ctrl Pts',(44.4639626455268,40.2918750180002,3.64284187937102));
#242236=CARTESIAN_POINT('Ctrl Pts',(44.2178916378581,40.2408978759484,3.77003198860292));
#242237=CARTESIAN_POINT('Ctrl Pts',(44.3029863283938,40.1466757825266,3.76980208962809));
#242238=CARTESIAN_POINT('Ctrl Pts',(44.3350138149322,40.1757689690794,3.64284193928359));
#242239=CARTESIAN_POINT('Ctrl Pts',(44.0645366033527,40.1025190721003,3.65553535416613));
#242240=CARTESIAN_POINT('Ctrl Pts',(44.1495800756941,40.0085488431226,3.65520057834485));
#242241=CARTESIAN_POINT('Ctrl Pts',(44.212256953616,40.0652381943521,3.55127910964236));
#242242=CARTESIAN_POINT('Ctrl Pts',(43.9791725362582,40.0254908126591,3.47153072139101));
#242243=CARTESIAN_POINT('Ctrl Pts',(44.0642551375171,39.9317222927449,3.47122746281612));
#242244=CARTESIAN_POINT('Ctrl Pts',(44.1439246138546,40.0037114790886,3.40413045901317));
#242245=CARTESIAN_POINT('Origin',(44.0588255818377,40.0979831325501,3.40423097483339));
#242246=CARTESIAN_POINT('Ctrl Pts',(46.8559036426985,41.7612723673365,2.90134173516054));
#242247=CARTESIAN_POINT('Ctrl Pts',(46.7709043015502,41.8563683535933,2.90163218716421));
#242248=CARTESIAN_POINT('Ctrl Pts',(46.6905216402897,41.7839914803029,2.83404198860292));
#242249=CARTESIAN_POINT('Ctrl Pts',(46.8897135983608,41.7917156448191,2.82853349835381));
#242250=CARTESIAN_POINT('Ctrl Pts',(46.8033160448221,41.8649095672142,2.85381483162275));
#242251=CARTESIAN_POINT('Ctrl Pts',(46.7243306652211,41.814433263085,2.79182701594198));
#242252=CARTESIAN_POINT('Ctrl Pts',(46.9062450310969,41.842544004588,2.7546882207368));
#242253=CARTESIAN_POINT('Ctrl Pts',(46.8289264627106,41.8933569085954,2.7928691308389));
#242254=CARTESIAN_POINT('Ctrl Pts',(46.7483907976682,41.8569022891471,2.74900763297958));
#242255=CARTESIAN_POINT('Ctrl Pts',(46.8892773184517,41.9695156381237,2.63954450640415));
#242256=CARTESIAN_POINT('Ctrl Pts',(46.8319191778368,41.9804178820379,2.69627684028872));
#242257=CARTESIAN_POINT('Ctrl Pts',(46.7612136652291,41.950787100749,2.68224356036506));
#242258=CARTESIAN_POINT('Ctrl Pts',(46.8534019544985,42.0474864684053,2.59908178706327));
#242259=CARTESIAN_POINT('Ctrl Pts',(46.8096319157677,42.0403508033704,2.65878704321586));
#242260=CARTESIAN_POINT('Ctrl Pts',(46.748432012186,42.0031091843004,2.65878198860292));
#242261=CARTESIAN_POINT('Ctrl Pts',(46.7942619810916,42.1132001506003,2.59908173516054));
#242262=CARTESIAN_POINT('Ctrl Pts',(46.7665330160779,42.0882450513177,2.65878198860292));
#242263=CARTESIAN_POINT('Ctrl Pts',(46.7142062431422,42.0411527846897,2.65878198860292));
#242264=CARTESIAN_POINT('Origin',(46.7755012272973,41.6896120874673,2.83404198860291));
#242265=CARTESIAN_POINT('Origin',(43.926434809502,39.9787779456778,3.11913648166835));
#242266=CARTESIAN_POINT('Origin',(43.7940440370144,39.8595727587358,2.83404198860291));
#242267=CARTESIAN_POINT('Origin',(46.6431106370583,41.5704070646225,3.11913648177571));
#242268=CARTESIAN_POINT('Origin',(46.5107200467156,41.4512020416176,3.40423097483339));
#242269=CARTESIAN_POINT('Ctrl Pts',(43.7143933160623,39.787077884675,2.90134173516052));
#242270=CARTESIAN_POINT('Ctrl Pts',(43.7993487829613,39.6934538167803,2.90103711553257));
#242271=CARTESIAN_POINT('Ctrl Pts',(43.8790236240219,39.7651933659001,2.8340419886029));
#242272=CARTESIAN_POINT('Ctrl Pts',(43.680628116452,39.7566748466924,2.8286299174798));
#242273=CARTESIAN_POINT('Ctrl Pts',(43.7668791656722,39.6846648960474,2.85314045886468));
#242274=CARTESIAN_POINT('Ctrl Pts',(43.8452566693654,39.7347894633637,2.79187960999967));
#242275=CARTESIAN_POINT('Ctrl Pts',(43.6642103943288,39.7061132086031,2.7547062579337));
#242276=CARTESIAN_POINT('Ctrl Pts',(43.7414086642733,39.6560595510442,2.79224250381923));
#242277=CARTESIAN_POINT('Ctrl Pts',(43.8213838166747,39.6925108309093,2.74901809108282));
#242278=CARTESIAN_POINT('Ctrl Pts',(43.6815693876451,39.579862457588,2.63947868311711));
#242279=CARTESIAN_POINT('Ctrl Pts',(43.7388169234803,39.5692094437566,2.69595066767941));
#242280=CARTESIAN_POINT('Ctrl Pts',(43.8091742082548,39.5991004926181,2.68220539436094));
#242281=CARTESIAN_POINT('Ctrl Pts',(43.7176736830026,39.5024012818818,2.59908178585113));
#242282=CARTESIAN_POINT('Ctrl Pts',(43.7613473163392,39.5096522555303,2.6587767094491));
#242283=CARTESIAN_POINT('Ctrl Pts',(43.8223603708606,39.5470931435004,2.6587819886029));
#242284=CARTESIAN_POINT('Ctrl Pts',(43.7765468711722,39.4370498736011,2.59908173516051));
#242285=CARTESIAN_POINT('Ctrl Pts',(43.8042633382929,39.4620188529812,2.6587819886029));
#242286=CARTESIAN_POINT('Ctrl Pts',(43.8565665267056,39.5091373124625,2.6587819886029));
#242287=CARTESIAN_POINT('Origin',(43.8565665267056,39.5091373124625,2.5317819886029));
#242288=CARTESIAN_POINT('Ctrl Pts',(46.1905628026484,41.1629311642483,3.77003198860293));
#242289=CARTESIAN_POINT('Ctrl Pts',(46.1054562527465,41.2574515636634,3.77003198860293));
#242290=CARTESIAN_POINT('Ctrl Pts',(46.1055833103431,41.2573104519064,3.64284238727623));
#242291=CARTESIAN_POINT('Ctrl Pts',(46.3519569306026,41.3079514313235,3.77003198860293));
#242292=CARTESIAN_POINT('Ctrl Pts',(46.2668393800555,41.4027622547774,3.77025506105961));
#242293=CARTESIAN_POINT('Ctrl Pts',(46.2345318643233,41.3734162510829,3.6428421064187));
#242294=CARTESIAN_POINT('Ctrl Pts',(46.5056000892405,41.4460100362752,3.65553527987858));
#242295=CARTESIAN_POINT('Ctrl Pts',(46.4204333915653,41.541059563398,3.65585996533035));
#242296=CARTESIAN_POINT('Ctrl Pts',(46.3572886670239,41.4839469723853,3.55127902710264));
#242297=CARTESIAN_POINT('Ctrl Pts',(46.5911245387429,41.5228599914565,3.47153072139101));
#242298=CARTESIAN_POINT('Ctrl Pts',(46.5059978248577,41.6181024753231,3.47182327905218));
#242299=CARTESIAN_POINT('Ctrl Pts',(46.4256208064858,41.5454735069379,3.40413028378015));
#242300=CARTESIAN_POINT('Origin',(46.1905628026484,41.1629311642483,3.64303198860293));
#242301=CARTESIAN_POINT('Origin',(5.70826774717982E-15,1.86363976210353E-13,
2.53178198860262));
#242302=CARTESIAN_POINT('Origin',(43.8769616275874,39.4864862581819,2.5317819886029));
#242303=CARTESIAN_POINT('Origin',(34.5756856720385,30.7048488218246,3.64303198860284));
#242304=CARTESIAN_POINT('Origin',(45.8923335519908,40.8943347850524,3.64299466007427));
#242305=CARTESIAN_POINT('Ctrl Pts',(43.7969047596346,39.4144401478992,2.59908173516051));
#242306=CARTESIAN_POINT('Ctrl Pts',(43.8246341160485,39.439394812269,2.6587819886029));
#242307=CARTESIAN_POINT('Ctrl Pts',(43.8769616275874,39.4864862581819,2.6587819886029));
#242308=CARTESIAN_POINT('Ctrl Pts',(43.8555436924523,39.3492813761648,2.59908193199951));
#242309=CARTESIAN_POINT('Ctrl Pts',(43.867352448424,39.3919218645341,2.65877685806761));
#242310=CARTESIAN_POINT('Ctrl Pts',(43.9110175468029,39.4486296259976,2.6587819886029));
#242311=CARTESIAN_POINT('Ctrl Pts',(43.9280312169045,39.3054399757364,2.63872492669796));
#242312=CARTESIAN_POINT('Ctrl Pts',(43.9237065964663,39.3632835603677,2.69532212015287));
#242313=CARTESIAN_POINT('Ctrl Pts',(43.9607655567553,39.4300423632766,2.68176836726652));
#242314=CARTESIAN_POINT('Ctrl Pts',(44.0526112349805,39.2744854109881,2.75442176402307));
#242315=CARTESIAN_POINT('Ctrl Pts',(44.0109847679687,39.3564679665378,2.79203179920179));
#242316=CARTESIAN_POINT('Ctrl Pts',(44.0555161714748,39.4322155454634,2.74885310748213));
#242317=CARTESIAN_POINT('Ctrl Pts',(44.1047669487876,39.2856498807577,2.82866089558405));
#242318=CARTESIAN_POINT('Ctrl Pts',(44.0421591564529,39.378959064333,2.85316563119197));
#242319=CARTESIAN_POINT('Ctrl Pts',(44.1002097724415,39.4516641984997,2.79189751796637));
#242320=CARTESIAN_POINT('Ctrl Pts',(44.1385184650375,39.3160391863692,2.90134173516051));
#242321=CARTESIAN_POINT('Ctrl Pts',(44.054287543984,39.4103156382734,2.90103711553257));
#242322=CARTESIAN_POINT('Ctrl Pts',(44.1339623850447,39.4820551873932,2.8340419886029));
#242323=CARTESIAN_POINT('Origin',(44.2189419720523,39.3876757945576,2.8340419886029));
#242324=CARTESIAN_POINT('Origin',(45.8594327453971,40.8647803215169,3.56647653971841));
#242325=CARTESIAN_POINT('Origin',(45.7986150108451,40.810019787355,3.42473028058514));
#242326=CARTESIAN_POINT('Origin',(44.3513327444871,39.5068809815264,3.11913648168166));
#242327=CARTESIAN_POINT('Origin',(44.4837235168756,39.626086168372,3.40423097483339));
#242328=CARTESIAN_POINT('Ctrl Pts',(45.5534068532511,40.5892333705625,3.36123028058511));
#242329=CARTESIAN_POINT('Ctrl Pts',(45.4684272662435,40.6836127633981,3.36123028058511));
#242330=CARTESIAN_POINT('Ctrl Pts',(45.4684272662435,40.6836127633981,3.23423028058511));
#242331=CARTESIAN_POINT('Ctrl Pts',(45.6201409680065,40.6496361736985,3.3612302805851));
#242332=CARTESIAN_POINT('Ctrl Pts',(45.5352552698624,40.7437849681305,3.36099641108467));
#242333=CARTESIAN_POINT('Ctrl Pts',(45.568762269447,40.7739548060672,3.23423043688378));
#242334=CARTESIAN_POINT('Ctrl Pts',(45.6832443225595,40.7067502157883,3.41054258905314));
#242335=CARTESIAN_POINT('Ctrl Pts',(45.5987613682814,40.8009661159843,3.41008815826067));
#242336=CARTESIAN_POINT('Ctrl Pts',(45.6636361529344,40.8593796344575,3.30819867304272));
#242337=CARTESIAN_POINT('Ctrl Pts',(45.7165002428306,40.73684933653,3.48823028058513));
#242338=CARTESIAN_POINT('Ctrl Pts',(45.6322662944332,40.831134086994,3.48794691941629));
#242339=CARTESIAN_POINT('Ctrl Pts',(45.7136354238375,40.9043991801906,3.42473028058514));
#242340=CARTESIAN_POINT('Origin',(45.5534068532511,40.5892333705625,3.23423028058511));
#242341=CARTESIAN_POINT('Ctrl Pts',(44.4033023070489,39.5544469813073,3.471530721391));
#242342=CARTESIAN_POINT('Ctrl Pts',(44.3189410241794,39.6488649595838,3.47122746285105));
#242343=CARTESIAN_POINT('Ctrl Pts',(44.3988635552004,39.7205730817654,3.40413046676823));
#242344=CARTESIAN_POINT('Ctrl Pts',(44.4888328647686,39.6312929306955,3.65553813458014));
#242345=CARTESIAN_POINT('Ctrl Pts',(44.4042668857097,39.7256930794157,3.65520336072211));
#242346=CARTESIAN_POINT('Ctrl Pts',(44.4671969296246,39.7821007282715,3.55128134519937));
#242347=CARTESIAN_POINT('Ctrl Pts',(44.6424847942248,39.769344436534,3.77003198860291));
#242348=CARTESIAN_POINT('Ctrl Pts',(44.5576736780983,39.8638218465938,3.76980209314121));
#242349=CARTESIAN_POINT('Ctrl Pts',(44.589954764068,39.8926323785408,3.64284195387446));
#242350=CARTESIAN_POINT('Ctrl Pts',(44.8038810887674,39.9143573409159,3.77003198860292));
#242351=CARTESIAN_POINT('Ctrl Pts',(44.7187742083304,40.0088781074273,3.77003198860292));
#242352=CARTESIAN_POINT('Ctrl Pts',(44.7189015969554,40.0087366280261,3.64284189403844));
#242353=CARTESIAN_POINT('Origin',(44.8038810887674,39.9143573409159,3.64303198860291));
#242354=CARTESIAN_POINT('Origin',(33.7433098572246,29.9553742717904,3.23423028058502));
#242355=CARTESIAN_POINT('Origin',(45.4410373245171,40.4880553924346,3.23423028058509));
#242356=CARTESIAN_POINT('Origin',(33.6129634723596,29.8380098596984,3.64303198860283));
#242357=CARTESIAN_POINT('Origin',(45.1021848870409,40.1828829233551,3.6429917172188));
#242358=CARTESIAN_POINT('Ctrl Pts',(45.2779489569772,40.3404336838195,3.48823028058509));
#242359=CARTESIAN_POINT('Ctrl Pts',(45.1929563204589,40.4355776097271,3.48852004212287));
#242360=CARTESIAN_POINT('Ctrl Pts',(45.1108495273512,40.3616483211486,3.42473028058509));
#242361=CARTESIAN_POINT('Ctrl Pts',(45.3113153943834,40.370636648342,3.41028005848439));
#242362=CARTESIAN_POINT('Ctrl Pts',(45.2262248134184,40.4655326953366,3.41074404220356));
#242363=CARTESIAN_POINT('Ctrl Pts',(45.1610177711079,40.4068200107225,3.30780486244019));
#242364=CARTESIAN_POINT('Ctrl Pts',(45.3745283705076,40.4278556061241,3.36123028058511));
#242365=CARTESIAN_POINT('Ctrl Pts',(45.289327944973,40.5223510101974,3.36146460586618));
#242366=CARTESIAN_POINT('Ctrl Pts',(45.2560606910586,40.4923970402279,3.23423045308455));
#242367=CARTESIAN_POINT('Ctrl Pts',(45.4410373245171,40.4880553924346,3.3612302805851));
#242368=CARTESIAN_POINT('Ctrl Pts',(45.3560577375096,40.5824347852702,3.3612302805851));
#242369=CARTESIAN_POINT('Ctrl Pts',(45.3560577375095,40.5824347852702,3.2342302805851));
#242370=CARTESIAN_POINT('Origin',(45.1958291143588,40.267268928313,3.4247302805851));
#242371=CARTESIAN_POINT('Origin',(45.1353740846431,40.2128349746518,3.56563113524746));
#242372=CARTESIAN_POINT('Origin',(40.8647803224535,45.8594327460082,3.56647653909442));
#242373=CARTESIAN_POINT('Origin',(40.8943347850519,45.8923335519907,3.64299466007502));
#242374=CARTESIAN_POINT('Origin',(40.8100197873546,45.7986150108454,3.42473028058516));
#242375=CARTESIAN_POINT('Ctrl Pts',(40.7368493365296,45.716500242831,3.48823028058516));
#242376=CARTESIAN_POINT('Ctrl Pts',(40.8311340869937,45.6322662944335,3.48794691941633));
#242377=CARTESIAN_POINT('Ctrl Pts',(40.9043991801903,45.7136354238378,3.42473028058517));
#242378=CARTESIAN_POINT('Ctrl Pts',(40.7066485019687,45.6831319408696,3.41028005925118));
#242379=CARTESIAN_POINT('Ctrl Pts',(40.8008642060138,45.5986481857971,3.40982512231093));
#242380=CARTESIAN_POINT('Ctrl Pts',(40.8592275074409,45.6634671987666,3.30780486372955));
#242381=CARTESIAN_POINT('Ctrl Pts',(40.6494327168507,45.619916185186,3.36123028058514));
#242382=CARTESIAN_POINT('Ctrl Pts',(40.7435821574131,45.535030025745,3.36099721048418));
#242383=CARTESIAN_POINT('Ctrl Pts',(40.773650498978,45.5684243021861,3.23423045308372));
#242384=CARTESIAN_POINT('Ctrl Pts',(40.5892333705622,45.5534068532514,3.36123028058514));
#242385=CARTESIAN_POINT('Ctrl Pts',(40.6836127633978,45.4684272662438,3.36123028058514));
#242386=CARTESIAN_POINT('Ctrl Pts',(40.6836127633978,45.4684272662438,3.23423028058514));
#242387=CARTESIAN_POINT('Origin',(40.5892333705622,45.5534068532514,3.23423028058513));
#242388=CARTESIAN_POINT('Origin',(-0.235948482089068,0.212448967519121,
3.64303198860263));
#242389=CARTESIAN_POINT('Origin',(41.162931164248,46.1905628026487,3.64303198860295));
#242390=CARTESIAN_POINT('Origin',(-0.235948482089068,0.212448967519124,
3.23423028058482));
#242391=CARTESIAN_POINT('Origin',(40.4880553924343,45.4410373245174,3.23423028058514));
#242392=CARTESIAN_POINT('Ctrl Pts',(41.5228599914562,46.5911245387432,3.47153072139104));
#242393=CARTESIAN_POINT('Ctrl Pts',(41.6181024670999,46.5059978322076,3.47182327902695));
#242394=CARTESIAN_POINT('Ctrl Pts',(41.5454735131716,46.4256208133853,3.40413028959057));
#242395=CARTESIAN_POINT('Ctrl Pts',(41.4460088704669,46.5055987918447,3.65553807120989));
#242396=CARTESIAN_POINT('Ctrl Pts',(41.5410583874239,46.4204321019804,3.65586275497117));
#242397=CARTESIAN_POINT('Ctrl Pts',(41.4839460439622,46.3572876358818,3.55128126837357));
#242398=CARTESIAN_POINT('Ctrl Pts',(41.3079491749525,46.3519544194664,3.77003198860296));
#242399=CARTESIAN_POINT('Ctrl Pts',(41.402759982507,46.2668368728718,3.77025505748482));
#242400=CARTESIAN_POINT('Ctrl Pts',(41.3734144470994,46.2345298607729,3.64284211731151));
#242401=CARTESIAN_POINT('Ctrl Pts',(41.162931164248,46.1905628026487,3.77003198860296));
#242402=CARTESIAN_POINT('Ctrl Pts',(41.2574515555201,46.1054562600787,3.77003198860296));
#242403=CARTESIAN_POINT('Ctrl Pts',(41.2573104519183,46.1055833103325,3.64284239821727));
#242404=CARTESIAN_POINT('Origin',(41.4512020416173,46.5107200467159,3.40423097483342));
#242405=CARTESIAN_POINT('Ctrl Pts',(40.4880553924343,45.4410373245174,3.36123028058514));
#242406=CARTESIAN_POINT('Ctrl Pts',(40.5824347852699,45.3560577375099,3.36123028058514));
#242407=CARTESIAN_POINT('Ctrl Pts',(40.5824347852699,45.3560577375099,3.23423028058514));
#242408=CARTESIAN_POINT('Ctrl Pts',(40.4276521486861,45.3743035899571,3.36123028058514));
#242409=CARTESIAN_POINT('Ctrl Pts',(40.5221480762948,45.2891025640481,3.36146538610193));
#242410=CARTESIAN_POINT('Ctrl Pts',(40.4920927345048,45.2557227253148,3.23423043688447));
#242411=CARTESIAN_POINT('Ctrl Pts',(40.370534927874,45.3112030195552,3.41054258693135));
#242412=CARTESIAN_POINT('Ctrl Pts',(40.4654317778751,45.226112733226,3.41100608859797));
#242413=CARTESIAN_POINT('Ctrl Pts',(40.4066678844421,45.1608488177577,3.30819866970886));
#242414=CARTESIAN_POINT('Ctrl Pts',(40.3404336838192,45.2779489569775,3.48823028058513));
#242415=CARTESIAN_POINT('Ctrl Pts',(40.4355776097268,45.1929563204592,3.48852004212291));
#242416=CARTESIAN_POINT('Ctrl Pts',(40.3616483211483,45.1108495273515,3.42473028058513));
#242417=CARTESIAN_POINT('Origin',(40.2672689283127,45.1958291143591,3.42473028058513));
#242418=CARTESIAN_POINT('Origin',(41.5704070646308,46.6431106370695,3.11913648178441));
#242419=CARTESIAN_POINT('Origin',(41.689612087467,46.7755012272976,2.83404198860295));
#242420=CARTESIAN_POINT('Origin',(40.2128349741391,45.135374083614,3.56563113460788));
#242421=CARTESIAN_POINT('Origin',(40.1828829233534,45.1021848870414,3.64299171721765));
#242422=CARTESIAN_POINT('Ctrl Pts',(42.1132001506,46.7942619810919,2.59908173516057));
#242423=CARTESIAN_POINT('Ctrl Pts',(42.0882450513174,46.7665330160782,2.65878198860295));
#242424=CARTESIAN_POINT('Ctrl Pts',(42.0411527846894,46.7142062431425,2.65878198860295));
#242425=CARTESIAN_POINT('Ctrl Pts',(42.0477032750705,46.8532067119189,2.59908193475557));
#242426=CARTESIAN_POINT('Ctrl Pts',(42.0405341034505,46.8094668591667,2.65878715325391));
#242427=CARTESIAN_POINT('Ctrl Pts',(42.0032346206986,46.7483190388774,2.65878198860295));
#242428=CARTESIAN_POINT('Ctrl Pts',(41.9705316734065,46.8890030154865,2.63878778849903));
#242429=CARTESIAN_POINT('Ctrl Pts',(41.9811230778542,46.8318174060856,2.69564460180121));
#242430=CARTESIAN_POINT('Ctrl Pts',(41.9515093836257,46.7612038509546,2.68180481624906));
#242431=CARTESIAN_POINT('Ctrl Pts',(41.8426461117367,46.906368706767,2.75443238878681));
#242432=CARTESIAN_POINT('Ctrl Pts',(41.8933796070866,46.8290619651514,2.79268340777156));
#242433=CARTESIAN_POINT('Ctrl Pts',(41.8570065263035,46.7485125544804,2.74885926835653));
#242434=CARTESIAN_POINT('Ctrl Pts',(41.7917018131131,46.889698257691,2.82856655361701));
#242435=CARTESIAN_POINT('Ctrl Pts',(41.8649047103987,46.80329765619,2.85384197230859));
#242436=CARTESIAN_POINT('Ctrl Pts',(41.8144193983038,46.7243152668223,2.79184624278478));
#242437=CARTESIAN_POINT('Ctrl Pts',(41.7612723673362,46.8559036426988,2.90134173516057));
#242438=CARTESIAN_POINT('Ctrl Pts',(41.856368353593,46.7709043015505,2.90163218716424));
#242439=CARTESIAN_POINT('Ctrl Pts',(41.7839914803026,46.69052164029,2.83404198860295));
#242440=CARTESIAN_POINT('Origin',(42.0411527846894,46.7142062431425,2.53178198860295));
#242441=CARTESIAN_POINT('Origin',(-0.235948482089068,0.212448967519121,
3.64303198860263));
#242442=CARTESIAN_POINT('Origin',(39.9143573409156,44.8038810887677,3.64303198860294));
#242443=CARTESIAN_POINT('Origin',(5.55434424446679E-15,1.857600133136E-13,
2.53178198860262));
#242444=CARTESIAN_POINT('Origin',(42.06380383897,46.6938111422607,2.53178198860295));
#242445=CARTESIAN_POINT('Ctrl Pts',(39.9143573409156,44.8038810887677,3.77003198860295));
#242446=CARTESIAN_POINT('Ctrl Pts',(40.0088781183435,44.7187741985014,3.77003198860295));
#242447=CARTESIAN_POINT('Ctrl Pts',(40.0087366280095,44.7189015969704,3.64284187937082));
#242448=CARTESIAN_POINT('Ctrl Pts',(39.7693421853883,44.6424822887499,3.77003198860294));
#242449=CARTESIAN_POINT('Ctrl Pts',(39.8638196089383,44.5576711710519,3.76980208962821));
#242450=CARTESIAN_POINT('Ctrl Pts',(39.8926305794718,44.5899527660329,3.64284193928301));
#242451=CARTESIAN_POINT('Ctrl Pts',(39.6312917695241,44.4888315723759,3.65553535416619));
#242452=CARTESIAN_POINT('Ctrl Pts',(39.7256919284542,44.404265585613,3.65520057834613));
#242453=CARTESIAN_POINT('Ctrl Pts',(39.78209980511,44.4671959043832,3.55127910964301));
#242454=CARTESIAN_POINT('Ctrl Pts',(39.554446981307,44.4033023070492,3.47153072139103));
#242455=CARTESIAN_POINT('Ctrl Pts',(39.6488649704636,44.3189410144585,3.47122746281614));
#242456=CARTESIAN_POINT('Ctrl Pts',(39.7205730900532,44.3988635644383,3.40413045901307));
#242457=CARTESIAN_POINT('Origin',(39.6260861683717,44.4837235168759,3.40423097483342));
#242458=CARTESIAN_POINT('Ctrl Pts',(42.2339804752701,46.4302753505428,2.90134173516057));
#242459=CARTESIAN_POINT('Ctrl Pts',(42.1395065320998,46.5159655405278,2.90163218716425));
#242460=CARTESIAN_POINT('Ctrl Pts',(42.0671296588095,46.4355828792673,2.83404198860295));
#242461=CARTESIAN_POINT('Ctrl Pts',(42.2644230274451,46.4640859592749,2.82853349835392));
#242462=CARTESIAN_POINT('Ctrl Pts',(42.1708479205161,46.5278479142008,2.85381483162254));
#242463=CARTESIAN_POINT('Ctrl Pts',(42.0975714415913,46.4693919041985,2.79182701594249));
#242464=CARTESIAN_POINT('Ctrl Pts',(42.2755508889262,46.51636388123,2.7546882207367));
#242465=CARTESIAN_POINT('Ctrl Pts',(42.1933444849786,46.5588164356976,2.7928691308386));
#242466=CARTESIAN_POINT('Ctrl Pts',(42.1170605480854,46.5141432491638,2.74900763297952));
#242467=CARTESIAN_POINT('Ctrl Pts',(42.2454039774545,46.6408663419436,2.63954450640431));
#242468=CARTESIAN_POINT('Ctrl Pts',(42.1872204559318,46.6457133039302,2.69627684028895));
#242469=CARTESIAN_POINT('Ctrl Pts',(42.1199995355541,46.608854104584,2.68224356036518));
#242470=CARTESIAN_POINT('Ctrl Pts',(42.2015749714292,46.7146600431957,2.59908178706372));
#242471=CARTESIAN_POINT('Ctrl Pts',(42.1587905896517,46.702988253195,2.65878704321409));
#242472=CARTESIAN_POINT('Ctrl Pts',(42.101818754756,46.6595535157377,2.65878198860295));
#242473=CARTESIAN_POINT('Ctrl Pts',(42.1358900227694,46.773831928426,2.59908173516057));
#242474=CARTESIAN_POINT('Ctrl Pts',(42.110921478106,46.7461150696875,2.65878198860295));
#242475=CARTESIAN_POINT('Ctrl Pts',(42.06380383897,46.6938111422607,2.65878198860295));
#242476=CARTESIAN_POINT('Origin',(42.1615090516451,46.3506032922597,2.83404198860294));
#242477=CARTESIAN_POINT('Origin',(39.5068809815356,44.3513327445017,3.11913648167102));
#242478=CARTESIAN_POINT('Origin',(39.3876757945573,44.2189419720526,2.83404198860293));
#242479=CARTESIAN_POINT('Origin',(42.0423040287647,46.2182127020528,3.11913648177573));
#242480=CARTESIAN_POINT('Origin',(41.9230990057955,46.0858221116781,3.40423097483343));
#242481=CARTESIAN_POINT('Ctrl Pts',(39.3160391863689,44.1385184650378,2.90134173516055));
#242482=CARTESIAN_POINT('Ctrl Pts',(39.4103156382731,44.0542875439843,2.90103711553261));
#242483=CARTESIAN_POINT('Ctrl Pts',(39.4820551873929,44.133962385045,2.83404198860293));
#242484=CARTESIAN_POINT('Ctrl Pts',(39.2856369388939,44.1047525536514,2.82862991747984));
#242485=CARTESIAN_POINT('Ctrl Pts',(39.3789425853234,44.0421527706804,2.85314045886445));
#242486=CARTESIAN_POINT('Ctrl Pts',(39.4516512848565,44.1001954303884,2.79187960999954));
#242487=CARTESIAN_POINT('Ctrl Pts',(39.2745942851002,44.0527517782419,2.75470625793367));
#242488=CARTESIAN_POINT('Ctrl Pts',(39.3566016867499,44.0110417363806,2.79224250381939));
#242489=CARTESIAN_POINT('Ctrl Pts',(39.4323285306302,44.0556530121007,2.7490180910829));
#242490=CARTESIAN_POINT('Ctrl Pts',(39.3050549810248,43.929007150946,2.63947868311719));
#242491=CARTESIAN_POINT('Ctrl Pts',(39.3631024520339,43.9243964923855,2.69595066767934));
#242492=CARTESIAN_POINT('Ctrl Pts',(39.4299498468378,43.961478133811,2.68220539436092));
#242493=CARTESIAN_POINT('Ctrl Pts',(39.3490583909342,43.8557442421763,2.59908178585127));
#242494=CARTESIAN_POINT('Ctrl Pts',(39.3917348424063,43.867520632012,2.65877670944998));
#242495=CARTESIAN_POINT('Ctrl Pts',(39.4485000225478,43.9111340157081,2.65878198860293));
#242496=CARTESIAN_POINT('Ctrl Pts',(39.4144401478989,43.7969047596349,2.59908173516055));
#242497=CARTESIAN_POINT('Ctrl Pts',(39.4393948122687,43.8246341160488,2.65878198860293));
#242498=CARTESIAN_POINT('Ctrl Pts',(39.4864862581816,43.8769616275877,2.65878198860293));
#242499=CARTESIAN_POINT('Origin',(39.4864862581816,43.8769616275877,2.53178198860293));
#242500=CARTESIAN_POINT('Ctrl Pts',(41.6348281284261,45.7656648676109,3.77003198860296));
#242501=CARTESIAN_POINT('Ctrl Pts',(41.540307729011,45.8507714175129,3.77003198860296));
#242502=CARTESIAN_POINT('Ctrl Pts',(41.540448840768,45.8506443599162,3.64284238727624));
#242503=CARTESIAN_POINT('Ctrl Pts',(41.7801793768013,45.926760978664,3.77003198860296));
#242504=CARTESIAN_POINT('Ctrl Pts',(41.6856176794258,46.0121552117493,3.77025506105888));
#242505=CARTESIAN_POINT('Ctrl Pts',(41.6565546403128,45.9795929135644,3.64284210641882));
#242506=CARTESIAN_POINT('Ctrl Pts',(41.9185498083239,46.0801233673962,3.65553527987865));
#242507=CARTESIAN_POINT('Ctrl Pts',(41.8239142817222,46.1657498592392,3.65585996533134));
#242508=CARTESIAN_POINT('Ctrl Pts',(41.7670853619627,46.1023497159527,3.55127902710263));
#242509=CARTESIAN_POINT('Ctrl Pts',(41.995572738225,46.1654920697614,3.47153072139104));
#242510=CARTESIAN_POINT('Ctrl Pts',(41.900956806909,46.2513146407506,3.47182327905221));
#242511=CARTESIAN_POINT('Ctrl Pts',(41.8286118967078,46.170681855241,3.40413028378016));
#242512=CARTESIAN_POINT('Origin',(41.6348281284261,45.7656648676109,3.64303198860296));
#242513=CARTESIAN_POINT('Origin',(5.70392627685665E-15,1.86368317680676E-13,
2.53178198860262));
#242514=CARTESIAN_POINT('Origin',(39.5091373124621,43.8565665267059,2.53178198860292));
#242515=CARTESIAN_POINT('Origin',(28.0951675083324,30.7283483363947,3.64303198860284));
#242516=CARTESIAN_POINT('Origin',(41.3663085755636,45.4673664422112,3.64299466007543));
#242517=CARTESIAN_POINT('Ctrl Pts',(39.4370498736007,43.7765468711725,2.59908173516055));
#242518=CARTESIAN_POINT('Ctrl Pts',(39.4620188529809,43.8042633382932,2.65878198860293));
#242519=CARTESIAN_POINT('Ctrl Pts',(39.5091373124622,43.8565665267059,2.65878198860293));
#242520=CARTESIAN_POINT('Ctrl Pts',(39.5021785224869,43.7178744835422,2.59908193199943));
#242521=CARTESIAN_POINT('Ctrl Pts',(39.509465444134,43.761515733968,2.65877685806608));
#242522=CARTESIAN_POINT('Ctrl Pts',(39.546963765375,43.8224770900137,2.65878198860293));
#242523=CARTESIAN_POINT('Ctrl Pts',(39.5788516269097,43.6818502604301,2.63872492669813));
#242524=CARTESIAN_POINT('Ctrl Pts',(39.5685043961838,43.7389249259239,2.69532212015309));
#242525=CARTESIAN_POINT('Ctrl Pts',(39.5983821485332,43.8091917332949,2.68176836726648));
#242526=CARTESIAN_POINT('Ctrl Pts',(39.7059848156962,43.6640874258691,2.75442176402296));
#242527=CARTESIAN_POINT('Ctrl Pts',(39.6560168722793,43.7412697217734,2.79203179920159));
#242528=CARTESIAN_POINT('Ctrl Pts',(39.6923865500763,43.8212571467116,2.74885310748224));
#242529=CARTESIAN_POINT('Ctrl Pts',(39.756687810178,43.6806424921201,2.82866089558422));
#242530=CARTESIAN_POINT('Ctrl Pts',(39.6846695243131,43.7668962219033,2.85316563119229));
#242531=CARTESIAN_POINT('Ctrl Pts',(39.7348023770065,43.8452710114193,2.79189751796648));
#242532=CARTESIAN_POINT('Ctrl Pts',(39.7870778846746,43.7143933160626,2.90134173516054));
#242533=CARTESIAN_POINT('Ctrl Pts',(39.69345381678,43.7993487829616,2.9010371155326));
#242534=CARTESIAN_POINT('Ctrl Pts',(39.7651933658998,43.8790236240223,2.83404198860292));
#242535=CARTESIAN_POINT('Origin',(39.8595727587354,43.7940440370147,2.83404198860294));
#242536=CARTESIAN_POINT('Origin',(41.3366772856877,45.4345348103664,3.56647653971819));
#242537=CARTESIAN_POINT('Origin',(41.2819167515328,45.3737170758075,3.42473028058517));
#242538=CARTESIAN_POINT('Origin',(39.9787779456606,43.926434809488,3.11913648168203));
#242539=CARTESIAN_POINT('Origin',(40.0979831325498,44.058825581838,3.40423097483342));
#242540=CARTESIAN_POINT('Ctrl Pts',(41.0611303347403,45.1285089182135,3.36123028058514));
#242541=CARTESIAN_POINT('Ctrl Pts',(40.9667509419047,45.2134885052211,3.36123028058514));
#242542=CARTESIAN_POINT('Ctrl Pts',(40.9667509419047,45.2134885052211,3.23423028058514));
#242543=CARTESIAN_POINT('Ctrl Pts',(41.121185060844,45.1955564429366,3.36123028058513));
#242544=CARTESIAN_POINT('Ctrl Pts',(41.0269231466356,45.2803165088396,3.36099641108276));
#242545=CARTESIAN_POINT('Ctrl Pts',(41.0570929845744,45.3138235084253,3.23423043688384));
#242546=CARTESIAN_POINT('Ctrl Pts',(41.1779726855671,45.2589537050066,3.41054258905318));
#242547=CARTESIAN_POINT('Ctrl Pts',(41.0841042944916,45.3438226072607,3.41008815826171));
#242548=CARTESIAN_POINT('Ctrl Pts',(41.1425178129631,45.408697391911,3.3081986730431));
#242549=CARTESIAN_POINT('Ctrl Pts',(41.2079002115907,45.292364129856,3.48823028058516));
#242550=CARTESIAN_POINT('Ctrl Pts',(41.1142722655005,45.3773275334108,3.48794691941632));
#242551=CARTESIAN_POINT('Ctrl Pts',(41.1875373586971,45.4586966628151,3.42473028058517));
#242552=CARTESIAN_POINT('Origin',(41.0611303347403,45.1285089182135,3.23423028058514));
#242553=CARTESIAN_POINT('Ctrl Pts',(40.0254908126588,43.9791725362585,3.47153072139104));
#242554=CARTESIAN_POINT('Ctrl Pts',(39.9317223035498,44.0642551277131,3.47122746285109));
#242555=CARTESIAN_POINT('Ctrl Pts',(40.0037114707677,44.1439246046466,3.40413046676837));
#242556=CARTESIAN_POINT('Ctrl Pts',(40.102520236037,44.0645378932555,3.65553813458016));
#242557=CARTESIAN_POINT('Ctrl Pts',(40.0085500157868,44.1495813562475,3.65520336072198));
#242558=CARTESIAN_POINT('Ctrl Pts',(40.0652391174801,44.2122579788868,3.55128134519927));
#242559=CARTESIAN_POINT('Ctrl Pts',(40.2409001323905,44.217894138564,3.77003198860295));
#242560=CARTESIAN_POINT('Ctrl Pts',(40.1466780419431,44.3029888158481,3.76980209314041));
#242561=CARTESIAN_POINT('Ctrl Pts',(40.1757707681154,44.3350158129976,3.64284195387457));
#242562=CARTESIAN_POINT('Ctrl Pts',(40.3862543050938,44.3789831537298,3.77003198860295));
#242563=CARTESIAN_POINT('Ctrl Pts',(40.2917335385825,44.4640900341667,3.77003198860295));
#242564=CARTESIAN_POINT('Ctrl Pts',(40.2918750179835,44.4639626455418,3.64284189403867));
#242565=CARTESIAN_POINT('Origin',(40.3862543050938,44.3789831537298,3.64303198860294));
#242566=CARTESIAN_POINT('Origin',(27.4203375923833,29.9788737863605,3.23423028058502));
#242567=CARTESIAN_POINT('Origin',(40.9599523566124,45.0161393894796,3.23423028058513));
#242568=CARTESIAN_POINT('Origin',(27.314662201079,29.8615093742685,3.64303198860283));
#242569=CARTESIAN_POINT('Origin',(40.6548553974681,44.6772189625517,3.64299171721807));
#242570=CARTESIAN_POINT('Ctrl Pts',(40.8131880745606,44.8522789915944,3.48823028058513));
#242571=CARTESIAN_POINT('Ctrl Pts',(40.7187157882337,44.9380175594365,3.4885200421229));
#242572=CARTESIAN_POINT('Ctrl Pts',(40.6447864996552,44.8559107663288,3.42473028058512));
#242573=CARTESIAN_POINT('Ctrl Pts',(40.8432146576636,44.8858042435441,3.41028005848437));
#242574=CARTESIAN_POINT('Ctrl Pts',(40.7486708738398,44.9712860523973,3.41074404220417));
#242575=CARTESIAN_POINT('Ctrl Pts',(40.6899581892278,44.9060790100841,3.30780486244021));
#242576=CARTESIAN_POINT('Ctrl Pts',(40.900100336764,44.9493173051411,3.36123028058514));
#242577=CARTESIAN_POINT('Ctrl Pts',(40.8054891887023,45.0343891839535,3.361464605865));
#242578=CARTESIAN_POINT('Ctrl Pts',(40.7755352187354,45.0011219300372,3.23423045308391));
#242579=CARTESIAN_POINT('Ctrl Pts',(40.9599523566124,45.0161393894796,3.36123028058514));
#242580=CARTESIAN_POINT('Ctrl Pts',(40.8655729637768,45.1011189764871,3.36123028058513));
#242581=CARTESIAN_POINT('Ctrl Pts',(40.8655729637768,45.1011189764871,3.23423028058514));
#242582=CARTESIAN_POINT('Origin',(40.7391658924908,44.7709311793212,3.42473028058512));
#242583=CARTESIAN_POINT('Origin',(40.6847319392794,44.7104761492012,3.5656311352478));
#242584=CARTESIAN_POINT('Origin',(35.8473027488291,49.8797426639498,3.5664765390943));
#242585=CARTESIAN_POINT('Origin',(35.8732562382986,49.915552518433,3.64299466007487));
#242586=CARTESIAN_POINT('Origin',(35.7991993820661,49.8135340601225,3.42473028058518));
#242587=CARTESIAN_POINT('Ctrl Pts',(35.7350130971388,49.7242207306177,3.48823028058519));
#242588=CARTESIAN_POINT('Ctrl Pts',(35.8375861910555,49.6503036646788,3.48794691941635));
#242589=CARTESIAN_POINT('Ctrl Pts',(35.9019445403517,49.7388853330814,3.4247302805852));
#242590=CARTESIAN_POINT('Ctrl Pts',(35.7084656432359,49.6878783768795,3.41028005925123));
#242591=CARTESIAN_POINT('Ctrl Pts',(35.8109961808893,49.6137056554185,3.40982512231065));
#242592=CARTESIAN_POINT('Ctrl Pts',(35.8622643302261,49.6842702092639,3.30780486372868));
#242593=CARTESIAN_POINT('Ctrl Pts',(35.6581711379713,49.6190282456269,3.36123028058517));
#242594=CARTESIAN_POINT('Ctrl Pts',(35.7606778378438,49.5444483977866,3.36099721048315));
#242595=CARTESIAN_POINT('Ctrl Pts',(35.7870908094894,49.5808027344238,3.23423045308355));
#242596=CARTESIAN_POINT('Ctrl Pts',(35.6052536882601,49.5465907136147,3.36123028058517));
#242597=CARTESIAN_POINT('Ctrl Pts',(35.7079988465457,49.4719419865736,3.36123028058517));
#242598=CARTESIAN_POINT('Ctrl Pts',(35.7079988465457,49.4719419865736,3.23423028058517));
#242599=CARTESIAN_POINT('Origin',(35.6052536882601,49.5465907136147,3.23423028058516));
#242600=CARTESIAN_POINT('Origin',(-0.256862895714041,0.186621817603044,
3.64303198860263));
#242601=CARTESIAN_POINT('Origin',(36.1092077731528,50.2402240048086,3.64303198860298));
#242602=CARTESIAN_POINT('Origin',(-0.256862895714041,0.186621817603046,
3.23423028058482));
#242603=CARTESIAN_POINT('Origin',(35.5163757878395,49.4242607783463,3.23423028058516));
#242604=CARTESIAN_POINT('Ctrl Pts',(36.4252947698678,50.6762142289951,3.47153072139107));
#242605=CARTESIAN_POINT('Ctrl Pts',(36.5289136610816,50.6015094050817,3.47182327902698));
#242606=CARTESIAN_POINT('Ctrl Pts',(36.465084262422,50.5139809070356,3.40413028959067));
#242607=CARTESIAN_POINT('Ctrl Pts',(36.3578045222551,50.5831238715081,3.65553807120993));
#242608=CARTESIAN_POINT('Ctrl Pts',(36.4612356912254,50.5083591136211,3.65586275497056));
#242609=CARTESIAN_POINT('Ctrl Pts',(36.41103660916,50.4395906940215,3.55128126837327));
#242610=CARTESIAN_POINT('Ctrl Pts',(36.2365613423282,50.4158900112697,3.77003198860299));
#242611=CARTESIAN_POINT('Ctrl Pts',(36.3397499727013,50.3411491755185,3.7702550574847));
#242612=CARTESIAN_POINT('Ctrl Pts',(36.3139421975383,50.3059517008892,3.64284211731151));
#242613=CARTESIAN_POINT('Ctrl Pts',(36.1092077731528,50.2402240048086,3.77003198860299));
#242614=CARTESIAN_POINT('Ctrl Pts',(36.2121064279405,50.1654637560307,3.77003198860299));
#242615=CARTESIAN_POINT('Ctrl Pts',(36.2119528169512,50.1655753609472,3.64284239821743));
#242616=CARTESIAN_POINT('Origin',(36.3624339277672,50.5887599058104,3.40423097483345));
#242617=CARTESIAN_POINT('Ctrl Pts',(35.5163757878395,49.4242607783463,3.36123028058516));
#242618=CARTESIAN_POINT('Ctrl Pts',(35.6191209461251,49.3496120513052,3.36123028058517));
#242619=CARTESIAN_POINT('Ctrl Pts',(35.6191209461251,49.3496120513052,3.23423028058516));
#242620=CARTESIAN_POINT('Ctrl Pts',(35.4632790141048,49.3515787599191,3.36123028058517));
#242621=CARTESIAN_POINT('Ctrl Pts',(35.5661632154422,49.2767219882436,3.36146538610113));
#242622=CARTESIAN_POINT('Ctrl Pts',(35.5397616632037,49.2403833690707,3.23423043688441));
#242623=CARTESIAN_POINT('Ctrl Pts',(35.4130704930569,49.282853485729,3.41054258693134));
#242624=CARTESIAN_POINT('Ctrl Pts',(35.5163418450526,49.2081487547905,3.41100608859837));
#242625=CARTESIAN_POINT('Ctrl Pts',(35.4647218031682,49.1370998624031,3.30819866970878));
#242626=CARTESIAN_POINT('Ctrl Pts',(35.3866101428259,49.2466351556015,3.48823028058516));
#242627=CARTESIAN_POINT('Ctrl Pts',(35.4901170100366,49.1720533660034,3.48852004212294));
#242628=CARTESIAN_POINT('Ctrl Pts',(35.4251752107437,49.0826686475737,3.42473028058516));
#242629=CARTESIAN_POINT('Origin',(35.3224300524581,49.1573173746149,3.42473028058515));
#242630=CARTESIAN_POINT('Origin',(36.4671473482298,50.7328855645265,3.11913648178361));
#242631=CARTESIAN_POINT('Origin',(36.5718607685321,50.8770112231005,2.83404198860297));
#242632=CARTESIAN_POINT('Origin',(35.2746135646412,49.091503625274,3.56563113460758));
#242633=CARTESIAN_POINT('Origin',(35.2482948100395,49.0553654007528,3.64299171721827));
#242634=CARTESIAN_POINT('Ctrl Pts',(36.9911673391707,50.9399462128204,2.59908173516059));
#242635=CARTESIAN_POINT('Ctrl Pts',(36.9692474126339,50.9097606317996,2.65878198860298));
#242636=CARTESIAN_POINT('Ctrl Pts',(36.9278827595326,50.8527980281388,2.65878198860298));
#242637=CARTESIAN_POINT('Ctrl Pts',(36.9198678602469,50.9917217504956,2.59908193475707));
#242638=CARTESIAN_POINT('Ctrl Pts',(36.91731002169,50.9474721267398,2.65878715325422));
#242639=CARTESIAN_POINT('Ctrl Pts',(36.8866065570942,50.8827604229952,2.65878198860298));
#242640=CARTESIAN_POINT('Ctrl Pts',(36.8393772800889,51.019255329238,2.63878778849925));
#242641=CARTESIAN_POINT('Ctrl Pts',(36.8558881875867,50.9634900918196,2.69564460180162));
#242642=CARTESIAN_POINT('Ctrl Pts',(36.8338178466775,50.8901678911827,2.68180481624929));
#242643=CARTESIAN_POINT('Ctrl Pts',(36.7103770798843,51.0231582082091,2.75443238878662));
#242644=CARTESIAN_POINT('Ctrl Pts',(36.7689134067396,50.9515780553178,2.79268340777113));
#242645=CARTESIAN_POINT('Ctrl Pts',(36.7411592876132,50.8676678805079,2.74885926835635));
#242646=CARTESIAN_POINT('Ctrl Pts',(36.6614543958831,51.0012539523494,2.82856655361719));
#242647=CARTESIAN_POINT('Ctrl Pts',(36.7432876021367,50.9229784487433,2.85384197230806));
#242648=CARTESIAN_POINT('Ctrl Pts',(36.7013347616507,50.8391515810788,2.79184624278497));
#242649=CARTESIAN_POINT('Ctrl Pts',(36.6347241449653,50.9644637245896,2.90134173516059));
#242650=CARTESIAN_POINT('Ctrl Pts',(36.7381840359683,50.889870256032,2.90163218716427));
#242651=CARTESIAN_POINT('Ctrl Pts',(36.6746059268177,50.8023624960594,2.83404198860298));
#242652=CARTESIAN_POINT('Origin',(36.9278827595326,50.8527980281388,2.53178198860298));
#242653=CARTESIAN_POINT('Origin',(-0.256862895714041,0.186621817603044,
3.64303198860263));
#242654=CARTESIAN_POINT('Origin',(35.0124214764584,48.7306271754179,3.64303198860296));
#242655=CARTESIAN_POINT('Origin',(5.56775724677592E-15,1.85749151678493E-13,
2.53178198860262));
#242656=CARTESIAN_POINT('Origin',(36.9525415975211,50.8348823336489,2.53178198860298));
#242657=CARTESIAN_POINT('Ctrl Pts',(35.0124214764584,48.7306271754179,3.77003198860297));
#242658=CARTESIAN_POINT('Ctrl Pts',(35.1153205516307,48.6558666212128,3.77003198860297));
#242659=CARTESIAN_POINT('Ctrl Pts',(35.1151665196294,48.6559785320124,3.64284187937079));
#242660=CARTESIAN_POINT('Ctrl Pts',(34.8850714976655,48.5549543235562,3.77003198860297));
#242661=CARTESIAN_POINT('Ctrl Pts',(34.987896539803,48.4804833899298,3.76980208963067));
#242662=CARTESIAN_POINT('Ctrl Pts',(35.0131753353112,48.5155997094322,3.64284193928456));
#242663=CARTESIAN_POINT('Ctrl Pts',(34.7638382096863,48.3877151240595,3.6555353541662));
#242664=CARTESIAN_POINT('Ctrl Pts',(34.8665607873066,48.3134799021725,3.65520057834321));
#242665=CARTESIAN_POINT('Ctrl Pts',(34.916081646202,48.3819617107295,3.55127910964134));
#242666=CARTESIAN_POINT('Ctrl Pts',(34.6963546279284,48.2946219293749,3.47153072139107));
#242667=CARTESIAN_POINT('Ctrl Pts',(34.7990735417351,48.2205921440832,3.47122746281618));
#242668=CARTESIAN_POINT('Ctrl Pts',(34.8620346554129,48.3075724095164,3.40413045901307));
#242669=CARTESIAN_POINT('Origin',(34.7591950625533,48.3820909175332,3.40423097483344));
#242670=CARTESIAN_POINT('Ctrl Pts',(37.149332979726,50.5905785208487,2.90134173516059));
#242671=CARTESIAN_POINT('Ctrl Pts',(37.0464195108252,50.6659240749086,2.90163218716426));
#242672=CARTESIAN_POINT('Ctrl Pts',(36.9828414016746,50.578416314936,2.83404198860297));
#242673=CARTESIAN_POINT('Ctrl Pts',(37.1760745934432,50.6273860247245,2.82853349835386));
#242674=CARTESIAN_POINT('Ctrl Pts',(37.0763471615769,50.6810174228649,2.85381483162332));
#242675=CARTESIAN_POINT('Ctrl Pts',(37.0095824157646,50.6152221632646,2.79182701594277));
#242676=CARTESIAN_POINT('Ctrl Pts',(37.1816769644886,50.6805407410142,2.75468822073683));
#242677=CARTESIAN_POINT('Ctrl Pts',(37.0954833955427,50.7141678268709,2.79286913083839));
#242678=CARTESIAN_POINT('Ctrl Pts',(37.0242869695753,50.6617655220318,2.74900763297936));
#242679=CARTESIAN_POINT('Ctrl Pts',(37.1386811500613,50.8012099538924,2.63954450640423));
#242680=CARTESIAN_POINT('Ctrl Pts',(37.0803097184695,50.7999485296222,2.69627684028912));
#242681=CARTESIAN_POINT('Ctrl Pts',(37.0173098767919,50.75626474932,2.68224356036539));
#242682=CARTESIAN_POINT('Ctrl Pts',(37.0873787017257,50.8700180268816,2.59908178706417));
#242683=CARTESIAN_POINT('Ctrl Pts',(37.0460487315411,50.8539379904897,2.65878704321598));
#242684=CARTESIAN_POINT('Ctrl Pts',(36.9939291606762,50.8047860147164,2.65878198860297));
#242685=CARTESIAN_POINT('Ctrl Pts',(37.0158684358559,50.9219998155902,2.59908173516059));
#242686=CARTESIAN_POINT('Ctrl Pts',(36.9939338721432,50.8918248691003,2.65878198860297));
#242687=CARTESIAN_POINT('Ctrl Pts',(36.9525415975211,50.8348823336489,2.65878198860297));
#242688=CARTESIAN_POINT('Origin',(37.0855865599602,50.5037675878948,2.83404198860297));
#242689=CARTESIAN_POINT('Origin',(34.6544814981904,48.2379650606703,3.11913648167033));
#242690=CARTESIAN_POINT('Origin',(34.549767933694,48.093839203715,2.83404198860297));
#242691=CARTESIAN_POINT('Origin',(36.9808731396113,50.3596419293399,3.11913648177612));
#242692=CARTESIAN_POINT('Origin',(36.8761597191953,50.2155162706046,3.40423097483345));
#242693=CARTESIAN_POINT('Ctrl Pts',(34.4869303039396,48.006368200519,2.90134173516058));
#242694=CARTESIAN_POINT('Ctrl Pts',(34.5894948283132,47.932453277904,2.90103711553263));
#242695=CARTESIAN_POINT('Ctrl Pts',(34.6525130919796,48.0191904766739,2.83404198860296));
#242696=CARTESIAN_POINT('Ctrl Pts',(34.460224101985,47.96960936212,2.82862991747999));
#242697=CARTESIAN_POINT('Ctrl Pts',(34.5595620694345,47.9171056031441,2.85314045886591));
#242698=CARTESIAN_POINT('Ctrl Pts',(34.6258053530818,47.9824304277183,2.79187961000031));
#242699=CARTESIAN_POINT('Ctrl Pts',(34.4546775021468,47.9167391807672,2.75470625793355));
#242700=CARTESIAN_POINT('Ctrl Pts',(34.5405955452484,47.8838297385499,2.79224250381907));
#242701=CARTESIAN_POINT('Ctrl Pts',(34.6112444014588,47.9361122396532,2.74901809108288));
#242702=CARTESIAN_POINT('Ctrl Pts',(34.4979061669209,47.7968564492225,2.63947868311738));
#242703=CARTESIAN_POINT('Ctrl Pts',(34.5561175928641,47.7983386612737,2.69595066767962));
#242704=CARTESIAN_POINT('Ctrl Pts',(34.6187227036514,47.8422046210395,2.682205394361));
#242705=CARTESIAN_POINT('Ctrl Pts',(34.5493265808152,47.7285944911493,2.59908178585215));
#242706=CARTESIAN_POINT('Ctrl Pts',(34.5905382782887,47.7447672725793,2.6587767094491));
#242707=CARTESIAN_POINT('Ctrl Pts',(34.6424336528586,47.7940753146444,2.65878198860296));
#242708=CARTESIAN_POINT('Ctrl Pts',(34.6205005703634,47.6769115920306,2.59908173516057));
#242709=CARTESIAN_POINT('Ctrl Pts',(34.6424200234574,47.7070975168467,2.65878198860296));
#242710=CARTESIAN_POINT('Ctrl Pts',(34.6837837831345,47.7640607692766,2.65878198860296));
#242711=CARTESIAN_POINT('Origin',(34.6837837831345,47.7640607692766,2.53178198860296));
#242712=CARTESIAN_POINT('Ctrl Pts',(36.6229335645808,49.8669803696028,3.77003198860299));
#242713=CARTESIAN_POINT('Ctrl Pts',(36.5200349009284,49.9417406248212,3.77003198860299));
#242714=CARTESIAN_POINT('Ctrl Pts',(36.5201885207956,49.9416290134546,3.64284238727641));
#242715=CARTESIAN_POINT('Ctrl Pts',(36.7506494346803,50.042387321932,3.77003198860298));
#242716=CARTESIAN_POINT('Ctrl Pts',(36.6476796282221,50.1174293675638,3.77025506106058));
#242717=CARTESIAN_POINT('Ctrl Pts',(36.6221794864693,50.0820075342373,3.64284210641899));
#242718=CARTESIAN_POINT('Ctrl Pts',(36.8722311236859,50.2093732240195,3.65553527987869));
#242719=CARTESIAN_POINT('Ctrl Pts',(36.7691636147942,50.2846385388115,3.65585996532951));
#242720=CARTESIAN_POINT('Ctrl Pts',(36.7192731293506,50.2156454684943,3.55127902710247));
#242721=CARTESIAN_POINT('Ctrl Pts',(36.9399086546485,50.3023253561998,3.47153072139107));
#242722=CARTESIAN_POINT('Ctrl Pts',(36.836840137845,50.3777877242642,3.47182327905223));
#242723=CARTESIAN_POINT('Ctrl Pts',(36.7733199617898,50.2900345513019,3.40413028378026));
#242724=CARTESIAN_POINT('Origin',(36.6229335645808,49.8669803696028,3.64303198860299));
#242725=CARTESIAN_POINT('Origin',(5.69915478234096E-15,1.86372181560749E-13,
2.53178198860262));
#242726=CARTESIAN_POINT('Origin',(34.7084426211231,47.7461450747867,2.53178198860296));
#242727=CARTESIAN_POINT('Origin',(21.7541926348211,29.4019141737118,3.64303198860283));
#242728=CARTESIAN_POINT('Origin',(36.3870656659268,49.5422481179705,3.64299466007604));
#242729=CARTESIAN_POINT('Ctrl Pts',(34.6451144164185,47.6590285860938,2.59908173516057));
#242730=CARTESIAN_POINT('Ctrl Pts',(34.6670494534017,47.6892031885516,2.65878198860296));
#242731=CARTESIAN_POINT('Ctrl Pts',(34.7084426211231,47.7461450747867,2.65878198860296));
#242732=CARTESIAN_POINT('Ctrl Pts',(34.7160192182667,47.6074854095247,2.59908193199937));
#242733=CARTESIAN_POINT('Ctrl Pts',(34.7187044685527,47.6516492793368,2.65877685806639));
#242734=CARTESIAN_POINT('Ctrl Pts',(34.7496251732007,47.7161963245904,2.65878198860296));
#242735=CARTESIAN_POINT('Ctrl Pts',(34.7960378560835,47.5796730526555,2.63872492669835));
#242736=CARTESIAN_POINT('Ctrl Pts',(34.7797813814945,47.6353534770324,2.69532212015306));
#242737=CARTESIAN_POINT('Ctrl Pts',(34.8021505789971,47.7083584310197,2.68176836726665));
#242738=CARTESIAN_POINT('Ctrl Pts',(34.9243313177594,47.5752965616148,2.75442176402279));
#242739=CARTESIAN_POINT('Ctrl Pts',(34.8665693571826,47.6468329724891,2.79203179920176));
#242740=CARTESIAN_POINT('Ctrl Pts',(34.8943788354696,47.7301838844735,2.74885310748212));
#242741=CARTESIAN_POINT('Ctrl Pts',(34.973026080298,47.5970608435769,2.82866089558435));
#242742=CARTESIAN_POINT('Ctrl Pts',(34.8923863483137,47.6753141056551,2.85316563119181));
#242743=CARTESIAN_POINT('Ctrl Pts',(34.934052171687,47.7584998599249,2.79189751796619));
#242744=CARTESIAN_POINT('Ctrl Pts',(34.9997217530259,47.6338034047602,2.90134173516057));
#242745=CARTESIAN_POINT('Ctrl Pts',(34.8977303031701,47.7085070967806,2.90103711553263));
#242746=CARTESIAN_POINT('Ctrl Pts',(34.9607485668365,47.7952442955505,2.83404198860296));
#242747=CARTESIAN_POINT('Origin',(35.0634937251221,47.7205955685093,2.83404198860295));
#242748=CARTESIAN_POINT('Origin',(36.361028539381,49.5064990280457,3.56647653971785));
#242749=CARTESIAN_POINT('Origin',(36.3129251734942,49.4402904249168,3.4247302805852));
#242750=CARTESIAN_POINT('Origin',(35.1682072895616,47.8647214254827,3.11913648168205));
#242751=CARTESIAN_POINT('Origin',(35.2729208539814,48.0088472823275,3.40423097483344));
#242752=CARTESIAN_POINT('Ctrl Pts',(36.1189794796882,49.173347078409,3.36123028058516));
#242753=CARTESIAN_POINT('Ctrl Pts',(36.0162343214026,49.2479958054501,3.36123028058517));
#242754=CARTESIAN_POINT('Ctrl Pts',(36.0162343214026,49.2479958054501,3.23423028058516));
#242755=CARTESIAN_POINT('Ctrl Pts',(36.1716968449925,49.2463047380085,3.36123028058516));
#242756=CARTESIAN_POINT('Ctrl Pts',(36.0690914679755,49.3207474263634,3.36099641108398));
#242757=CARTESIAN_POINT('Ctrl Pts',(36.0955935972127,49.3572244778968,3.23423043688375));
#242758=CARTESIAN_POINT('Ctrl Pts',(36.2215465627857,49.3152906263888,3.4105425890532));
#242759=CARTESIAN_POINT('Ctrl Pts',(36.1193211766499,49.3898826892493,3.41008815825999));
#242760=CARTESIAN_POINT('Ctrl Pts',(36.1706334382091,49.4605079583594,3.30819867304302));
#242761=CARTESIAN_POINT('Ctrl Pts',(36.247817802325,49.3516463037388,3.48823028058519));
#242762=CARTESIAN_POINT('Ctrl Pts',(36.1458216659124,49.4263574835553,3.48794691941635));
#242763=CARTESIAN_POINT('Ctrl Pts',(36.2101800152086,49.514939151958,3.4247302805852));
#242764=CARTESIAN_POINT('Origin',(36.1189794796882,49.173347078409,3.23423028058516));
#242765=CARTESIAN_POINT('Ctrl Pts',(35.2091516650527,47.922053073669,3.47153072139106));
#242766=CARTESIAN_POINT('Ctrl Pts',(35.1070032771118,47.9968680956255,3.47122746285111));
#242767=CARTESIAN_POINT('Ctrl Pts',(35.1702703521468,48.0836260518495,3.40413046676815));
#242768=CARTESIAN_POINT('Ctrl Pts',(35.2768360036064,48.0150025575608,3.65553813458022));
#242769=CARTESIAN_POINT('Ctrl Pts',(35.1744910995524,48.0897575808465,3.65520336072116));
#242770=CARTESIAN_POINT('Ctrl Pts',(35.2243181613716,48.1580164790724,3.55128134520005));
#242771=CARTESIAN_POINT('Ctrl Pts',(35.3984277477544,48.1819833392242,3.77003198860297));
#242772=CARTESIAN_POINT('Ctrl Pts',(35.2958269999286,48.2567629686463,3.76980209314327));
#242773=CARTESIAN_POINT('Ctrl Pts',(35.3214126203092,48.2916555365114,3.64284195387391));
#242774=CARTESIAN_POINT('Ctrl Pts',(35.5261472678865,48.3573835402122,3.77003198860298));
#242775=CARTESIAN_POINT('Ctrl Pts',(35.4232482045982,48.432144085783,3.77003198860298));
#242776=CARTESIAN_POINT('Ctrl Pts',(35.4234022246977,48.4320321836305,3.64284189403824));
#242777=CARTESIAN_POINT('Origin',(35.5261472678865,48.3573835402122,3.64303198860297));
#242778=CARTESIAN_POINT('Origin',(21.2334658618522,28.685195257892,3.23423028058501));
#242779=CARTESIAN_POINT('Origin',(36.0301015792676,49.0510171431406,3.23423028058516));
#242780=CARTESIAN_POINT('Origin',(21.151922343707,28.5729602337853,3.64303198860282));
#242781=CARTESIAN_POINT('Origin',(35.7621028045852,48.6820620414859,3.64299171721778));
#242782=CARTESIAN_POINT('Ctrl Pts',(35.9012693628904,48.8727133447946,3.48823028058515));
#242783=CARTESIAN_POINT('Ctrl Pts',(35.7983524848935,48.9481071848799,3.48852004212293));
#242784=CARTESIAN_POINT('Ctrl Pts',(35.7334106856005,48.8587224664503,3.42473028058515));
#242785=CARTESIAN_POINT('Ctrl Pts',(35.9276271141626,48.9091935744952,3.41028005848438));
#242786=CARTESIAN_POINT('Ctrl Pts',(35.8246659689632,48.9843245886195,3.41074404220615));
#242787=CARTESIAN_POINT('Ctrl Pts',(35.7730909105068,48.9133376106115,3.30780486244039));
#242788=CARTESIAN_POINT('Ctrl Pts',(35.9775622448338,48.9783048775141,3.36123028058516));
#242789=CARTESIAN_POINT('Ctrl Pts',(35.8745769537814,49.0530211657582,3.3614646058623));
#242790=CARTESIAN_POINT('Ctrl Pts',(35.8482644497253,49.0168051108897,3.23423045308385));
#242791=CARTESIAN_POINT('Ctrl Pts',(36.0301015792676,49.0510171431406,3.36123028058516));
#242792=CARTESIAN_POINT('Ctrl Pts',(35.927356420982,49.1256658701818,3.36123028058516));
#242793=CARTESIAN_POINT('Ctrl Pts',(35.927356420982,49.1256658701818,3.23423028058516));
#242794=CARTESIAN_POINT('Origin',(35.8361558438862,48.7840737394092,3.42473028058515));
#242795=CARTESIAN_POINT('Origin',(35.7883393569602,48.7182599907914,3.56563113524771));
#242796=CARTESIAN_POINT('Origin',(30.4370746247567,53.353559683258,3.56647653909472));
#242797=CARTESIAN_POINT('Origin',(30.4591427892367,53.3918862459819,3.64299466007685));
#242798=CARTESIAN_POINT('Origin',(30.3961554568836,53.2826856060848,3.42473028058522));
#242799=CARTESIAN_POINT('Ctrl Pts',(30.3416565762235,53.1871522506177,3.48823028058521));
#242800=CARTESIAN_POINT('Ctrl Pts',(30.4513942013112,53.1243619179798,3.48794691941637));
#242801=CARTESIAN_POINT('Ctrl Pts',(30.5061406831642,53.2191856060848,3.42473028058522));
#242802=CARTESIAN_POINT('Ctrl Pts',(30.3190533624383,53.1482340195359,3.41028005925124));
#242803=CARTESIAN_POINT('Ctrl Pts',(30.4287753876659,53.0851849835414,3.40982512231138));
#242804=CARTESIAN_POINT('Ctrl Pts',(30.4723866803445,53.1607219582423,3.30780486372914));
#242805=CARTESIAN_POINT('Ctrl Pts',(30.2762311741522,53.0745038491597,3.36123028058519));
#242806=CARTESIAN_POINT('Ctrl Pts',(30.3859720484839,53.0110474253434,3.36099721048323));
#242807=CARTESIAN_POINT('Ctrl Pts',(30.4084402641645,53.0499635164565,3.23423045308342));
#242808=CARTESIAN_POINT('Ctrl Pts',(30.2311753956711,52.996931757829,3.36123028058519));
#242809=CARTESIAN_POINT('Ctrl Pts',(30.3411606219517,52.933431757829,3.3612302805852));
#242810=CARTESIAN_POINT('Ctrl Pts',(30.3411606219517,52.933431757829,3.23423028058519));
#242811=CARTESIAN_POINT('Origin',(30.2311753956711,52.996931757829,3.23423028058518));
#242812=CARTESIAN_POINT('Origin',(-0.274963065701554,0.158750000000183,
3.64303198860263));
#242813=CARTESIAN_POINT('Origin',(30.6598643453574,53.7394427993289,3.64303198860301));
#242814=CARTESIAN_POINT('Origin',(-0.274963065701554,0.158750000000186,
3.23423028058481));
#242815=CARTESIAN_POINT('Origin',(30.1555713378337,52.8659816883962,3.23423028058518));
#242816=CARTESIAN_POINT('Ctrl Pts',(30.9286463962977,54.2060847114744,3.4715307213911));
#242817=CARTESIAN_POINT('Ctrl Pts',(31.0395064328261,54.1426202518669,3.47182327902701));
#242818=CARTESIAN_POINT('Ctrl Pts',(30.9851759176836,54.0488992551382,3.40413028959063));
#242819=CARTESIAN_POINT('Ctrl Pts',(30.8712564593359,54.1064496608377,3.65553807120995));
#242820=CARTESIAN_POINT('Ctrl Pts',(30.9819360667861,54.0429059732649,3.65586275496934));
#242821=CARTESIAN_POINT('Ctrl Pts',(30.9392002377703,53.9692670413566,3.55128126837215));
#242822=CARTESIAN_POINT('Ctrl Pts',(30.7681581606533,53.9274585619031,3.77003198860301));
#242823=CARTESIAN_POINT('Ctrl Pts',(30.8785940576189,53.8639133132292,3.77025505748627));
#242824=CARTESIAN_POINT('Ctrl Pts',(30.8566067980787,53.8262110069716,3.64284211731313));
#242825=CARTESIAN_POINT('Ctrl Pts',(30.6598643453574,53.7394427993289,3.77003198860301));
#242826=CARTESIAN_POINT('Ctrl Pts',(30.770013884466,53.6758479332734,3.77003198860301));
#242827=CARTESIAN_POINT('Ctrl Pts',(30.7698494490833,53.6759428700859,3.64284239821732));
#242828=CARTESIAN_POINT('Origin',(30.8752713784761,54.1125387249981,3.40423097483348));
#242829=CARTESIAN_POINT('Ctrl Pts',(30.1555713378337,52.8659816883962,3.36123028058519));
#242830=CARTESIAN_POINT('Ctrl Pts',(30.2655565641143,52.8024816883962,3.3612302805852));
#242831=CARTESIAN_POINT('Ctrl Pts',(30.2655565641143,52.8024816883962,3.23423028058519));
#242832=CARTESIAN_POINT('Ctrl Pts',(30.1103627734736,52.7881477055083,3.3612302805852));
#242833=CARTESIAN_POINT('Ctrl Pts',(30.2205080277004,52.724455334521,3.36146538609984));
#242834=CARTESIAN_POINT('Ctrl Pts',(30.1980495259467,52.6855560684213,3.23423043688359));
#242835=CARTESIAN_POINT('Ctrl Pts',(30.0676130472596,52.714550696011,3.41054258693135));
#242836=CARTESIAN_POINT('Ctrl Pts',(30.178127438708,52.6510500011272,3.4110060885991));
#242837=CARTESIAN_POINT('Ctrl Pts',(30.1342168083496,52.5749945583581,3.3081986697097));
#242838=CARTESIAN_POINT('Ctrl Pts',(30.0450834959835,52.6757649139398,3.48823028058518));
#242839=CARTESIAN_POINT('Ctrl Pts',(30.1558192616,52.6124111049559,3.48852004212296));
#242840=CARTESIAN_POINT('Ctrl Pts',(30.1005764675357,52.5167277788844,3.42473028058518));
#242841=CARTESIAN_POINT('Origin',(29.9905912412551,52.5802277788844,3.42473028058518));
#242842=CARTESIAN_POINT('Origin',(30.9643459342412,54.2668203812011,3.1191364817839));
#242843=CARTESIAN_POINT('Origin',(31.0534204898633,54.4211020372441,2.83404198860299));
#242844=CARTESIAN_POINT('Origin',(29.9499161072422,52.5097763801589,3.56563113460804));
#242845=CARTESIAN_POINT('Origin',(29.9275190026063,52.4710850656386,3.64299171721831));
#242846=CARTESIAN_POINT('Ctrl Pts',(31.4638515574739,54.5275217339722,2.59908173516061));
#242847=CARTESIAN_POINT('Ctrl Pts',(31.4452069629852,54.4952102564868,2.658781988603));
#242848=CARTESIAN_POINT('Ctrl Pts',(31.410023123206,54.4342359163066,2.658781988603));
#242849=CARTESIAN_POINT('Ctrl Pts',(31.3875306471682,54.5715608148716,2.59908193475593));
#242850=CARTESIAN_POINT('Ctrl Pts',(31.3896121658899,54.5272862282513,2.65878715325435));
#242851=CARTESIAN_POINT('Ctrl Pts',(31.3658411130341,54.4597196360203,2.65878198860299));
#242852=CARTESIAN_POINT('Ctrl Pts',(31.3046029601557,54.5905300051366,2.63878778849934));
#242853=CARTESIAN_POINT('Ctrl Pts',(31.3268524737457,54.536796115311,2.69564460180165));
#242854=CARTESIAN_POINT('Ctrl Pts',(31.3125672934291,54.4615686025422,2.6818048162492));
#242855=CARTESIAN_POINT('Ctrl Pts',(31.1759014746041,54.5809273110399,2.75443238878657));
#242856=CARTESIAN_POINT('Ctrl Pts',(31.2415992967183,54.5158579940077,2.79268340777109));
#242857=CARTESIAN_POINT('Ctrl Pts',(31.222768219186,54.4295063924932,2.74885926835648));
#242858=CARTESIAN_POINT('Ctrl Pts',(31.1295364123888,54.554029236008,2.82856655361725));
#242859=CARTESIAN_POINT('Ctrl Pts',(31.2191033458805,54.4847364330945,2.85384197230826));
#242860=CARTESIAN_POINT('Ctrl Pts',(31.1861426211015,54.3969835118375,2.79184624278637));
#242861=CARTESIAN_POINT('Ctrl Pts',(31.1067982185534,54.514646476914,2.90134173516061));
#242862=CARTESIAN_POINT('Ctrl Pts',(31.2174884860864,54.4512761425985,2.90163218716429));
#242863=CARTESIAN_POINT('Ctrl Pts',(31.1634057161439,54.3576020372441,2.83404198860299));
#242864=CARTESIAN_POINT('Origin',(31.410023123206,54.4342359163066,2.53178198860299));
#242865=CARTESIAN_POINT('Origin',(-0.274963065701554,0.158750000000183,
3.64303198860263));
#242866=CARTESIAN_POINT('Origin',(29.7268821954849,52.1234703131949,3.64303198860299));
#242867=CARTESIAN_POINT('Origin',(5.5822321212813E-15,1.85739751585078E-13,
2.53178198860262));
#242868=CARTESIAN_POINT('Origin',(31.4364195775134,54.4189959163065,2.531781988603));
#242869=CARTESIAN_POINT('Ctrl Pts',(29.7268821954848,52.1234703131949,3.770031988603));
#242870=CARTESIAN_POINT('Ctrl Pts',(29.8370321846009,52.0598751873275,3.770031988603));
#242871=CARTESIAN_POINT('Ctrl Pts',(29.8368672985391,52.0599703843396,3.64284187937097));
#242872=CARTESIAN_POINT('Ctrl Pts',(29.6185926664441,51.9354481180159,3.77003198860299));
#242873=CARTESIAN_POINT('Ctrl Pts',(29.7286387544923,51.8721332875977,3.76980208962975));
#242874=CARTESIAN_POINT('Ctrl Pts',(29.7501084151995,51.9096995898733,3.6428419392844));
#242875=CARTESIAN_POINT('Ctrl Pts',(29.5155047636219,51.7564527430638,3.65553535416625));
#242876=CARTESIAN_POINT('Ctrl Pts',(29.625424309881,51.6933616226671,3.65520057834456));
#242877=CARTESIAN_POINT('Ctrl Pts',(29.6675155901175,51.766644619996,3.55127910964152));
#242878=CARTESIAN_POINT('Ctrl Pts',(29.4581217525673,51.656815567543,3.47153072139108));
#242879=CARTESIAN_POINT('Ctrl Pts',(29.5680161811089,51.5939283753698,3.47122746281618));
#242880=CARTESIAN_POINT('Ctrl Pts',(29.6215404737379,51.6870133822662,3.40413045901316));
#242881=CARTESIAN_POINT('Origin',(29.5114749418004,51.7503740054945,3.40423097483347));
#242882=CARTESIAN_POINT('Ctrl Pts',(31.6576696180583,54.196600726121,2.90134173516062));
#242883=CARTESIAN_POINT('Ctrl Pts',(31.5474441649283,54.2607761425985,2.90163218716429));
#242884=CARTESIAN_POINT('Ctrl Pts',(31.4933613949858,54.1671020372441,2.834041988603));
#242885=CARTESIAN_POINT('Ctrl Pts',(31.6804173065992,54.2360018544275,2.82853349835383));
#242886=CARTESIAN_POINT('Ctrl Pts',(31.5756301844086,54.2789150989578,2.8538148316219));
#242887=CARTESIAN_POINT('Ctrl Pts',(31.5161086602376,54.2065014563934,2.79182701594197));
#242888=CARTESIAN_POINT('Ctrl Pts',(31.6804328064621,54.2894509908547,2.75468822073695));
#242889=CARTESIAN_POINT('Ctrl Pts',(31.5911964272961,54.3138841827107,2.79286913083871));
#242890=CARTESIAN_POINT('Ctrl Pts',(31.5258675551965,54.2543268901839,2.74900763297946));
#242891=CARTESIAN_POINT('Ctrl Pts',(31.6250591602192,54.4049648787501,2.63954450640416));
#242892=CARTESIAN_POINT('Ctrl Pts',(31.5671393481782,54.3976088886512,2.69627684028899));
#242893=CARTESIAN_POINT('Ctrl Pts',(31.5090508246495,54.3475791360318,2.68224356036534));
#242894=CARTESIAN_POINT('Ctrl Pts',(31.5668453499337,54.4680334478298,2.59908178706333));
#242895=CARTESIAN_POINT('Ctrl Pts',(31.5274226111438,54.4477213412904,2.65878704321649));
#242896=CARTESIAN_POINT('Ctrl Pts',(31.4807263372355,54.3933906465338,2.658781988603));
#242897=CARTESIAN_POINT('Ctrl Pts',(31.4902932482907,54.5122556166613,2.59908173516061));
#242898=CARTESIAN_POINT('Ctrl Pts',(31.4716329851988,54.4799531854482,2.65878198860299));
#242899=CARTESIAN_POINT('Ctrl Pts',(31.4364195775134,54.4189959163066,2.658781988603));
#242900=CARTESIAN_POINT('Origin',(31.6033466212664,54.1036020372441,2.83404198860299));
#242901=CARTESIAN_POINT('Origin',(29.4224002636359,51.5960921371862,3.11913648167172));
#242902=CARTESIAN_POINT('Origin',(29.3333255853454,51.4418102687787,2.83404198860297));
#242903=CARTESIAN_POINT('Origin',(31.514272065599,53.9493203812113,3.11913648177522));
#242904=CARTESIAN_POINT('Origin',(31.4251975098792,53.7950387249981,3.40423097483348));
#242905=CARTESIAN_POINT('Ctrl Pts',(29.2799753962461,51.3482501200168,2.90134173516059));
#242906=CARTESIAN_POINT('Ctrl Pts',(29.3897042746973,51.2854610232004,2.90103711553265));
#242907=CARTESIAN_POINT('Ctrl Pts',(29.443310811626,51.3783102687787,2.83404198860297));
#242908=CARTESIAN_POINT('Ctrl Pts',(29.2572578385501,51.3089010921304,2.82862991748004));
#242909=CARTESIAN_POINT('Ctrl Pts',(29.3615397594609,51.2670685993238,2.85314045886498));
#242910=CARTESIAN_POINT('Ctrl Pts',(29.4205918519436,51.3389598763138,2.79187960999971));
#242911=CARTESIAN_POINT('Ctrl Pts',(29.2572680623749,51.2557407616058,2.75470625793352));
#242912=CARTESIAN_POINT('Ctrl Pts',(29.3461554108687,51.2319924817691,2.79224250381934));
#242913=CARTESIAN_POINT('Ctrl Pts',(29.4109522357566,51.2913733902317,2.74901809108292));
#242914=CARTESIAN_POINT('Ctrl Pts',(29.3127910737013,51.1410333861059,2.63947868311743));
#242915=CARTESIAN_POINT('Ctrl Pts',(29.3705286780144,51.1485922293427,2.69595066767947));
#242916=CARTESIAN_POINT('Ctrl Pts',(29.4282055900902,51.1987619028148,2.68220539436099));
#242917=CARTESIAN_POINT('Ctrl Pts',(29.3710651187648,51.0785202710264,2.59908178585195));
#242918=CARTESIAN_POINT('Ctrl Pts',(29.4103605382587,51.0989122516748,2.65877670944929));
#242919=CARTESIAN_POINT('Ctrl Pts',(29.456817530672,51.1533747228786,2.65878198860297));
#242920=CARTESIAN_POINT('Ctrl Pts',(29.4472515437734,51.0345602039889,2.59908173516059));
#242921=CARTESIAN_POINT('Ctrl Pts',(29.4658956314766,51.066871973898,2.65878198860297));
#242922=CARTESIAN_POINT('Ctrl Pts',(29.501078514911,51.1278468659049,2.65878198860297));
#242923=CARTESIAN_POINT('Origin',(29.501078514911,51.1278468659049,2.53178198860297));
#242924=CARTESIAN_POINT('Ctrl Pts',(31.2097904767605,53.4219427993289,3.770031988603));
#242925=CARTESIAN_POINT('Ctrl Pts',(31.0996409281621,53.4855376708633,3.770031988603));
#242926=CARTESIAN_POINT('Ctrl Pts',(31.0998053730486,53.4854427285638,3.64284238727594));
#242927=CARTESIAN_POINT('Ctrl Pts',(31.3184716867865,53.6097387976567,3.77003198860301));
#242928=CARTESIAN_POINT('Ctrl Pts',(31.2082219299913,53.6736064794787,3.77025506106071));
#242929=CARTESIAN_POINT('Ctrl Pts',(31.1865640704871,53.6357132000298,3.64284210642032));
#242930=CARTESIAN_POINT('Ctrl Pts',(31.4219325588445,53.7885186806146,3.65553527987871));
#242931=CARTESIAN_POINT('Ctrl Pts',(31.3115622968574,53.8525981958205,3.65585996532953));
#242932=CARTESIAN_POINT('Ctrl Pts',(31.2691568563325,53.7787681009853,3.55127902710111));
#242933=CARTESIAN_POINT('Ctrl Pts',(31.4795232016789,53.8880358395973,3.4715307213911));
#242934=CARTESIAN_POINT('Ctrl Pts',(31.3691313396259,53.9523112232411,3.47182327905227));
#242935=CARTESIAN_POINT('Ctrl Pts',(31.3151318380581,53.858399104952,3.40413028378004));
#242936=CARTESIAN_POINT('Origin',(31.2097904767605,53.4219427993289,3.643031988603));
#242937=CARTESIAN_POINT('Origin',(5.69400554112516E-15,1.86375525517094E-13,
2.53178198860262));
#242938=CARTESIAN_POINT('Origin',(29.5274749692184,51.1126068659049,2.53178198860297));
#242939=CARTESIAN_POINT('Origin',(15.8305769983922,26.7843636743468,3.64303198860281));
#242940=CARTESIAN_POINT('Origin',(31.0091584503732,53.0743345559682,3.6429946600739));
#242941=CARTESIAN_POINT('Ctrl Pts',(29.4735998357337,51.019348010533,2.59908173516059));
#242942=CARTESIAN_POINT('Ctrl Pts',(29.4922606054645,51.0516501490689,2.65878198860298));
#242943=CARTESIAN_POINT('Ctrl Pts',(29.5274749692184,51.112606865905,2.65878198860297));
#242944=CARTESIAN_POINT('Ctrl Pts',(29.5495039426972,50.9754987628541,2.59908193199997));
#242945=CARTESIAN_POINT('Ctrl Pts',(29.5475581014581,51.0197013834526,2.65877685806694));
#242946=CARTESIAN_POINT('Ctrl Pts',(29.5715624158012,51.0871269269775,2.65878198860297));
#242947=CARTESIAN_POINT('Ctrl Pts',(29.6319914129671,50.9562029902291,2.63872492669847));
#242948=CARTESIAN_POINT('Ctrl Pts',(29.6100038038528,51.0098791271092,2.69532212015295));
#242949=CARTESIAN_POINT('Ctrl Pts',(29.6246193648995,51.0848223701589,2.68176836726675));
#242950=CARTESIAN_POINT('Ctrl Pts',(29.760039537519,50.9652607924607,2.75442176402272));
#242951=CARTESIAN_POINT('Ctrl Pts',(29.6951164119093,51.0303675504161,2.79203179920195));
#242952=CARTESIAN_POINT('Ctrl Pts',(29.7140610042231,51.1161687394136,2.74885310748206));
#242953=CARTESIAN_POINT('Ctrl Pts',(29.8061925581058,50.9919958361064,2.82866089558443));
#242954=CARTESIAN_POINT('Ctrl Pts',(29.7178148857791,51.0613912713631,2.85316563119302));
#242955=CARTESIAN_POINT('Ctrl Pts',(29.7505571803537,51.1484765898561,2.79189751796687));
#242956=CARTESIAN_POINT('Ctrl Pts',(29.8289013456884,51.0313275753411,2.90134173516059));
#242957=CARTESIAN_POINT('Ctrl Pts',(29.7196599535392,51.0949610232004,2.90103711553265));
#242958=CARTESIAN_POINT('Ctrl Pts',(29.7732664904679,51.1878102687787,2.83404198860297));
#242959=CARTESIAN_POINT('Origin',(29.8832517167485,51.1243102687787,2.83404198860297));
#242960=CARTESIAN_POINT('Origin',(30.9870007553607,53.0360596824713,3.56647653971874));
#242961=CARTESIAN_POINT('Origin',(30.9460815882867,52.9651856060848,3.42473028058523));
#242962=CARTESIAN_POINT('Origin',(29.972326394982,51.2785921372019,3.11913648168102));
#242963=CARTESIAN_POINT('Origin',(30.0614010732035,51.4328740054945,3.40423097483347));
#242964=CARTESIAN_POINT('Ctrl Pts',(30.7811015270742,52.679431757829,3.36123028058519));
#242965=CARTESIAN_POINT('Ctrl Pts',(30.6711163007936,52.742931757829,3.36123028058519));
#242966=CARTESIAN_POINT('Ctrl Pts',(30.6711163007936,52.742931757829,3.23423028058519));
#242967=CARTESIAN_POINT('Ctrl Pts',(30.8259039490946,52.757500212918,3.36123028058519));
#242968=CARTESIAN_POINT('Ctrl Pts',(30.7160792752564,52.8208099140555,3.36099641108374));
#242969=CARTESIAN_POINT('Ctrl Pts',(30.738623332912,52.8598573673263,3.23423043688369));
#242970=CARTESIAN_POINT('Ctrl Pts',(30.8682695960183,52.8313189037788,3.4105425890532));
#242971=CARTESIAN_POINT('Ctrl Pts',(30.758807217536,52.8948168809936,3.41008815826104));
#242972=CARTESIAN_POINT('Ctrl Pts',(30.8024560343135,52.9704188493381,3.30819867304328));
#242973=CARTESIAN_POINT('Ctrl Pts',(30.8905967158735,52.8702215132218,3.48823028058522));
#242974=CARTESIAN_POINT('Ctrl Pts',(30.7813498801531,52.9338619179798,3.48794691941637));
#242975=CARTESIAN_POINT('Ctrl Pts',(30.8360963620061,53.0286856060848,3.42473028058523));
#242976=CARTESIAN_POINT('Origin',(30.7811015270742,52.679431757829,3.23423028058519));
#242977=CARTESIAN_POINT('Ctrl Pts',(30.0070536838157,51.33988956927,3.47153072139108));
#242978=CARTESIAN_POINT('Ctrl Pts',(29.8976445761574,51.4036173326914,3.47122746285113));
#242979=CARTESIAN_POINT('Ctrl Pts',(29.9514963916953,51.4965132298825,3.40413046676816));
#242980=CARTESIAN_POINT('Ctrl Pts',(30.0646513737708,51.4394048060583,3.65553813458026));
#242981=CARTESIAN_POINT('Ctrl Pts',(29.9550530981048,51.503052357962,3.65520336072079));
#242982=CARTESIAN_POINT('Ctrl Pts',(29.997472204327,51.5761456730035,3.55128134519865));
#242983=CARTESIAN_POINT('Ctrl Pts',(30.1681227811157,51.6181806476923,3.77003198860299));
#242984=CARTESIAN_POINT('Ctrl Pts',(30.0582674911759,51.6818259279778,3.76980209314328));
#242985=CARTESIAN_POINT('Ctrl Pts',(30.0800656843521,51.7192017762862,3.6428419538755));
#242986=CARTESIAN_POINT('Ctrl Pts',(30.276808326888,51.8059703131949,3.77003198860299));
#242987=CARTESIAN_POINT('Ctrl Pts',(30.1666583504933,51.8695654317176,3.77003198860299));
#242988=CARTESIAN_POINT('Ctrl Pts',(30.1668232238147,51.8694702420611,3.64284189403824));
#242989=CARTESIAN_POINT('Origin',(30.276808326888,51.8059703131949,3.64303198860299));
#242990=CARTESIAN_POINT('Origin',(15.4537755657014,26.1317244485617,3.234230280585));
#242991=CARTESIAN_POINT('Origin',(30.7054974692368,52.5484816883962,3.23423028058518));
#242992=CARTESIAN_POINT('Origin',(15.3947701216591,26.0295240215572,3.64303198860281));
#242993=CARTESIAN_POINT('Origin',(30.4775331296737,52.1535342613183,3.64299171721843));
#242994=CARTESIAN_POINT('Ctrl Pts',(30.5960088312567,52.3576880233165,3.48823028058518));
#242995=CARTESIAN_POINT('Ctrl Pts',(30.4857749404419,52.4219111049559,3.48852004212296));
#242996=CARTESIAN_POINT('Ctrl Pts',(30.4305321463775,52.3262277788844,3.42473028058518));
#242997=CARTESIAN_POINT('Ctrl Pts',(30.6184089696598,52.3967235457371,3.41028005848445));
#242998=CARTESIAN_POINT('Ctrl Pts',(30.5081585269356,52.4606806140204,3.41074404220395));
#242999=CARTESIAN_POINT('Ctrl Pts',(30.4642861617693,52.3846914485024,3.30780486244026));
#243000=CARTESIAN_POINT('Ctrl Pts',(30.660846452162,52.4706758922788,3.36123028058519));
#243001=CARTESIAN_POINT('Ctrl Pts',(30.5506153465192,52.5342179826657,3.36146460586487));
#243002=CARTESIAN_POINT('Ctrl Pts',(30.5282325936728,52.495449917522,3.23423045308379));
#243003=CARTESIAN_POINT('Ctrl Pts',(30.7054974692368,52.5484816883962,3.36123028058519));
#243004=CARTESIAN_POINT('Ctrl Pts',(30.5955122429562,52.6119816883962,3.36123028058519));
#243005=CARTESIAN_POINT('Ctrl Pts',(30.5955122429562,52.6119816883962,3.23423028058519));
#243006=CARTESIAN_POINT('Origin',(30.5405173726582,52.2627277788844,3.42473028058517));
#243007=CARTESIAN_POINT('Origin',(30.4998422394564,52.1922763809702,3.56563113524778));
#243008=CARTESIAN_POINT('Origin',(24.6933715417281,56.2428239377268,3.56647653909482));
#243009=CARTESIAN_POINT('Origin',(24.711312597791,56.2832472948498,3.64299466007726));
#243010=CARTESIAN_POINT('Origin',(24.660084891711,56.168060898428,3.42473028058523));
#243011=CARTESIAN_POINT('Ctrl Pts',(24.6158705164593,56.0673542004328,3.48823028058523));
#243012=CARTESIAN_POINT('Ctrl Pts',(24.7315703643334,56.01637854512,3.48794691941639));
#243013=CARTESIAN_POINT('Ctrl Pts',(24.7761051648316,56.1164053447574,3.42473028058524));
#243014=CARTESIAN_POINT('Ctrl Pts',(24.5974591883329,56.0262864882908,3.41028005925126));
#243015=CARTESIAN_POINT('Ctrl Pts',(24.7131705636703,55.9750519161968,3.40982512231045));
#243016=CARTESIAN_POINT('Ctrl Pts',(24.7486471852376,56.0547337128522,3.30780486372799));
#243017=CARTESIAN_POINT('Ctrl Pts',(24.5625784858792,55.9484840819678,3.36123028058521));
#243018=CARTESIAN_POINT('Ctrl Pts',(24.6783511906842,55.8968463240315,3.36099721048404));
#243019=CARTESIAN_POINT('Ctrl Pts',(24.6966284839291,55.9378977967826,3.23423045308457));
#243020=CARTESIAN_POINT('Ctrl Pts',(24.525878019167,55.8666273273835,3.36123028058521));
#243021=CARTESIAN_POINT('Ctrl Pts',(24.6418982922876,55.8149717737129,3.36123028058521));
#243022=CARTESIAN_POINT('Ctrl Pts',(24.6418982922876,55.8149717737129,3.23423028058521));
#243023=CARTESIAN_POINT('Origin',(24.525878019167,55.8666273273835,3.23423028058521));
#243024=CARTESIAN_POINT('Origin',(-0.290050682801521,0.12913888417675,3.64303198860263));
#243025=CARTESIAN_POINT('Origin',(24.8746050278051,56.6498810128384,3.64303198860303));
#243026=CARTESIAN_POINT('Origin',(-0.29005068280152,0.129138884176753,3.23423028058481));
#243027=CARTESIAN_POINT('Origin',(24.4643761377916,55.72849184015,3.2342302805852));
#243028=CARTESIAN_POINT('Ctrl Pts',(25.0931373005745,57.1420619865024,3.47153072139112));
#243029=CARTESIAN_POINT('Ctrl Pts',(25.2100238766582,57.0905332211011,3.47182327902702));
#243030=CARTESIAN_POINT('Ctrl Pts',(25.1657875015263,56.9916465525422,3.40413028959063));
#243031=CARTESIAN_POINT('Ctrl Pts',(25.0464764504229,57.0369738651803,3.65553807120995));
#243032=CARTESIAN_POINT('Ctrl Pts',(25.1631918674189,56.9853474458578,3.65586275496902));
#243033=CARTESIAN_POINT('Ctrl Pts',(25.128387514131,56.9076448051904,3.55128126837224));
#243034=CARTESIAN_POINT('Ctrl Pts',(24.9626525995183,56.8481865914869,3.77003198860303));
#243035=CARTESIAN_POINT('Ctrl Pts',(25.0791258042763,56.7965331449332,3.77025505748708));
#243036=CARTESIAN_POINT('Ctrl Pts',(25.0611999573796,56.7567390814036,3.64284211731277));
#243037=CARTESIAN_POINT('Ctrl Pts',(24.8746050278051,56.6498810128384,3.77003198860303));
#243038=CARTESIAN_POINT('Ctrl Pts',(24.990798629834,56.5981482881658,3.77003198860303));
#243039=CARTESIAN_POINT('Ctrl Pts',(24.9906251716464,56.5982255167267,3.64284239821729));
#243040=CARTESIAN_POINT('Origin',(25.0498328948964,57.0434492461381,3.4042309748335));
#243041=CARTESIAN_POINT('Ctrl Pts',(24.4643761377916,55.72849184015,3.3612302805852));
#243042=CARTESIAN_POINT('Ctrl Pts',(24.5803964109122,55.6768362864794,3.36123028058521));
#243043=CARTESIAN_POINT('Ctrl Pts',(24.5803964109122,55.6768362864794,3.2342302805852));
#243044=CARTESIAN_POINT('Ctrl Pts',(24.427551097298,55.6463586582055,3.36123028058521));
#243045=CARTESIAN_POINT('Ctrl Pts',(24.5437506299578,55.5945285148468,3.36146538610306));
#243046=CARTESIAN_POINT('Ctrl Pts',(24.5254812387356,55.5534947903256,3.23423043688532));
#243047=CARTESIAN_POINT('Ctrl Pts',(24.3927285408587,55.5686962576416,3.41054258693139));
#243048=CARTESIAN_POINT('Ctrl Pts',(24.5092751529615,55.5170953257214,3.41100608859824));
#243049=CARTESIAN_POINT('Ctrl Pts',(24.4735550281879,55.4368666119059,3.3081986697084));
#243050=CARTESIAN_POINT('Ctrl Pts',(24.3743766270213,55.5277679687685,3.4882302805852));
#243051=CARTESIAN_POINT('Ctrl Pts',(24.4911280468225,55.4763362579877,3.48852004212298));
#243052=CARTESIAN_POINT('Ctrl Pts',(24.4461895095988,55.3754026508177,3.4247302805852));
#243053=CARTESIAN_POINT('Origin',(24.3301692364782,55.4270582044884,3.4247302805852));
#243054=CARTESIAN_POINT('Origin',(25.1222926664936,57.2061965577162,3.11913648178449));
#243055=CARTESIAN_POINT('Origin',(25.1947524379615,57.3689438691199,2.83404198860302));
#243056=CARTESIAN_POINT('Origin',(24.2970811015511,55.352741036646,3.56563113460901));
#243057=CARTESIAN_POINT('Origin',(24.2788510342448,55.3119205422648,3.64299171721853));
#243058=CARTESIAN_POINT('Ctrl Pts',(25.5918112338793,57.5176823163891,2.59908173516063));
#243059=CARTESIAN_POINT('Ctrl Pts',(25.5766462455175,57.483598953748,2.65878198860302));
#243060=CARTESIAN_POINT('Ctrl Pts',(25.5480287005717,57.4192809246791,2.65878198860302));
#243061=CARTESIAN_POINT('Ctrl Pts',(25.5113050800555,57.5535024391258,2.59908193475632));
#243062=CARTESIAN_POINT('Ctrl Pts',(25.5180031505025,57.5096879712802,2.65878715325401));
#243063=CARTESIAN_POINT('Ctrl Pts',(25.5014249500146,57.4400067642831,2.65878198860302));
#243064=CARTESIAN_POINT('Ctrl Pts',(25.4268488592818,57.5636994104963,2.63878778849911));
#243065=CARTESIAN_POINT('Ctrl Pts',(25.4545932086374,57.5125855880056,2.69564460180157));
#243066=CARTESIAN_POINT('Ctrl Pts',(25.4482497003385,57.4362769714773,2.68180481624919));
#243067=CARTESIAN_POINT('Ctrl Pts',(25.2998561687912,57.5406963524573,2.75443238878687));
#243068=CARTESIAN_POINT('Ctrl Pts',(25.3719956870768,57.4828507843377,2.7926834077713));
#243069=CARTESIAN_POINT('Ctrl Pts',(25.3622939683645,57.3950038423349,2.74885926835656));
#243070=CARTESIAN_POINT('Ctrl Pts',(25.2565567136862,57.5090991591924,2.82856655361708));
#243071=CARTESIAN_POINT('Ctrl Pts',(25.3528760603488,57.4495482434217,2.85384197230864));
#243072=CARTESIAN_POINT('Ctrl Pts',(25.3292685758746,57.3588307079384,2.79184624278516));
#243073=CARTESIAN_POINT('Ctrl Pts',(25.2380597013429,57.4675553545143,2.90134173516065));
#243074=CARTESIAN_POINT('Ctrl Pts',(25.3547675996714,57.4161024530846,2.90163218716432));
#243075=CARTESIAN_POINT('Ctrl Pts',(25.3107727110821,57.3172883154492,2.83404198860303));
#243076=CARTESIAN_POINT('Origin',(25.5480287005717,57.4192809246791,2.53178198860302));
#243077=CARTESIAN_POINT('Origin',(-0.290050682801521,0.12913888417675,3.64303198860263));
#243078=CARTESIAN_POINT('Origin',(24.1156489724276,54.9452378026831,3.64303198860301));
#243079=CARTESIAN_POINT('Origin',(5.59761027822878E-15,1.85731916022747E-13,
2.53178198860262));
#243080=CARTESIAN_POINT('Origin',(25.5758735661207,57.4068835917982,2.53178198860302));
#243081=CARTESIAN_POINT('Ctrl Pts',(24.1156489724276,54.9452378026831,3.77003198860302));
#243082=CARTESIAN_POINT('Ctrl Pts',(24.2318430491563,54.8935048666605,3.77003198860301));
#243083=CARTESIAN_POINT('Ctrl Pts',(24.2316691155602,54.8935823068868,3.64284187937092));
#243084=CARTESIAN_POINT('Ctrl Pts',(24.0276063358801,54.7469262747036,3.77003198860301));
#243085=CARTESIAN_POINT('Ctrl Pts',(24.1436677818719,54.6954612380267,3.7698020896317));
#243086=CARTESIAN_POINT('Ctrl Pts',(24.1610930816811,54.735065938806,3.64284193928378));
#243087=CARTESIAN_POINT('Ctrl Pts',(23.9437932708528,54.5581358350801,3.65553535416626));
#243088=CARTESIAN_POINT('Ctrl Pts',(24.0597054841979,54.5068800556897,3.6552005783446));
#243089=CARTESIAN_POINT('Ctrl Pts',(24.0939060249002,54.5841613379376,3.55127910964213));
#243090=CARTESIAN_POINT('Ctrl Pts',(23.8971395307767,54.4530463244695,3.4715307213911));
#243091=CARTESIAN_POINT('Ctrl Pts',(24.0130054476975,54.4019907306521,3.4712274628162));
#243092=CARTESIAN_POINT('Ctrl Pts',(24.056506495927,54.5001606201972,3.40413045901315));
#243093=CARTESIAN_POINT('Origin',(23.940420925912,54.5516691663897,3.40423097483348));
#243094=CARTESIAN_POINT('Ctrl Pts',(25.8191582032619,57.2088336324701,2.90134173516064));
#243095=CARTESIAN_POINT('Ctrl Pts',(25.7028284190332,57.2611357920727,2.90163218716432));
#243096=CARTESIAN_POINT('Ctrl Pts',(25.658833530444,57.1623216544374,2.83404198860302));
#243097=CARTESIAN_POINT('Ctrl Pts',(25.8376627381927,57.2503966981989,2.82853349835388));
#243098=CARTESIAN_POINT('Ctrl Pts',(25.7289639953178,57.2821216226341,2.85381483162346));
#243099=CARTESIAN_POINT('Ctrl Pts',(25.6773378230594,57.2038829761266,2.79182701594241));
#243100=CARTESIAN_POINT('Ctrl Pts',(25.8320911970514,57.3035546548414,2.75468822073695));
#243101=CARTESIAN_POINT('Ctrl Pts',(25.7407897001103,57.3185262575348,2.79286913083887));
#243102=CARTESIAN_POINT('Ctrl Pts',(25.6820441386715,57.2524664994801,2.74900763297955));
#243103=CARTESIAN_POINT('Ctrl Pts',(25.7649464042485,57.4126476234252,2.63954450640422));
#243104=CARTESIAN_POINT('Ctrl Pts',(25.7081127933386,57.3992776612639,2.69627684028889));
#243105=CARTESIAN_POINT('Ctrl Pts',(25.6555720179788,57.3434500727663,2.68224356036531));
#243106=CARTESIAN_POINT('Ctrl Pts',(25.7004590346999,57.4692856961532,2.5990817870655));
#243107=CARTESIAN_POINT('Ctrl Pts',(25.6633754510789,57.444964063152,2.65878704321591));
#243108=CARTESIAN_POINT('Ctrl Pts',(25.6226140882766,57.3860499078752,2.65878198860302));
#243109=CARTESIAN_POINT('Ctrl Pts',(25.6197038181297,57.5052637377734,2.59908173516064));
#243110=CARTESIAN_POINT('Ctrl Pts',(25.604522301406,57.4711877340332,2.65878198860302));
#243111=CARTESIAN_POINT('Ctrl Pts',(25.5758735661207,57.4068835917982,2.65878198860302));
#243112=CARTESIAN_POINT('Origin',(25.7748538035646,57.1106661007667,2.83404198860302));
#243113=CARTESIAN_POINT('Origin',(23.8679610547573,54.3889216310773,3.11913648167036));
#243114=CARTESIAN_POINT('Origin',(23.7955011834907,54.2261740956468,2.834041988603));
#243115=CARTESIAN_POINT('Origin',(25.7023940320475,56.9479187893683,3.11913648177501));
#243116=CARTESIAN_POINT('Origin',(25.6299342604994,56.785171477785,3.4042309748335));
#243117=CARTESIAN_POINT('Ctrl Pts',(23.7522229508827,54.1275498658876,2.90134173516062));
#243118=CARTESIAN_POINT('Ctrl Pts',(23.8679139708567,54.0765745253538,2.90103711553268));
#243119=CARTESIAN_POINT('Ctrl Pts',(23.9115214566113,54.1745185419762,2.834041988603));
#243120=CARTESIAN_POINT('Ctrl Pts',(23.733742935761,54.0860417646977,2.8286299174799));
#243121=CARTESIAN_POINT('Ctrl Pts',(23.8418262755866,54.0553388636012,2.85314045886498));
#243122=CARTESIAN_POINT('Ctrl Pts',(23.8930401898204,54.1330089371355,2.79187960999965));
#243123=CARTESIAN_POINT('Ctrl Pts',(23.7393098712349,54.0331737207071,2.75470625793376));
#243124=CARTESIAN_POINT('Ctrl Pts',(23.8301926567301,54.0188467943744,2.79224250381938));
#243125=CARTESIAN_POINT('Ctrl Pts',(23.8884275227223,54.0846755205376,2.74901809108294));
#243126=CARTESIAN_POINT('Ctrl Pts',(23.8065189073822,53.9248984592619,2.63947868311725));
#243127=CARTESIAN_POINT('Ctrl Pts',(23.8631501047898,53.9384511174158,2.69595066767948));
#243128=CARTESIAN_POINT('Ctrl Pts',(23.9152668978358,53.9943748351525,2.68220539436102));
#243129=CARTESIAN_POINT('Ctrl Pts',(23.8710081209825,53.8688190939459,2.59908178585064));
#243130=CARTESIAN_POINT('Ctrl Pts',(23.9079567336561,53.8932068550022,2.65877670945022));
#243131=CARTESIAN_POINT('Ctrl Pts',(23.9484663513836,53.9522270531159,2.658781988603));
#243132=CARTESIAN_POINT('Ctrl Pts',(23.9513722670364,53.833063494684,2.59908173516062));
#243133=CARTESIAN_POINT('Ctrl Pts',(23.9665367208223,53.8671470951733,2.658781988603));
#243134=CARTESIAN_POINT('Ctrl Pts',(23.9951532569806,53.9314655730807,2.658781988603));
#243135=CARTESIAN_POINT('Origin',(23.9951532569806,53.9314655730807,2.531781988603));
#243136=CARTESIAN_POINT('Ctrl Pts',(25.4547063934082,56.3916032444853,3.77003198860302));
#243137=CARTESIAN_POINT('Ctrl Pts',(25.338512781369,56.4433359736147,3.77003198860302));
#243138=CARTESIAN_POINT('Ctrl Pts',(25.3386862495819,56.4432587405904,3.64284238727598));
#243139=CARTESIAN_POINT('Ctrl Pts',(25.5431622092832,56.589730756554,3.77003198860303));
#243140=CARTESIAN_POINT('Ctrl Pts',(25.426840421557,56.6417243268787,3.7702550610602));
#243141=CARTESIAN_POINT('Ctrl Pts',(25.4092621323412,56.6017747680089,3.64284210642014));
#243142=CARTESIAN_POINT('Ctrl Pts',(25.6273687254288,56.778345870572,3.65553527987874));
#243143=CARTESIAN_POINT('Ctrl Pts',(25.510904950034,56.8305375176137,3.6558599653302));
#243144=CARTESIAN_POINT('Ctrl Pts',(25.4764491573042,56.7526792962305,3.55127902710133));
#243145=CARTESIAN_POINT('Ctrl Pts',(25.6742415049979,56.8833377255397,3.47153072139111));
#243146=CARTESIAN_POINT('Ctrl Pts',(25.5577357740375,56.935721910209,3.47182327905228));
#243147=CARTESIAN_POINT('Ctrl Pts',(25.5138485767963,56.8366797674139,3.40413028378006));
#243148=CARTESIAN_POINT('Origin',(25.4547063934082,56.3916032444853,3.64303198860302));
#243149=CARTESIAN_POINT('Origin',(5.68853496937358E-15,1.86378312912625E-13,
2.53178198860262));
#243150=CARTESIAN_POINT('Origin',(24.0229981225296,53.9190682401997,2.531781988603));
#243151=CARTESIAN_POINT('Origin',(10.5838037820516,22.9910091182299,3.64303198860278));
#243152=CARTESIAN_POINT('Origin',(25.2915084057467,56.0249274780507,3.64299466007881));
#243153=CARTESIAN_POINT('Ctrl Pts',(23.9791663275012,53.8206887816838,2.59908173516062));
#243154=CARTESIAN_POINT('Ctrl Pts',(23.9943483786816,53.8547645473083,2.658781988603));
#243155=CARTESIAN_POINT('Ctrl Pts',(24.0229981225296,53.9190682401997,2.658781988603));
#243156=CARTESIAN_POINT('Ctrl Pts',(24.0592381183002,53.785013884428,2.59908193199958));
#243157=CARTESIAN_POINT('Ctrl Pts',(24.052682504579,53.8287709626505,2.65877685806597));
#243158=CARTESIAN_POINT('Ctrl Pts',(24.069507432327,53.8983362760834,2.658781988603));
#243159=CARTESIAN_POINT('Ctrl Pts',(24.1432906710371,53.774446104571,2.63872492669847));
#243160=CARTESIAN_POINT('Ctrl Pts',(24.115812828244,53.8255298669652,2.69532212015298));
#243161=CARTESIAN_POINT('Ctrl Pts',(24.1225146216897,53.9015903052242,2.68176836726667));
#243162=CARTESIAN_POINT('Ctrl Pts',(24.2696905364172,53.7968389608978,2.75442176402277));
#243163=CARTESIAN_POINT('Ctrl Pts',(24.1983175571252,53.8548027426703,2.79203179920197));
#243164=CARTESIAN_POINT('Ctrl Pts',(24.2081897025475,53.9421141528987,2.74885310748219));
#243165=CARTESIAN_POINT('Ctrl Pts',(24.3127961529008,53.828251851494,2.82866089558446));
#243166=CARTESIAN_POINT('Ctrl Pts',(24.2176488245051,53.8880291490199,2.85316563119328));
#243167=CARTESIAN_POINT('Ctrl Pts',(24.241108858848,53.9780599067615,2.79189751796784));
#243168=CARTESIAN_POINT('Ctrl Pts',(24.3312692531087,53.8697418420147,2.90134173516062));
#243169=CARTESIAN_POINT('Ctrl Pts',(24.2159747902185,53.921607864342,2.90103711553268));
#243170=CARTESIAN_POINT('Ctrl Pts',(24.2595822759732,54.0195518809643,2.83404198860301));
#243171=CARTESIAN_POINT('Origin',(24.3756025490938,53.9678963272937,2.834041988603));
#243172=CARTESIAN_POINT('Origin',(25.2734729066204,55.9845461685094,3.56647653971757));
#243173=CARTESIAN_POINT('Origin',(25.2401862573141,55.9097831300749,3.42473028058525));
#243174=CARTESIAN_POINT('Origin',(24.4480624203051,54.1306438627325,3.1191364816796));
#243175=CARTESIAN_POINT('Origin',(24.5205222915151,54.2933913980366,3.40423097483349));
#243176=CARTESIAN_POINT('Ctrl Pts',(25.1059793847701,55.6083495590304,3.3612302805852));
#243177=CARTESIAN_POINT('Ctrl Pts',(24.9899591116494,55.660005112701,3.3612302805852));
#243178=CARTESIAN_POINT('Ctrl Pts',(24.9899591116494,55.660005112701,3.2342302805852));
#243179=CARTESIAN_POINT('Ctrl Pts',(25.142375998795,55.6906734752783,3.3612302805852));
#243180=CARTESIAN_POINT('Ctrl Pts',(25.0265352902397,55.7421565548659,3.36099641108629));
#243181=CARTESIAN_POINT('Ctrl Pts',(25.0448742789053,55.7833465978028,3.23423043688484));
#243182=CARTESIAN_POINT('Ctrl Pts',(25.1767934079544,55.7685161955958,3.41054258905326));
#243183=CARTESIAN_POINT('Ctrl Pts',(25.0612933298581,55.8202243900361,3.41008815825965));
#243184=CARTESIAN_POINT('Ctrl Pts',(25.0968004762779,55.8999747466307,3.30819867304262));
#243185=CARTESIAN_POINT('Ctrl Pts',(25.19493178753,55.8095395120009,3.48823028058524));
#243186=CARTESIAN_POINT('Ctrl Pts',(25.0796311836953,55.8614118841081,3.4879469194164));
#243187=CARTESIAN_POINT('Ctrl Pts',(25.1241659841935,55.9614386837455,3.42473028058525));
#243188=CARTESIAN_POINT('Origin',(25.10597938477,55.6083495590304,3.2342302805852));
#243189=CARTESIAN_POINT('Ctrl Pts',(24.4761921430391,54.1952354911874,3.4715307213911));
#243190=CARTESIAN_POINT('Ctrl Pts',(24.3607210247427,54.2471777813618,3.47122746285115));
#243191=CARTESIAN_POINT('Ctrl Pts',(24.4045675690227,54.3451938326304,3.40413046676837));
#243192=CARTESIAN_POINT('Ctrl Pts',(24.5230721320477,54.3002261711155,3.65553813458027));
#243193=CARTESIAN_POINT('Ctrl Pts',(24.4074212664101,54.3520689157434,3.65520336071997));
#243194=CARTESIAN_POINT('Ctrl Pts',(24.4419676644371,54.4291958219389,3.55128134519898));
#243195=CARTESIAN_POINT('Ctrl Pts',(24.607289548202,54.4888383671851,3.77003198860301));
#243196=CARTESIAN_POINT('Ctrl Pts',(24.4913833136911,54.5406519873239,3.76980209314289));
#243197=CARTESIAN_POINT('Ctrl Pts',(24.5091552540987,54.5801016184608,3.64284195387538));
#243198=CARTESIAN_POINT('Ctrl Pts',(24.6957503380306,54.68696003433,3.77003198860301));
#243199=CARTESIAN_POINT('Ctrl Pts',(24.5795562747216,54.7386929643777,3.77003198860301));
#243200=CARTESIAN_POINT('Ctrl Pts',(24.5797301948779,54.7386155301352,3.64284189403862));
#243201=CARTESIAN_POINT('Origin',(24.6957503380306,54.68696003433,3.64303198860301));
#243202=CARTESIAN_POINT('Origin',(10.3344596589366,22.4309730483567,3.23423028058497));
#243203=CARTESIAN_POINT('Origin',(25.0444775033946,55.4702140717969,3.2342302805852));
#243204=CARTESIAN_POINT('Origin',(10.295413467953,22.3432738675266,3.64303198860278));
#243205=CARTESIAN_POINT('Origin',(24.85904522396,55.0536014459541,3.64299171721827));
#243206=CARTESIAN_POINT('Ctrl Pts',(24.9555320242414,55.2690209153042,3.4882302805852));
#243207=CARTESIAN_POINT('Ctrl Pts',(24.8391888661843,55.3213695969758,3.48852004212297));
#243208=CARTESIAN_POINT('Ctrl Pts',(24.7942503289606,55.2204359898058,3.4247302805852));
#243209=CARTESIAN_POINT('Ctrl Pts',(24.9737291291703,55.3101840490933,3.41028005848448));
#243210=CARTESIAN_POINT('Ctrl Pts',(24.8573973158455,55.3622664445142,3.41074404220458));
#243211=CARTESIAN_POINT('Ctrl Pts',(24.821708318783,55.2821076446845,3.30780486243998));
#243212=CARTESIAN_POINT('Ctrl Pts',(25.0082040095654,55.3881672017732,3.36123028058521));
#243213=CARTESIAN_POINT('Ctrl Pts',(24.8919348043908,55.4398389138618,3.36146460586492));
#243214=CARTESIAN_POINT('Ctrl Pts',(24.8737270328797,55.3989435894769,3.23423045308494));
#243215=CARTESIAN_POINT('Ctrl Pts',(25.0444775033946,55.4702140717969,3.3612302805852));
#243216=CARTESIAN_POINT('Ctrl Pts',(24.928457230274,55.5218696254676,3.3612302805852));
#243217=CARTESIAN_POINT('Ctrl Pts',(24.928457230274,55.5218696254675,3.2342302805852));
#243218=CARTESIAN_POINT('Origin',(24.9102706020812,55.1687804361352,3.4247302805852));
#243219=CARTESIAN_POINT('Origin',(24.8771824678745,55.0944632691843,3.56563113524835));
#243220=CARTESIAN_POINT('Origin',(18.6791227126688,58.515880043567,3.56647653909436));
#243221=CARTESIAN_POINT('Origin',(18.6927400943491,58.5579573083292,3.64299466007643));
#243222=CARTESIAN_POINT('Origin',(18.6538332760103,58.4380471616457,3.42473028058524));
#243223=CARTESIAN_POINT('Ctrl Pts',(18.6203878281146,58.3332704847798,3.48823028058524));
#243224=CARTESIAN_POINT('Ctrl Pts',(18.7407822670301,58.294668006739,3.4879469194164));
#243225=CARTESIAN_POINT('Ctrl Pts',(18.7746174535798,58.3988020033601,3.42473028058524));
#243226=CARTESIAN_POINT('Ctrl Pts',(18.6063701040105,58.290503238026,3.41028005925128));
#243227=CARTESIAN_POINT('Ctrl Pts',(18.7268030714127,58.2516444665228,3.40982512231052));
#243228=CARTESIAN_POINT('Ctrl Pts',(18.7537563325803,58.3345980746929,3.30780486372867));
#243229=CARTESIAN_POINT('Ctrl Pts',(18.5798130476677,58.2094810151997,3.36123028058522));
#243230=CARTESIAN_POINT('Ctrl Pts',(18.7003491529667,58.1702276772278,3.36099721048497));
#243231=CARTESIAN_POINT('Ctrl Pts',(18.7142352739232,58.2129647630924,3.23423045308476));
#243232=CARTESIAN_POINT('Ctrl Pts',(18.5518699907149,58.1242364370959,3.36123028058522));
#243233=CARTESIAN_POINT('Ctrl Pts',(18.6726541682844,58.0849912788103,3.36123028058522));
#243234=CARTESIAN_POINT('Ctrl Pts',(18.6726541682844,58.0849912788103,3.23423028058522));
#243235=CARTESIAN_POINT('Origin',(18.5518699907149,58.1242364370959,3.23423028058522));
#243236=CARTESIAN_POINT('Origin',(-0.301960443923706,0.0981128957142288,
3.64303198860263));
#243237=CARTESIAN_POINT('Origin',(18.8168143322225,58.9396512752215,3.64303198860304));
#243238=CARTESIAN_POINT('Origin',(-0.301960443923706,0.0981128957142317,
3.23423028058481));
#243239=CARTESIAN_POINT('Origin',(18.505144113284,57.9804289733666,3.23423028058522));
#243240=CARTESIAN_POINT('Ctrl Pts',(18.9827025415095,59.451978872661,3.47153072139113));
#243241=CARTESIAN_POINT('Ctrl Pts',(19.1043350233606,59.4129503614029,3.47182327902704));
#243242=CARTESIAN_POINT('Ctrl Pts',(19.0706774512227,59.3099814440482,3.40413028959084));
#243243=CARTESIAN_POINT('Ctrl Pts',(18.9472820042048,59.3425890481026,3.65553807120996));
#243244=CARTESIAN_POINT('Ctrl Pts',(19.0687544722072,59.3034455268841,3.65586275497006));
#243245=CARTESIAN_POINT('Ctrl Pts',(19.0422629184333,59.2225305038464,3.55128126837233));
#243246=CARTESIAN_POINT('Ctrl Pts',(18.8836509927315,59.1460739925269,3.77003198860305));
#243247=CARTESIAN_POINT('Ctrl Pts',(19.0048854004761,59.1068782740652,3.77025505748499));
#243248=CARTESIAN_POINT('Ctrl Pts',(18.9912173655549,59.0654284453504,3.64284211731256));
#243249=CARTESIAN_POINT('Ctrl Pts',(18.8168143322225,58.9396512752215,3.77003198860304));
#243250=CARTESIAN_POINT('Ctrl Pts',(18.9377789557523,58.9003474864894,3.77003198860305));
#243251=CARTESIAN_POINT('Ctrl Pts',(18.9375983752043,58.9004061606661,3.64284239821769));
#243252=CARTESIAN_POINT('Origin',(18.9499432001057,59.3493798002282,3.40423097483351));
#243253=CARTESIAN_POINT('Ctrl Pts',(18.505144113284,57.9804289733666,3.36123028058522));
#243254=CARTESIAN_POINT('Ctrl Pts',(18.6259282908535,57.941183815081,3.36123028058522));
#243255=CARTESIAN_POINT('Ctrl Pts',(18.6259282908535,57.941183815081,3.23423028058522));
#243256=CARTESIAN_POINT('Ctrl Pts',(18.477106059509,57.8948964606934,3.36123028058522));
#243257=CARTESIAN_POINT('Ctrl Pts',(18.5980867642071,57.8554964068689,3.36146538610141));
#243258=CARTESIAN_POINT('Ctrl Pts',(18.5842066467862,57.8127777979911,3.23423043688481));
#243259=CARTESIAN_POINT('Ctrl Pts',(18.4505921960619,57.814019554574,3.41054258693141));
#243260=CARTESIAN_POINT('Ctrl Pts',(18.5718941197465,57.7748837362139,3.41100608859804));
#243261=CARTESIAN_POINT('Ctrl Pts',(18.5447558577167,57.6913607539433,3.3081986697087));
#243262=CARTESIAN_POINT('Ctrl Pts',(18.4366189870672,57.7713971777989,3.48823028058521));
#243263=CARTESIAN_POINT('Ctrl Pts',(18.5581069080659,57.7324510618073,3.48852004212299));
#243264=CARTESIAN_POINT('Ctrl Pts',(18.5239649837007,57.6273730232607,3.42473028058521));
#243265=CARTESIAN_POINT('Origin',(18.4031808061312,57.6666181815464,3.42473028058521));
#243266=CARTESIAN_POINT('Origin',(19.0049943031126,59.518809673581,3.11913648178592));
#243267=CARTESIAN_POINT('Origin',(19.0600454060086,59.6882395467423,2.83404198860303));
#243268=CARTESIAN_POINT('Origin',(18.3780421908163,57.5892494790278,3.56563113460797));
#243269=CARTESIAN_POINT('Origin',(18.3641788932756,57.5467470426664,3.64299171721853));
#243270=CARTESIAN_POINT('Ctrl Pts',(19.4393816709755,59.8776671349988,2.59908173516065));
#243271=CARTESIAN_POINT('Ctrl Pts',(19.4278624395265,59.8421853116555,2.65878198860303));
#243272=CARTESIAN_POINT('Ctrl Pts',(19.4061247292252,59.7752282754839,2.65878198860303));
#243273=CARTESIAN_POINT('Ctrl Pts',(19.3555723159021,59.9048758468124,2.59908193475641));
#243274=CARTESIAN_POINT('Ctrl Pts',(19.3668135526097,59.8620015382116,2.65878715325483));
#243275=CARTESIAN_POINT('Ctrl Pts',(19.3576098387255,59.7909691583393,2.65878198860303));
#243276=CARTESIAN_POINT('Ctrl Pts',(19.2705128813952,59.9061888791358,2.63878778849937));
#243277=CARTESIAN_POINT('Ctrl Pts',(19.3034480936186,59.8582551377154,2.69564460180157));
#243278=CARTESIAN_POINT('Ctrl Pts',(19.3051157581416,59.7817014705981,2.68180481624928));
#243279=CARTESIAN_POINT('Ctrl Pts',(19.1466203444579,59.8700374834727,2.75443238878662));
#243280=CARTESIAN_POINT('Ctrl Pts',(19.2244111832569,59.8200494324149,2.79268340777132));
#243281=CARTESIAN_POINT('Ctrl Pts',(19.2239451174252,59.7316696194044,2.74885926835648));
#243282=CARTESIAN_POINT('Ctrl Pts',(19.1068608943533,59.8340873574361,2.82856655361729));
#243283=CARTESIAN_POINT('Ctrl Pts',(19.2088773592693,59.7849307811039,2.85384197230968));
#243284=CARTESIAN_POINT('Ctrl Pts',(19.1948817636406,59.6922425516966,2.7918462427856));
#243285=CARTESIAN_POINT('Ctrl Pts',(19.092807720641,59.7908376697914,2.90134173516065));
#243286=CARTESIAN_POINT('Ctrl Pts',(19.2142545736082,59.7518659300028,2.90163218716432));
#243287=CARTESIAN_POINT('Ctrl Pts',(19.180829583578,59.6489943884566,2.83404198860303));
#243288=CARTESIAN_POINT('Origin',(19.4061247292252,59.7752282754839,2.53178198860303));
#243289=CARTESIAN_POINT('Origin',(-0.301960443923706,0.0981128957142288,
3.64303198860263));
#243290=CARTESIAN_POINT('Origin',(18.2401996527044,57.1650137687749,3.64303198860302));
#243291=CARTESIAN_POINT('Origin',(5.61372323131277E-15,1.8572573083956E-13,
2.53178198860262));
#243292=CARTESIAN_POINT('Origin',(19.4351129318419,59.7658094374954,2.53178198860303));
#243293=CARTESIAN_POINT('Ctrl Pts',(18.2401996527044,57.1650137687749,3.77003198860303));
#243294=CARTESIAN_POINT('Ctrl Pts',(18.3611647704259,57.12570981947,3.77003198860303));
#243295=CARTESIAN_POINT('Ctrl Pts',(18.3609836949485,57.1257686544592,3.64284187937102));
#243296=CARTESIAN_POINT('Ctrl Pts',(18.1733685221985,56.9585856505955,3.77003198860303));
#243297=CARTESIAN_POINT('Ctrl Pts',(18.2941737326411,56.9195342693639,3.76980208963088));
#243298=CARTESIAN_POINT('Ctrl Pts',(18.3073637563258,56.9607434512639,3.64284193928411));
#243299=CARTESIAN_POINT('Ctrl Pts',(18.1097485684436,56.7620685738649,3.65553535416627));
#243300=CARTESIAN_POINT('Ctrl Pts',(18.2303834904051,56.7232097045396,3.65520057834355));
#243301=CARTESIAN_POINT('Ctrl Pts',(18.2563185833005,56.8036425617911,3.55127910964214));
#243302=CARTESIAN_POINT('Ctrl Pts',(18.074335247489,56.6526781108326,3.47153072139112));
#243303=CARTESIAN_POINT('Ctrl Pts',(18.1949032015565,56.614013491141,3.47122746281622));
#243304=CARTESIAN_POINT('Ctrl Pts',(18.227904398799,56.7161926934813,3.40413045901321));
#243305=CARTESIAN_POINT('Origin',(18.1070706485041,56.7552848242273,3.4042309748335));
#243306=CARTESIAN_POINT('Ctrl Pts',(19.6977666881844,59.5942745858238,2.90134173516066));
#243307=CARTESIAN_POINT('Ctrl Pts',(19.5766071063167,59.6341304551459,2.90163218716433));
#243308=CARTESIAN_POINT('Ctrl Pts',(19.5431821162865,59.5312589135998,2.83404198860304));
#243309=CARTESIAN_POINT('Ctrl Pts',(19.711825329948,59.6375442153292,2.82853349835397));
#243310=CARTESIAN_POINT('Ctrl Pts',(19.6004058925608,59.6577332347587,2.85381483162415));
#243311=CARTESIAN_POINT('Ctrl Pts',(19.5572406993635,59.5745267832919,2.79182701594345));
#243312=CARTESIAN_POINT('Ctrl Pts',(19.7007277907734,59.68982858249,2.75468822073685));
#243313=CARTESIAN_POINT('Ctrl Pts',(19.6083614943633,59.6951745640079,2.79286913083897));
#243314=CARTESIAN_POINT('Ctrl Pts',(19.55684287225,59.6233361049592,2.74900763297965));
#243315=CARTESIAN_POINT('Ctrl Pts',(19.6225475038109,59.7913053863692,2.63954450640434));
#243316=CARTESIAN_POINT('Ctrl Pts',(19.5674227749671,59.7720679362492,2.69627684028884));
#243317=CARTESIAN_POINT('Ctrl Pts',(19.5210053955057,59.7110541706152,2.68224356036523));
#243318=CARTESIAN_POINT('Ctrl Pts',(19.5524931121161,59.84089242417,2.59908178706474));
#243319=CARTESIAN_POINT('Ctrl Pts',(19.5181549791683,59.8128277376115,2.65878704321603));
#243320=CARTESIAN_POINT('Ctrl Pts',(19.4837751174921,59.7499755976275,2.65878198860303));
#243321=CARTESIAN_POINT('Ctrl Pts',(19.4684195516695,59.8682321556244,2.59908173516065));
#243322=CARTESIAN_POINT('Ctrl Pts',(19.4568831131883,59.8327559231848,2.65878198860303));
#243323=CARTESIAN_POINT('Ctrl Pts',(19.4351129318419,59.7658094374954,2.65878198860303));
#243324=CARTESIAN_POINT('Origin',(19.663966293856,59.4920137553142,2.83404198860303));
#243325=CARTESIAN_POINT('Origin',(18.0520194698747,56.5858547179582,3.11913648167174));
#243326=CARTESIAN_POINT('Origin',(17.996968291141,56.4164246115666,2.83404198860302));
#243327=CARTESIAN_POINT('Origin',(19.6089151909119,59.3225838821511,3.11913648177552));
#243328=CARTESIAN_POINT('Origin',(19.5538640879531,59.1531540088001,3.40423097483351));
#243329=CARTESIAN_POINT('Ctrl Pts',(17.9642361803971,56.3138168485097,2.90134173516062));
#243330=CARTESIAN_POINT('Ctrl Pts',(18.0846218068694,56.2752137607568,2.90103711553268));
#243331=CARTESIAN_POINT('Ctrl Pts',(18.1177524687105,56.377179453281,2.83404198860301));
#243332=CARTESIAN_POINT('Ctrl Pts',(17.9501961787627,56.2706044454594,2.82862991748007));
#243333=CARTESIAN_POINT('Ctrl Pts',(18.060896753813,56.2513675234856,2.85314045886484));
#243334=CARTESIAN_POINT('Ctrl Pts',(18.1037113794376,56.3339654239819,2.79187961000007));
#243335=CARTESIAN_POINT('Ctrl Pts',(17.9612588333756,56.2186079213555,2.75470625793356));
#243336=CARTESIAN_POINT('Ctrl Pts',(18.0531413250553,56.2138593173288,2.79224250381926));
#243337=CARTESIAN_POINT('Ctrl Pts',(18.1041761987739,56.2854146278935,2.7490180910829));
#243338=CARTESIAN_POINT('Ctrl Pts',(18.0394175380795,56.1179510603879,2.63947868311746));
#243339=CARTESIAN_POINT('Ctrl Pts',(18.0943218653326,56.1373490477011,2.69595066767958));
#243340=CARTESIAN_POINT('Ctrl Pts',(18.1403075368578,56.1984140977479,2.68220539436108));
#243341=CARTESIAN_POINT('Ctrl Pts',(18.1094153628979,56.0689198620984,2.5990817858519));
#243342=CARTESIAN_POINT('Ctrl Pts',(18.1436123520193,56.09703620615,2.65877670944818));
#243343=CARTESIAN_POINT('Ctrl Pts',(18.1777307632123,56.1599674935334,2.65878198860301));
#243344=CARTESIAN_POINT('Ctrl Pts',(18.1930767435948,56.0417604764385,2.59908173516063));
#243345=CARTESIAN_POINT('Ctrl Pts',(18.2045954185344,56.0772424804486,2.65878198860301));
#243346=CARTESIAN_POINT('Ctrl Pts',(18.2263320786581,56.144199857553,2.65878198860301));
#243347=CARTESIAN_POINT('Origin',(18.2263320786581,56.144199857553,2.53178198860301));
#243348=CARTESIAN_POINT('Ctrl Pts',(19.42073522007,58.7434254837934,3.77003198860304));
#243349=CARTESIAN_POINT('Ctrl Pts',(19.2997705861191,58.7827292759117,3.77003198860304));
#243350=CARTESIAN_POINT('Ctrl Pts',(19.2999511771037,58.7826705983438,3.64284238727658));
#243351=CARTESIAN_POINT('Ctrl Pts',(19.4879965013588,58.9497137831224,3.77003198860305));
#243352=CARTESIAN_POINT('Ctrl Pts',(19.366877128552,58.9892635895157,3.77025506105909));
#243353=CARTESIAN_POINT('Ctrl Pts',(19.3535710010443,58.9476954469493,3.64284210642029));
#243354=CARTESIAN_POINT('Ctrl Pts',(19.5520260773861,59.1460976215389,3.65553527987872));
#243355=CARTESIAN_POINT('Ctrl Pts',(19.4307447900789,59.1858295778046,3.65585996533));
#243356=CARTESIAN_POINT('Ctrl Pts',(19.4046161500178,59.104796260842,3.55127902710136));
#243357=CARTESIAN_POINT('Ctrl Pts',(19.5876674457077,59.2554138597574,3.47153072139113));
#243358=CARTESIAN_POINT('Ctrl Pts',(19.4663243070093,59.2953329133627,3.4718232790523));
#243359=CARTESIAN_POINT('Ctrl Pts',(19.4330302514113,59.1922458725047,3.40413028378039));
#243360=CARTESIAN_POINT('Origin',(19.42073522007,58.7434254837934,3.64303198860304));
#243361=CARTESIAN_POINT('Origin',(5.68280300381509E-15,1.86380513208053E-13,
2.53178198860262));
#243362=CARTESIAN_POINT('Origin',(18.2553202812748,56.1347810195644,2.53178198860301));
#243363=CARTESIAN_POINT('Origin',(6.24367625034007,18.1886080242679,3.64303198860275));
#243364=CARTESIAN_POINT('Origin',(19.2967593024483,58.3616995707169,3.64299466007272));
#243365=CARTESIAN_POINT('Ctrl Pts',(18.2220120550216,56.0323588238393,2.59908173516063));
#243366=CARTESIAN_POINT('Ctrl Pts',(18.2335490499217,56.0678348753335,2.65878198860301));
#243367=CARTESIAN_POINT('Ctrl Pts',(18.2553202812748,56.1347810195644,2.65878198860301));
#243368=CARTESIAN_POINT('Ctrl Pts',(18.3053742463598,56.0052491386471,2.59908193200014));
#243369=CARTESIAN_POINT('Ctrl Pts',(18.2942806848333,56.0480812627894,2.65877685806711));
#243370=CARTESIAN_POINT('Ctrl Pts',(18.3037418885569,56.1190241739995,2.65878198860301));
#243371=CARTESIAN_POINT('Ctrl Pts',(18.3900709842071,56.0035251343647,2.63872492669841));
#243372=CARTESIAN_POINT('Ctrl Pts',(18.3574039607304,56.0514568378825,2.69532212015323));
#243373=CARTESIAN_POINT('Ctrl Pts',(18.356118560324,56.1278011372721,2.68176836726683));
#243374=CARTESIAN_POINT('Ctrl Pts',(18.5134377270388,56.0390077039671,2.75442176402285));
#243375=CARTESIAN_POINT('Ctrl Pts',(18.4363968713618,56.089193446234,2.79203179920166));
#243376=CARTESIAN_POINT('Ctrl Pts',(18.4370884086014,56.1770584756122,2.74885310748205));
#243377=CARTESIAN_POINT('Ctrl Pts',(18.5530236652641,56.0747542753111,2.82866089558444));
#243378=CARTESIAN_POINT('Ctrl Pts',(18.4521491348401,56.1242585025252,2.85316563119344));
#243379=CARTESIAN_POINT('Ctrl Pts',(18.4660698759072,56.2162483036944,2.79189751796711));
#243380=CARTESIAN_POINT('Ctrl Pts',(18.5670586829464,56.117947944099,2.90134173516062));
#243381=CARTESIAN_POINT('Ctrl Pts',(18.4469743395778,56.1574782858999,2.90103711553269));
#243382=CARTESIAN_POINT('Ctrl Pts',(18.4801050014189,56.2594439784241,2.83404198860301));
#243383=CARTESIAN_POINT('Origin',(18.6008891789884,56.2201988201385,2.83404198860301));
#243384=CARTESIAN_POINT('Origin',(19.2830435998982,58.3196542512025,3.56647653971879));
#243385=CARTESIAN_POINT('Origin',(19.2577541638577,58.2418213702176,3.42473028058526));
#243386=CARTESIAN_POINT('Origin',(18.6559403576614,56.3896289265331,3.1191364816817));
#243387=CARTESIAN_POINT('Origin',(18.7109915363516,56.5590590327992,3.4042309748335));
#243388=CARTESIAN_POINT('Ctrl Pts',(19.1557908785624,57.9280106456678,3.36123028058522));
#243389=CARTESIAN_POINT('Ctrl Pts',(19.0350067009929,57.9672558039534,3.36123028058522));
#243390=CARTESIAN_POINT('Ctrl Pts',(19.0350067009929,57.9672558039534,3.23423028058522));
#243391=CARTESIAN_POINT('Ctrl Pts',(19.1833829156708,58.0136880650214,3.36123028058522));
#243392=CARTESIAN_POINT('Ctrl Pts',(19.0627953474453,58.0527804636623,3.36099641108519));
#243393=CARTESIAN_POINT('Ctrl Pts',(19.0767283413219,58.0956618095378,3.23423043688451));
#243394=CARTESIAN_POINT('Ctrl Pts',(19.2094750027316,58.0947019536608,3.41054258905325));
#243395=CARTESIAN_POINT('Ctrl Pts',(19.0892026680436,58.1340538395318,3.41008815826041));
#243396=CARTESIAN_POINT('Ctrl Pts',(19.1161791203813,58.2170788227779,3.30819867304298));
#243397=CARTESIAN_POINT('Ctrl Pts',(19.2232259141438,58.1373965169896,3.48823028058524));
#243398=CARTESIAN_POINT('Ctrl Pts',(19.1031347997386,58.1769325318822,3.4879469194164));
#243399=CARTESIAN_POINT('Ctrl Pts',(19.1369699862882,58.2810665285032,3.42473028058525));
#243400=CARTESIAN_POINT('Origin',(19.1557908785624,57.9280106456678,3.23423028058522));
#243401=CARTESIAN_POINT('Ctrl Pts',(18.6771643191709,56.4568070719813,3.47153072139112));
#243402=CARTESIAN_POINT('Ctrl Pts',(18.556896315972,56.496394798308,3.47122746285117));
#243403=CARTESIAN_POINT('Ctrl Pts',(18.5902571970799,56.5984571192853,3.40413046676847));
#243404=CARTESIAN_POINT('Ctrl Pts',(18.7128129802638,56.5661228951886,3.65553813458026));
#243405=CARTESIAN_POINT('Ctrl Pts',(18.5923766197464,56.605592832572,3.65520336072198));
#243406=CARTESIAN_POINT('Ctrl Pts',(18.6186718120051,56.6859083114086,3.551281345199));
#243407=CARTESIAN_POINT('Ctrl Pts',(18.7768537015931,56.762504971004,3.77003198860303));
#243408=CARTESIAN_POINT('Ctrl Pts',(18.6561664154735,56.8019192501356,3.76980209314125));
#243409=CARTESIAN_POINT('Ctrl Pts',(18.669717390011,56.8430104456825,3.64284195387498));
#243410=CARTESIAN_POINT('Ctrl Pts',(18.8441205405518,56.9687879773468,3.77003198860303));
#243411=CARTESIAN_POINT('Ctrl Pts',(18.7231554368011,57.0080919221123,3.77003198860303));
#243412=CARTESIAN_POINT('Ctrl Pts',(18.7233364982868,57.0080330916693,3.64284189403878));
#243413=CARTESIAN_POINT('Origin',(18.8441205405518,56.9687879773468,3.64303198860303));
#243414=CARTESIAN_POINT('Origin',(6.09975091006187,17.7456513739113,3.23423028058494));
#243415=CARTESIAN_POINT('Origin',(19.1090650011314,57.7842031819385,3.23423028058522));
#243416=CARTESIAN_POINT('Origin',(6.07721283595898,17.6762863142852,3.64303198860275));
#243417=CARTESIAN_POINT('Origin',(18.9681964166833,57.3504898524409,3.64299171721779));
#243418=CARTESIAN_POINT('Ctrl Pts',(19.0416371860877,57.5748148483578,3.48823028058521));
#243419=CARTESIAN_POINT('Ctrl Pts',(18.9204594407744,57.6147155869504,3.48852004212298));
#243420=CARTESIAN_POINT('Ctrl Pts',(18.8863175164091,57.5096375484039,3.42473028058521));
#243421=CARTESIAN_POINT('Ctrl Pts',(19.055431886255,57.6176546016067,3.41028005848447));
#243422=CARTESIAN_POINT('Ctrl Pts',(18.9342932580184,57.6572916985394,3.41074404220401));
#243423=CARTESIAN_POINT('Ctrl Pts',(18.9071786451787,57.573841500985,3.30780486243988));
#243424=CARTESIAN_POINT('Ctrl Pts',(19.0815664505365,57.6988141606861,3.36123028058522));
#243425=CARTESIAN_POINT('Ctrl Pts',(18.9605330155752,57.7380493683874,3.36146460586551));
#243426=CARTESIAN_POINT('Ctrl Pts',(18.9466997135531,57.6954748424925,3.23423045308519));
#243427=CARTESIAN_POINT('Ctrl Pts',(19.1090650011314,57.7842031819385,3.36123028058522));
#243428=CARTESIAN_POINT('Ctrl Pts',(18.9882808235619,57.8234483402241,3.36123028058521));
#243429=CARTESIAN_POINT('Ctrl Pts',(18.9882808235619,57.8234483402241,3.23423028058522));
#243430=CARTESIAN_POINT('Origin',(19.0071016939786,57.4703923901183,3.42473028058521));
#243431=CARTESIAN_POINT('Origin',(18.9819630792876,57.3930236885637,3.5656311352486));
#243432=CARTESIAN_POINT('Origin',(12.4602215063116,60.1478239224139,3.5664765390944));
#243433=CARTESIAN_POINT('Origin',(12.4693660187271,60.1910940874977,3.6429946600763));
#243434=CARTESIAN_POINT('Origin',(12.443206359372,60.0677739512128,3.42473028058526));
#243435=CARTESIAN_POINT('Ctrl Pts',(12.4208962741585,59.9600752506739,3.48823028058526));
#243436=CARTESIAN_POINT('Ctrl Pts',(12.5446662374485,59.9342688867327,3.48794691941642));
#243437=CARTESIAN_POINT('Ctrl Pts',(12.5674311046652,60.0413691664789,3.42473028058527));
#243438=CARTESIAN_POINT('Ctrl Pts',(12.4114257351941,59.9160770362137,3.4102800592513));
#243439=CARTESIAN_POINT('Ctrl Pts',(12.5352608058697,59.8900198101371,3.40982512230947));
#243440=CARTESIAN_POINT('Ctrl Pts',(12.5533954010692,59.9753363727331,3.30780486372805));
#243441=CARTESIAN_POINT('Ctrl Pts',(12.393483289627,59.8327226933131,3.36123028058523));
#243442=CARTESIAN_POINT('Ctrl Pts',(12.5174621766264,59.806283843088,3.360997210486));
#243443=CARTESIAN_POINT('Ctrl Pts',(12.5268049860494,59.8502383056079,3.23423045308477));
#243444=CARTESIAN_POINT('Ctrl Pts',(12.3746037924162,59.745024249125,3.36123028058523));
#243445=CARTESIAN_POINT('Ctrl Pts',(12.4988285377094,59.7186194643911,3.36123028058523));
#243446=CARTESIAN_POINT('Ctrl Pts',(12.4988285377094,59.7186194643911,3.23423028058523));
#243447=CARTESIAN_POINT('Origin',(12.3746037924162,59.745024249125,3.23423028058523));
#243448=CARTESIAN_POINT('Origin',(-0.310561863232978,0.0660119618348215,
3.64303198860263));
#243449=CARTESIAN_POINT('Origin',(12.5528626811445,60.5836663843184,3.64303198860305));
#243450=CARTESIAN_POINT('Origin',(-0.310561863232978,0.0660119618348243,
3.23423028058481));
#243451=CARTESIAN_POINT('Origin',(12.3431658574209,59.5971203935661,3.23423028058523));
#243452=CARTESIAN_POINT('Ctrl Pts',(12.664289321014,61.1105274371643,3.47153072139115));
#243453=CARTESIAN_POINT('Ctrl Pts',(12.7893350777084,61.0844267845858,3.47182327902705));
#243454=CARTESIAN_POINT('Ctrl Pts',(12.7666250679676,60.9785037674411,3.40413028959073));
#243455=CARTESIAN_POINT('Ctrl Pts',(12.6404971713776,60.9980344071778,3.65553807121));
#243456=CARTESIAN_POINT('Ctrl Pts',(12.7653958126153,60.9718026486719,3.65586275496976));
#243457=CARTESIAN_POINT('Ctrl Pts',(12.7475073053531,60.8885617651958,3.55128126837296));
#243458=CARTESIAN_POINT('Ctrl Pts',(12.5977561540106,60.795944629793,3.77003198860306));
#243459=CARTESIAN_POINT('Ctrl Pts',(12.7224234952036,60.769636075915,3.77025505748515));
#243460=CARTESIAN_POINT('Ctrl Pts',(12.713163022104,60.7269846150103,3.64284211731234));
#243461=CARTESIAN_POINT('Ctrl Pts',(12.5528626811445,60.5836663843184,3.77003198860306));
#243462=CARTESIAN_POINT('Ctrl Pts',(12.6772730124468,60.5572221520606,3.77003198860306));
#243463=CARTESIAN_POINT('Ctrl Pts',(12.6770872880162,60.5572616290069,3.64284239821747));
#243464=CARTESIAN_POINT('Origin',(12.642433962084,61.0050661295708,3.40423097483353));
#243465=CARTESIAN_POINT('Ctrl Pts',(12.3431658574209,59.5971203935661,3.36123028058523));
#243466=CARTESIAN_POINT('Ctrl Pts',(12.4673906027141,59.5707156088323,3.36123028058523));
#243467=CARTESIAN_POINT('Ctrl Pts',(12.4673906027141,59.5707156088323,3.23423028058523));
#243468=CARTESIAN_POINT('Ctrl Pts',(12.3242219811461,59.5091256622729,3.36123028058523));
#243469=CARTESIAN_POINT('Ctrl Pts',(12.4486583679642,59.4825873732132,3.36146538610137));
#243470=CARTESIAN_POINT('Ctrl Pts',(12.4393195978193,59.4386519140009,3.23423043688482));
#243471=CARTESIAN_POINT('Ctrl Pts',(12.3063073021293,59.4259203549058,3.41054258693141));
#243472=CARTESIAN_POINT('Ctrl Pts',(12.4310355281324,59.399678430328,3.41100608859797));
#243473=CARTESIAN_POINT('Ctrl Pts',(12.4127764613285,59.3137762748663,3.30819866970841));
#243474=CARTESIAN_POINT('Ctrl Pts',(12.2968658913801,59.3820708699073,3.48823028058522));
#243475=CARTESIAN_POINT('Ctrl Pts',(12.4217592664911,59.3560370505016,3.48852004212301));
#243476=CARTESIAN_POINT('Ctrl Pts',(12.3987880210522,59.2479658375578,3.42473028058522));
#243477=CARTESIAN_POINT('Origin',(12.274563275759,59.2743706222917,3.42473028058521));
#243478=CARTESIAN_POINT('Origin',(12.6794732450923,61.1793222555443,3.11913648178318));
#243479=CARTESIAN_POINT('Origin',(12.7165125280164,61.3535783813234,2.83404198860304));
#243480=CARTESIAN_POINT('Origin',(12.2576496039892,59.1947980527949,3.56563113460905));
#243481=CARTESIAN_POINT('Origin',(12.2483049653996,59.1510793400373,3.64299171721803));
#243482=CARTESIAN_POINT('Ctrl Pts',(13.0739701745323,61.58161970227,2.59908173516066));
#243483=CARTESIAN_POINT('Ctrl Pts',(13.0662229071065,61.5451281645061,2.65878198860305));
#243484=CARTESIAN_POINT('Ctrl Pts',(13.0516031943527,61.4762657165318,2.65878198860305));
#243485=CARTESIAN_POINT('Ctrl Pts',(12.9877758510419,61.5999188988205,2.59908193475586));
#243486=CARTESIAN_POINT('Ctrl Pts',(13.0034370926712,61.55845448937,2.65878715325448));
#243487=CARTESIAN_POINT('Ctrl Pts',(13.0017087032042,61.4868491822359,2.65878198860305));
#243488=CARTESIAN_POINT('Ctrl Pts',(12.9030451317659,61.5923336062398,2.63878778849915));
#243489=CARTESIAN_POINT('Ctrl Pts',(12.9408103617799,61.5481051179918,2.69564460180149));
#243490=CARTESIAN_POINT('Ctrl Pts',(12.9504709278438,61.4721451382827,2.68180481624929));
#243491=CARTESIAN_POINT('Ctrl Pts',(12.7836101409429,61.543429955208,2.75443238878687));
#243492=CARTESIAN_POINT('Ctrl Pts',(12.8662000075465,61.5018471007597,2.79268340777146));
#243493=CARTESIAN_POINT('Ctrl Pts',(12.8749747009097,61.4139027244672,2.7488592683565));
#243494=CARTESIAN_POINT('Ctrl Pts',(12.7478263086954,61.5035207735038,2.82856655361713));
#243495=CARTESIAN_POINT('Ctrl Pts',(12.8544221781243,61.4652971063428,2.85384197230755));
#243496=CARTESIAN_POINT('Ctrl Pts',(12.8501918100168,61.3716536946531,2.79184624278469));
#243497=CARTESIAN_POINT('Ctrl Pts',(12.7383709431249,61.4590390555211,2.90134173516067));
#243498=CARTESIAN_POINT('Ctrl Pts',(12.8632261535953,61.4329754599101,2.90163218716434));
#243499=CARTESIAN_POINT('Ctrl Pts',(12.8407372733096,61.3271735965896,2.83404198860305));
#243500=CARTESIAN_POINT('Origin',(13.0516031943527,61.4762657165318,2.53178198860305));
#243501=CARTESIAN_POINT('Origin',(-0.310561863232978,0.0660119618348215,
3.64303198860263));
#243502=CARTESIAN_POINT('Origin',(12.164906888579,58.7584778814679,3.64303198860303));
#243503=CARTESIAN_POINT('Origin',(5.63039444364742E-15,1.85721263801678E-13,
2.53178198860262));
#243504=CARTESIAN_POINT('Origin',(13.0814171332231,61.4699285681957,2.53178198860305));
#243505=CARTESIAN_POINT('Ctrl Pts',(12.164906888579,58.7584778814679,3.77003198860304));
#243506=CARTESIAN_POINT('Ctrl Pts',(12.2893177281505,58.7320335411741,3.77003198860304));
#243507=CARTESIAN_POINT('Ctrl Pts',(12.289131494692,58.7320731263177,3.64284187937058));
#243508=CARTESIAN_POINT('Ctrl Pts',(12.1200194799684,58.5461948427483,3.77003198860304));
#243509=CARTESIAN_POINT('Ctrl Pts',(12.244244887697,58.5199849720738,3.76980208962962));
#243510=CARTESIAN_POINT('Ctrl Pts',(12.2530551225943,58.5623471386693,3.64284193928367));
#243511=CARTESIAN_POINT('Ctrl Pts',(12.0772896710124,58.3441042111269,3.65553535416629));
#243512=CARTESIAN_POINT('Ctrl Pts',(12.2013256001486,58.3180679977585,3.65520057834544));
#243513=CARTESIAN_POINT('Ctrl Pts',(12.2187110949215,58.4007711908097,3.5512791096424));
#243514=CARTESIAN_POINT('Ctrl Pts',(12.053504764932,58.2316113004783,3.47153072139112));
#243515=CARTESIAN_POINT('Ctrl Pts',(12.1774537884115,58.2057612725769,3.47122746281622));
#243516=CARTESIAN_POINT('Ctrl Pts',(12.1995935666436,58.3108302909898,3.40413045901298));
#243517=CARTESIAN_POINT('Origin',(12.0753355159231,58.3370777047237,3.40423097483351));
#243518=CARTESIAN_POINT('Ctrl Pts',(13.3605623192485,61.3267881959115,2.90134173516067));
#243519=CARTESIAN_POINT('Ctrl Pts',(13.2359003894749,61.3537611057085,2.90163218716434));
#243520=CARTESIAN_POINT('Ctrl Pts',(13.2134115091892,61.247959242388,2.83404198860305));
#243521=CARTESIAN_POINT('Ctrl Pts',(13.3700210384233,61.3712903180782,2.82853349835398));
#243522=CARTESIAN_POINT('Ctrl Pts',(13.2571016411965,61.3797222373777,2.85381483162378));
#243523=CARTESIAN_POINT('Ctrl Pts',(13.2228703539492,61.2924596082468,2.79182701594254));
#243524=CARTESIAN_POINT('Ctrl Pts',(13.3535190881771,61.4221282572892,2.75468822073686));
#243525=CARTESIAN_POINT('Ctrl Pts',(13.2610999767702,61.4177900459395,2.79286913083897));
#243526=CARTESIAN_POINT('Ctrl Pts',(13.2173727427873,61.3409599630867,2.74900763297962));
#243527=CARTESIAN_POINT('Ctrl Pts',(13.2651598666398,61.5148770953651,2.63954450640435));
#243528=CARTESIAN_POINT('Ctrl Pts',(13.2123479779269,61.4899829268156,2.69627684028887));
#243529=CARTESIAN_POINT('Ctrl Pts',(13.1725625528867,61.4244514636298,2.68224356036528));
#243530=CARTESIAN_POINT('Ctrl Pts',(13.1903059833735,61.5568698122757,2.59908178706413));
#243531=CARTESIAN_POINT('Ctrl Pts',(13.1590895168685,61.5253695547374,2.65878704321587));
#243532=CARTESIAN_POINT('Ctrl Pts',(13.1314678292776,61.4592680512445,2.65878198860305));
#243533=CARTESIAN_POINT('Ctrl Pts',(13.1038352065726,61.5752716937454,2.59908173516066));
#243534=CARTESIAN_POINT('Ctrl Pts',(13.0960702419678,61.538783917633,2.65878198860304));
#243535=CARTESIAN_POINT('Ctrl Pts',(13.0814171332231,61.4699285681957,2.65878198860305));
#243536=CARTESIAN_POINT('Origin',(13.3376362544824,61.2215544576541,2.83404198860303));
#243537=CARTESIAN_POINT('Origin',(12.0382961820467,58.1628213392049,3.11913648166998));
#243538=CARTESIAN_POINT('Origin',(12.0012568480858,57.9885649735462,2.83404198860302));
#243539=CARTESIAN_POINT('Origin',(13.3005969715131,61.0472983318734,3.11913648177627));
#243540=CARTESIAN_POINT('Origin',(13.26355768855,60.8730422059016,3.40423097483353));
#243541=CARTESIAN_POINT('Ctrl Pts',(11.9794294790611,57.8830978693158,2.90134173516064));
#243542=CARTESIAN_POINT('Ctrl Pts',(12.1031907419155,57.8572899778513,2.9010371155327));
#243543=CARTESIAN_POINT('Ctrl Pts',(12.125481593379,57.9621601888123,2.83404198860303));
#243544=CARTESIAN_POINT('Ctrl Pts',(11.9699833161086,57.8386546085358,2.82862991747999));
#243545=CARTESIAN_POINT('Ctrl Pts',(12.0820882677179,57.8310944294269,2.85314045886453));
#243546=CARTESIAN_POINT('Ctrl Pts',(12.1160345187366,57.9177151970034,2.79187960999944));
#243547=CARTESIAN_POINT('Ctrl Pts',(11.9864204851029,57.7880992891177,2.75470625793369));
#243548=CARTESIAN_POINT('Ctrl Pts',(12.0782959991609,57.7929810340976,2.79224250381943));
#243549=CARTESIAN_POINT('Ctrl Pts',(12.1215717318493,57.8694789541067,2.74901809108301));
#243550=CARTESIAN_POINT('Ctrl Pts',(12.0746725352387,57.6961636462599,2.63947868311736));
#243551=CARTESIAN_POINT('Ctrl Pts',(12.127248449038,57.7211944343231,2.69595066767949));
#243552=CARTESIAN_POINT('Ctrl Pts',(12.1665991704024,57.7867317752134,2.68220539436099));
#243553=CARTESIAN_POINT('Ctrl Pts',(12.1494120604582,57.6547178110654,2.59908178585209));
#243554=CARTESIAN_POINT('Ctrl Pts',(12.1804827566586,57.6862546895637,2.65877670944884));
#243555=CARTESIAN_POINT('Ctrl Pts',(12.2078361528635,57.7524075778605,2.65878198860302));
#243556=CARTESIAN_POINT('Ctrl Pts',(12.2354540642043,57.6364522029209,2.59908173516064));
#243557=CARTESIAN_POINT('Ctrl Pts',(12.2432007592846,57.6729438621908,2.65878198860302));
#243558=CARTESIAN_POINT('Ctrl Pts',(12.2578193919766,57.7418065394568,2.65878198860302));
#243559=CARTESIAN_POINT('Origin',(12.2578193919766,57.7418065394568,2.53178198860302));
#243560=CARTESIAN_POINT('Ctrl Pts',(13.1739864076105,60.4516424606491,3.77003198860306));
#243561=CARTESIAN_POINT('Ctrl Pts',(13.0495760655906,60.478086695185,3.77003198860305));
#243562=CARTESIAN_POINT('Ctrl Pts',(13.0497618007548,60.4780472159572,3.64284238727674));
#243563=CARTESIAN_POINT('Ctrl Pts',(13.2193162256457,60.6638314094602,3.77003198860306));
#243564=CARTESIAN_POINT('Ctrl Pts',(13.0947262769519,60.6905041359632,3.77025506105868));
#243565=CARTESIAN_POINT('Ctrl Pts',(13.0858380958638,60.6477728389727,3.64284210641966));
#243566=CARTESIAN_POINT('Ctrl Pts',(13.2624673401133,60.8658323498481,3.65553527987878));
#243567=CARTESIAN_POINT('Ctrl Pts',(13.1376973240562,60.8926693037166,3.65585996533079));
#243568=CARTESIAN_POINT('Ctrl Pts',(13.1201821075159,60.8093487091478,3.55127902710192));
#243569=CARTESIAN_POINT('Ctrl Pts',(13.2864868028994,60.978275279735,3.47153072139115));
#243570=CARTESIAN_POINT('Ctrl Pts',(13.1616357172828,61.0052918407717,3.47182327905231));
#243571=CARTESIAN_POINT('Ctrl Pts',(13.1392995799685,60.8992893450422,3.40413028378048));
#243572=CARTESIAN_POINT('Origin',(13.1739864076105,60.4516424606491,3.64303198860306));
#243573=CARTESIAN_POINT('Origin',(5.67687244506386E-15,1.86382102296481E-13,
2.53178198860262));
#243574=CARTESIAN_POINT('Origin',(12.2876333308469,57.7354693911207,2.53178198860302));
#243575=CARTESIAN_POINT('Origin',(3.00026883051124,12.588064422097,3.64303198860271));
#243576=CARTESIAN_POINT('Origin',(13.0905908661193,60.059048669913,3.64299466007489));
#243577=CARTESIAN_POINT('Ctrl Pts',(12.2652136052659,57.630126617196,2.59908173516064));
#243578=CARTESIAN_POINT('Ctrl Pts',(12.2729791421553,57.6666142715157,2.65878198860302));
#243579=CARTESIAN_POINT('Ctrl Pts',(12.2876333308469,57.7354693911207,2.65878198860302));
#243580=CARTESIAN_POINT('Ctrl Pts',(12.3509528635304,57.6118791634506,2.59908193199958));
#243581=CARTESIAN_POINT('Ctrl Pts',(12.3354428975797,57.6533170557974,2.65877685806754));
#243582=CARTESIAN_POINT('Ctrl Pts',(12.3374367183508,57.7248602994024,2.65878198860302));
#243583=CARTESIAN_POINT('Ctrl Pts',(12.4353658313041,57.6190178232952,2.63872492669831));
#243584=CARTESIAN_POINT('Ctrl Pts',(12.3978675338896,57.6632723181626,2.69532212015325));
#243585=CARTESIAN_POINT('Ctrl Pts',(12.3886090227466,57.739064034563,2.68176836726674));
#243586=CARTESIAN_POINT('Ctrl Pts',(12.5543478197373,57.6672013517155,2.75442176402297));
#243587=CARTESIAN_POINT('Ctrl Pts',(12.4724831634114,57.7090592089824,2.7920317992016));
#243588=CARTESIAN_POINT('Ctrl Pts',(12.463986515842,57.796515189861,2.74885310748216));
#243589=CARTESIAN_POINT('Ctrl Pts',(12.5899803678813,57.706889956891,2.82866089558436));
#243590=CARTESIAN_POINT('Ctrl Pts',(12.484483837894,57.7455787351211,2.85316563119316));
#243591=CARTESIAN_POINT('Ctrl Pts',(12.4887127671322,57.8385197202054,2.79189751796709));
#243592=CARTESIAN_POINT('Ctrl Pts',(12.599423532447,57.7513140650722,2.90134173516062));
#243593=CARTESIAN_POINT('Ctrl Pts',(12.4758649777951,57.7780756236498,2.90103711553269));
#243594=CARTESIAN_POINT('Ctrl Pts',(12.4981558292586,57.8829458346107,2.83404198860301));
#243595=CARTESIAN_POINT('Origin',(12.6223805745518,57.8565410498769,2.83404198860302));
#243596=CARTESIAN_POINT('Origin',(13.0813452322622,60.0157999977499,3.56647653971802));
#243597=CARTESIAN_POINT('Origin',(13.064330085838,59.9357500275435,3.42473028058526));
#243598=CARTESIAN_POINT('Origin',(12.6594199084546,58.0307974155296,3.11913648168123));
#243599=CARTESIAN_POINT('Origin',(12.6964592423891,58.2050537810544,3.40423097483351));
#243600=CARTESIAN_POINT('Ctrl Pts',(12.9957275188822,59.6130003254557,3.36123028058523));
#243601=CARTESIAN_POINT('Ctrl Pts',(12.871502773589,59.6394051101896,3.36123028058523));
#243602=CARTESIAN_POINT('Ctrl Pts',(12.871502773589,59.6394051101896,3.23423028058523));
#243603=CARTESIAN_POINT('Ctrl Pts',(13.0142126749434,59.7010925481787,3.36123028058523));
#243604=CARTESIAN_POINT('Ctrl Pts',(12.8901994296778,59.7273659613729,3.36099641108525));
#243605=CARTESIAN_POINT('Ctrl Pts',(12.8995737759687,59.7714687931883,3.2342304368846));
#243606=CARTESIAN_POINT('Ctrl Pts',(13.0316935695382,59.7843900000234,3.41054258905324));
#243607=CARTESIAN_POINT('Ctrl Pts',(12.9079667071289,59.8109544298286,3.41008815826004));
#243608=CARTESIAN_POINT('Ctrl Pts',(12.9261169057243,59.8963444006364,3.30819867304273));
#243609=CARTESIAN_POINT('Ctrl Pts',(13.0409063549237,59.8282880397057,3.48823028058525));
#243610=CARTESIAN_POINT('Ctrl Pts',(12.9173404733281,59.8550545325311,3.48794691941641));
#243611=CARTESIAN_POINT('Ctrl Pts',(12.9401053405448,59.9621548122774,3.42473028058526));
#243612=CARTESIAN_POINT('Origin',(12.9957275188822,59.6130003254557,3.23423028058523));
#243613=CARTESIAN_POINT('Ctrl Pts',(12.6735055745739,58.0998260601482,3.47153072139113));
#243614=CARTESIAN_POINT('Ctrl Pts',(12.5497583678832,58.1266254912132,3.47122746285118));
#243615=CARTESIAN_POINT('Ctrl Pts',(12.5722680770245,58.2316158657528,3.40413046676845));
#243616=CARTESIAN_POINT('Ctrl Pts',(12.6975323335625,58.2122693395992,3.65553813458025));
#243617=CARTESIAN_POINT('Ctrl Pts',(12.5736300041264,58.2389340288484,3.65520336072215));
#243618=CARTESIAN_POINT('Ctrl Pts',(12.5913858949922,58.3215581271264,3.55128134519927));
#243619=CARTESIAN_POINT('Ctrl Pts',(12.7406947165202,58.4142696920428,3.77003198860304));
#243620=CARTESIAN_POINT('Ctrl Pts',(12.6165486539543,58.4408527990764,3.76980209314164));
#243621=CARTESIAN_POINT('Ctrl Pts',(12.6257301953096,58.4831353552992,3.6428419538751));
#243622=CARTESIAN_POINT('Ctrl Pts',(12.786030615045,58.6264539577986,3.77003198860304));
#243623=CARTESIAN_POINT('Ctrl Pts',(12.6616197898427,58.6528982950381,3.77003198860304));
#243624=CARTESIAN_POINT('Ctrl Pts',(12.6618060089105,58.6528587129534,3.64284189403875));
#243625=CARTESIAN_POINT('Origin',(12.786030615045,58.6264539577986,3.64303198860304));
#243626=CARTESIAN_POINT('Origin',(2.93511643966546,12.2815465224194,3.2342302805849));
#243627=CARTESIAN_POINT('Origin',(12.9642895838869,59.4650964698968,3.23423028058523));
#243628=CARTESIAN_POINT('Origin',(2.92491386234291,12.2335471699534,3.64303198860271));
#243629=CARTESIAN_POINT('Origin',(12.8695280801142,59.0190342907438,3.64299171721836));
#243630=CARTESIAN_POINT('Ctrl Pts',(12.9191181862044,59.2498070616281,3.48823028058522));
#243631=CARTESIAN_POINT('Ctrl Pts',(12.7944335023706,59.2768226963,3.488520042123));
#243632=CARTESIAN_POINT('Ctrl Pts',(12.7714622569318,59.1687514833563,3.42473028058522));
#243633=CARTESIAN_POINT('Ctrl Pts',(12.9283593439854,59.2938540730364,3.4102800584845));
#243634=CARTESIAN_POINT('Ctrl Pts',(12.8037411209988,59.3206115991505,3.41074404220436));
#243635=CARTESIAN_POINT('Ctrl Pts',(12.7854979657562,59.2347843016993,3.30780486244024));
#243636=CARTESIAN_POINT('Ctrl Pts',(12.9458672564001,59.3773008374016,3.36123028058523));
#243637=CARTESIAN_POINT('Ctrl Pts',(12.8213956592925,59.4036696715712,3.36146460586425));
#243638=CARTESIAN_POINT('Ctrl Pts',(12.8120883873131,59.3598823995799,3.23423045308459));
#243639=CARTESIAN_POINT('Ctrl Pts',(12.9642895838869,59.4650964698969,3.36123028058523));
#243640=CARTESIAN_POINT('Ctrl Pts',(12.8400648385937,59.4915012546307,3.36123028058523));
#243641=CARTESIAN_POINT('Ctrl Pts',(12.8400648385937,59.4915012546307,3.23423028058523));
#243642=CARTESIAN_POINT('Origin',(12.895687002225,59.1423466986224,3.42473028058522));
#243643=CARTESIAN_POINT('Origin',(12.8787733309736,59.0627741301473,3.56563113524825));
#243644=CARTESIAN_POINT('Origin',(6.1048035056639,61.1207756556243,3.56647653909506));
#243645=CARTESIAN_POINT('Origin',(6.10937495961997,61.1647646440472,3.64299466007747));
#243646=CARTESIAN_POINT('Origin',(6.09624906995219,61.0393856393806,3.42473028058526));
#243647=CARTESIAN_POINT('Ctrl Pts',(6.08531878138301,60.9299448846692,3.48823028058527));
#243648=CARTESIAN_POINT('Ctrl Pts',(6.21110821942915,60.9172173747512,3.48794691941643));
#243649=CARTESIAN_POINT('Ctrl Pts',(6.22255335066396,61.0261105245456,3.42473028058528));
#243650=CARTESIAN_POINT('Ctrl Pts',(6.08049918876605,60.8851977561472,3.4102800592513));
#243651=CARTESIAN_POINT('Ctrl Pts',(6.20637959976662,60.8722275639182,3.40982512230992));
#243652=CARTESIAN_POINT('Ctrl Pts',(6.21549684257615,60.958972334824,3.3078048637285));
#243653=CARTESIAN_POINT('Ctrl Pts',(6.07136793516312,60.8004245407961,3.36123028058523));
#243654=CARTESIAN_POINT('Ctrl Pts',(6.19743126523161,60.7870898478944,3.36099721048525));
#243655=CARTESIAN_POINT('Ctrl Pts',(6.2021284013467,60.8317801127822,3.23423045308461));
#243656=CARTESIAN_POINT('Ctrl Pts',(6.0617588454155,60.7112330730306,3.36123028058524));
#243657=CARTESIAN_POINT('Ctrl Pts',(6.18806312612727,60.6979579581956,3.36123028058524));
#243658=CARTESIAN_POINT('Ctrl Pts',(6.18806312612727,60.6979579581956,3.23423028058524));
#243659=CARTESIAN_POINT('Origin',(6.0617588454155,60.7112330730306,3.23423028058524));
#243660=CARTESIAN_POINT('Origin',(-0.315760701779421,0.0331877870876628,
3.64303198860263));
#243661=CARTESIAN_POINT('Origin',(6.15137923967656,61.5639141665614,3.64303198860306));
#243662=CARTESIAN_POINT('Origin',(-0.315760701779421,0.0331877870876657,
3.23423028058481));
#243663=CARTESIAN_POINT('Origin',(6.04595329345041,60.5608532912345,3.23423028058524));
#243664=CARTESIAN_POINT('Ctrl Pts',(6.20712349654444,62.0995362748661,3.47153072139115));
#243665=CARTESIAN_POINT('Ctrl Pts',(6.33421250060471,62.0866494451787,3.47182327902705));
#243666=CARTESIAN_POINT('Ctrl Pts',(6.32269886887974,61.9789328429856,3.40413028959051));
#243667=CARTESIAN_POINT('Ctrl Pts',(6.19522040634608,61.9851725366288,3.65553807121));
#243668=CARTESIAN_POINT('Ctrl Pts',(6.3221768051615,61.9721399414754,3.65586275496991));
#243669=CARTESIAN_POINT('Ctrl Pts',(6.31308733464731,61.8874852020943,3.55128126837335));
#243670=CARTESIAN_POINT('Ctrl Pts',(6.17383766261686,61.7797221753255,3.77003198860307));
#243671=CARTESIAN_POINT('Ctrl Pts',(6.30057205577832,61.7665890280519,3.7702550574855));
#243672=CARTESIAN_POINT('Ctrl Pts',(6.29582060418308,61.7232032332899,3.64284211731174));
#243673=CARTESIAN_POINT('Ctrl Pts',(6.15137923967656,61.5639141665614,3.77003198860306));
#243674=CARTESIAN_POINT('Ctrl Pts',(6.2778722131273,61.5506192193204,3.77003198860306));
#243675=CARTESIAN_POINT('Ctrl Pts',(6.27768337964964,61.5506390665186,3.64284239821706));
#243676=CARTESIAN_POINT('Origin',(6.19641157197444,61.9923681882671,3.40423097483353));
#243677=CARTESIAN_POINT('Ctrl Pts',(6.04595329345041,60.5608532912346,3.36123028058524));
#243678=CARTESIAN_POINT('Ctrl Pts',(6.17225757416218,60.5475781763996,3.36123028058524));
#243679=CARTESIAN_POINT('Ctrl Pts',(6.17225757416218,60.5475781763996,3.23423028058524));
#243680=CARTESIAN_POINT('Ctrl Pts',(6.03631114774998,60.471360430011,3.36123028058524));
#243681=CARTESIAN_POINT('Ctrl Pts',(6.16283986559469,60.4579746647638,3.3614653861017));
#243682=CARTESIAN_POINT('Ctrl Pts',(6.15814476024342,60.4133037213019,3.23423043688466));
#243683=CARTESIAN_POINT('Ctrl Pts',(6.02719193013372,60.3867383361561,3.41054258693141));
#243684=CARTESIAN_POINT('Ctrl Pts',(6.15397990991439,60.3736778173775,3.41100608859788));
#243685=CARTESIAN_POINT('Ctrl Pts',(6.14480008849003,60.2863376507181,3.30819866970873));
#243686=CARTESIAN_POINT('Ctrl Pts',(6.02238575970256,60.3421421670677,3.48823028058523));
#243687=CARTESIAN_POINT('Ctrl Pts',(6.14931623097227,60.3293058762214,3.48852004212301));
#243688=CARTESIAN_POINT('Ctrl Pts',(6.13776734223196,60.2194255397047,3.42473028058523));
#243689=CARTESIAN_POINT('Origin',(6.01146306152019,60.2327006545397,3.42473028058523));
#243690=CARTESIAN_POINT('Origin',(6.2150332248564,62.1695413802855,3.11913648178491));
#243691=CARTESIAN_POINT('Origin',(6.23365487766605,62.3467145720971,2.83404198860306));
#243692=CARTESIAN_POINT('Origin',(6.00295964302148,60.1517960317852,3.56563113460852));
#243693=CARTESIAN_POINT('Origin',(5.99823604520098,60.107340034,3.64299171721827));
#243694=CARTESIAN_POINT('Ctrl Pts',(6.56531752495282,62.6108711573008,2.59908173516067));
#243695=CARTESIAN_POINT('Ctrl Pts',(6.56142710223332,62.5737697140404,2.65878198860305));
#243696=CARTESIAN_POINT('Ctrl Pts',(6.55408556365926,62.5037563256537,2.65878198860305));
#243697=CARTESIAN_POINT('Ctrl Pts',(6.47768259609056,62.6200603487597,2.59908193475804));
#243698=CARTESIAN_POINT('Ctrl Pts',(6.49759225479945,62.5804601312001,2.65878715325562));
#243699=CARTESIAN_POINT('Ctrl Pts',(6.50335812634732,62.5090664195359,2.65878198860305));
#243700=CARTESIAN_POINT('Ctrl Pts',(6.39420891953744,62.6036598373292,2.63878778849925));
#243701=CARTESIAN_POINT('Ctrl Pts',(6.43639040357906,62.5636211788261,2.69564460180146));
#243702=CARTESIAN_POINT('Ctrl Pts',(6.45393802800011,62.4890871199582,2.68180481624927));
#243703=CARTESIAN_POINT('Ctrl Pts',(6.28054002958118,62.5425397295637,2.7544323887868));
#243704=CARTESIAN_POINT('Ctrl Pts',(6.36702405212782,62.5098176621802,2.79268340777155));
#243705=CARTESIAN_POINT('Ctrl Pts',(6.38494336730958,62.4232722595961,2.74885926835655));
#243706=CARTESIAN_POINT('Ctrl Pts',(6.24912387034457,62.4991087455378,2.82856655361721));
#243707=CARTESIAN_POINT('Ctrl Pts',(6.35913125763789,62.4722367740494,2.85384197230859));
#243708=CARTESIAN_POINT('Ctrl Pts',(6.36471246584707,62.3786641568876,2.79184624278505));
#243709=CARTESIAN_POINT('Ctrl Pts',(6.24436990788039,62.4538823482277,2.90134173516068));
#243710=CARTESIAN_POINT('Ctrl Pts',(6.3712655360405,62.441012455002,2.90163218716435));
#243711=CARTESIAN_POINT('Ctrl Pts',(6.35995915837782,62.3334394572621,2.83404198860306));
#243712=CARTESIAN_POINT('Origin',(6.55408556365926,62.5037563256537,2.53178198860305));
#243713=CARTESIAN_POINT('Origin',(-0.315760701779421,0.0331877870876628,
3.64303198860263));
#243714=CARTESIAN_POINT('Origin',(5.95633285891191,59.7081718144894,3.64303198860304));
#243715=CARTESIAN_POINT('Origin',(5.64744126194172E-15,1.85718563850903E-13,
2.53178198860262));
#243716=CARTESIAN_POINT('Origin',(6.58439859103008,62.5005702980933,2.53178198860305));
#243717=CARTESIAN_POINT('Ctrl Pts',(5.95633285891191,59.7081718144894,3.77003198860305));
#243718=CARTESIAN_POINT('Ctrl Pts',(6.08282634913973,59.6948768129329,3.77003198860305));
#243719=CARTESIAN_POINT('Ctrl Pts',(6.08263699811363,59.6948967145278,3.64284187937077));
#243720=CARTESIAN_POINT('Ctrl Pts',(5.93388096803625,59.4923596726255,3.77003198860305));
#243721=CARTESIAN_POINT('Ctrl Pts',(6.0601655334876,59.4792784733333,3.76980208962958));
#243722=CARTESIAN_POINT('Ctrl Pts',(6.06449945282239,59.5223294958626,3.64284193928352));
#243723=CARTESIAN_POINT('Ctrl Pts',(5.91250946061108,59.2869096333632,3.6555353541663));
#243724=CARTESIAN_POINT('Ctrl Pts',(6.03858743332218,59.2739813341586,3.65520057834539));
#243725=CARTESIAN_POINT('Ctrl Pts',(6.04723285085753,59.3580487495165,3.55127910964277));
#243726=CARTESIAN_POINT('Ctrl Pts',(5.90061356181238,59.1725467709679,3.47153072139113));
#243727=CARTESIAN_POINT('Ctrl Pts',(6.02658564326405,59.159794553172,3.47122746281623));
#243728=CARTESIAN_POINT('Ctrl Pts',(6.03762143444287,59.266602229504,3.40413045901309));
#243729=CARTESIAN_POINT('Origin',(5.91130048050323,59.2797173540688,3.40423097483352));
#243730=CARTESIAN_POINT('Ctrl Pts',(6.87697683366544,62.3873926810693,2.90134173516067));
#243731=CARTESIAN_POINT('Ctrl Pts',(6.75017837817581,62.401187110497,2.90163218716435));
#243732=CARTESIAN_POINT('Ctrl Pts',(6.73887200051313,62.2936141127571,2.83404198860306));
#243733=CARTESIAN_POINT('Ctrl Pts',(6.88173199854461,62.4326397213344,2.82853349835381));
#243734=CARTESIAN_POINT('Ctrl Pts',(6.76854981002487,62.4292221586341,2.85381483162498));
#243735=CARTESIAN_POINT('Ctrl Pts',(6.74362747387393,62.3388594194642,2.79182701594424));
#243736=CARTESIAN_POINT('Ctrl Pts',(6.86000643604706,62.4814742414947,2.75468822073712));
#243737=CARTESIAN_POINT('Ctrl Pts',(6.76854707276813,62.4674993676284,2.79286913083863));
#243738=CARTESIAN_POINT('Ctrl Pts',(6.73309031164157,62.3865194274376,2.74900763297951));
#243739=CARTESIAN_POINT('Ctrl Pts',(6.76243636205683,62.5644789380886,2.63954450640411));
#243740=CARTESIAN_POINT('Ctrl Pts',(6.71251593157878,62.5342007968301,2.69627684028914));
#243741=CARTESIAN_POINT('Ctrl Pts',(6.67979835840238,62.464869612516,2.68224356036541));
#243742=CARTESIAN_POINT('Ctrl Pts',(6.68360310202785,62.5984172531145,2.59908178706448));
#243743=CARTESIAN_POINT('Ctrl Pts',(6.65585031610561,62.56382654801,2.65878704321526));
#243744=CARTESIAN_POINT('Ctrl Pts',(6.63528943158918,62.495199902913,2.65878198860306));
#243745=CARTESIAN_POINT('Ctrl Pts',(6.59568250079866,62.6076796697356,2.59908173516068));
#243746=CARTESIAN_POINT('Ctrl Pts',(6.59177408464754,62.5705801176612,2.65878198860306));
#243747=CARTESIAN_POINT('Ctrl Pts',(6.58439859103009,62.5005702980933,2.65878198860306));
#243748=CARTESIAN_POINT('Origin',(6.8651762812249,62.2803389979221,2.83404198860306));
#243749=CARTESIAN_POINT('Origin',(5.89267880207495,59.1025439185017,3.11913648167056));
#243750=CARTESIAN_POINT('Origin',(5.8740571235785,58.9253704827882,2.83404198860304));
#243751=CARTESIAN_POINT('Origin',(6.84655462836425,62.1031658061012,3.11913648177577));
#243752=CARTESIAN_POINT('Origin',(6.82793297553329,61.9259926140921,3.40423097483353));
#243753=CARTESIAN_POINT('Ctrl Pts',(5.86337364149561,58.8181995570487,2.90134173516065));
#243754=CARTESIAN_POINT('Ctrl Pts',(5.98915458643775,58.8054696185322,2.90103711553271));
#243755=CARTESIAN_POINT('Ctrl Pts',(6.00036140429027,58.9120953679532,2.83404198860304));
#243756=CARTESIAN_POINT('Ctrl Pts',(5.85862481136466,58.7730123682042,2.82862991748005));
#243757=CARTESIAN_POINT('Ctrl Pts',(5.97090589422292,58.7772117628631,2.85314045886508));
#243758=CARTESIAN_POINT('Ctrl Pts',(5.99561184840489,58.8669063622639,2.79187961000089));
#243759=CARTESIAN_POINT('Ctrl Pts',(5.8802564056756,58.7244521481309,2.75470625793363));
#243760=CARTESIAN_POINT('Ctrl Pts',(5.9711183347537,58.7389107566978,2.79224250381922));
#243761=CARTESIAN_POINT('Ctrl Pts',(6.00616078842873,58.8195131589312,2.74901809108296));
#243762=CARTESIAN_POINT('Ctrl Pts',(5.97763489331424,58.6422449895252,2.63947868311745));
#243763=CARTESIAN_POINT('Ctrl Pts',(6.02730636094599,58.6726343357865,2.69595066767966));
#243764=CARTESIAN_POINT('Ctrl Pts',(6.05959099741147,58.7419259266992,2.68220539436107));
#243765=CARTESIAN_POINT('Ctrl Pts',(6.05629725705618,58.6088386066686,2.59908178585166));
#243766=CARTESIAN_POINT('Ctrl Pts',(6.08390124328611,58.6434504949727,2.65877670944951));
#243767=CARTESIAN_POINT('Ctrl Pts',(6.10418993497023,58.7121001992973,2.65878198860303));
#243768=CARTESIAN_POINT('Ctrl Pts',(6.14377718965303,58.599666897865,2.59908173516065));
#243769=CARTESIAN_POINT('Ctrl Pts',(6.14766703046151,58.6367684021394,2.65878198860303));
#243770=CARTESIAN_POINT('Ctrl Pts',(6.15500747092297,58.7067819056645,2.65878198860303));
#243771=CARTESIAN_POINT('Origin',(6.15500747092297,58.7067819056645,2.53178198860303));
#243772=CARTESIAN_POINT('Ctrl Pts',(6.78290064323541,61.4975385923864,3.77003198860306));
#243773=CARTESIAN_POINT('Ctrl Pts',(6.65640765888743,61.5108335407728,3.77003198860306));
#243774=CARTESIAN_POINT('Ctrl Pts',(6.65659650327857,61.5108136924275,3.64284238727617));
#243775=CARTESIAN_POINT('Ctrl Pts',(6.80580235504208,61.7133034041537,3.77003198860307));
#243776=CARTESIAN_POINT('Ctrl Pts',(6.67910686401112,61.7268068187944,3.77025506105831));
#243777=CARTESIAN_POINT('Ctrl Pts',(6.67473401011702,61.6833805404071,3.64284210641898));
#243778=CARTESIAN_POINT('Ctrl Pts',(6.82760223531318,61.918708281938,3.65553527987875));
#243779=CARTESIAN_POINT('Ctrl Pts',(6.7007104969118,61.9323562021251,3.65585996533108));
#243780=CARTESIAN_POINT('Ctrl Pts',(6.69200060426984,61.8476612078251,3.5512790271024));
#243781=CARTESIAN_POINT('Ctrl Pts',(6.8397366303024,62.0330459552234,3.47153072139115));
#243782=CARTESIAN_POINT('Ctrl Pts',(6.71274549238771,62.0468640245952,3.47182327905232));
#243783=CARTESIAN_POINT('Ctrl Pts',(6.70161199275238,61.9391074595192,3.40413028378018));
#243784=CARTESIAN_POINT('Origin',(6.78290064323541,61.4975385923864,3.64303198860306));
#243785=CARTESIAN_POINT('Origin',(5.67080826956262E-15,1.86383062767523E-13,
2.53178198860262));
#243786=CARTESIAN_POINT('Origin',(6.1853204982938,58.7035958781041,2.53178198860303));
#243787=CARTESIAN_POINT('Origin',(0.995615674755264,6.43520020182058,3.64303198860267));
#243788=CARTESIAN_POINT('Origin',(6.74099917688016,61.0983782637181,3.64299466007516));
#243789=CARTESIAN_POINT('Ctrl Pts',(6.17403490859001,58.5964866834553,2.59908173516065));
#243790=CARTESIAN_POINT('Ctrl Pts',(6.17794390662153,58.6335861742244,2.65878198860303));
#243791=CARTESIAN_POINT('Ctrl Pts',(6.1853204982938,58.7035958781041,2.65878198860303));
#243792=CARTESIAN_POINT('Ctrl Pts',(6.26121185652527,58.5873013840791,2.59908193199986));
#243793=CARTESIAN_POINT('Ctrl Pts',(6.24145541658269,58.6268910424095,2.65877685806751));
#243794=CARTESIAN_POINT('Ctrl Pts',(6.23596000968385,58.6982507756613,2.65878198860303));
#243795=CARTESIAN_POINT('Ctrl Pts',(6.34441620808585,58.6032244953992,2.63872492669832));
#243796=CARTESIAN_POINT('Ctrl Pts',(6.30249747592707,58.643316920109,2.69532212015315));
#243797=CARTESIAN_POINT('Ctrl Pts',(6.285367292233,58.7177256636154,2.68176836726675));
#243798=CARTESIAN_POINT('Ctrl Pts',(6.45770985055657,58.6635810738167,2.75442176402299));
#243799=CARTESIAN_POINT('Ctrl Pts',(6.37191831988765,58.6966524426405,2.79203179920177));
#243800=CARTESIAN_POINT('Ctrl Pts',(6.35432657855797,58.7827411889912,2.74885310748218));
#243801=CARTESIAN_POINT('Ctrl Pts',(6.4889986109651,58.7067768761602,2.82866089558439));
#243802=CARTESIAN_POINT('Ctrl Pts',(6.38003592347226,58.7342263230563,2.85316563119207));
#243803=CARTESIAN_POINT('Ctrl Pts',(6.37452670784949,58.8271002111747,2.79189751796582));
#243804=CARTESIAN_POINT('Ctrl Pts',(6.49374646112722,58.7519447039091,2.90134173516067));
#243805=CARTESIAN_POINT('Ctrl Pts',(6.36806742857307,58.7656442740273,2.90103711553272));
#243806=CARTESIAN_POINT('Ctrl Pts',(6.37927424642559,58.8722700234482,2.83404198860304));
#243807=CARTESIAN_POINT('Origin',(6.50557852713736,58.8589949086133,2.83404198860304));
#243808=CARTESIAN_POINT('Origin',(6.73632490881142,61.0544000804066,3.56647653971863));
#243809=CARTESIAN_POINT('Origin',(6.72777047351104,60.9730100652056,3.42473028058528));
#243810=CARTESIAN_POINT('Origin',(6.52420020557758,59.0361683443166,3.11913648168054));
#243811=CARTESIAN_POINT('Origin',(6.54282188406209,59.2133417798938,3.40423097483352));
#243812=CARTESIAN_POINT('Ctrl Pts',(6.69328024897436,60.6448574988556,3.36123028058524));
#243813=CARTESIAN_POINT('Ctrl Pts',(6.56697596826259,60.6581326136906,3.36123028058524));
#243814=CARTESIAN_POINT('Ctrl Pts',(6.56697596826259,60.6581326136906,3.23423028058524));
#243815=CARTESIAN_POINT('Ctrl Pts',(6.70245599674977,60.7343993681216,3.36123028058524));
#243816=CARTESIAN_POINT('Ctrl Pts',(6.57637578951156,60.7475659388558,3.36099641108513));
#243817=CARTESIAN_POINT('Ctrl Pts',(6.58108878091668,60.7924070567558,3.23423043688444));
#243818=CARTESIAN_POINT('Ctrl Pts',(6.71113417453879,60.8190677588582,3.41054258905326));
#243819=CARTESIAN_POINT('Ctrl Pts',(6.58530836180227,60.8325536871463,3.41008815825976));
#243820=CARTESIAN_POINT('Ctrl Pts',(6.59443344928435,60.9193730951266,3.30819867304253));
#243821=CARTESIAN_POINT('Ctrl Pts',(6.7157078966939,60.8636883187847,3.48823028058527));
#243822=CARTESIAN_POINT('Ctrl Pts',(6.59002106156447,60.8773920302463,3.48794691941643));
#243823=CARTESIAN_POINT('Ctrl Pts',(6.60146619279927,60.9862851800406,3.42473028058528));
#243824=CARTESIAN_POINT('Origin',(6.69328024897435,60.6448574988556,3.23423028058524));
#243825=CARTESIAN_POINT('Ctrl Pts',(6.53099325080036,59.1062911958299,3.47153072139113));
#243826=CARTESIAN_POINT('Ctrl Pts',(6.4051226409098,59.1200087114584,3.47122746285118));
#243827=CARTESIAN_POINT('Ctrl Pts',(6.41653455700106,59.2267768430463,3.40413046676828));
#243828=CARTESIAN_POINT('Ctrl Pts',(6.54313486548357,59.2206299794253,3.65553813458027));
#243829=CARTESIAN_POINT('Ctrl Pts',(6.41712406698097,59.2341972766231,3.6552033607226));
#243830=CARTESIAN_POINT('Ctrl Pts',(6.42614611919713,59.3182247474321,3.55128134519992));
#243831=CARTESIAN_POINT('Ctrl Pts',(6.5649460139707,59.4260354503641,3.77003198860305));
#243832=CARTESIAN_POINT('Ctrl Pts',(6.43870134519751,59.439496135217,3.76980209314202));
#243833=CARTESIAN_POINT('Ctrl Pts',(6.44341285848436,59.4825067955809,3.64284195387452));
#243834=CARTESIAN_POINT('Ctrl Pts',(6.58785426247077,59.6417962403145,3.77003198860305));
#243835=CARTESIAN_POINT('Ctrl Pts',(6.46136078685214,59.6550912403355,3.77003198860305));
#243836=CARTESIAN_POINT('Ctrl Pts',(6.46155012324721,59.6550713402785,3.64284189403843));
#243837=CARTESIAN_POINT('Origin',(6.58785426247077,59.6417962403145,3.64303198860305));
#243838=CARTESIAN_POINT('Origin',(0.979147644052797,6.27851735587401,3.23423028058486));
#243839=CARTESIAN_POINT('Origin',(6.67747469700926,60.4944777170596,3.23423028058524));
#243840=CARTESIAN_POINT('Origin',(0.976568823008617,6.25398151259742,3.64303198860267));
#243841=CARTESIAN_POINT('Origin',(6.62985850077821,60.0409538388298,3.64299171721826));
#243842=CARTESIAN_POINT('Ctrl Pts',(6.65505462397376,60.2756459899121,3.48823028058522));
#243843=CARTESIAN_POINT('Ctrl Pts',(6.52822907310758,60.2894805317164,3.488520042123));
#243844=CARTESIAN_POINT('Ctrl Pts',(6.51668018436727,60.1796001951997,3.42473028058522));
#243845=CARTESIAN_POINT('Ctrl Pts',(6.65964099131244,60.3204176712047,3.41028005848447));
#243846=CARTESIAN_POINT('Ctrl Pts',(6.5329085169049,60.3340024654481,3.41074404220456));
#243847=CARTESIAN_POINT('Ctrl Pts',(6.52373669508342,60.2467384099283,3.3078048624401));
#243848=CARTESIAN_POINT('Ctrl Pts',(6.66833043150643,60.4052373806433,3.36123028058524));
#243849=CARTESIAN_POINT('Ctrl Pts',(6.54178440911712,60.4184509388135,3.36146460586437));
#243850=CARTESIAN_POINT('Ctrl Pts',(6.53710513959985,60.3739306632437,3.23423045308454));
#243851=CARTESIAN_POINT('Ctrl Pts',(6.67747469700926,60.4944777170596,3.36123028058524));
#243852=CARTESIAN_POINT('Ctrl Pts',(6.5511704162975,60.5077528318946,3.36123028058524));
#243853=CARTESIAN_POINT('Ctrl Pts',(6.55117041629749,60.5077528318946,3.23423028058524));
#243854=CARTESIAN_POINT('Origin',(6.64298446507904,60.1663250803647,3.42473028058523));
#243855=CARTESIAN_POINT('Origin',(6.63448104699032,60.0854204586813,3.56563113524822));
#243856=CARTESIAN_POINT('Origin',(-0.31749999970759,61.4240753804098,3.56647653909432));
#243857=CARTESIAN_POINT('Origin',(-0.317551690015093,61.4683012396087,3.6429946600749));
#243858=CARTESIAN_POINT('Origin',(-0.317500000000209,61.3422370451707,3.42473028058526));
#243859=CARTESIAN_POINT('Ctrl Pts',(-0.316930737396123,61.2322532920974,
3.48823028058527));
#243860=CARTESIAN_POINT('Ctrl Pts',(-0.190500000000209,61.2327440814647,
3.48794691941643));
#243861=CARTESIAN_POINT('Ctrl Pts',(-0.190500000000209,61.3422370451707,
3.42473028058528));
#243862=CARTESIAN_POINT('Ctrl Pts',(-0.317046579199837,61.1872475084176,
3.41028005925129));
#243863=CARTESIAN_POINT('Ctrl Pts',(-0.190500000001825,61.187506454177,
3.40982512230997));
#243864=CARTESIAN_POINT('Ctrl Pts',(-0.190500000000208,61.2747290395328,
3.30780486372837));
#243865=CARTESIAN_POINT('Ctrl Pts',(-0.317266596913697,61.1019842137034,
3.36123028058524));
#243866=CARTESIAN_POINT('Ctrl Pts',(-0.190500000000084,61.1018997758103,
3.36099721048488));
#243867=CARTESIAN_POINT('Ctrl Pts',(-0.190500000000208,61.14683620717,3.23423045308409));
#243868=CARTESIAN_POINT('Ctrl Pts',(-0.317500000000208,61.0122769227458,
3.36123028058524));
#243869=CARTESIAN_POINT('Ctrl Pts',(-0.190500000000207,61.0122769227458,
3.36123028058524));
#243870=CARTESIAN_POINT('Ctrl Pts',(-0.190500000000207,61.0122769227458,
3.23423028058524));
#243871=CARTESIAN_POINT('Origin',(-0.317500000000208,61.0122769227458,3.23423028058524));
#243872=CARTESIAN_POINT('Origin',(-0.317499999999994,1.82709072144943E-13,
3.64303198860263));
#243873=CARTESIAN_POINT('Origin',(-0.317500000000211,61.8696548221182,3.64303198860306));
#243874=CARTESIAN_POINT('Origin',(-0.317499999999994,1.85563719214605E-13,
3.23423028058481));
#243875=CARTESIAN_POINT('Origin',(-0.317500000000207,60.8610688070709,3.23423028058524));
#243876=CARTESIAN_POINT('Ctrl Pts',(-0.318048871877342,62.408169597977,
3.47153072139115));
#243877=CARTESIAN_POINT('Ctrl Pts',(-0.190309034175511,62.4086377819836,
3.47182327902706));
#243878=CARTESIAN_POINT('Ctrl Pts',(-0.190500142125266,62.3003077603773,
3.40413028959066));
#243879=CARTESIAN_POINT('Ctrl Pts',(-0.317932489890151,62.2931881445373,
3.65553807121));
#243880=CARTESIAN_POINT('Ctrl Pts',(-0.190309294367321,62.2934975005775,
3.65586275497125));
#243881=CARTESIAN_POINT('Ctrl Pts',(-0.19050014199568,62.2083564003277,
3.55128126837385));
#243882=CARTESIAN_POINT('Ctrl Pts',(-0.31772268616762,62.0866281564674,
3.77003198860307));
#243883=CARTESIAN_POINT('Ctrl Pts',(-0.190309769569843,62.0868143053063,
3.77025505748512));
#243884=CARTESIAN_POINT('Ctrl Pts',(-0.190500141762077,62.0431695205371,
3.64284211731146));
#243885=CARTESIAN_POINT('Ctrl Pts',(-0.31750000000021,61.8696548221183,
3.77003198860307));
#243886=CARTESIAN_POINT('Ctrl Pts',(-0.190310267889154,61.8696548221182,
3.77003198860307));
#243887=CARTESIAN_POINT('Ctrl Pts',(-0.190500141514125,61.8696548221183,
3.64284239821734));
#243888=CARTESIAN_POINT('Origin',(-0.317500000000212,62.3004688883556,3.40423097483353));
#243889=CARTESIAN_POINT('Ctrl Pts',(-0.317500000000207,60.8610688070709,
3.36123028058524));
#243890=CARTESIAN_POINT('Ctrl Pts',(-0.190500000000207,60.8610688070709,
3.36123028058524));
#243891=CARTESIAN_POINT('Ctrl Pts',(-0.190500000000207,60.8610688070709,
3.23423028058524));
#243892=CARTESIAN_POINT('Ctrl Pts',(-0.317734773760476,60.7710583184322,
3.36123028058524));
#243893=CARTESIAN_POINT('Ctrl Pts',(-0.190500000000322,60.7709717342392,
3.36146538610154));
#243894=CARTESIAN_POINT('Ctrl Pts',(-0.190500000000206,60.7260547307348,
3.23423043688425));
#243895=CARTESIAN_POINT('Ctrl Pts',(-0.31795861791923,60.685946575458,3.41054258693139));
#243896=CARTESIAN_POINT('Ctrl Pts',(-0.190499999999005,60.6862105562605,
3.41100608859939));
#243897=CARTESIAN_POINT('Ctrl Pts',(-0.190500000000206,60.5983892955427,
3.30819866970959));
#243898=CARTESIAN_POINT('Ctrl Pts',(-0.318076890623573,60.6410923272407,
3.48823028058523));
#243899=CARTESIAN_POINT('Ctrl Pts',(-0.190500000000212,60.6415942020423,
3.488520042123));
#243900=CARTESIAN_POINT('Ctrl Pts',(-0.190500000000206,60.5311086139136,
3.42473028058523));
#243901=CARTESIAN_POINT('Origin',(-0.317500000000206,60.5311086139136,3.42473028058523));
#243902=CARTESIAN_POINT('Origin',(-0.317499999976043,62.4786179998491,3.11913648178467));
#243903=CARTESIAN_POINT('Origin',(-0.317500000000213,62.6567671111301,2.83404198860305));
#243904=CARTESIAN_POINT('Origin',(-0.317499999993752,60.4497583458794,3.56563113460841));
#243905=CARTESIAN_POINT('Origin',(-0.317550804320552,60.4050521322805,3.64299171721841));
#243906=CARTESIAN_POINT('Ctrl Pts',(-0.015266117311081,62.954144805765,
2.59908173516067));
#243907=CARTESIAN_POINT('Ctrl Pts',(-0.0152570710388482,62.9168399481845,
2.65878198860306));
#243908=CARTESIAN_POINT('Ctrl Pts',(-0.0152400000002138,62.8464427007198,
2.65878198860306));
#243909=CARTESIAN_POINT('Ctrl Pts',(-0.103381504925414,62.9541233134301,
2.59908193475651));
#243910=CARTESIAN_POINT('Ctrl Pts',(-0.0794415635237897,62.9168211560343,
2.65878715325392));
#243911=CARTESIAN_POINT('Ctrl Pts',(-0.0662446030561493,62.8464212442882,
2.65878198860306));
#243912=CARTESIAN_POINT('Ctrl Pts',(-0.184683583688025,62.9290872705828,
2.63878778849938));
#243913=CARTESIAN_POINT('Ctrl Pts',(-0.138547994784516,62.893677113745,
2.69564460180164));
#243914=CARTESIAN_POINT('Ctrl Pts',(-0.113305567451785,62.8213855864657,
2.68180481624935));
#243915=CARTESIAN_POINT('Ctrl Pts',(-0.291340992631915,62.8564203507744,
2.75443238878668));
#243916=CARTESIAN_POINT('Ctrl Pts',(-0.201910351191571,62.8329175802744,
2.79268340777131));
#243917=CARTESIAN_POINT('Ctrl Pts',(-0.175042741958052,62.7487193609391,
2.74885926835647));
#243918=CARTESIAN_POINT('Ctrl Pts',(-0.318045276842852,62.8099434033763,
2.8285665536173));
#243919=CARTESIAN_POINT('Ctrl Pts',(-0.20583163564296,62.7947175425021,
2.85384197230965));
#243920=CARTESIAN_POINT('Ctrl Pts',(-0.190500000000215,62.7022409210456,
2.7918462427865));
#243921=CARTESIAN_POINT('Ctrl Pts',(-0.318045750793259,62.7644678366121,
2.90134173516068));
#243922=CARTESIAN_POINT('Ctrl Pts',(-0.19050000000021,62.764932651015,2.90163218716436));
#243923=CARTESIAN_POINT('Ctrl Pts',(-0.190500000000213,62.6567671111301,
2.83404198860306));
#243924=CARTESIAN_POINT('Origin',(-0.0152400000002138,62.8464427007198,
2.53178198860305));
#243925=CARTESIAN_POINT('Origin',(-0.317499999999994,1.82709072144943E-13,
3.64303198860263));
#243926=CARTESIAN_POINT('Origin',(-0.317500000000204,60.0036905223732,3.64303198860304));
#243927=CARTESIAN_POINT('Origin',(-3.02076666443335E-17,1.91412545152793E-13,
2.53178198860262));
#243928=CARTESIAN_POINT('Origin',(0.0152399999997862,62.8464427007198,2.53178198860306));
#243929=CARTESIAN_POINT('Ctrl Pts',(-0.317500000000204,60.0036905223732,
3.77003198860305));
#243930=CARTESIAN_POINT('Ctrl Pts',(-0.190309748265563,60.0036905223732,
3.77003198860305));
#243931=CARTESIAN_POINT('Ctrl Pts',(-0.190500142289733,60.0036905223732,
3.6428418793711));
#243932=CARTESIAN_POINT('Ctrl Pts',(-0.317270385524616,59.7867137603526,
3.77003198860305));
#243933=CARTESIAN_POINT('Ctrl Pts',(-0.190310262476488,59.7869045527981,
3.76980208962936));
#243934=CARTESIAN_POINT('Ctrl Pts',(-0.190500142032665,59.8301727552489,
3.64284193928328));
#243935=CARTESIAN_POINT('Ctrl Pts',(-0.317049440713829,59.580155267073,
3.65553535416627));
#243936=CARTESIAN_POINT('Ctrl Pts',(-0.190310761082532,59.5804765271859,
3.65520057834489));
#243937=CARTESIAN_POINT('Ctrl Pts',(-0.190500141785308,59.6649871046561,
3.55127910964259));
#243938=CARTESIAN_POINT('Ctrl Pts',(-0.316925998273249,59.4651754363834,
3.47153072139113));
#243939=CARTESIAN_POINT('Ctrl Pts',(-0.190311035335302,59.4656607446595,
3.47122746281624));
#243940=CARTESIAN_POINT('Ctrl Pts',(-0.190500141647104,59.5730368716577,
3.40413045901326));
#243941=CARTESIAN_POINT('Origin',(-0.317500000000203,59.5728760150044,3.40423097483352));
#243942=CARTESIAN_POINT('Ctrl Pts',(0.318045750792832,62.7644678366121,
2.90134173516067));
#243943=CARTESIAN_POINT('Ctrl Pts',(0.190499999999787,62.764932651015,2.90163218716435));
#243944=CARTESIAN_POINT('Ctrl Pts',(0.190499999999787,62.6567671111301,
2.83404198860305));
#243945=CARTESIAN_POINT('Ctrl Pts',(0.318045262794965,62.8099640589336,
2.82853349835403));
#243946=CARTESIAN_POINT('Ctrl Pts',(0.2058403307229,62.7947344577637,2.85381483162476));
#243947=CARTESIAN_POINT('Ctrl Pts',(0.190499999999787,62.7022616416342,
2.79182701594311));
#243948=CARTESIAN_POINT('Ctrl Pts',(0.291334117855211,62.8562601188217,
2.75468822073678));
#243949=CARTESIAN_POINT('Ctrl Pts',(0.201836550627546,62.8328016940826,
2.79286913083901));
#243950=CARTESIAN_POINT('Ctrl Pts',(0.175038734051964,62.7485591297234,
2.74900763297961));
#243951=CARTESIAN_POINT('Ctrl Pts',(0.185622189560167,62.9286112571072,
2.63954450640446));
#243952=CARTESIAN_POINT('Ctrl Pts',(0.139140155999877,62.8932808767901,
2.69627684028887));
#243953=CARTESIAN_POINT('Ctrl Pts',(0.113848895265485,62.8209095783127,
2.6822435603653));
#243954=CARTESIAN_POINT('Ctrl Pts',(0.103673266462632,62.9541233349678,
2.59908178706367));
#243955=CARTESIAN_POINT('Ctrl Pts',(0.0796882264534906,62.9168211653024,
2.65878704321514));
#243956=CARTESIAN_POINT('Ctrl Pts',(0.0664134143649273,62.8464212664865,
2.65878198860306));
#243957=CARTESIAN_POINT('Ctrl Pts',(0.0152661173106522,62.954144805765,
2.59908173516067));
#243958=CARTESIAN_POINT('Ctrl Pts',(0.0152570710384197,62.9168399481845,
2.65878198860306));
#243959=CARTESIAN_POINT('Ctrl Pts',(0.0152399999997859,62.8464427007198,
2.65878198860306));
#243960=CARTESIAN_POINT('Origin',(0.317499999999787,62.6567671111301,2.83404198860304));
#243961=CARTESIAN_POINT('Origin',(-0.317499999971749,59.394726658624,3.1191364816716));
#243962=CARTESIAN_POINT('Origin',(-0.317500000000201,59.2165773020943,2.83404198860304));
#243963=CARTESIAN_POINT('Origin',(0.31749999997701,62.4786179998349,3.11913648177581));
#243964=CARTESIAN_POINT('Origin',(0.317499999999788,62.3004688883556,3.40423097483353));
#243965=CARTESIAN_POINT('Ctrl Pts',(-0.316922544675889,59.108876741935,
2.90134173516064));
#243966=CARTESIAN_POINT('Ctrl Pts',(-0.190500000000207,59.1093642282368,
2.9010371155327));
#243967=CARTESIAN_POINT('Ctrl Pts',(-0.190500000000201,59.2165773020943,
2.83404198860303));
#243968=CARTESIAN_POINT('Ctrl Pts',(-0.316922012809374,59.0634407053231,
2.82862991748008));
#243969=CARTESIAN_POINT('Ctrl Pts',(-0.205694973740556,59.0793536643045,
2.85314045886453));
#243970=CARTESIAN_POINT('Ctrl Pts',(-0.190500000000201,59.1711393827296,
2.79187960999964));
#243971=CARTESIAN_POINT('Ctrl Pts',(-0.290332993455134,59.0174076205277,
2.7547062579336));
#243972=CARTESIAN_POINT('Ctrl Pts',(-0.20148015166603,59.0412846811397,
2.79224250381941));
#243973=CARTESIAN_POINT('Ctrl Pts',(-0.175054909459902,59.1251084688123,
2.74901809108301));
#243974=CARTESIAN_POINT('Ctrl Pts',(-0.18489496740184,58.9458296250065,
2.63947868311748));
#243975=CARTESIAN_POINT('Ctrl Pts',(-0.138672156931446,58.9812445774294,
2.69595066767951));
#243976=CARTESIAN_POINT('Ctrl Pts',(-0.113807322597986,59.0535312451935,
2.68220539436102));
#243977=CARTESIAN_POINT('Ctrl Pts',(-0.103171606455878,58.9208287018092,
2.59908178585124));
#243978=CARTESIAN_POINT('Ctrl Pts',(-0.0793367652459801,58.9581363848287,
2.65877670944864));
#243979=CARTESIAN_POINT('Ctrl Pts',(-0.0663350652345453,59.0285307646524,
2.65878198860303));
#243980=CARTESIAN_POINT('Ctrl Pts',(-0.0152121934561203,58.9208513795075,
2.59908173516065));
#243981=CARTESIAN_POINT('Ctrl Pts',(-0.0152218248293074,58.9581562369415,
2.65878198860303));
#243982=CARTESIAN_POINT('Ctrl Pts',(-0.0152400000002007,59.0285534841298,
2.65878198860303));
#243983=CARTESIAN_POINT('Origin',(-0.0152400000002004,59.0285534841298,
2.53178198860303));
#243984=CARTESIAN_POINT('Ctrl Pts',(0.31749999999979,61.8696548221183,3.77003198860307));
#243985=CARTESIAN_POINT('Ctrl Pts',(0.190310256931134,61.8696548221183,
3.77003198860307));
#243986=CARTESIAN_POINT('Ctrl Pts',(0.190500141530038,61.8696548221183,
3.64284238727611));
#243987=CARTESIAN_POINT('Ctrl Pts',(0.317722689632019,62.0866315324122,
3.77003198860307));
#243988=CARTESIAN_POINT('Ctrl Pts',(0.190309758575237,62.0868176889507,
3.77025506105805));
#243989=CARTESIAN_POINT('Ctrl Pts',(0.190500141778022,62.0431722165645,
3.64284210641846));
#243990=CARTESIAN_POINT('Ctrl Pts',(0.317932491655467,62.2931898887683,
3.65553527987874));
#243991=CARTESIAN_POINT('Ctrl Pts',(0.190309283349448,62.2934992458087,
3.65585996533256));
#243992=CARTESIAN_POINT('Ctrl Pts',(0.190500142011647,62.2083577878533,
3.55127902710321));
#243993=CARTESIAN_POINT('Ctrl Pts',(0.318048871876917,62.408169597977,3.47153072139115));
#243994=CARTESIAN_POINT('Ctrl Pts',(0.190309023146207,62.4086377820241,
3.47182327905231));
#243995=CARTESIAN_POINT('Ctrl Pts',(0.190500142141247,62.3003077510786,
3.40413028378014));
#243996=CARTESIAN_POINT('Origin',(0.31749999999979,61.8696548221183,3.64303198860307));
#243997=CARTESIAN_POINT('Origin',(4.1196902326603E-16,1.9163609199248E-13,
2.53178198860262));
#243998=CARTESIAN_POINT('Origin',(0.0152399999997996,59.0285534841298,2.53178198860303));
#243999=CARTESIAN_POINT('Origin',(0.317500000000005,-3.23223802458442E-14,
3.64303198860263));
#244000=CARTESIAN_POINT('Origin',(0.317551690013334,61.4683012396078,3.64299466007611));
#244001=CARTESIAN_POINT('Ctrl Pts',(0.0152121934557198,58.9208513795075,
2.59908173516065));
#244002=CARTESIAN_POINT('Ctrl Pts',(0.0152218248289066,58.9581562369415,
2.65878198860303));
#244003=CARTESIAN_POINT('Ctrl Pts',(0.0152399999997995,59.0285534841298,
2.65878198860303));
#244004=CARTESIAN_POINT('Ctrl Pts',(0.102871702177208,58.9208288705622,
2.59908193199955));
#244005=CARTESIAN_POINT('Ctrl Pts',(0.0790852439333024,58.9581365422945,
2.65877685806598));
#244006=CARTESIAN_POINT('Ctrl Pts',(0.0661608181923186,59.0285309330229,
2.65878198860303));
#244007=CARTESIAN_POINT('Ctrl Pts',(0.183955833237286,58.9453619764185,
2.63872492669837));
#244008=CARTESIAN_POINT('Ctrl Pts',(0.138075936735604,58.9808530699765,
2.6953221201532));
#244009=CARTESIAN_POINT('Ctrl Pts',(0.113261762367936,59.0530636028228,
2.68176836726675));
#244010=CARTESIAN_POINT('Ctrl Pts',(0.290319860890481,59.0172303255296,
2.75442176402292));
#244011=CARTESIAN_POINT('Ctrl Pts',(0.201541405841888,59.041152869072,2.79203179920166));
#244012=CARTESIAN_POINT('Ctrl Pts',(0.175047309551012,59.1249311745759,
2.74885310748217));
#244013=CARTESIAN_POINT('Ctrl Pts',(0.316922027357146,59.0634600627913,
2.82866089558442));
#244014=CARTESIAN_POINT('Ctrl Pts',(0.205687000365689,59.0793694364681,
2.8531656311923));
#244015=CARTESIAN_POINT('Ctrl Pts',(0.190499999999799,59.1711586818657,
2.79189751796687));
#244016=CARTESIAN_POINT('Ctrl Pts',(0.316922544675488,59.108876741935,2.90134173516064));
#244017=CARTESIAN_POINT('Ctrl Pts',(0.190499999999804,59.1093642282368,
2.9010371155327));
#244018=CARTESIAN_POINT('Ctrl Pts',(0.190499999999799,59.2165773020943,
2.83404198860303));
#244019=CARTESIAN_POINT('Origin',(0.317499999999799,59.2165773020943,2.83404198860303));
#244020=CARTESIAN_POINT('Origin',(0.317499999995335,61.4240753793297,3.56647653971789));
#244021=CARTESIAN_POINT('Origin',(0.317499999999791,61.3422370451707,3.42473028058527));
#244022=CARTESIAN_POINT('Origin',(0.317499999969512,59.3947266586068,3.11913648168234));
#244023=CARTESIAN_POINT('Origin',(0.317499999999798,59.5728760150044,3.40423097483352));
#244024=CARTESIAN_POINT('Ctrl Pts',(0.317499999999793,61.0122769227458,
3.36123028058524));
#244025=CARTESIAN_POINT('Ctrl Pts',(0.190499999999793,61.0122769227458,
3.36123028058524));
#244026=CARTESIAN_POINT('Ctrl Pts',(0.190499999999793,61.0122769227458,
3.23423028058524));
#244027=CARTESIAN_POINT('Ctrl Pts',(0.317265808076183,61.1022873990973,
3.36123028058524));
#244028=CARTESIAN_POINT('Ctrl Pts',(0.190499999999665,61.1022028716689,
3.36099641108502));
#244029=CARTESIAN_POINT('Ctrl Pts',(0.190499999999792,61.1472909869829,
3.23423043688409));
#244030=CARTESIAN_POINT('Ctrl Pts',(0.317046189128874,61.1873990841187,
3.41054258905327));
#244031=CARTESIAN_POINT('Ctrl Pts',(0.190499999999403,61.1876587562349,
3.41008815826007));
#244032=CARTESIAN_POINT('Ctrl Pts',(0.190499999999792,61.2749563897851,
3.30819867304325));
#244033=CARTESIAN_POINT('Ctrl Pts',(0.316930737395706,61.2322532920974,
3.48823028058526));
#244034=CARTESIAN_POINT('Ctrl Pts',(0.190499999999791,61.2327440814647,
3.48794691941642));
#244035=CARTESIAN_POINT('Ctrl Pts',(0.190499999999791,61.3422370451707,
3.42473028058527));
#244036=CARTESIAN_POINT('Origin',(0.317499999999793,61.0122769227458,3.23423028058524));
#244037=CARTESIAN_POINT('Ctrl Pts',(0.316925998272845,59.4651754363834,
3.47153072139113));
#244038=CARTESIAN_POINT('Ctrl Pts',(0.190311049925297,59.4656607446036,
3.47122746285118));
#244039=CARTESIAN_POINT('Ctrl Pts',(0.190500141624843,59.5730368592468,
3.40413046676854));
#244040=CARTESIAN_POINT('Ctrl Pts',(0.317049442578967,59.5801570044832,
3.6555381345803));
#244041=CARTESIAN_POINT('Ctrl Pts',(0.190310775691579,59.5804782634891,
3.65520336072179));
#244042=CARTESIAN_POINT('Ctrl Pts',(0.190500141763024,59.6649884842734,
3.55128134519974));
#244043=CARTESIAN_POINT('Ctrl Pts',(0.317270389088637,59.7867171285937,
3.77003198860305));
#244044=CARTESIAN_POINT('Ctrl Pts',(0.190310277118373,59.7869079131808,
3.76980209314153));
#244045=CARTESIAN_POINT('Ctrl Pts',(0.190500142010346,59.8301754438912,
3.64284195387455));
#244046=CARTESIAN_POINT('Ctrl Pts',(0.317499999999796,60.0036905223732,
3.77003198860305));
#244047=CARTESIAN_POINT('Ctrl Pts',(0.190309762954983,60.0036905223732,
3.77003198860305));
#244048=CARTESIAN_POINT('Ctrl Pts',(0.190500142267369,60.0036905223733,
3.64284189403892));
#244049=CARTESIAN_POINT('Origin',(0.317499999999796,60.0036905223732,3.64303198860304));
#244050=CARTESIAN_POINT('Origin',(0.317500000000005,-2.42053524934248E-14,
3.23423028058481));
#244051=CARTESIAN_POINT('Origin',(0.317499999999793,60.8610688070709,3.23423028058524));
#244052=CARTESIAN_POINT('Origin',(0.317500000000005,-2.62359339360319E-14,
3.64303198860263));
#244053=CARTESIAN_POINT('Origin',(0.317550804319973,60.4050521322806,3.64299171721856));
#244054=CARTESIAN_POINT('Ctrl Pts',(0.31807689062316,60.6410923272407,3.48823028058523));
#244055=CARTESIAN_POINT('Ctrl Pts',(0.190499999999794,60.6415942020423,
3.48852004212301));
#244056=CARTESIAN_POINT('Ctrl Pts',(0.190499999999794,60.5311086139136,
3.42473028058523));
#244057=CARTESIAN_POINT('Ctrl Pts',(0.317958218318559,60.6860981505086,
3.41028005848445));
#244058=CARTESIAN_POINT('Ctrl Pts',(0.190500000001774,60.6863613750278,
3.41074404220382));
#244059=CARTESIAN_POINT('Ctrl Pts',(0.190499999999794,60.5986166446954,
3.30780486243962));
#244060=CARTESIAN_POINT('Ctrl Pts',(0.317733982967334,60.7713615025342,
3.36123028058524));
#244061=CARTESIAN_POINT('Ctrl Pts',(0.190499999999791,60.7712750142,3.36146460586396));
#244062=CARTESIAN_POINT('Ctrl Pts',(0.190499999999794,60.7265095085055,
3.23423045308419));
#244063=CARTESIAN_POINT('Ctrl Pts',(0.317499999999793,60.8610688070709,
3.36123028058524));
#244064=CARTESIAN_POINT('Ctrl Pts',(0.190499999999793,60.8610688070709,
3.36123028058524));
#244065=CARTESIAN_POINT('Ctrl Pts',(0.190499999999793,60.8610688070709,
3.23423028058524));
#244066=CARTESIAN_POINT('Origin',(0.317499999999794,60.5311086139136,3.42473028058523));
#244067=CARTESIAN_POINT('Origin',(0.317500000301406,60.4497583469877,3.56563113524828));
#244068=CARTESIAN_POINT('Origin',(-6.73632490863879,61.0544000815117,3.5664765390945));
#244069=CARTESIAN_POINT('Origin',(-6.74099917687954,61.0983782637177,3.64299466007596));
#244070=CARTESIAN_POINT('Origin',(-6.72777047351144,60.9730100652056,3.42473028058526));
#244071=CARTESIAN_POINT('Ctrl Pts',(-6.7157078966943,60.8636883187846,3.48823028058527));
#244072=CARTESIAN_POINT('Ctrl Pts',(-6.59002106156486,60.8773920302462,
3.48794691941643));
#244073=CARTESIAN_POINT('Ctrl Pts',(-6.60146619279967,60.9862851800406,
3.42473028058528));
#244074=CARTESIAN_POINT('Ctrl Pts',(-6.71111871849844,60.8189169727311,
3.41028005925127));
#244075=CARTESIAN_POINT('Ctrl Pts',(-6.58529244190401,60.8324022194122,
3.40982512231045));
#244076=CARTESIAN_POINT('Ctrl Pts',(-6.5944096847118,60.9191469903184,3.30780486372902));
#244077=CARTESIAN_POINT('Ctrl Pts',(-6.70242508976228,60.7340977611531,
3.36123028058523));
#244078=CARTESIAN_POINT('Ctrl Pts',(-6.57634410736717,60.7472645033899,
3.36099721048488));
#244079=CARTESIAN_POINT('Ctrl Pts',(-6.58104124348246,60.7919547682776,
3.23423045308408));
#244080=CARTESIAN_POINT('Ctrl Pts',(-6.69328024897476,60.6448574988556,
3.36123028058524));
#244081=CARTESIAN_POINT('Ctrl Pts',(-6.56697596826299,60.6581326136906,
3.36123028058524));
#244082=CARTESIAN_POINT('Ctrl Pts',(-6.56697596826298,60.6581326136906,
3.23423028058524));
#244083=CARTESIAN_POINT('Origin',(-6.69328024897475,60.6448574988556,3.23423028058523));
#244084=CARTESIAN_POINT('Origin',(-0.315760701779421,-0.0331877870872973,
3.64303198860263));
#244085=CARTESIAN_POINT('Origin',(-6.78290064323581,61.4975385923864,3.64303198860306));
#244086=CARTESIAN_POINT('Origin',(-0.315760701779421,-0.0331877870872945,
3.23423028058481));
#244087=CARTESIAN_POINT('Origin',(-6.67747469700966,60.4944777170595,3.23423028058524));
#244088=CARTESIAN_POINT('Ctrl Pts',(-6.83973663030281,62.0330459552234,
3.47153072139115));
#244089=CARTESIAN_POINT('Ctrl Pts',(-6.71274550335253,62.0468640234021,
3.47182327902705));
#244090=CARTESIAN_POINT('Ctrl Pts',(-6.70161199370846,61.9391074687687,
3.40413028959077));
#244091=CARTESIAN_POINT('Ctrl Pts',(-6.82760205123568,61.9187065474467,
3.65553807120999));
#244092=CARTESIAN_POINT('Ctrl Pts',(-6.70071032543994,61.932354465303,3.65586275496994));
#244093=CARTESIAN_POINT('Ctrl Pts',(-6.69200045921793,61.8476598279012,
3.55128126837326));
#244094=CARTESIAN_POINT('Ctrl Pts',(-6.80580199871472,61.7133000470648,
3.77003198860307));
#244095=CARTESIAN_POINT('Ctrl Pts',(-6.67910652125809,61.7268034525367,
3.77025505748508));
#244096=CARTESIAN_POINT('Ctrl Pts',(-6.67473372828963,61.6833778591512,
3.64284211731167));
#244097=CARTESIAN_POINT('Ctrl Pts',(-6.78290064323581,61.4975385923864,
3.77003198860306));
#244098=CARTESIAN_POINT('Ctrl Pts',(-6.65640766978556,61.5108335396274,
3.77003198860306));
#244099=CARTESIAN_POINT('Ctrl Pts',(-6.65659650326273,61.5108136924291,
3.64284239821755));
#244100=CARTESIAN_POINT('Origin',(-6.8279329755337,61.9259926140921,3.40423097483353));
#244101=CARTESIAN_POINT('Ctrl Pts',(-6.67747469700966,60.4944777170595,
3.36123028058524));
#244102=CARTESIAN_POINT('Ctrl Pts',(-6.55117041629789,60.5077528318945,
3.36123028058524));
#244103=CARTESIAN_POINT('Ctrl Pts',(-6.55117041629789,60.5077528318945,
3.23423028058524));
#244104=CARTESIAN_POINT('Ctrl Pts',(-6.66829952659951,60.4049357747552,
3.36123028058523));
#244105=CARTESIAN_POINT('Ctrl Pts',(-6.54175270773032,60.4181493202568,
3.36146538610149));
#244106=CARTESIAN_POINT('Ctrl Pts',(-6.53705760237914,60.3734783767969,
3.23423043688413));
#244107=CARTESIAN_POINT('Ctrl Pts',(-6.65962554481719,60.3202668847284,
3.41054258693142));
#244108=CARTESIAN_POINT('Ctrl Pts',(-6.53289275205069,60.333852472875,3.41100608859868));
#244109=CARTESIAN_POINT('Ctrl Pts',(-6.52371293062573,60.246512306213,3.30819866970914));
#244110=CARTESIAN_POINT('Ctrl Pts',(-6.65505462397415,60.275645989912,3.48823028058522));
#244111=CARTESIAN_POINT('Ctrl Pts',(-6.52822907310798,60.2894805317163,
3.488520042123));
#244112=CARTESIAN_POINT('Ctrl Pts',(-6.51668018436767,60.1796001951997,
3.42473028058522));
#244113=CARTESIAN_POINT('Origin',(-6.64298446507943,60.1663250803647,3.42473028058523));
#244114=CARTESIAN_POINT('Origin',(-6.8465546283654,62.1031658061152,3.11913648178458));
#244115=CARTESIAN_POINT('Origin',(-6.86517628122531,62.2803389979221,2.83404198860306));
#244116=CARTESIAN_POINT('Origin',(-6.63448104656892,60.0854204576118,3.56563113460873));
#244117=CARTESIAN_POINT('Origin',(-6.62985850077851,60.0409538388298,3.6429917172183));
#244118=CARTESIAN_POINT('Ctrl Pts',(-6.59568250079906,62.6076796697356,
2.59908173516068));
#244119=CARTESIAN_POINT('Ctrl Pts',(-6.59177408464795,62.5705801176611,
2.65878198860306));
#244120=CARTESIAN_POINT('Ctrl Pts',(-6.58439859103049,62.5005702980932,
2.65878198860306));
#244121=CARTESIAN_POINT('Ctrl Pts',(-6.68331293653974,62.5984477290804,
2.59908193475628));
#244122=CARTESIAN_POINT('Ctrl Pts',(-6.65560500345282,62.5638523220918,
2.65878715325384));
#244123=CARTESIAN_POINT('Ctrl Pts',(-6.63512154272671,62.4952175264277,
2.65878198860306));
#244124=CARTESIAN_POINT('Ctrl Pts',(-6.76155265492276,62.5650504549419,
2.63878778849935));
#244125=CARTESIAN_POINT('Ctrl Pts',(-6.71196843232432,62.5346567608582,
2.69564460180145));
#244126=CARTESIAN_POINT('Ctrl Pts',(-6.6793077633958,62.4653998062674,2.68180481624927));
#244127=CARTESIAN_POINT('Ctrl Pts',(-6.86003002196296,62.4816328770703,
2.7544323887867));
#244128=CARTESIAN_POINT('Ctrl Pts',(-6.76863258245071,62.4676069047251,
2.79268340777157));
#244129=CARTESIAN_POINT('Ctrl Pts',(-6.73311104631486,62.3866783619501,
2.74885926835654));
#244130=CARTESIAN_POINT('Ctrl Pts',(-6.88172985342186,62.4326191774619,
2.82856655361726));
#244131=CARTESIAN_POINT('Ctrl Pts',(-6.76853939445094,62.4292062449167,
2.85384197230834));
#244132=CARTESIAN_POINT('Ctrl Pts',(-6.74362530798282,62.3388388123828,
2.79184624278531));
#244133=CARTESIAN_POINT('Ctrl Pts',(-6.87697683366585,62.3873926810693,
2.90134173516067));
#244134=CARTESIAN_POINT('Ctrl Pts',(-6.75017837817622,62.401187110497,2.90163218716435));
#244135=CARTESIAN_POINT('Ctrl Pts',(-6.73887200051354,62.2936141127571,
2.83404198860306));
#244136=CARTESIAN_POINT('Origin',(-6.58439859103049,62.5005702980932,2.53178198860305));
#244137=CARTESIAN_POINT('Origin',(-0.315760701779421,-0.0331877870872973,
3.64303198860263));
#244138=CARTESIAN_POINT('Origin',(-6.58785426247116,59.6417962403144,3.64303198860304));
#244139=CARTESIAN_POINT('Origin',(-1.29720108988942E-17,1.91413448435235E-13,
2.53178198860262));
#244140=CARTESIAN_POINT('Origin',(-6.55408556365967,62.5037563256536,2.53178198860305));
#244141=CARTESIAN_POINT('Ctrl Pts',(-6.58785426247116,59.6417962403144,
3.77003198860305));
#244142=CARTESIAN_POINT('Ctrl Pts',(-6.46136077224333,59.6550912418709,
3.77003198860305));
#244143=CARTESIAN_POINT('Ctrl Pts',(-6.46155012326944,59.6550713402761,
3.64284187937076));
#244144=CARTESIAN_POINT('Ctrl Pts',(-6.56494565834896,59.4260321009471,
3.77003198860305));
#244145=CARTESIAN_POINT('Ctrl Pts',(-6.43870097938028,59.4394927947741,
3.76980208962928));
#244146=CARTESIAN_POINT('Ctrl Pts',(-6.44341257746682,59.4825041216641,
3.64284193928295));
#244147=CARTESIAN_POINT('Ctrl Pts',(-6.54313468201896,59.2206282517278,
3.65553535416626));
#244148=CARTESIAN_POINT('Ctrl Pts',(-6.41712387096215,59.2341955513573,
3.6552005783464));
#244149=CARTESIAN_POINT('Ctrl Pts',(-6.4261459750101,59.3182233753711,3.55127910964297));
#244150=CARTESIAN_POINT('Ctrl Pts',(-6.53099325080075,59.1062911958298,
3.47153072139114));
#244151=CARTESIAN_POINT('Ctrl Pts',(-6.4051226264057,59.1200087130391,3.47122746281624));
#244152=CARTESIAN_POINT('Ctrl Pts',(-6.41653455832046,59.2267768553867,
3.40413045901309));
#244153=CARTESIAN_POINT('Origin',(-6.54282188406247,59.2133417798938,3.40423097483351));
#244154=CARTESIAN_POINT('Ctrl Pts',(-6.2443699078808,62.4538823482277,2.90134173516068));
#244155=CARTESIAN_POINT('Ctrl Pts',(-6.37126553604091,62.441012455002,2.90163218716435));
#244156=CARTESIAN_POINT('Ctrl Pts',(-6.35995915837823,62.3334394572621,
2.83404198860306));
#244157=CARTESIAN_POINT('Ctrl Pts',(-6.2491260434095,62.4991292864734,2.82853349835389));
#244158=CARTESIAN_POINT('Ctrl Pts',(-6.35912437831714,62.4722545055302,
2.85381483162355));
#244159=CARTESIAN_POINT('Ctrl Pts',(-6.36471463173889,62.3786847639678,
2.79182701594274));
#244160=CARTESIAN_POINT('Ctrl Pts',(-6.28053011789765,62.5423796567684,
2.75468822073702));
#244161=CARTESIAN_POINT('Ctrl Pts',(-6.36708533499892,62.5096946965653,
2.79286913083867));
#244162=CARTESIAN_POINT('Ctrl Pts',(-6.38493060453728,62.423112487203,2.74900763297952));
#244163=CARTESIAN_POINT('Ctrl Pts',(-6.39322569848903,62.6032845425348,
2.63954450640421));
#244164=CARTESIAN_POINT('Ctrl Pts',(-6.435760068245,62.5632890102009,2.69627684028913));
#244165=CARTESIAN_POINT('Ctrl Pts',(-6.45334792019218,62.4886705126497,
2.6822435603654));
#244166=CARTESIAN_POINT('Ctrl Pts',(-6.47739243510518,62.6200908675654,
2.59908178706386));
#244167=CARTESIAN_POINT('Ctrl Pts',(-6.49734694408372,62.5804859237138,
2.65878704321526));
#244168=CARTESIAN_POINT('Ctrl Pts',(-6.50319024212541,62.5090840872034,
2.65878198860306));
#244169=CARTESIAN_POINT('Ctrl Pts',(-6.56531752495323,62.6108711573007,
2.59908173516068));
#244170=CARTESIAN_POINT('Ctrl Pts',(-6.56142710223373,62.5737697140404,
2.65878198860306));
#244171=CARTESIAN_POINT('Ctrl Pts',(-6.55408556365967,62.5037563256536,
2.65878198860306));
#244172=CARTESIAN_POINT('Origin',(-6.23365487766645,62.3467145720971,2.83404198860306));
#244173=CARTESIAN_POINT('Origin',(-6.52420020557968,59.0361683443311,3.11913648167141));
#244174=CARTESIAN_POINT('Origin',(-6.50557852713774,58.8589949086132,2.83404198860304));
#244175=CARTESIAN_POINT('Origin',(-6.21503322485406,62.1695413802722,3.11913648177653));
#244176=CARTESIAN_POINT('Origin',(-6.19641157197484,61.9923681882671,3.40423097483353));
#244177=CARTESIAN_POINT('Ctrl Pts',(-6.4937464611276,58.751944703909,2.90134173516065));
#244178=CARTESIAN_POINT('Ctrl Pts',(-6.36806742857345,58.7656442740272,
2.90103711553271));
#244179=CARTESIAN_POINT('Ctrl Pts',(-6.37927424642597,58.8722700234482,
2.83404198860304));
#244180=CARTESIAN_POINT('Ctrl Pts',(-6.48899657309077,58.7067576262548,
2.82862991747987));
#244181=CARTESIAN_POINT('Ctrl Pts',(-6.38004220452892,58.7342098038493,
2.85314045886452));
#244182=CARTESIAN_POINT('Ctrl Pts',(-6.37452469054063,58.8270810177594,
2.79187960999977));
#244183=CARTESIAN_POINT('Ctrl Pts',(-6.45774144355337,58.6637560248476,
2.75470625793387));
#244184=CARTESIAN_POINT('Ctrl Pts',(-6.37187117938144,58.6967899354331,
2.79224250381965));
#244185=CARTESIAN_POINT('Ctrl Pts',(-6.3543526691279,58.7829167175853,2.749018091083));
#244186=CARTESIAN_POINT('Ctrl Pts',(-6.34539908016339,58.6035914159082,
2.6394786831172));
#244187=CARTESIAN_POINT('Ctrl Pts',(-6.30313135363873,58.6436439608619,
2.69595066767937));
#244188=CARTESIAN_POINT('Ctrl Pts',(-6.2859587457653,58.718133717619,2.68220539436104));
#244189=CARTESIAN_POINT('Ctrl Pts',(-6.26151010025748,58.5872698677177,
2.59908178585244));
#244190=CARTESIAN_POINT('Ctrl Pts',(-6.24170554357565,58.6268645946703,
2.65877670944895));
#244191=CARTESIAN_POINT('Ctrl Pts',(-6.23613328458301,58.6982323944376,
2.65878198860303));
#244192=CARTESIAN_POINT('Ctrl Pts',(-6.1740349085904,58.5964866834552,2.59908173516065));
#244193=CARTESIAN_POINT('Ctrl Pts',(-6.17794390662191,58.6335861742244,
2.65878198860303));
#244194=CARTESIAN_POINT('Ctrl Pts',(-6.18532049829418,58.7035958781041,
2.65878198860303));
#244195=CARTESIAN_POINT('Origin',(-6.18532049829418,58.7035958781041,2.53178198860303));
#244196=CARTESIAN_POINT('Ctrl Pts',(-6.15137923967696,61.5639141665613,
3.77003198860306));
#244197=CARTESIAN_POINT('Ctrl Pts',(-6.27787222402482,61.550619218175,3.77003198860306));
#244198=CARTESIAN_POINT('Ctrl Pts',(-6.2776833796338,61.5506390665203,3.64284238727629));
#244199=CARTESIAN_POINT('Ctrl Pts',(-6.1738380120536,61.7797255331388,3.77003198860307));
#244200=CARTESIAN_POINT('Ctrl Pts',(-6.30057242039907,61.7665923920111,
3.77025506105846));
#244201=CARTESIAN_POINT('Ctrl Pts',(-6.29582088597906,61.7232059145522,
3.64284210641876));
#244202=CARTESIAN_POINT('Ctrl Pts',(-6.19522058691297,61.9851742714892,
3.65553527987877));
#244203=CARTESIAN_POINT('Ctrl Pts',(-6.32217699854561,61.9721416759944,
3.65585996533129));
#244204=CARTESIAN_POINT('Ctrl Pts',(-6.31308747966707,61.887486582018,3.55127902710258));
#244205=CARTESIAN_POINT('Ctrl Pts',(-6.20712349654484,62.099536274866,3.47153072139116));
#244206=CARTESIAN_POINT('Ctrl Pts',(-6.33421251157735,62.0866494440661,
3.47182327905233));
#244207=CARTESIAN_POINT('Ctrl Pts',(-6.3226988678919,61.9789328337399,3.40413028378025));
#244208=CARTESIAN_POINT('Origin',(-6.15137923967696,61.5639141665613,3.64303198860306));
#244209=CARTESIAN_POINT('Origin',(4.05837671390568E-16,1.91635770661944E-13,
2.53178198860262));
#244210=CARTESIAN_POINT('Origin',(-6.15500747092336,58.7067819056644,2.53178198860303));
#244211=CARTESIAN_POINT('Origin',(0.995615674755347,-6.43520020182062,3.64303198860258));
#244212=CARTESIAN_POINT('Origin',(-6.10937495961934,61.1647646440485,3.64299466007523));
#244213=CARTESIAN_POINT('Ctrl Pts',(-6.14377718965342,58.599666897865,2.59908173516065));
#244214=CARTESIAN_POINT('Ctrl Pts',(-6.1476670304619,58.6367684021394,2.65878198860303));
#244215=CARTESIAN_POINT('Ctrl Pts',(-6.15500747092336,58.7067819056644,
2.65878198860303));
#244216=CARTESIAN_POINT('Ctrl Pts',(-6.05659553606712,58.6088074259633,
2.59908193199927));
#244217=CARTESIAN_POINT('Ctrl Pts',(-6.08415140319808,58.6434243604378,
2.65877685806593));
#244218=CARTESIAN_POINT('Ctrl Pts',(-6.10436324506824,58.7120821529689,
2.65878198860303));
#244219=CARTESIAN_POINT('Ctrl Pts',(-5.97852000021548,58.6416817365141,
2.63872492669843));
#244220=CARTESIAN_POINT('Ctrl Pts',(-6.02785839131291,58.6721826510723,
2.69532212015316));
#244221=CARTESIAN_POINT('Ctrl Pts',(-6.06008468706722,58.74140381955,2.68176836726669));
#244222=CARTESIAN_POINT('Ctrl Pts',(-5.8802509339248,58.7242744516465,2.75442176402287));
#244223=CARTESIAN_POINT('Ctrl Pts',(-5.97104363802158,58.7387860695145,
2.79203179920173));
#244224=CARTESIAN_POINT('Ctrl Pts',(-6.00614981441032,58.8193360415243,
2.74885310748223));
#244225=CARTESIAN_POINT('Ctrl Pts',(-5.85862682030282,58.7730316211509,
2.82866089558445));
#244226=CARTESIAN_POINT('Ctrl Pts',(-5.97091547255964,58.7772266151799,
2.85316563119314));
#244227=CARTESIAN_POINT('Ctrl Pts',(-5.99561386571444,58.8669255556785,
2.79189751796691));
#244228=CARTESIAN_POINT('Ctrl Pts',(-5.863373641496,58.8181995570487,2.90134173516065));
#244229=CARTESIAN_POINT('Ctrl Pts',(-5.98915458643814,58.8054696185322,
2.90103711553271));
#244230=CARTESIAN_POINT('Ctrl Pts',(-6.00036140429066,58.9120953679532,
2.83404198860303));
#244231=CARTESIAN_POINT('Origin',(-5.87405712357889,58.9253704827882,2.83404198860304));
#244232=CARTESIAN_POINT('Origin',(-6.10480350526266,61.1207756545815,3.56647653971801));
#244233=CARTESIAN_POINT('Origin',(-6.09624906995259,61.0393856393806,3.42473028058528));
#244234=CARTESIAN_POINT('Origin',(-5.89267880207494,59.102543918484,3.11913648168155));
#244235=CARTESIAN_POINT('Origin',(-5.91130048050362,59.2797173540687,3.40423097483352));
#244236=CARTESIAN_POINT('Ctrl Pts',(-6.0617588454159,60.7112330730305,3.36123028058524));
#244237=CARTESIAN_POINT('Ctrl Pts',(-6.18806312612767,60.6979579581956,
3.36123028058524));
#244238=CARTESIAN_POINT('Ctrl Pts',(-6.18806312612767,60.6979579581955,
3.23423028058524));
#244239=CARTESIAN_POINT('Ctrl Pts',(-6.0714004111828,60.8007259828527,3.36123028058523));
#244240=CARTESIAN_POINT('Ctrl Pts',(-6.19746294737662,60.7873912833601,
3.36099641108498));
#244241=CARTESIAN_POINT('Ctrl Pts',(-6.2021759387818,60.8322324012611,3.23423043688417));
#244242=CARTESIAN_POINT('Ctrl Pts',(-6.08051542067558,60.8853484607272,
3.41054258905327));
#244243=CARTESIAN_POINT('Ctrl Pts',(-6.20639551966748,60.8723790316521,
3.41008815825964));
#244244=CARTESIAN_POINT('Ctrl Pts',(-6.2155206071494,60.9591984396311,3.30819867304283));
#244245=CARTESIAN_POINT('Ctrl Pts',(-6.08531878138341,60.9299448846692,
3.48823028058526));
#244246=CARTESIAN_POINT('Ctrl Pts',(-6.21110821942955,60.9172173747512,
3.48794691941642));
#244247=CARTESIAN_POINT('Ctrl Pts',(-6.22255335066436,61.0261105245456,
3.42473028058527));
#244248=CARTESIAN_POINT('Origin',(-6.0617588454159,60.7112330730305,3.23423028058524));
#244249=CARTESIAN_POINT('Ctrl Pts',(-5.90061356181277,59.1725467709679,
3.47153072139113));
#244250=CARTESIAN_POINT('Ctrl Pts',(-6.02658562874803,59.1597945546414,
3.47122746285117));
#244251=CARTESIAN_POINT('Ctrl Pts',(-6.0376214331677,59.2666022171587,3.40413046676841));
#244252=CARTESIAN_POINT('Ctrl Pts',(-5.91250964036455,59.2869113614507,
3.65553813458027));
#244253=CARTESIAN_POINT('Ctrl Pts',(-6.03858760028769,59.2739830624797,
3.65520336072141));
#244254=CARTESIAN_POINT('Ctrl Pts',(-6.0472329950892,59.3580501215762,3.55128134519959));
#244255=CARTESIAN_POINT('Ctrl Pts',(-5.9338813165692,59.4923630227876,3.77003198860305));
#244256=CARTESIAN_POINT('Ctrl Pts',(-6.06016587018168,59.479281816836,3.76980209314187));
#244257=CARTESIAN_POINT('Ctrl Pts',(-6.06449973388402,59.522332169772,3.64284195387442));
#244258=CARTESIAN_POINT('Ctrl Pts',(-5.9563328589123,59.7081718144894,3.77003198860305));
#244259=CARTESIAN_POINT('Ctrl Pts',(-6.08282633453069,59.6948768144684,
3.77003198860305));
#244260=CARTESIAN_POINT('Ctrl Pts',(-6.08263699813586,59.6948967145254,
3.64284189403867));
#244261=CARTESIAN_POINT('Origin',(-5.9563328589123,59.7081718144894,3.64303198860304));
#244262=CARTESIAN_POINT('Origin',(0.97914764405288,-6.27851735587403,3.23423028058477));
#244263=CARTESIAN_POINT('Origin',(-6.04595329345081,60.5608532912345,3.23423028058524));
#244264=CARTESIAN_POINT('Origin',(0.9765688230087,-6.25398151259745,3.64303198860258));
#244265=CARTESIAN_POINT('Origin',(-5.99823604520139,60.1073400339999,3.64299171721827));
#244266=CARTESIAN_POINT('Ctrl Pts',(-6.02238575970296,60.3421421670677,
3.48823028058523));
#244267=CARTESIAN_POINT('Ctrl Pts',(-6.14931623097267,60.3293058762213,
3.48852004212301));
#244268=CARTESIAN_POINT('Ctrl Pts',(-6.13776734223235,60.2194255397047,
3.42473028058523));
#244269=CARTESIAN_POINT('Ctrl Pts',(-6.02720817145212,60.386889039093,3.41028005848448));
#244270=CARTESIAN_POINT('Ctrl Pts',(-6.15399567477082,60.3738278099536,
3.41074404220489));
#244271=CARTESIAN_POINT('Ctrl Pts',(-6.1448238529486,60.2865637544341,3.30780486244054));
#244272=CARTESIAN_POINT('Ctrl Pts',(-6.03634362557923,60.4716618705783,
3.36123028058524));
#244273=CARTESIAN_POINT('Ctrl Pts',(-6.16287156698234,60.4582762833179,
3.36146460586411));
#244274=CARTESIAN_POINT('Ctrl Pts',(-6.15819229746487,60.413756007748,3.23423045308427));
#244275=CARTESIAN_POINT('Ctrl Pts',(-6.04595329345081,60.5608532912345,
3.36123028058524));
#244276=CARTESIAN_POINT('Ctrl Pts',(-6.17225757416258,60.5475781763995,
3.36123028058524));
#244277=CARTESIAN_POINT('Ctrl Pts',(-6.17225757416258,60.5475781763995,
3.23423028058524));
#244278=CARTESIAN_POINT('Origin',(-6.01146306152058,60.2327006545397,3.42473028058522));
#244279=CARTESIAN_POINT('Origin',(-6.00295964283336,60.1517960329196,3.56563113524853));
#244280=CARTESIAN_POINT('Origin',(-13.0813452322045,60.0157999988659,3.5664765390947));
#244281=CARTESIAN_POINT('Origin',(-13.0905908661195,60.0590486699126,3.64299466007543));
#244282=CARTESIAN_POINT('Origin',(-13.0643300858384,59.9357500275434,3.42473028058525));
#244283=CARTESIAN_POINT('Ctrl Pts',(-13.0409063549241,59.8282880397056,
3.48823028058526));
#244284=CARTESIAN_POINT('Ctrl Pts',(-12.9173404733285,59.855054532531,3.48794691941642));
#244285=CARTESIAN_POINT('Ctrl Pts',(-12.9401053405452,59.9621548122773,
3.42473028058527));
#244286=CARTESIAN_POINT('Ctrl Pts',(-13.0316624367251,59.7842416555147,
3.41028005925126));
#244287=CARTESIAN_POINT('Ctrl Pts',(-12.9079350417501,59.8108054559368,
3.40982512231019));
#244288=CARTESIAN_POINT('Ctrl Pts',(-12.9260696369491,59.8961220185315,
3.30780486372868));
#244289=CARTESIAN_POINT('Ctrl Pts',(-13.0141504107549,59.7007958241046,
3.36123028058523));
#244290=CARTESIAN_POINT('Ctrl Pts',(-12.8901364125053,59.7270694888855,
3.36099721048454));
#244291=CARTESIAN_POINT('Ctrl Pts',(-12.8994792219294,59.7710239514062,
3.2342304530839));
#244292=CARTESIAN_POINT('Ctrl Pts',(-12.9957275188826,59.6130003254556,
3.36123028058523));
#244293=CARTESIAN_POINT('Ctrl Pts',(-12.8715027735894,59.6394051101895,
3.36123028058523));
#244294=CARTESIAN_POINT('Ctrl Pts',(-12.8715027735894,59.6394051101895,
3.23423028058523));
#244295=CARTESIAN_POINT('Origin',(-12.9957275188826,59.6130003254556,3.23423028058522));
#244296=CARTESIAN_POINT('Origin',(-0.310561863232978,-0.066011961834456,
3.64303198860263));
#244297=CARTESIAN_POINT('Origin',(-13.1739864076109,60.451642460649,3.64303198860305));
#244298=CARTESIAN_POINT('Origin',(-0.310561863232978,-0.0660119618344531,
3.23423028058481));
#244299=CARTESIAN_POINT('Origin',(-12.9642895838873,59.4650964698968,3.23423028058523));
#244300=CARTESIAN_POINT('Ctrl Pts',(-13.2864868028998,60.9782752797349,
3.47153072139114));
#244301=CARTESIAN_POINT('Ctrl Pts',(-13.1616357280625,61.005291838439,3.47182327902704));
#244302=CARTESIAN_POINT('Ctrl Pts',(-13.1392995818862,60.8992893541408,
3.40413028959089));
#244303=CARTESIAN_POINT('Ctrl Pts',(-13.2624669757411,60.8658306440997,
3.65553807120998));
#244304=CARTESIAN_POINT('Ctrl Pts',(-13.1376969719796,60.8926675943329,
3.65586275497022));
#244305=CARTESIAN_POINT('Ctrl Pts',(-13.1201818190176,60.8093473519467,
3.55128126837324));
#244306=CARTESIAN_POINT('Ctrl Pts',(-13.2193155203587,60.6638281080081,
3.77003198860305));
#244307=CARTESIAN_POINT('Ctrl Pts',(-13.0947255842073,60.690500823973,3.77025505748489));
#244308=CARTESIAN_POINT('Ctrl Pts',(-13.0858375353125,60.6477702018628,
3.64284211731156));
#244309=CARTESIAN_POINT('Ctrl Pts',(-13.1739864076109,60.451642460649,3.77003198860306));
#244310=CARTESIAN_POINT('Ctrl Pts',(-13.049576076309,60.4780866929068,3.77003198860306));
#244311=CARTESIAN_POINT('Ctrl Pts',(-13.0497618007392,60.4780472159605,
3.64284239821778));
#244312=CARTESIAN_POINT('Origin',(-13.2635576885504,60.8730422059015,3.40423097483352));
#244313=CARTESIAN_POINT('Ctrl Pts',(-12.9642895838873,59.4650964698968,
3.36123028058523));
#244314=CARTESIAN_POINT('Ctrl Pts',(-12.8400648385941,59.4915012546306,
3.36123028058523));
#244315=CARTESIAN_POINT('Ctrl Pts',(-12.8400648385941,59.4915012546306,
3.23423028058523));
#244316=CARTESIAN_POINT('Ctrl Pts',(-12.9458049943933,59.3770041141846,
3.36123028058523));
#244317=CARTESIAN_POINT('Ctrl Pts',(-12.8213326038438,59.4033730190078,
3.36146538610137));
#244318=CARTESIAN_POINT('Ctrl Pts',(-12.8119938336987,59.3594375597966,
3.23423043688395));
#244319=CARTESIAN_POINT('Ctrl Pts',(-12.9283282206289,59.2937057271827,
3.4105425869314));
#244320=CARTESIAN_POINT('Ctrl Pts',(-12.8037097640135,59.3204640761313,
3.41100608859929));
#244321=CARTESIAN_POINT('Ctrl Pts',(-12.7854506972092,59.2345619206681,
3.30819866970998));
#244322=CARTESIAN_POINT('Ctrl Pts',(-12.9191181862048,59.2498070616281,
3.48823028058521));
#244323=CARTESIAN_POINT('Ctrl Pts',(-12.794433502371,59.2768226962999,3.48852004212299));
#244324=CARTESIAN_POINT('Ctrl Pts',(-12.7714622569322,59.1687514833562,
3.42473028058521));
#244325=CARTESIAN_POINT('Origin',(-12.8956870022254,59.1423466986223,3.42473028058522));
#244326=CARTESIAN_POINT('Origin',(-13.300596971516,61.0472983318851,3.1191364817838));
#244327=CARTESIAN_POINT('Origin',(-13.3376362544828,61.221554457654,2.83404198860304));
#244328=CARTESIAN_POINT('Origin',(-12.8787733304452,59.0627741291259,3.56563113460799));
#244329=CARTESIAN_POINT('Origin',(-12.8695280801149,59.0190342907436,3.64299171721817));
#244330=CARTESIAN_POINT('Ctrl Pts',(-13.103835206573,61.5752716937453,2.59908173516067));
#244331=CARTESIAN_POINT('Ctrl Pts',(-13.0960702419682,61.5387839176329,
2.65878198860306));
#244332=CARTESIAN_POINT('Ctrl Pts',(-13.0814171332235,61.4699285681956,
2.65878198860305));
#244333=CARTESIAN_POINT('Ctrl Pts',(-13.1900205930482,61.5569304518442,
2.59908193475517));
#244334=CARTESIAN_POINT('Ctrl Pts',(-13.1588482421902,61.5254208297847,
2.65878715325409));
#244335=CARTESIAN_POINT('Ctrl Pts',(-13.1313027022865,61.4593031273797,
2.65878198860305));
#244336=CARTESIAN_POINT('Ctrl Pts',(-13.2643407403244,61.515537853938,2.63878778849929));
#244337=CARTESIAN_POINT('Ctrl Pts',(-13.2118511391497,61.4904936222811,
2.69564460180163));
#244338=CARTESIAN_POINT('Ctrl Pts',(-13.1721300657491,61.4250300340664,
2.68180481624929));
#244339=CARTESIAN_POINT('Ctrl Pts',(-13.3535591268197,61.4222835584428,
2.75443238878675));
#244340=CARTESIAN_POINT('Ctrl Pts',(-13.2611962587093,61.4178880557408,
2.79268340777125));
#244341=CARTESIAN_POINT('Ctrl Pts',(-13.2174099770541,61.3411158595758,
2.74885926835651));
#244342=CARTESIAN_POINT('Ctrl Pts',(-13.3700167576322,61.3712701109737,
2.82856655361722));
#244343=CARTESIAN_POINT('Ctrl Pts',(-13.2570896192445,61.3797074995631,
2.8538419723086));
#244344=CARTESIAN_POINT('Ctrl Pts',(-13.2228660458969,61.292439340452,2.79184624278546));
#244345=CARTESIAN_POINT('Ctrl Pts',(-13.3605623192489,61.3267881959114,
2.90134173516065));
#244346=CARTESIAN_POINT('Ctrl Pts',(-13.2359003894753,61.3537611057084,
2.90163218716433));
#244347=CARTESIAN_POINT('Ctrl Pts',(-13.2134115091896,61.2479592423879,
2.83404198860304));
#244348=CARTESIAN_POINT('Origin',(-13.0814171332235,61.4699285681956,2.53178198860305));
#244349=CARTESIAN_POINT('Origin',(-0.310561863232978,-0.066011961834456,
3.64303198860263));
#244350=CARTESIAN_POINT('Origin',(-12.7860306150453,58.6264539577985,3.64303198860303));
#244351=CARTESIAN_POINT('Origin',(4.07480739540194E-18,1.9141614838601E-13,
2.53178198860262));
#244352=CARTESIAN_POINT('Origin',(-13.0516031943531,61.4762657165317,2.53178198860305));
#244353=CARTESIAN_POINT('Ctrl Pts',(-12.7860306150453,58.6264539577985,
3.77003198860304));
#244354=CARTESIAN_POINT('Ctrl Pts',(-12.6616197754742,58.6528982980922,
3.77003198860304));
#244355=CARTESIAN_POINT('Ctrl Pts',(-12.6618060089323,58.6528587129487,
3.64284187937092));
#244356=CARTESIAN_POINT('Ctrl Pts',(-12.7406940127365,58.414266398147,3.77003198860304));
#244357=CARTESIAN_POINT('Ctrl Pts',(-12.6165479409684,58.4408495151706,
3.76980208962871));
#244358=CARTESIAN_POINT('Ctrl Pts',(-12.6257296363315,58.4831327254065,
3.64284193928292));
#244359=CARTESIAN_POINT('Ctrl Pts',(-12.6975319705105,58.2122676405433,
3.65553535416627));
#244360=CARTESIAN_POINT('Ctrl Pts',(-12.5736296288415,58.2389323335244,
3.65520057834584));
#244361=CARTESIAN_POINT('Ctrl Pts',(-12.5913856081751,58.3215567776511,
3.55127910964328));
#244362=CARTESIAN_POINT('Ctrl Pts',(-12.6735055745743,58.0998260601481,
3.47153072139113));
#244363=CARTESIAN_POINT('Ctrl Pts',(-12.5497583536236,58.1266254943014,
3.47122746281623));
#244364=CARTESIAN_POINT('Ctrl Pts',(-12.5722680796266,58.2316158778878,
3.40413045901317));
#244365=CARTESIAN_POINT('Origin',(-12.6964592423895,58.2050537810543,3.40423097483351));
#244366=CARTESIAN_POINT('Ctrl Pts',(-12.7383709431253,61.459039055521,2.90134173516066));
#244367=CARTESIAN_POINT('Ctrl Pts',(-12.8632261535957,61.43297545991,2.90163218716434));
#244368=CARTESIAN_POINT('Ctrl Pts',(-12.84073727331,61.3271735965895,2.83404198860304));
#244369=CARTESIAN_POINT('Ctrl Pts',(-12.7478306169676,61.503540974767,2.82853349835378));
#244370=CARTESIAN_POINT('Ctrl Pts',(-12.8544171899352,61.4653154597768,
2.85381483162427));
#244371=CARTESIAN_POINT('Ctrl Pts',(-12.8501961180702,61.371673962449,2.79182701594335));
#244372=CARTESIAN_POINT('Ctrl Pts',(-12.7835835513933,61.5432717953613,
2.75468822073712));
#244373=CARTESIAN_POINT('Ctrl Pts',(-12.8662481012967,61.5017184029585,
2.79286913083838));
#244374=CARTESIAN_POINT('Ctrl Pts',(-12.8749453072905,61.4137451613973,
2.74900763297951));
#244375=CARTESIAN_POINT('Ctrl Pts',(-12.9020280679172,61.5920631419348,
2.6395445064041));
#244376=CARTESIAN_POINT('Ctrl Pts',(-12.940148758413,61.5478406570054,2.69627684028927));
#244377=CARTESIAN_POINT('Ctrl Pts',(-12.9498405053864,61.4717924962547,
2.68224356036539));
#244378=CARTESIAN_POINT('Ctrl Pts',(-12.9874904696724,61.5999795805214,
2.59908178706412));
#244379=CARTESIAN_POINT('Ctrl Pts',(-13.0031958218445,61.5585057825391,
2.65878704321686));
#244380=CARTESIAN_POINT('Ctrl Pts',(-13.0015435854427,61.4868843017926,
2.65878198860305));
#244381=CARTESIAN_POINT('Ctrl Pts',(-13.0739701745327,61.5816197022699,
2.59908173516066));
#244382=CARTESIAN_POINT('Ctrl Pts',(-13.0662229071069,61.545128164506,2.65878198860305));
#244383=CARTESIAN_POINT('Ctrl Pts',(-13.0516031943531,61.4762657165317,
2.65878198860305));
#244384=CARTESIAN_POINT('Origin',(-12.7165125280168,61.3535783813233,2.83404198860304));
#244385=CARTESIAN_POINT('Origin',(-12.6594199084583,58.0307974155462,3.1191364816706));
#244386=CARTESIAN_POINT('Origin',(-12.6223805745521,57.8565410498768,2.83404198860303));
#244387=CARTESIAN_POINT('Origin',(-12.6794732450929,61.1793222555332,3.11913648177642));
#244388=CARTESIAN_POINT('Origin',(-12.6424339620844,61.0050661295708,3.40423097483352));
#244389=CARTESIAN_POINT('Ctrl Pts',(-12.5994235324474,57.7513140650721,
2.90134173516064));
#244390=CARTESIAN_POINT('Ctrl Pts',(-12.4758649777955,57.7780756236497,
2.9010371155327));
#244391=CARTESIAN_POINT('Ctrl Pts',(-12.4981558292589,57.8829458346107,
2.83404198860303));
#244392=CARTESIAN_POINT('Ctrl Pts',(-12.5899763290073,57.7068710254546,
2.82862991748001));
#244393=CARTESIAN_POINT('Ctrl Pts',(-12.4844883578139,57.7455616498605,
2.85314045886469));
#244394=CARTESIAN_POINT('Ctrl Pts',(-12.4887087546166,57.8385008428016,
2.79187960999965));
#244395=CARTESIAN_POINT('Ctrl Pts',(-12.5543975270268,57.6673720419788,
2.75470625793368));
#244396=CARTESIAN_POINT('Ctrl Pts',(-12.4724506530562,57.7092008760992,
2.79224250381918));
#244397=CARTESIAN_POINT('Ctrl Pts',(-12.4640308112191,57.7966870296831,
2.74901809108302));
#244398=CARTESIAN_POINT('Ctrl Pts',(-12.4363816727425,57.6192799956675,
2.63947868311738));
#244399=CARTESIAN_POINT('Ctrl Pts',(-12.39853212422,57.6635313090894,2.69595066767966));
#244400=CARTESIAN_POINT('Ctrl Pts',(-12.3892398894927,57.7394080294761,
2.682205394361));
#244401=CARTESIAN_POINT('Ctrl Pts',(-12.3512461790954,57.6118166447798,
2.59908178585153));
#244402=CARTESIAN_POINT('Ctrl Pts',(-12.3356888898091,57.6532646075497,
2.65877670944829));
#244403=CARTESIAN_POINT('Ctrl Pts',(-12.3376071226707,57.7248239067131,
2.65878198860303));
#244404=CARTESIAN_POINT('Ctrl Pts',(-12.2652136052663,57.6301266171959,
2.59908173516064));
#244405=CARTESIAN_POINT('Ctrl Pts',(-12.2729791421557,57.6666142715156,
2.65878198860303));
#244406=CARTESIAN_POINT('Ctrl Pts',(-12.2876333308473,57.7354693911206,
2.65878198860303));
#244407=CARTESIAN_POINT('Origin',(-12.2876333308473,57.7354693911206,2.53178198860303));
#244408=CARTESIAN_POINT('Ctrl Pts',(-12.5528626811449,60.5836663843183,
3.77003198860306));
#244409=CARTESIAN_POINT('Ctrl Pts',(-12.6772730231651,60.5572221497823,
3.77003198860306));
#244410=CARTESIAN_POINT('Ctrl Pts',(-12.6770872880007,60.5572616290102,
3.64284238727649));
#244411=CARTESIAN_POINT('Ctrl Pts',(-12.5977568525211,60.7959479326854,
3.77003198860306));
#244412=CARTESIAN_POINT('Ctrl Pts',(-12.7224242094581,60.769639383333,3.77025506105759));
#244413=CARTESIAN_POINT('Ctrl Pts',(-12.7131635826242,60.7269872521273,
3.64284210641873));
#244414=CARTESIAN_POINT('Ctrl Pts',(-12.6404975322968,60.9980361136602,
3.65553527987876));
#244415=CARTESIAN_POINT('Ctrl Pts',(-12.7653961862431,60.971804353475,3.65585996533132));
#244416=CARTESIAN_POINT('Ctrl Pts',(-12.74750759382,60.8885631224031,3.55127902710283));
#244417=CARTESIAN_POINT('Ctrl Pts',(-12.6642893210144,61.1105274371642,
3.47153072139114));
#244418=CARTESIAN_POINT('Ctrl Pts',(-12.7893350885049,61.0844267823323,
3.4718232790523));
#244419=CARTESIAN_POINT('Ctrl Pts',(-12.7666250660187,60.9785037583492,
3.40413028378034));
#244420=CARTESIAN_POINT('Origin',(-12.5528626811449,60.5836663843183,3.64303198860306));
#244421=CARTESIAN_POINT('Origin',(3.9977349588932E-16,1.91634810190902E-13,
2.53178198860262));
#244422=CARTESIAN_POINT('Origin',(-12.257819391977,57.7418065394567,2.53178198860302));
#244423=CARTESIAN_POINT('Origin',(3.00026883051142,-12.588064422097,3.64303198860254));
#244424=CARTESIAN_POINT('Origin',(-12.469366018725,60.1910940874988,3.64299466007543));
#244425=CARTESIAN_POINT('Ctrl Pts',(-12.2354540642047,57.6364522029208,
2.59908173516064));
#244426=CARTESIAN_POINT('Ctrl Pts',(-12.2432007592849,57.6729438621907,
2.65878198860303));
#244427=CARTESIAN_POINT('Ctrl Pts',(-12.257819391977,57.7418065394567,2.65878198860303));
#244428=CARTESIAN_POINT('Ctrl Pts',(-12.1497054461945,57.6546556225247,
2.59908193199989));
#244429=CARTESIAN_POINT('Ctrl Pts',(-12.1807288143667,57.686202549369,2.65877685806701));
#244430=CARTESIAN_POINT('Ctrl Pts',(-12.208006627196,57.7523715145547,2.65878198860303));
#244431=CARTESIAN_POINT('Ctrl Pts',(-12.0754939174599,57.6955109599437,
2.63872492669841));
#244432=CARTESIAN_POINT('Ctrl Pts',(-12.1277502414152,57.7206875210981,
2.69532212015305));
#244433=CARTESIAN_POINT('Ctrl Pts',(-12.1670355805165,57.7861609236009,
2.68176836726676));
#244434=CARTESIAN_POINT('Ctrl Pts',(-11.9863964689867,57.7879231380268,
2.75442176402287));
#244435=CARTESIAN_POINT('Ctrl Pts',(-12.0782086782662,57.7928648378996,
2.79203179920193));
#244436=CARTESIAN_POINT('Ctrl Pts',(-12.1215423041375,57.8693039540647,
2.74885310748215));
#244437=CARTESIAN_POINT('Ctrl Pts',(-11.9699873265232,57.8386735460215,
2.82866089558444));
#244438=CARTESIAN_POINT('Ctrl Pts',(-12.0820993460723,57.8311081991745,
2.85316563119132));
#244439=CARTESIAN_POINT('Ctrl Pts',(-12.1160385312532,57.9177340744078,
2.79189751796604));
#244440=CARTESIAN_POINT('Ctrl Pts',(-11.9794294790614,57.8830978693157,
2.90134173516063));
#244441=CARTESIAN_POINT('Ctrl Pts',(-12.1031907419159,57.8572899778512,
2.90103711553269));
#244442=CARTESIAN_POINT('Ctrl Pts',(-12.1254815933794,57.9621601888122,
2.83404198860302));
#244443=CARTESIAN_POINT('Origin',(-12.0012568480862,57.9885649735461,2.83404198860303));
#244444=CARTESIAN_POINT('Origin',(-12.4602215058063,60.1478239214158,3.56647653971874));
#244445=CARTESIAN_POINT('Origin',(-12.4432063593724,60.0677739512127,3.42473028058527));
#244446=CARTESIAN_POINT('Origin',(-12.0382961820438,58.1628213391883,3.11913648168055));
#244447=CARTESIAN_POINT('Origin',(-12.0753355159235,58.3370777047236,3.40423097483351));
#244448=CARTESIAN_POINT('Ctrl Pts',(-12.3746037924166,59.7450242491249,
3.36123028058523));
#244449=CARTESIAN_POINT('Ctrl Pts',(-12.4988285377098,59.7186194643911,
3.36123028058523));
#244450=CARTESIAN_POINT('Ctrl Pts',(-12.4988285377098,59.7186194643911,
3.23423028058523));
#244451=CARTESIAN_POINT('Ctrl Pts',(-12.3935470970146,59.8330190893701,
3.36123028058523));
#244452=CARTESIAN_POINT('Ctrl Pts',(-12.5175251937993,59.806580315575,3.3609964110852));
#244453=CARTESIAN_POINT('Ctrl Pts',(-12.5268995400898,59.850683147391,3.23423043688408));
#244454=CARTESIAN_POINT('Ctrl Pts',(-12.4114576311013,59.9162252185218,
3.41054258905328));
#244455=CARTESIAN_POINT('Ctrl Pts',(-12.5352924712483,59.8901687840295,
3.4100881582603));
#244456=CARTESIAN_POINT('Ctrl Pts',(-12.5534426698448,59.9755587548362,
3.30819867304362));
#244457=CARTESIAN_POINT('Ctrl Pts',(-12.4208962741589,59.9600752506738,
3.48823028058525));
#244458=CARTESIAN_POINT('Ctrl Pts',(-12.5446662374489,59.9342688867326,
3.48794691941641));
#244459=CARTESIAN_POINT('Ctrl Pts',(-12.5674311046656,60.0413691664789,
3.42473028058526));
#244460=CARTESIAN_POINT('Origin',(-12.3746037924166,59.7450242491249,3.23423028058523));
#244461=CARTESIAN_POINT('Ctrl Pts',(-12.0535047649324,58.2316113004782,
3.47153072139112));
#244462=CARTESIAN_POINT('Ctrl Pts',(-12.1774537741283,58.2057612755557,
3.47122746285117));
#244463=CARTESIAN_POINT('Ctrl Pts',(-12.1995935640849,58.3108302788452,
3.40413046676848));
#244464=CARTESIAN_POINT('Ctrl Pts',(-12.0772900304161,58.3441059109584,
3.65553813458028));
#244465=CARTESIAN_POINT('Ctrl Pts',(-12.2013259468593,58.3180696991587,
3.65520336072124));
#244466=CARTESIAN_POINT('Ctrl Pts',(-12.2187113817826,58.4007725402778,
3.55128134519947));
#244467=CARTESIAN_POINT('Ctrl Pts',(-12.1200201767772,58.5461981381267,
3.77003198860304));
#244468=CARTESIAN_POINT('Ctrl Pts',(-12.2442455720352,58.5199882620668,
3.7698020931422));
#244469=CARTESIAN_POINT('Ctrl Pts',(-12.2530556816156,58.5623497685507,
3.64284195387449));
#244470=CARTESIAN_POINT('Ctrl Pts',(-12.1649068885794,58.7584778814678,
3.77003198860304));
#244471=CARTESIAN_POINT('Ctrl Pts',(-12.2893177137816,58.7320335442283,
3.77003198860304));
#244472=CARTESIAN_POINT('Ctrl Pts',(-12.2891314947139,58.732073126313,3.64284189403881));
#244473=CARTESIAN_POINT('Origin',(-12.1649068885794,58.7584778814678,3.64303198860303));
#244474=CARTESIAN_POINT('Origin',(2.93511643966563,-12.2815465224194,3.23423028058473));
#244475=CARTESIAN_POINT('Origin',(-12.3431658574213,59.597120393566,3.23423028058523));
#244476=CARTESIAN_POINT('Origin',(2.92491386234308,-12.2335471699534,3.64303198860254));
#244477=CARTESIAN_POINT('Origin',(-12.2483049654,59.1510793400373,3.64299171721807));
#244478=CARTESIAN_POINT('Ctrl Pts',(-12.2968658913805,59.3820708699072,
3.48823028058522));
#244479=CARTESIAN_POINT('Ctrl Pts',(-12.4217592664914,59.3560370505015,
3.488520042123));
#244480=CARTESIAN_POINT('Ctrl Pts',(-12.3987880210526,59.2479658375578,
3.42473028058522));
#244481=CARTESIAN_POINT('Ctrl Pts',(-12.3063392072225,59.4260685345963,
3.41028005848446));
#244482=CARTESIAN_POINT('Ctrl Pts',(-12.4310668851206,59.3998259533514,
3.41074404220392));
#244483=CARTESIAN_POINT('Ctrl Pts',(-12.4128237298765,59.3139986558986,
3.30780486244002));
#244484=CARTESIAN_POINT('Ctrl Pts',(-12.3242857901776,59.5094220566596,
3.36123028058523));
#244485=CARTESIAN_POINT('Ctrl Pts',(-12.4487214234132,59.482884025773,3.36146460586469));
#244486=CARTESIAN_POINT('Ctrl Pts',(-12.4394141514343,59.439096753783,3.23423045308409));
#244487=CARTESIAN_POINT('Ctrl Pts',(-12.3431658574213,59.597120393566,3.36123028058523));
#244488=CARTESIAN_POINT('Ctrl Pts',(-12.4673906027145,59.5707156088322,
3.36123028058523));
#244489=CARTESIAN_POINT('Ctrl Pts',(-12.4673906027145,59.5707156088322,
3.23423028058523));
#244490=CARTESIAN_POINT('Origin',(-12.2745632757594,59.2743706222916,3.42473028058522));
#244491=CARTESIAN_POINT('Origin',(-12.2576496039195,59.1947980539417,3.56563113524832));
#244492=CARTESIAN_POINT('Origin',(-19.283043599957,58.3196542523189,3.56647653909532));
#244493=CARTESIAN_POINT('Origin',(-19.2967593024444,58.3616995707145,3.64299466007843));
#244494=CARTESIAN_POINT('Origin',(-19.2577541638581,58.2418213702175,3.42473028058524));
#244495=CARTESIAN_POINT('Ctrl Pts',(-19.2232259141442,58.1373965169894,
3.48823028058524));
#244496=CARTESIAN_POINT('Ctrl Pts',(-19.103134799739,58.176932531882,3.48794691941641));
#244497=CARTESIAN_POINT('Ctrl Pts',(-19.1369699862886,58.2810665285031,
3.42473028058526));
#244498=CARTESIAN_POINT('Ctrl Pts',(-19.2094285342454,58.0945576760634,
3.41028005925126));
#244499=CARTESIAN_POINT('Ctrl Pts',(-19.0891556041227,58.1339089916642,
3.40982512231099));
#244500=CARTESIAN_POINT('Ctrl Pts',(-19.1161088652899,58.2168625998383,
3.30780486372909));
#244501=CARTESIAN_POINT('Ctrl Pts',(-19.1832899764623,58.0133994748122,
3.36123028058522));
#244502=CARTESIAN_POINT('Ctrl Pts',(-19.0627016856748,58.0524922023721,
3.36099721048474));
#244503=CARTESIAN_POINT('Ctrl Pts',(-19.0765878066315,58.0952292882337,
3.23423045308334));
#244504=CARTESIAN_POINT('Ctrl Pts',(-19.1557908785627,57.9280106456677,
3.36123028058522));
#244505=CARTESIAN_POINT('Ctrl Pts',(-19.0350067009933,57.9672558039533,
3.36123028058521));
#244506=CARTESIAN_POINT('Ctrl Pts',(-19.0350067009933,57.9672558039533,
3.23423028058522));
#244507=CARTESIAN_POINT('Origin',(-19.1557908785627,57.9280106456677,3.23423028058521));
#244508=CARTESIAN_POINT('Origin',(-0.301960443923705,-0.0981128957138633,
3.64303198860263));
#244509=CARTESIAN_POINT('Origin',(-19.4207352200703,58.7434254837933,3.64303198860303));
#244510=CARTESIAN_POINT('Origin',(-0.301960443923705,-0.0981128957138604,
3.23423028058481));
#244511=CARTESIAN_POINT('Origin',(-19.1090650011318,57.7842031819384,3.23423028058521));
#244512=CARTESIAN_POINT('Ctrl Pts',(-19.5876674457081,59.2554138597572,
3.47153072139113));
#244513=CARTESIAN_POINT('Ctrl Pts',(-19.4663243174857,59.2953329099162,
3.47182327902703));
#244514=CARTESIAN_POINT('Ctrl Pts',(-19.4330302542693,59.1922458813527,
3.40413028959058));
#244515=CARTESIAN_POINT('Ctrl Pts',(-19.5520255367089,59.1460959632226,
3.65553807120998));
#244516=CARTESIAN_POINT('Ctrl Pts',(-19.4307442612511,59.185827914589,3.65586275496843));
#244517=CARTESIAN_POINT('Ctrl Pts',(-19.4046157212344,59.104794941234,3.5512812683721));
#244518=CARTESIAN_POINT('Ctrl Pts',(-19.4879954548414,58.9497105734781,
3.77003198860303));
#244519=CARTESIAN_POINT('Ctrl Pts',(-19.3668760934058,58.989260368079,3.77025505748724));
#244520=CARTESIAN_POINT('Ctrl Pts',(-19.35357016791,58.9476928828774,3.64284211731298));
#244521=CARTESIAN_POINT('Ctrl Pts',(-19.4207352200704,58.7434254837933,
3.77003198860303));
#244522=CARTESIAN_POINT('Ctrl Pts',(-19.2997705965402,58.7827292725257,
3.77003198860303));
#244523=CARTESIAN_POINT('Ctrl Pts',(-19.2999511770886,58.7826705983487,
3.64284239821721));
#244524=CARTESIAN_POINT('Origin',(-19.5538640879535,59.1531540088,3.40423097483351));
#244525=CARTESIAN_POINT('Ctrl Pts',(-19.1090650011318,57.7842031819384,
3.36123028058522));
#244526=CARTESIAN_POINT('Ctrl Pts',(-18.9882808235623,57.823448340224,3.36123028058521));
#244527=CARTESIAN_POINT('Ctrl Pts',(-18.9882808235623,57.823448340224,3.23423028058522));
#244528=CARTESIAN_POINT('Ctrl Pts',(-19.0814735135847,57.698525571102,3.36123028058522));
#244529=CARTESIAN_POINT('Ctrl Pts',(-18.9604392969147,57.7377609320132,
3.36146538610115));
#244530=CARTESIAN_POINT('Ctrl Pts',(-18.9465591794955,57.6950423231356,
3.2342304368842));
#244531=CARTESIAN_POINT('Ctrl Pts',(-19.0553854270309,57.6175103216839,
3.4105425869314));
#244532=CARTESIAN_POINT('Ctrl Pts',(-18.934246652453,57.6571482613565,3.41100608859792));
#244533=CARTESIAN_POINT('Ctrl Pts',(-18.9071083904249,57.5736252790843,
3.30819866970861));
#244534=CARTESIAN_POINT('Ctrl Pts',(-19.041637186088,57.5748148483577,3.48823028058522));
#244535=CARTESIAN_POINT('Ctrl Pts',(-18.9204594407748,57.6147155869503,
3.488520042123));
#244536=CARTESIAN_POINT('Ctrl Pts',(-18.8863175164095,57.5096375484038,
3.42473028058522));
#244537=CARTESIAN_POINT('Origin',(-19.007101693979,57.4703923901181,3.42473028058521));
#244538=CARTESIAN_POINT('Origin',(-19.6089151909145,59.3225838821627,3.11913648178295));
#244539=CARTESIAN_POINT('Origin',(-19.6639662938564,59.492013755314,2.83404198860302));
#244540=CARTESIAN_POINT('Origin',(-18.9819630786544,57.3930236876033,3.56563113460828));
#244541=CARTESIAN_POINT('Origin',(-18.968196416683,57.3504898524415,3.64299171721863));
#244542=CARTESIAN_POINT('Ctrl Pts',(-19.4684195516699,59.8682321556243,
2.59908173516064));
#244543=CARTESIAN_POINT('Ctrl Pts',(-19.4568831131886,59.8327559231847,
2.65878198860303));
#244544=CARTESIAN_POINT('Ctrl Pts',(-19.4351129318423,59.7658094374952,
2.65878198860303));
#244545=CARTESIAN_POINT('Ctrl Pts',(-19.5522156237501,59.8409825629609,
2.59908193475531));
#244546=CARTESIAN_POINT('Ctrl Pts',(-19.5179203859192,59.8129039518386,
2.65878715325381));
#244547=CARTESIAN_POINT('Ctrl Pts',(-19.4836145615383,59.7500277420819,
2.65878198860303));
#244548=CARTESIAN_POINT('Ctrl Pts',(-19.6218019328333,59.7920481472526,
2.63878778849926));
#244549=CARTESIAN_POINT('Ctrl Pts',(-19.5669820401371,59.7726277678656,
2.69564460180159));
#244550=CARTESIAN_POINT('Ctrl Pts',(-19.5206357546565,59.7116747787983,
2.6818048162492));
#244551=CARTESIAN_POINT('Ctrl Pts',(-19.7007838434712,59.6899788477098,
2.75443238878672));
#244552=CARTESIAN_POINT('Ctrl Pts',(-19.6084674936735,59.6952619726978,
2.79268340777122));
#244553=CARTESIAN_POINT('Ctrl Pts',(-19.556896198164,59.6234872553903,2.74885926835654));
#244554=CARTESIAN_POINT('Ctrl Pts',(-19.7118189603902,59.6375245663858,
2.82856655361718));
#244555=CARTESIAN_POINT('Ctrl Pts',(-19.6003923959449,59.6577198343146,
2.85384197230828));
#244556=CARTESIAN_POINT('Ctrl Pts',(-19.5572342963493,59.5745070768393,
2.7918462427852));
#244557=CARTESIAN_POINT('Ctrl Pts',(-19.6977666881848,59.5942745858237,
2.90134173516065));
#244558=CARTESIAN_POINT('Ctrl Pts',(-19.5766071063171,59.6341304551458,
2.90163218716432));
#244559=CARTESIAN_POINT('Ctrl Pts',(-19.5431821162869,59.5312589135997,
2.83404198860303));
#244560=CARTESIAN_POINT('Origin',(-19.4351129318423,59.7658094374952,2.53178198860302));
#244561=CARTESIAN_POINT('Origin',(-0.301960443923705,-0.0981128957138633,
3.64303198860263));
#244562=CARTESIAN_POINT('Origin',(-18.8441205405522,56.9687879773467,3.64303198860302));
#244563=CARTESIAN_POINT('Origin',(2.07460197300515E-17,1.91420615423891E-13,
2.53178198860262));
#244564=CARTESIAN_POINT('Origin',(-19.4061247292256,59.7752282754838,2.53178198860303));
#244565=CARTESIAN_POINT('Ctrl Pts',(-18.8441205405522,56.9687879773467,
3.77003198860302));
#244566=CARTESIAN_POINT('Ctrl Pts',(-18.7231554228303,57.0080919266517,
3.77003198860302));
#244567=CARTESIAN_POINT('Ctrl Pts',(-18.7233364983081,57.0080330916624,
3.64284187937061));
#244568=CARTESIAN_POINT('Ctrl Pts',(-18.7768526573589,56.7625017687178,
3.77003198860302));
#244569=CARTESIAN_POINT('Ctrl Pts',(-18.6561653631322,56.8019160587479,
3.76980208963145));
#244570=CARTESIAN_POINT('Ctrl Pts',(-18.6697165591968,56.8430078886273,
3.64284193928381));
#244571=CARTESIAN_POINT('Ctrl Pts',(-18.7128124416019,56.5661212433893,
3.65553535416627));
#244572=CARTESIAN_POINT('Ctrl Pts',(-18.5923760693072,56.6055911857614,
3.6552005783438));
#244573=CARTESIAN_POINT('Ctrl Pts',(-18.6186713857001,56.6859069993048,
3.55127910964221));
#244574=CARTESIAN_POINT('Ctrl Pts',(-18.6771643191712,56.4568070719812,
3.47153072139111));
#244575=CARTESIAN_POINT('Ctrl Pts',(-18.556896302113,56.4963948028698,3.47122746281622));
#244576=CARTESIAN_POINT('Ctrl Pts',(-18.5902572009363,56.5984571310821,
3.404130459013));
#244577=CARTESIAN_POINT('Origin',(-18.7109915363519,56.559059032799,3.4042309748335));
#244578=CARTESIAN_POINT('Ctrl Pts',(-19.0928077206414,59.7908376697913,
2.90134173516066));
#244579=CARTESIAN_POINT('Ctrl Pts',(-19.2142545736086,59.7518659300027,
2.90163218716433));
#244580=CARTESIAN_POINT('Ctrl Pts',(-19.1808295835784,59.6489943884565,
2.83404198860303));
#244581=CARTESIAN_POINT('Ctrl Pts',(-19.1068672906321,59.8341069976973,
2.82853349835402));
#244582=CARTESIAN_POINT('Ctrl Pts',(-19.2088743168605,59.7849495553999,
2.85381483162332));
#244583=CARTESIAN_POINT('Ctrl Pts',(-19.1948881666552,59.6922622581478,
2.79182701594224));
#244584=CARTESIAN_POINT('Ctrl Pts',(-19.1465773683631,59.8698829694069,
2.75468822073679));
#244585=CARTESIAN_POINT('Ctrl Pts',(-19.2244455609618,59.8199164124671,
2.7928691308392));
#244586=CARTESIAN_POINT('Ctrl Pts',(-19.2238994150016,59.7315159919506,
2.74900763297943));
#244587=CARTESIAN_POINT('Ctrl Pts',(-19.2694731179103,59.9060262085836,
2.63954450640438));
#244588=CARTESIAN_POINT('Ctrl Pts',(-19.3027624708828,59.8580612818576,
2.69627684028872));
#244589=CARTESIAN_POINT('Ctrl Pts',(-19.3044519280753,59.7814166574713,
2.68224356036543));
#244590=CARTESIAN_POINT('Ctrl Pts',(-19.3552948408467,59.9049660265688,
2.59908178706424));
#244591=CARTESIAN_POINT('Ctrl Pts',(-19.3665789650877,59.8620777700636,
2.65878704321562));
#244592=CARTESIAN_POINT('Ctrl Pts',(-19.3574492964903,59.7910213450153,
2.65878198860303));
#244593=CARTESIAN_POINT('Ctrl Pts',(-19.4393816709759,59.8776671349986,
2.59908173516064));
#244594=CARTESIAN_POINT('Ctrl Pts',(-19.4278624395269,59.8421853116554,
2.65878198860302));
#244595=CARTESIAN_POINT('Ctrl Pts',(-19.4061247292256,59.7752282754838,
2.65878198860303));
#244596=CARTESIAN_POINT('Origin',(-19.0600454060089,59.6882395467421,2.83404198860304));
#244597=CARTESIAN_POINT('Origin',(-18.655940357667,56.3896289265487,3.11913648167136));
#244598=CARTESIAN_POINT('Origin',(-18.6008891789888,56.2201988201384,2.83404198860301));
#244599=CARTESIAN_POINT('Origin',(-19.0049943031078,59.5188096735657,3.11913648177589));
#244600=CARTESIAN_POINT('Origin',(-18.949943200106,59.3493798002281,3.40423097483351));
#244601=CARTESIAN_POINT('Ctrl Pts',(-18.5670586829468,56.1179479440989,
2.90134173516062));
#244602=CARTESIAN_POINT('Ctrl Pts',(-18.4469743395782,56.1574782858998,
2.90103711553268));
#244603=CARTESIAN_POINT('Ctrl Pts',(-18.4801050014193,56.259443978424,2.834041988603));
#244604=CARTESIAN_POINT('Ctrl Pts',(-18.5530176696412,56.0747358697604,
2.8286299174799));
#244605=CARTESIAN_POINT('Ctrl Pts',(-18.452151844104,56.1242410383984,2.85314045886485));
#244606=CARTESIAN_POINT('Ctrl Pts',(-18.4660639121463,56.2162299491243,
2.79187961000028));
#244607=CARTESIAN_POINT('Ctrl Pts',(-18.5135050040177,56.0391722633448,
2.75470625793378));
#244608=CARTESIAN_POINT('Ctrl Pts',(-18.4363793473475,56.0893377355419,
2.79224250381961));
#244609=CARTESIAN_POINT('Ctrl Pts',(-18.4371504234766,56.1772247439502,
2.74901809108305));
#244610=CARTESIAN_POINT('Ctrl Pts',(-18.3911086652348,56.0036796861847,
2.63947868311724));
#244611=CARTESIAN_POINT('Ctrl Pts',(-18.3580919822893,56.0516449414231,
2.69595066767933));
#244612=CARTESIAN_POINT('Ctrl Pts',(-18.3567819283755,56.1280773042133,
2.68220539436091));
#244613=CARTESIAN_POINT('Ctrl Pts',(-18.3056594201307,56.0051563026342,
2.59908178585092));
#244614=CARTESIAN_POINT('Ctrl Pts',(-18.2945198471559,56.0480033886673,
2.65877670944816));
#244615=CARTESIAN_POINT('Ctrl Pts',(-18.3039075553121,56.1189701685708,
2.658781988603));
#244616=CARTESIAN_POINT('Ctrl Pts',(-18.2220120550219,56.0323588238392,
2.59908173516062));
#244617=CARTESIAN_POINT('Ctrl Pts',(-18.233549049922,56.0678348753333,2.65878198860301));
#244618=CARTESIAN_POINT('Ctrl Pts',(-18.2553202812751,56.1347810195643,
2.658781988603));
#244619=CARTESIAN_POINT('Origin',(-18.2553202812751,56.1347810195643,2.531781988603));
#244620=CARTESIAN_POINT('Ctrl Pts',(-18.8168143322229,58.9396512752214,
3.77003198860304));
#244621=CARTESIAN_POINT('Ctrl Pts',(-18.9377789661744,58.900347483103,3.77003198860304));
#244622=CARTESIAN_POINT('Ctrl Pts',(-18.9375983751891,58.900406160671,3.642842387276));
#244623=CARTESIAN_POINT('Ctrl Pts',(-18.8836520326609,59.1460772043118,
3.77003198860304));
#244624=CARTESIAN_POINT('Ctrl Pts',(-19.0048864565378,59.1068814887035,
3.77025506105942));
#244625=CARTESIAN_POINT('Ctrl Pts',(-18.9912181986572,59.0654310094274,
3.64284210641963));
#244626=CARTESIAN_POINT('Ctrl Pts',(-18.9472825415244,59.3425907075099,
3.65553527987875));
#244627=CARTESIAN_POINT('Ctrl Pts',(-19.0687550219954,59.3034471832927,
3.65585996533051));
#244628=CARTESIAN_POINT('Ctrl Pts',(-19.042263347188,59.2225318234693,3.55127902710181));
#244629=CARTESIAN_POINT('Ctrl Pts',(-18.9827025415099,59.4519788726608,
3.47153072139112));
#244630=CARTESIAN_POINT('Ctrl Pts',(-19.104335033863,59.412950358033,3.47182327905229));
#244631=CARTESIAN_POINT('Ctrl Pts',(-19.0706774483339,59.3099814352092,
3.40413028378007));
#244632=CARTESIAN_POINT('Origin',(-18.8168143322229,58.9396512752214,3.64303198860304));
#244633=CARTESIAN_POINT('Origin',(3.93842937138093E-16,1.91633221102474E-13,
2.53178198860262));
#244634=CARTESIAN_POINT('Origin',(-18.2263320786585,56.1441998575529,2.531781988603));
#244635=CARTESIAN_POINT('Origin',(6.24367625034032,-18.1886080242679,3.6430319886025));
#244636=CARTESIAN_POINT('Origin',(-18.6927400943494,58.5579573083284,3.64299466007759));
#244637=CARTESIAN_POINT('Ctrl Pts',(-18.1930767435952,56.0417604764384,
2.59908173516062));
#244638=CARTESIAN_POINT('Ctrl Pts',(-18.2045954185348,56.0772424804485,
2.65878198860301));
#244639=CARTESIAN_POINT('Ctrl Pts',(-18.2263320786585,56.1441998575529,
2.658781988603));
#244640=CARTESIAN_POINT('Ctrl Pts',(-18.1097006409637,56.068827347073,2.5990819319998));
#244641=CARTESIAN_POINT('Ctrl Pts',(-18.1438516116621,56.0969586315483,
2.65877685806732));
#244642=CARTESIAN_POINT('Ctrl Pts',(-18.177896534026,56.1599138083643,2.658781988603));
#244643=CARTESIAN_POINT('Ctrl Pts',(-18.0401661963854,56.1172160917341,
2.63872492669835));
#244644=CARTESIAN_POINT('Ctrl Pts',(-18.0947679219784,56.1367924598138,
2.69532212015302));
#244645=CARTESIAN_POINT('Ctrl Pts',(-18.1406818860299,56.1978007560414,
2.68176836726667));
#244646=CARTESIAN_POINT('Ctrl Pts',(-17.9612165360192,56.2184352456066,
2.75442176402289));
#244647=CARTESIAN_POINT('Ctrl Pts',(-18.0530423367033,56.2137528851845,
2.7920317992019));
#244648=CARTESIAN_POINT('Ctrl Pts',(-18.1041286397845,56.2852436625536,
2.74885310748219));
#244649=CARTESIAN_POINT('Ctrl Pts',(-17.9502021467132,56.2706228600013,
2.82866089558439));
#244650=CARTESIAN_POINT('Ctrl Pts',(-18.0609092108088,56.2513800597978,
2.85316563119196));
#244651=CARTESIAN_POINT('Ctrl Pts',(-18.1037173431993,56.3339837785517,
2.79189751796651));
#244652=CARTESIAN_POINT('Ctrl Pts',(-17.9642361803975,56.3138168485096,
2.9013417351606));
#244653=CARTESIAN_POINT('Ctrl Pts',(-18.0846218068697,56.2752137607567,
2.90103711553267));
#244654=CARTESIAN_POINT('Ctrl Pts',(-18.1177524687109,56.3771794532808,
2.83404198860299));
#244655=CARTESIAN_POINT('Origin',(-17.9969682911414,56.4164246115665,2.834041988603));
#244656=CARTESIAN_POINT('Origin',(-18.6791227120619,58.5158800426281,3.56647653971818));
#244657=CARTESIAN_POINT('Origin',(-18.6538332760107,58.4380471616456,3.42473028058526));
#244658=CARTESIAN_POINT('Origin',(-18.0520194698684,56.5858547179441,3.11913648168137));
#244659=CARTESIAN_POINT('Origin',(-18.1070706485045,56.7552848242271,3.4042309748335));
#244660=CARTESIAN_POINT('Ctrl Pts',(-18.5518699907153,58.1242364370958,
3.36123028058522));
#244661=CARTESIAN_POINT('Ctrl Pts',(-18.6726541682848,58.0849912788101,
3.36123028058522));
#244662=CARTESIAN_POINT('Ctrl Pts',(-18.6726541682848,58.0849912788101,
3.23423028058522));
#244663=CARTESIAN_POINT('Ctrl Pts',(-18.5799074873338,58.2097691178806,
3.36123028058522));
#244664=CARTESIAN_POINT('Ctrl Pts',(-18.7004428147365,58.1705159385199,
3.36099641108529));
#244665=CARTESIAN_POINT('Ctrl Pts',(-18.7143758086138,58.2133972843944,
3.23423043688374));
#244666=CARTESIAN_POINT('Ctrl Pts',(-18.6064173144572,58.2906472745458,
3.41054258905323));
#244667=CARTESIAN_POINT('Ctrl Pts',(-18.7268501353369,58.2517893143872,
3.41008815826052));
#244668=CARTESIAN_POINT('Ctrl Pts',(-18.7538265876733,58.3348142976348,
3.30819867304345));
#244669=CARTESIAN_POINT('Ctrl Pts',(-18.620387828115,58.3332704847797,3.48823028058524));
#244670=CARTESIAN_POINT('Ctrl Pts',(-18.7407822670305,58.2946680067389,
3.4879469194164));
#244671=CARTESIAN_POINT('Ctrl Pts',(-18.7746174535802,58.3988020033599,
3.42473028058525));
#244672=CARTESIAN_POINT('Origin',(-18.5518699907153,58.1242364370958,3.23423028058522));
#244673=CARTESIAN_POINT('Ctrl Pts',(-18.0743352474894,56.6526781108325,
3.47153072139111));
#244674=CARTESIAN_POINT('Ctrl Pts',(-18.1949031876636,56.6140134955963,
3.47122746285116));
#244675=CARTESIAN_POINT('Ctrl Pts',(-18.227904394985,56.7161926816712,3.40413046676836));
#244676=CARTESIAN_POINT('Ctrl Pts',(-18.1097491035603,56.7620702268162,
3.65553813458026));
#244677=CARTESIAN_POINT('Ctrl Pts',(-18.2303840130631,56.7232113603728,
3.65520336072152));
#244678=CARTESIAN_POINT('Ctrl Pts',(-18.2563190096467,56.803643873878,3.55128134519884));
#244679=CARTESIAN_POINT('Ctrl Pts',(-18.1733695596533,56.9585888550844,
3.77003198860302));
#244680=CARTESIAN_POINT('Ctrl Pts',(-18.2941747571319,56.9195374698037,
3.76980209314226));
#244681=CARTESIAN_POINT('Ctrl Pts',(-18.3073645871833,56.9607460083081,
3.64284195387558));
#244682=CARTESIAN_POINT('Ctrl Pts',(-18.2401996527048,57.1650137687748,
3.77003198860302));
#244683=CARTESIAN_POINT('Ctrl Pts',(-18.3611647564557,57.1257098240093,
3.77003198860303));
#244684=CARTESIAN_POINT('Ctrl Pts',(-18.3609836949697,57.1257686544523,
3.64284189403859));
#244685=CARTESIAN_POINT('Origin',(-18.2401996527048,57.1650137687748,3.64303198860302));
#244686=CARTESIAN_POINT('Origin',(6.09975091006211,-17.7456513739113,3.23423028058469));
#244687=CARTESIAN_POINT('Origin',(-18.5051441132844,57.9804289733665,3.23423028058522));
#244688=CARTESIAN_POINT('Origin',(6.07721283595922,-17.6762863142852,3.6430319886025));
#244689=CARTESIAN_POINT('Origin',(-18.3641788932754,57.5467470426661,3.64299171721799));
#244690=CARTESIAN_POINT('Ctrl Pts',(-18.4366189870675,57.7713971777988,
3.48823028058521));
#244691=CARTESIAN_POINT('Ctrl Pts',(-18.5581069080663,57.7324510618071,
3.48852004212298));
#244692=CARTESIAN_POINT('Ctrl Pts',(-18.523964983701,57.6273730232606,3.4247302805852));
#244693=CARTESIAN_POINT('Ctrl Pts',(-18.450639415372,57.8141635875299,3.4102800584845));
#244694=CARTESIAN_POINT('Ctrl Pts',(-18.5719407253105,57.7750271733958,
3.41074404220504));
#244695=CARTESIAN_POINT('Ctrl Pts',(-18.5448261124707,57.691576975842,3.30780486244105));
#244696=CARTESIAN_POINT('Ctrl Pts',(-18.4772005006358,57.8951845615414,
3.36123028058522));
#244697=CARTESIAN_POINT('Ctrl Pts',(-18.5981804828652,57.855784843245,3.36146460586404));
#244698=CARTESIAN_POINT('Ctrl Pts',(-18.584347180845,57.813210317349,3.23423045308373));
#244699=CARTESIAN_POINT('Ctrl Pts',(-18.5051441132844,57.9804289733665,
3.36123028058522));
#244700=CARTESIAN_POINT('Ctrl Pts',(-18.6259282908539,57.9411838150808,
3.36123028058522));
#244701=CARTESIAN_POINT('Ctrl Pts',(-18.6259282908539,57.9411838150808,
3.23423028058522));
#244702=CARTESIAN_POINT('Origin',(-18.4031808061315,57.6666181815462,3.42473028058521));
#244703=CARTESIAN_POINT('Origin',(-18.3780421908669,57.5892494801769,3.56563113524799));
#244704=CARTESIAN_POINT('Origin',(-25.2734729067966,55.9845461696125,3.56647653909435));
#244705=CARTESIAN_POINT('Origin',(-25.2915084057495,56.0249274780519,3.64299466007493));
#244706=CARTESIAN_POINT('Origin',(-25.2401862573144,55.9097831300747,3.42473028058522));
#244707=CARTESIAN_POINT('Ctrl Pts',(-25.1949317875303,55.8095395120008,
3.48823028058522));
#244708=CARTESIAN_POINT('Ctrl Pts',(-25.0796311836956,55.8614118841079,
3.48794691941638));
#244709=CARTESIAN_POINT('Ctrl Pts',(-25.1241659841938,55.9614386837454,
3.42473028058523));
#244710=CARTESIAN_POINT('Ctrl Pts',(-25.1767321129103,55.7683775656463,
3.41028005925127));
#244711=CARTESIAN_POINT('Ctrl Pts',(-25.0612313830298,55.8200852551871,
3.40982512230946));
#244712=CARTESIAN_POINT('Ctrl Pts',(-25.0967080045987,55.8997670518378,
3.30780486372847));
#244713=CARTESIAN_POINT('Ctrl Pts',(-25.1422534028245,55.6903961807898,
3.3612302805852));
#244714=CARTESIAN_POINT('Ctrl Pts',(-25.0264120100478,55.741879663018,3.36099721048499));
#244715=CARTESIAN_POINT('Ctrl Pts',(-25.0446893032921,55.7829311357722,
3.23423045308483));
#244716=CARTESIAN_POINT('Ctrl Pts',(-25.1059793847704,55.6083495590302,
3.3612302805852));
#244717=CARTESIAN_POINT('Ctrl Pts',(-24.9899591116498,55.6600051127008,
3.3612302805852));
#244718=CARTESIAN_POINT('Ctrl Pts',(-24.9899591116498,55.6600051127009,
3.2342302805852));
#244719=CARTESIAN_POINT('Origin',(-25.1059793847704,55.6083495590302,3.2342302805852));
#244720=CARTESIAN_POINT('Origin',(-0.29005068280152,-0.129138884176384,
3.64303198860263));
#244721=CARTESIAN_POINT('Origin',(-25.4547063934086,56.3916032444851,3.64303198860301));
#244722=CARTESIAN_POINT('Origin',(-0.29005068280152,-0.129138884176381,
3.23423028058481));
#244723=CARTESIAN_POINT('Origin',(-25.044477503395,55.4702140717967,3.2342302805852));
#244724=CARTESIAN_POINT('Ctrl Pts',(-25.6742415049982,56.8833377255395,
3.47153072139111));
#244725=CARTESIAN_POINT('Ctrl Pts',(-25.5577357840968,56.9357219056861,
3.47182327902701));
#244726=CARTESIAN_POINT('Ctrl Pts',(-25.5138485805638,56.8366797759151,
3.40413028959052));
#244727=CARTESIAN_POINT('Ctrl Pts',(-25.6273680143746,56.7783442778553,
3.65553807120996));
#244728=CARTESIAN_POINT('Ctrl Pts',(-25.5109042502522,56.8305359187867,
3.65586275497023));
#244729=CARTESIAN_POINT('Ctrl Pts',(-25.4764485929327,56.7526780286707,
3.55128126837251));
#244730=CARTESIAN_POINT('Ctrl Pts',(-25.5431608329951,56.5897276738853,
3.77003198860302));
#244731=CARTESIAN_POINT('Ctrl Pts',(-25.4268390553461,56.6417212312926,
3.7702550574865));
#244732=CARTESIAN_POINT('Ctrl Pts',(-25.409261035753,56.6017723050706,3.64284211731288));
#244733=CARTESIAN_POINT('Ctrl Pts',(-25.4547063934086,56.3916032444851,
3.77003198860302));
#244734=CARTESIAN_POINT('Ctrl Pts',(-25.3385127913796,56.4433359691578,
3.77003198860302));
#244735=CARTESIAN_POINT('Ctrl Pts',(-25.3386862495673,56.4432587405969,
3.6428423982171));
#244736=CARTESIAN_POINT('Origin',(-25.6299342604998,56.7851714777848,3.40423097483349));
#244737=CARTESIAN_POINT('Ctrl Pts',(-25.044477503395,55.4702140717967,3.3612302805852));
#244738=CARTESIAN_POINT('Ctrl Pts',(-24.9284572302744,55.5218696254674,
3.3612302805852));
#244739=CARTESIAN_POINT('Ctrl Pts',(-24.9284572302744,55.5218696254674,
3.2342302805852));
#244740=CARTESIAN_POINT('Ctrl Pts',(-25.008081415906,55.38788990767,3.3612302805852));
#244741=CARTESIAN_POINT('Ctrl Pts',(-24.8918114493206,55.4395618538373,
3.36146538610207));
#244742=CARTESIAN_POINT('Ctrl Pts',(-24.8735420580978,55.3985281293134,
3.234230436885));
#244743=CARTESIAN_POINT('Ctrl Pts',(-24.9736678430969,55.310045415862,3.41054258693138));
#244744=CARTESIAN_POINT('Ctrl Pts',(-24.8573359723256,55.3621286647047,
3.41100608859807));
#244745=CARTESIAN_POINT('Ctrl Pts',(-24.8216158475502,55.281899950894,3.30819866970868));
#244746=CARTESIAN_POINT('Ctrl Pts',(-24.9555320242418,55.2690209153041,
3.48823028058519));
#244747=CARTESIAN_POINT('Ctrl Pts',(-24.8391888661847,55.3213695969756,
3.48852004212297));
#244748=CARTESIAN_POINT('Ctrl Pts',(-24.794250328961,55.2204359898057,3.42473028058518));
#244749=CARTESIAN_POINT('Origin',(-24.9102706020816,55.1687804361351,3.42473028058517));
#244750=CARTESIAN_POINT('Origin',(-25.7023940320541,56.9479187893831,3.11913648178511));
#244751=CARTESIAN_POINT('Origin',(-25.774853803565,57.1106661007666,2.83404198860301));
#244752=CARTESIAN_POINT('Origin',(-24.8771824671419,55.0944632682977,3.56563113460869));
#244753=CARTESIAN_POINT('Origin',(-24.8590452239605,55.0536014459536,3.64299171721809));
#244754=CARTESIAN_POINT('Ctrl Pts',(-25.61970381813,57.5052637377733,2.59908173516063));
#244755=CARTESIAN_POINT('Ctrl Pts',(-25.6045223014064,57.471187734033,2.65878198860301));
#244756=CARTESIAN_POINT('Ctrl Pts',(-25.5758735661211,57.406883591798,2.65878198860301));
#244757=CARTESIAN_POINT('Ctrl Pts',(-25.7001924885134,57.4694043465871,
2.59908193475586));
#244758=CARTESIAN_POINT('Ctrl Pts',(-25.6631501095125,57.4450643815424,
2.65878715325347));
#244759=CARTESIAN_POINT('Ctrl Pts',(-25.6224598624455,57.3861185493459,
2.65878198860301));
#244760=CARTESIAN_POINT('Ctrl Pts',(-25.7642825572405,57.4134642487753,
2.63878778849914));
#244761=CARTESIAN_POINT('Ctrl Pts',(-25.7077329912391,57.3998804953988,
2.69564460180175));
#244762=CARTESIAN_POINT('Ctrl Pts',(-25.6552692732808,57.3441059191832,
2.68180481624934));
#244763=CARTESIAN_POINT('Ctrl Pts',(-25.8321626496791,57.3036982377904,
2.7544323887868));
#244764=CARTESIAN_POINT('Ctrl Pts',(-25.7409042554409,57.3186021074456,
2.792683407771));
#244765=CARTESIAN_POINT('Ctrl Pts',(-25.6821129719827,57.2526112478171,
2.74885926835637));
#244766=CARTESIAN_POINT('Ctrl Pts',(-25.8376543496551,57.2503778226941,
2.82856655361711));
#244767=CARTESIAN_POINT('Ctrl Pts',(-25.7289491719114,57.2821097063804,
2.85384197230861));
#244768=CARTESIAN_POINT('Ctrl Pts',(-25.6773293952369,57.2038640469265,
2.79184624278536));
#244769=CARTESIAN_POINT('Ctrl Pts',(-25.8191582032623,57.2088336324699,
2.90134173516062));
#244770=CARTESIAN_POINT('Ctrl Pts',(-25.7028284190336,57.2611357920725,
2.9016321871643));
#244771=CARTESIAN_POINT('Ctrl Pts',(-25.6588335304443,57.1623216544372,
2.83404198860301));
#244772=CARTESIAN_POINT('Origin',(-25.5758735661211,57.406883591798,2.531781988603));
#244773=CARTESIAN_POINT('Origin',(-0.29005068280152,-0.129138884176384,
3.64303198860263));
#244774=CARTESIAN_POINT('Origin',(-24.695750338031,54.6869600343298,3.643031988603));
#244775=CARTESIAN_POINT('Origin',(3.68589728140384E-17,1.91426800607079E-13,
2.53178198860262));
#244776=CARTESIAN_POINT('Origin',(-25.5480287005721,57.419280924679,2.53178198860301));
#244777=CARTESIAN_POINT('Ctrl Pts',(-24.695750338031,54.6869600343298,3.77003198860301));
#244778=CARTESIAN_POINT('Ctrl Pts',(-24.5795562613022,54.7386929703524,
3.77003198860301));
#244779=CARTESIAN_POINT('Ctrl Pts',(-24.5797301948983,54.7386155301261,
3.64284187937088));
#244780=CARTESIAN_POINT('Ctrl Pts',(-24.6072881749585,54.4888352915936,
3.770031988603));
#244781=CARTESIAN_POINT('Ctrl Pts',(-24.4913819335251,54.5406489234201,
3.7698020896306));
#244782=CARTESIAN_POINT('Ctrl Pts',(-24.5091541605498,54.5800991622551,
3.64284193928419));
#244783=CARTESIAN_POINT('Ctrl Pts',(-24.5230714236766,54.3002245846703,
3.65553535416623));
#244784=CARTESIAN_POINT('Ctrl Pts',(-24.40742054685,54.352067335487,3.65520057834444));
#244785=CARTESIAN_POINT('Ctrl Pts',(-24.4419671033163,54.4291945615863,
3.55127910964207));
#244786=CARTESIAN_POINT('Ctrl Pts',(-24.4761921430394,54.1952354911873,
3.47153072139109));
#244787=CARTESIAN_POINT('Ctrl Pts',(-24.3607210114368,54.2471777873471,
3.47122746281619));
#244788=CARTESIAN_POINT('Ctrl Pts',(-24.4045675740909,54.3451938439592,
3.40413045901312));
#244789=CARTESIAN_POINT('Origin',(-24.5205222915154,54.2933913980364,3.40423097483348));
#244790=CARTESIAN_POINT('Ctrl Pts',(-25.2380597013433,57.4675553545141,
2.90134173516062));
#244791=CARTESIAN_POINT('Ctrl Pts',(-25.3547675996718,57.4161024530844,
2.9016321871643));
#244792=CARTESIAN_POINT('Ctrl Pts',(-25.3107727110825,57.3172883154491,
2.83404198860301));
#244793=CARTESIAN_POINT('Ctrl Pts',(-25.2565651278915,57.5091180232692,
2.82853349835384));
#244794=CARTESIAN_POINT('Ctrl Pts',(-25.352874997054,57.4495672328903,2.8538148316236));
#244795=CARTESIAN_POINT('Ctrl Pts',(-25.3292770036983,57.3588496371392,
2.79182701594351));
#244796=CARTESIAN_POINT('Ctrl Pts',(-25.299797277006,57.5405471770609,2.75468822073698));
#244797=CARTESIAN_POINT('Ctrl Pts',(-25.3720159720864,57.4827148996386,
2.79286913083892));
#244798=CARTESIAN_POINT('Ctrl Pts',(-25.3622324578622,57.3948558336733,
2.7490076329796));
#244799=CARTESIAN_POINT('Ctrl Pts',(-25.4257977880273,57.5636463159496,
2.63954450640416));
#244800=CARTESIAN_POINT('Ctrl Pts',(-25.4538910783598,57.5124644612013,
2.69627684028882));
#244801=CARTESIAN_POINT('Ctrl Pts',(-25.447559735724,57.4360631077224,2.68224356036522));
#244802=CARTESIAN_POINT('Ctrl Pts',(-25.5110385513887,57.553621128909,2.59908178706464));
#244803=CARTESIAN_POINT('Ctrl Pts',(-25.5177778164714,57.5097883065936,
2.65878704321651));
#244804=CARTESIAN_POINT('Ctrl Pts',(-25.5012707422378,57.4400754463041,
2.65878198860301));
#244805=CARTESIAN_POINT('Ctrl Pts',(-25.5918112338797,57.5176823163889,
2.59908173516063));
#244806=CARTESIAN_POINT('Ctrl Pts',(-25.5766462455179,57.4835989537478,
2.658781988603));
#244807=CARTESIAN_POINT('Ctrl Pts',(-25.5480287005721,57.419280924679,2.65878198860301));
#244808=CARTESIAN_POINT('Origin',(-25.1947524379619,57.3689438691197,2.83404198860301));
#244809=CARTESIAN_POINT('Origin',(-24.448062420315,54.1306438627484,3.11913648166798));
#244810=CARTESIAN_POINT('Origin',(-24.3756025490941,53.9678963272935,2.83404198860299));
#244811=CARTESIAN_POINT('Origin',(-25.1222926664895,57.2061965577035,3.11913648177619));
#244812=CARTESIAN_POINT('Origin',(-25.0498328948967,57.0434492461379,3.40423097483349));
#244813=CARTESIAN_POINT('Ctrl Pts',(-24.331269253109,53.8697418420146,2.9013417351606));
#244814=CARTESIAN_POINT('Ctrl Pts',(-24.2159747902189,53.9216078643418,
2.90103711553266));
#244815=CARTESIAN_POINT('Ctrl Pts',(-24.2595822759735,54.0195518809642,
2.83404198860299));
#244816=CARTESIAN_POINT('Ctrl Pts',(-24.3127882662189,53.8282341734839,
2.82862991747986));
#244817=CARTESIAN_POINT('Ctrl Pts',(-24.2176496934283,53.8880114973694,
2.85314045886434));
#244818=CARTESIAN_POINT('Ctrl Pts',(-24.2411010091826,53.9780422761234,
2.79187960999972));
#244819=CARTESIAN_POINT('Ctrl Pts',(-24.2697746459842,53.796995586443,2.7547062579338));
#244820=CARTESIAN_POINT('Ctrl Pts',(-24.1983152114491,53.8549480733042,
2.79224250381927));
#244821=CARTESIAN_POINT('Ctrl Pts',(-24.2082687574725,53.9422730280822,
2.7490180910829));
#244822=CARTESIAN_POINT('Ctrl Pts',(-24.1443388226041,53.7744913425365,
2.63947868311718));
#244823=CARTESIAN_POINT('Ctrl Pts',(-24.1165167429224,53.8256450222191,
2.69595066767952));
#244824=CARTESIAN_POINT('Ctrl Pts',(-24.1232032230476,53.9017956184506,
2.68220539436103));
#244825=CARTESIAN_POINT('Ctrl Pts',(-24.0595120258535,53.7848917482051,
2.59908178585127));
#244826=CARTESIAN_POINT('Ctrl Pts',(-24.0529122166851,53.8286685158653,
2.65877670944914));
#244827=CARTESIAN_POINT('Ctrl Pts',(-24.0696665464387,53.8982652496131,
2.65878198860299));
#244828=CARTESIAN_POINT('Ctrl Pts',(-23.9791663275016,53.8206887816837,
2.5990817351606));
#244829=CARTESIAN_POINT('Ctrl Pts',(-23.994348378682,53.8547645473082,2.65878198860299));
#244830=CARTESIAN_POINT('Ctrl Pts',(-24.0229981225299,53.9190682401996,
2.65878198860299));
#244831=CARTESIAN_POINT('Origin',(-24.0229981225299,53.9190682401996,2.53178198860299));
#244832=CARTESIAN_POINT('Ctrl Pts',(-24.8746050278055,56.6498810128383,
3.77003198860302));
#244833=CARTESIAN_POINT('Ctrl Pts',(-24.9907986398446,56.5981482837088,
3.77003198860302));
#244834=CARTESIAN_POINT('Ctrl Pts',(-24.9906251716318,56.5982255167332,
3.64284238727605));
#244835=CARTESIAN_POINT('Ctrl Pts',(-24.9626539694726,56.8481896769757,
3.77003198860302));
#244836=CARTESIAN_POINT('Ctrl Pts',(-25.0791271905709,56.7965362315773,
3.77025506105699));
#244837=CARTESIAN_POINT('Ctrl Pts',(-25.0612010539378,56.7567415443529,
3.6428421064198));
#244838=CARTESIAN_POINT('Ctrl Pts',(-25.0464771582518,57.0369754593331,
3.6555352798787));
#244839=CARTESIAN_POINT('Ctrl Pts',(-25.1631925873306,56.9853490357227,
3.65585996533181));
#244840=CARTESIAN_POINT('Ctrl Pts',(-25.1283880784745,56.9076460727658,
3.5512790271019));
#244841=CARTESIAN_POINT('Ctrl Pts',(-25.0931373005748,57.1420619865022,
3.47153072139112));
#244842=CARTESIAN_POINT('Ctrl Pts',(-25.2100238867504,57.090533216652,3.47182327905228));
#244843=CARTESIAN_POINT('Ctrl Pts',(-25.1657874977295,56.991646544054,3.4041302837801));
#244844=CARTESIAN_POINT('Origin',(-24.8746050278055,56.6498810128383,3.64303198860302));
#244845=CARTESIAN_POINT('Origin',(3.8811097157961E-16,1.91631020807046E-13,
2.53178198860262));
#244846=CARTESIAN_POINT('Origin',(-23.995153256981,53.9314655730805,2.531781988603));
#244847=CARTESIAN_POINT('Origin',(10.5838037820519,-22.9910091182298,3.64303198860247));
#244848=CARTESIAN_POINT('Origin',(-24.7113125977919,56.2832472948497,3.64299466007609));
#244849=CARTESIAN_POINT('Ctrl Pts',(-23.9513722670367,53.8330634946838,
2.5990817351606));
#244850=CARTESIAN_POINT('Ctrl Pts',(-23.9665367208226,53.8671470951731,
2.65878198860298));
#244851=CARTESIAN_POINT('Ctrl Pts',(-23.995153256981,53.9314655730805,2.65878198860299));
#244852=CARTESIAN_POINT('Ctrl Pts',(-23.8712821658121,53.8686972660502,
2.5990819319995));
#244853=CARTESIAN_POINT('Ctrl Pts',(-23.9081865738555,53.8931046959191,
2.65877685806726));
#244854=CARTESIAN_POINT('Ctrl Pts',(-23.9486256024603,53.9521563342736,
2.65878198860299));
#244855=CARTESIAN_POINT('Ctrl Pts',(-23.8071866393157,53.9240892607411,
2.6387249266983));
#244856=CARTESIAN_POINT('Ctrl Pts',(-23.8635355386145,53.9378509529601,
2.69532212015307));
#244857=CARTESIAN_POINT('Ctrl Pts',(-23.915575084618,53.9937257232528,2.68176836726675));
#244858=CARTESIAN_POINT('Ctrl Pts',(-23.7392497560571,54.0330064121716,
2.75442176402291));
#244859=CARTESIAN_POINT('Ctrl Pts',(-23.8300830854579,54.0187512923761,
2.7920317992018));
#244860=CARTESIAN_POINT('Ctrl Pts',(-23.8883623535218,54.0845104630314,
2.74885310748208));
#244861=CARTESIAN_POINT('Ctrl Pts',(-23.7337507958627,54.086059454542,2.82866089558432));
#244862=CARTESIAN_POINT('Ctrl Pts',(-23.8418399747444,54.0553500291281,
2.85316563119161));
#244863=CARTESIAN_POINT('Ctrl Pts',(-23.8930480394869,54.1330265677741,
2.79189751796665));
#244864=CARTESIAN_POINT('Ctrl Pts',(-23.752222950883,54.1275498658874,2.90134173516061));
#244865=CARTESIAN_POINT('Ctrl Pts',(-23.8679139708571,54.0765745253537,
2.90103711553267));
#244866=CARTESIAN_POINT('Ctrl Pts',(-23.9115214566117,54.174518541976,2.83404198860299));
#244867=CARTESIAN_POINT('Origin',(-23.7955011834911,54.2261740956467,2.83404198860299));
#244868=CARTESIAN_POINT('Origin',(-24.6933715410266,56.2428239368568,3.56647653971843));
#244869=CARTESIAN_POINT('Origin',(-24.6600848917114,56.1680608984279,3.42473028058524));
#244870=CARTESIAN_POINT('Origin',(-23.8679610547528,54.3889216310619,3.11913648168028));
#244871=CARTESIAN_POINT('Origin',(-23.9404209259123,54.5516691663896,3.40423097483349));
#244872=CARTESIAN_POINT('Ctrl Pts',(-24.5258780191674,55.8666273273834,
3.3612302805852));
#244873=CARTESIAN_POINT('Ctrl Pts',(-24.641898292288,55.8149717737127,3.3612302805852));
#244874=CARTESIAN_POINT('Ctrl Pts',(-24.641898292288,55.8149717737127,3.2342302805852));
#244875=CARTESIAN_POINT('Ctrl Pts',(-24.5627025231274,55.948760734758,3.3612302805852));
#244876=CARTESIAN_POINT('Ctrl Pts',(-24.6784744708784,55.8971232158773,
3.36099641108608));
#244877=CARTESIAN_POINT('Ctrl Pts',(-24.6968134595438,55.9383132588145,
3.23423043688449));
#244878=CARTESIAN_POINT('Ctrl Pts',(-24.5975211960717,56.0264248009281,
3.41054258905324));
#244879=CARTESIAN_POINT('Ctrl Pts',(-24.7132325104962,55.9751910510484,
3.41008815825971));
#244880=CARTESIAN_POINT('Ctrl Pts',(-24.7487396569165,56.0549414076424,
3.3081986730429));
#244881=CARTESIAN_POINT('Ctrl Pts',(-24.6158705164596,56.0673542004327,
3.48823028058522));
#244882=CARTESIAN_POINT('Ctrl Pts',(-24.7315703643338,56.0163785451198,
3.48794691941638));
#244883=CARTESIAN_POINT('Ctrl Pts',(-24.776105164832,56.1164053447573,3.42473028058524));
#244884=CARTESIAN_POINT('Origin',(-24.5258780191674,55.8666273273834,3.2342302805852));
#244885=CARTESIAN_POINT('Ctrl Pts',(-23.8971395307771,54.4530463244693,
3.4715307213911));
#244886=CARTESIAN_POINT('Ctrl Pts',(-24.0130054343467,54.4019907365351,
3.47122746285114));
#244887=CARTESIAN_POINT('Ctrl Pts',(-24.0565064908996,54.5001606088507,
3.40413046676809));
#244888=CARTESIAN_POINT('Ctrl Pts',(-23.943793975817,54.558137423042,3.65553813458026));
#244889=CARTESIAN_POINT('Ctrl Pts',(-24.0597061770712,54.5068816478237,
3.65520336072303));
#244890=CARTESIAN_POINT('Ctrl Pts',(-24.0939065860602,54.5841625982689,
3.55128134519959));
#244891=CARTESIAN_POINT('Ctrl Pts',(-24.0276077026098,54.7469293531954,
3.770031988603));
#244892=CARTESIAN_POINT('Ctrl Pts',(-24.1436691352855,54.6954643138445,
3.76980209314153));
#244893=CARTESIAN_POINT('Ctrl Pts',(-24.161094175272,54.7350683949965,3.64284195387456));
#244894=CARTESIAN_POINT('Ctrl Pts',(-24.1156489724279,54.9452378026829,
3.77003198860301));
#244895=CARTESIAN_POINT('Ctrl Pts',(-24.2318430357374,54.893504872635,3.77003198860301));
#244896=CARTESIAN_POINT('Ctrl Pts',(-24.2316691155806,54.8935823068777,
3.6428418940381));
#244897=CARTESIAN_POINT('Origin',(-24.1156489724279,54.9452378026829,3.64303198860301));
#244898=CARTESIAN_POINT('Origin',(10.3344596589369,-22.4309730483566,3.23423028058466));
#244899=CARTESIAN_POINT('Origin',(-24.4643761377919,55.7284918401499,3.2342302805852));
#244900=CARTESIAN_POINT('Origin',(10.2954134679533,-22.3432738675265,3.64303198860247));
#244901=CARTESIAN_POINT('Origin',(-24.2788510342447,55.3119205422646,3.64299171721813));
#244902=CARTESIAN_POINT('Ctrl Pts',(-24.3743766270216,55.5277679687684,
3.4882302805852));
#244903=CARTESIAN_POINT('Ctrl Pts',(-24.4911280468228,55.4763362579875,
3.48852004212298));
#244904=CARTESIAN_POINT('Ctrl Pts',(-24.4461895095991,55.3754026508176,
3.42473028058519));
#244905=CARTESIAN_POINT('Ctrl Pts',(-24.3927905570427,55.5688345658067,
3.41028005848444));
#244906=CARTESIAN_POINT('Ctrl Pts',(-24.5093364964839,55.5172331055217,
3.41074404220413));
#244907=CARTESIAN_POINT('Ctrl Pts',(-24.4736474994205,55.4370743056939,
3.30780486243907));
#244908=CARTESIAN_POINT('Ctrl Pts',(-24.4276751358083,55.6466353090197,
3.3612302805852));
#244909=CARTESIAN_POINT('Ctrl Pts',(-24.5438739850314,55.5948055748758,
3.36146460586418));
#244910=CARTESIAN_POINT('Ctrl Pts',(-24.525666213519,55.5539102504903,3.23423045308528));
#244911=CARTESIAN_POINT('Ctrl Pts',(-24.4643761377919,55.7284918401499,
3.3612302805852));
#244912=CARTESIAN_POINT('Ctrl Pts',(-24.5803964109126,55.6768362864793,
3.36123028058519));
#244913=CARTESIAN_POINT('Ctrl Pts',(-24.5803964109126,55.6768362864792,
3.2342302805852));
#244914=CARTESIAN_POINT('Origin',(-24.3301692364785,55.4270582044882,3.42473028058519));
#244915=CARTESIAN_POINT('Origin',(-24.2970811017194,55.3527410377817,3.56563113524755));
#244916=CARTESIAN_POINT('Origin',(-30.9870007556519,53.0360596835511,3.56647653909477));
#244917=CARTESIAN_POINT('Origin',(-31.0091584503732,53.0743345559675,3.64299466007354));
#244918=CARTESIAN_POINT('Origin',(-30.9460815882871,52.9651856060846,3.4247302805852));
#244919=CARTESIAN_POINT('Ctrl Pts',(-30.8905967158739,52.8702215132216,
3.4882302805852));
#244920=CARTESIAN_POINT('Ctrl Pts',(-30.7813498801535,52.9338619179796,
3.48794691941636));
#244921=CARTESIAN_POINT('Ctrl Pts',(-30.8360963620065,53.0286856060846,
3.42473028058521));
#244922=CARTESIAN_POINT('Ctrl Pts',(-30.8681941459792,52.8311874403356,
3.41028005925123));
#244923=CARTESIAN_POINT('Ctrl Pts',(-30.7587310665078,52.89468498354,3.40982512231133));
#244924=CARTESIAN_POINT('Ctrl Pts',(-30.8023423591859,52.9702219582407,
3.3078048637286));
#244925=CARTESIAN_POINT('Ctrl Pts',(-30.8257530395495,52.757237252247,3.36123028058518));
#244926=CARTESIAN_POINT('Ctrl Pts',(-30.7159277273256,52.8205474253446,
3.36099721048368));
#244927=CARTESIAN_POINT('Ctrl Pts',(-30.7383959430073,52.8594635164573,
3.23423045308469));
#244928=CARTESIAN_POINT('Ctrl Pts',(-30.7811015270746,52.6794317578288,
3.36123028058517));
#244929=CARTESIAN_POINT('Ctrl Pts',(-30.671116300794,52.7429317578288,3.36123028058517));
#244930=CARTESIAN_POINT('Ctrl Pts',(-30.671116300794,52.7429317578288,3.23423028058518));
#244931=CARTESIAN_POINT('Origin',(-30.7811015270746,52.6794317578288,3.23423028058517));
#244932=CARTESIAN_POINT('Origin',(-0.274963065701553,-0.158749999999817,
3.64303198860263));
#244933=CARTESIAN_POINT('Origin',(-31.2097904767608,53.4219427993287,3.64303198860299));
#244934=CARTESIAN_POINT('Origin',(-0.274963065701553,-0.158749999999815,
3.23423028058481));
#244935=CARTESIAN_POINT('Origin',(-30.7054974692372,52.5484816883959,3.23423028058517));
#244936=CARTESIAN_POINT('Ctrl Pts',(-31.4795232016792,53.8880358395971,
3.47153072139108));
#244937=CARTESIAN_POINT('Ctrl Pts',(-31.3691313491574,53.9523112176915,
3.47182327902699));
#244938=CARTESIAN_POINT('Ctrl Pts',(-31.3151318426936,53.8583991130128,
3.40413028959054));
#244939=CARTESIAN_POINT('Ctrl Pts',(-31.4219316852005,53.7885171709487,
3.65553807120994));
#244940=CARTESIAN_POINT('Ctrl Pts',(-31.3115614337831,53.8525966788921,
3.65586275496921));
#244941=CARTESIAN_POINT('Ctrl Pts',(-31.2691561625559,53.7787668993609,
3.55128126837211));
#244942=CARTESIAN_POINT('Ctrl Pts',(-31.3184699958136,53.6097358757351,
3.770031988603));
#244943=CARTESIAN_POINT('Ctrl Pts',(-31.2082202476926,53.6736035436622,
3.77025505748471));
#244944=CARTESIAN_POINT('Ctrl Pts',(-31.1865627224596,53.6357108652094,
3.64284211731288));
#244945=CARTESIAN_POINT('Ctrl Pts',(-31.2097904767608,53.4219427993287,
3.770031988603));
#244946=CARTESIAN_POINT('Ctrl Pts',(-31.099640937652,53.4855376653843,3.770031988603));
#244947=CARTESIAN_POINT('Ctrl Pts',(-31.0998053730349,53.4854427285717,
3.64284239821717));
#244948=CARTESIAN_POINT('Origin',(-31.4251975098795,53.7950387249979,3.40423097483346));
#244949=CARTESIAN_POINT('Ctrl Pts',(-30.7054974692372,52.548481688396,3.36123028058517));
#244950=CARTESIAN_POINT('Ctrl Pts',(-30.5955122429565,52.611981688396,3.36123028058518));
#244951=CARTESIAN_POINT('Ctrl Pts',(-30.5955122429565,52.611981688396,3.23423028058518));
#244952=CARTESIAN_POINT('Ctrl Pts',(-30.6606955449566,52.4704129317487,
3.36123028058518));
#244953=CARTESIAN_POINT('Ctrl Pts',(-30.550463706539,52.5339553345181,3.36146538610162));
#244954=CARTESIAN_POINT('Ctrl Pts',(-30.5280052047886,52.4950560684206,
3.23423043688486));
#244955=CARTESIAN_POINT('Ctrl Pts',(-30.6183335281992,52.3965920780923,
3.41054258693136));
#244956=CARTESIAN_POINT('Ctrl Pts',(-30.5080831175509,52.460550001133,3.41100608859922));
#244957=CARTESIAN_POINT('Ctrl Pts',(-30.4641724871923,52.3844945583586,
3.30819866970894));
#244958=CARTESIAN_POINT('Ctrl Pts',(-30.5960088312571,52.3576880233162,
3.48823028058517));
#244959=CARTESIAN_POINT('Ctrl Pts',(-30.4857749404422,52.4219111049557,
3.48852004212295));
#244960=CARTESIAN_POINT('Ctrl Pts',(-30.4305321463779,52.3262277788842,
3.42473028058517));
#244961=CARTESIAN_POINT('Origin',(-30.5405173726585,52.2627277788841,3.42473028058517));
#244962=CARTESIAN_POINT('Origin',(-31.5142720656054,53.9493203812247,3.11913648178448));
#244963=CARTESIAN_POINT('Origin',(-31.6033466212668,54.1036020372439,2.83404198860299));
#244964=CARTESIAN_POINT('Origin',(-30.4998422386358,52.1922763801653,3.56563113460844));
#244965=CARTESIAN_POINT('Origin',(-30.4775331296739,52.1535342613182,3.64299171721854));
#244966=CARTESIAN_POINT('Ctrl Pts',(-31.490293248291,54.5122556166611,2.5990817351606));
#244967=CARTESIAN_POINT('Ctrl Pts',(-31.4716329851992,54.4799531854479,
2.65878198860299));
#244968=CARTESIAN_POINT('Ctrl Pts',(-31.4364195775137,54.4189959163064,
2.65878198860299));
#244969=CARTESIAN_POINT('Ctrl Pts',(-31.566592666262,54.4681793099462,2.59908193475589));
#244970=CARTESIAN_POINT('Ctrl Pts',(-31.5272089901455,54.4478446647271,
2.65878715325492));
#244971=CARTESIAN_POINT('Ctrl Pts',(-31.4805801312544,54.3934750329635,
2.65878198860299));
#244972=CARTESIAN_POINT('Ctrl Pts',(-31.6244843104272,54.4058464214487,
2.63878778849906));
#244973=CARTESIAN_POINT('Ctrl Pts',(-31.5668246399999,54.3982481205276,
2.69564460180167));
#244974=CARTESIAN_POINT('Ctrl Pts',(-31.5088182930362,54.3482630350912,
2.68180481624915));
#244975=CARTESIAN_POINT('Ctrl Pts',(-31.6805188761701,54.2895863184077,
2.75443238878683));
#244976=CARTESIAN_POINT('Ctrl Pts',(-31.5913182835554,54.313947642815,2.79268340777106));
#244977=CARTESIAN_POINT('Ctrl Pts',(-31.5259511417533,54.2544636505344,
2.74885926835652));
#244978=CARTESIAN_POINT('Ctrl Pts',(-31.6804069909878,54.2359839591654,
2.82856655361705));
#244979=CARTESIAN_POINT('Ctrl Pts',(-31.5756141966206,54.2789047974521,
2.8538419723087));
#244980=CARTESIAN_POINT('Ctrl Pts',(-31.5160982999436,54.2064835118371,
2.79184624278552));
#244981=CARTESIAN_POINT('Ctrl Pts',(-31.6576696180587,54.1966007261208,
2.9013417351606));
#244982=CARTESIAN_POINT('Ctrl Pts',(-31.5474441649286,54.2607761425983,
2.90163218716428));
#244983=CARTESIAN_POINT('Ctrl Pts',(-31.4933613949861,54.1671020372439,
2.83404198860299));
#244984=CARTESIAN_POINT('Origin',(-31.4364195775137,54.4189959163064,2.53178198860298));
#244985=CARTESIAN_POINT('Origin',(-0.274963065701553,-0.158749999999817,
3.64303198860263));
#244986=CARTESIAN_POINT('Origin',(-30.2768083268883,51.8059703131947,3.64303198860298));
#244987=CARTESIAN_POINT('Origin',(5.22371297615238E-17,1.9143463616941E-13,
2.53178198860262));
#244988=CARTESIAN_POINT('Origin',(-31.4100231232064,54.4342359163063,2.53178198860299));
#244989=CARTESIAN_POINT('Ctrl Pts',(-30.2768083268883,51.8059703131947,
3.77003198860299));
#244990=CARTESIAN_POINT('Ctrl Pts',(-30.1666583377716,51.8695654390624,
3.77003198860298));
#244991=CARTESIAN_POINT('Ctrl Pts',(-30.166823223834,51.8694702420499,3.6428418793701));
#244992=CARTESIAN_POINT('Ctrl Pts',(-30.16812109391,51.6181777324911,3.77003198860298));
#244993=CARTESIAN_POINT('Ctrl Pts',(-30.0582657983062,51.6818230251234,
3.76980208963163));
#244994=CARTESIAN_POINT('Ctrl Pts',(-30.0800643400516,51.7191994478449,
3.64284193928342));
#244995=CARTESIAN_POINT('Ctrl Pts',(-30.0646505034496,51.4394033023499,
3.65553535416622));
#244996=CARTESIAN_POINT('Ctrl Pts',(-29.9550522173019,51.5030508615802,
3.65520057834434));
#244997=CARTESIAN_POINT('Ctrl Pts',(-29.997471514536,51.5761444782058,3.55127910964262));
#244998=CARTESIAN_POINT('Ctrl Pts',(-30.007053683816,51.3398895692697,3.47153072139107));
#244999=CARTESIAN_POINT('Ctrl Pts',(-29.8976445635498,51.403617340035,3.47122746281617));
#245000=CARTESIAN_POINT('Ctrl Pts',(-29.9514963979201,51.4965132406197,
3.4041304590127));
#245001=CARTESIAN_POINT('Origin',(-30.0614010732039,51.4328740054943,3.40423097483345));
#245002=CARTESIAN_POINT('Ctrl Pts',(-31.1067982185537,54.5146464769138,
2.90134173516061));
#245003=CARTESIAN_POINT('Ctrl Pts',(-31.2174884860867,54.4512761425983,
2.90163218716428));
#245004=CARTESIAN_POINT('Ctrl Pts',(-31.1634057161443,54.3576020372439,
2.83404198860299));
#245005=CARTESIAN_POINT('Ctrl Pts',(-31.1295467523322,54.5540471172221,
2.82853349835397));
#245006=CARTESIAN_POINT('Ctrl Pts',(-31.2191042733515,54.4847554296828,
2.85381483162437));
#245007=CARTESIAN_POINT('Ctrl Pts',(-31.1861529813966,54.3970014563942,
2.79182701594386));
#245008=CARTESIAN_POINT('Ctrl Pts',(-31.1758273123591,54.5807851087098,
2.75468822073672));
#245009=CARTESIAN_POINT('Ctrl Pts',(-31.2416052667856,54.5157207333386,
2.79286913083887));
#245010=CARTESIAN_POINT('Ctrl Pts',(-31.2226915745265,54.4293656242365,
2.74900763297948));
#245011=CARTESIAN_POINT('Ctrl Pts',(-31.3035520968883,54.5905870683103,
2.63954450640437));
#245012=CARTESIAN_POINT('Ctrl Pts',(-31.3261415286126,54.5367490446508,
2.69627684028885));
#245013=CARTESIAN_POINT('Ctrl Pts',(-31.3118587536635,54.4614280312966,
2.6822435603653));
#245014=CARTESIAN_POINT('Ctrl Pts',(-31.3872779850338,54.5717067142919,
2.59908178706413));
#245015=CARTESIAN_POINT('Ctrl Pts',(-31.3893985541597,54.5274095677402,
2.65878704321626));
#245016=CARTESIAN_POINT('Ctrl Pts',(-31.3656949292513,54.4598040608986,
2.65878198860299));
#245017=CARTESIAN_POINT('Ctrl Pts',(-31.4638515574743,54.527521733972,2.5990817351606));
#245018=CARTESIAN_POINT('Ctrl Pts',(-31.4452069629856,54.4952102564866,
2.65878198860298));
#245019=CARTESIAN_POINT('Ctrl Pts',(-31.4100231232064,54.4342359163063,
2.65878198860299));
#245020=CARTESIAN_POINT('Origin',(-31.0534204898636,54.4211020372439,2.83404198860299));
#245021=CARTESIAN_POINT('Origin',(-29.9723263949899,51.2785921372171,3.11913648167029));
#245022=CARTESIAN_POINT('Origin',(-29.8832517167489,51.1243102687785,2.83404198860297));
#245023=CARTESIAN_POINT('Origin',(-30.9643459342328,54.2668203811892,3.11913648177482));
#245024=CARTESIAN_POINT('Origin',(-30.8752713784764,54.1125387249979,3.40423097483347));
#245025=CARTESIAN_POINT('Ctrl Pts',(-29.8289013456888,51.0313275753409,
2.90134173516058));
#245026=CARTESIAN_POINT('Ctrl Pts',(-29.7196599535395,51.0949610232002,
2.90103711553264));
#245027=CARTESIAN_POINT('Ctrl Pts',(-29.7732664904682,51.1878102687785,
2.83404198860297));
#245028=CARTESIAN_POINT('Ctrl Pts',(-29.8061828667728,50.991979079321,2.82862991747989));
#245029=CARTESIAN_POINT('Ctrl Pts',(-29.7178139048439,51.0613736255813,
2.8531404588653));
#245030=CARTESIAN_POINT('Ctrl Pts',(-29.7505475307857,51.1484598763132,
2.79187960999984));
#245031=CARTESIAN_POINT('Ctrl Pts',(-29.7601395581528,50.9654077681508,
2.7547062579337));
#245032=CARTESIAN_POINT('Ctrl Pts',(-29.695129270271,51.0305123301031,2.79224250381932));
#245033=CARTESIAN_POINT('Ctrl Pts',(-29.7141562330556,51.1163184807721,
2.74901809108292));
#245034=CARTESIAN_POINT('Ctrl Pts',(-29.6330385513051,50.9561384187039,
2.63947868311724));
#245035=CARTESIAN_POINT('Ctrl Pts',(-29.6107158994147,51.0099200724111,
2.69595066767946));
#245036=CARTESIAN_POINT('Ctrl Pts',(-29.6253256551032,51.0849545802165,
2.68220539436098));
#245037=CARTESIAN_POINT('Ctrl Pts',(-29.5497635830448,50.9753486645705,
2.59908178585179));
#245038=CARTESIAN_POINT('Ctrl Pts',(-29.5477758465718,51.019575486427,2.65877670944799));
#245039=CARTESIAN_POINT('Ctrl Pts',(-29.5717132339817,51.0870396576443,
2.65878198860297));
#245040=CARTESIAN_POINT('Ctrl Pts',(-29.473599835734,51.0193480105328,2.59908173516058));
#245041=CARTESIAN_POINT('Ctrl Pts',(-29.4922606054649,51.0516501490686,
2.65878198860297));
#245042=CARTESIAN_POINT('Ctrl Pts',(-29.5274749692187,51.1126068659047,
2.65878198860297));
#245043=CARTESIAN_POINT('Origin',(-29.5274749692187,51.1126068659048,2.53178198860297));
#245044=CARTESIAN_POINT('Ctrl Pts',(-30.6598643453577,53.7394427993287,
3.770031988603));
#245045=CARTESIAN_POINT('Ctrl Pts',(-30.7700138939558,53.6758479277944,
3.770031988603));
#245046=CARTESIAN_POINT('Ctrl Pts',(-30.7698494490696,53.6759428700938,
3.64284238727623));
#245047=CARTESIAN_POINT('Ctrl Pts',(-30.7681598456252,53.9274614872894,
3.770031988603));
#245048=CARTESIAN_POINT('Ctrl Pts',(-30.8785957589627,53.863916238056,3.7702550610604));
#245049=CARTESIAN_POINT('Ctrl Pts',(-30.8566081460792,53.8262133418089,
3.64284210641982));
#245050=CARTESIAN_POINT('Ctrl Pts',(-30.8712573299214,54.1064511722693,
3.6555352798787));
#245051=CARTESIAN_POINT('Ctrl Pts',(-30.9819369489455,54.0429074791663,
3.6558599653291));
#245052=CARTESIAN_POINT('Ctrl Pts',(-30.9392009315185,53.9692682429957,
3.55127902710151));
#245053=CARTESIAN_POINT('Ctrl Pts',(-30.9286463962981,54.2060847114742,
3.4715307213911));
#245054=CARTESIAN_POINT('Ctrl Pts',(-31.0395064423978,54.1426202463874,
3.47182327905226));
#245055=CARTESIAN_POINT('Ctrl Pts',(-30.9851759130205,54.0488992470934,
3.40413028378019));
#245056=CARTESIAN_POINT('Origin',(-30.6598643453577,53.7394427993287,3.643031988603));
#245057=CARTESIAN_POINT('Origin',(3.8264039982802E-16,1.91628233411515E-13,
2.53178198860262));
#245058=CARTESIAN_POINT('Origin',(-29.5010785149114,51.1278468659047,2.53178198860297));
#245059=CARTESIAN_POINT('Origin',(15.8305769983926,-26.7843636743467,3.64303198860244));
#245060=CARTESIAN_POINT('Origin',(-30.4591427892365,53.3918862459827,3.64299466007577));
#245061=CARTESIAN_POINT('Ctrl Pts',(-29.4472515437738,51.0345602039887,
2.59908173516058));
#245062=CARTESIAN_POINT('Ctrl Pts',(-29.4658956314769,51.0668719738978,
2.65878198860297));
#245063=CARTESIAN_POINT('Ctrl Pts',(-29.5010785149114,51.1278468659047,
2.65878198860297));
#245064=CARTESIAN_POINT('Ctrl Pts',(-29.3713249278652,51.0783704650312,
2.59908193199997));
#245065=CARTESIAN_POINT('Ctrl Pts',(-29.4105784408376,51.0987866273871,
2.65877685806747));
#245066=CARTESIAN_POINT('Ctrl Pts',(-29.4569685172222,51.1532877451704,
2.65878198860297));
#245067=CARTESIAN_POINT('Ctrl Pts',(-29.3133705634514,51.1401588234664,
2.63872492669834));
#245068=CARTESIAN_POINT('Ctrl Pts',(-29.3708492661237,51.1479550638448,
2.69532212015298));
#245069=CARTESIAN_POINT('Ctrl Pts',(-29.4284442379232,51.1980841325265,
2.68176836726662));
#245070=CARTESIAN_POINT('Ctrl Pts',(-29.2571907880104,51.2555806533512,
2.75442176402282));
#245071=CARTESIAN_POINT('Ctrl Pts',(-29.3460364571626,51.231908956258,2.79203179920187));
#245072=CARTESIAN_POINT('Ctrl Pts',(-29.4108701703527,51.291216048965,2.74885310748217));
#245073=CARTESIAN_POINT('Ctrl Pts',(-29.2572675046848,51.3089178634639,
2.82866089558435));
#245074=CARTESIAN_POINT('Ctrl Pts',(-29.3615545506875,51.2670782717307,
2.85316563119275));
#245075=CARTESIAN_POINT('Ctrl Pts',(-29.4206015015119,51.3389765898555,
2.79189751796689));
#245076=CARTESIAN_POINT('Ctrl Pts',(-29.2799753962465,51.3482501200166,
2.90134173516058));
#245077=CARTESIAN_POINT('Ctrl Pts',(-29.3897042746976,51.2854610232002,
2.90103711553264));
#245078=CARTESIAN_POINT('Ctrl Pts',(-29.4433108116264,51.3783102687785,
2.83404198860296));
#245079=CARTESIAN_POINT('Origin',(-29.3333255853457,51.4418102687785,2.83404198860297));
#245080=CARTESIAN_POINT('Origin',(-30.437074623967,53.3535596824666,3.56647653971834));
#245081=CARTESIAN_POINT('Origin',(-30.396155456884,53.2826856060846,3.42473028058522));
#245082=CARTESIAN_POINT('Origin',(-29.4224002636271,51.5960921371734,3.11913648168138));
#245083=CARTESIAN_POINT('Origin',(-29.5114749418008,51.7503740054943,3.40423097483346));
#245084=CARTESIAN_POINT('Ctrl Pts',(-30.2311753956715,52.9969317578288,
3.36123028058518));
#245085=CARTESIAN_POINT('Ctrl Pts',(-30.3411606219521,52.9334317578288,
3.36123028058518));
#245086=CARTESIAN_POINT('Ctrl Pts',(-30.3411606219521,52.9334317578288,
3.23423028058518));
#245087=CARTESIAN_POINT('Ctrl Pts',(-30.2763834500034,53.0747660209935,
3.36123028058517));
#245088=CARTESIAN_POINT('Ctrl Pts',(-30.3861235964137,53.0113099140535,
3.36099641108513));
#245089=CARTESIAN_POINT('Ctrl Pts',(-30.4086676540701,53.0503573673254,
3.23423043688446));
#245090=CARTESIAN_POINT('Ctrl Pts',(-30.3191294880994,53.1483650929086,
3.4105425890532));
#245091=CARTESIAN_POINT('Ctrl Pts',(-30.4288515386952,53.0853168809963,
3.41008815825925));
#245092=CARTESIAN_POINT('Ctrl Pts',(-30.4725003554725,53.1609188493387,
3.30819867304248));
#245093=CARTESIAN_POINT('Ctrl Pts',(-30.3416565762239,53.1871522506175,
3.4882302805852));
#245094=CARTESIAN_POINT('Ctrl Pts',(-30.4513942013116,53.1243619179796,
3.48794691941636));
#245095=CARTESIAN_POINT('Ctrl Pts',(-30.5061406831646,53.2191856060846,
3.42473028058521));
#245096=CARTESIAN_POINT('Origin',(-30.2311753956715,52.9969317578288,3.23423028058518));
#245097=CARTESIAN_POINT('Ctrl Pts',(-29.4581217525676,51.6568155675428,
3.47153072139108));
#245098=CARTESIAN_POINT('Ctrl Pts',(-29.5680161684457,51.5939283826163,
3.47122746285112));
#245099=CARTESIAN_POINT('Ctrl Pts',(-29.6215404675518,51.687013371507,3.40413046676838));
#245100=CARTESIAN_POINT('Ctrl Pts',(-29.5155056307129,51.7564542486371,
3.65553813458023));
#245101=CARTESIAN_POINT('Ctrl Pts',(-29.6254251653839,51.6933631336535,
3.65520336072106));
#245102=CARTESIAN_POINT('Ctrl Pts',(-29.6675162799456,51.7666458147686,
3.55128134519885));
#245103=CARTESIAN_POINT('Ctrl Pts',(-29.6185943474775,51.9354510367807,
3.77003198860299));
#245104=CARTESIAN_POINT('Ctrl Pts',(-29.7286404220038,51.8721362050945,
3.76980209314207));
#245105=CARTESIAN_POINT('Ctrl Pts',(-29.7501097595399,51.9097019182946,
3.64284195387509));
#245106=CARTESIAN_POINT('Ctrl Pts',(-29.7268821954852,52.1234703131947,
3.77003198860299));
#245107=CARTESIAN_POINT('Ctrl Pts',(-29.8370321718796,52.0598751946722,
3.77003198860299));
#245108=CARTESIAN_POINT('Ctrl Pts',(-29.8368672985585,52.0599703843284,
3.64284189403866));
#245109=CARTESIAN_POINT('Origin',(-29.7268821954852,52.1234703131947,3.64303198860299));
#245110=CARTESIAN_POINT('Origin',(15.4537755657018,-26.1317244485615,3.23423028058463));
#245111=CARTESIAN_POINT('Origin',(-30.155571337834,52.865981688396,3.23423028058518));
#245112=CARTESIAN_POINT('Origin',(15.3947701216595,-26.0295240215571,3.64303198860244));
#245113=CARTESIAN_POINT('Origin',(-29.9275190026067,52.4710850656384,3.64299171721842));
#245114=CARTESIAN_POINT('Ctrl Pts',(-30.0450834959839,52.6757649139396,
3.48823028058517));
#245115=CARTESIAN_POINT('Ctrl Pts',(-30.1558192616004,52.6124111049557,
3.48852004212295));
#245116=CARTESIAN_POINT('Ctrl Pts',(-30.100576467536,52.5167277788842,3.42473028058517));
#245117=CARTESIAN_POINT('Ctrl Pts',(-30.0676891808483,52.7146817640555,
3.41028005848446));
#245118=CARTESIAN_POINT('Ctrl Pts',(-30.1782028480936,52.6511806140212,
3.41074404220526));
#245119=CARTESIAN_POINT('Ctrl Pts',(-30.1343304829282,52.5751914485028,
3.30780486243987));
#245120=CARTESIAN_POINT('Ctrl Pts',(-30.1105150503705,52.7884098752467,
3.36123028058518));
#245121=CARTESIAN_POINT('Ctrl Pts',(-30.2206596676762,52.7247179826659,
3.36146460586334));
#245122=CARTESIAN_POINT('Ctrl Pts',(-30.198276914831,52.6859499175213,3.23423045308457));
#245123=CARTESIAN_POINT('Ctrl Pts',(-30.155571337834,52.865981688396,3.36123028058518));
#245124=CARTESIAN_POINT('Ctrl Pts',(-30.2655565641147,52.802481688396,3.36123028058518));
#245125=CARTESIAN_POINT('Ctrl Pts',(-30.2655565641147,52.802481688396,3.23423028058518));
#245126=CARTESIAN_POINT('Origin',(-29.9905912412554,52.5802277788842,3.42473028058516));
#245127=CARTESIAN_POINT('Origin',(-29.9499161075312,52.5097763812718,3.56563113524792));
#245128=CARTESIAN_POINT('Origin',(-36.3610285397818,49.5064990290886,3.56647653909468));
#245129=CARTESIAN_POINT('Origin',(-36.3870656659258,49.5422481179709,3.64299466007638));
#245130=CARTESIAN_POINT('Origin',(-36.3129251734945,49.4402904249166,3.42473028058517));
#245131=CARTESIAN_POINT('Ctrl Pts',(-36.2478178023253,49.3516463037385,
3.48823028058518));
#245132=CARTESIAN_POINT('Ctrl Pts',(-36.1458216659127,49.4263574835551,
3.48794691941634));
#245133=CARTESIAN_POINT('Ctrl Pts',(-36.2101800152089,49.5149391519577,
3.42473028058519));
#245134=CARTESIAN_POINT('Ctrl Pts',(-36.2214577843987,49.3151677697922,
3.41028005925121));
#245135=CARTESIAN_POINT('Ctrl Pts',(-36.119231655743,49.3897594742935,3.40982512230947));
#245136=CARTESIAN_POINT('Ctrl Pts',(-36.1704998050837,49.4603240281409,
3.30780486372769));
#245137=CARTESIAN_POINT('Ctrl Pts',(-36.1715192752718,49.2460589922057,
3.36123028058515));
#245138=CARTESIAN_POINT('Ctrl Pts',(-36.0689133127008,49.320502216666,3.36099721048578));
#245139=CARTESIAN_POINT('Ctrl Pts',(-36.0953262843463,49.3568565532997,
3.23423045308452));
#245140=CARTESIAN_POINT('Ctrl Pts',(-36.1189794796885,49.1733470784087,
3.36123028058515));
#245141=CARTESIAN_POINT('Ctrl Pts',(-36.0162343214029,49.2479958054499,
3.36123028058515));
#245142=CARTESIAN_POINT('Ctrl Pts',(-36.0162343214029,49.2479958054499,
3.23423028058515));
#245143=CARTESIAN_POINT('Origin',(-36.1189794796885,49.1733470784087,3.23423028058515));
#245144=CARTESIAN_POINT('Origin',(-0.256862895714039,-0.186621817602678,
3.64303198860262));
#245145=CARTESIAN_POINT('Origin',(-36.6229335645812,49.8669803696026,3.64303198860296));
#245146=CARTESIAN_POINT('Origin',(-0.256862895714039,-0.186621817602675,
3.23423028058481));
#245147=CARTESIAN_POINT('Origin',(-36.0301015792679,49.0510171431404,3.23423028058515));
#245148=CARTESIAN_POINT('Ctrl Pts',(-36.9399086546489,50.3023253561995,
3.47153072139106));
#245149=CARTESIAN_POINT('Ctrl Pts',(-36.836840146744,50.3777877177487,3.47182327902697));
#245150=CARTESIAN_POINT('Ctrl Pts',(-36.7733199672423,50.2900345588339,
3.40413028959065));
#245151=CARTESIAN_POINT('Ctrl Pts',(-36.8722300970236,50.2093718139452,
3.65553807120991));
#245152=CARTESIAN_POINT('Ctrl Pts',(-36.7691625978843,50.2846371204111,
3.65586275496825));
#245153=CARTESIAN_POINT('Ctrl Pts',(-36.7192723137702,50.2156443459715,
3.55128126837211));
#245154=CARTESIAN_POINT('Ctrl Pts',(-36.7506474475451,50.042384592773,3.77003198860298));
#245155=CARTESIAN_POINT('Ctrl Pts',(-36.6476776482601,50.1174266236792,
3.77025505748624));
#245156=CARTESIAN_POINT('Ctrl Pts',(-36.6221779017714,50.0820053531149,
3.64284211731276));
#245157=CARTESIAN_POINT('Ctrl Pts',(-36.6229335645812,49.8669803696026,
3.77003198860297));
#245158=CARTESIAN_POINT('Ctrl Pts',(-36.5200349097935,49.9417406183804,
3.77003198860298));
#245159=CARTESIAN_POINT('Ctrl Pts',(-36.5201885207827,49.9416290134639,
3.6428423982174));
#245160=CARTESIAN_POINT('Origin',(-36.8761597191957,50.2155162706044,3.40423097483344));
#245161=CARTESIAN_POINT('Ctrl Pts',(-36.0301015792679,49.0510171431404,
3.36123028058515));
#245162=CARTESIAN_POINT('Ctrl Pts',(-35.9273564209823,49.1256658701815,
3.36123028058514));
#245163=CARTESIAN_POINT('Ctrl Pts',(-35.9273564209823,49.1256658701815,
3.23423028058515));
#245164=CARTESIAN_POINT('Ctrl Pts',(-35.9773846774562,48.9780591316059,
3.36123028058515));
#245165=CARTESIAN_POINT('Ctrl Pts',(-35.8743986902969,49.0527758071183,
3.36146538610325));
#245166=CARTESIAN_POINT('Ctrl Pts',(-35.8479971380602,49.016437187946,3.23423043688466));
#245167=CARTESIAN_POINT('Ctrl Pts',(-35.927538343867,48.9090707128239,3.41054258693134));
#245168=CARTESIAN_POINT('Ctrl Pts',(-35.8245773199118,48.9842025736696,
3.41100608859765));
#245169=CARTESIAN_POINT('Ctrl Pts',(-35.7729572780264,48.9131536812808,
3.30819866970901));
#245170=CARTESIAN_POINT('Ctrl Pts',(-35.9012693628907,48.8727133447944,
3.48823028058515));
#245171=CARTESIAN_POINT('Ctrl Pts',(-35.7983524848938,48.9481071848797,
3.48852004212292));
#245172=CARTESIAN_POINT('Ctrl Pts',(-35.7334106856009,48.85872246645,3.42473028058514));
#245173=CARTESIAN_POINT('Origin',(-35.8361558438865,48.7840737394089,3.42473028058514));
#245174=CARTESIAN_POINT('Origin',(-36.9808731396222,50.3596419293465,3.11913648178346));
#245175=CARTESIAN_POINT('Origin',(-37.0855865599605,50.5037675878945,2.83404198860296));
#245176=CARTESIAN_POINT('Origin',(-35.7883393560616,48.7182599900759,3.56563113460856));
#245177=CARTESIAN_POINT('Origin',(-35.7621028045853,48.6820620414862,3.64299171721815));
#245178=CARTESIAN_POINT('Ctrl Pts',(-37.0158684358562,50.92199981559,2.59908173516058));
#245179=CARTESIAN_POINT('Ctrl Pts',(-36.9939338721435,50.8918248691,2.65878198860296));
#245180=CARTESIAN_POINT('Ctrl Pts',(-36.9525415975215,50.8348823336486,
2.65878198860296));
#245181=CARTESIAN_POINT('Ctrl Pts',(-37.0871426490251,50.8701895025862,
2.59908193475566));
#245182=CARTESIAN_POINT('Ctrl Pts',(-37.0458491715926,50.8540829678254,
2.6587871532543));
#245183=CARTESIAN_POINT('Ctrl Pts',(-36.9937925764114,50.8048852215561,
2.65878198860296));
#245184=CARTESIAN_POINT('Ctrl Pts',(-37.1382015956599,50.8021467555735,
2.63878778849934));
#245185=CARTESIAN_POINT('Ctrl Pts',(-37.0800635522212,50.8006171556815,
2.69564460180152));
#245186=CARTESIAN_POINT('Ctrl Pts',(-37.0171501059291,50.7569692080812,
2.68180481624921));
#245187=CARTESIAN_POINT('Ctrl Pts',(-37.1817767082792,50.6806663304943,
2.75443238878651));
#245188=CARTESIAN_POINT('Ctrl Pts',(-37.0956112176478,50.7142182018865,
2.7926834077713));
#245189=CARTESIAN_POINT('Ctrl Pts',(-37.0243843935852,50.6618927960202,
2.74885926835641));
#245190=CARTESIAN_POINT('Ctrl Pts',(-37.176062463776,50.6273693057705,2.82856655361725));
#245191=CARTESIAN_POINT('Ctrl Pts',(-37.0763301845674,50.6810088489708,
2.8538419723077));
#245192=CARTESIAN_POINT('Ctrl Pts',(-37.0095702365079,50.6152053999551,
2.79184624278479));
#245193=CARTESIAN_POINT('Ctrl Pts',(-37.1493329797263,50.5905785208484,
2.90134173516059));
#245194=CARTESIAN_POINT('Ctrl Pts',(-37.0464195108255,50.6659240749083,
2.90163218716426));
#245195=CARTESIAN_POINT('Ctrl Pts',(-36.9828414016749,50.5784163149357,
2.83404198860297));
#245196=CARTESIAN_POINT('Origin',(-36.9525415975215,50.8348823336486,2.53178198860296));
#245197=CARTESIAN_POINT('Origin',(-0.256862895714039,-0.186621817602678,
3.64303198860262));
#245198=CARTESIAN_POINT('Origin',(-35.5261472678868,48.3573835402119,3.64303198860295));
#245199=CARTESIAN_POINT('Origin',(6.67120042669033E-17,1.91444036262824E-13,
2.53178198860262));
#245200=CARTESIAN_POINT('Origin',(-36.9278827595329,50.8527980281385,2.53178198860296));
#245201=CARTESIAN_POINT('Ctrl Pts',(-35.5261472678868,48.3573835402119,
3.77003198860296));
#245202=CARTESIAN_POINT('Ctrl Pts',(-35.4232481927148,48.4321440944168,
3.77003198860297));
#245203=CARTESIAN_POINT('Ctrl Pts',(-35.4234022247158,48.4320321836174,
3.6428418793712));
#245204=CARTESIAN_POINT('Ctrl Pts',(-35.3984257650681,48.1819806163551,
3.77003198860296));
#245205=CARTESIAN_POINT('Ctrl Pts',(-35.2958250128973,48.2567602586438,
3.76980208962953));
#245206=CARTESIAN_POINT('Ctrl Pts',(-35.321411039981,48.2916533613383,3.6428419392844));
#245207=CARTESIAN_POINT('Ctrl Pts',(-35.2768349808748,48.0150011530616,
3.65553535416619));
#245208=CARTESIAN_POINT('Ctrl Pts',(-35.1744900671665,48.0897561847352,
3.65520057834429));
#245209=CARTESIAN_POINT('Ctrl Pts',(-35.224317350473,48.1580153629285,3.55127910964166));
#245210=CARTESIAN_POINT('Ctrl Pts',(-35.209151665053,47.9220530736687,3.47153072139105));
#245211=CARTESIAN_POINT('Ctrl Pts',(-35.1070032653418,47.996868104246,3.47122746281616));
#245212=CARTESIAN_POINT('Ctrl Pts',(-35.1702703594593,48.0836260618765,
3.40413045901328));
#245213=CARTESIAN_POINT('Origin',(-35.2729208539817,48.0088472823272,3.40423097483344));
#245214=CARTESIAN_POINT('Ctrl Pts',(-36.6347241449657,50.9644637245893,
2.90134173516059));
#245215=CARTESIAN_POINT('Ctrl Pts',(-36.7381840359687,50.8898702560318,
2.90163218716426));
#245216=CARTESIAN_POINT('Ctrl Pts',(-36.674605926818,50.8023624960591,2.83404198860297));
#245217=CARTESIAN_POINT('Ctrl Pts',(-36.6614665482801,51.0012706547893,
2.82853349835384));
#245218=CARTESIAN_POINT('Ctrl Pts',(-36.7432905102105,50.9229972443181,
2.85381483162359));
#245219=CARTESIAN_POINT('Ctrl Pts',(-36.7013469409081,50.8391683443878,
2.79182701594228));
#245220=CARTESIAN_POINT('Ctrl Pts',(-36.7102884597168,51.0230245369438,
2.75468822073687));
#245221=CARTESIAN_POINT('Ctrl Pts',(-36.768904996455,50.9514409225354,2.79286913083867));
#245222=CARTESIAN_POINT('Ctrl Pts',(-36.7410683485314,50.8675358949426,
2.74900763297943));
#245223=CARTESIAN_POINT('Ctrl Pts',(-36.8383381382864,51.0194219249362,
2.63954450640419));
#245224=CARTESIAN_POINT('Ctrl Pts',(-36.855176216862,50.9635175930193,2.69627684028899));
#245225=CARTESIAN_POINT('Ctrl Pts',(-36.8330984946708,50.8901021525742,
2.68224356036531));
#245226=CARTESIAN_POINT('Ctrl Pts',(-36.9196318328648,50.9918932610489,
2.59908178706395));
#245227=CARTESIAN_POINT('Ctrl Pts',(-36.9171104726355,50.9476171190701,
2.6587870432158));
#245228=CARTESIAN_POINT('Ctrl Pts',(-36.8864699989252,50.8828596657528,
2.65878198860296));
#245229=CARTESIAN_POINT('Ctrl Pts',(-36.991167339171,50.9399462128202,2.59908173516058));
#245230=CARTESIAN_POINT('Ctrl Pts',(-36.9692474126343,50.9097606317994,
2.65878198860296));
#245231=CARTESIAN_POINT('Ctrl Pts',(-36.9278827595329,50.8527980281385,
2.65878198860296));
#245232=CARTESIAN_POINT('Origin',(-36.5718607685324,50.8770112231003,2.83404198860297));
#245233=CARTESIAN_POINT('Origin',(-35.1682072895741,47.8647214254955,3.11913648167096));
#245234=CARTESIAN_POINT('Origin',(-35.0634937251224,47.7205955685091,2.83404198860295));
#245235=CARTESIAN_POINT('Origin',(-36.4671473482213,50.7328855645148,3.1191364817745));
#245236=CARTESIAN_POINT('Origin',(-36.3624339277676,50.5887599058101,3.40423097483344));
#245237=CARTESIAN_POINT('Ctrl Pts',(-34.9997217530263,47.63380340476,2.90134173516056));
#245238=CARTESIAN_POINT('Ctrl Pts',(-34.8977303031704,47.7085070967804,
2.90103711553262));
#245239=CARTESIAN_POINT('Ctrl Pts',(-34.9607485668368,47.7952442955502,
2.83404198860294));
#245240=CARTESIAN_POINT('Ctrl Pts',(-34.9730146904938,47.5970451916073,
2.82862991747985));
#245241=CARTESIAN_POINT('Ctrl Pts',(-34.8923835282622,47.6752966590749,
2.85314045886441));
#245242=CARTESIAN_POINT('Ctrl Pts',(-34.9340408279393,47.758484246595,2.79187960999962));
#245243=CARTESIAN_POINT('Ctrl Pts',(-34.9244461536127,47.5754322771536,
2.75470625793369));
#245244=CARTESIAN_POINT('Ctrl Pts',(-34.8665972787025,47.6469756149924,
2.79224250381933));
#245245=CARTESIAN_POINT('Ctrl Pts',(-34.8944891948624,47.7303228514093,
2.74901809108295));
#245246=CARTESIAN_POINT('Ctrl Pts',(-34.7970725085258,47.5794993790986,
2.63947868311719));
#245247=CARTESIAN_POINT('Ctrl Pts',(-34.7804938560724,47.6353197637776,
2.69595066767939));
#245248=CARTESIAN_POINT('Ctrl Pts',(-34.8028668197836,47.7084160893876,
2.6822053943609));
#245249=CARTESIAN_POINT('Ctrl Pts',(-34.7162617467346,47.607308993689,2.59908178585189));
#245250=CARTESIAN_POINT('Ctrl Pts',(-34.7189078610144,47.6515013114278,
2.65877670944888));
#245251=CARTESIAN_POINT('Ctrl Pts',(-34.7497660430534,47.7160937685341,
2.65878198860294));
#245252=CARTESIAN_POINT('Ctrl Pts',(-34.6451144164188,47.6590285860936,
2.59908173516056));
#245253=CARTESIAN_POINT('Ctrl Pts',(-34.667049453402,47.6892031885514,2.65878198860294));
#245254=CARTESIAN_POINT('Ctrl Pts',(-34.7084426211234,47.7461450747865,
2.65878198860294));
#245255=CARTESIAN_POINT('Origin',(-34.7084426211234,47.7461450747865,2.53178198860294));
#245256=CARTESIAN_POINT('Ctrl Pts',(-36.1092077731531,50.2402240048083,
3.77003198860298));
#245257=CARTESIAN_POINT('Ctrl Pts',(-36.2121064368056,50.1654637495898,
3.77003198860298));
#245258=CARTESIAN_POINT('Ctrl Pts',(-36.2119528169383,50.1655753609565,
3.64284238727626));
#245259=CARTESIAN_POINT('Ctrl Pts',(-36.2365633238548,50.4158927445036,
3.77003198860298));
#245260=CARTESIAN_POINT('Ctrl Pts',(-36.3397519704521,50.3411519064821,
3.77025506106023));
#245261=CARTESIAN_POINT('Ctrl Pts',(-36.313943782211,50.3059538820312,3.64284210641963));
#245262=CARTESIAN_POINT('Ctrl Pts',(-36.3578055460589,50.5831252836592,
3.65553527987867));
#245263=CARTESIAN_POINT('Ctrl Pts',(-36.4612367259606,50.5083605190664,
3.65585996532998));
#245264=CARTESIAN_POINT('Ctrl Pts',(-36.4110374247136,50.4395918165619,
3.55127902710161));
#245265=CARTESIAN_POINT('Ctrl Pts',(-36.4252947698681,50.6762142289948,
3.47153072139106));
#245266=CARTESIAN_POINT('Ctrl Pts',(-36.5289136700282,50.6015093986316,
3.47182327905222));
#245267=CARTESIAN_POINT('Ctrl Pts',(-36.4650842569434,50.5139808995223,
3.40413028378018));
#245268=CARTESIAN_POINT('Origin',(-36.1092077731531,50.2402240048083,3.64303198860298));
#245269=CARTESIAN_POINT('Origin',(3.77491158612227E-16,1.9162488945517E-13,
2.53178198860262));
#245270=CARTESIAN_POINT('Origin',(-34.6837837831348,47.7640607692763,2.53178198860295));
#245271=CARTESIAN_POINT('Origin',(21.7541926348216,-29.4019141737115,3.64303198860242));
#245272=CARTESIAN_POINT('Origin',(-35.8732562382987,49.9155525184325,3.64299466007571));
#245273=CARTESIAN_POINT('Ctrl Pts',(-34.6205005703637,47.6769115920304,
2.59908173516056));
#245274=CARTESIAN_POINT('Ctrl Pts',(-34.6424200234577,47.7070975168464,
2.65878198860294));
#245275=CARTESIAN_POINT('Ctrl Pts',(-34.6837837831348,47.7640607692763,
2.65878198860294));
#245276=CARTESIAN_POINT('Ctrl Pts',(-34.5495693076635,47.7284183483607,
2.59908193199947));
#245277=CARTESIAN_POINT('Ctrl Pts',(-34.5907418558606,47.7446195594533,
2.6587768580676));
#245278=CARTESIAN_POINT('Ctrl Pts',(-34.6425747206424,47.7939730310167,
2.65878198860294));
#245279=CARTESIAN_POINT('Ctrl Pts',(-34.4983910654767,47.7959261043557,
2.63872492669839));
#245280=CARTESIAN_POINT('Ctrl Pts',(-34.5563698228278,47.7976714756521,
2.69532212015316));
#245281=CARTESIAN_POINT('Ctrl Pts',(-34.6188891978598,47.8415056181568,
2.68176836726693));
#245282=CARTESIAN_POINT('Ctrl Pts',(-34.4545839152296,47.9165880269727,
2.75442176402273));
#245283=CARTESIAN_POINT('Ctrl Pts',(-34.5404685123898,47.883759104649,2.79203179920163));
#245284=CARTESIAN_POINT('Ctrl Pts',(-34.6111463389771,47.9359643384886,
2.74885310748182));
#245285=CARTESIAN_POINT('Ctrl Pts',(-34.4602354682505,47.9696250311914,
2.82866089558438));
#245286=CARTESIAN_POINT('Ctrl Pts',(-34.5595777906764,47.917113676462,2.85316563119214));
#245287=CARTESIAN_POINT('Ctrl Pts',(-34.6258166968302,47.9824460410478,
2.79189751796674));
#245288=CARTESIAN_POINT('Ctrl Pts',(-34.4869303039399,48.0063682005187,
2.90134173516055));
#245289=CARTESIAN_POINT('Ctrl Pts',(-34.5894948283136,47.9324532779038,
2.90103711553262));
#245290=CARTESIAN_POINT('Ctrl Pts',(-34.6525130919799,48.0191904766737,
2.83404198860294));
#245291=CARTESIAN_POINT('Origin',(-34.5497679336943,48.0938392037148,2.83404198860294));
#245292=CARTESIAN_POINT('Origin',(-35.8473027479613,49.8797426632452,3.56647653971789));
#245293=CARTESIAN_POINT('Origin',(-35.7991993820664,49.8135340601223,3.42473028058518));
#245294=CARTESIAN_POINT('Origin',(-34.6544814981826,48.2379650606549,3.11913648168096));
#245295=CARTESIAN_POINT('Origin',(-34.7591950625536,48.3820909175329,3.40423097483344));
#245296=CARTESIAN_POINT('Ctrl Pts',(-35.6052536882604,49.5465907136145,
3.36123028058515));
#245297=CARTESIAN_POINT('Ctrl Pts',(-35.707998846546,49.4719419865733,3.36123028058515));
#245298=CARTESIAN_POINT('Ctrl Pts',(-35.707998846546,49.4719419865733,3.23423028058515));
#245299=CARTESIAN_POINT('Ctrl Pts',(-35.6583499840569,49.6192730640963,
3.36123028058515));
#245300=CARTESIAN_POINT('Ctrl Pts',(-35.7608559931183,49.5446936074887,
3.36099641108576));
#245301=CARTESIAN_POINT('Ctrl Pts',(-35.7873581223564,49.5811706590203,
3.23423043688435));
#245302=CARTESIAN_POINT('Ctrl Pts',(-35.7085550527713,49.6880007749199,
3.4105425890532));
#245303=CARTESIAN_POINT('Ctrl Pts',(-35.8110857017895,49.6138288703731,
3.41008815825907));
#245304=CARTESIAN_POINT('Ctrl Pts',(-35.8623979633523,49.6844541394821,
3.30819867304266));
#245305=CARTESIAN_POINT('Ctrl Pts',(-35.7350130971391,49.7242207306175,
3.48823028058517));
#245306=CARTESIAN_POINT('Ctrl Pts',(-35.8375861910559,49.6503036646785,
3.48794691941633));
#245307=CARTESIAN_POINT('Ctrl Pts',(-35.9019445403521,49.7388853330811,
3.42473028058518));
#245308=CARTESIAN_POINT('Origin',(-35.6052536882604,49.5465907136145,3.23423028058515));
#245309=CARTESIAN_POINT('Ctrl Pts',(-34.6963546279287,48.2946219293746,
3.47153072139105));
#245310=CARTESIAN_POINT('Ctrl Pts',(-34.7990735298985,48.2205921526139,
3.4712274628511));
#245311=CARTESIAN_POINT('Ctrl Pts',(-34.8620346481358,48.3075723994625,
3.40413046676847));
#245312=CARTESIAN_POINT('Ctrl Pts',(-34.7638392294003,48.387716530751,3.65553813458021));
#245313=CARTESIAN_POINT('Ctrl Pts',(-34.8665617960676,48.3134813154541,
3.65520336072058));
#245314=CARTESIAN_POINT('Ctrl Pts',(-34.91608245714,48.3819628268521,3.55128134519854));
#245315=CARTESIAN_POINT('Ctrl Pts',(-34.8850734745832,48.5549570506165,
3.77003198860297));
#245316=CARTESIAN_POINT('Ctrl Pts',(-34.9878985031393,48.4804861171435,
3.76980209314202));
#245317=CARTESIAN_POINT('Ctrl Pts',(-35.0131769156724,48.5156018845747,
3.64284195387532));
#245318=CARTESIAN_POINT('Ctrl Pts',(-35.0124214764587,48.7306271754176,
3.77003198860296));
#245319=CARTESIAN_POINT('Ctrl Pts',(-35.1153205397465,48.6558666298471,
3.77003198860297));
#245320=CARTESIAN_POINT('Ctrl Pts',(-35.1151665196474,48.6559785319993,
3.64284189403885));
#245321=CARTESIAN_POINT('Origin',(-35.0124214764587,48.7306271754176,3.64303198860296));
#245322=CARTESIAN_POINT('Origin',(21.2334658618526,-28.6851952578917,3.23423028058461));
#245323=CARTESIAN_POINT('Origin',(-35.5163757878398,49.4242607783461,3.23423028058515));
#245324=CARTESIAN_POINT('Origin',(21.1519223437074,-28.572960233785,3.64303198860243));
#245325=CARTESIAN_POINT('Origin',(-35.2482948100393,49.0553654007527,3.6429917172178));
#245326=CARTESIAN_POINT('Ctrl Pts',(-35.3866101428262,49.2466351556013,
3.48823028058515));
#245327=CARTESIAN_POINT('Ctrl Pts',(-35.4901170100369,49.1720533660031,
3.48852004212293));
#245328=CARTESIAN_POINT('Ctrl Pts',(-35.425175210744,49.0826686475735,3.42473028058515));
#245329=CARTESIAN_POINT('Ctrl Pts',(-35.4131599099208,49.2829758776408,
3.41028005848442));
#245330=CARTESIAN_POINT('Ctrl Pts',(-35.5164304941051,49.2082707697419,
3.41074404220321));
#245331=CARTESIAN_POINT('Ctrl Pts',(-35.4648554356506,49.1372837917352,
3.30780486243953));
#245332=CARTESIAN_POINT('Ctrl Pts',(-35.4634578610114,49.3518235761952,
3.36123028058516));
#245333=CARTESIAN_POINT('Ctrl Pts',(-35.5663414789262,49.276967346882,3.36146460586564));
#245334=CARTESIAN_POINT('Ctrl Pts',(-35.5400289748685,49.2407512920126,
3.23423045308515));
#245335=CARTESIAN_POINT('Ctrl Pts',(-35.5163757878398,49.4242607783461,
3.36123028058515));
#245336=CARTESIAN_POINT('Ctrl Pts',(-35.6191209461254,49.3496120513049,
3.36123028058514));
#245337=CARTESIAN_POINT('Ctrl Pts',(-35.6191209461254,49.3496120513049,
3.23423028058515));
#245338=CARTESIAN_POINT('Origin',(-35.3224300524584,49.1573173746146,3.42473028058514));
#245339=CARTESIAN_POINT('Origin',(-35.2746135650455,49.0915036263509,3.56563113524782));
#245340=CARTESIAN_POINT('Origin',(-41.3366772861972,45.4345348113618,3.56647653909426));
#245341=CARTESIAN_POINT('Origin',(-41.3663085755642,45.467366442211,3.64299466007489));
#245342=CARTESIAN_POINT('Origin',(-41.2819167515331,45.3737170758072,3.42473028058515));
#245343=CARTESIAN_POINT('Ctrl Pts',(-41.2079002115909,45.2923641298557,
3.48823028058514));
#245344=CARTESIAN_POINT('Ctrl Pts',(-41.1142722655008,45.3773275334105,
3.4879469194163));
#245345=CARTESIAN_POINT('Ctrl Pts',(-41.1875373586974,45.4586966628148,
3.42473028058515));
#245346=CARTESIAN_POINT('Ctrl Pts',(-41.1778715515056,45.2588408013002,
3.41028005925117));
#245347=CARTESIAN_POINT('Ctrl Pts',(-41.0840023845225,45.3437094247737,
3.40982512230944));
#245348=CARTESIAN_POINT('Ctrl Pts',(-41.1423656859486,45.4085284377442,
3.30780486372889));
#245349=CARTESIAN_POINT('Ctrl Pts',(-41.1209827764377,45.195330604445,3.36123028058512));
#245350=CARTESIAN_POINT('Ctrl Pts',(-41.0267203359219,45.2800912647195,
3.36099721048581));
#245351=CARTESIAN_POINT('Ctrl Pts',(-41.0567886774847,45.3134855411626,
3.23423045308423));
#245352=CARTESIAN_POINT('Ctrl Pts',(-41.0611303347406,45.1285089182133,
3.36123028058512));
#245353=CARTESIAN_POINT('Ctrl Pts',(-40.966750941905,45.2134885052208,3.36123028058512));
#245354=CARTESIAN_POINT('Ctrl Pts',(-40.966750941905,45.2134885052208,3.23423028058512));
#245355=CARTESIAN_POINT('Origin',(-41.0611303347406,45.1285089182133,3.23423028058512));
#245356=CARTESIAN_POINT('Origin',(-0.235948482089066,-0.212448967518755,
3.64303198860262));
#245357=CARTESIAN_POINT('Origin',(-41.6348281284264,45.7656648676106,3.64303198860294));
#245358=CARTESIAN_POINT('Origin',(-0.235948482089066,-0.212448967518752,
3.23423028058481));
#245359=CARTESIAN_POINT('Origin',(-40.9599523566127,45.0161393894793,3.23423028058512));
#245360=CARTESIAN_POINT('Ctrl Pts',(-41.9955727382253,46.1654920697612,
3.47153072139103));
#245361=CARTESIAN_POINT('Ctrl Pts',(-41.9009568150781,46.2513146333408,
3.47182327902694));
#245362=CARTESIAN_POINT('Ctrl Pts',(-41.8286119029177,46.1706818621617,
3.4041302895905));
#245363=CARTESIAN_POINT('Ctrl Pts',(-41.9185486398936,46.0801220723613,
3.65553807120985));
#245364=CARTESIAN_POINT('Ctrl Pts',(-41.8239131221222,46.1657485549054,
3.65586275497224));
#245365=CARTESIAN_POINT('Ctrl Pts',(-41.7670844335152,46.1023486848312,
3.55128126837279));
#245366=CARTESIAN_POINT('Ctrl Pts',(-41.7801771152745,45.92675847217,3.77003198860295));
#245367=CARTESIAN_POINT('Ctrl Pts',(-41.6856154234933,46.0121526898589,
3.77025505748236));
#245368=CARTESIAN_POINT('Ctrl Pts',(-41.6565528363061,45.9795909100358,
3.64284211731202));
#245369=CARTESIAN_POINT('Ctrl Pts',(-41.6348281284264,45.7656648676106,
3.77003198860294));
#245370=CARTESIAN_POINT('Ctrl Pts',(-41.5403077371542,45.8507714101807,
3.77003198860294));
#245371=CARTESIAN_POINT('Ctrl Pts',(-41.5404488407561,45.8506443599269,
3.64284239821714));
#245372=CARTESIAN_POINT('Origin',(-41.9230990057958,46.0858221116778,3.40423097483341));
#245373=CARTESIAN_POINT('Ctrl Pts',(-40.9599523566127,45.0161393894793,
3.36123028058512));
#245374=CARTESIAN_POINT('Ctrl Pts',(-40.8655729637771,45.1011189764869,
3.36123028058512));
#245375=CARTESIAN_POINT('Ctrl Pts',(-40.8655729637771,45.1011189764869,
3.23423028058512));
#245376=CARTESIAN_POINT('Ctrl Pts',(-40.8998980546751,44.9490914663013,
3.36123028058512));
#245377=CARTESIAN_POINT('Ctrl Pts',(-40.8052862548003,45.034163803023,3.36146538610349));
#245378=CARTESIAN_POINT('Ctrl Pts',(-40.7752309130104,45.0007839642901,
3.23423043688437));
#245379=CARTESIAN_POINT('Ctrl Pts',(-40.8431135311196,44.8856913339442,
3.4105425869313));
#245380=CARTESIAN_POINT('Ctrl Pts',(-40.7485699563858,44.9711739722047,
3.41100608859769));
#245381=CARTESIAN_POINT('Ctrl Pts',(-40.6898060629513,44.9059100567371,
3.30819866970974));
#245382=CARTESIAN_POINT('Ctrl Pts',(-40.8131880745608,44.8522789915941,
3.48823028058512));
#245383=CARTESIAN_POINT('Ctrl Pts',(-40.7187157882339,44.9380175594362,
3.48852004212289));
#245384=CARTESIAN_POINT('Ctrl Pts',(-40.6447864996555,44.8559107663285,
3.42473028058512));
#245385=CARTESIAN_POINT('Origin',(-40.7391658924911,44.770931179321,3.42473028058512));
#245386=CARTESIAN_POINT('Origin',(-42.0423040287732,46.2182127020604,3.1191364817828));
#245387=CARTESIAN_POINT('Origin',(-42.1615090516454,46.3506032922594,2.83404198860293));
#245388=CARTESIAN_POINT('Origin',(-40.684731938309,44.710476148586,3.56563113460894));
#245389=CARTESIAN_POINT('Origin',(-40.6548553974685,44.677218962551,3.64299171721771));
#245390=CARTESIAN_POINT('Ctrl Pts',(-42.1358900227697,46.7738319284257,
2.59908173516055));
#245391=CARTESIAN_POINT('Ctrl Pts',(-42.1109214781063,46.7461150696872,
2.65878198860294));
#245392=CARTESIAN_POINT('Ctrl Pts',(-42.0638038389703,46.6938111422604,
2.65878198860294));
#245393=CARTESIAN_POINT('Ctrl Pts',(-42.2013581359411,46.7148552537641,
2.59908193475657));
#245394=CARTESIAN_POINT('Ctrl Pts',(-42.1586072771691,46.7031532960226,
2.65878715325504));
#245395=CARTESIAN_POINT('Ctrl Pts',(-42.1016932886506,46.6596664560533,
2.65878198860294));
#245396=CARTESIAN_POINT('Ctrl Pts',(-42.2450249725428,46.6418481388114,
2.6387877884991));
#245397=CARTESIAN_POINT('Ctrl Pts',(-42.1870455286633,46.6464039985658,
2.6956446018015));
#245398=CARTESIAN_POINT('Ctrl Pts',(-42.1199142759249,46.6095714048491,
2.6818048162493));
#245399=CARTESIAN_POINT('Ctrl Pts',(-42.2756632139848,46.5164783566528,
2.75443238878669));
#245400=CARTESIAN_POINT('Ctrl Pts',(-42.1934768724829,46.5588531737054,
2.7926834077712));
#245401=CARTESIAN_POINT('Ctrl Pts',(-42.1171707421505,46.5142596423501,
2.74885926835627));
#245402=CARTESIAN_POINT('Ctrl Pts',(-42.2644092166194,46.4640705998043,
2.82856655361705));
#245403=CARTESIAN_POINT('Ctrl Pts',(-42.1708301402953,46.5278411618568,
2.85384197230856));
#245404=CARTESIAN_POINT('Ctrl Pts',(-42.0975575768117,46.4693765058001,
2.79184624278606));
#245405=CARTESIAN_POINT('Ctrl Pts',(-42.2339804752703,46.4302753505425,
2.90134173516055));
#245406=CARTESIAN_POINT('Ctrl Pts',(-42.1395065321001,46.5159655405275,
2.90163218716423));
#245407=CARTESIAN_POINT('Ctrl Pts',(-42.0671296588098,46.435582879267,2.83404198860294));
#245408=CARTESIAN_POINT('Origin',(-42.0638038389703,46.6938111422604,2.53178198860293));
#245409=CARTESIAN_POINT('Origin',(-0.235948482089066,-0.212448967518755,
3.64303198860262));
#245410=CARTESIAN_POINT('Origin',(-40.386254305094,44.3789831537295,3.64303198860293));
#245411=CARTESIAN_POINT('Origin',(8.01250065760356E-17,1.91454897897931E-13,
2.53178198860262));
#245412=CARTESIAN_POINT('Origin',(-42.0411527846897,46.7142062431422,2.53178198860294));
#245413=CARTESIAN_POINT('Ctrl Pts',(-40.386254305094,44.3789831537295,3.77003198860293));
#245414=CARTESIAN_POINT('Ctrl Pts',(-40.2917335276657,44.4640900439962,
3.77003198860293));
#245415=CARTESIAN_POINT('Ctrl Pts',(-40.2918750180001,44.4639626455268,
3.64284187937025));
#245416=CARTESIAN_POINT('Ctrl Pts',(-40.2408978759463,44.2178916378598,
3.77003198860293));
#245417=CARTESIAN_POINT('Ctrl Pts',(-40.1466757825282,44.3029863283998,
3.76980208962917));
#245418=CARTESIAN_POINT('Ctrl Pts',(-40.1757689690817,44.3350138149348,
3.64284193928323));
#245419=CARTESIAN_POINT('Ctrl Pts',(-40.1025190720996,44.0645366033534,
3.65553535416617));
#245420=CARTESIAN_POINT('Ctrl Pts',(-40.0085488431153,44.1495800756908,
3.65520057834612));
#245421=CARTESIAN_POINT('Ctrl Pts',(-40.0652381943495,44.2122569536132,
3.55127910964266));
#245422=CARTESIAN_POINT('Ctrl Pts',(-40.025490812659,43.9791725362583,3.47153072139102));
#245423=CARTESIAN_POINT('Ctrl Pts',(-39.9317222927443,44.0642551375177,
3.47122746281612));
#245424=CARTESIAN_POINT('Ctrl Pts',(-40.003711479089,44.1439246138551,3.40413045901276));
#245425=CARTESIAN_POINT('Origin',(-40.0979831325501,44.0588255818378,3.4042309748334));
#245426=CARTESIAN_POINT('Ctrl Pts',(-41.7612723673365,46.8559036426985,
2.90134173516056));
#245427=CARTESIAN_POINT('Ctrl Pts',(-41.8563683535932,46.7709043015502,
2.90163218716423));
#245428=CARTESIAN_POINT('Ctrl Pts',(-41.7839914803029,46.6905216402897,
2.83404198860294));
#245429=CARTESIAN_POINT('Ctrl Pts',(-41.7917156448183,46.8897135983615,
2.82853349835382));
#245430=CARTESIAN_POINT('Ctrl Pts',(-41.8649095672149,46.8033160448246,
2.85381483162464));
#245431=CARTESIAN_POINT('Ctrl Pts',(-41.8144332630853,46.7243306652216,
2.79182701594319));
#245432=CARTESIAN_POINT('Ctrl Pts',(-41.8425440045881,46.9062450310967,
2.75468822073682));
#245433=CARTESIAN_POINT('Ctrl Pts',(-41.893356908596,46.8289264627106,2.79286913083891));
#245434=CARTESIAN_POINT('Ctrl Pts',(-41.8569022891475,46.7483907976684,
2.74900763297939));
#245435=CARTESIAN_POINT('Ctrl Pts',(-41.9695156381235,46.8892773184519,
2.63954450640417));
#245436=CARTESIAN_POINT('Ctrl Pts',(-41.9804178820373,46.8319191778368,
2.69627684028874));
#245437=CARTESIAN_POINT('Ctrl Pts',(-41.9507871007486,46.7612136652289,
2.68224356036528));
#245438=CARTESIAN_POINT('Ctrl Pts',(-42.0474864684049,46.8534019544978,
2.59908178706453));
#245439=CARTESIAN_POINT('Ctrl Pts',(-42.0403508033696,46.8096319157664,
2.65878704321511));
#245440=CARTESIAN_POINT('Ctrl Pts',(-42.0031091843005,46.7484320121859,
2.65878198860294));
#245441=CARTESIAN_POINT('Ctrl Pts',(-42.1132001506003,46.7942619810917,
2.59908173516055));
#245442=CARTESIAN_POINT('Ctrl Pts',(-42.0882450513177,46.7665330160779,
2.65878198860293));
#245443=CARTESIAN_POINT('Ctrl Pts',(-42.0411527846897,46.7142062431422,
2.65878198860294));
#245444=CARTESIAN_POINT('Origin',(-41.6896120874673,46.7755012272973,2.83404198860294));
#245445=CARTESIAN_POINT('Origin',(-39.978777945671,43.9264348095002,3.11913648167199));
#245446=CARTESIAN_POINT('Origin',(-39.8595727587357,43.7940440370144,2.83404198860291));
#245447=CARTESIAN_POINT('Origin',(-41.5704070646268,46.6431106370601,3.11913648177836));
#245448=CARTESIAN_POINT('Origin',(-41.4512020416176,46.5107200467157,3.40423097483342));
#245449=CARTESIAN_POINT('Ctrl Pts',(-39.7870778846749,43.7143933160623,
2.90134173516053));
#245450=CARTESIAN_POINT('Ctrl Pts',(-39.6934538167802,43.7993487829613,
2.90103711553259));
#245451=CARTESIAN_POINT('Ctrl Pts',(-39.7651933659001,43.879023624022,2.83404198860291));
#245452=CARTESIAN_POINT('Ctrl Pts',(-39.7566748466934,43.6806281164511,
2.82862991747978));
#245453=CARTESIAN_POINT('Ctrl Pts',(-39.6846648960477,43.76687916567,2.85314045886605));
#245454=CARTESIAN_POINT('Ctrl Pts',(-39.7347894633637,43.8452566693654,
2.79187960999937));
#245455=CARTESIAN_POINT('Ctrl Pts',(-39.7061132086031,43.6642103943288,
2.75470625793373));
#245456=CARTESIAN_POINT('Ctrl Pts',(-39.6560595510442,43.7414086642734,
2.79224250381934));
#245457=CARTESIAN_POINT('Ctrl Pts',(-39.6925108309095,43.8213838166748,
2.74901809108295));
#245458=CARTESIAN_POINT('Ctrl Pts',(-39.5798624575879,43.6815693876452,
2.63947868311711));
#245459=CARTESIAN_POINT('Ctrl Pts',(-39.5692094437565,43.7388169234803,
2.69595066767937));
#245460=CARTESIAN_POINT('Ctrl Pts',(-39.5991004926179,43.8091742082548,
2.68220539436085));
#245461=CARTESIAN_POINT('Ctrl Pts',(-39.5024012818819,43.7176736830028,
2.5990817858515));
#245462=CARTESIAN_POINT('Ctrl Pts',(-39.5096522555301,43.761347316339,2.6587767094482));
#245463=CARTESIAN_POINT('Ctrl Pts',(-39.5470931435014,43.8223603708617,
2.65878198860291));
#245464=CARTESIAN_POINT('Ctrl Pts',(-39.437049873601,43.7765468711722,2.59908173516053));
#245465=CARTESIAN_POINT('Ctrl Pts',(-39.4620188529811,43.8042633382929,
2.65878198860292));
#245466=CARTESIAN_POINT('Ctrl Pts',(-39.5091373124624,43.8565665267056,
2.65878198860292));
#245467=CARTESIAN_POINT('Origin',(-39.5091373124624,43.8565665267056,2.53178198860292));
#245468=CARTESIAN_POINT('Ctrl Pts',(-41.1629311642483,46.1905628026485,
3.77003198860295));
#245469=CARTESIAN_POINT('Ctrl Pts',(-41.2574515636632,46.1054562527467,
3.77003198860295));
#245470=CARTESIAN_POINT('Ctrl Pts',(-41.2573104519064,46.1055833103431,
3.6428423872765));
#245471=CARTESIAN_POINT('Ctrl Pts',(-41.307951431326,46.3519569306005,3.77003198860295));
#245472=CARTESIAN_POINT('Ctrl Pts',(-41.4027622547777,46.2668393800569,
3.77025506105729));
#245473=CARTESIAN_POINT('Ctrl Pts',(-41.3734162510841,46.2345318643247,
3.64284210641953));
#245474=CARTESIAN_POINT('Ctrl Pts',(-41.4460100362743,46.5056000892413,
3.65553527987864));
#245475=CARTESIAN_POINT('Ctrl Pts',(-41.5410595633947,46.4204333915661,
3.65585996533167));
#245476=CARTESIAN_POINT('Ctrl Pts',(-41.4839469723838,46.3572886670224,
3.55127902710186));
#245477=CARTESIAN_POINT('Ctrl Pts',(-41.5228599914565,46.591124538743,3.47153072139103));
#245478=CARTESIAN_POINT('Ctrl Pts',(-41.6181024753229,46.5059978248579,
3.47182327905219));
#245479=CARTESIAN_POINT('Ctrl Pts',(-41.545473506938,46.425620806486,3.40413028378029));
#245480=CARTESIAN_POINT('Origin',(-41.1629311642483,46.1905628026485,3.64303198860295));
#245481=CARTESIAN_POINT('Origin',(3.72719664096539E-16,1.91621025575097E-13,
2.53178198860262));
#245482=CARTESIAN_POINT('Origin',(-39.4864862581819,43.8769616275874,2.53178198860292));
#245483=CARTESIAN_POINT('Origin',(28.0951675083328,-30.7283483363944,3.64303198860241));
#245484=CARTESIAN_POINT('Origin',(-40.8943347850524,45.8923335519903,3.64299466007517));
#245485=CARTESIAN_POINT('Ctrl Pts',(-39.4144401478992,43.7969047596346,
2.59908173516053));
#245486=CARTESIAN_POINT('Ctrl Pts',(-39.439394812269,43.8246341160485,2.65878198860292));
#245487=CARTESIAN_POINT('Ctrl Pts',(-39.4864862581819,43.8769616275874,
2.65878198860292));
#245488=CARTESIAN_POINT('Ctrl Pts',(-39.3492813761645,43.8555436924523,
2.59908193199924));
#245489=CARTESIAN_POINT('Ctrl Pts',(-39.3919218645329,43.8673524484227,
2.65877685806688));
#245490=CARTESIAN_POINT('Ctrl Pts',(-39.4486296259964,43.9110175468016,
2.65878198860292));
#245491=CARTESIAN_POINT('Ctrl Pts',(-39.3054399757367,43.9280312169046,
2.63872492669844));
#245492=CARTESIAN_POINT('Ctrl Pts',(-39.3632835603679,43.923706596467,2.69532212015284));
#245493=CARTESIAN_POINT('Ctrl Pts',(-39.4300423632768,43.9607655567558,
2.68176836726669));
#245494=CARTESIAN_POINT('Ctrl Pts',(-39.2744854109877,44.0526112349805,
2.75442176402264));
#245495=CARTESIAN_POINT('Ctrl Pts',(-39.3564679665374,44.0109847679682,
2.79203179920206));
#245496=CARTESIAN_POINT('Ctrl Pts',(-39.4322155454631,44.0555161714744,
2.748853107482));
#245497=CARTESIAN_POINT('Ctrl Pts',(-39.285649880758,44.1047669487877,2.82866089558441));
#245498=CARTESIAN_POINT('Ctrl Pts',(-39.3789590643335,44.042159156452,2.8531656311921));
#245499=CARTESIAN_POINT('Ctrl Pts',(-39.4516641984998,44.1002097724416,
2.79189751796671));
#245500=CARTESIAN_POINT('Ctrl Pts',(-39.3160391863692,44.1385184650376,
2.90134173516053));
#245501=CARTESIAN_POINT('Ctrl Pts',(-39.4103156382734,44.054287543984,2.90103711553259));
#245502=CARTESIAN_POINT('Ctrl Pts',(-39.4820551873932,44.1339623850447,
2.83404198860292));
#245503=CARTESIAN_POINT('Origin',(-39.3876757945576,44.2189419720523,2.83404198860292));
#245504=CARTESIAN_POINT('Origin',(-40.8647803215171,45.8594327453968,3.56647653971846));
#245505=CARTESIAN_POINT('Origin',(-40.8100197873549,45.7986150108451,3.42473028058516));
#245506=CARTESIAN_POINT('Origin',(-39.5068809815279,44.3513327444866,3.11913648168124));
#245507=CARTESIAN_POINT('Origin',(-39.626086168372,44.4837235168756,3.4042309748334));
#245508=CARTESIAN_POINT('Ctrl Pts',(-40.5892333705625,45.5534068532511,
3.36123028058513));
#245509=CARTESIAN_POINT('Ctrl Pts',(-40.6836127633981,45.4684272662436,
3.36123028058513));
#245510=CARTESIAN_POINT('Ctrl Pts',(-40.6836127633981,45.4684272662436,
3.23423028058513));
#245511=CARTESIAN_POINT('Ctrl Pts',(-40.649636173697,45.6201409680079,3.36123028058513));
#245512=CARTESIAN_POINT('Ctrl Pts',(-40.7437849681275,45.5352552698608,
3.36099641108633));
#245513=CARTESIAN_POINT('Ctrl Pts',(-40.7739548060672,45.5687622694471,
3.23423043688415));
#245514=CARTESIAN_POINT('Ctrl Pts',(-40.7067502157893,45.6832443225586,
3.41054258905314));
#245515=CARTESIAN_POINT('Ctrl Pts',(-40.8009661159856,45.5987613682859,
3.41008815825837));
#245516=CARTESIAN_POINT('Ctrl Pts',(-40.8593796344574,45.6636361529343,
3.3081986730425));
#245517=CARTESIAN_POINT('Ctrl Pts',(-40.7368493365299,45.7165002428307,
3.48823028058515));
#245518=CARTESIAN_POINT('Ctrl Pts',(-40.8311340869939,45.6322662944332,
3.48794691941631));
#245519=CARTESIAN_POINT('Ctrl Pts',(-40.9043991801906,45.7136354238376,
3.42473028058516));
#245520=CARTESIAN_POINT('Origin',(-40.5892333705625,45.5534068532511,3.23423028058513));
#245521=CARTESIAN_POINT('Ctrl Pts',(-39.5544469813073,44.4033023070489,
3.47153072139102));
#245522=CARTESIAN_POINT('Ctrl Pts',(-39.6488649595839,44.3189410241794,
3.47122746285107));
#245523=CARTESIAN_POINT('Ctrl Pts',(-39.7205730817654,44.3988635552005,
3.4041304667682));
#245524=CARTESIAN_POINT('Ctrl Pts',(-39.631292930691,44.4888328647726,3.65553813458016));
#245525=CARTESIAN_POINT('Ctrl Pts',(-39.7256930794102,44.4042668857101,
3.65520336072188));
#245526=CARTESIAN_POINT('Ctrl Pts',(-39.7821007282713,44.4671969296244,
3.55128134519921));
#245527=CARTESIAN_POINT('Ctrl Pts',(-39.769344436532,44.6424847942267,3.77003198860293));
#245528=CARTESIAN_POINT('Ctrl Pts',(-39.8638218465944,44.5576736781012,
3.76980209314289));
#245529=CARTESIAN_POINT('Ctrl Pts',(-39.8926323785409,44.5899547640682,
3.64284195387469));
#245530=CARTESIAN_POINT('Ctrl Pts',(-39.9143573409159,44.8038810887674,
3.77003198860294));
#245531=CARTESIAN_POINT('Ctrl Pts',(-40.0088781074273,44.7187742083304,
3.77003198860294));
#245532=CARTESIAN_POINT('Ctrl Pts',(-40.0087366280261,44.7189015969554,
3.64284189403838));
#245533=CARTESIAN_POINT('Origin',(-39.9143573409159,44.8038810887674,3.64303198860294));
#245534=CARTESIAN_POINT('Origin',(27.4203375923837,-29.9788737863602,3.23423028058461));
#245535=CARTESIAN_POINT('Origin',(-40.4880553924346,45.4410373245172,3.23423028058512));
#245536=CARTESIAN_POINT('Origin',(27.3146622010794,-29.8615093742682,3.64303198860242));
#245537=CARTESIAN_POINT('Origin',(-40.1828829233545,45.102184887041,3.64299171721827));
#245538=CARTESIAN_POINT('Ctrl Pts',(-40.3404336838195,45.2779489569772,
3.48823028058512));
#245539=CARTESIAN_POINT('Ctrl Pts',(-40.435577609727,45.1929563204589,3.4885200421229));
#245540=CARTESIAN_POINT('Ctrl Pts',(-40.3616483211486,45.1108495273513,
3.42473028058512));
#245541=CARTESIAN_POINT('Ctrl Pts',(-40.3706366483438,45.3113153943819,
3.41028005848437));
#245542=CARTESIAN_POINT('Ctrl Pts',(-40.4655326953357,45.2262248134114,
3.41074404220252));
#245543=CARTESIAN_POINT('Ctrl Pts',(-40.4068200107207,45.161017771106,3.30780486243924));
#245544=CARTESIAN_POINT('Ctrl Pts',(-40.4278556061233,45.3745283705083,
3.36123028058512));
#245545=CARTESIAN_POINT('Ctrl Pts',(-40.5223510101983,45.2893279449781,
3.3614646058656));
#245546=CARTESIAN_POINT('Ctrl Pts',(-40.4923970402292,45.25606069106,3.23423045308495));
#245547=CARTESIAN_POINT('Ctrl Pts',(-40.4880553924346,45.4410373245172,
3.36123028058512));
#245548=CARTESIAN_POINT('Ctrl Pts',(-40.5824347852702,45.3560577375096,
3.36123028058512));
#245549=CARTESIAN_POINT('Ctrl Pts',(-40.5824347852702,45.3560577375096,
3.23423028058512));
#245550=CARTESIAN_POINT('Origin',(-40.267268928313,45.1958291143588,3.42473028058512));
#245551=CARTESIAN_POINT('Origin',(-40.2128349746541,45.1353740846429,3.56563113524829));
#245552=CARTESIAN_POINT('Origin',(-45.8594327460063,40.8647803224533,3.56647653909523));
#245553=CARTESIAN_POINT('Origin',(-45.8923335519879,40.8943347850518,3.64299466007835));
#245554=CARTESIAN_POINT('Origin',(-45.7986150108453,40.8100197873546,3.42473028058512));
#245555=CARTESIAN_POINT('Ctrl Pts',(-45.7165002428309,40.7368493365297,
3.48823028058511));
#245556=CARTESIAN_POINT('Ctrl Pts',(-45.6322662944335,40.8311340869937,
3.48794691941628));
#245557=CARTESIAN_POINT('Ctrl Pts',(-45.7136354238378,40.9043991801903,
3.42473028058512));
#245558=CARTESIAN_POINT('Ctrl Pts',(-45.6831319408669,40.7066485019717,
3.41028005925112));
#245559=CARTESIAN_POINT('Ctrl Pts',(-45.5986481857945,40.8008642060163,
3.40982512231164));
#245560=CARTESIAN_POINT('Ctrl Pts',(-45.6634671987684,40.8592275074426,
3.30780486372857));
#245561=CARTESIAN_POINT('Ctrl Pts',(-45.619916185183,40.649432716854,3.36123028058509));
#245562=CARTESIAN_POINT('Ctrl Pts',(-45.5350300257419,40.7435821574166,
3.36099721048318));
#245563=CARTESIAN_POINT('Ctrl Pts',(-45.5684243021846,40.7736504989767,
3.23423045308402));
#245564=CARTESIAN_POINT('Ctrl Pts',(-45.5534068532514,40.5892333705622,
3.36123028058509));
#245565=CARTESIAN_POINT('Ctrl Pts',(-45.4684272662438,40.6836127633978,
3.3612302805851));
#245566=CARTESIAN_POINT('Ctrl Pts',(-45.4684272662438,40.6836127633978,
3.23423028058509));
#245567=CARTESIAN_POINT('Origin',(-45.5534068532514,40.5892333705622,3.23423028058509));
#245568=CARTESIAN_POINT('Origin',(-0.212448967518931,-0.23594848208889,
3.64303198860262));
#245569=CARTESIAN_POINT('Origin',(-46.1905628026487,41.162931164248,3.64303198860291));
#245570=CARTESIAN_POINT('Origin',(-0.212448967518931,-0.235948482088887,
3.23423028058481));
#245571=CARTESIAN_POINT('Origin',(-45.4410373245174,40.4880553924343,3.23423028058509));
#245572=CARTESIAN_POINT('Ctrl Pts',(-46.5911245387432,41.5228599914562,
3.471530721391));
#245573=CARTESIAN_POINT('Ctrl Pts',(-46.5059978322078,41.6181024670996,
3.4718232790269));
#245574=CARTESIAN_POINT('Ctrl Pts',(-46.4256208133854,41.5454735131718,
3.40413028959072));
#245575=CARTESIAN_POINT('Ctrl Pts',(-46.5055987918433,41.4460088704684,
3.65553807120985));
#245576=CARTESIAN_POINT('Ctrl Pts',(-46.4204321019747,41.5410583874226,
3.65586275496986));
#245577=CARTESIAN_POINT('Ctrl Pts',(-46.357287635879,41.4839460439597,3.5512812683726));
#245578=CARTESIAN_POINT('Ctrl Pts',(-46.3519544194661,41.3079491749529,
3.77003198860292));
#245579=CARTESIAN_POINT('Ctrl Pts',(-46.266836872876,41.4027599825079,3.77025505748455));
#245580=CARTESIAN_POINT('Ctrl Pts',(-46.2345298607751,41.3734144471015,
3.64284211731201));
#245581=CARTESIAN_POINT('Ctrl Pts',(-46.1905628026487,41.162931164248,3.77003198860291));
#245582=CARTESIAN_POINT('Ctrl Pts',(-46.1054562600789,41.2574515555199,
3.77003198860291));
#245583=CARTESIAN_POINT('Ctrl Pts',(-46.1055833103324,41.2573104519183,
3.64284239821759));
#245584=CARTESIAN_POINT('Origin',(-46.5107200467159,41.4512020416173,3.40423097483338));
#245585=CARTESIAN_POINT('Ctrl Pts',(-45.4410373245174,40.4880553924343,
3.36123028058509));
#245586=CARTESIAN_POINT('Ctrl Pts',(-45.3560577375098,40.5824347852699,
3.36123028058509));
#245587=CARTESIAN_POINT('Ctrl Pts',(-45.3560577375098,40.5824347852699,
3.23423028058509));
#245588=CARTESIAN_POINT('Ctrl Pts',(-45.3743035899554,40.4276521486878,
3.36123028058509));
#245589=CARTESIAN_POINT('Ctrl Pts',(-45.2891025640467,40.5221480762966,
3.36146538610229));
#245590=CARTESIAN_POINT('Ctrl Pts',(-45.2557227253145,40.4920927345046,
3.23423043688486));
#245591=CARTESIAN_POINT('Ctrl Pts',(-45.3112030195546,40.3705349278746,
3.41054258693126));
#245592=CARTESIAN_POINT('Ctrl Pts',(-45.2261127332244,40.4654317778764,
3.41100608859753));
#245593=CARTESIAN_POINT('Ctrl Pts',(-45.160848817758,40.4066678844424,3.30819866970865));
#245594=CARTESIAN_POINT('Ctrl Pts',(-45.2779489569775,40.3404336838192,
3.48823028058509));
#245595=CARTESIAN_POINT('Ctrl Pts',(-45.1929563204591,40.4355776097268,
3.48852004212286));
#245596=CARTESIAN_POINT('Ctrl Pts',(-45.1108495273515,40.3616483211483,
3.42473028058508));
#245597=CARTESIAN_POINT('Origin',(-45.1958291143591,40.2672689283127,3.42473028058508));
#245598=CARTESIAN_POINT('Origin',(-46.6431106370687,41.5704070646328,3.11913648178481));
#245599=CARTESIAN_POINT('Origin',(-46.7755012272975,41.689612087467,2.83404198860289));
#245600=CARTESIAN_POINT('Origin',(-45.1353740836137,40.2128349741376,3.56563113460713));
#245601=CARTESIAN_POINT('Origin',(-45.1021848870412,40.1828829233542,3.64299171721822));
#245602=CARTESIAN_POINT('Ctrl Pts',(-46.7942619810919,42.1132001506,2.59908173516052));
#245603=CARTESIAN_POINT('Ctrl Pts',(-46.7665330160781,42.0882450513175,
2.6587819886029));
#245604=CARTESIAN_POINT('Ctrl Pts',(-46.7142062431425,42.0411527846894,
2.6587819886029));
#245605=CARTESIAN_POINT('Ctrl Pts',(-46.8532067119185,42.0477032750704,
2.59908193475599));
#245606=CARTESIAN_POINT('Ctrl Pts',(-46.8094668591651,42.0405341034491,
2.65878715325439));
#245607=CARTESIAN_POINT('Ctrl Pts',(-46.748319038876,42.0032346206976,2.6587819886029));
#245608=CARTESIAN_POINT('Ctrl Pts',(-46.8890030154866,41.9705316734064,
2.63878778849898));
#245609=CARTESIAN_POINT('Ctrl Pts',(-46.8318174060858,41.9811230778545,
2.69564460180142));
#245610=CARTESIAN_POINT('Ctrl Pts',(-46.7612038509552,41.951509383626,2.68180481624926));
#245611=CARTESIAN_POINT('Ctrl Pts',(-46.9063687067669,41.8426461117369,
2.75443238878675));
#245612=CARTESIAN_POINT('Ctrl Pts',(-46.829061965151,41.8933796070863,2.79268340777128));
#245613=CARTESIAN_POINT('Ctrl Pts',(-46.7485125544798,41.8570065263033,
2.74885926835625));
#245614=CARTESIAN_POINT('Ctrl Pts',(-46.8896982576903,41.7917018131138,
2.82856655361699));
#245615=CARTESIAN_POINT('Ctrl Pts',(-46.803297656188,41.8649047103983,2.85384197230712));
#245616=CARTESIAN_POINT('Ctrl Pts',(-46.7243152668219,41.8144193983035,
2.79184624278388));
#245617=CARTESIAN_POINT('Ctrl Pts',(-46.8559036426987,41.7612723673362,
2.90134173516052));
#245618=CARTESIAN_POINT('Ctrl Pts',(-46.7709043015504,41.856368353593,2.9016321871642));
#245619=CARTESIAN_POINT('Ctrl Pts',(-46.6905216402899,41.7839914803026,
2.8340419886029));
#245620=CARTESIAN_POINT('Origin',(-46.7142062431425,42.0411527846894,2.5317819886029));
#245621=CARTESIAN_POINT('Origin',(-0.212448967518931,-0.23594848208889,
3.64303198860262));
#245622=CARTESIAN_POINT('Origin',(-44.8038810887676,39.9143573409156,3.6430319886029));
#245623=CARTESIAN_POINT('Origin',(9.23291810287662E-17,1.91467102072384E-13,
2.53178198860262));
#245624=CARTESIAN_POINT('Origin',(-46.6938111422607,42.06380383897,2.53178198860291));
#245625=CARTESIAN_POINT('Ctrl Pts',(-44.8038810887676,39.9143573409156,
3.7700319886029));
#245626=CARTESIAN_POINT('Ctrl Pts',(-44.7187741985014,40.0088781183435,
3.77003198860291));
#245627=CARTESIAN_POINT('Ctrl Pts',(-44.7189015969704,40.0087366280095,
3.64284187937085));
#245628=CARTESIAN_POINT('Ctrl Pts',(-44.6424822887494,39.7693421853888,
3.7700319886029));
#245629=CARTESIAN_POINT('Ctrl Pts',(-44.5576711710503,39.8638196089388,
3.76980208962854));
#245630=CARTESIAN_POINT('Ctrl Pts',(-44.5899527660323,39.8926305794714,
3.64284193928371));
#245631=CARTESIAN_POINT('Ctrl Pts',(-44.4888315723752,39.6312917695248,
3.65553535416614));
#245632=CARTESIAN_POINT('Ctrl Pts',(-44.4042655856132,39.7256919284555,
3.65520057834546));
#245633=CARTESIAN_POINT('Ctrl Pts',(-44.4671959043838,39.7820998051106,
3.55127910964227));
#245634=CARTESIAN_POINT('Ctrl Pts',(-44.4033023070491,39.554446981307,3.47153072139098));
#245635=CARTESIAN_POINT('Ctrl Pts',(-44.3189410144585,39.6488649704636,
3.47122746281608));
#245636=CARTESIAN_POINT('Ctrl Pts',(-44.3988635644382,39.7205730900532,
3.40413045901305));
#245637=CARTESIAN_POINT('Origin',(-44.4837235168759,39.6260861683717,3.40423097483337));
#245638=CARTESIAN_POINT('Ctrl Pts',(-46.4302753505427,42.2339804752701,
2.90134173516052));
#245639=CARTESIAN_POINT('Ctrl Pts',(-46.5159655405277,42.1395065320999,
2.9016321871642));
#245640=CARTESIAN_POINT('Ctrl Pts',(-46.4355828792672,42.0671296588095,
2.8340419886029));
#245641=CARTESIAN_POINT('Ctrl Pts',(-46.4640859592741,42.2644230274459,
2.82853349835383));
#245642=CARTESIAN_POINT('Ctrl Pts',(-46.5278479142006,42.1708479205174,
2.85381483162313));
#245643=CARTESIAN_POINT('Ctrl Pts',(-46.4693919041987,42.0975714415916,
2.79182701594276));
#245644=CARTESIAN_POINT('Ctrl Pts',(-46.5163638812299,42.2755508889262,
2.75468822073671));
#245645=CARTESIAN_POINT('Ctrl Pts',(-46.5588164356976,42.1933444849783,
2.79286913083864));
#245646=CARTESIAN_POINT('Ctrl Pts',(-46.5141432491638,42.1170605480854,
2.7490076329795));
#245647=CARTESIAN_POINT('Ctrl Pts',(-46.6408663419435,42.2454039774545,
2.6395445064042));
#245648=CARTESIAN_POINT('Ctrl Pts',(-46.6457133039302,42.1872204559321,
2.69627684028881));
#245649=CARTESIAN_POINT('Ctrl Pts',(-46.6088541045839,42.1199995355541,
2.6822435603651));
#245650=CARTESIAN_POINT('Ctrl Pts',(-46.7146600431957,42.2015749714294,
2.59908178706335));
#245651=CARTESIAN_POINT('Ctrl Pts',(-46.7029882531945,42.1587905896511,
2.65878704321545));
#245652=CARTESIAN_POINT('Ctrl Pts',(-46.6595535157374,42.1018187547559,
2.6587819886029));
#245653=CARTESIAN_POINT('Ctrl Pts',(-46.773831928426,42.1358900227694,2.59908173516052));
#245654=CARTESIAN_POINT('Ctrl Pts',(-46.7461150696874,42.1109214781061,
2.6587819886029));
#245655=CARTESIAN_POINT('Ctrl Pts',(-46.6938111422607,42.06380383897,2.6587819886029));
#245656=CARTESIAN_POINT('Origin',(-46.3506032922596,42.1615090516451,2.83404198860289));
#245657=CARTESIAN_POINT('Origin',(-44.3513327444991,39.5068809815365,3.11913648167179));
#245658=CARTESIAN_POINT('Origin',(-44.2189419720525,39.3876757945573,2.83404198860289));
#245659=CARTESIAN_POINT('Origin',(-46.2182127020521,42.042304028765,3.11913648177552));
#245660=CARTESIAN_POINT('Origin',(-46.085822111678,41.9230990057955,3.40423097483339));
#245661=CARTESIAN_POINT('Ctrl Pts',(-44.1385184650378,39.3160391863689,
2.9013417351605));
#245662=CARTESIAN_POINT('Ctrl Pts',(-44.0542875439842,39.4103156382731,
2.90103711553256));
#245663=CARTESIAN_POINT('Ctrl Pts',(-44.1339623850449,39.482055187393,2.83404198860288));
#245664=CARTESIAN_POINT('Ctrl Pts',(-44.1047525536513,39.285636938894,2.82862991747977));
#245665=CARTESIAN_POINT('Ctrl Pts',(-44.042152770681,39.3789425853231,2.85314045886458));
#245666=CARTESIAN_POINT('Ctrl Pts',(-44.1001954303878,39.4516512848561,
2.79187961000011));
#245667=CARTESIAN_POINT('Ctrl Pts',(-44.0527517782421,39.2745942850999,
2.7547062579337));
#245668=CARTESIAN_POINT('Ctrl Pts',(-44.0110417363808,39.3566016867497,
2.79224250381919));
#245669=CARTESIAN_POINT('Ctrl Pts',(-44.0556530121008,39.4323285306301,
2.74901809108306));
#245670=CARTESIAN_POINT('Ctrl Pts',(-43.9290071509456,39.3050549810251,
2.63947868311709));
#245671=CARTESIAN_POINT('Ctrl Pts',(-43.9243964923851,39.3631024520343,
2.6959506676794));
#245672=CARTESIAN_POINT('Ctrl Pts',(-43.9614781338108,39.4299498468379,
2.68220539436068));
#245673=CARTESIAN_POINT('Ctrl Pts',(-43.8557442421764,39.349058390934,2.59908178585111));
#245674=CARTESIAN_POINT('Ctrl Pts',(-43.8675206320104,39.3917348424044,
2.65877670944926));
#245675=CARTESIAN_POINT('Ctrl Pts',(-43.9111340157076,39.4485000225472,
2.65878198860288));
#245676=CARTESIAN_POINT('Ctrl Pts',(-43.7969047596348,39.4144401478989,
2.5990817351605));
#245677=CARTESIAN_POINT('Ctrl Pts',(-43.8246341160487,39.4393948122688,
2.65878198860288));
#245678=CARTESIAN_POINT('Ctrl Pts',(-43.8769616275876,39.4864862581816,
2.65878198860288));
#245679=CARTESIAN_POINT('Origin',(-43.8769616275876,39.4864862581816,2.53178198860288));
#245680=CARTESIAN_POINT('Ctrl Pts',(-45.7656648676108,41.6348281284262,
3.77003198860292));
#245681=CARTESIAN_POINT('Ctrl Pts',(-45.850771417513,41.5403077290108,3.77003198860292));
#245682=CARTESIAN_POINT('Ctrl Pts',(-45.8506443599162,41.540448840768,3.64284238727584));
#245683=CARTESIAN_POINT('Ctrl Pts',(-45.926760978667,41.780179376798,3.77003198860292));
#245684=CARTESIAN_POINT('Ctrl Pts',(-46.0121552117534,41.6856176794229,
3.77025506105564));
#245685=CARTESIAN_POINT('Ctrl Pts',(-45.979592913563,41.6565546403116,3.64284210641854));
#245686=CARTESIAN_POINT('Ctrl Pts',(-46.0801233673956,41.9185498083246,
3.65553527987863));
#245687=CARTESIAN_POINT('Ctrl Pts',(-46.165749859238,41.8239142817211,3.65585996533324));
#245688=CARTESIAN_POINT('Ctrl Pts',(-46.1023497159542,41.7670853619641,
3.5512790271029));
#245689=CARTESIAN_POINT('Ctrl Pts',(-46.1654920697614,41.995572738225,3.47153072139099));
#245690=CARTESIAN_POINT('Ctrl Pts',(-46.2513146407508,41.9009568069088,
3.47182327905216));
#245691=CARTESIAN_POINT('Ctrl Pts',(-46.1706818552407,41.8286118967076,
3.40413028377992));
#245692=CARTESIAN_POINT('Origin',(-45.7656648676108,41.6348281284262,3.64303198860292));
#245693=CARTESIAN_POINT('Origin',(3.68378193773366E-16,1.91616684104774E-13,
2.53178198860262));
#245694=CARTESIAN_POINT('Origin',(-43.8565665267058,39.5091373124622,2.53178198860288));
#245695=CARTESIAN_POINT('Origin',(34.5756856720389,-30.7048488218242,3.64303198860241));
#245696=CARTESIAN_POINT('Origin',(-45.4673664422109,41.3663085755629,3.64299466007616));
#245697=CARTESIAN_POINT('Ctrl Pts',(-43.7765468711724,39.4370498736008,
2.5990817351605));
#245698=CARTESIAN_POINT('Ctrl Pts',(-43.8042633382931,39.4620188529809,
2.65878198860288));
#245699=CARTESIAN_POINT('Ctrl Pts',(-43.8565665267058,39.5091373124622,
2.65878198860288));
#245700=CARTESIAN_POINT('Ctrl Pts',(-43.717874483542,39.5021785224867,2.59908193199899));
#245701=CARTESIAN_POINT('Ctrl Pts',(-43.7615157339669,39.5094654441329,
2.65877685806683));
#245702=CARTESIAN_POINT('Ctrl Pts',(-43.822477090013,39.5469637653744,2.65878198860288));
#245703=CARTESIAN_POINT('Ctrl Pts',(-43.6818502604299,39.5788516269098,
2.63872492669802));
#245704=CARTESIAN_POINT('Ctrl Pts',(-43.7389249259236,39.5685043961838,
2.69532212015301));
#245705=CARTESIAN_POINT('Ctrl Pts',(-43.8091917332946,39.5983821485331,
2.6817683672665));
#245706=CARTESIAN_POINT('Ctrl Pts',(-43.6640874258692,39.7059848156962,
2.75442176402299));
#245707=CARTESIAN_POINT('Ctrl Pts',(-43.7412697217737,39.6560168722793,
2.79203179920158));
#245708=CARTESIAN_POINT('Ctrl Pts',(-43.8212571467117,39.6923865500764,
2.74885310748213));
#245709=CARTESIAN_POINT('Ctrl Pts',(-43.6806424921191,39.7566878101789,
2.82866089558412));
#245710=CARTESIAN_POINT('Ctrl Pts',(-43.7668962219017,39.684669524315,2.85316563119281));
#245711=CARTESIAN_POINT('Ctrl Pts',(-43.8452710114193,39.7348023770065,
2.79189751796631));
#245712=CARTESIAN_POINT('Ctrl Pts',(-43.7143933160625,39.7870778846747,
2.9013417351605));
#245713=CARTESIAN_POINT('Ctrl Pts',(-43.7993487829615,39.69345381678,2.90103711553256));
#245714=CARTESIAN_POINT('Ctrl Pts',(-43.8790236240222,39.7651933658998,
2.83404198860289));
#245715=CARTESIAN_POINT('Origin',(-43.7940440370146,39.8595727587355,2.83404198860289));
#245716=CARTESIAN_POINT('Origin',(-45.4345348103666,41.3366772856881,3.56647653971791));
#245717=CARTESIAN_POINT('Origin',(-45.3737170758075,41.2819167515328,3.42473028058513));
#245718=CARTESIAN_POINT('Origin',(-43.9264348094881,39.9787779456592,3.11913648168251));
#245719=CARTESIAN_POINT('Origin',(-44.058825581838,40.0979831325499,3.40423097483338));
#245720=CARTESIAN_POINT('Ctrl Pts',(-45.1285089182135,41.0611303347403,
3.36123028058509));
#245721=CARTESIAN_POINT('Ctrl Pts',(-45.2134885052211,40.9667509419047,
3.3612302805851));
#245722=CARTESIAN_POINT('Ctrl Pts',(-45.2134885052211,40.9667509419047,
3.23423028058509));
#245723=CARTESIAN_POINT('Ctrl Pts',(-45.1955564429365,41.121185060844,3.36123028058509));
#245724=CARTESIAN_POINT('Ctrl Pts',(-45.2803165088389,41.0269231466363,
3.36099641108286));
#245725=CARTESIAN_POINT('Ctrl Pts',(-45.3138235084265,41.0570929845756,
3.23423043688394));
#245726=CARTESIAN_POINT('Ctrl Pts',(-45.2589537050067,41.177972685567,3.41054258905313));
#245727=CARTESIAN_POINT('Ctrl Pts',(-45.3438226072599,41.0841042944923,
3.41008815826159));
#245728=CARTESIAN_POINT('Ctrl Pts',(-45.4086973919092,41.1425178129616,
3.30819867304353));
#245729=CARTESIAN_POINT('Ctrl Pts',(-45.2923641298559,41.2079002115907,
3.48823028058512));
#245730=CARTESIAN_POINT('Ctrl Pts',(-45.3773275334107,41.1142722655006,
3.48794691941628));
#245731=CARTESIAN_POINT('Ctrl Pts',(-45.4586966628151,41.1875373586972,
3.42473028058512));
#245732=CARTESIAN_POINT('Origin',(-45.1285089182135,41.0611303347403,3.23423028058509));
#245733=CARTESIAN_POINT('Ctrl Pts',(-43.9791725362585,40.0254908126588,
3.471530721391));
#245734=CARTESIAN_POINT('Ctrl Pts',(-44.064255127713,39.9317223035499,3.47122746285105));
#245735=CARTESIAN_POINT('Ctrl Pts',(-44.1439246046464,40.0037114707677,
3.40413046676838));
#245736=CARTESIAN_POINT('Ctrl Pts',(-44.0645378932546,40.102520236038,3.65553813458013));
#245737=CARTESIAN_POINT('Ctrl Pts',(-44.1495813562469,40.0085500157883,
3.65520336072072));
#245738=CARTESIAN_POINT('Ctrl Pts',(-44.2122579788868,40.0652391174802,
3.55128134519897));
#245739=CARTESIAN_POINT('Ctrl Pts',(-44.2178941385633,40.2409001323912,
3.77003198860291));
#245740=CARTESIAN_POINT('Ctrl Pts',(-44.3029888158473,40.1466780419432,
3.76980209314169));
#245741=CARTESIAN_POINT('Ctrl Pts',(-44.3350158129974,40.1757707681154,
3.64284195387508));
#245742=CARTESIAN_POINT('Ctrl Pts',(-44.3789831537298,40.3862543050938,
3.77003198860291));
#245743=CARTESIAN_POINT('Ctrl Pts',(-44.4640900341665,40.2917335385827,
3.77003198860291));
#245744=CARTESIAN_POINT('Ctrl Pts',(-44.4639626455417,40.2918750179836,
3.64284189403873));
#245745=CARTESIAN_POINT('Origin',(-44.3789831537298,40.3862543050938,3.64303198860291));
#245746=CARTESIAN_POINT('Origin',(33.743309857225,-29.95537427179,3.23423028058461));
#245747=CARTESIAN_POINT('Origin',(-45.0161393894795,40.9599523566124,3.23423028058509));
#245748=CARTESIAN_POINT('Origin',(33.61296347236,-29.838009859698,3.64303198860242));
#245749=CARTESIAN_POINT('Origin',(-44.6772189625502,40.6548553974686,3.64299171721674));
#245750=CARTESIAN_POINT('Ctrl Pts',(-44.8522789915944,40.8131880745606,
3.48823028058509));
#245751=CARTESIAN_POINT('Ctrl Pts',(-44.9380175594364,40.7187157882337,
3.48852004212287));
#245752=CARTESIAN_POINT('Ctrl Pts',(-44.8559107663287,40.6447864996552,
3.42473028058509));
#245753=CARTESIAN_POINT('Ctrl Pts',(-44.8858042435428,40.843214657665,3.41028005848434));
#245754=CARTESIAN_POINT('Ctrl Pts',(-44.9712860523935,40.7486708738403,
3.41074404220265));
#245755=CARTESIAN_POINT('Ctrl Pts',(-44.9060790100831,40.689958189227,3.30780486243972));
#245756=CARTESIAN_POINT('Ctrl Pts',(-44.9493173051407,40.9001003367644,
3.3612302805851));
#245757=CARTESIAN_POINT('Ctrl Pts',(-45.0343891839537,40.8054891887047,
3.36146460586606));
#245758=CARTESIAN_POINT('Ctrl Pts',(-45.0011219300378,40.775535218736,3.23423045308401));
#245759=CARTESIAN_POINT('Ctrl Pts',(-45.0161393894795,40.9599523566124,
3.36123028058509));
#245760=CARTESIAN_POINT('Ctrl Pts',(-45.1011189764871,40.8655729637768,
3.36123028058509));
#245761=CARTESIAN_POINT('Ctrl Pts',(-45.1011189764871,40.8655729637768,
3.23423028058509));
#245762=CARTESIAN_POINT('Origin',(-44.7709311793212,40.7391658924908,3.42473028058509));
#245763=CARTESIAN_POINT('Origin',(-44.7104761492019,40.6847319392793,3.56563113524801));
#245764=CARTESIAN_POINT('Origin',(-49.8797426639493,35.847302748828,3.56647653909474));
#245765=CARTESIAN_POINT('Origin',(-49.915552518432,35.8732562382988,3.64299466007634));
#245766=CARTESIAN_POINT('Origin',(-49.8135340601225,35.7991993820661,3.42473028058508));
#245767=CARTESIAN_POINT('Ctrl Pts',(-49.7242207306177,35.7350130971388,
3.48823028058508));
#245768=CARTESIAN_POINT('Ctrl Pts',(-49.6503036646787,35.8375861910556,
3.48794691941624));
#245769=CARTESIAN_POINT('Ctrl Pts',(-49.7388853330813,35.9019445403518,
3.42473028058509));
#245770=CARTESIAN_POINT('Ctrl Pts',(-49.6878783768796,35.7084656432358,
3.41028005925112));
#245771=CARTESIAN_POINT('Ctrl Pts',(-49.613705655414,35.8109961808853,3.40982512231007));
#245772=CARTESIAN_POINT('Ctrl Pts',(-49.6842702092612,35.8622643302242,
3.3078048637291));
#245773=CARTESIAN_POINT('Ctrl Pts',(-49.6190282456272,35.6581711379708,
3.36123028058506));
#245774=CARTESIAN_POINT('Ctrl Pts',(-49.5444483977897,35.760677837847,3.36099721048571));
#245775=CARTESIAN_POINT('Ctrl Pts',(-49.5808027344257,35.7870908094908,
3.23423045308381));
#245776=CARTESIAN_POINT('Ctrl Pts',(-49.5465907136146,35.6052536882601,
3.36123028058506));
#245777=CARTESIAN_POINT('Ctrl Pts',(-49.4719419865735,35.7079988465457,
3.36123028058506));
#245778=CARTESIAN_POINT('Ctrl Pts',(-49.4719419865735,35.7079988465457,
3.23423028058506));
#245779=CARTESIAN_POINT('Origin',(-49.5465907136146,35.6052536882601,3.23423028058506));
#245780=CARTESIAN_POINT('Origin',(-0.186621817602853,-0.256862895713863,
3.64303198860262));
#245781=CARTESIAN_POINT('Origin',(-50.2402240048085,36.1092077731528,3.64303198860287));
#245782=CARTESIAN_POINT('Origin',(-0.186621817602853,-0.25686289571386,
3.23423028058481));
#245783=CARTESIAN_POINT('Origin',(-49.4242607783462,35.5163757878395,3.23423028058505));
#245784=CARTESIAN_POINT('Ctrl Pts',(-50.676214228995,36.4252947698678,3.47153072139096));
#245785=CARTESIAN_POINT('Ctrl Pts',(-50.6015094050814,36.5289136610819,
3.47182327902686));
#245786=CARTESIAN_POINT('Ctrl Pts',(-50.5139809070353,36.4650842624218,
3.40413028959039));
#245787=CARTESIAN_POINT('Ctrl Pts',(-50.5831238715073,36.3578045222561,
3.65553807120982));
#245788=CARTESIAN_POINT('Ctrl Pts',(-50.5083591136207,36.4612356912264,
3.65586275496999));
#245789=CARTESIAN_POINT('Ctrl Pts',(-50.439590694023,36.4110366091612,3.55128126837341));
#245790=CARTESIAN_POINT('Ctrl Pts',(-50.4158900112687,36.2365613423295,
3.77003198860288));
#245791=CARTESIAN_POINT('Ctrl Pts',(-50.3411491755171,36.3397499727027,
3.77025505748535));
#245792=CARTESIAN_POINT('Ctrl Pts',(-50.3059517008877,36.3139421975373,
3.64284211731124));
#245793=CARTESIAN_POINT('Ctrl Pts',(-50.2402240048085,36.1092077731528,
3.77003198860288));
#245794=CARTESIAN_POINT('Ctrl Pts',(-50.1654637560305,36.2121064279407,
3.77003198860288));
#245795=CARTESIAN_POINT('Ctrl Pts',(-50.1655753609471,36.2119528169512,
3.64284239821701));
#245796=CARTESIAN_POINT('Origin',(-50.5887599058103,36.3624339277672,3.40423097483334));
#245797=CARTESIAN_POINT('Ctrl Pts',(-49.4242607783463,35.5163757878395,
3.36123028058505));
#245798=CARTESIAN_POINT('Ctrl Pts',(-49.3496120513051,35.6191209461251,
3.36123028058505));
#245799=CARTESIAN_POINT('Ctrl Pts',(-49.3496120513051,35.6191209461251,
3.23423028058505));
#245800=CARTESIAN_POINT('Ctrl Pts',(-49.3515787599192,35.4632790141046,
3.36123028058505));
#245801=CARTESIAN_POINT('Ctrl Pts',(-49.2767219882431,35.5661632154426,
3.3614653861002));
#245802=CARTESIAN_POINT('Ctrl Pts',(-49.2403833690702,35.5397616632035,
3.23423043688465));
#245803=CARTESIAN_POINT('Ctrl Pts',(-49.2828534857269,35.4130704930598,
3.41054258693124));
#245804=CARTESIAN_POINT('Ctrl Pts',(-49.2081487547882,35.5163418450556,
3.41100608859887));
#245805=CARTESIAN_POINT('Ctrl Pts',(-49.1370998624035,35.4647218031686,
3.30819866970857));
#245806=CARTESIAN_POINT('Ctrl Pts',(-49.2466351556014,35.3866101428259,
3.48823028058505));
#245807=CARTESIAN_POINT('Ctrl Pts',(-49.1720533660033,35.4901170100366,
3.48852004212283));
#245808=CARTESIAN_POINT('Ctrl Pts',(-49.0826686475736,35.4251752107437,
3.42473028058505));
#245809=CARTESIAN_POINT('Origin',(-49.1573173746148,35.3224300524581,3.42473028058505));
#245810=CARTESIAN_POINT('Origin',(-50.7328855645271,36.4671473482322,3.11913648178468));
#245811=CARTESIAN_POINT('Origin',(-50.8770112231004,36.5718607685321,2.83404198860286));
#245812=CARTESIAN_POINT('Origin',(-49.0915036252753,35.274613564645,3.5656311346094));
#245813=CARTESIAN_POINT('Origin',(-49.0553654007528,35.2482948100391,3.64299171721782));
#245814=CARTESIAN_POINT('Ctrl Pts',(-50.9399462128204,36.9911673391707,
2.59908173516048));
#245815=CARTESIAN_POINT('Ctrl Pts',(-50.9097606317996,36.969247412634,2.65878198860286));
#245816=CARTESIAN_POINT('Ctrl Pts',(-50.8527980281387,36.9278827595326,
2.65878198860287));
#245817=CARTESIAN_POINT('Ctrl Pts',(-50.9917217504959,36.9198678602472,
2.59908193475632));
#245818=CARTESIAN_POINT('Ctrl Pts',(-50.9474721267405,36.9173100216906,
2.65878715325524));
#245819=CARTESIAN_POINT('Ctrl Pts',(-50.8827604229953,36.8866065570943,
2.65878198860287));
#245820=CARTESIAN_POINT('Ctrl Pts',(-51.019255329238,36.839377280089,2.63878778849898));
#245821=CARTESIAN_POINT('Ctrl Pts',(-50.9634900918195,36.8558881875867,
2.69564460180132));
#245822=CARTESIAN_POINT('Ctrl Pts',(-50.8901678911826,36.8338178466775,
2.6818048162491));
#245823=CARTESIAN_POINT('Ctrl Pts',(-51.0231582082089,36.7103770798843,
2.75443238878668));
#245824=CARTESIAN_POINT('Ctrl Pts',(-50.9515780553177,36.7689134067396,
2.79268340777122));
#245825=CARTESIAN_POINT('Ctrl Pts',(-50.8676678805079,36.7411592876132,
2.74885926835633));
#245826=CARTESIAN_POINT('Ctrl Pts',(-51.0012539523497,36.6614543958828,
2.82856655361696));
#245827=CARTESIAN_POINT('Ctrl Pts',(-50.9229784487439,36.7432876021376,
2.85384197230838));
#245828=CARTESIAN_POINT('Ctrl Pts',(-50.8391515810796,36.7013347616514,
2.79184624278597));
#245829=CARTESIAN_POINT('Ctrl Pts',(-50.9644637245895,36.6347241449654,
2.90134173516048));
#245830=CARTESIAN_POINT('Ctrl Pts',(-50.8898702560319,36.7381840359683,
2.90163218716416));
#245831=CARTESIAN_POINT('Ctrl Pts',(-50.8023624960593,36.6746059268177,
2.83404198860287));
#245832=CARTESIAN_POINT('Origin',(-50.8527980281387,36.9278827595326,2.53178198860286));
#245833=CARTESIAN_POINT('Origin',(-0.186621817602853,-0.256862895713863,
3.64303198860262));
#245834=CARTESIAN_POINT('Origin',(-48.7306271754178,35.0124214764584,3.64303198860286));
#245835=CARTESIAN_POINT('Origin',(1.03190816135906E-16,1.91480515074693E-13,
2.53178198860262));
#245836=CARTESIAN_POINT('Origin',(-50.8348823336488,36.9525415975211,2.53178198860287));
#245837=CARTESIAN_POINT('Ctrl Pts',(-48.7306271754178,35.0124214764584,
3.77003198860287));
#245838=CARTESIAN_POINT('Ctrl Pts',(-48.6558666212127,35.1153205516307,
3.77003198860288));
#245839=CARTESIAN_POINT('Ctrl Pts',(-48.6559785320123,35.1151665196294,
3.64284187937076));
#245840=CARTESIAN_POINT('Ctrl Pts',(-48.5549543235562,34.8850714976654,
3.77003198860287));
#245841=CARTESIAN_POINT('Ctrl Pts',(-48.4804833899302,34.9878965398035,
3.7698020896276));
#245842=CARTESIAN_POINT('Ctrl Pts',(-48.5155997094332,35.013175335312,3.64284193928272));
#245843=CARTESIAN_POINT('Ctrl Pts',(-48.387715124058,34.7638382096883,3.65553535416607));
#245844=CARTESIAN_POINT('Ctrl Pts',(-48.3134799021678,34.8665607873114,
3.65520057834561));
#245845=CARTESIAN_POINT('Ctrl Pts',(-48.381961710728,34.9160816462009,3.55127910964313));
#245846=CARTESIAN_POINT('Ctrl Pts',(-48.2946219293748,34.6963546279284,
3.47153072139095));
#245847=CARTESIAN_POINT('Ctrl Pts',(-48.2205921440832,34.7990735417351,
3.47122746281605));
#245848=CARTESIAN_POINT('Ctrl Pts',(-48.3075724095163,34.8620346554129,
3.404130459013));
#245849=CARTESIAN_POINT('Origin',(-48.3820909175331,34.7591950625533,3.40423097483334));
#245850=CARTESIAN_POINT('Ctrl Pts',(-50.5905785208486,37.149332979726,2.90134173516048));
#245851=CARTESIAN_POINT('Ctrl Pts',(-50.6659240749085,37.0464195108252,
2.90163218716416));
#245852=CARTESIAN_POINT('Ctrl Pts',(-50.5784163149359,36.9828414016746,
2.83404198860287));
#245853=CARTESIAN_POINT('Ctrl Pts',(-50.6273860247241,37.1760745934437,
2.82853349835373));
#245854=CARTESIAN_POINT('Ctrl Pts',(-50.6810174228646,37.076347161577,2.85381483162311));
#245855=CARTESIAN_POINT('Ctrl Pts',(-50.6152221632643,37.0095824157645,
2.79182701594214));
#245856=CARTESIAN_POINT('Ctrl Pts',(-50.6805407410139,37.181676964489,2.75468822073675));
#245857=CARTESIAN_POINT('Ctrl Pts',(-50.7141678268708,37.095483395543,2.79286913083874));
#245858=CARTESIAN_POINT('Ctrl Pts',(-50.6617655220316,37.0242869695755,
2.74900763297951));
#245859=CARTESIAN_POINT('Ctrl Pts',(-50.8012099538927,37.138681150061,2.6395445064041));
#245860=CARTESIAN_POINT('Ctrl Pts',(-50.7999485296221,37.0803097184692,
2.69627684028872));
#245861=CARTESIAN_POINT('Ctrl Pts',(-50.7562647493201,37.0173098767918,
2.68224356036502));
#245862=CARTESIAN_POINT('Ctrl Pts',(-50.8700180268811,37.0873787017258,
2.59908178706437));
#245863=CARTESIAN_POINT('Ctrl Pts',(-50.8539379904871,37.0460487315396,
2.6587870432151));
#245864=CARTESIAN_POINT('Ctrl Pts',(-50.8047860147156,36.9939291606759,
2.65878198860286));
#245865=CARTESIAN_POINT('Ctrl Pts',(-50.9219998155902,37.0158684358559,
2.59908173516048));
#245866=CARTESIAN_POINT('Ctrl Pts',(-50.8918248691002,36.9939338721432,
2.65878198860286));
#245867=CARTESIAN_POINT('Ctrl Pts',(-50.8348823336488,36.9525415975211,
2.65878198860287));
#245868=CARTESIAN_POINT('Origin',(-50.5037675878947,37.0855865599602,2.83404198860287));
#245869=CARTESIAN_POINT('Origin',(-48.2379650606672,34.6544814981911,3.11913648167148));
#245870=CARTESIAN_POINT('Origin',(-48.093839203715,34.549767933694,2.83404198860285));
#245871=CARTESIAN_POINT('Origin',(-50.3596419293379,36.9808731396133,3.11913648177577));
#245872=CARTESIAN_POINT('Origin',(-50.2155162706046,36.8761597191953,3.40423097483335));
#245873=CARTESIAN_POINT('Ctrl Pts',(-48.0063682005189,34.4869303039396,
2.90134173516046));
#245874=CARTESIAN_POINT('Ctrl Pts',(-47.9324532779039,34.5894948283133,
2.90103711553253));
#245875=CARTESIAN_POINT('Ctrl Pts',(-48.0191904766738,34.6525130919796,
2.83404198860285));
#245876=CARTESIAN_POINT('Ctrl Pts',(-47.9696093621199,34.4602241019851,
2.82862991747992));
#245877=CARTESIAN_POINT('Ctrl Pts',(-47.917105603147,34.5595620694344,2.85314045886476));
#245878=CARTESIAN_POINT('Ctrl Pts',(-47.9824304277182,34.6258053530819,
2.79187961000006));
#245879=CARTESIAN_POINT('Ctrl Pts',(-47.9167391807671,34.4546775021468,
2.75470625793343));
#245880=CARTESIAN_POINT('Ctrl Pts',(-47.8838297385501,34.5405955452484,
2.79224250381911));
#245881=CARTESIAN_POINT('Ctrl Pts',(-47.9361122396531,34.6112444014589,
2.74901809108276));
#245882=CARTESIAN_POINT('Ctrl Pts',(-47.7968564492224,34.4979061669209,
2.63947868311727));
#245883=CARTESIAN_POINT('Ctrl Pts',(-47.7983386612733,34.5561175928641,
2.69595066767943));
#245884=CARTESIAN_POINT('Ctrl Pts',(-47.8422046210394,34.6187227036514,
2.6822053943609));
#245885=CARTESIAN_POINT('Ctrl Pts',(-47.7285944911489,34.549326580815,2.59908178585132));
#245886=CARTESIAN_POINT('Ctrl Pts',(-47.7447672725779,34.5905382782875,
2.65877670944887));
#245887=CARTESIAN_POINT('Ctrl Pts',(-47.7940753146439,34.6424336528583,
2.65878198860285));
#245888=CARTESIAN_POINT('Ctrl Pts',(-47.6769115920305,34.6205005703634,
2.59908173516047));
#245889=CARTESIAN_POINT('Ctrl Pts',(-47.7070975168465,34.6424200234574,
2.65878198860285));
#245890=CARTESIAN_POINT('Ctrl Pts',(-47.7640607692765,34.6837837831345,
2.65878198860285));
#245891=CARTESIAN_POINT('Origin',(-47.7640607692765,34.6837837831345,2.53178198860285));
#245892=CARTESIAN_POINT('Ctrl Pts',(-49.8669803696028,36.6229335645809,
3.77003198860288));
#245893=CARTESIAN_POINT('Ctrl Pts',(-49.9417406248213,36.5200349009283,
3.77003198860289));
#245894=CARTESIAN_POINT('Ctrl Pts',(-49.9416290134545,36.5201885207956,
3.64284238727612));
#245895=CARTESIAN_POINT('Ctrl Pts',(-50.0423873219327,36.7506494346794,
3.77003198860288));
#245896=CARTESIAN_POINT('Ctrl Pts',(-50.1174293675641,36.6476796282231,
3.77025506105648));
#245897=CARTESIAN_POINT('Ctrl Pts',(-50.0820075342365,36.6221794864687,
3.64284210641859));
#245898=CARTESIAN_POINT('Ctrl Pts',(-50.2093732240185,36.872231123687,3.65553527987858));
#245899=CARTESIAN_POINT('Ctrl Pts',(-50.2846385388092,36.7691636147952,
3.65585996533204));
#245900=CARTESIAN_POINT('Ctrl Pts',(-50.2156454684952,36.7192731293512,
3.55127902710267));
#245901=CARTESIAN_POINT('Ctrl Pts',(-50.3023253561997,36.9399086546485,
3.47153072139096));
#245902=CARTESIAN_POINT('Ctrl Pts',(-50.3777877242642,36.8368401378449,
3.47182327905213));
#245903=CARTESIAN_POINT('Ctrl Pts',(-50.2900345513017,36.7733199617897,
3.40413028378005));
#245904=CARTESIAN_POINT('Origin',(-49.8669803696028,36.6229335645809,3.64303198860288));
#245905=CARTESIAN_POINT('Origin',(3.64514313700082E-16,1.91611912610258E-13,
2.53178198860262));
#245906=CARTESIAN_POINT('Origin',(-47.7461450747866,34.7084426211231,2.53178198860285));
#245907=CARTESIAN_POINT('Origin',(40.911747809259,-29.3316730956001,3.64303198860243));
#245908=CARTESIAN_POINT('Origin',(-49.5422481179709,36.3870656659281,3.6429946600739));
#245909=CARTESIAN_POINT('Ctrl Pts',(-47.6590285860937,34.6451144164185,
2.59908173516047));
#245910=CARTESIAN_POINT('Ctrl Pts',(-47.6892031885515,34.6670494534017,
2.65878198860286));
#245911=CARTESIAN_POINT('Ctrl Pts',(-47.7461450747866,34.7084426211231,
2.65878198860285));
#245912=CARTESIAN_POINT('Ctrl Pts',(-47.6074854095247,34.7160192182667,
2.59908193199939));
#245913=CARTESIAN_POINT('Ctrl Pts',(-47.6516492793366,34.718704468553,2.65877685806607));
#245914=CARTESIAN_POINT('Ctrl Pts',(-47.7161963245898,34.7496251732003,
2.65878198860285));
#245915=CARTESIAN_POINT('Ctrl Pts',(-47.5796730526554,34.7960378560836,
2.63872492669829));
#245916=CARTESIAN_POINT('Ctrl Pts',(-47.6353534770329,34.7797813814945,
2.69532212015307));
#245917=CARTESIAN_POINT('Ctrl Pts',(-47.7083584310196,34.8021505789971,
2.68176836726655));
#245918=CARTESIAN_POINT('Ctrl Pts',(-47.5752965616147,34.9243313177595,
2.75442176402265));
#245919=CARTESIAN_POINT('Ctrl Pts',(-47.6468329724884,34.8665693571826,
2.7920317992015));
#245920=CARTESIAN_POINT('Ctrl Pts',(-47.7301838844734,34.8943788354696,
2.74885310748201));
#245921=CARTESIAN_POINT('Ctrl Pts',(-47.5970608435764,34.9730260802987,
2.82866089558427));
#245922=CARTESIAN_POINT('Ctrl Pts',(-47.6753141056554,34.8923863483139,
2.85316563119179));
#245923=CARTESIAN_POINT('Ctrl Pts',(-47.7584998599246,34.9340521716868,
2.79189751796643));
#245924=CARTESIAN_POINT('Ctrl Pts',(-47.6338034047601,34.999721753026,2.90134173516047));
#245925=CARTESIAN_POINT('Ctrl Pts',(-47.7085070967805,34.8977303031701,
2.90103711553253));
#245926=CARTESIAN_POINT('Ctrl Pts',(-47.7952442955504,34.9607485668365,
2.83404198860285));
#245927=CARTESIAN_POINT('Origin',(-47.7205955685092,35.0634937251221,2.83404198860286));
#245928=CARTESIAN_POINT('Origin',(-49.5064990280443,36.3610285393819,3.56647653971805));
#245929=CARTESIAN_POINT('Origin',(-49.4402904249167,36.3129251734942,3.42473028058509));
#245930=CARTESIAN_POINT('Origin',(-47.8647214254834,35.1682072895626,3.11913648168123));
#245931=CARTESIAN_POINT('Origin',(-48.0088472823274,35.2729208539814,3.40423097483334));
#245932=CARTESIAN_POINT('Ctrl Pts',(-49.1733470784089,36.1189794796882,
3.36123028058506));
#245933=CARTESIAN_POINT('Ctrl Pts',(-49.2479958054501,36.0162343214026,
3.36123028058506));
#245934=CARTESIAN_POINT('Ctrl Pts',(-49.2479958054501,36.0162343214026,
3.23423028058506));
#245935=CARTESIAN_POINT('Ctrl Pts',(-49.2463047380073,36.1716968449942,
3.36123028058506));
#245936=CARTESIAN_POINT('Ctrl Pts',(-49.3207474263649,36.0690914679788,
3.36099641108653));
#245937=CARTESIAN_POINT('Ctrl Pts',(-49.3572244778977,36.0955935972133,
3.23423043688382));
#245938=CARTESIAN_POINT('Ctrl Pts',(-49.3152906263876,36.2215465627872,
3.4105425890531));
#245939=CARTESIAN_POINT('Ctrl Pts',(-49.3898826892439,36.1193211766501,
3.41008815825897));
#245940=CARTESIAN_POINT('Ctrl Pts',(-49.4605079583581,36.1706334382083,
3.30819867304314));
#245941=CARTESIAN_POINT('Ctrl Pts',(-49.3516463037387,36.247817802325,3.48823028058507));
#245942=CARTESIAN_POINT('Ctrl Pts',(-49.4263574835553,36.1458216659124,
3.48794691941623));
#245943=CARTESIAN_POINT('Ctrl Pts',(-49.5149391519579,36.2101800152086,
3.42473028058508));
#245944=CARTESIAN_POINT('Origin',(-49.1733470784089,36.1189794796882,3.23423028058506));
#245945=CARTESIAN_POINT('Ctrl Pts',(-47.9220530736689,35.2091516650527,
3.47153072139096));
#245946=CARTESIAN_POINT('Ctrl Pts',(-47.9968680956249,35.1070032771125,
3.47122746285101));
#245947=CARTESIAN_POINT('Ctrl Pts',(-48.0836260518489,35.1702703521464,
3.40413046676846));
#245948=CARTESIAN_POINT('Ctrl Pts',(-48.0150025575578,35.2768360036103,
3.6555381345801));
#245949=CARTESIAN_POINT('Ctrl Pts',(-48.0897575808477,35.1744910995569,
3.65520336072258));
#245950=CARTESIAN_POINT('Ctrl Pts',(-48.1580164790759,35.2243181613741,
3.55128134519869));
#245951=CARTESIAN_POINT('Ctrl Pts',(-48.1819833392252,35.3984277477531,
3.77003198860287));
#245952=CARTESIAN_POINT('Ctrl Pts',(-48.2567629686426,35.2958269999292,
3.76980209313974));
#245953=CARTESIAN_POINT('Ctrl Pts',(-48.2916555365082,35.321412620307,3.64284195387526));
#245954=CARTESIAN_POINT('Ctrl Pts',(-48.3573835402121,35.5261472678865,
3.77003198860287));
#245955=CARTESIAN_POINT('Ctrl Pts',(-48.4321440857825,35.4232482045988,
3.77003198860288));
#245956=CARTESIAN_POINT('Ctrl Pts',(-48.4320321836304,35.4234022246978,
3.64284189403891));
#245957=CARTESIAN_POINT('Origin',(-48.3573835402121,35.5261472678865,3.64303198860286));
#245958=CARTESIAN_POINT('Origin',(39.9252688514649,-28.6149541797803,3.23423028058462));
#245959=CARTESIAN_POINT('Origin',(-49.0510171431405,36.0301015792676,3.23423028058506));
#245960=CARTESIAN_POINT('Origin',(39.7707905934409,-28.5027191556737,3.64303198860243));
#245961=CARTESIAN_POINT('Origin',(-48.6820620414858,35.7621028045852,3.64299171721768));
#245962=CARTESIAN_POINT('Ctrl Pts',(-48.8727133447945,35.9012693628904,
3.48823028058505));
#245963=CARTESIAN_POINT('Ctrl Pts',(-48.9481071848799,35.7983524848935,
3.48852004212283));
#245964=CARTESIAN_POINT('Ctrl Pts',(-48.8587224664502,35.7334106856006,
3.42473028058505));
#245965=CARTESIAN_POINT('Ctrl Pts',(-48.9091935744932,35.9276271141652,
3.41028005848429));
#245966=CARTESIAN_POINT('Ctrl Pts',(-48.9843245886213,35.8246659689648,
3.4107440422049));
#245967=CARTESIAN_POINT('Ctrl Pts',(-48.9133376106124,35.7730909105076,
3.30780486244038));
#245968=CARTESIAN_POINT('Ctrl Pts',(-48.9783048775114,35.9775622448375,
3.36123028058506));
#245969=CARTESIAN_POINT('Ctrl Pts',(-49.0530211657533,35.8745769537851,
3.36146460586455));
#245970=CARTESIAN_POINT('Ctrl Pts',(-49.0168051108889,35.8482644497248,
3.23423045308401));
#245971=CARTESIAN_POINT('Ctrl Pts',(-49.0510171431405,36.0301015792676,
3.36123028058506));
#245972=CARTESIAN_POINT('Ctrl Pts',(-49.1256658701817,35.927356420982,3.36123028058506));
#245973=CARTESIAN_POINT('Ctrl Pts',(-49.1256658701817,35.927356420982,3.23423028058506));
#245974=CARTESIAN_POINT('Origin',(-48.7840737394091,35.8361558438862,3.42473028058505));
#245975=CARTESIAN_POINT('Origin',(-48.7182599907926,35.7883393569606,3.5656311352483));
#245976=CARTESIAN_POINT('Origin',(-53.3535596832588,30.4370746247569,3.56647653909402));
#245977=CARTESIAN_POINT('Origin',(-53.3918862459828,30.4591427892372,3.64299466007387));
#245978=CARTESIAN_POINT('Origin',(-53.2826856060847,30.3961554568836,3.42473028058504));
#245979=CARTESIAN_POINT('Ctrl Pts',(-53.1871522506177,30.3416565762235,
3.48823028058504));
#245980=CARTESIAN_POINT('Ctrl Pts',(-53.1243619179797,30.4513942013112,
3.4879469194162));
#245981=CARTESIAN_POINT('Ctrl Pts',(-53.2191856060847,30.5061406831642,
3.42473028058505));
#245982=CARTESIAN_POINT('Ctrl Pts',(-53.1482340195358,30.3190533624383,
3.41028005925105));
#245983=CARTESIAN_POINT('Ctrl Pts',(-53.085184983539,30.4287753876654,3.40982512231084));
#245984=CARTESIAN_POINT('Ctrl Pts',(-53.1607219582407,30.4723866803437,
3.30780486372897));
#245985=CARTESIAN_POINT('Ctrl Pts',(-53.0745038491598,30.2762311741519,
3.36123028058502));
#245986=CARTESIAN_POINT('Ctrl Pts',(-53.0110474253448,30.3859720484845,
3.36099721048431));
#245987=CARTESIAN_POINT('Ctrl Pts',(-53.0499635164575,30.4084402641651,
3.23423045308386));
#245988=CARTESIAN_POINT('Ctrl Pts',(-52.9969317578289,30.2311753956711,
3.36123028058502));
#245989=CARTESIAN_POINT('Ctrl Pts',(-52.9334317578289,30.3411606219517,
3.36123028058502));
#245990=CARTESIAN_POINT('Ctrl Pts',(-52.9334317578289,30.3411606219517,
3.23423028058502));
#245991=CARTESIAN_POINT('Origin',(-52.9969317578289,30.2311753956711,3.23423028058502));
#245992=CARTESIAN_POINT('Origin',(-0.158749999999993,-0.274963065701376,
3.64303198860262));
#245993=CARTESIAN_POINT('Origin',(-53.7394427993288,30.6598643453573,3.64303198860283));
#245994=CARTESIAN_POINT('Origin',(-0.158749999999993,-0.274963065701374,
3.23423028058481));
#245995=CARTESIAN_POINT('Origin',(-52.8659816883961,30.1555713378337,3.23423028058502));
#245996=CARTESIAN_POINT('Ctrl Pts',(-54.2060847114743,30.9286463962977,
3.47153072139093));
#245997=CARTESIAN_POINT('Ctrl Pts',(-54.1426202518671,31.0395064328256,
3.47182327902683));
#245998=CARTESIAN_POINT('Ctrl Pts',(-54.0488992551385,30.9851759176838,
3.40413028959074));
#245999=CARTESIAN_POINT('Ctrl Pts',(-54.1064496608378,30.8712564593355,
3.65553807120978));
#246000=CARTESIAN_POINT('Ctrl Pts',(-54.0429059732648,30.9819360667867,
3.65586275496898));
#246001=CARTESIAN_POINT('Ctrl Pts',(-53.9692670413545,30.9392002377691,
3.55128126837296));
#246002=CARTESIAN_POINT('Ctrl Pts',(-53.9274585619028,30.7681581606536,
3.77003198860284));
#246003=CARTESIAN_POINT('Ctrl Pts',(-53.8639133132293,30.8785940576181,
3.77025505748651));
#246004=CARTESIAN_POINT('Ctrl Pts',(-53.8262110069733,30.8566067980797,
3.64284211731175));
#246005=CARTESIAN_POINT('Ctrl Pts',(-53.7394427993288,30.6598643453573,
3.77003198860284));
#246006=CARTESIAN_POINT('Ctrl Pts',(-53.6758479332736,30.7700138844656,
3.77003198860284));
#246007=CARTESIAN_POINT('Ctrl Pts',(-53.6759428700858,30.7698494490833,
3.64284239821767));
#246008=CARTESIAN_POINT('Origin',(-54.1125387249981,30.875271378476,3.40423097483331));
#246009=CARTESIAN_POINT('Ctrl Pts',(-52.8659816883961,30.1555713378337,
3.36123028058502));
#246010=CARTESIAN_POINT('Ctrl Pts',(-52.8024816883961,30.2655565641143,
3.36123028058501));
#246011=CARTESIAN_POINT('Ctrl Pts',(-52.8024816883961,30.2655565641143,
3.23423028058502));
#246012=CARTESIAN_POINT('Ctrl Pts',(-52.7881477055081,30.1103627734739,
3.36123028058502));
#246013=CARTESIAN_POINT('Ctrl Pts',(-52.7244553345228,30.2205080277008,
3.36146538610177));
#246014=CARTESIAN_POINT('Ctrl Pts',(-52.6855560684232,30.1980495259478,
3.234230436884));
#246015=CARTESIAN_POINT('Ctrl Pts',(-52.7145506960111,30.0676130472592,
3.41054258693121));
#246016=CARTESIAN_POINT('Ctrl Pts',(-52.6510500011257,30.1781274387056,
3.41100608859674));
#246017=CARTESIAN_POINT('Ctrl Pts',(-52.5749945583554,30.1342168083481,
3.3081986697083));
#246018=CARTESIAN_POINT('Ctrl Pts',(-52.6757649139397,30.0450834959835,
3.48823028058501));
#246019=CARTESIAN_POINT('Ctrl Pts',(-52.6124111049558,30.1558192616,3.48852004212279));
#246020=CARTESIAN_POINT('Ctrl Pts',(-52.5167277788843,30.1005764675357,
3.42473028058501));
#246021=CARTESIAN_POINT('Origin',(-52.5802277788843,29.9905912412551,3.42473028058501));
#246022=CARTESIAN_POINT('Origin',(-54.2668203812018,30.9643459342447,3.11913648178522));
#246023=CARTESIAN_POINT('Origin',(-54.421102037244,31.0534204898633,2.83404198860282));
#246024=CARTESIAN_POINT('Origin',(-52.5097763801594,29.949916107244,3.56563113460861));
#246025=CARTESIAN_POINT('Origin',(-52.4710850656385,29.9275190026057,3.64299171721761));
#246026=CARTESIAN_POINT('Ctrl Pts',(-54.5275217339721,31.4638515574739,
2.59908173516044));
#246027=CARTESIAN_POINT('Ctrl Pts',(-54.4952102564867,31.4452069629852,
2.65878198860283));
#246028=CARTESIAN_POINT('Ctrl Pts',(-54.4342359163065,31.410023123206,2.65878198860283));
#246029=CARTESIAN_POINT('Ctrl Pts',(-54.5715608148709,31.3875306471678,
2.59908193475695));
#246030=CARTESIAN_POINT('Ctrl Pts',(-54.5272862282516,31.3896121658904,
2.6587871532535));
#246031=CARTESIAN_POINT('Ctrl Pts',(-54.4597196360178,31.3658411130327,
2.65878198860283));
#246032=CARTESIAN_POINT('Ctrl Pts',(-54.5905300051366,31.3046029601557,
2.63878778849901));
#246033=CARTESIAN_POINT('Ctrl Pts',(-54.5367961153115,31.3268524737457,
2.69564460180151));
#246034=CARTESIAN_POINT('Ctrl Pts',(-54.4615686025421,31.3125672934291,
2.68180481624904));
#246035=CARTESIAN_POINT('Ctrl Pts',(-54.5809273110397,31.175901474604,2.75443238878657));
#246036=CARTESIAN_POINT('Ctrl Pts',(-54.515857994007,31.2415992967183,2.79268340777087));
#246037=CARTESIAN_POINT('Ctrl Pts',(-54.4295063924931,31.222768219186,2.74885926835632));
#246038=CARTESIAN_POINT('Ctrl Pts',(-54.5540292360081,31.1295364123886,
2.82856655361696));
#246039=CARTESIAN_POINT('Ctrl Pts',(-54.4847364330947,31.2191033458789,
2.85384197230791));
#246040=CARTESIAN_POINT('Ctrl Pts',(-54.396983511837,31.1861426211012,2.79184624278568));
#246041=CARTESIAN_POINT('Ctrl Pts',(-54.514646476914,31.1067982185534,2.90134173516044));
#246042=CARTESIAN_POINT('Ctrl Pts',(-54.4512761425984,31.2174884860864,
2.90163218716412));
#246043=CARTESIAN_POINT('Ctrl Pts',(-54.357602037244,31.1634057161439,2.83404198860283));
#246044=CARTESIAN_POINT('Origin',(-54.4342359163065,31.410023123206,2.53178198860283));
#246045=CARTESIAN_POINT('Origin',(-0.158749999999993,-0.274963065701376,
3.64303198860262));
#246046=CARTESIAN_POINT('Origin',(-52.1234703131948,29.7268821954848,3.64303198860283));
#246047=CARTESIAN_POINT('Origin',(1.12590909550281E-16,1.91494989949198E-13,
2.53178198860262));
#246048=CARTESIAN_POINT('Origin',(-54.4189959163065,31.4364195775134,2.53178198860283));
#246049=CARTESIAN_POINT('Ctrl Pts',(-52.1234703131948,29.7268821954848,
3.77003198860283));
#246050=CARTESIAN_POINT('Ctrl Pts',(-52.0598751873274,29.8370321846009,
3.77003198860283));
#246051=CARTESIAN_POINT('Ctrl Pts',(-52.0599703843396,29.8368672985391,
3.64284187937076));
#246052=CARTESIAN_POINT('Ctrl Pts',(-51.9354481180168,29.6185926664424,
3.77003198860283));
#246053=CARTESIAN_POINT('Ctrl Pts',(-51.8721332876009,29.7286387544935,
3.76980208962903));
#246054=CARTESIAN_POINT('Ctrl Pts',(-51.9096995898738,29.7501084151998,
3.64284193928298));
#246055=CARTESIAN_POINT('Ctrl Pts',(-51.7564527430635,29.5155047636222,
3.65553535416608));
#246056=CARTESIAN_POINT('Ctrl Pts',(-51.6933616226613,29.6254243098818,
3.65520057834604));
#246057=CARTESIAN_POINT('Ctrl Pts',(-51.7666446199951,29.6675155901171,
3.5512791096425));
#246058=CARTESIAN_POINT('Ctrl Pts',(-51.6568155675429,29.4581217525673,
3.47153072139092));
#246059=CARTESIAN_POINT('Ctrl Pts',(-51.5939283753697,29.5680161811089,
3.47122746281603));
#246060=CARTESIAN_POINT('Ctrl Pts',(-51.6870133822662,29.6215404737379,
3.40413045901299));
#246061=CARTESIAN_POINT('Origin',(-51.7503740054945,29.5114749418004,3.4042309748333));
#246062=CARTESIAN_POINT('Ctrl Pts',(-54.1966007261209,31.6576696180583,
2.90134173516045));
#246063=CARTESIAN_POINT('Ctrl Pts',(-54.2607761425984,31.5474441649282,
2.90163218716412));
#246064=CARTESIAN_POINT('Ctrl Pts',(-54.167102037244,31.4933613949858,2.83404198860283));
#246065=CARTESIAN_POINT('Ctrl Pts',(-54.2360018544265,31.6804173066008,
2.82853349835366));
#246066=CARTESIAN_POINT('Ctrl Pts',(-54.2789150989575,31.5756301844106,
2.85381483162275));
#246067=CARTESIAN_POINT('Ctrl Pts',(-54.2065014563932,31.5161086602375,
2.79182701594199));
#246068=CARTESIAN_POINT('Ctrl Pts',(-54.2894509908545,31.6804328064624,
2.75468822073677));
#246069=CARTESIAN_POINT('Ctrl Pts',(-54.3138841827106,31.5911964272961,
2.79286913083857));
#246070=CARTESIAN_POINT('Ctrl Pts',(-54.2543268901841,31.5258675551966,
2.7490076329792));
#246071=CARTESIAN_POINT('Ctrl Pts',(-54.4049648787501,31.6250591602189,
2.639544506404));
#246072=CARTESIAN_POINT('Ctrl Pts',(-54.3976088886511,31.5671393481783,
2.6962768402888));
#246073=CARTESIAN_POINT('Ctrl Pts',(-54.3475791360315,31.5090508246494,
2.68224356036526));
#246074=CARTESIAN_POINT('Ctrl Pts',(-54.4680334478295,31.5668453499338,
2.59908178706341));
#246075=CARTESIAN_POINT('Ctrl Pts',(-54.4477213412886,31.5274226111428,
2.65878704321531));
#246076=CARTESIAN_POINT('Ctrl Pts',(-54.393390646533,31.480726337235,2.65878198860283));
#246077=CARTESIAN_POINT('Ctrl Pts',(-54.5122556166612,31.4902932482907,
2.59908173516044));
#246078=CARTESIAN_POINT('Ctrl Pts',(-54.4799531854481,31.4716329851988,
2.65878198860282));
#246079=CARTESIAN_POINT('Ctrl Pts',(-54.4189959163065,31.4364195775134,
2.65878198860283));
#246080=CARTESIAN_POINT('Origin',(-54.103602037244,31.6033466212664,2.83404198860283));
#246081=CARTESIAN_POINT('Origin',(-51.5960921371858,29.4224002636375,3.11913648167122));
#246082=CARTESIAN_POINT('Origin',(-51.4418102687787,29.3333255853454,2.83404198860282));
#246083=CARTESIAN_POINT('Origin',(-53.9493203812135,31.5142720655985,3.11913648177612));
#246084=CARTESIAN_POINT('Origin',(-53.7950387249981,31.4251975098792,3.40423097483331));
#246085=CARTESIAN_POINT('Ctrl Pts',(-51.3482501200167,29.2799753962461,
2.90134173516043));
#246086=CARTESIAN_POINT('Ctrl Pts',(-51.2854610232003,29.3897042746973,
2.90103711553249));
#246087=CARTESIAN_POINT('Ctrl Pts',(-51.3783102687786,29.443310811626,2.83404198860281));
#246088=CARTESIAN_POINT('Ctrl Pts',(-51.3089010921302,29.2572578385501,
2.8286299174797));
#246089=CARTESIAN_POINT('Ctrl Pts',(-51.2670685993223,29.3615397594617,
2.85314045886478));
#246090=CARTESIAN_POINT('Ctrl Pts',(-51.3389598763136,29.4205918519436,
2.79187960999942));
#246091=CARTESIAN_POINT('Ctrl Pts',(-51.255740761606,29.2572680623748,2.75470625793364));
#246092=CARTESIAN_POINT('Ctrl Pts',(-51.2319924817693,29.3461554108688,
2.79224250381917));
#246093=CARTESIAN_POINT('Ctrl Pts',(-51.2913733902319,29.4109522357566,
2.7490180910829));
#246094=CARTESIAN_POINT('Ctrl Pts',(-51.1410333861056,29.3127910737014,
2.639478683117));
#246095=CARTESIAN_POINT('Ctrl Pts',(-51.1485922293422,29.3705286780144,
2.69595066767927));
#246096=CARTESIAN_POINT('Ctrl Pts',(-51.1987619028145,29.4282055900902,
2.68220539436071));
#246097=CARTESIAN_POINT('Ctrl Pts',(-51.0785202710261,29.3710651187646,
2.59908178585132));
#246098=CARTESIAN_POINT('Ctrl Pts',(-51.0989122516721,29.4103605382571,
2.65877670944931));
#246099=CARTESIAN_POINT('Ctrl Pts',(-51.1533747228768,29.4568175306709,
2.65878198860281));
#246100=CARTESIAN_POINT('Ctrl Pts',(-51.0345602039888,29.4472515437734,
2.59908173516043));
#246101=CARTESIAN_POINT('Ctrl Pts',(-51.0668719738979,29.4658956314766,
2.65878198860281));
#246102=CARTESIAN_POINT('Ctrl Pts',(-51.1278468659049,29.501078514911,2.65878198860281));
#246103=CARTESIAN_POINT('Origin',(-51.1278468659049,29.501078514911,2.53178198860281));
#246104=CARTESIAN_POINT('Ctrl Pts',(-53.4219427993288,31.2097904767605,
3.77003198860284));
#246105=CARTESIAN_POINT('Ctrl Pts',(-53.485537670863,31.0996409281624,3.77003198860284));
#246106=CARTESIAN_POINT('Ctrl Pts',(-53.4854427285637,31.0998053730486,
3.6428423872761));
#246107=CARTESIAN_POINT('Ctrl Pts',(-53.6097387976567,31.3184716867865,
3.77003198860284));
#246108=CARTESIAN_POINT('Ctrl Pts',(-53.6736064794794,31.2082219299895,
3.77025506105862));
#246109=CARTESIAN_POINT('Ctrl Pts',(-53.6357132000306,31.1865640704877,
3.64284210641857));
#246110=CARTESIAN_POINT('Ctrl Pts',(-53.7885186806134,31.4219325588464,
3.65553527987851));
#246111=CARTESIAN_POINT('Ctrl Pts',(-53.8525981958195,31.3115622968595,
3.65585996533086));
#246112=CARTESIAN_POINT('Ctrl Pts',(-53.7787681009843,31.2691568563319,
3.55127902710232));
#246113=CARTESIAN_POINT('Ctrl Pts',(-53.8880358395972,31.4795232016788,
3.47153072139091));
#246114=CARTESIAN_POINT('Ctrl Pts',(-53.9523112232409,31.3691313396262,
3.47182327905207));
#246115=CARTESIAN_POINT('Ctrl Pts',(-53.8583991049521,31.3151318380582,
3.40413028378002));
#246116=CARTESIAN_POINT('Origin',(-53.4219427993288,31.2097904767605,3.64303198860284));
#246117=CARTESIAN_POINT('Origin',(3.61170357355341E-16,1.91606763369042E-13,
2.53178198860262));
#246118=CARTESIAN_POINT('Origin',(-51.1126068659049,29.5274749692184,2.53178198860281));
#246119=CARTESIAN_POINT('Origin',(46.8255917980726,-26.6681506086448,3.64303198860244));
#246120=CARTESIAN_POINT('Origin',(-53.0743345559677,31.009158450368,3.64299466007833));
#246121=CARTESIAN_POINT('Ctrl Pts',(-51.0193480105329,29.4735998357337,
2.59908173516043));
#246122=CARTESIAN_POINT('Ctrl Pts',(-51.0516501490688,29.4922606054645,
2.65878198860282));
#246123=CARTESIAN_POINT('Ctrl Pts',(-51.1126068659049,29.5274749692184,
2.65878198860281));
#246124=CARTESIAN_POINT('Ctrl Pts',(-50.9754987628538,29.549503942697,2.59908193199938));
#246125=CARTESIAN_POINT('Ctrl Pts',(-51.0197013834523,29.5475581014579,
2.65877685806621));
#246126=CARTESIAN_POINT('Ctrl Pts',(-51.0871269269763,29.5715624158005,
2.65878198860281));
#246127=CARTESIAN_POINT('Ctrl Pts',(-50.956202990229,29.6319914129672,2.63872492669836));
#246128=CARTESIAN_POINT('Ctrl Pts',(-51.0098791271091,29.610003803853,2.69532212015288));
#246129=CARTESIAN_POINT('Ctrl Pts',(-51.0848223701588,29.6246193648996,
2.68176836726668));
#246130=CARTESIAN_POINT('Ctrl Pts',(-50.9652607924605,29.760039537519,2.75442176402251));
#246131=CARTESIAN_POINT('Ctrl Pts',(-51.0303675504159,29.6951164119092,
2.79203179920169));
#246132=CARTESIAN_POINT('Ctrl Pts',(-51.1161687394135,29.714061004223,2.74885310748181));
#246133=CARTESIAN_POINT('Ctrl Pts',(-50.9919958361067,29.8061925581053,
2.82866089558436));
#246134=CARTESIAN_POINT('Ctrl Pts',(-51.0613912713661,29.7178148857784,
2.85316563119081));
#246135=CARTESIAN_POINT('Ctrl Pts',(-51.1484765898567,29.7505571803541,
2.79189751796605));
#246136=CARTESIAN_POINT('Ctrl Pts',(-51.031327575341,29.8289013456885,2.90134173516043));
#246137=CARTESIAN_POINT('Ctrl Pts',(-51.0949610232003,29.7196599535392,
2.90103711553249));
#246138=CARTESIAN_POINT('Ctrl Pts',(-51.1878102687787,29.7732664904679,
2.83404198860282));
#246139=CARTESIAN_POINT('Origin',(-51.1243102687787,29.8832517167485,2.83404198860282));
#246140=CARTESIAN_POINT('Origin',(-53.0360596824721,30.9870007553611,3.56647653971802));
#246141=CARTESIAN_POINT('Origin',(-52.9651856060848,30.9460815882867,3.42473028058505));
#246142=CARTESIAN_POINT('Origin',(-51.2785921372026,29.9723263949818,3.11913648168053));
#246143=CARTESIAN_POINT('Origin',(-51.4328740054945,30.0614010732035,3.40423097483331));
#246144=CARTESIAN_POINT('Ctrl Pts',(-52.6794317578289,30.7811015270742,
3.36123028058502));
#246145=CARTESIAN_POINT('Ctrl Pts',(-52.7429317578289,30.6711163007936,
3.36123028058502));
#246146=CARTESIAN_POINT('Ctrl Pts',(-52.7429317578289,30.6711163007936,
3.23423028058502));
#246147=CARTESIAN_POINT('Ctrl Pts',(-52.7575002129176,30.8259039490951,
3.36123028058502));
#246148=CARTESIAN_POINT('Ctrl Pts',(-52.8208099140592,30.7160792752582,
3.36099641108606));
#246149=CARTESIAN_POINT('Ctrl Pts',(-52.8598573673268,30.7386233329124,
3.23423043688387));
#246150=CARTESIAN_POINT('Ctrl Pts',(-52.8313189037795,30.868269596017,3.41054258905305));
#246151=CARTESIAN_POINT('Ctrl Pts',(-52.8948168809878,30.7588072175349,
3.41008815826047));
#246152=CARTESIAN_POINT('Ctrl Pts',(-52.9704188493371,30.802456034313,3.30819867304317));
#246153=CARTESIAN_POINT('Ctrl Pts',(-52.8702215132218,30.8905967158735,
3.48823028058505));
#246154=CARTESIAN_POINT('Ctrl Pts',(-52.9338619179797,30.7813498801531,
3.48794691941621));
#246155=CARTESIAN_POINT('Ctrl Pts',(-53.0286856060847,30.8360963620061,
3.42473028058507));
#246156=CARTESIAN_POINT('Origin',(-52.6794317578289,30.7811015270742,3.23423028058502));
#246157=CARTESIAN_POINT('Ctrl Pts',(-51.3398895692699,30.0070536838157,
3.47153072139093));
#246158=CARTESIAN_POINT('Ctrl Pts',(-51.4036173326911,29.8976445761579,
3.47122746285098));
#246159=CARTESIAN_POINT('Ctrl Pts',(-51.496513229882,29.951496391695,3.40413046676832));
#246160=CARTESIAN_POINT('Ctrl Pts',(-51.4394048060573,30.0646513737723,
3.65553813458008));
#246161=CARTESIAN_POINT('Ctrl Pts',(-51.5030523579633,29.9550530981051,
3.65520336072249));
#246162=CARTESIAN_POINT('Ctrl Pts',(-51.576145673005,29.9974722043279,3.5512813451994));
#246163=CARTESIAN_POINT('Ctrl Pts',(-51.6181806476919,30.1681227811164,
3.77003198860284));
#246164=CARTESIAN_POINT('Ctrl Pts',(-51.6818259279757,30.0582674911775,
3.76980209314012));
#246165=CARTESIAN_POINT('Ctrl Pts',(-51.7192017762845,30.0800656843511,
3.64284195387447));
#246166=CARTESIAN_POINT('Ctrl Pts',(-51.8059703131948,30.276808326888,3.77003198860284));
#246167=CARTESIAN_POINT('Ctrl Pts',(-51.8695654317172,30.1666583504938,
3.77003198860284));
#246168=CARTESIAN_POINT('Ctrl Pts',(-51.869470242061,30.1668232238147,3.64284189403868));
#246169=CARTESIAN_POINT('Origin',(-51.8059703131948,30.276808326888,3.64303198860283));
#246170=CARTESIAN_POINT('Origin',(45.6951875000003,-26.0155113828597,3.23423028058464));
#246171=CARTESIAN_POINT('Origin',(-52.5484816883961,30.7054974692368,3.23423028058502));
#246172=CARTESIAN_POINT('Origin',(45.5181711678734,-25.9133109558552,3.64303198860245));
#246173=CARTESIAN_POINT('Origin',(-52.1535342613176,30.4775331296739,3.64299171721775));
#246174=CARTESIAN_POINT('Ctrl Pts',(-52.3576880233164,30.5960088312567,
3.48823028058501));
#246175=CARTESIAN_POINT('Ctrl Pts',(-52.4219111049558,30.4857749404419,
3.48852004212278));
#246176=CARTESIAN_POINT('Ctrl Pts',(-52.3262277788843,30.4305321463775,
3.424730280585));
#246177=CARTESIAN_POINT('Ctrl Pts',(-52.3967235457371,30.6184089696597,
3.4102800584843));
#246178=CARTESIAN_POINT('Ctrl Pts',(-52.4606806140212,30.5081585269373,
3.41074404220383));
#246179=CARTESIAN_POINT('Ctrl Pts',(-52.384691448504,30.4642861617703,3.30780486244033));
#246180=CARTESIAN_POINT('Ctrl Pts',(-52.4706758922786,30.6608464521622,
3.36123028058502));
#246181=CARTESIAN_POINT('Ctrl Pts',(-52.5342179826647,30.5506153465184,
3.3614646058652));
#246182=CARTESIAN_POINT('Ctrl Pts',(-52.4954499175206,30.5282325936721,
3.23423045308406));
#246183=CARTESIAN_POINT('Ctrl Pts',(-52.5484816883961,30.7054974692368,
3.36123028058502));
#246184=CARTESIAN_POINT('Ctrl Pts',(-52.6119816883961,30.5955122429562,
3.36123028058501));
#246185=CARTESIAN_POINT('Ctrl Pts',(-52.6119816883961,30.5955122429562,
3.23423028058502));
#246186=CARTESIAN_POINT('Origin',(-52.2627277788843,30.5405173726582,3.42473028058501));
#246187=CARTESIAN_POINT('Origin',(-52.1922763809702,30.4998422394563,3.56563113524767));
#246188=CARTESIAN_POINT('Origin',(-56.2428239377265,24.6933715417287,3.56647653909453));
#246189=CARTESIAN_POINT('Origin',(-56.2832472948504,24.7113125977908,3.64299466007575));
#246190=CARTESIAN_POINT('Origin',(-56.1680608984279,24.660084891711,3.424730280585));
#246191=CARTESIAN_POINT('Ctrl Pts',(-56.0673542004327,24.6158705164592,
3.488230280585));
#246192=CARTESIAN_POINT('Ctrl Pts',(-56.0163785451199,24.7315703643334,
3.48794691941616));
#246193=CARTESIAN_POINT('Ctrl Pts',(-56.1164053447573,24.7761051648316,
3.42473028058502));
#246194=CARTESIAN_POINT('Ctrl Pts',(-56.0262864882911,24.597459188332,3.41028005925102));
#246195=CARTESIAN_POINT('Ctrl Pts',(-55.9750519161937,24.7131705636677,
3.40982512230903));
#246196=CARTESIAN_POINT('Ctrl Pts',(-56.0547337128495,24.7486471852365,
3.30780486372868));
#246197=CARTESIAN_POINT('Ctrl Pts',(-55.9484840819677,24.562578485879,3.36123028058498));
#246198=CARTESIAN_POINT('Ctrl Pts',(-55.8968463240337,24.6783511906859,
3.36099721048674));
#246199=CARTESIAN_POINT('Ctrl Pts',(-55.9378977967844,24.69662848393,3.23423045308409));
#246200=CARTESIAN_POINT('Ctrl Pts',(-55.8666273273834,24.525878019167,3.36123028058498));
#246201=CARTESIAN_POINT('Ctrl Pts',(-55.8149717737128,24.6418982922876,
3.36123028058497));
#246202=CARTESIAN_POINT('Ctrl Pts',(-55.8149717737128,24.6418982922876,
3.23423028058498));
#246203=CARTESIAN_POINT('Origin',(-55.8666273273834,24.525878019167,3.23423028058497));
#246204=CARTESIAN_POINT('Origin',(-0.129138884176559,-0.290050682801343,
3.64303198860262));
#246205=CARTESIAN_POINT('Origin',(-56.6498810128383,24.8746050278051,3.64303198860279));
#246206=CARTESIAN_POINT('Origin',(-0.129138884176559,-0.29005068280134,
3.23423028058481));
#246207=CARTESIAN_POINT('Origin',(-55.7284918401499,24.4643761377916,3.23423028058498));
#246208=CARTESIAN_POINT('Ctrl Pts',(-57.1420619865023,25.0931373005744,
3.47153072139088));
#246209=CARTESIAN_POINT('Ctrl Pts',(-57.0905332211012,25.2100238766579,
3.47182327902679));
#246210=CARTESIAN_POINT('Ctrl Pts',(-56.9916465525424,25.1657875015263,
3.40413028959055));
#246211=CARTESIAN_POINT('Ctrl Pts',(-57.0369738651803,25.0464764504226,
3.65553807120975));
#246212=CARTESIAN_POINT('Ctrl Pts',(-56.9853474458572,25.1631918674186,
3.65586275496955));
#246213=CARTESIAN_POINT('Ctrl Pts',(-56.907644805189,25.1283875141304,3.55128126837268));
#246214=CARTESIAN_POINT('Ctrl Pts',(-56.8481865914867,24.9626525995186,
3.7700319886028));
#246215=CARTESIAN_POINT('Ctrl Pts',(-56.7965331449335,25.0791258042764,
3.7702550574856));
#246216=CARTESIAN_POINT('Ctrl Pts',(-56.7567390814047,25.0611999573801,
3.64284211731171));
#246217=CARTESIAN_POINT('Ctrl Pts',(-56.6498810128383,24.8746050278051,
3.7700319886028));
#246218=CARTESIAN_POINT('Ctrl Pts',(-56.5981482881659,24.9907986298337,
3.7700319886028));
#246219=CARTESIAN_POINT('Ctrl Pts',(-56.5982255167266,24.9906251716463,
3.64284239821737));
#246220=CARTESIAN_POINT('Origin',(-57.043449246138,25.0498328948963,3.40423097483326));
#246221=CARTESIAN_POINT('Ctrl Pts',(-55.7284918401499,24.4643761377916,
3.36123028058498));
#246222=CARTESIAN_POINT('Ctrl Pts',(-55.6768362864793,24.5803964109122,
3.36123028058498));
#246223=CARTESIAN_POINT('Ctrl Pts',(-55.6768362864793,24.5803964109122,
3.23423028058498));
#246224=CARTESIAN_POINT('Ctrl Pts',(-55.6463586582055,24.427551097298,3.36123028058498));
#246225=CARTESIAN_POINT('Ctrl Pts',(-55.5945285148498,24.5437506299587,
3.36146538610153));
#246226=CARTESIAN_POINT('Ctrl Pts',(-55.553494790327,24.5254812387363,3.23423043688422));
#246227=CARTESIAN_POINT('Ctrl Pts',(-55.5686962576411,24.3927285408595,
3.41054258693117));
#246228=CARTESIAN_POINT('Ctrl Pts',(-55.5170953257178,24.5092751529588,
3.41100608859789));
#246229=CARTESIAN_POINT('Ctrl Pts',(-55.4368666119039,24.473555028187,3.3081986697083));
#246230=CARTESIAN_POINT('Ctrl Pts',(-55.5277679687684,24.3743766270213,
3.48823028058497));
#246231=CARTESIAN_POINT('Ctrl Pts',(-55.4763362579876,24.4911280468225,
3.48852004212275));
#246232=CARTESIAN_POINT('Ctrl Pts',(-55.3754026508176,24.4461895095988,
3.42473028058497));
#246233=CARTESIAN_POINT('Origin',(-55.4270582044882,24.3301692364781,3.42473028058497));
#246234=CARTESIAN_POINT('Origin',(-57.2061965577146,25.1222926664932,3.11913648178331));
#246235=CARTESIAN_POINT('Origin',(-57.3689438691197,25.1947524379615,2.83404198860278));
#246236=CARTESIAN_POINT('Origin',(-55.3527410366462,24.2970811015512,3.56563113460896));
#246237=CARTESIAN_POINT('Origin',(-55.3119205422646,24.2788510342445,3.64299171721806));
#246238=CARTESIAN_POINT('Ctrl Pts',(-57.517682316389,25.5918112338793,2.5990817351604));
#246239=CARTESIAN_POINT('Ctrl Pts',(-57.4835989537479,25.5766462455175,
2.65878198860279));
#246240=CARTESIAN_POINT('Ctrl Pts',(-57.419280924679,25.5480287005717,2.65878198860279));
#246241=CARTESIAN_POINT('Ctrl Pts',(-57.5535024391259,25.5113050800556,
2.5990819347557));
#246242=CARTESIAN_POINT('Ctrl Pts',(-57.5096879712795,25.518003150502,2.6587871532529));
#246243=CARTESIAN_POINT('Ctrl Pts',(-57.4400067642825,25.5014249500143,
2.65878198860279));
#246244=CARTESIAN_POINT('Ctrl Pts',(-57.5636994104961,25.4268488592817,
2.63878778849897));
#246245=CARTESIAN_POINT('Ctrl Pts',(-57.5125855880052,25.4545932086376,
2.69564460180146));
#246246=CARTESIAN_POINT('Ctrl Pts',(-57.4362769714766,25.4482497003383,
2.68180481624888));
#246247=CARTESIAN_POINT('Ctrl Pts',(-57.5406963524572,25.2998561687912,
2.75443238878654));
#246248=CARTESIAN_POINT('Ctrl Pts',(-57.4828507843378,25.3719956870766,
2.79268340777082));
#246249=CARTESIAN_POINT('Ctrl Pts',(-57.3950038423353,25.3622939683647,
2.7488592683564));
#246250=CARTESIAN_POINT('Ctrl Pts',(-57.5090991591923,25.2565567136861,
2.82856655361693));
#246251=CARTESIAN_POINT('Ctrl Pts',(-57.4495482434205,25.3528760603489,
2.85384197230783));
#246252=CARTESIAN_POINT('Ctrl Pts',(-57.3588307079376,25.3292685758743,
2.79184624278451));
#246253=CARTESIAN_POINT('Ctrl Pts',(-57.4675553545142,25.2380597013429,
2.90134173516042));
#246254=CARTESIAN_POINT('Ctrl Pts',(-57.4161024530845,25.3547675996714,
2.90163218716409));
#246255=CARTESIAN_POINT('Ctrl Pts',(-57.3172883154491,25.3107727110821,
2.83404198860279));
#246256=CARTESIAN_POINT('Origin',(-57.419280924679,25.5480287005717,2.53178198860278));
#246257=CARTESIAN_POINT('Origin',(-0.129138884176559,-0.290050682801343,
3.64303198860262));
#246258=CARTESIAN_POINT('Origin',(-54.945237802683,24.1156489724276,3.64303198860279));
#246259=CARTESIAN_POINT('Origin',(1.20426471881346E-16,1.91510368106146E-13,
2.53178198860262));
#246260=CARTESIAN_POINT('Origin',(-57.4068835917981,25.5758735661207,2.53178198860279));
#246261=CARTESIAN_POINT('Ctrl Pts',(-54.945237802683,24.1156489724276,3.7700319886028));
#246262=CARTESIAN_POINT('Ctrl Pts',(-54.8935048666604,24.2318430491564,
3.7700319886028));
#246263=CARTESIAN_POINT('Ctrl Pts',(-54.8935823068867,24.2316691155602,
3.64284187937053));
#246264=CARTESIAN_POINT('Ctrl Pts',(-54.7469262747044,24.0276063358781,
3.77003198860279));
#246265=CARTESIAN_POINT('Ctrl Pts',(-54.6954612380262,24.143667781871,3.76980208962941));
#246266=CARTESIAN_POINT('Ctrl Pts',(-54.7350659388072,24.1610930816817,
3.64284193928226));
#246267=CARTESIAN_POINT('Ctrl Pts',(-54.5581358350812,23.9437932708499,
3.65553535416599));
#246268=CARTESIAN_POINT('Ctrl Pts',(-54.5068800556916,24.0597054841956,
3.65520057834569));
#246269=CARTESIAN_POINT('Ctrl Pts',(-54.5841613379359,24.0939060248995,
3.55127910964314));
#246270=CARTESIAN_POINT('Ctrl Pts',(-54.4530463244694,23.8971395307767,
3.47153072139089));
#246271=CARTESIAN_POINT('Ctrl Pts',(-54.401990730652,24.0130054476976,3.47122746281599));
#246272=CARTESIAN_POINT('Ctrl Pts',(-54.5001606201972,24.056506495927,3.40413045901284));
#246273=CARTESIAN_POINT('Origin',(-54.5516691663896,23.940420925912,3.40423097483326));
#246274=CARTESIAN_POINT('Ctrl Pts',(-57.20883363247,25.8191582032619,2.90134173516041));
#246275=CARTESIAN_POINT('Ctrl Pts',(-57.2611357920726,25.7028284190332,
2.90163218716408));
#246276=CARTESIAN_POINT('Ctrl Pts',(-57.1623216544372,25.658833530444,2.83404198860279));
#246277=CARTESIAN_POINT('Ctrl Pts',(-57.2503966981986,25.837662738193,2.82853349835371));
#246278=CARTESIAN_POINT('Ctrl Pts',(-57.2821216226326,25.7289639953178,
2.85381483162252));
#246279=CARTESIAN_POINT('Ctrl Pts',(-57.203882976126,25.6773378230591,2.79182701594196));
#246280=CARTESIAN_POINT('Ctrl Pts',(-57.3035546548414,25.8320911970514,
2.75468822073663));
#246281=CARTESIAN_POINT('Ctrl Pts',(-57.3185262575346,25.74078970011,2.79286913083853));
#246282=CARTESIAN_POINT('Ctrl Pts',(-57.2524664994803,25.6820441386716,
2.74900763297921));
#246283=CARTESIAN_POINT('Ctrl Pts',(-57.4126476234251,25.7649464042484,
2.63954450640406));
#246284=CARTESIAN_POINT('Ctrl Pts',(-57.3992776612638,25.7081127933389,
2.69627684028873));
#246285=CARTESIAN_POINT('Ctrl Pts',(-57.3434500727659,25.6555720179788,
2.68224356036517));
#246286=CARTESIAN_POINT('Ctrl Pts',(-57.4692856961543,25.7004590347004,
2.59908178706325));
#246287=CARTESIAN_POINT('Ctrl Pts',(-57.4449640631538,25.6633754510796,
2.65878704321563));
#246288=CARTESIAN_POINT('Ctrl Pts',(-57.3860499078785,25.622614088278,2.65878198860279));
#246289=CARTESIAN_POINT('Ctrl Pts',(-57.5052637377733,25.6197038181296,
2.5990817351604));
#246290=CARTESIAN_POINT('Ctrl Pts',(-57.471187734033,25.604522301406,2.65878198860278));
#246291=CARTESIAN_POINT('Ctrl Pts',(-57.4068835917981,25.5758735661207,
2.65878198860279));
#246292=CARTESIAN_POINT('Origin',(-57.1106661007666,25.7748538035646,2.83404198860279));
#246293=CARTESIAN_POINT('Origin',(-54.3889216310782,23.8679610547562,3.11913648166977));
#246294=CARTESIAN_POINT('Origin',(-54.2261740956467,23.7955011834907,2.83404198860278));
#246295=CARTESIAN_POINT('Origin',(-56.9479187893697,25.7023940320473,3.11913648177554));
#246296=CARTESIAN_POINT('Origin',(-56.7851714777849,25.6299342604994,3.40423097483327));
#246297=CARTESIAN_POINT('Ctrl Pts',(-54.1275498658875,23.7522229508827,
2.90134173516039));
#246298=CARTESIAN_POINT('Ctrl Pts',(-54.0765745253537,23.8679139708567,
2.90103711553245));
#246299=CARTESIAN_POINT('Ctrl Pts',(-54.1745185419761,23.9115214566113,
2.83404198860278));
#246300=CARTESIAN_POINT('Ctrl Pts',(-54.0860417646975,23.7337429357612,
2.8286299174797));
#246301=CARTESIAN_POINT('Ctrl Pts',(-54.0553388636011,23.8418262755866,
2.85314045886488));
#246302=CARTESIAN_POINT('Ctrl Pts',(-54.1330089371355,23.8930401898205,
2.79187960999932));
#246303=CARTESIAN_POINT('Ctrl Pts',(-54.033173720707,23.7393098712348,2.75470625793354));
#246304=CARTESIAN_POINT('Ctrl Pts',(-54.0188467943743,23.8301926567297,
2.79224250381919));
#246305=CARTESIAN_POINT('Ctrl Pts',(-54.0846755205375,23.8884275227223,
2.74901809108279));
#246306=CARTESIAN_POINT('Ctrl Pts',(-53.9248984592617,23.8065189073823,
2.63947868311703));
#246307=CARTESIAN_POINT('Ctrl Pts',(-53.9384511174157,23.8631501047901,
2.69595066767925));
#246308=CARTESIAN_POINT('Ctrl Pts',(-53.9943748351524,23.9152668978359,
2.68220539436073));
#246309=CARTESIAN_POINT('Ctrl Pts',(-53.8688190939458,23.8710081209824,
2.59908178585034));
#246310=CARTESIAN_POINT('Ctrl Pts',(-53.8932068550001,23.9079567336549,
2.65877670944961));
#246311=CARTESIAN_POINT('Ctrl Pts',(-53.9522270531151,23.9484663513832,
2.65878198860278));
#246312=CARTESIAN_POINT('Ctrl Pts',(-53.8330634946839,23.9513722670364,
2.59908173516039));
#246313=CARTESIAN_POINT('Ctrl Pts',(-53.8671470951732,23.9665367208223,
2.65878198860277));
#246314=CARTESIAN_POINT('Ctrl Pts',(-53.9314655730806,23.9951532569806,
2.65878198860278));
#246315=CARTESIAN_POINT('Origin',(-53.9314655730806,23.9951532569806,2.53178198860278));
#246316=CARTESIAN_POINT('Ctrl Pts',(-56.3916032444852,25.4547063934082,
3.7700319886028));
#246317=CARTESIAN_POINT('Ctrl Pts',(-56.4433359736143,25.3385127813696,
3.7700319886028));
#246318=CARTESIAN_POINT('Ctrl Pts',(-56.4432587405903,25.3386862495819,
3.64284238727646));
#246319=CARTESIAN_POINT('Ctrl Pts',(-56.5897307565553,25.5431622092801,
3.7700319886028));
#246320=CARTESIAN_POINT('Ctrl Pts',(-56.6417243268817,25.4268404215571,
3.77025506105722));
#246321=CARTESIAN_POINT('Ctrl Pts',(-56.6017747680111,25.4092621323422,
3.64284210641916));
#246322=CARTESIAN_POINT('Ctrl Pts',(-56.7783458705719,25.627368725429,3.65553527987848));
#246323=CARTESIAN_POINT('Ctrl Pts',(-56.83053751761,25.5109049500325,3.65585996533094));
#246324=CARTESIAN_POINT('Ctrl Pts',(-56.752679296228,25.4764491573031,3.55127902710191));
#246325=CARTESIAN_POINT('Ctrl Pts',(-56.8833377255396,25.6742415049979,
3.47153072139089));
#246326=CARTESIAN_POINT('Ctrl Pts',(-56.9357219102086,25.5577357740382,
3.47182327905205));
#246327=CARTESIAN_POINT('Ctrl Pts',(-56.8366797674144,25.5138485767966,
3.40413028378021));
#246328=CARTESIAN_POINT('Origin',(-56.3916032444852,25.4547063934082,3.6430319886028));
#246329=CARTESIAN_POINT('Origin',(3.58382961824622E-16,1.91601292797291E-13,
2.53178198860262));
#246330=CARTESIAN_POINT('Origin',(-53.9190682401996,24.0229981225296,2.53178198860278));
#246331=CARTESIAN_POINT('Origin',(52.0578415156897,-22.8300973196044,3.64303198860247));
#246332=CARTESIAN_POINT('Origin',(-56.0249274780513,25.2915084057492,3.64299466007644));
#246333=CARTESIAN_POINT('Ctrl Pts',(-53.8206887816837,23.9791663275012,
2.59908173516039));
#246334=CARTESIAN_POINT('Ctrl Pts',(-53.8547645473082,23.9943483786816,
2.65878198860278));
#246335=CARTESIAN_POINT('Ctrl Pts',(-53.9190682401996,24.0229981225296,
2.65878198860278));
#246336=CARTESIAN_POINT('Ctrl Pts',(-53.7850138844278,24.0592381183001,
2.59908193199912));
#246337=CARTESIAN_POINT('Ctrl Pts',(-53.8287709626499,24.052682504579,2.65877685806659));
#246338=CARTESIAN_POINT('Ctrl Pts',(-53.8983362760843,24.0695074323274,
2.65878198860278));
#246339=CARTESIAN_POINT('Ctrl Pts',(-53.7744461045708,24.143290671037,2.63872492669814));
#246340=CARTESIAN_POINT('Ctrl Pts',(-53.8255298669648,24.1158128282435,
2.69532212015291));
#246341=CARTESIAN_POINT('Ctrl Pts',(-53.9015903052238,24.1225146216896,
2.68176836726646));
#246342=CARTESIAN_POINT('Ctrl Pts',(-53.7968389608977,24.2696905364172,
2.75442176402266));
#246343=CARTESIAN_POINT('Ctrl Pts',(-53.8548027426705,24.1983175571256,
2.79203179920153));
#246344=CARTESIAN_POINT('Ctrl Pts',(-53.9421141528989,24.2081897025477,
2.74885310748195));
#246345=CARTESIAN_POINT('Ctrl Pts',(-53.8282518514941,24.3127961529002,
2.82866089558418));
#246346=CARTESIAN_POINT('Ctrl Pts',(-53.8880291490212,24.2176488245029,
2.85316563119191));
#246347=CARTESIAN_POINT('Ctrl Pts',(-53.9780599067629,24.2411088588486,
2.79189751796559));
#246348=CARTESIAN_POINT('Ctrl Pts',(-53.8697418420146,24.3312692531087,
2.9013417351604));
#246349=CARTESIAN_POINT('Ctrl Pts',(-53.9216078643418,24.2159747902186,
2.90103711553245));
#246350=CARTESIAN_POINT('Ctrl Pts',(-54.0195518809642,24.2595822759732,
2.83404198860278));
#246351=CARTESIAN_POINT('Origin',(-53.9678963272936,24.3756025490938,2.83404198860278));
#246352=CARTESIAN_POINT('Origin',(-55.9845461685076,25.2734729066172,3.56647653971902));
#246353=CARTESIAN_POINT('Origin',(-55.9097831300748,25.240186257314,3.42473028058502));
#246354=CARTESIAN_POINT('Origin',(-54.1306438627318,24.4480624203028,3.11913648168032));
#246355=CARTESIAN_POINT('Origin',(-54.2933913980365,24.520522291515,3.40423097483327));
#246356=CARTESIAN_POINT('Ctrl Pts',(-55.6083495590303,25.10597938477,3.36123028058498));
#246357=CARTESIAN_POINT('Ctrl Pts',(-55.6600051127009,24.9899591116494,
3.36123028058499));
#246358=CARTESIAN_POINT('Ctrl Pts',(-55.6600051127009,24.9899591116494,
3.23423028058498));
#246359=CARTESIAN_POINT('Ctrl Pts',(-55.6906734752783,25.1423759987947,
3.36123028058498));
#246360=CARTESIAN_POINT('Ctrl Pts',(-55.7421565548659,25.0265352902406,
3.36099641108368));
#246361=CARTESIAN_POINT('Ctrl Pts',(-55.7833465978035,25.0448742789056,
3.23423043688348));
#246362=CARTESIAN_POINT('Ctrl Pts',(-55.768516195595,25.1767934079559,3.410542589053));
#246363=CARTESIAN_POINT('Ctrl Pts',(-55.820224390035,25.061293329859,3.41008815826136));
#246364=CARTESIAN_POINT('Ctrl Pts',(-55.8999747466295,25.0968004762774,
3.30819867304359));
#246365=CARTESIAN_POINT('Ctrl Pts',(-55.8095395120008,25.19493178753,3.488230280585));
#246366=CARTESIAN_POINT('Ctrl Pts',(-55.861411884108,25.0796311836952,3.48794691941616));
#246367=CARTESIAN_POINT('Ctrl Pts',(-55.9614386837454,25.1241659841934,
3.42473028058501));
#246368=CARTESIAN_POINT('Origin',(-55.6083495590303,25.10597938477,3.23423028058498));
#246369=CARTESIAN_POINT('Ctrl Pts',(-54.1952354911873,24.4761921430391,
3.47153072139088));
#246370=CARTESIAN_POINT('Ctrl Pts',(-54.2471777813618,24.3607210247425,
3.47122746285093));
#246371=CARTESIAN_POINT('Ctrl Pts',(-54.3451938326304,24.4045675690227,
3.40413046676807));
#246372=CARTESIAN_POINT('Ctrl Pts',(-54.3002261711157,24.5230721320469,
3.65553813458001));
#246373=CARTESIAN_POINT('Ctrl Pts',(-54.3520689157403,24.4074212664128,
3.65520336072174));
#246374=CARTESIAN_POINT('Ctrl Pts',(-54.4291958219382,24.4419676644368,
3.55128134519984));
#246375=CARTESIAN_POINT('Ctrl Pts',(-54.4888383671851,24.6072895482019,
3.7700319886028));
#246376=CARTESIAN_POINT('Ctrl Pts',(-54.5406519873247,24.491383313692,3.76980209314061));
#246377=CARTESIAN_POINT('Ctrl Pts',(-54.5801016184612,24.5091552540989,
3.64284195387371));
#246378=CARTESIAN_POINT('Ctrl Pts',(-54.6869600343299,24.6957503380306,
3.7700319886028));
#246379=CARTESIAN_POINT('Ctrl Pts',(-54.7386929643777,24.5795562747215,
3.7700319886028));
#246380=CARTESIAN_POINT('Ctrl Pts',(-54.7386155301351,24.5797301948779,
3.64284189403826));
#246381=CARTESIAN_POINT('Origin',(-54.6869600343299,24.6957503380306,3.64303198860279));
#246382=CARTESIAN_POINT('Origin',(50.7999799080417,-22.2700612497312,3.23423028058466));
#246383=CARTESIAN_POINT('Origin',(-55.4702140717968,25.0444775033946,3.23423028058498));
#246384=CARTESIAN_POINT('Origin',(50.603004322856,-22.1823620689011,3.64303198860248));
#246385=CARTESIAN_POINT('Origin',(-55.0536014459535,24.8590452239602,3.64299171721763));
#246386=CARTESIAN_POINT('Ctrl Pts',(-55.2690209153042,24.9555320242414,
3.48823028058497));
#246387=CARTESIAN_POINT('Ctrl Pts',(-55.3213695969757,24.8391888661843,
3.48852004212275));
#246388=CARTESIAN_POINT('Ctrl Pts',(-55.2204359898058,24.7942503289606,
3.42473028058497));
#246389=CARTESIAN_POINT('Ctrl Pts',(-55.3101840490931,24.9737291291706,
3.41028005848422));
#246390=CARTESIAN_POINT('Ctrl Pts',(-55.3622664445104,24.8573973158465,
3.4107440422034));
#246391=CARTESIAN_POINT('Ctrl Pts',(-55.2821076446828,24.8217083187823,
3.30780486244012));
#246392=CARTESIAN_POINT('Ctrl Pts',(-55.3881672017731,25.0082040095652,
3.36123028058498));
#246393=CARTESIAN_POINT('Ctrl Pts',(-55.4398389138642,24.8919348043908,
3.36146460586493));
#246394=CARTESIAN_POINT('Ctrl Pts',(-55.3989435894779,24.8737270328802,
3.23423045308367));
#246395=CARTESIAN_POINT('Ctrl Pts',(-55.4702140717968,25.0444775033946,
3.36123028058498));
#246396=CARTESIAN_POINT('Ctrl Pts',(-55.5218696254674,24.928457230274,3.36123028058498));
#246397=CARTESIAN_POINT('Ctrl Pts',(-55.5218696254674,24.928457230274,3.23423028058498));
#246398=CARTESIAN_POINT('Origin',(-55.1687804361351,24.9102706020812,3.42473028058497));
#246399=CARTESIAN_POINT('Origin',(-55.0944632691843,24.8771824678739,3.56563113524807));
#246400=CARTESIAN_POINT('Origin',(-58.515880043567,18.6791227126687,3.56647653909402));
#246401=CARTESIAN_POINT('Origin',(-58.5579573083296,18.6927400943494,3.64299466007494));
#246402=CARTESIAN_POINT('Origin',(-58.4380471616456,18.6538332760103,3.42473028058495));
#246403=CARTESIAN_POINT('Ctrl Pts',(-58.3332704847797,18.6203878281146,
3.48823028058495));
#246404=CARTESIAN_POINT('Ctrl Pts',(-58.2946680067389,18.7407822670301,
3.48794691941612));
#246405=CARTESIAN_POINT('Ctrl Pts',(-58.3988020033599,18.7746174535798,
3.42473028058497));
#246406=CARTESIAN_POINT('Ctrl Pts',(-58.2905032380262,18.6063701040096,
3.41028005925101));
#246407=CARTESIAN_POINT('Ctrl Pts',(-58.2516444665222,18.7268030714108,
3.40982512231007));
#246408=CARTESIAN_POINT('Ctrl Pts',(-58.3345980746907,18.7537563325796,
3.30780486372936));
#246409=CARTESIAN_POINT('Ctrl Pts',(-58.2094810152003,18.5798130476651,
3.36123028058494));
#246410=CARTESIAN_POINT('Ctrl Pts',(-58.1702276772291,18.7003491529649,
3.36099721048529));
#246411=CARTESIAN_POINT('Ctrl Pts',(-58.2129647630938,18.7142352739237,
3.23423045308396));
#246412=CARTESIAN_POINT('Ctrl Pts',(-58.1242364370958,18.5518699907149,
3.36123028058493));
#246413=CARTESIAN_POINT('Ctrl Pts',(-58.0849912788101,18.6726541682844,
3.36123028058493));
#246414=CARTESIAN_POINT('Ctrl Pts',(-58.0849912788101,18.6726541682844,
3.23423028058494));
#246415=CARTESIAN_POINT('Origin',(-58.1242364370958,18.5518699907149,3.23423028058493));
#246416=CARTESIAN_POINT('Origin',(-0.0981128957140385,-0.301960443923528,
3.64303198860262));
#246417=CARTESIAN_POINT('Origin',(-58.9396512752214,18.8168143322225,3.64303198860275));
#246418=CARTESIAN_POINT('Origin',(-0.0981128957140384,-0.301960443923525,
3.23423028058481));
#246419=CARTESIAN_POINT('Origin',(-57.9804289733665,18.505144113284,3.23423028058494));
#246420=CARTESIAN_POINT('Ctrl Pts',(-59.4519788726609,18.9827025415095,
3.47153072139084));
#246421=CARTESIAN_POINT('Ctrl Pts',(-59.4129503614028,19.1043350233604,
3.47182327902675));
#246422=CARTESIAN_POINT('Ctrl Pts',(-59.3099814440482,19.0706774512227,
3.40413028959061));
#246423=CARTESIAN_POINT('Ctrl Pts',(-59.3425890481021,18.9472820042059,
3.6555380712097));
#246424=CARTESIAN_POINT('Ctrl Pts',(-59.3034455268834,19.068754472209,3.65586275497007));
#246425=CARTESIAN_POINT('Ctrl Pts',(-59.2225305038472,19.0422629184336,
3.55128126837305));
#246426=CARTESIAN_POINT('Ctrl Pts',(-59.1460739925265,18.8836509927323,
3.77003198860275));
#246427=CARTESIAN_POINT('Ctrl Pts',(-59.1068782740642,19.0048854004787,
3.77025505748436));
#246428=CARTESIAN_POINT('Ctrl Pts',(-59.0654284453496,18.9912173655546,
3.64284211731149));
#246429=CARTESIAN_POINT('Ctrl Pts',(-58.9396512752214,18.8168143322225,
3.77003198860276));
#246430=CARTESIAN_POINT('Ctrl Pts',(-58.9003474864893,18.9377789557521,
3.77003198860276));
#246431=CARTESIAN_POINT('Ctrl Pts',(-58.900406160666,18.9375983752043,3.64284239821752));
#246432=CARTESIAN_POINT('Origin',(-59.3493798002281,18.9499432001056,3.40423097483323));
#246433=CARTESIAN_POINT('Ctrl Pts',(-57.9804289733665,18.505144113284,3.36123028058493));
#246434=CARTESIAN_POINT('Ctrl Pts',(-57.9411838150808,18.6259282908535,
3.36123028058494));
#246435=CARTESIAN_POINT('Ctrl Pts',(-57.9411838150808,18.6259282908535,
3.23423028058494));
#246436=CARTESIAN_POINT('Ctrl Pts',(-57.8948964606932,18.4771060595091,
3.36123028058493));
#246437=CARTESIAN_POINT('Ctrl Pts',(-57.8554964068695,18.5980867642079,
3.36146538610022));
#246438=CARTESIAN_POINT('Ctrl Pts',(-57.8127777979929,18.5842066467868,
3.23423043688421));
#246439=CARTESIAN_POINT('Ctrl Pts',(-57.8140195545743,18.4505921960606,
3.41054258693111));
#246440=CARTESIAN_POINT('Ctrl Pts',(-57.774883736214,18.5718941197416,3.41100608859805));
#246441=CARTESIAN_POINT('Ctrl Pts',(-57.6913607539405,18.5447558577158,
3.30819866970792));
#246442=CARTESIAN_POINT('Ctrl Pts',(-57.7713971777988,18.4366189870671,
3.48823028058494));
#246443=CARTESIAN_POINT('Ctrl Pts',(-57.7324510618071,18.5581069080659,
3.48852004212272));
#246444=CARTESIAN_POINT('Ctrl Pts',(-57.6273730232606,18.5239649837006,
3.42473028058494));
#246445=CARTESIAN_POINT('Origin',(-57.6666181815462,18.4031808061312,3.42473028058492));
#246446=CARTESIAN_POINT('Origin',(-59.5188096735787,19.0049943031105,3.11913648178394));
#246447=CARTESIAN_POINT('Origin',(-59.6882395467421,19.0600454060085,2.83404198860275));
#246448=CARTESIAN_POINT('Origin',(-57.5892494790288,18.3780421908176,3.56563113460855));
#246449=CARTESIAN_POINT('Origin',(-57.5467470426661,18.3641788932749,3.64299171721772));
#246450=CARTESIAN_POINT('Ctrl Pts',(-59.8776671349986,19.4393816709755,
2.59908173516036));
#246451=CARTESIAN_POINT('Ctrl Pts',(-59.8421853116553,19.4278624395265,
2.65878198860274));
#246452=CARTESIAN_POINT('Ctrl Pts',(-59.7752282754838,19.4061247292252,
2.65878198860274));
#246453=CARTESIAN_POINT('Ctrl Pts',(-59.9048758468121,19.3555723159024,
2.59908193475616));
#246454=CARTESIAN_POINT('Ctrl Pts',(-59.8620015382112,19.3668135526098,
2.65878715325449));
#246455=CARTESIAN_POINT('Ctrl Pts',(-59.790969158339,19.3576098387254,2.65878198860274));
#246456=CARTESIAN_POINT('Ctrl Pts',(-59.9061888791359,19.2705128813948,
2.63878778849885));
#246457=CARTESIAN_POINT('Ctrl Pts',(-59.8582551377161,19.3034480936186,
2.69564460180143));
#246458=CARTESIAN_POINT('Ctrl Pts',(-59.7817014705988,19.3051157581418,
2.6818048162491));
#246459=CARTESIAN_POINT('Ctrl Pts',(-59.8700374834723,19.1466203444582,
2.75443238878656));
#246460=CARTESIAN_POINT('Ctrl Pts',(-59.8200494324138,19.2244111832569,
2.79268340777083));
#246461=CARTESIAN_POINT('Ctrl Pts',(-59.7316696194034,19.223945117425,2.74885926835608));
#246462=CARTESIAN_POINT('Ctrl Pts',(-59.834087357436,19.1068608943533,2.82856655361682));
#246463=CARTESIAN_POINT('Ctrl Pts',(-59.7849307811037,19.2088773592683,
2.85384197230915));
#246464=CARTESIAN_POINT('Ctrl Pts',(-59.6922425516974,19.1948817636409,
2.79184624278575));
#246465=CARTESIAN_POINT('Ctrl Pts',(-59.7908376697913,19.092807720641,2.90134173516036));
#246466=CARTESIAN_POINT('Ctrl Pts',(-59.7518659300027,19.2142545736082,
2.90163218716404));
#246467=CARTESIAN_POINT('Ctrl Pts',(-59.6489943884565,19.180829583578,2.83404198860275));
#246468=CARTESIAN_POINT('Origin',(-59.7752282754838,19.4061247292252,2.53178198860274));
#246469=CARTESIAN_POINT('Origin',(-0.0981128957140385,-0.301960443923528,
3.64303198860262));
#246470=CARTESIAN_POINT('Origin',(-57.1650137687748,18.2401996527044,3.64303198860275));
#246471=CARTESIAN_POINT('Origin',(1.26611655068502E-16,1.9152648105923E-13,
2.53178198860262));
#246472=CARTESIAN_POINT('Origin',(-59.7658094374952,19.4351129318419,2.53178198860275));
#246473=CARTESIAN_POINT('Ctrl Pts',(-57.1650137687748,18.2401996527044,
3.77003198860275));
#246474=CARTESIAN_POINT('Ctrl Pts',(-57.1257098194699,18.3611647704261,
3.77003198860276));
#246475=CARTESIAN_POINT('Ctrl Pts',(-57.1257686544591,18.3609836949485,
3.64284187937046));
#246476=CARTESIAN_POINT('Ctrl Pts',(-56.9585856505954,18.1733685221988,
3.77003198860275));
#246477=CARTESIAN_POINT('Ctrl Pts',(-56.9195342693643,18.294173732641,3.76980208962824));
#246478=CARTESIAN_POINT('Ctrl Pts',(-56.960743451265,18.3073637563262,3.64284193928231));
#246479=CARTESIAN_POINT('Ctrl Pts',(-56.7620685738644,18.1097485684446,
3.65553535416594));
#246480=CARTESIAN_POINT('Ctrl Pts',(-56.7232097045379,18.2303834904073,
3.65520057834524));
#246481=CARTESIAN_POINT('Ctrl Pts',(-56.8036425617896,18.2563185833,3.55127910964302));
#246482=CARTESIAN_POINT('Ctrl Pts',(-56.6526781108325,18.074335247489,3.47153072139085));
#246483=CARTESIAN_POINT('Ctrl Pts',(-56.6140134911408,18.1949032015568,
3.47122746281596));
#246484=CARTESIAN_POINT('Ctrl Pts',(-56.7161926934815,18.227904398799,3.4041304590128));
#246485=CARTESIAN_POINT('Origin',(-56.7552848242271,18.1070706485041,3.40423097483322));
#246486=CARTESIAN_POINT('Ctrl Pts',(-59.5942745858237,19.6977666881844,
2.90134173516036));
#246487=CARTESIAN_POINT('Ctrl Pts',(-59.6341304551458,19.5766071063167,
2.90163218716403));
#246488=CARTESIAN_POINT('Ctrl Pts',(-59.5312589135996,19.5431821162865,
2.83404198860274));
#246489=CARTESIAN_POINT('Ctrl Pts',(-59.6375442153294,19.7118253299471,
2.82853349835361));
#246490=CARTESIAN_POINT('Ctrl Pts',(-59.6577332347577,19.6004058925602,
2.85381483162321));
#246491=CARTESIAN_POINT('Ctrl Pts',(-59.5745267832912,19.5572406993633,
2.79182701594235));
#246492=CARTESIAN_POINT('Ctrl Pts',(-59.6898285824899,19.7007277907733,
2.75468822073662));
#246493=CARTESIAN_POINT('Ctrl Pts',(-59.6951745640078,19.6083614943631,
2.79286913083837));
#246494=CARTESIAN_POINT('Ctrl Pts',(-59.6233361049588,19.5568428722498,
2.74900763297926));
#246495=CARTESIAN_POINT('Ctrl Pts',(-59.7913053863691,19.622547503811,2.63954450640398));
#246496=CARTESIAN_POINT('Ctrl Pts',(-59.7720679362491,19.5674227749672,
2.69627684028876));
#246497=CARTESIAN_POINT('Ctrl Pts',(-59.7110541706153,19.5210053955059,
2.68224356036503));
#246498=CARTESIAN_POINT('Ctrl Pts',(-59.8408924241701,19.5524931121162,
2.59908178706402));
#246499=CARTESIAN_POINT('Ctrl Pts',(-59.8128277376111,19.5181549791681,
2.65878704321515));
#246500=CARTESIAN_POINT('Ctrl Pts',(-59.7499755976262,19.4837751174916,
2.65878198860274));
#246501=CARTESIAN_POINT('Ctrl Pts',(-59.8682321556243,19.4684195516695,
2.59908173516036));
#246502=CARTESIAN_POINT('Ctrl Pts',(-59.8327559231847,19.4568831131882,
2.65878198860274));
#246503=CARTESIAN_POINT('Ctrl Pts',(-59.7658094374952,19.4351129318419,
2.65878198860274));
#246504=CARTESIAN_POINT('Origin',(-59.492013755314,19.663966293856,2.83404198860274));
#246505=CARTESIAN_POINT('Origin',(-56.5858547179581,18.0520194698739,3.11913648167164));
#246506=CARTESIAN_POINT('Origin',(-56.4164246115664,17.996968291141,2.83404198860274));
#246507=CARTESIAN_POINT('Origin',(-59.3225838821509,19.6089151909108,3.119136481775));
#246508=CARTESIAN_POINT('Origin',(-59.1531540088,19.5538640879531,3.40423097483322));
#246509=CARTESIAN_POINT('Ctrl Pts',(-56.3138168485096,17.9642361803971,
2.90134173516035));
#246510=CARTESIAN_POINT('Ctrl Pts',(-56.2752137607567,18.0846218068693,
2.90103711553241));
#246511=CARTESIAN_POINT('Ctrl Pts',(-56.3771794532808,18.1177524687105,
2.83404198860273));
#246512=CARTESIAN_POINT('Ctrl Pts',(-56.2706044454592,17.9501961787628,
2.82862991747976));
#246513=CARTESIAN_POINT('Ctrl Pts',(-56.2513675234854,18.0608967538129,
2.85314045886472));
#246514=CARTESIAN_POINT('Ctrl Pts',(-56.3339654239818,18.1037113794377,
2.79187960999963));
#246515=CARTESIAN_POINT('Ctrl Pts',(-56.2186079213554,17.9612588333756,
2.75470625793333));
#246516=CARTESIAN_POINT('Ctrl Pts',(-56.2138593173287,18.0531413250551,
2.79224250381896));
#246517=CARTESIAN_POINT('Ctrl Pts',(-56.2854146278934,18.1041761987738,
2.74901809108272));
#246518=CARTESIAN_POINT('Ctrl Pts',(-56.1179510603878,18.0394175380795,
2.63947868311715));
#246519=CARTESIAN_POINT('Ctrl Pts',(-56.1373490477009,18.0943218653327,
2.69595066767932));
#246520=CARTESIAN_POINT('Ctrl Pts',(-56.1984140977478,18.1403075368578,
2.68220539436072));
#246521=CARTESIAN_POINT('Ctrl Pts',(-56.0689198620979,18.1094153628977,
2.59908178585092));
#246522=CARTESIAN_POINT('Ctrl Pts',(-56.0970362061497,18.1436123520191,
2.65877670944927));
#246523=CARTESIAN_POINT('Ctrl Pts',(-56.1599674935319,18.1777307632118,
2.65878198860274));
#246524=CARTESIAN_POINT('Ctrl Pts',(-56.0417604764384,18.1930767435948,
2.59908173516036));
#246525=CARTESIAN_POINT('Ctrl Pts',(-56.0772424804485,18.2045954185344,
2.65878198860274));
#246526=CARTESIAN_POINT('Ctrl Pts',(-56.1441998575528,18.2263320786581,
2.65878198860274));
#246527=CARTESIAN_POINT('Origin',(-56.1441998575528,18.2263320786581,2.53178198860275));
#246528=CARTESIAN_POINT('Ctrl Pts',(-58.7434254837933,19.4207352200699,
3.77003198860276));
#246529=CARTESIAN_POINT('Ctrl Pts',(-58.7827292759115,19.2997705861193,
3.77003198860276));
#246530=CARTESIAN_POINT('Ctrl Pts',(-58.7826705983437,19.2999511771037,
3.64284238727657));
#246531=CARTESIAN_POINT('Ctrl Pts',(-58.9497137831219,19.4879965013601,
3.77003198860276));
#246532=CARTESIAN_POINT('Ctrl Pts',(-58.9892635895159,19.3668771285532,
3.77025506105737));
#246533=CARTESIAN_POINT('Ctrl Pts',(-58.9476954469502,19.3535710010446,
3.64284210641904));
#246534=CARTESIAN_POINT('Ctrl Pts',(-59.1460976215386,19.5520260773866,
3.65553527987843));
#246535=CARTESIAN_POINT('Ctrl Pts',(-59.1858295778038,19.4307447900779,
3.6558599653305));
#246536=CARTESIAN_POINT('Ctrl Pts',(-59.1047962608408,19.4046161500175,
3.55127902710187));
#246537=CARTESIAN_POINT('Ctrl Pts',(-59.2554138597572,19.5876674457077,
3.47153072139085));
#246538=CARTESIAN_POINT('Ctrl Pts',(-59.2953329133625,19.4663243070095,
3.47182327905201));
#246539=CARTESIAN_POINT('Ctrl Pts',(-59.1922458725048,19.4330302514113,
3.40413028378025));
#246540=CARTESIAN_POINT('Origin',(-58.7434254837933,19.4207352200699,3.64303198860276));
#246541=CARTESIAN_POINT('Origin',(3.56182666396657E-16,1.91595560831732E-13,
2.53178198860262));
#246542=CARTESIAN_POINT('Origin',(-56.1347810195643,18.2553202812748,2.53178198860275));
#246543=CARTESIAN_POINT('Origin',(56.3788528200609,-17.9847604760577,3.64303198860251));
#246544=CARTESIAN_POINT('Origin',(-58.3616995707159,19.2967593024454,3.64299466007577));
#246545=CARTESIAN_POINT('Ctrl Pts',(-56.0323588238392,18.2220120550216,
2.59908173516036));
#246546=CARTESIAN_POINT('Ctrl Pts',(-56.0678348753334,18.2335490499217,
2.65878198860274));
#246547=CARTESIAN_POINT('Ctrl Pts',(-56.1347810195643,18.2553202812748,
2.65878198860274));
#246548=CARTESIAN_POINT('Ctrl Pts',(-56.0052491386462,18.3053742463597,
2.5990819319987));
#246549=CARTESIAN_POINT('Ctrl Pts',(-56.0480812627873,18.2942806848323,
2.65877685806566));
#246550=CARTESIAN_POINT('Ctrl Pts',(-56.119024173998,18.3037418885564,2.65878198860274));
#246551=CARTESIAN_POINT('Ctrl Pts',(-56.0035251343646,18.3900709842069,
2.63872492669813));
#246552=CARTESIAN_POINT('Ctrl Pts',(-56.0514568378816,18.3574039607309,
2.69532212015273));
#246553=CARTESIAN_POINT('Ctrl Pts',(-56.1278011372716,18.3561185603239,
2.68176836726657));
#246554=CARTESIAN_POINT('Ctrl Pts',(-56.0390077039669,18.513437727039,2.75442176402259));
#246555=CARTESIAN_POINT('Ctrl Pts',(-56.0891934462348,18.4363968713614,
2.79203179920177));
#246556=CARTESIAN_POINT('Ctrl Pts',(-56.1770584756123,18.4370884086015,
2.74885310748176));
#246557=CARTESIAN_POINT('Ctrl Pts',(-56.0747542753112,18.5530236652633,
2.82866089558416));
#246558=CARTESIAN_POINT('Ctrl Pts',(-56.1242585025269,18.4521491348384,
2.85316563119105));
#246559=CARTESIAN_POINT('Ctrl Pts',(-56.2162483036943,18.4660698759072,
2.79189751796651));
#246560=CARTESIAN_POINT('Ctrl Pts',(-56.1179479440989,18.5670586829464,
2.90134173516037));
#246561=CARTESIAN_POINT('Ctrl Pts',(-56.1574782858998,18.4469743395778,
2.90103711553242));
#246562=CARTESIAN_POINT('Ctrl Pts',(-56.259443978424,18.4801050014189,2.83404198860274));
#246563=CARTESIAN_POINT('Origin',(-56.2201988201384,18.6008891789884,2.83404198860274));
#246564=CARTESIAN_POINT('Origin',(-58.3196542512031,19.2830435998995,3.56647653971794));
#246565=CARTESIAN_POINT('Origin',(-58.2418213702175,19.2577541638577,3.42473028058497));
#246566=CARTESIAN_POINT('Origin',(-56.3896289265335,18.6559403576611,3.1191364816812));
#246567=CARTESIAN_POINT('Origin',(-56.559059032799,18.7109915363515,3.40423097483323));
#246568=CARTESIAN_POINT('Ctrl Pts',(-57.9280106456677,19.1557908785623,
3.36123028058494));
#246569=CARTESIAN_POINT('Ctrl Pts',(-57.9672558039533,19.0350067009929,
3.36123028058494));
#246570=CARTESIAN_POINT('Ctrl Pts',(-57.9672558039533,19.0350067009929,
3.23423028058494));
#246571=CARTESIAN_POINT('Ctrl Pts',(-58.0136880650209,19.1833829156716,
3.36123028058494));
#246572=CARTESIAN_POINT('Ctrl Pts',(-58.0527804636619,19.0627953474459,
3.36099641108439));
#246573=CARTESIAN_POINT('Ctrl Pts',(-58.0956618095386,19.0767283413221,
3.23423043688335));
#246574=CARTESIAN_POINT('Ctrl Pts',(-58.0947019536603,19.2094750027326,
3.41054258905298));
#246575=CARTESIAN_POINT('Ctrl Pts',(-58.1340538395309,19.0892026680465,
3.41008815826044));
#246576=CARTESIAN_POINT('Ctrl Pts',(-58.2170788227766,19.1161791203809,
3.30819867304366));
#246577=CARTESIAN_POINT('Ctrl Pts',(-58.1373965169895,19.2232259141438,
3.48823028058497));
#246578=CARTESIAN_POINT('Ctrl Pts',(-58.1769325318821,19.1031347997386,
3.48794691941613));
#246579=CARTESIAN_POINT('Ctrl Pts',(-58.2810665285031,19.1369699862882,
3.42473028058499));
#246580=CARTESIAN_POINT('Origin',(-57.9280106456677,19.1557908785624,3.23423028058494));
#246581=CARTESIAN_POINT('Ctrl Pts',(-56.4568070719812,18.6771643191708,
3.47153072139085));
#246582=CARTESIAN_POINT('Ctrl Pts',(-56.496394798308,18.5568963159714,3.47122746285089));
#246583=CARTESIAN_POINT('Ctrl Pts',(-56.5984571192857,18.5902571970801,
3.40413046676783));
#246584=CARTESIAN_POINT('Ctrl Pts',(-56.5661228951882,18.7128129802646,
3.65553813458));
#246585=CARTESIAN_POINT('Ctrl Pts',(-56.6055928325701,18.5923766197431,
3.6552033607218));
#246586=CARTESIAN_POINT('Ctrl Pts',(-56.6859083114038,18.6186718120036,
3.55128134520018));
#246587=CARTESIAN_POINT('Ctrl Pts',(-56.7625049710034,18.7768537015941,
3.77003198860276));
#246588=CARTESIAN_POINT('Ctrl Pts',(-56.8019192501371,18.6561664154749,
3.76980209314185));
#246589=CARTESIAN_POINT('Ctrl Pts',(-56.8430104456864,18.6697173900123,
3.64284195387339));
#246590=CARTESIAN_POINT('Ctrl Pts',(-56.9687879773467,18.8441205405518,
3.77003198860276));
#246591=CARTESIAN_POINT('Ctrl Pts',(-57.0080919221124,18.7231554368004,
3.77003198860276));
#246592=CARTESIAN_POINT('Ctrl Pts',(-57.0080330916692,18.7233364982868,
3.64284189403783));
#246593=CARTESIAN_POINT('Origin',(-56.9687879773467,18.8441205405518,3.64303198860275));
#246594=CARTESIAN_POINT('Origin',(55.0155724295761,-17.5418038257011,3.2342302805847));
#246595=CARTESIAN_POINT('Origin',(-57.7842031819384,19.1090650011314,3.23423028058494));
#246596=CARTESIAN_POINT('Origin',(54.8020887275097,-17.472438766075,3.64303198860251));
#246597=CARTESIAN_POINT('Origin',(-57.3504898524405,18.9681964166837,3.64299171721716));
#246598=CARTESIAN_POINT('Ctrl Pts',(-57.5748148483577,19.0416371860876,
3.48823028058493));
#246599=CARTESIAN_POINT('Ctrl Pts',(-57.6147155869503,18.9204594407744,
3.48852004212271));
#246600=CARTESIAN_POINT('Ctrl Pts',(-57.5096375484038,18.8863175164091,
3.42473028058493));
#246601=CARTESIAN_POINT('Ctrl Pts',(-57.6176546016069,19.055431886254,3.41028005848419));
#246602=CARTESIAN_POINT('Ctrl Pts',(-57.6572916985355,18.9342932580161,
3.41074404220455));
#246603=CARTESIAN_POINT('Ctrl Pts',(-57.5738415009814,18.9071786451776,
3.30780486243969));
#246604=CARTESIAN_POINT('Ctrl Pts',(-57.6988141606862,19.0815664505357,
3.36123028058494));
#246605=CARTESIAN_POINT('Ctrl Pts',(-57.7380493683907,18.960533015575,3.36146460586262));
#246606=CARTESIAN_POINT('Ctrl Pts',(-57.695474842495,18.946699713554,3.23423045308351));
#246607=CARTESIAN_POINT('Ctrl Pts',(-57.7842031819384,19.1090650011314,
3.36123028058494));
#246608=CARTESIAN_POINT('Ctrl Pts',(-57.823448340224,18.9882808235619,3.36123028058494));
#246609=CARTESIAN_POINT('Ctrl Pts',(-57.823448340224,18.9882808235619,3.23423028058494));
#246610=CARTESIAN_POINT('Origin',(-57.4703923901182,19.0071016939786,3.42473028058494));
#246611=CARTESIAN_POINT('Origin',(-57.393023688561,18.9819630792892,3.56563113524718));
#246612=CARTESIAN_POINT('Origin',(-60.1478239224122,12.4602215063118,3.56647653909494));
#246613=CARTESIAN_POINT('Origin',(-60.1910940874972,12.4693660187259,3.64299466007661));
#246614=CARTESIAN_POINT('Origin',(-60.0677739512127,12.443206359372,3.42473028058491));
#246615=CARTESIAN_POINT('Ctrl Pts',(-59.9600752506738,12.4208962741585,
3.48823028058492));
#246616=CARTESIAN_POINT('Ctrl Pts',(-59.9342688867326,12.5446662374485,
3.48794691941608));
#246617=CARTESIAN_POINT('Ctrl Pts',(-60.0413691664788,12.5674311046652,
3.42473028058493));
#246618=CARTESIAN_POINT('Ctrl Pts',(-59.9160770362135,12.4114257351943,
3.41028005925095));
#246619=CARTESIAN_POINT('Ctrl Pts',(-59.8900198101354,12.5352608058721,
3.40982512231051));
#246620=CARTESIAN_POINT('Ctrl Pts',(-59.9753363727317,12.5533954010689,
3.30780486372868));
#246621=CARTESIAN_POINT('Ctrl Pts',(-59.832722693313,12.3934832896268,3.36123028058489));
#246622=CARTESIAN_POINT('Ctrl Pts',(-59.8062838430887,12.5174621766264,
3.36099721048421));
#246623=CARTESIAN_POINT('Ctrl Pts',(-59.8502383056086,12.5268049860496,
3.23423045308356));
#246624=CARTESIAN_POINT('Ctrl Pts',(-59.7450242491248,12.3746037924162,
3.36123028058489));
#246625=CARTESIAN_POINT('Ctrl Pts',(-59.718619464391,12.4988285377094,3.36123028058489));
#246626=CARTESIAN_POINT('Ctrl Pts',(-59.718619464391,12.4988285377094,3.23423028058489));
#246627=CARTESIAN_POINT('Origin',(-59.7450242491248,12.3746037924162,3.23423028058489));
#246628=CARTESIAN_POINT('Origin',(-0.0660119618346311,-0.3105618632328,
3.64303198860262));
#246629=CARTESIAN_POINT('Origin',(-60.5836663843182,12.5528626811445,3.64303198860271));
#246630=CARTESIAN_POINT('Origin',(-0.0660119618346311,-0.310561863232797,
3.23423028058481));
#246631=CARTESIAN_POINT('Origin',(-59.597120393566,12.3431658574209,3.23423028058489));
#246632=CARTESIAN_POINT('Ctrl Pts',(-61.1105274371642,12.6642893210139,
3.47153072139079));
#246633=CARTESIAN_POINT('Ctrl Pts',(-61.0844267845857,12.7893350777085,
3.4718232790267));
#246634=CARTESIAN_POINT('Ctrl Pts',(-60.9785037674409,12.7666250679675,
3.40413028959035));
#246635=CARTESIAN_POINT('Ctrl Pts',(-60.9980344071773,12.6404971713792,
3.65553807120965));
#246636=CARTESIAN_POINT('Ctrl Pts',(-60.9718026486737,12.7653958126131,
3.65586275496998));
#246637=CARTESIAN_POINT('Ctrl Pts',(-60.8885617651964,12.7475073053532,
3.55128126837319));
#246638=CARTESIAN_POINT('Ctrl Pts',(-60.7959446297927,12.597756154011,3.77003198860271));
#246639=CARTESIAN_POINT('Ctrl Pts',(-60.7696360759136,12.7224234952047,
3.77025505748454));
#246640=CARTESIAN_POINT('Ctrl Pts',(-60.7269846150095,12.7131630221038,
3.64284211731139));
#246641=CARTESIAN_POINT('Ctrl Pts',(-60.5836663843182,12.5528626811445,
3.77003198860271));
#246642=CARTESIAN_POINT('Ctrl Pts',(-60.5572221520604,12.6772730124468,
3.77003198860271));
#246643=CARTESIAN_POINT('Ctrl Pts',(-60.5572616290068,12.6770872880162,
3.64284239821708));
#246644=CARTESIAN_POINT('Origin',(-61.0050661295707,12.642433962084,3.40423097483317));
#246645=CARTESIAN_POINT('Ctrl Pts',(-59.597120393566,12.3431658574209,3.36123028058489));
#246646=CARTESIAN_POINT('Ctrl Pts',(-59.5707156088321,12.4673906027141,
3.36123028058489));
#246647=CARTESIAN_POINT('Ctrl Pts',(-59.5707156088321,12.4673906027141,
3.23423028058489));
#246648=CARTESIAN_POINT('Ctrl Pts',(-59.5091256622726,12.3242219811465,
3.36123028058489));
#246649=CARTESIAN_POINT('Ctrl Pts',(-59.4825873732106,12.448658367964,3.36146538610087));
#246650=CARTESIAN_POINT('Ctrl Pts',(-59.4386519140004,12.4393195978192,
3.23423043688379));
#246651=CARTESIAN_POINT('Ctrl Pts',(-59.4259203549057,12.3063073021292,
3.41054258693107));
#246652=CARTESIAN_POINT('Ctrl Pts',(-59.3996784303307,12.431035528135,3.41100608859863));
#246653=CARTESIAN_POINT('Ctrl Pts',(-59.3137762748665,12.4127764613286,
3.30819866970867));
#246654=CARTESIAN_POINT('Ctrl Pts',(-59.3820708699071,12.2968658913801,
3.48823028058489));
#246655=CARTESIAN_POINT('Ctrl Pts',(-59.3560370505014,12.421759266491,3.48852004212267));
#246656=CARTESIAN_POINT('Ctrl Pts',(-59.2479658375577,12.3987880210522,
3.42473028058489));
#246657=CARTESIAN_POINT('Origin',(-59.2743706222916,12.274563275759,3.42473028058489));
#246658=CARTESIAN_POINT('Origin',(-61.1793222555445,12.6794732450926,3.11913648178304));
#246659=CARTESIAN_POINT('Origin',(-61.3535783813233,12.7165125280164,2.83404198860269));
#246660=CARTESIAN_POINT('Origin',(-59.194798052794,12.2576496039905,3.56563113460843));
#246661=CARTESIAN_POINT('Origin',(-59.1510793400372,12.2483049653999,3.64299171721795));
#246662=CARTESIAN_POINT('Ctrl Pts',(-61.5816197022698,13.0739701745323,
2.59908173516032));
#246663=CARTESIAN_POINT('Ctrl Pts',(-61.545128164506,13.0662229071065,2.6587819886027));
#246664=CARTESIAN_POINT('Ctrl Pts',(-61.4762657165316,13.0516031943527,
2.6587819886027));
#246665=CARTESIAN_POINT('Ctrl Pts',(-61.5999188988198,12.9877758510418,
2.59908193475642));
#246666=CARTESIAN_POINT('Ctrl Pts',(-61.5584544893681,13.0034370926708,
2.65878715325387));
#246667=CARTESIAN_POINT('Ctrl Pts',(-61.4868491822337,13.0017087032038,
2.6587819886027));
#246668=CARTESIAN_POINT('Ctrl Pts',(-61.5923336062397,12.9030451317659,
2.63878778849879));
#246669=CARTESIAN_POINT('Ctrl Pts',(-61.5481051179917,12.94081036178,2.69564460180113));
#246670=CARTESIAN_POINT('Ctrl Pts',(-61.4721451382825,12.9504709278438,
2.68180481624893));
#246671=CARTESIAN_POINT('Ctrl Pts',(-61.5434299552079,12.7836101409429,
2.75443238878653));
#246672=CARTESIAN_POINT('Ctrl Pts',(-61.5018471007596,12.8662000075464,
2.79268340777113));
#246673=CARTESIAN_POINT('Ctrl Pts',(-61.4139027244671,12.8749747009097,
2.74885926835616));
#246674=CARTESIAN_POINT('Ctrl Pts',(-61.5035207735036,12.7478263086953,
2.82856655361677));
#246675=CARTESIAN_POINT('Ctrl Pts',(-61.4652971063431,12.8544221781235,
2.85384197230771));
#246676=CARTESIAN_POINT('Ctrl Pts',(-61.3716536946531,12.8501918100168,
2.79184624278451));
#246677=CARTESIAN_POINT('Ctrl Pts',(-61.4590390555209,12.7383709431249,
2.9013417351603));
#246678=CARTESIAN_POINT('Ctrl Pts',(-61.43297545991,12.8632261535953,2.90163218716398));
#246679=CARTESIAN_POINT('Ctrl Pts',(-61.3271735965894,12.8407372733096,
2.83404198860269));
#246680=CARTESIAN_POINT('Origin',(-61.4762657165316,13.0516031943527,2.53178198860269));
#246681=CARTESIAN_POINT('Origin',(-0.0660119618346311,-0.3105618632328,
3.64303198860262));
#246682=CARTESIAN_POINT('Origin',(-58.7584778814677,12.164906888579,3.64303198860271));
#246683=CARTESIAN_POINT('Origin',(1.31078692950416E-16,1.91543152271565E-13,
2.53178198860262));
#246684=CARTESIAN_POINT('Origin',(-61.4699285681955,13.081417133223,2.5317819886027));
#246685=CARTESIAN_POINT('Ctrl Pts',(-58.7584778814677,12.164906888579,3.77003198860271));
#246686=CARTESIAN_POINT('Ctrl Pts',(-58.732033541174,12.2893177281502,3.77003198860271));
#246687=CARTESIAN_POINT('Ctrl Pts',(-58.7320731263175,12.289131494692,3.64284187937051));
#246688=CARTESIAN_POINT('Ctrl Pts',(-58.5461948427482,12.1200194799681,
3.77003198860271));
#246689=CARTESIAN_POINT('Ctrl Pts',(-58.5199849720728,12.2442448876967,
3.76980208962782));
#246690=CARTESIAN_POINT('Ctrl Pts',(-58.5623471386682,12.253055122594,3.64284193928217));
#246691=CARTESIAN_POINT('Ctrl Pts',(-58.3441042111264,12.0772896710143,
3.65553535416591));
#246692=CARTESIAN_POINT('Ctrl Pts',(-58.3180679977595,12.2013256001486,
3.65520057834582));
#246693=CARTESIAN_POINT('Ctrl Pts',(-58.4007711908105,12.2187110949217,
3.55127910964302));
#246694=CARTESIAN_POINT('Ctrl Pts',(-58.2316113004782,12.053504764932,3.47153072139081));
#246695=CARTESIAN_POINT('Ctrl Pts',(-58.2057612725768,12.1774537884112,
3.47122746281592));
#246696=CARTESIAN_POINT('Ctrl Pts',(-58.3108302909894,12.1995935666435,
3.4041304590128));
#246697=CARTESIAN_POINT('Origin',(-58.3370777047235,12.0753355159231,3.40423097483318));
#246698=CARTESIAN_POINT('Ctrl Pts',(-61.3267881959114,13.3605623192485,
2.90134173516031));
#246699=CARTESIAN_POINT('Ctrl Pts',(-61.3537611057084,13.2359003894749,
2.90163218716398));
#246700=CARTESIAN_POINT('Ctrl Pts',(-61.2479592423879,13.2134115091892,
2.8340419886027));
#246701=CARTESIAN_POINT('Ctrl Pts',(-61.3712903180781,13.3700210384231,
2.82853349835361));
#246702=CARTESIAN_POINT('Ctrl Pts',(-61.3797222373789,13.2571016411954,
2.85381483162365));
#246703=CARTESIAN_POINT('Ctrl Pts',(-61.2924596082466,13.2228703539492,
2.79182701594243));
#246704=CARTESIAN_POINT('Ctrl Pts',(-61.422128257289,13.353519088177,2.75468822073652));
#246705=CARTESIAN_POINT('Ctrl Pts',(-61.4177900459394,13.2610999767702,
2.79286913083864));
#246706=CARTESIAN_POINT('Ctrl Pts',(-61.3409599630868,13.2173727427873,
2.74900763297921));
#246707=CARTESIAN_POINT('Ctrl Pts',(-61.5148770953649,13.2651598666399,
2.639544506404));
#246708=CARTESIAN_POINT('Ctrl Pts',(-61.4899829268154,13.2123479779268,
2.69627684028851));
#246709=CARTESIAN_POINT('Ctrl Pts',(-61.4244514636294,13.1725625528867,
2.68224356036499));
#246710=CARTESIAN_POINT('Ctrl Pts',(-61.5568698122752,13.1903059833734,
2.59908178706443));
#246711=CARTESIAN_POINT('Ctrl Pts',(-61.525369554737,13.1590895168685,2.65878704321593));
#246712=CARTESIAN_POINT('Ctrl Pts',(-61.4592680512443,13.1314678292776,
2.65878198860269));
#246713=CARTESIAN_POINT('Ctrl Pts',(-61.5752716937452,13.1038352065726,
2.59908173516031));
#246714=CARTESIAN_POINT('Ctrl Pts',(-61.5387839176329,13.0960702419678,
2.65878198860269));
#246715=CARTESIAN_POINT('Ctrl Pts',(-61.4699285681955,13.081417133223,2.65878198860269));
#246716=CARTESIAN_POINT('Origin',(-61.221554457654,13.3376362544824,2.8340419886027));
#246717=CARTESIAN_POINT('Origin',(-58.1628213392034,12.0382961820491,3.11913648167021));
#246718=CARTESIAN_POINT('Origin',(-57.988564973546,12.0012568480858,2.8340419886027));
#246719=CARTESIAN_POINT('Origin',(-61.047298331873,13.3005969715131,3.11913648177578));
#246720=CARTESIAN_POINT('Origin',(-60.8730422059014,13.26355768855,3.40423097483318));
#246721=CARTESIAN_POINT('Ctrl Pts',(-57.8830978693156,11.979429479061,2.90134173516031));
#246722=CARTESIAN_POINT('Ctrl Pts',(-57.8572899778512,12.1031907419155,
2.90103711553237));
#246723=CARTESIAN_POINT('Ctrl Pts',(-57.9621601888121,12.125481593379,2.83404198860269));
#246724=CARTESIAN_POINT('Ctrl Pts',(-57.8386546085357,11.9699833161087,
2.82862991747971));
#246725=CARTESIAN_POINT('Ctrl Pts',(-57.8310944294261,12.0820882677183,
2.85314045886447));
#246726=CARTESIAN_POINT('Ctrl Pts',(-57.9177151970033,12.1160345187366,
2.79187960999925));
#246727=CARTESIAN_POINT('Ctrl Pts',(-57.7880992891175,11.9864204851029,
2.75470625793335));
#246728=CARTESIAN_POINT('Ctrl Pts',(-57.7929810340972,12.0782959991609,
2.79224250381911));
#246729=CARTESIAN_POINT('Ctrl Pts',(-57.8694789541063,12.1215717318493,
2.74901809108265));
#246730=CARTESIAN_POINT('Ctrl Pts',(-57.6961636462598,12.0746725352387,
2.63947868311705));
#246731=CARTESIAN_POINT('Ctrl Pts',(-57.7211944343233,12.127248449038,2.69595066767917));
#246732=CARTESIAN_POINT('Ctrl Pts',(-57.7867317752136,12.1665991704024,
2.68220539436071));
#246733=CARTESIAN_POINT('Ctrl Pts',(-57.6547178110645,12.149412060458,2.59908178585055));
#246734=CARTESIAN_POINT('Ctrl Pts',(-57.6862546895618,12.1804827566583,
2.65877670944877));
#246735=CARTESIAN_POINT('Ctrl Pts',(-57.7524075778586,12.2078361528631,
2.6587819886027));
#246736=CARTESIAN_POINT('Ctrl Pts',(-57.6364522029208,12.2354540642043,
2.59908173516031));
#246737=CARTESIAN_POINT('Ctrl Pts',(-57.6729438621907,12.2432007592845,
2.6587819886027));
#246738=CARTESIAN_POINT('Ctrl Pts',(-57.7418065394566,12.2578193919766,
2.6587819886027));
#246739=CARTESIAN_POINT('Origin',(-57.7418065394566,12.2578193919766,2.5317819886027));
#246740=CARTESIAN_POINT('Ctrl Pts',(-60.451642460649,13.1739864076105,3.77003198860272));
#246741=CARTESIAN_POINT('Ctrl Pts',(-60.478086695185,13.0495760655902,3.77003198860272));
#246742=CARTESIAN_POINT('Ctrl Pts',(-60.478047215957,13.0497618007548,3.64284238727605));
#246743=CARTESIAN_POINT('Ctrl Pts',(-60.6638314094603,13.2193162256446,
3.77003198860272));
#246744=CARTESIAN_POINT('Ctrl Pts',(-60.6905041359628,13.094726276951,3.77025506105687));
#246745=CARTESIAN_POINT('Ctrl Pts',(-60.6477728389709,13.0858380958634,
3.64284210641796));
#246746=CARTESIAN_POINT('Ctrl Pts',(-60.865832349848,13.2624673401135,3.65553527987841));
#246747=CARTESIAN_POINT('Ctrl Pts',(-60.8926693037172,13.1376973240556,
3.65585996533169));
#246748=CARTESIAN_POINT('Ctrl Pts',(-60.8093487091495,13.1201821075163,
3.55127902710262));
#246749=CARTESIAN_POINT('Ctrl Pts',(-60.9782752797349,13.2864868028994,
3.4715307213908));
#246750=CARTESIAN_POINT('Ctrl Pts',(-61.0052918407716,13.1616357172824,
3.47182327905196));
#246751=CARTESIAN_POINT('Ctrl Pts',(-60.8992893450418,13.1392995799685,
3.40413028377995));
#246752=CARTESIAN_POINT('Origin',(-60.451642460649,13.1739864076105,3.64303198860272));
#246753=CARTESIAN_POINT('Origin',(3.54593577968597E-16,1.91589630272981E-13,
2.53178198860262));
#246754=CARTESIAN_POINT('Origin',(-57.7354693911205,12.2876333308469,2.5317819886027));
#246755=CARTESIAN_POINT('Origin',(59.5987607253196,-12.3435145206981,3.64303198860255));
#246756=CARTESIAN_POINT('Origin',(-60.0590486699121,13.0905908661183,3.64299466007645));
#246757=CARTESIAN_POINT('Ctrl Pts',(-57.6301266171958,12.2652136052659,
2.59908173516031));
#246758=CARTESIAN_POINT('Ctrl Pts',(-57.6666142715156,12.2729791421553,
2.6587819886027));
#246759=CARTESIAN_POINT('Ctrl Pts',(-57.7354693911205,12.2876333308469,
2.6587819886027));
#246760=CARTESIAN_POINT('Ctrl Pts',(-57.6118791634502,12.3509528635303,
2.59908193199883));
#246761=CARTESIAN_POINT('Ctrl Pts',(-57.6533170557967,12.3354428975795,
2.65877685806624));
#246762=CARTESIAN_POINT('Ctrl Pts',(-57.7248602994014,12.3374367183506,
2.6587819886027));
#246763=CARTESIAN_POINT('Ctrl Pts',(-57.619017823295,12.4353658313042,2.63872492669789));
#246764=CARTESIAN_POINT('Ctrl Pts',(-57.6632723181621,12.3978675338897,
2.6953221201529));
#246765=CARTESIAN_POINT('Ctrl Pts',(-57.7390640345625,12.3886090227466,
2.68176836726647));
#246766=CARTESIAN_POINT('Ctrl Pts',(-57.6672013517154,12.5543478197373,
2.75442176402273));
#246767=CARTESIAN_POINT('Ctrl Pts',(-57.7090592089825,12.4724831634112,
2.79203179920132));
#246768=CARTESIAN_POINT('Ctrl Pts',(-57.7965151898611,12.463986515842,2.74885310748178));
#246769=CARTESIAN_POINT('Ctrl Pts',(-57.7068899568908,12.5899803678813,
2.82866089558396));
#246770=CARTESIAN_POINT('Ctrl Pts',(-57.7455787351221,12.4844838378936,
2.85316563119178));
#246771=CARTESIAN_POINT('Ctrl Pts',(-57.8385197202049,12.4887127671321,
2.79189751796692));
#246772=CARTESIAN_POINT('Ctrl Pts',(-57.7513140650721,12.599423532447,2.90134173516031));
#246773=CARTESIAN_POINT('Ctrl Pts',(-57.7780756236496,12.4758649777951,
2.90103711553237));
#246774=CARTESIAN_POINT('Ctrl Pts',(-57.8829458346106,12.4981558292586,
2.83404198860269));
#246775=CARTESIAN_POINT('Origin',(-57.8565410498767,12.6223805745517,2.83404198860269));
#246776=CARTESIAN_POINT('Origin',(-60.0157999977489,13.08134523226,3.56647653971844));
#246777=CARTESIAN_POINT('Origin',(-59.9357500275434,13.064330085838,3.42473028058494));
#246778=CARTESIAN_POINT('Origin',(-58.0307974155282,12.6594199084519,3.11913648168203));
#246779=CARTESIAN_POINT('Origin',(-58.2050537810542,12.6964592423891,3.40423097483318));
#246780=CARTESIAN_POINT('Ctrl Pts',(-59.6130003254556,12.9957275188822,
3.3612302805849));
#246781=CARTESIAN_POINT('Ctrl Pts',(-59.6394051101894,12.871502773589,3.36123028058489));
#246782=CARTESIAN_POINT('Ctrl Pts',(-59.6394051101894,12.871502773589,3.2342302805849));
#246783=CARTESIAN_POINT('Ctrl Pts',(-59.7010925481785,13.0142126749435,
3.3612302805849));
#246784=CARTESIAN_POINT('Ctrl Pts',(-59.7273659613738,12.8901994296778,
3.36099641108629));
#246785=CARTESIAN_POINT('Ctrl Pts',(-59.7714687931894,12.899573775969,3.23423043688377));
#246786=CARTESIAN_POINT('Ctrl Pts',(-59.7843900000233,13.031693569538,3.41054258905291));
#246787=CARTESIAN_POINT('Ctrl Pts',(-59.8109544298277,12.9079667071257,
3.41008815825905));
#246788=CARTESIAN_POINT('Ctrl Pts',(-59.8963444006345,12.9261169057239,
3.30819867304326));
#246789=CARTESIAN_POINT('Ctrl Pts',(-59.8282880397056,13.0409063549237,
3.48823028058492));
#246790=CARTESIAN_POINT('Ctrl Pts',(-59.855054532531,12.9173404733281,3.48794691941607));
#246791=CARTESIAN_POINT('Ctrl Pts',(-59.9621548122772,12.9401053405448,
3.42473028058493));
#246792=CARTESIAN_POINT('Origin',(-59.6130003254556,12.9957275188822,3.2342302805849));
#246793=CARTESIAN_POINT('Ctrl Pts',(-58.0998260601481,12.6735055745739,
3.4715307213908));
#246794=CARTESIAN_POINT('Ctrl Pts',(-58.1266254912132,12.5497583678826,
3.47122746285085));
#246795=CARTESIAN_POINT('Ctrl Pts',(-58.2316158657531,12.5722680770246,
3.40413046676782));
#246796=CARTESIAN_POINT('Ctrl Pts',(-58.212269339599,12.6975323335629,3.65553813457996));
#246797=CARTESIAN_POINT('Ctrl Pts',(-58.2389340288442,12.5736300041249,
3.65520336072351));
#246798=CARTESIAN_POINT('Ctrl Pts',(-58.3215581271232,12.5913858949916,
3.55128134520024));
#246799=CARTESIAN_POINT('Ctrl Pts',(-58.4142696920426,12.7406947165204,
3.77003198860271));
#246800=CARTESIAN_POINT('Ctrl Pts',(-58.4408527990795,12.616548653954,3.7698020931406));
#246801=CARTESIAN_POINT('Ctrl Pts',(-58.4831353553017,12.6257301953102,
3.6428419538732));
#246802=CARTESIAN_POINT('Ctrl Pts',(-58.6264539577984,12.7860306150449,
3.77003198860272));
#246803=CARTESIAN_POINT('Ctrl Pts',(-58.6528982950381,12.6616197898421,
3.77003198860271));
#246804=CARTESIAN_POINT('Ctrl Pts',(-58.6528587129532,12.6618060089104,
3.64284189403786));
#246805=CARTESIAN_POINT('Origin',(-58.6264539577984,12.7860306150449,3.64303198860271));
#246806=CARTESIAN_POINT('Origin',(58.1567073854023,-12.0369966210205,3.23423028058474));
#246807=CARTESIAN_POINT('Origin',(-59.4650964698967,12.9642895838869,3.2342302805849));
#246808=CARTESIAN_POINT('Origin',(57.9308881865556,-11.9889972685545,3.64303198860255));
#246809=CARTESIAN_POINT('Origin',(-59.0190342907429,12.8695280801151,3.64299171721718));
#246810=CARTESIAN_POINT('Ctrl Pts',(-59.249807061628,12.9191181862044,3.48823028058489));
#246811=CARTESIAN_POINT('Ctrl Pts',(-59.2768226962999,12.7944335023706,
3.48852004212266));
#246812=CARTESIAN_POINT('Ctrl Pts',(-59.1687514833561,12.7714622569318,
3.42473028058488));
#246813=CARTESIAN_POINT('Ctrl Pts',(-59.2938540730359,12.9283593439868,
3.41028005848414));
#246814=CARTESIAN_POINT('Ctrl Pts',(-59.3206115991486,12.8037411209987,
3.410744042203));
#246815=CARTESIAN_POINT('Ctrl Pts',(-59.2347843016971,12.7854979657557,
3.30780486243963));
#246816=CARTESIAN_POINT('Ctrl Pts',(-59.3773008374015,12.9458672563999,
3.3612302805849));
#246817=CARTESIAN_POINT('Ctrl Pts',(-59.4036696715723,12.8213956592928,
3.36146460586466));
#246818=CARTESIAN_POINT('Ctrl Pts',(-59.3598823995813,12.8120883873135,
3.23423045308393));
#246819=CARTESIAN_POINT('Ctrl Pts',(-59.4650964698967,12.9642895838869,
3.3612302805849));
#246820=CARTESIAN_POINT('Ctrl Pts',(-59.4915012546306,12.8400648385937,
3.36123028058489));
#246821=CARTESIAN_POINT('Ctrl Pts',(-59.4915012546306,12.8400648385937,
3.2342302805849));
#246822=CARTESIAN_POINT('Origin',(-59.1423466986223,12.895687002225,3.42473028058489));
#246823=CARTESIAN_POINT('Origin',(-59.0627741301468,12.8787733309741,3.5656311352478));
#246824=CARTESIAN_POINT('Origin',(-61.1207756556248,6.10480350566248,3.56647653909434));
#246825=CARTESIAN_POINT('Origin',(-61.1647646440477,6.10937495961987,3.64299466007599));
#246826=CARTESIAN_POINT('Origin',(-61.0393856393804,6.09624906995217,3.42473028058487));
#246827=CARTESIAN_POINT('Ctrl Pts',(-60.9299448846691,6.08531878138299,
3.48823028058487));
#246828=CARTESIAN_POINT('Ctrl Pts',(-60.9172173747511,6.21110821942913,
3.48794691941604));
#246829=CARTESIAN_POINT('Ctrl Pts',(-61.0261105245455,6.22255335066394,
3.42473028058489));
#246830=CARTESIAN_POINT('Ctrl Pts',(-60.885197756147,6.08049918876632,3.4102800592509));
#246831=CARTESIAN_POINT('Ctrl Pts',(-60.8722275639178,6.20637959976664,
3.40982512230967));
#246832=CARTESIAN_POINT('Ctrl Pts',(-60.9589723348236,6.21549684257611,
3.30780486372855));
#246833=CARTESIAN_POINT('Ctrl Pts',(-60.800424540796,6.07136793516325,3.36123028058485));
#246834=CARTESIAN_POINT('Ctrl Pts',(-60.7870898478943,6.19743126523199,
3.36099721048481));
#246835=CARTESIAN_POINT('Ctrl Pts',(-60.8317801127822,6.20212840134671,
3.23423045308369));
#246836=CARTESIAN_POINT('Ctrl Pts',(-60.7112330730304,6.06175884541548,
3.36123028058485));
#246837=CARTESIAN_POINT('Ctrl Pts',(-60.6979579581954,6.18806312612726,
3.36123028058485));
#246838=CARTESIAN_POINT('Ctrl Pts',(-60.6979579581954,6.18806312612726,
3.23423028058485));
#246839=CARTESIAN_POINT('Origin',(-60.7112330730304,6.06175884541549,3.23423028058484));
#246840=CARTESIAN_POINT('Origin',(-0.0331877870874725,-0.315760701779243,
3.64303198860262));
#246841=CARTESIAN_POINT('Origin',(-61.5639141665612,6.15137923967653,3.64303198860266));
#246842=CARTESIAN_POINT('Origin',(-0.0331877870874724,-0.31576070177924,
3.23423028058481));
#246843=CARTESIAN_POINT('Origin',(-60.5608532912344,6.04595329345039,3.23423028058485));
#246844=CARTESIAN_POINT('Ctrl Pts',(-62.0995362748659,6.20712349654441,
3.47153072139075));
#246845=CARTESIAN_POINT('Ctrl Pts',(-62.0866494451786,6.33421250060425,
3.47182327902666));
#246846=CARTESIAN_POINT('Ctrl Pts',(-61.9789328429858,6.32269886887975,
3.40413028959034));
#246847=CARTESIAN_POINT('Ctrl Pts',(-61.9851725366286,6.19522040634676,
3.65553807120959));
#246848=CARTESIAN_POINT('Ctrl Pts',(-61.9721399414742,6.32217680516095,
3.6558627549699));
#246849=CARTESIAN_POINT('Ctrl Pts',(-61.887485202092,6.31308733464707,3.55128126837344));
#246850=CARTESIAN_POINT('Ctrl Pts',(-61.7797221753254,6.17383766261707,
3.77003198860267));
#246851=CARTESIAN_POINT('Ctrl Pts',(-61.7665890280525,6.30057205577847,
3.7702550574842));
#246852=CARTESIAN_POINT('Ctrl Pts',(-61.7232032332917,6.29582060418326,
3.64284211731065));
#246853=CARTESIAN_POINT('Ctrl Pts',(-61.5639141665612,6.15137923967653,
3.77003198860267));
#246854=CARTESIAN_POINT('Ctrl Pts',(-61.5506192193202,6.27787221312685,
3.77003198860267));
#246855=CARTESIAN_POINT('Ctrl Pts',(-61.5506390665185,6.27768337964962,
3.6428423982171));
#246856=CARTESIAN_POINT('Origin',(-61.9923681882669,6.19641157197441,3.40423097483313));
#246857=CARTESIAN_POINT('Ctrl Pts',(-60.5608532912344,6.04595329345039,
3.36123028058485));
#246858=CARTESIAN_POINT('Ctrl Pts',(-60.5475781763994,6.17225757416217,
3.36123028058485));
#246859=CARTESIAN_POINT('Ctrl Pts',(-60.5475781763994,6.17225757416217,
3.23423028058485));
#246860=CARTESIAN_POINT('Ctrl Pts',(-60.4713604300108,6.03631114775018,
3.36123028058485));
#246861=CARTESIAN_POINT('Ctrl Pts',(-60.457974664764,6.16283986559477,3.36146538610095));
#246862=CARTESIAN_POINT('Ctrl Pts',(-60.4133037213016,6.1581447602434,3.23423043688392));
#246863=CARTESIAN_POINT('Ctrl Pts',(-60.3867383361559,6.02719193013363,
3.41054258693102));
#246864=CARTESIAN_POINT('Ctrl Pts',(-60.3736778173768,6.1539799099147,3.41100608859762));
#246865=CARTESIAN_POINT('Ctrl Pts',(-60.286337650718,6.14480008849002,3.30819866970862));
#246866=CARTESIAN_POINT('Ctrl Pts',(-60.3421421670675,6.02238575970255,
3.48823028058484));
#246867=CARTESIAN_POINT('Ctrl Pts',(-60.3293058762212,6.14931623097225,
3.48852004212262));
#246868=CARTESIAN_POINT('Ctrl Pts',(-60.2194255397045,6.13776734223194,
3.42473028058484));
#246869=CARTESIAN_POINT('Origin',(-60.2327006545395,6.01146306152017,3.42473028058484));
#246870=CARTESIAN_POINT('Origin',(-62.1695413802837,6.21503322485355,3.11913648178332));
#246871=CARTESIAN_POINT('Origin',(-62.3467145720969,6.23365487766603,2.83404198860265));
#246872=CARTESIAN_POINT('Origin',(-60.151796031785,6.00295964302194,3.56563113460813));
#246873=CARTESIAN_POINT('Origin',(-60.1073400339998,5.998236045201,3.64299171721792));
#246874=CARTESIAN_POINT('Ctrl Pts',(-62.6108711573006,6.5653175249528,2.59908173516027));
#246875=CARTESIAN_POINT('Ctrl Pts',(-62.5737697140402,6.5614271022333,2.65878198860266));
#246876=CARTESIAN_POINT('Ctrl Pts',(-62.5037563256535,6.55408556365924,
2.65878198860265));
#246877=CARTESIAN_POINT('Ctrl Pts',(-62.6200603487601,6.47768259609059,
2.59908193475661));
#246878=CARTESIAN_POINT('Ctrl Pts',(-62.5804601312005,6.49759225479933,
2.65878715325419));
#246879=CARTESIAN_POINT('Ctrl Pts',(-62.5090664195363,6.50335812634736,
2.65878198860265));
#246880=CARTESIAN_POINT('Ctrl Pts',(-62.6036598373291,6.39420891953742,
2.63878778849883));
#246881=CARTESIAN_POINT('Ctrl Pts',(-62.5636211788254,6.4363904035792,2.69564460180115));
#246882=CARTESIAN_POINT('Ctrl Pts',(-62.4890871199581,6.45393802800009,
2.68180481624886));
#246883=CARTESIAN_POINT('Ctrl Pts',(-62.5425397295635,6.28054002958117,
2.7544323887864));
#246884=CARTESIAN_POINT('Ctrl Pts',(-62.5098176621807,6.36702405212765,
2.792683407771));
#246885=CARTESIAN_POINT('Ctrl Pts',(-62.423272259596,6.38494336730957,2.74885926835614));
#246886=CARTESIAN_POINT('Ctrl Pts',(-62.4991087455376,6.24912387034458,
2.82856655361681));
#246887=CARTESIAN_POINT('Ctrl Pts',(-62.4722367740483,6.35913125763809,
2.85384197230793));
#246888=CARTESIAN_POINT('Ctrl Pts',(-62.3786641568872,6.36471246584703,
2.79184624278445));
#246889=CARTESIAN_POINT('Ctrl Pts',(-62.4538823482276,6.24436990788037,
2.90134173516025));
#246890=CARTESIAN_POINT('Ctrl Pts',(-62.4410124550019,6.37126553604047,
2.90163218716393));
#246891=CARTESIAN_POINT('Ctrl Pts',(-62.3334394572619,6.3599591583778,2.83404198860264));
#246892=CARTESIAN_POINT('Origin',(-62.5037563256535,6.55408556365924,2.53178198860265));
#246893=CARTESIAN_POINT('Origin',(-0.0331877870874725,-0.315760701779243,
3.64303198860262));
#246894=CARTESIAN_POINT('Origin',(-59.7081718144893,5.95633285891189,3.64303198860266));
#246895=CARTESIAN_POINT('Origin',(1.33778643725276E-16,1.91560199089859E-13,
2.53178198860262));
#246896=CARTESIAN_POINT('Origin',(-62.5005702980931,6.58439859103007,2.53178198860265));
#246897=CARTESIAN_POINT('Ctrl Pts',(-59.7081718144893,5.95633285891189,
3.77003198860267));
#246898=CARTESIAN_POINT('Ctrl Pts',(-59.6948768129328,6.08282634913945,
3.77003198860267));
#246899=CARTESIAN_POINT('Ctrl Pts',(-59.6948967145276,6.08263699811361,
3.64284187937066));
#246900=CARTESIAN_POINT('Ctrl Pts',(-59.4923596726254,5.9338809680367,3.77003198860267));
#246901=CARTESIAN_POINT('Ctrl Pts',(-59.4792784733315,6.06016553348737,
3.76980208962841));
#246902=CARTESIAN_POINT('Ctrl Pts',(-59.5223294958604,6.06449945282216,
3.64284193928277));
#246903=CARTESIAN_POINT('Ctrl Pts',(-59.2869096333629,5.91250946061126,
3.65553535416586));
#246904=CARTESIAN_POINT('Ctrl Pts',(-59.2739813341607,6.03858743332211,
3.65520057834496));
#246905=CARTESIAN_POINT('Ctrl Pts',(-59.3580487495188,6.04723285085777,
3.55127910964236));
#246906=CARTESIAN_POINT('Ctrl Pts',(-59.1725467709678,5.90061356181236,
3.47153072139075));
#246907=CARTESIAN_POINT('Ctrl Pts',(-59.1597945531718,6.02658564326377,
3.47122746281586));
#246908=CARTESIAN_POINT('Ctrl Pts',(-59.2666022295036,6.03762143444283,
3.40413045901285));
#246909=CARTESIAN_POINT('Origin',(-59.2797173540686,5.91130048050322,3.40423097483314));
#246910=CARTESIAN_POINT('Ctrl Pts',(-62.3873926810692,6.87697683366542,
2.90134173516027));
#246911=CARTESIAN_POINT('Ctrl Pts',(-62.4011871104969,6.75017837817579,
2.90163218716395));
#246912=CARTESIAN_POINT('Ctrl Pts',(-62.293614112757,6.73887200051311,2.83404198860265));
#246913=CARTESIAN_POINT('Ctrl Pts',(-62.4326397213342,6.88173199854474,
2.8285334983535));
#246914=CARTESIAN_POINT('Ctrl Pts',(-62.4292221586318,6.76854981002497,
2.8538148316231));
#246915=CARTESIAN_POINT('Ctrl Pts',(-62.3388594194628,6.74362747387379,
2.79182701594245));
#246916=CARTESIAN_POINT('Ctrl Pts',(-62.4814742414946,6.86000643604713,
2.75468822073656));
#246917=CARTESIAN_POINT('Ctrl Pts',(-62.4674993676282,6.76854707276811,
2.79286913083876));
#246918=CARTESIAN_POINT('Ctrl Pts',(-62.3865194274374,6.73309031164165,
2.74900763297921));
#246919=CARTESIAN_POINT('Ctrl Pts',(-62.5644789380884,6.76243636205672,
2.63954450640386));
#246920=CARTESIAN_POINT('Ctrl Pts',(-62.5342007968299,6.71251593157883,
2.69627684028836));
#246921=CARTESIAN_POINT('Ctrl Pts',(-62.4648696125158,6.67979835840227,
2.6822435603649));
#246922=CARTESIAN_POINT('Ctrl Pts',(-62.5984172531145,6.68360310202791,
2.59908178706377));
#246923=CARTESIAN_POINT('Ctrl Pts',(-62.5638265480135,6.65585031610604,
2.65878704321558));
#246924=CARTESIAN_POINT('Ctrl Pts',(-62.4951999029147,6.63528943158945,
2.65878198860265));
#246925=CARTESIAN_POINT('Ctrl Pts',(-62.6076796697355,6.59568250079864,
2.59908173516026));
#246926=CARTESIAN_POINT('Ctrl Pts',(-62.570580117661,6.59177408464752,2.65878198860265));
#246927=CARTESIAN_POINT('Ctrl Pts',(-62.5005702980931,6.58439859103007,
2.65878198860265));
#246928=CARTESIAN_POINT('Origin',(-62.280338997922,6.86517628122488,2.83404198860265));
#246929=CARTESIAN_POINT('Origin',(-59.1025439185019,5.89267880207498,3.11913648166995));
#246930=CARTESIAN_POINT('Origin',(-58.925370482788,5.87405712357849,2.83404198860266));
#246931=CARTESIAN_POINT('Origin',(-62.1031658061019,6.84655462836655,3.11913648177607));
#246932=CARTESIAN_POINT('Origin',(-61.925992614092,6.82793297553327,3.40423097483314));
#246933=CARTESIAN_POINT('Ctrl Pts',(-58.8181995570485,5.8633736414956,2.90134173516027));
#246934=CARTESIAN_POINT('Ctrl Pts',(-58.8054696185321,5.98915458643774,
2.90103711553232));
#246935=CARTESIAN_POINT('Ctrl Pts',(-58.912095367953,6.00036140429026,2.83404198860265));
#246936=CARTESIAN_POINT('Ctrl Pts',(-58.773012368204,5.85862481136443,2.8286299174796));
#246937=CARTESIAN_POINT('Ctrl Pts',(-58.777211762863,5.97090589422323,2.85314045886469));
#246938=CARTESIAN_POINT('Ctrl Pts',(-58.8669063622641,5.99561184840491,
2.79187960999987));
#246939=CARTESIAN_POINT('Ctrl Pts',(-58.7244521481309,5.88025640567561,
2.75470625793339));
#246940=CARTESIAN_POINT('Ctrl Pts',(-58.7389107566976,5.97111833475351,
2.7922425038187));
#246941=CARTESIAN_POINT('Ctrl Pts',(-58.8195131589313,6.00616078842875,
2.74901809108258));
#246942=CARTESIAN_POINT('Ctrl Pts',(-58.6422449895249,5.97763489331422,
2.63947868311692));
#246943=CARTESIAN_POINT('Ctrl Pts',(-58.6726343357863,6.02730636094616,
2.69595066767936));
#246944=CARTESIAN_POINT('Ctrl Pts',(-58.7419259266988,6.05959099741143,
2.68220539436069));
#246945=CARTESIAN_POINT('Ctrl Pts',(-58.6088386066677,6.05629725705607,
2.59908178585));
#246946=CARTESIAN_POINT('Ctrl Pts',(-58.6434504949716,6.08390124328586,
2.65877670944815));
#246947=CARTESIAN_POINT('Ctrl Pts',(-58.7121001992953,6.10418993497001,
2.65878198860265));
#246948=CARTESIAN_POINT('Ctrl Pts',(-58.5996668978649,6.14377718965303,
2.59908173516027));
#246949=CARTESIAN_POINT('Ctrl Pts',(-58.6367684021393,6.14766703046151,
2.65878198860265));
#246950=CARTESIAN_POINT('Ctrl Pts',(-58.7067819056643,6.15500747092296,
2.65878198860265));
#246951=CARTESIAN_POINT('Origin',(-58.7067819056643,6.15500747092296,2.53178198860265));
#246952=CARTESIAN_POINT('Ctrl Pts',(-61.4975385923863,6.78290064323539,
3.77003198860267));
#246953=CARTESIAN_POINT('Ctrl Pts',(-61.5108335407726,6.65640765888754,
3.77003198860267));
#246954=CARTESIAN_POINT('Ctrl Pts',(-61.5108136924273,6.65659650327855,
3.64284238727592));
#246955=CARTESIAN_POINT('Ctrl Pts',(-61.7133034041535,6.80580235504213,
3.77003198860267));
#246956=CARTESIAN_POINT('Ctrl Pts',(-61.7268068187931,6.6791068640109,3.77025506105739));
#246957=CARTESIAN_POINT('Ctrl Pts',(-61.6833805404074,6.67473401011705,
3.64284210641797));
#246958=CARTESIAN_POINT('Ctrl Pts',(-61.9187082819379,6.82760223531323,
3.65553527987831));
#246959=CARTESIAN_POINT('Ctrl Pts',(-61.9323562021263,6.70071049691211,
3.6558599653315));
#246960=CARTESIAN_POINT('Ctrl Pts',(-61.8476612078244,6.69200060426976,
3.55127902710253));
#246961=CARTESIAN_POINT('Ctrl Pts',(-62.0330459552233,6.83973663030238,
3.47153072139074));
#246962=CARTESIAN_POINT('Ctrl Pts',(-62.046864024595,6.71274549238783,3.47182327905191));
#246963=CARTESIAN_POINT('Ctrl Pts',(-61.9391074595191,6.70161199275237,
3.40413028377984));
#246964=CARTESIAN_POINT('Origin',(-61.4975385923863,6.78290064323539,3.64303198860267));
#246965=CARTESIAN_POINT('Origin',(3.53633106925806E-16,1.9158356609748E-13,
2.53178198860262));
#246966=CARTESIAN_POINT('Origin',(-58.7035958781039,6.18532049829379,2.53178198860266));
#246967=CARTESIAN_POINT('Origin',(61.5757885448748,-6.15262728712807,3.64303198860259));
#246968=CARTESIAN_POINT('Origin',(-61.0983782637171,6.74099917687887,3.6429946600764));
#246969=CARTESIAN_POINT('Ctrl Pts',(-58.5964866834551,6.17403490859001,
2.59908173516027));
#246970=CARTESIAN_POINT('Ctrl Pts',(-58.6335861742242,6.17794390662152,
2.65878198860266));
#246971=CARTESIAN_POINT('Ctrl Pts',(-58.7035958781039,6.18532049829379,
2.65878198860265));
#246972=CARTESIAN_POINT('Ctrl Pts',(-58.5873013840785,6.26121185652523,
2.59908193199888));
#246973=CARTESIAN_POINT('Ctrl Pts',(-58.6268910424078,6.24145541658251,
2.65877685806582));
#246974=CARTESIAN_POINT('Ctrl Pts',(-58.6982507756608,6.2359600096838,2.65878198860266));
#246975=CARTESIAN_POINT('Ctrl Pts',(-58.603224495399,6.34441620808584,2.63872492669796));
#246976=CARTESIAN_POINT('Ctrl Pts',(-58.6433169201089,6.3024974759271,2.69532212015277));
#246977=CARTESIAN_POINT('Ctrl Pts',(-58.7177256636152,6.285367292233,2.68176836726637));
#246978=CARTESIAN_POINT('Ctrl Pts',(-58.6635810738165,6.45770985055656,
2.75442176402258));
#246979=CARTESIAN_POINT('Ctrl Pts',(-58.6966524426403,6.3719183198876,2.79203179920138));
#246980=CARTESIAN_POINT('Ctrl Pts',(-58.7827411889911,6.35432657855795,
2.74885310748179));
#246981=CARTESIAN_POINT('Ctrl Pts',(-58.70677687616,6.48899861096533,2.82866089558398));
#246982=CARTESIAN_POINT('Ctrl Pts',(-58.7342263230558,6.38003592347143,
2.85316563119172));
#246983=CARTESIAN_POINT('Ctrl Pts',(-58.8271002111739,6.37452670784941,
2.7918975179661));
#246984=CARTESIAN_POINT('Ctrl Pts',(-58.7519447039089,6.49374646112721,
2.90134173516027));
#246985=CARTESIAN_POINT('Ctrl Pts',(-58.7656442740271,6.36806742857306,
2.90103711553233));
#246986=CARTESIAN_POINT('Ctrl Pts',(-58.8722700234481,6.37927424642558,
2.83404198860265));
#246987=CARTESIAN_POINT('Origin',(-58.8589949086131,6.50557852713735,2.83404198860265));
#246988=CARTESIAN_POINT('Origin',(-61.0544000804056,6.7363249088106,3.56647653971873));
#246989=CARTESIAN_POINT('Origin',(-60.9730100652055,6.72777047351102,3.42473028058489));
#246990=CARTESIAN_POINT('Origin',(-59.0361683443159,6.52420020557762,3.11913648168046));
#246991=CARTESIAN_POINT('Origin',(-59.2133417798937,6.54282188406207,3.40423097483314));
#246992=CARTESIAN_POINT('Ctrl Pts',(-60.6448574988555,6.69328024897434,
3.36123028058485));
#246993=CARTESIAN_POINT('Ctrl Pts',(-60.6581326136904,6.56697596826257,
3.36123028058485));
#246994=CARTESIAN_POINT('Ctrl Pts',(-60.6581326136904,6.56697596826257,
3.23423028058485));
#246995=CARTESIAN_POINT('Ctrl Pts',(-60.7343993681214,6.70245599674945,
3.36123028058485));
#246996=CARTESIAN_POINT('Ctrl Pts',(-60.7475659388568,6.57637578951112,
3.36099641108469));
#246997=CARTESIAN_POINT('Ctrl Pts',(-60.7924070567573,6.58108878091684,
3.23423043688388));
#246998=CARTESIAN_POINT('Ctrl Pts',(-60.819067758858,6.71113417453917,3.41054258905289));
#246999=CARTESIAN_POINT('Ctrl Pts',(-60.8325536871445,6.58530836180369,
3.41008815825983));
#247000=CARTESIAN_POINT('Ctrl Pts',(-60.9193730951243,6.59443344928411,
3.30819867304282));
#247001=CARTESIAN_POINT('Ctrl Pts',(-60.8636883187845,6.71570789669389,
3.48823028058487));
#247002=CARTESIAN_POINT('Ctrl Pts',(-60.8773920302461,6.59002106156445,
3.48794691941603));
#247003=CARTESIAN_POINT('Ctrl Pts',(-60.9862851800405,6.60146619279925,
3.42473028058488));
#247004=CARTESIAN_POINT('Origin',(-60.6448574988555,6.69328024897434,3.23423028058485));
#247005=CARTESIAN_POINT('Ctrl Pts',(-59.1062911958297,6.53099325080035,
3.47153072139076));
#247006=CARTESIAN_POINT('Ctrl Pts',(-59.1200087114583,6.40512264090967,
3.4712274628508));
#247007=CARTESIAN_POINT('Ctrl Pts',(-59.2267768430462,6.41653455700106,
3.40413046676784));
#247008=CARTESIAN_POINT('Ctrl Pts',(-59.2206299794252,6.543134865483,3.6555381345799));
#247009=CARTESIAN_POINT('Ctrl Pts',(-59.2341972766254,6.41712406698062,
3.65520336072206));
#247010=CARTESIAN_POINT('Ctrl Pts',(-59.318224747432,6.42614611919712,3.55128134519965));
#247011=CARTESIAN_POINT('Ctrl Pts',(-59.4260354503639,6.5649460139706,3.77003198860267));
#247012=CARTESIAN_POINT('Ctrl Pts',(-59.4394961352151,6.43870134519708,
3.76980209314093));
#247013=CARTESIAN_POINT('Ctrl Pts',(-59.4825067955808,6.44341285848436,
3.64284195387372));
#247014=CARTESIAN_POINT('Ctrl Pts',(-59.6417962403143,6.58785426247075,
3.77003198860267));
#247015=CARTESIAN_POINT('Ctrl Pts',(-59.6550912403353,6.461360786852,3.77003198860267));
#247016=CARTESIAN_POINT('Ctrl Pts',(-59.6550713402783,6.4615501232472,3.64284189403793));
#247017=CARTESIAN_POINT('Origin',(-59.6417962403143,6.58785426247075,3.64303198860266));
#247018=CARTESIAN_POINT('Origin',(60.0850508448142,-5.99594444118149,3.23423028058478));
#247019=CARTESIAN_POINT('Origin',(-60.4944777170594,6.67747469700925,3.23423028058485));
#247020=CARTESIAN_POINT('Origin',(59.8516078896891,-5.97140859790491,3.64303198860259));
#247021=CARTESIAN_POINT('Origin',(-60.04095383883,6.62985850077774,3.64299171721822));
#247022=CARTESIAN_POINT('Ctrl Pts',(-60.2756459899119,6.65505462397374,
3.48823028058484));
#247023=CARTESIAN_POINT('Ctrl Pts',(-60.2894805317162,6.52822907310757,
3.48852004212262));
#247024=CARTESIAN_POINT('Ctrl Pts',(-60.1796001951996,6.51668018436725,
3.42473028058484));
#247025=CARTESIAN_POINT('Ctrl Pts',(-60.3204176712045,6.65964099131241,
3.41028005848409));
#247026=CARTESIAN_POINT('Ctrl Pts',(-60.3340024654463,6.53290851690435,
3.41074404220402));
#247027=CARTESIAN_POINT('Ctrl Pts',(-60.2467384099271,6.5237366950833,3.30780486243953));
#247028=CARTESIAN_POINT('Ctrl Pts',(-60.4052373806432,6.66833043150632,
3.36123028058485));
#247029=CARTESIAN_POINT('Ctrl Pts',(-60.4184509388145,6.5417844091174,3.36146460586362));
#247030=CARTESIAN_POINT('Ctrl Pts',(-60.3739306632443,6.53710513959992,
3.23423045308403));
#247031=CARTESIAN_POINT('Ctrl Pts',(-60.4944777170594,6.67747469700925,
3.36123028058485));
#247032=CARTESIAN_POINT('Ctrl Pts',(-60.5077528318944,6.55117041629748,
3.36123028058485));
#247033=CARTESIAN_POINT('Ctrl Pts',(-60.5077528318944,6.55117041629748,
3.23423028058485));
#247034=CARTESIAN_POINT('Origin',(-60.1663250803646,6.64298446507902,3.42473028058484));
#247035=CARTESIAN_POINT('Origin',(-60.0854204586811,6.63448104699066,3.56563113524784));
#247036=CARTESIAN_POINT('Origin',(-61.4240753804095,-0.317499999706852,
3.56647653909397));
#247037=CARTESIAN_POINT('Origin',(-61.4683012396086,-0.317551690014747,
3.64299466007431));
#247038=CARTESIAN_POINT('Origin',(-61.3422370451705,-0.317499999999815,
3.42473028058483));
#247039=CARTESIAN_POINT('Ctrl Pts',(-61.2322532920972,-0.316930737395729,
3.48823028058483));
#247040=CARTESIAN_POINT('Ctrl Pts',(-61.2327440814645,-0.190499999999815,
3.48794691941599));
#247041=CARTESIAN_POINT('Ctrl Pts',(-61.3422370451705,-0.190499999999815,
3.42473028058484));
#247042=CARTESIAN_POINT('Ctrl Pts',(-61.1872475084174,-0.317046579199451,
3.41028005925088));
#247043=CARTESIAN_POINT('Ctrl Pts',(-61.187506454176,-0.190499999998209,
3.4098251223097));
#247044=CARTESIAN_POINT('Ctrl Pts',(-61.274729039531,-0.190499999999814,
3.30780486372827));
#247045=CARTESIAN_POINT('Ctrl Pts',(-61.1019842137032,-0.317266596913308,
3.3612302805848));
#247046=CARTESIAN_POINT('Ctrl Pts',(-61.1018997758106,-0.190499999999807,
3.36099721048453));
#247047=CARTESIAN_POINT('Ctrl Pts',(-61.1468362071711,-0.190499999999813,
3.23423045308374));
#247048=CARTESIAN_POINT('Ctrl Pts',(-61.0122769227456,-0.317499999999814,
3.3612302805848));
#247049=CARTESIAN_POINT('Ctrl Pts',(-61.0122769227456,-0.190499999999814,
3.3612302805848));
#247050=CARTESIAN_POINT('Ctrl Pts',(-61.0122769227456,-0.190499999999813,
3.2342302805848));
#247051=CARTESIAN_POINT('Origin',(-61.0122769227456,-0.317499999999813,
3.2342302805848));
#247052=CARTESIAN_POINT('Origin',(5.50819412990574E-15,-0.317499999999816,
3.64303198860262));
#247053=CARTESIAN_POINT('Origin',(-61.8696548221181,-0.317499999999816,
3.64303198860261));
#247054=CARTESIAN_POINT('Origin',(5.56576032196012E-15,-0.317499999999813,
3.23423028058481));
#247055=CARTESIAN_POINT('Origin',(-60.8610688070707,-0.317499999999813,
3.2342302805848));
#247056=CARTESIAN_POINT('Ctrl Pts',(-62.4081695979768,-0.318048871876944,
3.4715307213907));
#247057=CARTESIAN_POINT('Ctrl Pts',(-62.4086377819835,-0.190309034175174,
3.47182327902661));
#247058=CARTESIAN_POINT('Ctrl Pts',(-62.3003077603771,-0.190500142124869,
3.40413028959024));
#247059=CARTESIAN_POINT('Ctrl Pts',(-62.2931881445371,-0.317932489889758,
3.65553807120955));
#247060=CARTESIAN_POINT('Ctrl Pts',(-62.2934975005736,-0.190309294367597,
3.65586275496964));
#247061=CARTESIAN_POINT('Ctrl Pts',(-62.208356400327,-0.190500141995283,
3.55128126837315));
#247062=CARTESIAN_POINT('Ctrl Pts',(-62.0866281564673,-0.317722686167228,
3.77003198860262));
#247063=CARTESIAN_POINT('Ctrl Pts',(-62.0868143053089,-0.190309769569541,
3.77025505748483));
#247064=CARTESIAN_POINT('Ctrl Pts',(-62.0431695205374,-0.190500141761682,
3.64284211731126));
#247065=CARTESIAN_POINT('Ctrl Pts',(-61.8696548221181,-0.317499999999817,
3.77003198860262));
#247066=CARTESIAN_POINT('Ctrl Pts',(-61.8696548221181,-0.190310267888814,
3.77003198860262));
#247067=CARTESIAN_POINT('Ctrl Pts',(-61.8696548221181,-0.190500141513731,
3.64284239821695));
#247068=CARTESIAN_POINT('Origin',(-62.3004688883554,-0.317499999999815,
3.40423097483308));
#247069=CARTESIAN_POINT('Ctrl Pts',(-60.8610688070707,-0.317499999999814,
3.3612302805848));
#247070=CARTESIAN_POINT('Ctrl Pts',(-60.8610688070707,-0.190499999999814,
3.3612302805848));
#247071=CARTESIAN_POINT('Ctrl Pts',(-60.8610688070707,-0.190499999999813,
3.2342302805848));
#247072=CARTESIAN_POINT('Ctrl Pts',(-60.7710583184321,-0.317734773760083,
3.3612302805848));
#247073=CARTESIAN_POINT('Ctrl Pts',(-60.7709717342411,-0.190499999999814,
3.36146538610122));
#247074=CARTESIAN_POINT('Ctrl Pts',(-60.7260547307361,-0.190499999999813,
3.23423043688408));
#247075=CARTESIAN_POINT('Ctrl Pts',(-60.6859465754578,-0.317958617918848,
3.41054258693099));
#247076=CARTESIAN_POINT('Ctrl Pts',(-60.6862105562575,-0.190499999999749,
3.41100608859814));
#247077=CARTESIAN_POINT('Ctrl Pts',(-60.5983892955404,-0.190499999999814,
3.3081986697084));
#247078=CARTESIAN_POINT('Ctrl Pts',(-60.6410923272405,-0.318076890623181,
3.48823028058479));
#247079=CARTESIAN_POINT('Ctrl Pts',(-60.6415942020421,-0.190499999999815,
3.48852004212257));
#247080=CARTESIAN_POINT('Ctrl Pts',(-60.5311086139135,-0.190499999999815,
3.42473028058479));
#247081=CARTESIAN_POINT('Origin',(-60.5311086139134,-0.317499999999815,
3.42473028058479));
#247082=CARTESIAN_POINT('Origin',(-62.4786179998484,-0.317499999977906,
3.11913648178393));
#247083=CARTESIAN_POINT('Origin',(-62.6567671111299,-0.31749999999981,2.8340419886026));
#247084=CARTESIAN_POINT('Origin',(-60.4497583458792,-0.317499999992805,
3.56563113460798));
#247085=CARTESIAN_POINT('Origin',(-60.4050521322801,-0.317550804320556,
3.64299171721764));
#247086=CARTESIAN_POINT('Ctrl Pts',(-62.9541448057648,-0.0152661173106757,
2.59908173516023));
#247087=CARTESIAN_POINT('Ctrl Pts',(-62.9168399481843,-0.0152570710384434,
2.65878198860261));
#247088=CARTESIAN_POINT('Ctrl Pts',(-62.8464427007196,-0.0152399999998093,
2.65878198860261));
#247089=CARTESIAN_POINT('Ctrl Pts',(-62.9541233134298,-0.103381504925207,
2.59908193475622));
#247090=CARTESIAN_POINT('Ctrl Pts',(-62.9168211560341,-0.0794415635235094,
2.65878715325368));
#247091=CARTESIAN_POINT('Ctrl Pts',(-62.8464212442881,-0.0662446030558591,
2.65878198860261));
#247092=CARTESIAN_POINT('Ctrl Pts',(-62.9290872705828,-0.184683583687337,
2.63878778849871));
#247093=CARTESIAN_POINT('Ctrl Pts',(-62.8936771137448,-0.138547994783951,
2.69564460180094));
#247094=CARTESIAN_POINT('Ctrl Pts',(-62.8213855864655,-0.113305567451219,
2.68180481624873));
#247095=CARTESIAN_POINT('Ctrl Pts',(-62.8564203507741,-0.291340992631772,
2.75443238878643));
#247096=CARTESIAN_POINT('Ctrl Pts',(-62.8329175802742,-0.201910351191337,
2.79268340777113));
#247097=CARTESIAN_POINT('Ctrl Pts',(-62.7487193609389,-0.175042741957798,
2.74885926835618));
#247098=CARTESIAN_POINT('Ctrl Pts',(-62.8099434033762,-0.318045276842425,
2.82856655361668));
#247099=CARTESIAN_POINT('Ctrl Pts',(-62.7947175425039,-0.205831635642229,
2.8538419723101));
#247100=CARTESIAN_POINT('Ctrl Pts',(-62.7022409210457,-0.190499999999808,
2.79184624278614));
#247101=CARTESIAN_POINT('Ctrl Pts',(-62.7644678366119,-0.318045750792856,
2.90134173516021));
#247102=CARTESIAN_POINT('Ctrl Pts',(-62.7649326510149,-0.190499999999814,
2.90163218716389));
#247103=CARTESIAN_POINT('Ctrl Pts',(-62.6567671111299,-0.190499999999811,
2.8340419886026));
#247104=CARTESIAN_POINT('Origin',(5.50819412990574E-15,-0.317499999999816,
3.64303198860262));
#247105=CARTESIAN_POINT('Origin',(-60.003690522373,-0.317499999999816,3.64303198860261));
#247106=CARTESIAN_POINT('Ctrl Pts',(-60.003690522373,-0.317499999999817,
3.77003198860262));
#247107=CARTESIAN_POINT('Ctrl Pts',(-60.003690522373,-0.190309748265136,
3.77003198860262));
#247108=CARTESIAN_POINT('Ctrl Pts',(-60.003690522373,-0.190500142289345,
3.64284187937063));
#247109=CARTESIAN_POINT('Ctrl Pts',(-59.7867137603524,-0.317270385524247,
3.77003198860262));
#247110=CARTESIAN_POINT('Ctrl Pts',(-59.7869045527985,-0.19031026247621,
3.76980208962919));
#247111=CARTESIAN_POINT('Ctrl Pts',(-59.8301727552496,-0.190500142032278,
3.64284193928308));
#247112=CARTESIAN_POINT('Ctrl Pts',(-59.5801552670728,-0.317049440713426,
3.65553535416585));
#247113=CARTESIAN_POINT('Ctrl Pts',(-59.5804765271849,-0.19031076108168,
3.65520057834448));
#247114=CARTESIAN_POINT('Ctrl Pts',(-59.6649871046547,-0.190500141784922,
3.55127910964229));
#247115=CARTESIAN_POINT('Ctrl Pts',(-59.4651754363832,-0.316925998272862,
3.47153072139072));
#247116=CARTESIAN_POINT('Ctrl Pts',(-59.4656607446594,-0.190311035334875,
3.47122746281582));
#247117=CARTESIAN_POINT('Ctrl Pts',(-59.5730368716575,-0.190500141646717,
3.40413045901282));
#247118=CARTESIAN_POINT('Origin',(-59.5728760150042,-0.317499999999815,
3.40423097483309));
#247119=CARTESIAN_POINT('Ctrl Pts',(-62.7644678366119,0.318045750793234,
2.90134173516022));
#247120=CARTESIAN_POINT('Ctrl Pts',(-62.7649326510149,0.190500000000189,
2.9016321871639));
#247121=CARTESIAN_POINT('Ctrl Pts',(-62.6567671111299,0.190500000000189,
2.83404198860261));
#247122=CARTESIAN_POINT('Ctrl Pts',(-62.8099640589334,0.318045262795371,
2.8285334983536));
#247123=CARTESIAN_POINT('Ctrl Pts',(-62.7947344577641,0.205840330723214,
2.85381483162463));
#247124=CARTESIAN_POINT('Ctrl Pts',(-62.7022616416344,0.19050000000019,
2.7918270159431));
#247125=CARTESIAN_POINT('Ctrl Pts',(-62.8562601188215,0.291334117855617,
2.75468822073633));
#247126=CARTESIAN_POINT('Ctrl Pts',(-62.8328016940824,0.201836550627952,
2.79286913083856));
#247127=CARTESIAN_POINT('Ctrl Pts',(-62.7485591297232,0.175038734052367,
2.74900763297916));
#247128=CARTESIAN_POINT('Ctrl Pts',(-62.928611257107,0.185622189560568,
2.63954450640401));
#247129=CARTESIAN_POINT('Ctrl Pts',(-62.8932808767899,0.139140156000274,
2.69627684028842));
#247130=CARTESIAN_POINT('Ctrl Pts',(-62.8209095783125,0.113848895265888,
2.68224356036486));
#247131=CARTESIAN_POINT('Ctrl Pts',(-62.9541233349672,0.103673266463023,
2.59908178706383));
#247132=CARTESIAN_POINT('Ctrl Pts',(-62.9168211653022,0.0796882264538794,
2.65878704321555));
#247133=CARTESIAN_POINT('Ctrl Pts',(-62.8464212664863,0.0664134143653284,
2.6587819886026));
#247134=CARTESIAN_POINT('Ctrl Pts',(-62.9541448057648,0.0152661173110572,
2.59908173516022));
#247135=CARTESIAN_POINT('Ctrl Pts',(-62.9168399481843,0.0152570710388243,
2.6587819886026));
#247136=CARTESIAN_POINT('Ctrl Pts',(-62.8464427007196,0.0152400000001903,
2.6587819886026));
#247137=CARTESIAN_POINT('Origin',(-62.6567671111299,0.317500000000189,2.83404198860261));
#247138=CARTESIAN_POINT('Origin',(-59.3947266586247,-0.317499999970537,
3.11913648167064));
#247139=CARTESIAN_POINT('Origin',(-59.2165773020941,-0.31749999999981,2.83404198860261));
#247140=CARTESIAN_POINT('Origin',(-62.4786179998343,0.317499999978364,3.11913648177509));
#247141=CARTESIAN_POINT('Origin',(-62.3004688883554,0.317500000000185,3.40423097483309));
#247142=CARTESIAN_POINT('Ctrl Pts',(-59.1088767419348,-0.3169225446755,
2.90134173516022));
#247143=CARTESIAN_POINT('Ctrl Pts',(-59.1093642282366,-0.190499999999805,
2.90103711553229));
#247144=CARTESIAN_POINT('Ctrl Pts',(-59.2165773020941,-0.190499999999811,
2.83404198860261));
#247145=CARTESIAN_POINT('Ctrl Pts',(-59.0634407053229,-0.316922012808971,
2.82862991747963));
#247146=CARTESIAN_POINT('Ctrl Pts',(-59.0793536643041,-0.205694973741207,
2.85314045886453));
#247147=CARTESIAN_POINT('Ctrl Pts',(-59.1711393827293,-0.19049999999981,
2.79187960999928));
#247148=CARTESIAN_POINT('Ctrl Pts',(-59.0174076205275,-0.290332993454825,
2.75470625793324));
#247149=CARTESIAN_POINT('Ctrl Pts',(-59.0412846811395,-0.201480151665693,
2.79224250381906));
#247150=CARTESIAN_POINT('Ctrl Pts',(-59.1251084688121,-0.175054909459551,
2.74901809108263));
#247151=CARTESIAN_POINT('Ctrl Pts',(-58.9458296250063,-0.184894967401365,
2.63947868311699));
#247152=CARTESIAN_POINT('Ctrl Pts',(-58.9812445774292,-0.138672156931012,
2.69595066767904));
#247153=CARTESIAN_POINT('Ctrl Pts',(-59.0535312451933,-0.113807322597554,
2.68220539436056));
#247154=CARTESIAN_POINT('Ctrl Pts',(-58.9208287018092,-0.103171606455547,
2.59908178585108));
#247155=CARTESIAN_POINT('Ctrl Pts',(-58.9581363848291,-0.0793367652456228,
2.65877670944851));
#247156=CARTESIAN_POINT('Ctrl Pts',(-59.0285307646525,-0.0663350652341827,
2.65878198860261));
#247157=CARTESIAN_POINT('Ctrl Pts',(-58.9208513795073,-0.0152121934557294,
2.59908173516023));
#247158=CARTESIAN_POINT('Ctrl Pts',(-58.9581562369413,-0.0152218248289167,
2.65878198860261));
#247159=CARTESIAN_POINT('Ctrl Pts',(-59.0285534841296,-0.0152399999998097,
2.65878198860261));
#247160=CARTESIAN_POINT('Ctrl Pts',(-61.8696548221181,0.317500000000183,
3.77003198860263));
#247161=CARTESIAN_POINT('Ctrl Pts',(-61.8696548221181,0.19031025693173,
3.77003198860263));
#247162=CARTESIAN_POINT('Ctrl Pts',(-61.8696548221181,0.190500141530432,
3.64284238727587));
#247163=CARTESIAN_POINT('Ctrl Pts',(-62.086631532412,0.317722689632413,
3.77003198860263));
#247164=CARTESIAN_POINT('Ctrl Pts',(-62.0868176889521,0.190309758575909,
3.77025506105731));
#247165=CARTESIAN_POINT('Ctrl Pts',(-62.0431722165663,0.190500141778416,
3.64284210641793));
#247166=CARTESIAN_POINT('Ctrl Pts',(-62.2931898887681,0.317932491655863,
3.65553527987828));
#247167=CARTESIAN_POINT('Ctrl Pts',(-62.2934992458064,0.190309283350215,
3.65585996533176));
#247168=CARTESIAN_POINT('Ctrl Pts',(-62.2083577878509,0.190500142012043,
3.55127902710248));
#247169=CARTESIAN_POINT('Ctrl Pts',(-62.4081695979768,0.318048871877314,
3.47153072139072));
#247170=CARTESIAN_POINT('Ctrl Pts',(-62.4086377820239,0.190309023146808,
3.47182327905188));
#247171=CARTESIAN_POINT('Ctrl Pts',(-62.3003077510786,0.190500142141644,
3.40413028377981));
#247172=CARTESIAN_POINT('Origin',(-61.8696548221181,0.317500000000184,3.64303198860263));
#247173=CARTESIAN_POINT('Origin',(62.2224557307631,0.317500000000184,3.64303198860263));
#247174=CARTESIAN_POINT('Origin',(-61.4683012396086,0.317551690015293,3.64299466007411));
#247175=CARTESIAN_POINT('Ctrl Pts',(-58.9208513795073,0.015212193456111,
2.59908173516023));
#247176=CARTESIAN_POINT('Ctrl Pts',(-58.9581562369413,0.0152218248292975,
2.65878198860261));
#247177=CARTESIAN_POINT('Ctrl Pts',(-59.0285534841296,0.0152400000001907,
2.65878198860261));
#247178=CARTESIAN_POINT('Ctrl Pts',(-58.9208288705614,0.102871702177517,
2.59908193199826));
#247179=CARTESIAN_POINT('Ctrl Pts',(-58.9581365422946,0.0790852439334556,
2.65877685806665));
#247180=CARTESIAN_POINT('Ctrl Pts',(-59.0285309330208,0.0661608181926717,
2.65878198860261));
#247181=CARTESIAN_POINT('Ctrl Pts',(-58.9453619764183,0.183955833237801,
2.63872492669805));
#247182=CARTESIAN_POINT('Ctrl Pts',(-58.9808530699758,0.138075936736365,
2.69532212015272));
#247183=CARTESIAN_POINT('Ctrl Pts',(-59.0530636028226,0.113261762368398,
2.6817683672664));
#247184=CARTESIAN_POINT('Ctrl Pts',(-59.0172303255293,0.290319860890742,
2.7544217640224));
#247185=CARTESIAN_POINT('Ctrl Pts',(-59.0411528690725,0.201541405841922,
2.79203179920141));
#247186=CARTESIAN_POINT('Ctrl Pts',(-59.1249311745757,0.175047309551329,
2.74885310748167));
#247187=CARTESIAN_POINT('Ctrl Pts',(-59.0634600627912,0.316922027357541,
2.82866089558407));
#247188=CARTESIAN_POINT('Ctrl Pts',(-59.0793694364673,0.205687000366578,
2.85316563119202));
#247189=CARTESIAN_POINT('Ctrl Pts',(-59.1711586818655,0.190500000000188,
2.79189751796659));
#247190=CARTESIAN_POINT('Ctrl Pts',(-59.1088767419348,0.316922544675878,
2.90134173516021));
#247191=CARTESIAN_POINT('Ctrl Pts',(-59.1093642282366,0.190500000000191,
2.90103711553228));
#247192=CARTESIAN_POINT('Ctrl Pts',(-59.2165773020941,0.190500000000189,
2.8340419886026));
#247193=CARTESIAN_POINT('Origin',(-59.2165773020941,0.317500000000189,2.83404198860261));
#247194=CARTESIAN_POINT('Origin',(-61.4240753793289,0.317499999995613,3.56647653971782));
#247195=CARTESIAN_POINT('Origin',(-61.3422370451705,0.317500000000185,3.42473028058485));
#247196=CARTESIAN_POINT('Origin',(-59.3947266586075,0.317499999970762,3.11913648168139));
#247197=CARTESIAN_POINT('Origin',(-59.5728760150042,0.317500000000185,3.4042309748331));
#247198=CARTESIAN_POINT('Ctrl Pts',(-61.0122769227456,0.317500000000186,
3.36123028058481));
#247199=CARTESIAN_POINT('Ctrl Pts',(-61.0122769227456,0.190500000000186,
3.36123028058481));
#247200=CARTESIAN_POINT('Ctrl Pts',(-61.0122769227456,0.190500000000187,
3.23423028058481));
#247201=CARTESIAN_POINT('Ctrl Pts',(-61.1022873990971,0.317265808076579,
3.36123028058481));
#247202=CARTESIAN_POINT('Ctrl Pts',(-61.1022028716701,0.190500000000177,
3.36099641108414));
#247203=CARTESIAN_POINT('Ctrl Pts',(-61.1472909869831,0.190500000000187,
3.23423043688322));
#247204=CARTESIAN_POINT('Ctrl Pts',(-61.1873990841185,0.317046189129288,
3.41054258905284));
#247205=CARTESIAN_POINT('Ctrl Pts',(-61.1876587562329,0.190500000000658,
3.41008815826044));
#247206=CARTESIAN_POINT('Ctrl Pts',(-61.2749563897845,0.190500000000186,
3.30819867304323));
#247207=CARTESIAN_POINT('Ctrl Pts',(-61.2322532920972,0.316930737396099,
3.48823028058483));
#247208=CARTESIAN_POINT('Ctrl Pts',(-61.2327440814645,0.190500000000185,
3.48794691941599));
#247209=CARTESIAN_POINT('Ctrl Pts',(-61.3422370451705,0.190500000000185,
3.42473028058484));
#247210=CARTESIAN_POINT('Origin',(-61.0122769227456,0.317500000000187,3.23423028058481));
#247211=CARTESIAN_POINT('Ctrl Pts',(-59.4651754363832,0.316925998273232,
3.47153072139073));
#247212=CARTESIAN_POINT('Ctrl Pts',(-59.4656607446034,0.190311049925318,
3.47122746285077));
#247213=CARTESIAN_POINT('Ctrl Pts',(-59.573036859247,0.190500141625231,
3.40413046676793));
#247214=CARTESIAN_POINT('Ctrl Pts',(-59.5801570044831,0.317049442579369,
3.65553813457986));
#247215=CARTESIAN_POINT('Ctrl Pts',(-59.580478263487,0.190310775687526,
3.65520336072214));
#247216=CARTESIAN_POINT('Ctrl Pts',(-59.6649884842716,0.190500141763417,
3.55128134519983));
#247217=CARTESIAN_POINT('Ctrl Pts',(-59.7867171285936,0.317270389089027,
3.77003198860263));
#247218=CARTESIAN_POINT('Ctrl Pts',(-59.7869079131821,0.190310277118411,
3.76980209314073));
#247219=CARTESIAN_POINT('Ctrl Pts',(-59.8301754438925,0.190500142010734,
3.64284195387335));
#247220=CARTESIAN_POINT('Ctrl Pts',(-60.003690522373,0.317500000000183,
3.77003198860263));
#247221=CARTESIAN_POINT('Ctrl Pts',(-60.003690522373,0.190309762955,3.77003198860263));
#247222=CARTESIAN_POINT('Ctrl Pts',(-60.003690522373,0.190500142267757,
3.64284189403812));
#247223=CARTESIAN_POINT('Origin',(-60.0036905223731,0.317500000000184,3.64303198860262));
#247224=CARTESIAN_POINT('Origin',(60.71525,0.317500000000187,3.23423028058482));
#247225=CARTESIAN_POINT('Origin',(-60.8610688070707,0.317500000000187,3.23423028058481));
#247226=CARTESIAN_POINT('Origin',(60.4792282238308,0.317500000000184,3.64303198860263));
#247227=CARTESIAN_POINT('Origin',(-60.4050521322799,0.317550804321294,3.64299171721729));
#247228=CARTESIAN_POINT('Ctrl Pts',(-60.6410923272405,0.318076890623551,
3.4882302805848));
#247229=CARTESIAN_POINT('Ctrl Pts',(-60.6415942020421,0.190500000000185,
3.48852004212258));
#247230=CARTESIAN_POINT('Ctrl Pts',(-60.5311086139134,0.190500000000185,
3.4247302805848));
#247231=CARTESIAN_POINT('Ctrl Pts',(-60.6860981505083,0.317958218318944,
3.41028005848407));
#247232=CARTESIAN_POINT('Ctrl Pts',(-60.68636137503,0.19049999999811,3.41074404220421));
#247233=CARTESIAN_POINT('Ctrl Pts',(-60.5986166446967,0.190500000000186,
3.30780486243976));
#247234=CARTESIAN_POINT('Ctrl Pts',(-60.771361502534,0.317733982967741,
3.36123028058481));
#247235=CARTESIAN_POINT('Ctrl Pts',(-60.7712750141981,0.190500000000186,
3.36146460586327));
#247236=CARTESIAN_POINT('Ctrl Pts',(-60.7265095085042,0.190500000000187,
3.2342304530835));
#247237=CARTESIAN_POINT('Ctrl Pts',(-60.8610688070707,0.317500000000186,
3.36123028058481));
#247238=CARTESIAN_POINT('Ctrl Pts',(-60.8610688070707,0.190500000000186,
3.36123028058481));
#247239=CARTESIAN_POINT('Ctrl Pts',(-60.8610688070707,0.190500000000187,
3.23423028058481));
#247240=CARTESIAN_POINT('Origin',(-60.5311086139135,0.317500000000185,3.4247302805848));
#247241=CARTESIAN_POINT('Origin',(-60.4497583469882,0.317500000300915,3.56563113524826));
#247242=CARTESIAN_POINT('Origin',(-61.0544000815108,-6.73632490863893,3.56647653909441));
#247243=CARTESIAN_POINT('Origin',(-61.0983782637178,-6.74099917688073,3.64299466007533));
#247244=CARTESIAN_POINT('Origin',(-60.9730100652054,-6.72777047351147,3.42473028058479));
#247245=CARTESIAN_POINT('Ctrl Pts',(-60.8636883187844,-6.71570789669434,
3.48823028058478));
#247246=CARTESIAN_POINT('Ctrl Pts',(-60.877392030246,-6.59002106156489,
3.48794691941594));
#247247=CARTESIAN_POINT('Ctrl Pts',(-60.9862851800404,-6.60146619279971,
3.42473028058479));
#247248=CARTESIAN_POINT('Ctrl Pts',(-60.8189169727308,-6.71111871849892,
3.41028005925082));
#247249=CARTESIAN_POINT('Ctrl Pts',(-60.8324022194101,-6.58529244190266,
3.40982512231079));
#247250=CARTESIAN_POINT('Ctrl Pts',(-60.9191469903169,-6.5944096847117,
3.30780486372924));
#247251=CARTESIAN_POINT('Ctrl Pts',(-60.7340977611528,-6.70242508976285,
3.36123028058476));
#247252=CARTESIAN_POINT('Ctrl Pts',(-60.7472645033911,-6.57634410736815,
3.36099721048396));
#247253=CARTESIAN_POINT('Ctrl Pts',(-60.7919547682784,-6.58104124348259,
3.23423045308317));
#247254=CARTESIAN_POINT('Ctrl Pts',(-60.6448574988554,-6.69328024897479,
3.36123028058476));
#247255=CARTESIAN_POINT('Ctrl Pts',(-60.6581326136904,-6.56697596826302,
3.36123028058476));
#247256=CARTESIAN_POINT('Ctrl Pts',(-60.6581326136904,-6.56697596826301,
3.23423028058476));
#247257=CARTESIAN_POINT('Origin',(-60.6448574988554,-6.69328024897478,3.23423028058476));
#247258=CARTESIAN_POINT('Origin',(0.0331877870874877,-0.315760701779243,
3.64303198860262));
#247259=CARTESIAN_POINT('Origin',(-61.4975385923862,-6.78290064323585,3.64303198860257));
#247260=CARTESIAN_POINT('Origin',(0.0331877870874878,-0.31576070177924,
3.23423028058481));
#247261=CARTESIAN_POINT('Origin',(-60.4944777170593,-6.67747469700969,3.23423028058476));
#247262=CARTESIAN_POINT('Ctrl Pts',(-62.0330459552232,-6.83973663030285,
3.47153072139065));
#247263=CARTESIAN_POINT('Ctrl Pts',(-62.0468640234019,-6.71274550335289,
3.47182327902656));
#247264=CARTESIAN_POINT('Ctrl Pts',(-61.9391074687688,-6.70161199370852,
3.40413028959046));
#247265=CARTESIAN_POINT('Ctrl Pts',(-61.9187065474464,-6.82760205123647,
3.65553807120948));
#247266=CARTESIAN_POINT('Ctrl Pts',(-61.9323544653005,-6.70071032544166,
3.65586275496829));
#247267=CARTESIAN_POINT('Ctrl Pts',(-61.8476598278987,-6.69200045921773,
3.55128126837219));
#247268=CARTESIAN_POINT('Ctrl Pts',(-61.7133000470646,-6.80580199871468,
3.77003198860258));
#247269=CARTESIAN_POINT('Ctrl Pts',(-61.7268034525382,-6.67910652125862,
3.77025505748531));
#247270=CARTESIAN_POINT('Ctrl Pts',(-61.683377859153,-6.67473372828988,
3.6428421173117));
#247271=CARTESIAN_POINT('Ctrl Pts',(-61.4975385923862,-6.78290064323585,
3.77003198860258));
#247272=CARTESIAN_POINT('Ctrl Pts',(-61.5108335396271,-6.65640766978592,
3.77003198860258));
#247273=CARTESIAN_POINT('Ctrl Pts',(-61.5108136924289,-6.65659650326277,
3.64284239821739));
#247274=CARTESIAN_POINT('Origin',(-61.9259926140919,-6.82793297553373,3.40423097483304));
#247275=CARTESIAN_POINT('Ctrl Pts',(-60.4944777170593,-6.67747469700969,
3.36123028058476));
#247276=CARTESIAN_POINT('Ctrl Pts',(-60.5077528318943,-6.55117041629792,
3.36123028058476));
#247277=CARTESIAN_POINT('Ctrl Pts',(-60.5077528318943,-6.55117041629792,
3.23423028058476));
#247278=CARTESIAN_POINT('Ctrl Pts',(-60.404935774755,-6.6682995265994,3.36123028058476));
#247279=CARTESIAN_POINT('Ctrl Pts',(-60.4181493202581,-6.54175270773036,
3.36146538610052));
#247280=CARTESIAN_POINT('Ctrl Pts',(-60.3734783767987,-6.53705760237938,
3.23423043688339));
#247281=CARTESIAN_POINT('Ctrl Pts',(-60.3202668847282,-6.65962554481726,
3.41054258693096));
#247282=CARTESIAN_POINT('Ctrl Pts',(-60.333852472873,-6.53289275204893,
3.41100608859807));
#247283=CARTESIAN_POINT('Ctrl Pts',(-60.2465123062101,-6.52371293062548,
3.30819866970814));
#247284=CARTESIAN_POINT('Ctrl Pts',(-60.2756459899118,-6.65505462397419,
3.48823028058475));
#247285=CARTESIAN_POINT('Ctrl Pts',(-60.2894805317161,-6.52822907310801,
3.48852004212253));
#247286=CARTESIAN_POINT('Ctrl Pts',(-60.1796001951995,-6.51668018436769,
3.42473028058475));
#247287=CARTESIAN_POINT('Origin',(-60.1663250803645,-6.64298446507947,3.42473028058476));
#247288=CARTESIAN_POINT('Origin',(-62.1031658061158,-6.84655462836542,3.11913648178459));
#247289=CARTESIAN_POINT('Origin',(-62.2803389979219,-6.86517628122534,2.83404198860255));
#247290=CARTESIAN_POINT('Origin',(-60.0854204576107,-6.63448104656949,3.56563113460775));
#247291=CARTESIAN_POINT('Origin',(-60.0409538388298,-6.62985850077836,3.642991717218));
#247292=CARTESIAN_POINT('Ctrl Pts',(-62.6076796697354,-6.5956825007991,
2.59908173516018));
#247293=CARTESIAN_POINT('Ctrl Pts',(-62.5705801176609,-6.59177408464798,
2.65878198860256));
#247294=CARTESIAN_POINT('Ctrl Pts',(-62.500570298093,-6.58439859103053,
2.65878198860256));
#247295=CARTESIAN_POINT('Ctrl Pts',(-62.5984477290795,-6.68331293653973,
2.59908193475685));
#247296=CARTESIAN_POINT('Ctrl Pts',(-62.5638523220891,-6.65560500345264,
2.65878715325316));
#247297=CARTESIAN_POINT('Ctrl Pts',(-62.495217526425,-6.63512154272647,
2.65878198860256));
#247298=CARTESIAN_POINT('Ctrl Pts',(-62.5650504549418,-6.76155265492275,
2.63878778849855));
#247299=CARTESIAN_POINT('Ctrl Pts',(-62.5346567608586,-6.71196843232427,
2.69564460180106));
#247300=CARTESIAN_POINT('Ctrl Pts',(-62.4653998062675,-6.67930776339584,
2.68180481624875));
#247301=CARTESIAN_POINT('Ctrl Pts',(-62.4816328770699,-6.86003002196304,
2.75443238878649));
#247302=CARTESIAN_POINT('Ctrl Pts',(-62.4676069047243,-6.76863258245081,
2.79268340777087));
#247303=CARTESIAN_POINT('Ctrl Pts',(-62.3866783619495,-6.73311104631488,
2.74885926835607));
#247304=CARTESIAN_POINT('Ctrl Pts',(-62.4326191774618,-6.88172985342201,
2.82856655361655));
#247305=CARTESIAN_POINT('Ctrl Pts',(-62.4292062449166,-6.7685393944507,
2.85384197230759));
#247306=CARTESIAN_POINT('Ctrl Pts',(-62.3388388123826,-6.74362530798286,
2.79184624278463));
#247307=CARTESIAN_POINT('Ctrl Pts',(-62.3873926810691,-6.87697683366589,
2.90134173516017));
#247308=CARTESIAN_POINT('Ctrl Pts',(-62.4011871104968,-6.75017837817627,
2.90163218716385));
#247309=CARTESIAN_POINT('Ctrl Pts',(-62.2936141127569,-6.73887200051357,
2.83404198860256));
#247310=CARTESIAN_POINT('Origin',(-62.500570298093,-6.58439859103053,2.53178198860256));
#247311=CARTESIAN_POINT('Origin',(0.0331877870874877,-0.315760701779243,
3.64303198860262));
#247312=CARTESIAN_POINT('Origin',(-59.6417962403142,-6.58785426247119,3.64303198860257));
#247313=CARTESIAN_POINT('Origin',(1.33778643725275E-16,1.9159467040135E-13,
2.53178198860262));
#247314=CARTESIAN_POINT('Origin',(-62.5037563256534,-6.5540855636597,2.53178198860256));
#247315=CARTESIAN_POINT('Ctrl Pts',(-59.6417962403142,-6.58785426247119,
3.77003198860258));
#247316=CARTESIAN_POINT('Ctrl Pts',(-59.6550912418707,-6.46136077224357,
3.77003198860258));
#247317=CARTESIAN_POINT('Ctrl Pts',(-59.6550713402759,-6.46155012326947,
3.64284187937051));
#247318=CARTESIAN_POINT('Ctrl Pts',(-59.4260321009468,-6.56494565834898,
3.77003198860258));
#247319=CARTESIAN_POINT('Ctrl Pts',(-59.4394927947708,-6.43870097938016,
3.76980208962867));
#247320=CARTESIAN_POINT('Ctrl Pts',(-59.4825041216629,-6.44341257746673,
3.6428419392824));
#247321=CARTESIAN_POINT('Ctrl Pts',(-59.2206282517276,-6.54313468201961,
3.65553535416582));
#247322=CARTESIAN_POINT('Ctrl Pts',(-59.2341955513614,-6.41712387095958,
3.65520057834495));
#247323=CARTESIAN_POINT('Ctrl Pts',(-59.3182233753721,-6.42614597501026,
3.55127910964254));
#247324=CARTESIAN_POINT('Ctrl Pts',(-59.1062911958296,-6.53099325080078,
3.47153072139067));
#247325=CARTESIAN_POINT('Ctrl Pts',(-59.1200087130388,-6.40512262640595,
3.47122746281577));
#247326=CARTESIAN_POINT('Ctrl Pts',(-59.2267768553863,-6.41653455832047,
3.40413045901273));
#247327=CARTESIAN_POINT('Origin',(-59.2133417798936,-6.5428218840625,3.40423097483305));
#247328=CARTESIAN_POINT('Ctrl Pts',(-62.4538823482275,-6.24436990788084,
2.90134173516018));
#247329=CARTESIAN_POINT('Ctrl Pts',(-62.4410124550018,-6.37126553604095,
2.90163218716386));
#247330=CARTESIAN_POINT('Ctrl Pts',(-62.3334394572618,-6.35995915837826,
2.83404198860256));
#247331=CARTESIAN_POINT('Ctrl Pts',(-62.4991292864732,-6.2491260434095,
2.82853349835336));
#247332=CARTESIAN_POINT('Ctrl Pts',(-62.4722545055301,-6.3591243783159,
2.853814831623));
#247333=CARTESIAN_POINT('Ctrl Pts',(-62.378684763968,-6.36471463173897,
2.79182701594267));
#247334=CARTESIAN_POINT('Ctrl Pts',(-62.5423796567682,-6.28053011789769,
2.75468822073656));
#247335=CARTESIAN_POINT('Ctrl Pts',(-62.5096946965644,-6.3670853349991,
2.79286913083837));
#247336=CARTESIAN_POINT('Ctrl Pts',(-62.4231124872028,-6.38493060453731,
2.74900763297902));
#247337=CARTESIAN_POINT('Ctrl Pts',(-62.6032845425346,-6.39322569848907,
2.63954450640367));
#247338=CARTESIAN_POINT('Ctrl Pts',(-62.5632890102013,-6.43576006824488,
2.69627684028849));
#247339=CARTESIAN_POINT('Ctrl Pts',(-62.4886705126495,-6.45334792019221,
2.6822435603649));
#247340=CARTESIAN_POINT('Ctrl Pts',(-62.6200908675648,-6.47739243510518,
2.59908178706394));
#247341=CARTESIAN_POINT('Ctrl Pts',(-62.5804859237136,-6.4973469440839,
2.65878704321556));
#247342=CARTESIAN_POINT('Ctrl Pts',(-62.5090840872032,-6.50319024212545,
2.65878198860256));
#247343=CARTESIAN_POINT('Ctrl Pts',(-62.6108711573005,-6.56531752495327,
2.59908173516017));
#247344=CARTESIAN_POINT('Ctrl Pts',(-62.5737697140402,-6.56142710223376,
2.65878198860256));
#247345=CARTESIAN_POINT('Ctrl Pts',(-62.5037563256534,-6.55408556365971,
2.65878198860256));
#247346=CARTESIAN_POINT('Origin',(-62.3467145720969,-6.23365487766649,2.83404198860256));
#247347=CARTESIAN_POINT('Origin',(-59.0361683443312,-6.52420020558021,3.1191364816707));
#247348=CARTESIAN_POINT('Origin',(-58.858994908613,-6.50557852713776,2.83404198860257));
#247349=CARTESIAN_POINT('Origin',(-62.1695413802711,-6.21503322485295,3.11913648177538));
#247350=CARTESIAN_POINT('Origin',(-61.9923681882668,-6.19641157197488,3.40423097483306));
#247351=CARTESIAN_POINT('Ctrl Pts',(-58.7519447039088,-6.49374646112762,
2.90134173516018));
#247352=CARTESIAN_POINT('Ctrl Pts',(-58.765644274027,-6.36806742857347,
2.90103711553224));
#247353=CARTESIAN_POINT('Ctrl Pts',(-58.872270023448,-6.37927424642599,
2.83404198860256));
#247354=CARTESIAN_POINT('Ctrl Pts',(-58.7067576262547,-6.48899657309071,
2.82862991747961));
#247355=CARTESIAN_POINT('Ctrl Pts',(-58.7342098038486,-6.38004220452862,
2.85314045886468));
#247356=CARTESIAN_POINT('Ctrl Pts',(-58.8270810177594,-6.37452469054068,
2.79187960999949));
#247357=CARTESIAN_POINT('Ctrl Pts',(-58.6637560248472,-6.45774144355344,
2.75470625793313));
#247358=CARTESIAN_POINT('Ctrl Pts',(-58.6967899354322,-6.37187117938152,
2.79224250381903));
#247359=CARTESIAN_POINT('Ctrl Pts',(-58.7829167175845,-6.35435266912788,
2.74901809108255));
#247360=CARTESIAN_POINT('Ctrl Pts',(-58.6035914159081,-6.34539908016337,
2.63947868311702));
#247361=CARTESIAN_POINT('Ctrl Pts',(-58.6436439608623,-6.30313135363866,
2.69595066767901));
#247362=CARTESIAN_POINT('Ctrl Pts',(-58.7181337176194,-6.28595874576537,
2.68220539436055));
#247363=CARTESIAN_POINT('Ctrl Pts',(-58.587269867717,-6.2615101002575,2.59908178585113));
#247364=CARTESIAN_POINT('Ctrl Pts',(-58.626864594668,-6.24170554357555,
2.65877670944858));
#247365=CARTESIAN_POINT('Ctrl Pts',(-58.6982323944353,-6.23613328458285,
2.65878198860256));
#247366=CARTESIAN_POINT('Ctrl Pts',(-58.596486683455,-6.17403490859042,
2.59908173516018));
#247367=CARTESIAN_POINT('Ctrl Pts',(-58.6335861742241,-6.17794390662193,
2.65878198860256));
#247368=CARTESIAN_POINT('Ctrl Pts',(-58.7035958781038,-6.1853204982942,
2.65878198860256));
#247369=CARTESIAN_POINT('Origin',(-58.7035958781038,-6.1853204982942,2.53178198860256));
#247370=CARTESIAN_POINT('Ctrl Pts',(-61.5639141665611,-6.151379239677,3.77003198860258));
#247371=CARTESIAN_POINT('Ctrl Pts',(-61.5506192181748,-6.27787222402455,
3.77003198860258));
#247372=CARTESIAN_POINT('Ctrl Pts',(-61.5506390665201,-6.27768337963384,
3.64284238727612));
#247373=CARTESIAN_POINT('Ctrl Pts',(-61.7797255331385,-6.17383801205345,
3.77003198860258));
#247374=CARTESIAN_POINT('Ctrl Pts',(-61.7665923920122,-6.30057242039938,
3.7702550610584));
#247375=CARTESIAN_POINT('Ctrl Pts',(-61.7232059145542,-6.29582088597933,
3.64284210641908));
#247376=CARTESIAN_POINT('Ctrl Pts',(-61.985174271489,-6.19522058691269,
3.65553527987829));
#247377=CARTESIAN_POINT('Ctrl Pts',(-61.9721416759926,-6.32217699854317,
3.65585996532999));
#247378=CARTESIAN_POINT('Ctrl Pts',(-61.8874865820152,-6.31308747966684,
3.55127902710126));
#247379=CARTESIAN_POINT('Ctrl Pts',(-62.0995362748658,-6.20712349654488,
3.47153072139067));
#247380=CARTESIAN_POINT('Ctrl Pts',(-62.0866494440659,-6.33421251157708,
3.47182327905183));
#247381=CARTESIAN_POINT('Ctrl Pts',(-61.97893283374,-6.32269886789197,3.40413028377992));
#247382=CARTESIAN_POINT('Origin',(-61.5639141665611,-6.151379239677,3.64303198860258));
#247383=CARTESIAN_POINT('Origin',(3.53633106925806E-16,1.91571303393729E-13,
2.53178198860262));
#247384=CARTESIAN_POINT('Origin',(-58.7067819056642,-6.15500747092338,2.53178198860257));
#247385=CARTESIAN_POINT('Origin',(61.5094129706996,6.78414869068811,3.64303198860268));
#247386=CARTESIAN_POINT('Origin',(-61.1647646440478,-6.10937495961993,3.64299466007541));
#247387=CARTESIAN_POINT('Ctrl Pts',(-58.5996668978648,-6.14377718965343,
2.59908173516018));
#247388=CARTESIAN_POINT('Ctrl Pts',(-58.6367684021392,-6.14766703046192,
2.65878198860256));
#247389=CARTESIAN_POINT('Ctrl Pts',(-58.7067819056642,-6.15500747092338,
2.65878198860256));
#247390=CARTESIAN_POINT('Ctrl Pts',(-58.6088074259633,-6.05659553606725,
2.59908193199915));
#247391=CARTESIAN_POINT('Ctrl Pts',(-58.6434243604382,-6.08415140319828,
2.65877685806559));
#247392=CARTESIAN_POINT('Ctrl Pts',(-58.7120821529692,-6.10436324506838,
2.65878198860257));
#247393=CARTESIAN_POINT('Ctrl Pts',(-58.6416817365139,-5.97852000021539,
2.638724926698));
#247394=CARTESIAN_POINT('Ctrl Pts',(-58.672182651072,-6.02785839131278,
2.69532212015275));
#247395=CARTESIAN_POINT('Ctrl Pts',(-58.7414038195498,-6.06008468706717,
2.6817683672663));
#247396=CARTESIAN_POINT('Ctrl Pts',(-58.7242744516463,-5.88025093392494,
2.75442176402237));
#247397=CARTESIAN_POINT('Ctrl Pts',(-58.7387860695143,-5.97104363802175,
2.79203179920121));
#247398=CARTESIAN_POINT('Ctrl Pts',(-58.819336041524,-6.00614981441041,
2.74885310748169));
#247399=CARTESIAN_POINT('Ctrl Pts',(-58.7730316211507,-5.85862682030298,
2.82866089558398));
#247400=CARTESIAN_POINT('Ctrl Pts',(-58.7772266151798,-5.97091547255899,
2.85316563119286));
#247401=CARTESIAN_POINT('Ctrl Pts',(-58.8669255556784,-5.99561386571448,
2.79189751796636));
#247402=CARTESIAN_POINT('Ctrl Pts',(-58.8181995570484,-5.86337364149602,
2.90134173516017));
#247403=CARTESIAN_POINT('Ctrl Pts',(-58.805469618532,-5.98915458643816,
2.90103711553223));
#247404=CARTESIAN_POINT('Ctrl Pts',(-58.9120953679529,-6.00036140429068,
2.83404198860256));
#247405=CARTESIAN_POINT('Origin',(-58.925370482788,-5.87405712357891,2.83404198860256));
#247406=CARTESIAN_POINT('Origin',(-61.1207756545814,-6.1048035052631,3.56647653971749));
#247407=CARTESIAN_POINT('Origin',(-61.0393856393803,-6.09624906995262,3.4247302805848));
#247408=CARTESIAN_POINT('Origin',(-59.1025439184828,-5.89267880207806,3.1191364816815));
#247409=CARTESIAN_POINT('Origin',(-59.2797173540685,-5.91130048050365,3.40423097483305));
#247410=CARTESIAN_POINT('Ctrl Pts',(-60.7112330730303,-6.06175884541593,
3.36123028058477));
#247411=CARTESIAN_POINT('Ctrl Pts',(-60.6979579581953,-6.1880631261277,
3.36123028058476));
#247412=CARTESIAN_POINT('Ctrl Pts',(-60.6979579581953,-6.1880631261277,
3.23423028058476));
#247413=CARTESIAN_POINT('Ctrl Pts',(-60.8007259828525,-6.07140041118295,
3.36123028058477));
#247414=CARTESIAN_POINT('Ctrl Pts',(-60.7873912833613,-6.19746294737669,
3.36099641108453));
#247415=CARTESIAN_POINT('Ctrl Pts',(-60.8322324012612,-6.20217593878186,
3.23423043688326));
#247416=CARTESIAN_POINT('Ctrl Pts',(-60.8853484607269,-6.08051542067575,
3.41054258905279));
#247417=CARTESIAN_POINT('Ctrl Pts',(-60.8723790316499,-6.20639551966844,
3.41008815825962));
#247418=CARTESIAN_POINT('Ctrl Pts',(-60.9591984396306,-6.21552060714939,
3.30819867304277));
#247419=CARTESIAN_POINT('Ctrl Pts',(-60.929944884669,-6.08531878138344,
3.48823028058478));
#247420=CARTESIAN_POINT('Ctrl Pts',(-60.917217374751,-6.21110821942958,
3.48794691941594));
#247421=CARTESIAN_POINT('Ctrl Pts',(-61.0261105245453,-6.22255335066439,
3.42473028058479));
#247422=CARTESIAN_POINT('Origin',(-60.7112330730303,-6.06175884541593,3.23423028058476));
#247423=CARTESIAN_POINT('Ctrl Pts',(-59.1725467709677,-5.90061356181279,
3.47153072139067));
#247424=CARTESIAN_POINT('Ctrl Pts',(-59.1597945546412,-6.02658562874829,
3.47122746285072));
#247425=CARTESIAN_POINT('Ctrl Pts',(-59.2666022171587,-6.03762143316774,
3.40413046676782));
#247426=CARTESIAN_POINT('Ctrl Pts',(-59.2869113614504,-5.91250964036502,
3.65553813457981));
#247427=CARTESIAN_POINT('Ctrl Pts',(-59.2739830624761,-6.03858760028889,
3.65520336072254));
#247428=CARTESIAN_POINT('Ctrl Pts',(-59.3580501215732,-6.04723299508893,
3.55128134519992));
#247429=CARTESIAN_POINT('Ctrl Pts',(-59.4923630227874,-5.9338813165696,
3.77003198860258));
#247430=CARTESIAN_POINT('Ctrl Pts',(-59.4792818168382,-6.06016587018229,
3.76980209314047));
#247431=CARTESIAN_POINT('Ctrl Pts',(-59.522332169774,-6.06449973388429,
3.64284195387353));
#247432=CARTESIAN_POINT('Ctrl Pts',(-59.7081718144892,-5.95633285891234,
3.77003198860258));
#247433=CARTESIAN_POINT('Ctrl Pts',(-59.6948768144682,-6.08282633453096,
3.77003198860258));
#247434=CARTESIAN_POINT('Ctrl Pts',(-59.6948967145252,-6.08263699813589,
3.64284189403797));
#247435=CARTESIAN_POINT('Origin',(-59.7081718144892,-5.95633285891233,3.64303198860258));
#247436=CARTESIAN_POINT('Origin',(60.0186752706391,6.62746584474152,3.23423028058487));
#247437=CARTESIAN_POINT('Origin',(-60.5608532912343,-6.04595329345084,3.23423028058476));
#247438=CARTESIAN_POINT('Origin',(59.785232315514,6.60293000146494,3.64303198860268));
#247439=CARTESIAN_POINT('Origin',(-60.1073400339995,-5.99823604520077,3.64299171721722));
#247440=CARTESIAN_POINT('Ctrl Pts',(-60.3421421670674,-6.02238575970299,
3.48823028058475));
#247441=CARTESIAN_POINT('Ctrl Pts',(-60.3293058762211,-6.1493162309727,
3.48852004212253));
#247442=CARTESIAN_POINT('Ctrl Pts',(-60.2194255397044,-6.13776734223238,
3.42473028058475));
#247443=CARTESIAN_POINT('Ctrl Pts',(-60.3868890390927,-6.02720817145267,
3.41028005848404));
#247444=CARTESIAN_POINT('Ctrl Pts',(-60.373827809955,-6.15399567476977,
3.41074404220476));
#247445=CARTESIAN_POINT('Ctrl Pts',(-60.2865637544338,-6.14482385294861,
3.30780486244026));
#247446=CARTESIAN_POINT('Ctrl Pts',(-60.4716618705781,-6.03634362557944,
3.36123028058477));
#247447=CARTESIAN_POINT('Ctrl Pts',(-60.4582762833165,-6.16287156698251,
3.3614646058637));
#247448=CARTESIAN_POINT('Ctrl Pts',(-60.4137560077479,-6.1581922974649,
3.23423045308351));
#247449=CARTESIAN_POINT('Ctrl Pts',(-60.5608532912343,-6.04595329345084,
3.36123028058477));
#247450=CARTESIAN_POINT('Ctrl Pts',(-60.5475781763993,-6.17225757416261,
3.36123028058476));
#247451=CARTESIAN_POINT('Ctrl Pts',(-60.5475781763993,-6.17225757416261,
3.23423028058476));
#247452=CARTESIAN_POINT('Origin',(-60.2327006545395,-6.01146306152061,3.42473028058475));
#247453=CARTESIAN_POINT('Origin',(-60.1517960329186,-6.00295964283186,3.56563113524748));
#247454=CARTESIAN_POINT('Origin',(-60.0157999988654,-13.0813452322047,3.56647653909434));
#247455=CARTESIAN_POINT('Origin',(-60.0590486699119,-13.0905908661191,3.64299466007557));
#247456=CARTESIAN_POINT('Origin',(-59.9357500275432,-13.0643300858384,3.42473028058474));
#247457=CARTESIAN_POINT('Ctrl Pts',(-59.8282880397054,-13.0409063549241,
3.48823028058474));
#247458=CARTESIAN_POINT('Ctrl Pts',(-59.8550545325308,-12.9173404733285,
3.4879469194159));
#247459=CARTESIAN_POINT('Ctrl Pts',(-59.9621548122771,-12.9401053405452,
3.42473028058475));
#247460=CARTESIAN_POINT('Ctrl Pts',(-59.7842416555145,-13.0316624367252,
3.41028005925074));
#247461=CARTESIAN_POINT('Ctrl Pts',(-59.8108054559345,-12.9079350417482,
3.40982512231036));
#247462=CARTESIAN_POINT('Ctrl Pts',(-59.8961220185277,-12.9260696369484,
3.30780486372917));
#247463=CARTESIAN_POINT('Ctrl Pts',(-59.7007958241042,-13.0141504107553,
3.36123028058472));
#247464=CARTESIAN_POINT('Ctrl Pts',(-59.727069488887,-12.8901364125062,
3.360997210484));
#247465=CARTESIAN_POINT('Ctrl Pts',(-59.7710239514086,-12.89947922193,3.23423045308327));
#247466=CARTESIAN_POINT('Ctrl Pts',(-59.6130003254554,-12.9957275188826,
3.36123028058472));
#247467=CARTESIAN_POINT('Ctrl Pts',(-59.6394051101893,-12.8715027735894,
3.36123028058472));
#247468=CARTESIAN_POINT('Ctrl Pts',(-59.6394051101892,-12.8715027735894,
3.23423028058472));
#247469=CARTESIAN_POINT('Origin',(-59.6130003254554,-12.9957275188826,3.23423028058471));
#247470=CARTESIAN_POINT('Origin',(0.0660119618346463,-0.310561863232799,
3.64303198860262));
#247471=CARTESIAN_POINT('Origin',(-60.4516424606488,-13.1739864076109,3.64303198860252));
#247472=CARTESIAN_POINT('Origin',(0.0660119618346464,-0.310561863232796,
3.23423028058481));
#247473=CARTESIAN_POINT('Origin',(-59.4650964698965,-12.9642895838873,3.23423028058472));
#247474=CARTESIAN_POINT('Ctrl Pts',(-60.9782752797347,-13.2864868028998,
3.47153072139062));
#247475=CARTESIAN_POINT('Ctrl Pts',(-61.0052918384388,-13.1616357280624,
3.47182327902652));
#247476=CARTESIAN_POINT('Ctrl Pts',(-60.8992893541404,-13.1392995818861,
3.40413028959028));
#247477=CARTESIAN_POINT('Ctrl Pts',(-60.8658306440995,-13.2624669757411,
3.65553807120949));
#247478=CARTESIAN_POINT('Ctrl Pts',(-60.8926675943329,-13.1376969719828,
3.65586275496964));
#247479=CARTESIAN_POINT('Ctrl Pts',(-60.8093473519473,-13.1201818190178,
3.55128126837224));
#247480=CARTESIAN_POINT('Ctrl Pts',(-60.663828108008,-13.2193155203586,
3.77003198860253));
#247481=CARTESIAN_POINT('Ctrl Pts',(-60.6905008239722,-13.0947255842065,
3.77025505748485));
#247482=CARTESIAN_POINT('Ctrl Pts',(-60.6477702018618,-13.0858375353123,
3.64284211731165));
#247483=CARTESIAN_POINT('Ctrl Pts',(-60.4516424606488,-13.1739864076109,
3.77003198860253));
#247484=CARTESIAN_POINT('Ctrl Pts',(-60.4780866929066,-13.0495760763088,
3.77003198860253));
#247485=CARTESIAN_POINT('Ctrl Pts',(-60.4780472159603,-13.0497618007392,
3.64284239821708));
#247486=CARTESIAN_POINT('Origin',(-60.8730422059013,-13.2635576885504,3.404230974833));
#247487=CARTESIAN_POINT('Ctrl Pts',(-59.4650964698965,-12.9642895838873,
3.36123028058472));
#247488=CARTESIAN_POINT('Ctrl Pts',(-59.4915012546304,-12.8400648385941,
3.36123028058472));
#247489=CARTESIAN_POINT('Ctrl Pts',(-59.4915012546304,-12.8400648385941,
3.23423028058472));
#247490=CARTESIAN_POINT('Ctrl Pts',(-59.3770041141842,-12.9458049943938,
3.36123028058472));
#247491=CARTESIAN_POINT('Ctrl Pts',(-59.4033730190084,-12.8213326038442,
3.36146538610113));
#247492=CARTESIAN_POINT('Ctrl Pts',(-59.3594375597972,-12.8119938336989,
3.23423043688373));
#247493=CARTESIAN_POINT('Ctrl Pts',(-59.2937057271822,-12.9283282206302,
3.4105425869309));
#247494=CARTESIAN_POINT('Ctrl Pts',(-59.3204640761297,-12.8037097640144,
3.41100608859826));
#247495=CARTESIAN_POINT('Ctrl Pts',(-59.2345619206667,-12.785450697209,
3.30819866970894));
#247496=CARTESIAN_POINT('Ctrl Pts',(-59.2498070616278,-12.9191181862048,
3.48823028058471));
#247497=CARTESIAN_POINT('Ctrl Pts',(-59.2768226962997,-12.794433502371,
3.48852004212249));
#247498=CARTESIAN_POINT('Ctrl Pts',(-59.168751483356,-12.7714622569322,
3.42473028058471));
#247499=CARTESIAN_POINT('Origin',(-59.1423466986221,-12.8956870022254,3.42473028058471));
#247500=CARTESIAN_POINT('Origin',(-61.047298331887,-13.3005969715144,3.11913648178439));
#247501=CARTESIAN_POINT('Origin',(-61.2215544576538,-13.3376362544828,2.8340419886025));
#247502=CARTESIAN_POINT('Origin',(-59.0627741291267,-12.8787733304439,3.56563113460793));
#247503=CARTESIAN_POINT('Origin',(-59.0190342907434,-12.8695280801149,3.64299171721761));
#247504=CARTESIAN_POINT('Ctrl Pts',(-61.575271693745,-13.103835206573,2.59908173516014));
#247505=CARTESIAN_POINT('Ctrl Pts',(-61.5387839176327,-13.0960702419683,
2.65878198860252));
#247506=CARTESIAN_POINT('Ctrl Pts',(-61.4699285681953,-13.0814171332235,
2.65878198860252));
#247507=CARTESIAN_POINT('Ctrl Pts',(-61.5569304518435,-13.1900205930481,
2.59908193475538));
#247508=CARTESIAN_POINT('Ctrl Pts',(-61.5254208297816,-13.1588482421894,
2.65878715325286));
#247509=CARTESIAN_POINT('Ctrl Pts',(-61.4593031273767,-13.1313027022859,
2.65878198860252));
#247510=CARTESIAN_POINT('Ctrl Pts',(-61.5155378539379,-13.2643407403246,
2.63878778849859));
#247511=CARTESIAN_POINT('Ctrl Pts',(-61.4904936222817,-13.2118511391502,
2.69564460180109));
#247512=CARTESIAN_POINT('Ctrl Pts',(-61.4250300340668,-13.1721300657494,
2.68180481624885));
#247513=CARTESIAN_POINT('Ctrl Pts',(-61.4222835584425,-13.3535591268196,
2.75443238878635));
#247514=CARTESIAN_POINT('Ctrl Pts',(-61.4178880557396,-13.2611962587088,
2.79268340777075));
#247515=CARTESIAN_POINT('Ctrl Pts',(-61.341115859575,-13.2174099770539,
2.74885926835587));
#247516=CARTESIAN_POINT('Ctrl Pts',(-61.3712701109735,-13.3700167576324,
2.82856655361658));
#247517=CARTESIAN_POINT('Ctrl Pts',(-61.3797074995628,-13.257089619245,
2.85384197230779));
#247518=CARTESIAN_POINT('Ctrl Pts',(-61.292439340452,-13.2228660458969,
2.79184624278483));
#247519=CARTESIAN_POINT('Ctrl Pts',(-61.3267881959112,-13.3605623192489,
2.90134173516012));
#247520=CARTESIAN_POINT('Ctrl Pts',(-61.3537611057082,-13.2359003894753,
2.9016321871638));
#247521=CARTESIAN_POINT('Ctrl Pts',(-61.2479592423877,-13.2134115091896,
2.83404198860251));
#247522=CARTESIAN_POINT('Origin',(-61.4699285681953,-13.0814171332235,2.53178198860251));
#247523=CARTESIAN_POINT('Origin',(0.0660119618346463,-0.310561863232799,
3.64303198860262));
#247524=CARTESIAN_POINT('Origin',(-58.6264539577983,-12.7860306150454,3.64303198860253));
#247525=CARTESIAN_POINT('Origin',(1.31078692950418E-16,1.91611717219644E-13,
2.53178198860262));
#247526=CARTESIAN_POINT('Origin',(-61.4762657165315,-13.0516031943531,2.53178198860252));
#247527=CARTESIAN_POINT('Ctrl Pts',(-58.6264539577983,-12.7860306150454,
3.77003198860253));
#247528=CARTESIAN_POINT('Ctrl Pts',(-58.652898298092,-12.6616197754743,
3.77003198860253));
#247529=CARTESIAN_POINT('Ctrl Pts',(-58.6528587129485,-12.6618060089323,
3.64284187937045));
#247530=CARTESIAN_POINT('Ctrl Pts',(-58.4142663981464,-12.7406940127381,
3.77003198860254));
#247531=CARTESIAN_POINT('Ctrl Pts',(-58.4408495151697,-12.6165479409694,
3.76980208962975));
#247532=CARTESIAN_POINT('Ctrl Pts',(-58.4831327254059,-12.6257296363314,
3.64284193928275));
#247533=CARTESIAN_POINT('Ctrl Pts',(-58.2122676405432,-12.6975319705099,
3.65553535416578));
#247534=CARTESIAN_POINT('Ctrl Pts',(-58.2389323335244,-12.5736296288428,
3.65520057834408));
#247535=CARTESIAN_POINT('Ctrl Pts',(-58.3215567776512,-12.5913856081752,
3.55127910964244));
#247536=CARTESIAN_POINT('Ctrl Pts',(-58.0998260601479,-12.6735055745743,
3.47153072139062));
#247537=CARTESIAN_POINT('Ctrl Pts',(-58.1266254943011,-12.5497583536237,
3.47122746281572));
#247538=CARTESIAN_POINT('Ctrl Pts',(-58.2316158778875,-12.5722680796267,
3.40413045901267));
#247539=CARTESIAN_POINT('Origin',(-58.2050537810541,-12.6964592423895,3.40423097483301));
#247540=CARTESIAN_POINT('Ctrl Pts',(-61.4590390555208,-12.7383709431253,
2.90134173516013));
#247541=CARTESIAN_POINT('Ctrl Pts',(-61.4329754599098,-12.8632261535958,
2.90163218716381));
#247542=CARTESIAN_POINT('Ctrl Pts',(-61.3271735965892,-12.8407372733101,
2.83404198860251));
#247543=CARTESIAN_POINT('Ctrl Pts',(-61.5035409747665,-12.7478306169679,
2.82853349835352));
#247544=CARTESIAN_POINT('Ctrl Pts',(-61.465315459776,-12.8544171899346,
2.8538148316239));
#247545=CARTESIAN_POINT('Ctrl Pts',(-61.3716739624486,-12.8501961180702,
2.79182701594278));
#247546=CARTESIAN_POINT('Ctrl Pts',(-61.5432717953614,-12.7835835513932,
2.75468822073622));
#247547=CARTESIAN_POINT('Ctrl Pts',(-61.5017184029595,-12.8662481012967,
2.79286913083806));
#247548=CARTESIAN_POINT('Ctrl Pts',(-61.4137451613973,-12.8749453072906,
2.749007632979));
#247549=CARTESIAN_POINT('Ctrl Pts',(-61.5920631419343,-12.9020280679173,
2.63954450640393));
#247550=CARTESIAN_POINT('Ctrl Pts',(-61.547840657004,-12.940148758413,2.69627684028861));
#247551=CARTESIAN_POINT('Ctrl Pts',(-61.4717924962541,-12.9498405053864,
2.68224356036484));
#247552=CARTESIAN_POINT('Ctrl Pts',(-61.5999795805209,-12.9874904696722,
2.59908178706399));
#247553=CARTESIAN_POINT('Ctrl Pts',(-61.5585057825381,-13.0031958218442,
2.65878704321563));
#247554=CARTESIAN_POINT('Ctrl Pts',(-61.4868843017912,-13.0015435854425,
2.65878198860251));
#247555=CARTESIAN_POINT('Ctrl Pts',(-61.5816197022697,-13.0739701745327,
2.59908173516013));
#247556=CARTESIAN_POINT('Ctrl Pts',(-61.5451281645058,-13.0662229071069,
2.65878198860251));
#247557=CARTESIAN_POINT('Ctrl Pts',(-61.4762657165315,-13.0516031943531,
2.65878198860251));
#247558=CARTESIAN_POINT('Origin',(-61.3535783813231,-12.7165125280169,2.83404198860251));
#247559=CARTESIAN_POINT('Origin',(-58.0307974155439,-12.6594199084572,3.11913648167152));
#247560=CARTESIAN_POINT('Origin',(-57.8565410498766,-12.6223805745522,2.83404198860253));
#247561=CARTESIAN_POINT('Origin',(-61.1793222555325,-12.6794732450918,3.11913648177545));
#247562=CARTESIAN_POINT('Origin',(-61.0050661295705,-12.6424339620845,3.40423097483301));
#247563=CARTESIAN_POINT('Ctrl Pts',(-57.7513140650719,-12.5994235324474,
2.90134173516015));
#247564=CARTESIAN_POINT('Ctrl Pts',(-57.7780756236494,-12.4758649777955,
2.9010371155322));
#247565=CARTESIAN_POINT('Ctrl Pts',(-57.8829458346104,-12.498155829259,
2.83404198860253));
#247566=CARTESIAN_POINT('Ctrl Pts',(-57.7068710254543,-12.5899763290076,
2.82862991747951));
#247567=CARTESIAN_POINT('Ctrl Pts',(-57.7455616498587,-12.4844883578129,
2.85314045886467));
#247568=CARTESIAN_POINT('Ctrl Pts',(-57.8385008428013,-12.4887087546166,
2.79187960999924));
#247569=CARTESIAN_POINT('Ctrl Pts',(-57.6673720419785,-12.5543975270269,
2.75470625793316));
#247570=CARTESIAN_POINT('Ctrl Pts',(-57.7092008760996,-12.472450653056,
2.79224250381896));
#247571=CARTESIAN_POINT('Ctrl Pts',(-57.7966870296828,-12.4640308112191,
2.7490180910825));
#247572=CARTESIAN_POINT('Ctrl Pts',(-57.6192799956673,-12.4363816727425,
2.63947868311689));
#247573=CARTESIAN_POINT('Ctrl Pts',(-57.6635313090886,-12.3985321242202,
2.69595066767898));
#247574=CARTESIAN_POINT('Ctrl Pts',(-57.7394080294758,-12.3892398894927,
2.68220539436051));
#247575=CARTESIAN_POINT('Ctrl Pts',(-57.6118166447789,-12.3512461790953,
2.59908178584993));
#247576=CARTESIAN_POINT('Ctrl Pts',(-57.6532646075496,-12.3356888898089,
2.6587767094484));
#247577=CARTESIAN_POINT('Ctrl Pts',(-57.7248239067111,-12.3376071226704,
2.65878198860252));
#247578=CARTESIAN_POINT('Ctrl Pts',(-57.6301266171956,-12.2652136052663,
2.59908173516014));
#247579=CARTESIAN_POINT('Ctrl Pts',(-57.6666142715154,-12.2729791421557,
2.65878198860252));
#247580=CARTESIAN_POINT('Ctrl Pts',(-57.7354693911204,-12.2876333308473,
2.65878198860252));
#247581=CARTESIAN_POINT('Origin',(-57.7354693911203,-12.2876333308473,2.53178198860252));
#247582=CARTESIAN_POINT('Ctrl Pts',(-60.5836663843181,-12.552862681145,
3.77003198860254));
#247583=CARTESIAN_POINT('Ctrl Pts',(-60.5572221497821,-12.6772730231647,
3.77003198860254));
#247584=CARTESIAN_POINT('Ctrl Pts',(-60.55726162901,-12.6770872880007,3.6428423872764));
#247585=CARTESIAN_POINT('Ctrl Pts',(-60.7959479326851,-12.5977568525212,
3.77003198860254));
#247586=CARTESIAN_POINT('Ctrl Pts',(-60.7696393833362,-12.7224242094577,
3.77025506105595));
#247587=CARTESIAN_POINT('Ctrl Pts',(-60.7269872521295,-12.7131635826248,
3.64284210641857));
#247588=CARTESIAN_POINT('Ctrl Pts',(-60.99803611366,-12.6404975322969,3.65553527987824));
#247589=CARTESIAN_POINT('Ctrl Pts',(-60.9718043534706,-12.7653961862418,
3.65585996533041));
#247590=CARTESIAN_POINT('Ctrl Pts',(-60.8885631224,-12.7475075938194,3.55127902710186));
#247591=CARTESIAN_POINT('Ctrl Pts',(-61.110527437164,-12.6642893210144,
3.47153072139063));
#247592=CARTESIAN_POINT('Ctrl Pts',(-61.0844267823321,-12.7893350885045,
3.47182327905179));
#247593=CARTESIAN_POINT('Ctrl Pts',(-60.9785037583493,-12.7666250660188,
3.40413028378005));
#247594=CARTESIAN_POINT('Origin',(-60.5836663843181,-12.552862681145,3.64303198860254));
#247595=CARTESIAN_POINT('Origin',(3.545935779686E-16,1.91565239218228E-13,
2.53178198860262));
#247596=CARTESIAN_POINT('Origin',(-57.7418065394565,-12.257819391977,2.53178198860253));
#247597=CARTESIAN_POINT('Origin',(59.4667368016499,12.9646382471652,3.64303198860272));
#247598=CARTESIAN_POINT('Origin',(-60.1910940874975,-12.469366018727,3.64299466007616));
#247599=CARTESIAN_POINT('Ctrl Pts',(-57.6364522029206,-12.2354540642047,
2.59908173516014));
#247600=CARTESIAN_POINT('Ctrl Pts',(-57.6729438621905,-12.2432007592849,
2.65878198860252));
#247601=CARTESIAN_POINT('Ctrl Pts',(-57.7418065394565,-12.257819391977,
2.65878198860252));
#247602=CARTESIAN_POINT('Ctrl Pts',(-57.6546556225242,-12.1497054461945,
2.59908193199905));
#247603=CARTESIAN_POINT('Ctrl Pts',(-57.6862025493678,-12.1807288143665,
2.65877685806624));
#247604=CARTESIAN_POINT('Ctrl Pts',(-57.7523715145536,-12.2080066271958,
2.65878198860252));
#247605=CARTESIAN_POINT('Ctrl Pts',(-57.6955109599434,-12.0754939174599,
2.63872492669794));
#247606=CARTESIAN_POINT('Ctrl Pts',(-57.7206875210979,-12.1277502414152,
2.69532212015257));
#247607=CARTESIAN_POINT('Ctrl Pts',(-57.7861609236006,-12.1670355805165,
2.68176836726627));
#247608=CARTESIAN_POINT('Ctrl Pts',(-57.7879231380265,-11.9863964689867,
2.75442176402234));
#247609=CARTESIAN_POINT('Ctrl Pts',(-57.7928648378994,-12.0782086782662,
2.79203179920141));
#247610=CARTESIAN_POINT('Ctrl Pts',(-57.8693039540644,-12.1215423041375,
2.74885310748163));
#247611=CARTESIAN_POINT('Ctrl Pts',(-57.8386735460213,-11.969987326523,
2.82866089558395));
#247612=CARTESIAN_POINT('Ctrl Pts',(-57.8311081991717,-12.0820993460742,
2.85316563119138));
#247613=CARTESIAN_POINT('Ctrl Pts',(-57.9177340744069,-12.1160385312531,
2.79189751796634));
#247614=CARTESIAN_POINT('Ctrl Pts',(-57.8830978693155,-11.9794294790614,
2.90134173516013));
#247615=CARTESIAN_POINT('Ctrl Pts',(-57.857289977851,-12.1031907419159,
2.90103711553219));
#247616=CARTESIAN_POINT('Ctrl Pts',(-57.962160188812,-12.1254815933794,
2.83404198860251));
#247617=CARTESIAN_POINT('Origin',(-57.9885649735458,-12.0012568480862,2.83404198860252));
#247618=CARTESIAN_POINT('Origin',(-60.1478239214165,-12.4602215058061,3.56647653971771));
#247619=CARTESIAN_POINT('Origin',(-60.0677739512125,-12.4432063593725,3.42473028058475));
#247620=CARTESIAN_POINT('Origin',(-58.1628213391876,-12.0382961820437,3.11913648168035));
#247621=CARTESIAN_POINT('Origin',(-58.3370777047234,-12.0753355159235,3.40423097483301));
#247622=CARTESIAN_POINT('Ctrl Pts',(-59.7450242491247,-12.3746037924167,
3.36123028058472));
#247623=CARTESIAN_POINT('Ctrl Pts',(-59.7186194643908,-12.4988285377098,
3.36123028058472));
#247624=CARTESIAN_POINT('Ctrl Pts',(-59.7186194643908,-12.4988285377098,
3.23423028058472));
#247625=CARTESIAN_POINT('Ctrl Pts',(-59.8330190893699,-12.3935470970144,
3.36123028058472));
#247626=CARTESIAN_POINT('Ctrl Pts',(-59.8065803155762,-12.5175251937998,
3.36099641108486));
#247627=CARTESIAN_POINT('Ctrl Pts',(-59.8506831473911,-12.5268995400899,
3.23423043688348));
#247628=CARTESIAN_POINT('Ctrl Pts',(-59.9162252185214,-12.4114576311019,
3.41054258905275));
#247629=CARTESIAN_POINT('Ctrl Pts',(-59.8901687840271,-12.5352924712482,
3.41008815826019));
#247630=CARTESIAN_POINT('Ctrl Pts',(-59.9755587548356,-12.5534426698447,
3.30819867304325));
#247631=CARTESIAN_POINT('Ctrl Pts',(-59.9600752506736,-12.4208962741589,
3.48823028058475));
#247632=CARTESIAN_POINT('Ctrl Pts',(-59.9342688867324,-12.5446662374489,
3.48794691941591));
#247633=CARTESIAN_POINT('Ctrl Pts',(-60.0413691664786,-12.5674311046657,
3.42473028058476));
#247634=CARTESIAN_POINT('Origin',(-59.7450242491247,-12.3746037924167,3.23423028058472));
#247635=CARTESIAN_POINT('Ctrl Pts',(-58.231611300478,-12.0535047649324,
3.47153072139064));
#247636=CARTESIAN_POINT('Ctrl Pts',(-58.2057612755554,-12.1774537741286,
3.47122746285068));
#247637=CARTESIAN_POINT('Ctrl Pts',(-58.3108302788452,-12.199593564085,
3.40413046676783));
#247638=CARTESIAN_POINT('Ctrl Pts',(-58.344105910958,-12.077290030417,3.65553813457981));
#247639=CARTESIAN_POINT('Ctrl Pts',(-58.3180696991555,-12.2013259468605,
3.65520336072148));
#247640=CARTESIAN_POINT('Ctrl Pts',(-58.4007725402744,-12.2187113817819,
3.55128134519937));
#247641=CARTESIAN_POINT('Ctrl Pts',(-58.546198138126,-12.1200201767791,
3.77003198860254));
#247642=CARTESIAN_POINT('Ctrl Pts',(-58.5199882620682,-12.244245572038,
3.7698020931417));
#247643=CARTESIAN_POINT('Ctrl Pts',(-58.5623497685532,-12.2530556816162,
3.64284195387403));
#247644=CARTESIAN_POINT('Ctrl Pts',(-58.7584778814675,-12.1649068885794,
3.77003198860254));
#247645=CARTESIAN_POINT('Ctrl Pts',(-58.732033544228,-12.2893177137819,
3.77003198860254));
#247646=CARTESIAN_POINT('Ctrl Pts',(-58.7320731263128,-12.2891314947139,
3.64284189403801));
#247647=CARTESIAN_POINT('Origin',(-58.7584778814675,-12.1649068885794,3.64303198860253));
#247648=CARTESIAN_POINT('Origin',(58.0246834617327,12.6581203474876,3.23423028058491));
#247649=CARTESIAN_POINT('Origin',(-59.5971203935658,-12.3431658574213,3.23423028058472));
#247650=CARTESIAN_POINT('Origin',(57.798864262886,12.6101209950216,3.64303198860272));
#247651=CARTESIAN_POINT('Origin',(-59.1510793400371,-12.2483049654003,3.64299171721781));
#247652=CARTESIAN_POINT('Ctrl Pts',(-59.382070869907,-12.2968658913806,
3.48823028058472));
#247653=CARTESIAN_POINT('Ctrl Pts',(-59.3560370505013,-12.4217592664915,
3.48852004212249));
#247654=CARTESIAN_POINT('Ctrl Pts',(-59.2479658375575,-12.3987880210526,
3.42473028058472));
#247655=CARTESIAN_POINT('Ctrl Pts',(-59.4260685345959,-12.3063392072229,
3.41028005848397));
#247656=CARTESIAN_POINT('Ctrl Pts',(-59.3998259533508,-12.4310668851207,
3.41074404220355));
#247657=CARTESIAN_POINT('Ctrl Pts',(-59.3139986558987,-12.4128237298766,
3.30780486243951));
#247658=CARTESIAN_POINT('Ctrl Pts',(-59.5094220566594,-12.324285790178,
3.36123028058472));
#247659=CARTESIAN_POINT('Ctrl Pts',(-59.4828840257729,-12.4487214234133,
3.36146460586388));
#247660=CARTESIAN_POINT('Ctrl Pts',(-59.4390967537825,-12.4394141514343,
3.23423045308373));
#247661=CARTESIAN_POINT('Ctrl Pts',(-59.5971203935658,-12.3431658574213,
3.36123028058472));
#247662=CARTESIAN_POINT('Ctrl Pts',(-59.570715608832,-12.4673906027145,
3.36123028058472));
#247663=CARTESIAN_POINT('Ctrl Pts',(-59.570715608832,-12.4673906027145,
3.23423028058472));
#247664=CARTESIAN_POINT('Origin',(-59.2743706222914,-12.2745632757594,3.42473028058471));
#247665=CARTESIAN_POINT('Origin',(-59.1947980539411,-12.2576496039197,3.56563113524763));
#247666=CARTESIAN_POINT('Origin',(-58.3196542523182,-19.283043599958,3.56647653909482));
#247667=CARTESIAN_POINT('Origin',(-58.3616995707146,-19.2967593024447,3.64299466007676));
#247668=CARTESIAN_POINT('Origin',(-58.2418213702172,-19.2577541638581,3.4247302805847));
#247669=CARTESIAN_POINT('Ctrl Pts',(-58.1373965169892,-19.2232259141442,
3.48823028058469));
#247670=CARTESIAN_POINT('Ctrl Pts',(-58.1769325318818,-19.103134799739,
3.48794691941586));
#247671=CARTESIAN_POINT('Ctrl Pts',(-58.2810665285028,-19.1369699862886,
3.4247302805847));
#247672=CARTESIAN_POINT('Ctrl Pts',(-58.0945576760629,-19.2094285342461,
3.41028005925071));
#247673=CARTESIAN_POINT('Ctrl Pts',(-58.1339089916623,-19.089155604121,
3.40982512231007));
#247674=CARTESIAN_POINT('Ctrl Pts',(-58.2168625998339,-19.1161088652885,
3.30780486372894));
#247675=CARTESIAN_POINT('Ctrl Pts',(-58.0133994748117,-19.1832899764629,
3.36123028058467));
#247676=CARTESIAN_POINT('Ctrl Pts',(-58.0524922023731,-19.062701685676,
3.36099721048547));
#247677=CARTESIAN_POINT('Ctrl Pts',(-58.0952292882365,-19.0765878066325,
3.23423045308378));
#247678=CARTESIAN_POINT('Ctrl Pts',(-57.9280106456674,-19.1557908785628,
3.36123028058467));
#247679=CARTESIAN_POINT('Ctrl Pts',(-57.967255803953,-19.0350067009933,
3.36123028058467));
#247680=CARTESIAN_POINT('Ctrl Pts',(-57.967255803953,-19.0350067009933,
3.23423028058467));
#247681=CARTESIAN_POINT('Origin',(-57.9280106456674,-19.1557908785628,3.23423028058466));
#247682=CARTESIAN_POINT('Origin',(0.0981128957140535,-0.301960443923527,
3.64303198860262));
#247683=CARTESIAN_POINT('Origin',(-58.7434254837931,-19.4207352200704,3.64303198860248));
#247684=CARTESIAN_POINT('Origin',(0.0981128957140536,-0.301960443923524,
3.23423028058481));
#247685=CARTESIAN_POINT('Origin',(-57.7842031819381,-19.1090650011318,3.23423028058467));
#247686=CARTESIAN_POINT('Ctrl Pts',(-59.255413859757,-19.5876674457081,
3.47153072139057));
#247687=CARTESIAN_POINT('Ctrl Pts',(-59.295332909916,-19.4663243174857,
3.47182327902648));
#247688=CARTESIAN_POINT('Ctrl Pts',(-59.1922458813524,-19.4330302542694,
3.40413028959002));
#247689=CARTESIAN_POINT('Ctrl Pts',(-59.1460959632219,-19.5520255367103,
3.65553807120939));
#247690=CARTESIAN_POINT('Ctrl Pts',(-59.1858279145902,-19.4307442612507,
3.65586275497065));
#247691=CARTESIAN_POINT('Ctrl Pts',(-59.1047949412349,-19.4046157212348,
3.5512812683731));
#247692=CARTESIAN_POINT('Ctrl Pts',(-58.9497105734781,-19.4879954548406,
3.77003198860249));
#247693=CARTESIAN_POINT('Ctrl Pts',(-58.989260368078,-19.3668760934051,
3.77025505748352));
#247694=CARTESIAN_POINT('Ctrl Pts',(-58.9476928828763,-19.3535701679098,
3.64284211731077));
#247695=CARTESIAN_POINT('Ctrl Pts',(-58.7434254837931,-19.4207352200704,
3.77003198860249));
#247696=CARTESIAN_POINT('Ctrl Pts',(-58.7827292725254,-19.2997705965402,
3.77003198860249));
#247697=CARTESIAN_POINT('Ctrl Pts',(-58.7826705983485,-19.2999511770886,
3.64284239821665));
#247698=CARTESIAN_POINT('Origin',(-59.1531540087997,-19.5538640879535,3.40423097483296));
#247699=CARTESIAN_POINT('Ctrl Pts',(-57.7842031819381,-19.1090650011318,
3.36123028058467));
#247700=CARTESIAN_POINT('Ctrl Pts',(-57.8234483402237,-18.9882808235623,
3.36123028058467));
#247701=CARTESIAN_POINT('Ctrl Pts',(-57.8234483402237,-18.9882808235623,
3.23423028058467));
#247702=CARTESIAN_POINT('Ctrl Pts',(-57.6985255711015,-19.0814735135855,
3.36123028058467));
#247703=CARTESIAN_POINT('Ctrl Pts',(-57.7377609320117,-18.9604392969161,
3.36146538610164));
#247704=CARTESIAN_POINT('Ctrl Pts',(-57.6950423231347,-18.9465591794953,
3.23423043688409));
#247705=CARTESIAN_POINT('Ctrl Pts',(-57.6175103216832,-19.0553854270321,
3.41054258693084));
#247706=CARTESIAN_POINT('Ctrl Pts',(-57.6571482613567,-18.934246652455,
3.41100608859688));
#247707=CARTESIAN_POINT('Ctrl Pts',(-57.5736252790849,-18.9071083904251,
3.30819866970798));
#247708=CARTESIAN_POINT('Ctrl Pts',(-57.5748148483574,-19.041637186088,
3.48823028058467));
#247709=CARTESIAN_POINT('Ctrl Pts',(-57.61471558695,-18.9204594407748,3.48852004212245));
#247710=CARTESIAN_POINT('Ctrl Pts',(-57.5096375484035,-18.8863175164095,
3.42473028058467));
#247711=CARTESIAN_POINT('Origin',(-57.4703923901179,-19.007101693979,3.42473028058467));
#247712=CARTESIAN_POINT('Origin',(-59.3225838821635,-19.6089151909163,3.11913648178334));
#247713=CARTESIAN_POINT('Origin',(-59.4920137553138,-19.6639662938564,2.83404198860248));
#247714=CARTESIAN_POINT('Origin',(-57.3930236876031,-18.981963078654,3.56563113460772));
#247715=CARTESIAN_POINT('Origin',(-57.3504898524409,-18.9681964166834,3.64299171721756));
#247716=CARTESIAN_POINT('Ctrl Pts',(-59.868232155624,-19.4684195516699,
2.59908173516009));
#247717=CARTESIAN_POINT('Ctrl Pts',(-59.8327559231845,-19.4568831131887,
2.65878198860247));
#247718=CARTESIAN_POINT('Ctrl Pts',(-59.765809437495,-19.4351129318423,
2.65878198860247));
#247719=CARTESIAN_POINT('Ctrl Pts',(-59.8409825629599,-19.5522156237497,
2.59908193475607));
#247720=CARTESIAN_POINT('Ctrl Pts',(-59.812903951835,-19.517920385918,2.65878715325408));
#247721=CARTESIAN_POINT('Ctrl Pts',(-59.750027742079,-19.4836145615373,
2.65878198860247));
#247722=CARTESIAN_POINT('Ctrl Pts',(-59.7920481472524,-19.6218019328335,
2.63878778849849));
#247723=CARTESIAN_POINT('Ctrl Pts',(-59.7726277678657,-19.5669820401374,
2.69564460180101));
#247724=CARTESIAN_POINT('Ctrl Pts',(-59.7116747787984,-19.5206357546567,
2.68180481624872));
#247725=CARTESIAN_POINT('Ctrl Pts',(-59.6899788477095,-19.700783843471,
2.75443238878638));
#247726=CARTESIAN_POINT('Ctrl Pts',(-59.6952619726973,-19.6084674936732,
2.79268340777071));
#247727=CARTESIAN_POINT('Ctrl Pts',(-59.6234872553897,-19.5568961981639,
2.74885926835593));
#247728=CARTESIAN_POINT('Ctrl Pts',(-59.6375245663856,-19.7118189603901,
2.8285665536165));
#247729=CARTESIAN_POINT('Ctrl Pts',(-59.6577198343148,-19.6003923959454,
2.85384197230792));
#247730=CARTESIAN_POINT('Ctrl Pts',(-59.5745070768389,-19.5572342963493,
2.79184624278432));
#247731=CARTESIAN_POINT('Ctrl Pts',(-59.5942745858234,-19.6977666881848,
2.90134173516009));
#247732=CARTESIAN_POINT('Ctrl Pts',(-59.6341304551456,-19.5766071063171,
2.90163218716376));
#247733=CARTESIAN_POINT('Ctrl Pts',(-59.5312589135994,-19.5431821162869,
2.83404198860247));
#247734=CARTESIAN_POINT('Origin',(-59.765809437495,-19.4351129318423,2.53178198860247));
#247735=CARTESIAN_POINT('Origin',(0.0981128957140535,-0.301960443923527,
3.64303198860262));
#247736=CARTESIAN_POINT('Origin',(-56.9687879773464,-18.8441205405522,3.64303198860249));
#247737=CARTESIAN_POINT('Origin',(1.26611655068499E-16,1.91628388431979E-13,
2.53178198860262));
#247738=CARTESIAN_POINT('Origin',(-59.7752282754835,-19.4061247292256,2.53178198860247));
#247739=CARTESIAN_POINT('Ctrl Pts',(-56.9687879773464,-18.8441205405522,
3.77003198860249));
#247740=CARTESIAN_POINT('Ctrl Pts',(-57.0080919266514,-18.7231554228304,
3.77003198860249));
#247741=CARTESIAN_POINT('Ctrl Pts',(-57.0080330916622,-18.7233364983081,
3.64284187937016));
#247742=CARTESIAN_POINT('Ctrl Pts',(-56.7625017687168,-18.7768526573614,
3.77003198860249));
#247743=CARTESIAN_POINT('Ctrl Pts',(-56.8019160587471,-18.6561653631346,
3.76980208962846));
#247744=CARTESIAN_POINT('Ctrl Pts',(-56.843007888628,-18.6697165591971,
3.64284193928235));
#247745=CARTESIAN_POINT('Ctrl Pts',(-56.5661212433886,-18.7128124416032,
3.65553535416569));
#247746=CARTESIAN_POINT('Ctrl Pts',(-56.6055911857604,-18.5923760693085,
3.65520057834524));
#247747=CARTESIAN_POINT('Ctrl Pts',(-56.6859069993033,-18.6186713856998,
3.55127910964282));
#247748=CARTESIAN_POINT('Ctrl Pts',(-56.456807071981,-18.6771643191712,
3.47153072139058));
#247749=CARTESIAN_POINT('Ctrl Pts',(-56.4963948028695,-18.5568963021131,
3.47122746281569));
#247750=CARTESIAN_POINT('Ctrl Pts',(-56.5984571310818,-18.5902572009363,
3.4041304590125));
#247751=CARTESIAN_POINT('Origin',(-56.5590590327988,-18.7109915363519,3.40423097483296));
#247752=CARTESIAN_POINT('Ctrl Pts',(-59.790837669791,-19.0928077206414,
2.9013417351601));
#247753=CARTESIAN_POINT('Ctrl Pts',(-59.7518659300024,-19.2142545736086,
2.90163218716377));
#247754=CARTESIAN_POINT('Ctrl Pts',(-59.6489943884562,-19.1808295835784,
2.83404198860248));
#247755=CARTESIAN_POINT('Ctrl Pts',(-59.8341069976971,-19.1068672906322,
2.82853349835337));
#247756=CARTESIAN_POINT('Ctrl Pts',(-59.7849495554008,-19.2088743168621,
2.85381483162398));
#247757=CARTESIAN_POINT('Ctrl Pts',(-59.6922622581484,-19.1948881666554,
2.79182701594271));
#247758=CARTESIAN_POINT('Ctrl Pts',(-59.8698829694067,-19.1465773683629,
2.75468822073635));
#247759=CARTESIAN_POINT('Ctrl Pts',(-59.8199164124675,-19.2244455609612,
2.7928691308379));
#247760=CARTESIAN_POINT('Ctrl Pts',(-59.7315159919506,-19.2238994150015,
2.74900763297901));
#247761=CARTESIAN_POINT('Ctrl Pts',(-59.9060262085834,-19.2694731179105,
2.63954450640372));
#247762=CARTESIAN_POINT('Ctrl Pts',(-59.8580612818569,-19.3027624708835,
2.69627684028866));
#247763=CARTESIAN_POINT('Ctrl Pts',(-59.7814166574708,-19.3044519280754,
2.68224356036474));
#247764=CARTESIAN_POINT('Ctrl Pts',(-59.904966026569,-19.3552948408466,
2.59908178706307));
#247765=CARTESIAN_POINT('Ctrl Pts',(-59.8620777700639,-19.3665789650873,
2.65878704321424));
#247766=CARTESIAN_POINT('Ctrl Pts',(-59.7910213450151,-19.3574492964902,
2.65878198860247));
#247767=CARTESIAN_POINT('Ctrl Pts',(-59.8776671349984,-19.4393816709759,
2.59908173516009));
#247768=CARTESIAN_POINT('Ctrl Pts',(-59.8421853116551,-19.4278624395269,
2.65878198860247));
#247769=CARTESIAN_POINT('Ctrl Pts',(-59.7752282754835,-19.4061247292257,
2.65878198860247));
#247770=CARTESIAN_POINT('Origin',(-59.6882395467419,-19.060045406009,2.83404198860248));
#247771=CARTESIAN_POINT('Origin',(-56.3896289265483,-18.6559403576673,3.11913648167084));
#247772=CARTESIAN_POINT('Origin',(-56.2201988201381,-18.6008891789888,2.83404198860249));
#247773=CARTESIAN_POINT('Origin',(-59.5188096735656,-19.0049943031088,3.11913648177563));
#247774=CARTESIAN_POINT('Origin',(-59.3493798002278,-18.9499432001061,3.40423097483296));
#247775=CARTESIAN_POINT('Ctrl Pts',(-56.1179479440987,-18.5670586829468,
2.9013417351601));
#247776=CARTESIAN_POINT('Ctrl Pts',(-56.1574782858995,-18.4469743395782,
2.90103711553216));
#247777=CARTESIAN_POINT('Ctrl Pts',(-56.2594439784237,-18.4801050014193,
2.83404198860248));
#247778=CARTESIAN_POINT('Ctrl Pts',(-56.0747358697601,-18.5530176696411,
2.82862991747934));
#247779=CARTESIAN_POINT('Ctrl Pts',(-56.1242410384002,-18.4521518441032,
2.85314045886312));
#247780=CARTESIAN_POINT('Ctrl Pts',(-56.2162299491247,-18.4660639121465,
2.79187960999912));
#247781=CARTESIAN_POINT('Ctrl Pts',(-56.0391722633446,-18.5135050040176,
2.75470625793334));
#247782=CARTESIAN_POINT('Ctrl Pts',(-56.0893377355413,-18.4363793473478,
2.79224250381873));
#247783=CARTESIAN_POINT('Ctrl Pts',(-56.1772247439499,-18.4371504234765,
2.74901809108246));
#247784=CARTESIAN_POINT('Ctrl Pts',(-56.0036796861843,-18.3911086652349,
2.63947868311664));
#247785=CARTESIAN_POINT('Ctrl Pts',(-56.0516449414232,-18.3580919822889,
2.69595066767906));
#247786=CARTESIAN_POINT('Ctrl Pts',(-56.1280773042131,-18.3567819283755,
2.68220539436048));
#247787=CARTESIAN_POINT('Ctrl Pts',(-56.0051563026341,-18.3056594201307,
2.59908178585071));
#247788=CARTESIAN_POINT('Ctrl Pts',(-56.0480033886679,-18.2945198471564,
2.65877670944857));
#247789=CARTESIAN_POINT('Ctrl Pts',(-56.1189701685705,-18.303907555312,
2.65878198860248));
#247790=CARTESIAN_POINT('Ctrl Pts',(-56.032358823839,-18.2220120550219,
2.5990817351601));
#247791=CARTESIAN_POINT('Ctrl Pts',(-56.0678348753331,-18.233549049922,
2.65878198860248));
#247792=CARTESIAN_POINT('Ctrl Pts',(-56.134781019564,-18.2553202812751,
2.65878198860248));
#247793=CARTESIAN_POINT('Origin',(-56.1347810195641,-18.2553202812751,2.53178198860248));
#247794=CARTESIAN_POINT('Ctrl Pts',(-58.9396512752212,-18.8168143322229,
3.77003198860249));
#247795=CARTESIAN_POINT('Ctrl Pts',(-58.9003474831029,-18.9377789661738,
3.77003198860249));
#247796=CARTESIAN_POINT('Ctrl Pts',(-58.9004061606708,-18.9375983751892,
3.64284238727605));
#247797=CARTESIAN_POINT('Ctrl Pts',(-59.1460772043116,-18.8836520326607,
3.77003198860249));
#247798=CARTESIAN_POINT('Ctrl Pts',(-59.1068814887054,-19.0048864565374,
3.77025506105755));
#247799=CARTESIAN_POINT('Ctrl Pts',(-59.065431009429,-18.9912181986578,
3.64284210641866));
#247800=CARTESIAN_POINT('Ctrl Pts',(-59.3425907075088,-18.9472825415269,
3.6555352798782));
#247801=CARTESIAN_POINT('Ctrl Pts',(-59.3034471832889,-19.068755021998,
3.65585996533024));
#247802=CARTESIAN_POINT('Ctrl Pts',(-59.2225318234672,-19.0422633471874,
3.55127902710179));
#247803=CARTESIAN_POINT('Ctrl Pts',(-59.4519788726606,-18.9827025415099,
3.47153072139058));
#247804=CARTESIAN_POINT('Ctrl Pts',(-59.4129503580329,-19.1043350338624,
3.47182327905174));
#247805=CARTESIAN_POINT('Ctrl Pts',(-59.3099814352094,-19.0706774483341,
3.40413028377984));
#247806=CARTESIAN_POINT('Origin',(-58.9396512752212,-18.8168143322229,3.64303198860249));
#247807=CARTESIAN_POINT('Origin',(3.56182666396656E-16,1.91559308659476E-13,
2.53178198860262));
#247808=CARTESIAN_POINT('Origin',(-56.1441998575526,-18.2263320786585,2.53178198860249));
#247809=CARTESIAN_POINT('Origin',(56.1826270286323,18.5886813639062,3.64303198860276));
#247810=CARTESIAN_POINT('Origin',(-58.5579573083294,-18.6927400943493,3.64299466007528));
#247811=CARTESIAN_POINT('Ctrl Pts',(-56.0417604764382,-18.1930767435951,
2.5990817351601));
#247812=CARTESIAN_POINT('Ctrl Pts',(-56.0772424804483,-18.2045954185348,
2.65878198860249));
#247813=CARTESIAN_POINT('Ctrl Pts',(-56.1441998575526,-18.2263320786585,
2.65878198860248));
#247814=CARTESIAN_POINT('Ctrl Pts',(-56.0688273470724,-18.1097006409635,
2.59908193199874));
#247815=CARTESIAN_POINT('Ctrl Pts',(-56.0969586315473,-18.1438516116617,
2.65877685806618));
#247816=CARTESIAN_POINT('Ctrl Pts',(-56.159913808364,-18.1778965340259,
2.65878198860248));
#247817=CARTESIAN_POINT('Ctrl Pts',(-56.1172160917339,-18.0401661963854,
2.6387249266979));
#247818=CARTESIAN_POINT('Ctrl Pts',(-56.1367924598133,-18.0947679219786,
2.69532212015264));
#247819=CARTESIAN_POINT('Ctrl Pts',(-56.1978007560412,-18.1406818860299,
2.68176836726611));
#247820=CARTESIAN_POINT('Ctrl Pts',(-56.2184352456063,-17.9612165360192,
2.75442176402231));
#247821=CARTESIAN_POINT('Ctrl Pts',(-56.2137528851846,-18.0530423367032,
2.79203179920121));
#247822=CARTESIAN_POINT('Ctrl Pts',(-56.2852436625533,-18.1041286397845,
2.74885310748172));
#247823=CARTESIAN_POINT('Ctrl Pts',(-56.270622860001,-17.9502021467133,
2.8286608955839));
#247824=CARTESIAN_POINT('Ctrl Pts',(-56.2513800597986,-18.060909210809,
2.85316563119087));
#247825=CARTESIAN_POINT('Ctrl Pts',(-56.333983778552,-18.1037173431995,
2.79189751796545));
#247826=CARTESIAN_POINT('Ctrl Pts',(-56.3138168485093,-17.9642361803975,
2.9013417351601));
#247827=CARTESIAN_POINT('Ctrl Pts',(-56.2752137607564,-18.0846218068697,
2.90103711553217));
#247828=CARTESIAN_POINT('Ctrl Pts',(-56.3771794532806,-18.1177524687109,
2.83404198860248));
#247829=CARTESIAN_POINT('Origin',(-56.4164246115662,-17.9969682911414,2.83404198860249));
#247830=CARTESIAN_POINT('Origin',(-58.5158800426277,-18.6791227120619,3.56647653971777));
#247831=CARTESIAN_POINT('Origin',(-58.4380471616453,-18.6538332760107,3.42473028058471));
#247832=CARTESIAN_POINT('Origin',(-56.5858547179447,-18.0520194698677,3.11913648168048));
#247833=CARTESIAN_POINT('Origin',(-56.7552848242269,-18.1070706485045,3.40423097483297));
#247834=CARTESIAN_POINT('Ctrl Pts',(-58.1242364370955,-18.5518699907153,
3.36123028058468));
#247835=CARTESIAN_POINT('Ctrl Pts',(-58.0849912788099,-18.6726541682848,
3.36123028058468));
#247836=CARTESIAN_POINT('Ctrl Pts',(-58.0849912788099,-18.6726541682848,
3.23423028058468));
#247837=CARTESIAN_POINT('Ctrl Pts',(-58.2097691178804,-18.5799074873338,
3.36123028058468));
#247838=CARTESIAN_POINT('Ctrl Pts',(-58.1705159385191,-18.7004428147373,
3.36099641108398));
#247839=CARTESIAN_POINT('Ctrl Pts',(-58.2133972843951,-18.714375808614,
3.23423043688317));
#247840=CARTESIAN_POINT('Ctrl Pts',(-58.2906472745454,-18.6064173144575,
3.4105425890527));
#247841=CARTESIAN_POINT('Ctrl Pts',(-58.2517893143873,-18.7268501353373,
3.41008815826044));
#247842=CARTESIAN_POINT('Ctrl Pts',(-58.3348142976333,-18.7538265876729,
3.30819867304329));
#247843=CARTESIAN_POINT('Ctrl Pts',(-58.3332704847794,-18.620387828115,
3.48823028058469));
#247844=CARTESIAN_POINT('Ctrl Pts',(-58.2946680067386,-18.7407822670305,
3.48794691941585));
#247845=CARTESIAN_POINT('Ctrl Pts',(-58.3988020033597,-18.7746174535802,
3.42473028058469));
#247846=CARTESIAN_POINT('Origin',(-58.1242364370955,-18.5518699907153,3.23423028058468));
#247847=CARTESIAN_POINT('Ctrl Pts',(-56.6526781108322,-18.0743352474894,
3.47153072139058));
#247848=CARTESIAN_POINT('Ctrl Pts',(-56.614013495596,-18.1949031876638,
3.47122746285063));
#247849=CARTESIAN_POINT('Ctrl Pts',(-56.7161926816712,-18.2279043949851,
3.40413046676769));
#247850=CARTESIAN_POINT('Ctrl Pts',(-56.7620702268155,-18.1097491035617,
3.65553813457973));
#247851=CARTESIAN_POINT('Ctrl Pts',(-56.7232113603666,-18.2303840130672,
3.65520336072325));
#247852=CARTESIAN_POINT('Ctrl Pts',(-56.8036438738754,-18.256319009646,
3.55128134519965));
#247853=CARTESIAN_POINT('Ctrl Pts',(-56.958588855084,-18.1733695596539,
3.7700319886025));
#247854=CARTESIAN_POINT('Ctrl Pts',(-56.9195374698063,-18.2941747571338,
3.76980209314045));
#247855=CARTESIAN_POINT('Ctrl Pts',(-56.9607460083098,-18.3073645871839,
3.6428419538737));
#247856=CARTESIAN_POINT('Ctrl Pts',(-57.1650137687746,-18.2401996527048,
3.7700319886025));
#247857=CARTESIAN_POINT('Ctrl Pts',(-57.125709824009,-18.3611647564559,
3.7700319886025));
#247858=CARTESIAN_POINT('Ctrl Pts',(-57.125768654452,-18.3609836949698,
3.6428418940378));
#247859=CARTESIAN_POINT('Origin',(-57.1650137687745,-18.2401996527048,3.64303198860249));
#247860=CARTESIAN_POINT('Origin',(54.8193466381475,18.1457247135496,3.23423028058495));
#247861=CARTESIAN_POINT('Origin',(-57.9804289733662,-18.5051441132844,3.23423028058468));
#247862=CARTESIAN_POINT('Origin',(54.6058629360811,18.0763596539235,3.64303198860276));
#247863=CARTESIAN_POINT('Origin',(-57.5467470426659,-18.3641788932753,3.64299171721742));
#247864=CARTESIAN_POINT('Ctrl Pts',(-57.7713971777985,-18.4366189870675,
3.48823028058468));
#247865=CARTESIAN_POINT('Ctrl Pts',(-57.7324510618069,-18.5581069080663,
3.48852004212245));
#247866=CARTESIAN_POINT('Ctrl Pts',(-57.6273730232604,-18.523964983701,
3.42473028058467));
#247867=CARTESIAN_POINT('Ctrl Pts',(-57.8141635875296,-18.4506394153724,
3.41028005848391));
#247868=CARTESIAN_POINT('Ctrl Pts',(-57.7750271733929,-18.5719407253121,
3.41074404220449));
#247869=CARTESIAN_POINT('Ctrl Pts',(-57.6915769758397,-18.5448261124701,
3.30780486243967));
#247870=CARTESIAN_POINT('Ctrl Pts',(-57.8951845615404,-18.4772005006378,
3.36123028058468));
#247871=CARTESIAN_POINT('Ctrl Pts',(-57.8557848432456,-18.5981804828674,
3.36146460586278));
#247872=CARTESIAN_POINT('Ctrl Pts',(-57.8132103173503,-18.5843471808455,
3.23423045308354));
#247873=CARTESIAN_POINT('Ctrl Pts',(-57.9804289733662,-18.5051441132844,
3.36123028058468));
#247874=CARTESIAN_POINT('Ctrl Pts',(-57.9411838150806,-18.6259282908539,
3.36123028058468));
#247875=CARTESIAN_POINT('Ctrl Pts',(-57.9411838150806,-18.6259282908539,
3.23423028058468));
#247876=CARTESIAN_POINT('Origin',(-57.666618181546,-18.4031808061316,3.42473028058467));
#247877=CARTESIAN_POINT('Origin',(-57.5892494801773,-18.3780421908695,3.56563113524827));
#247878=CARTESIAN_POINT('Origin',(-55.9845461696115,-25.2734729067952,3.56647653909449));
#247879=CARTESIAN_POINT('Origin',(-56.0249274780511,-25.2915084057487,3.64299466007633));
#247880=CARTESIAN_POINT('Origin',(-55.9097831300745,-25.2401862573144,3.42473028058465));
#247881=CARTESIAN_POINT('Ctrl Pts',(-55.8095395120005,-25.1949317875303,
3.48823028058466));
#247882=CARTESIAN_POINT('Ctrl Pts',(-55.8614118841077,-25.0796311836956,
3.48794691941582));
#247883=CARTESIAN_POINT('Ctrl Pts',(-55.9614386837451,-25.1241659841938,
3.42473028058467));
#247884=CARTESIAN_POINT('Ctrl Pts',(-55.7683775656455,-25.1767321129116,
3.41028005925067));
#247885=CARTESIAN_POINT('Ctrl Pts',(-55.8200852551846,-25.0612313830326,
3.40982512230957));
#247886=CARTESIAN_POINT('Ctrl Pts',(-55.8997670518381,-25.096708004599,
3.30780486372802));
#247887=CARTESIAN_POINT('Ctrl Pts',(-55.690396180789,-25.1422534028259,
3.36123028058463));
#247888=CARTESIAN_POINT('Ctrl Pts',(-55.7418796630183,-25.026412010048,
3.36099721048382));
#247889=CARTESIAN_POINT('Ctrl Pts',(-55.7829311357716,-25.0446893032919,
3.23423045308383));
#247890=CARTESIAN_POINT('Ctrl Pts',(-55.6083495590299,-25.1059793847704,
3.36123028058463));
#247891=CARTESIAN_POINT('Ctrl Pts',(-55.6600051127006,-24.9899591116498,
3.36123028058464));
#247892=CARTESIAN_POINT('Ctrl Pts',(-55.6600051127006,-24.9899591116498,
3.23423028058463));
#247893=CARTESIAN_POINT('Origin',(-55.6083495590299,-25.1059793847704,3.23423028058462));
#247894=CARTESIAN_POINT('Origin',(0.129138884176574,-0.290050682801341,
3.64303198860262));
#247895=CARTESIAN_POINT('Origin',(-56.3916032444848,-25.4547063934086,3.64303198860244));
#247896=CARTESIAN_POINT('Origin',(0.129138884176574,-0.290050682801338,
3.23423028058481));
#247897=CARTESIAN_POINT('Origin',(-55.4702140717965,-25.044477503395,3.23423028058463));
#247898=CARTESIAN_POINT('Ctrl Pts',(-56.8833377255392,-25.6742415049982,
3.47153072139053));
#247899=CARTESIAN_POINT('Ctrl Pts',(-56.9357219056855,-25.5577357840975,
3.47182327902644));
#247900=CARTESIAN_POINT('Ctrl Pts',(-56.8366797759155,-25.5138485805641,
3.40413028959036));
#247901=CARTESIAN_POINT('Ctrl Pts',(-56.7783442778551,-25.6273680143744,
3.65553807120938));
#247902=CARTESIAN_POINT('Ctrl Pts',(-56.8305359187788,-25.5109042502505,
3.65586275496827));
#247903=CARTESIAN_POINT('Ctrl Pts',(-56.7526780286657,-25.4764485929306,
3.55128126837231));
#247904=CARTESIAN_POINT('Ctrl Pts',(-56.589727673884,-25.5431608329973,
3.77003198860245));
#247905=CARTESIAN_POINT('Ctrl Pts',(-56.6417212312968,-25.4268390553501,
3.77025505748496));
#247906=CARTESIAN_POINT('Ctrl Pts',(-56.6017723050744,-25.4092610357548,
3.64284211731128));
#247907=CARTESIAN_POINT('Ctrl Pts',(-56.3916032444848,-25.4547063934086,
3.77003198860245));
#247908=CARTESIAN_POINT('Ctrl Pts',(-56.4433359691572,-25.3385127913803,
3.77003198860245));
#247909=CARTESIAN_POINT('Ctrl Pts',(-56.4432587405966,-25.3386862495674,
3.64284239821732));
#247910=CARTESIAN_POINT('Origin',(-56.7851714777845,-25.6299342604998,3.40423097483292));
#247911=CARTESIAN_POINT('Ctrl Pts',(-55.4702140717965,-25.044477503395,
3.36123028058463));
#247912=CARTESIAN_POINT('Ctrl Pts',(-55.5218696254671,-24.9284572302744,
3.36123028058463));
#247913=CARTESIAN_POINT('Ctrl Pts',(-55.5218696254671,-24.9284572302744,
3.23423028058463));
#247914=CARTESIAN_POINT('Ctrl Pts',(-55.3878899076689,-25.0080814159077,
3.36123028058463));
#247915=CARTESIAN_POINT('Ctrl Pts',(-55.4395618538395,-24.891811449323,
3.36146538609948));
#247916=CARTESIAN_POINT('Ctrl Pts',(-55.3985281293145,-24.8735420580984,
3.23423043688414));
#247917=CARTESIAN_POINT('Ctrl Pts',(-55.3100454158615,-24.9736678430974,
3.41054258693083));
#247918=CARTESIAN_POINT('Ctrl Pts',(-55.3621286647007,-24.8573359723233,
3.41100608859791));
#247919=CARTESIAN_POINT('Ctrl Pts',(-55.281899950892,-24.8216158475494,
3.30819866970784));
#247920=CARTESIAN_POINT('Ctrl Pts',(-55.2690209153038,-24.9555320242418,
3.48823028058463));
#247921=CARTESIAN_POINT('Ctrl Pts',(-55.3213695969754,-24.8391888661847,
3.48852004212241));
#247922=CARTESIAN_POINT('Ctrl Pts',(-55.2204359898054,-24.794250328961,
3.42473028058463));
#247923=CARTESIAN_POINT('Origin',(-55.1687804361348,-24.9102706020816,3.42473028058462));
#247924=CARTESIAN_POINT('Origin',(-56.9479187893834,-25.7023940320541,3.11913648178483));
#247925=CARTESIAN_POINT('Origin',(-57.1106661007663,-25.774853803565,2.83404198860243));
#247926=CARTESIAN_POINT('Origin',(-55.0944632682977,-24.8771824671427,3.56563113460843));
#247927=CARTESIAN_POINT('Origin',(-55.0536014459533,-24.8590452239606,3.64299171721736));
#247928=CARTESIAN_POINT('Ctrl Pts',(-57.505263737773,-25.61970381813,2.59908173516005));
#247929=CARTESIAN_POINT('Ctrl Pts',(-57.4711877340327,-25.6045223014064,
2.65878198860243));
#247930=CARTESIAN_POINT('Ctrl Pts',(-57.4068835917977,-25.5758735661211,
2.65878198860243));
#247931=CARTESIAN_POINT('Ctrl Pts',(-57.4694043465864,-25.7001924885133,
2.59908193475593));
#247932=CARTESIAN_POINT('Ctrl Pts',(-57.4450643815381,-25.6631501095106,
2.65878715325272));
#247933=CARTESIAN_POINT('Ctrl Pts',(-57.3861185493435,-25.6224598624446,
2.65878198860243));
#247934=CARTESIAN_POINT('Ctrl Pts',(-57.413464248775,-25.7642825572403,
2.63878778849862));
#247935=CARTESIAN_POINT('Ctrl Pts',(-57.3998804953982,-25.7077329912391,
2.695644601801));
#247936=CARTESIAN_POINT('Ctrl Pts',(-57.3441059191826,-25.6552692732806,
2.6818048162487));
#247937=CARTESIAN_POINT('Ctrl Pts',(-57.3036982377901,-25.8321626496792,
2.75443238878616));
#247938=CARTESIAN_POINT('Ctrl Pts',(-57.3186021074456,-25.7409042554409,
2.79268340777062));
#247939=CARTESIAN_POINT('Ctrl Pts',(-57.2526112478171,-25.6821129719829,
2.74885926835585));
#247940=CARTESIAN_POINT('Ctrl Pts',(-57.2503778226939,-25.8376543496546,
2.82856655361658));
#247941=CARTESIAN_POINT('Ctrl Pts',(-57.2821097063791,-25.7289491719107,
2.85384197230723));
#247942=CARTESIAN_POINT('Ctrl Pts',(-57.2038640469253,-25.6773293952365,
2.79184624278389));
#247943=CARTESIAN_POINT('Ctrl Pts',(-57.2088336324697,-25.8191582032623,
2.90134173516005));
#247944=CARTESIAN_POINT('Ctrl Pts',(-57.2611357920723,-25.7028284190336,
2.90163218716373));
#247945=CARTESIAN_POINT('Ctrl Pts',(-57.1623216544369,-25.6588335304443,
2.83404198860243));
#247946=CARTESIAN_POINT('Origin',(-57.4068835917977,-25.5758735661211,2.53178198860243));
#247947=CARTESIAN_POINT('Origin',(0.129138884176574,-0.290050682801341,
3.64303198860262));
#247948=CARTESIAN_POINT('Origin',(-54.6869600343295,-24.695750338031,3.64303198860244));
#247949=CARTESIAN_POINT('Origin',(1.20426471881346E-16,1.91644501385063E-13,
2.53178198860262));
#247950=CARTESIAN_POINT('Origin',(-57.4192809246787,-25.5480287005721,2.53178198860243));
#247951=CARTESIAN_POINT('Ctrl Pts',(-54.6869600343295,-24.695750338031,
3.77003198860245));
#247952=CARTESIAN_POINT('Ctrl Pts',(-54.7386929703522,-24.5795562613021,
3.77003198860245));
#247953=CARTESIAN_POINT('Ctrl Pts',(-54.7386155301258,-24.5797301948983,
3.64284187937016));
#247954=CARTESIAN_POINT('Ctrl Pts',(-54.4888352915928,-24.6072881749595,
3.77003198860245));
#247955=CARTESIAN_POINT('Ctrl Pts',(-54.5406489234192,-24.4913819335271,
3.76980208962808));
#247956=CARTESIAN_POINT('Ctrl Pts',(-54.5800991622554,-24.5091541605501,
3.64284193928258));
#247957=CARTESIAN_POINT('Ctrl Pts',(-54.3002245846692,-24.5230714236785,
3.65553535416566));
#247958=CARTESIAN_POINT('Ctrl Pts',(-54.3520673354853,-24.4074205468523,
3.65520057834542));
#247959=CARTESIAN_POINT('Ctrl Pts',(-54.4291945615855,-24.4419671033161,
3.55127910964222));
#247960=CARTESIAN_POINT('Ctrl Pts',(-54.195235491187,-24.4761921430394,
3.47153072139054));
#247961=CARTESIAN_POINT('Ctrl Pts',(-54.2471777873469,-24.3607210114367,
3.47122746281565));
#247962=CARTESIAN_POINT('Ctrl Pts',(-54.3451938439591,-24.404567574091,
3.40413045901249));
#247963=CARTESIAN_POINT('Origin',(-54.2933913980362,-24.5205222915154,3.40423097483292));
#247964=CARTESIAN_POINT('Ctrl Pts',(-57.4675553545138,-25.2380597013433,
2.90134173516005));
#247965=CARTESIAN_POINT('Ctrl Pts',(-57.4161024530841,-25.3547675996718,
2.90163218716372));
#247966=CARTESIAN_POINT('Ctrl Pts',(-57.3172883154488,-25.3107727110825,
2.83404198860243));
#247967=CARTESIAN_POINT('Ctrl Pts',(-57.5091180232691,-25.2565651278911,
2.82853349835322));
#247968=CARTESIAN_POINT('Ctrl Pts',(-57.4495672328898,-25.3528749970538,
2.85381483162274));
#247969=CARTESIAN_POINT('Ctrl Pts',(-57.3588496371379,-25.3292770036978,
2.79182701594154));
#247970=CARTESIAN_POINT('Ctrl Pts',(-57.5405471770606,-25.2997972770061,
2.75468822073643));
#247971=CARTESIAN_POINT('Ctrl Pts',(-57.482714899638,-25.3720159720864,
2.79286913083823));
#247972=CARTESIAN_POINT('Ctrl Pts',(-57.3948558336728,-25.3622324578622,
2.74900763297892));
#247973=CARTESIAN_POINT('Ctrl Pts',(-57.5636463159494,-25.4257977880272,
2.63954450640355));
#247974=CARTESIAN_POINT('Ctrl Pts',(-57.5124644612013,-25.4538910783598,
2.69627684028832));
#247975=CARTESIAN_POINT('Ctrl Pts',(-57.4360631077225,-25.447559735724,
2.68224356036474));
#247976=CARTESIAN_POINT('Ctrl Pts',(-57.553621128909,-25.5110385513889,
2.59908178706347));
#247977=CARTESIAN_POINT('Ctrl Pts',(-57.5097883065914,-25.5177778164706,
2.65878704321553));
#247978=CARTESIAN_POINT('Ctrl Pts',(-57.4400754463034,-25.5012707422377,
2.65878198860243));
#247979=CARTESIAN_POINT('Ctrl Pts',(-57.5176823163886,-25.5918112338797,
2.59908173516005));
#247980=CARTESIAN_POINT('Ctrl Pts',(-57.4835989537475,-25.5766462455179,
2.65878198860242));
#247981=CARTESIAN_POINT('Ctrl Pts',(-57.4192809246787,-25.5480287005721,
2.65878198860243));
#247982=CARTESIAN_POINT('Origin',(-57.3689438691194,-25.1947524379619,2.83404198860243));
#247983=CARTESIAN_POINT('Origin',(-54.1306438627469,-24.4480624203116,3.119136481669));
#247984=CARTESIAN_POINT('Origin',(-53.9678963272933,-24.3756025490941,2.83404198860245));
#247985=CARTESIAN_POINT('Origin',(-57.2061965577021,-25.122292666487,3.1191364817743));
#247986=CARTESIAN_POINT('Origin',(-57.0434492461377,-25.0498328948967,3.40423097483292));
#247987=CARTESIAN_POINT('Ctrl Pts',(-53.8697418420143,-24.331269253109,
2.90134173516006));
#247988=CARTESIAN_POINT('Ctrl Pts',(-53.9216078643415,-24.2159747902189,
2.90103711553211));
#247989=CARTESIAN_POINT('Ctrl Pts',(-54.0195518809639,-24.2595822759735,
2.83404198860244));
#247990=CARTESIAN_POINT('Ctrl Pts',(-53.8282341734841,-24.312788266218,
2.82862991747947));
#247991=CARTESIAN_POINT('Ctrl Pts',(-53.8880114973696,-24.2176496934278,
2.85314045886338));
#247992=CARTESIAN_POINT('Ctrl Pts',(-53.9780422761238,-24.2411010091829,
2.79187960999867));
#247993=CARTESIAN_POINT('Ctrl Pts',(-53.7969955864425,-24.2697746459844,
2.75470625793306));
#247994=CARTESIAN_POINT('Ctrl Pts',(-53.8549480733037,-24.198315211449,
2.79224250381917));
#247995=CARTESIAN_POINT('Ctrl Pts',(-53.9422730280817,-24.2082687574724,
2.74901809108243));
#247996=CARTESIAN_POINT('Ctrl Pts',(-53.7744913425365,-24.144338822604,
2.63947868311684));
#247997=CARTESIAN_POINT('Ctrl Pts',(-53.8256450222191,-24.1165167429226,
2.6959506676787));
#247998=CARTESIAN_POINT('Ctrl Pts',(-53.9017956184507,-24.1232032230477,
2.68220539436042));
#247999=CARTESIAN_POINT('Ctrl Pts',(-53.7848917482046,-24.0595120258536,
2.59908178585046));
#248000=CARTESIAN_POINT('Ctrl Pts',(-53.8286685158642,-24.0529122166849,
2.65877670944823));
#248001=CARTESIAN_POINT('Ctrl Pts',(-53.8982652496121,-24.0696665464385,
2.65878198860244));
#248002=CARTESIAN_POINT('Ctrl Pts',(-53.8206887816834,-23.9791663275016,
2.59908173516006));
#248003=CARTESIAN_POINT('Ctrl Pts',(-53.8547645473079,-23.9943483786819,
2.65878198860244));
#248004=CARTESIAN_POINT('Ctrl Pts',(-53.9190682401993,-24.0229981225299,
2.65878198860244));
#248005=CARTESIAN_POINT('Origin',(-53.9190682401993,-24.0229981225299,2.53178198860244));
#248006=CARTESIAN_POINT('Ctrl Pts',(-56.649881012838,-24.8746050278055,
3.77003198860245));
#248007=CARTESIAN_POINT('Ctrl Pts',(-56.5981482837086,-24.9907986398445,
3.77003198860245));
#248008=CARTESIAN_POINT('Ctrl Pts',(-56.5982255167329,-24.9906251716318,
3.64284238727567));
#248009=CARTESIAN_POINT('Ctrl Pts',(-56.8481896769752,-24.9626539694732,
3.77003198860245));
#248010=CARTESIAN_POINT('Ctrl Pts',(-56.7965362315762,-25.0791271905735,
3.77025506105898));
#248011=CARTESIAN_POINT('Ctrl Pts',(-56.756741544354,-25.0612010539384,
3.64284210641817));
#248012=CARTESIAN_POINT('Ctrl Pts',(-57.0369754593333,-25.0464771582507,
3.65553527987811));
#248013=CARTESIAN_POINT('Ctrl Pts',(-56.9853490357224,-25.1631925873298,
3.65585996532915));
#248014=CARTESIAN_POINT('Ctrl Pts',(-56.9076460727639,-25.1283880784738,
3.55127902710193));
#248015=CARTESIAN_POINT('Ctrl Pts',(-57.1420619865019,-25.0931373005748,
3.47153072139054));
#248016=CARTESIAN_POINT('Ctrl Pts',(-57.0905332166518,-25.2100238867502,
3.47182327905171));
#248017=CARTESIAN_POINT('Ctrl Pts',(-56.9916465440539,-25.1657874977296,
3.40413028377963));
#248018=CARTESIAN_POINT('Origin',(-56.649881012838,-24.8746050278055,3.64303198860245));
#248019=CARTESIAN_POINT('Origin',(3.58382961824623E-16,1.91553576693918E-13,
2.53178198860262));
#248020=CARTESIAN_POINT('Origin',(-53.9314655730802,-23.995153256981,2.53178198860244));
#248021=CARTESIAN_POINT('Origin',(51.799563747336,23.4101986852084,3.64303198860279));
#248022=CARTESIAN_POINT('Origin',(-56.2832472948498,-24.7113125977909,3.64299466007597));
#248023=CARTESIAN_POINT('Ctrl Pts',(-53.8330634946836,-23.9513722670367,
2.59908173516006));
#248024=CARTESIAN_POINT('Ctrl Pts',(-53.8671470951729,-23.9665367208226,
2.65878198860245));
#248025=CARTESIAN_POINT('Ctrl Pts',(-53.9314655730802,-23.995153256981,
2.65878198860244));
#248026=CARTESIAN_POINT('Ctrl Pts',(-53.8686972660494,-23.8712821658119,
2.59908193199817));
#248027=CARTESIAN_POINT('Ctrl Pts',(-53.8931046959169,-23.9081865738546,
2.65877685806513));
#248028=CARTESIAN_POINT('Ctrl Pts',(-53.9521563342717,-23.9486256024595,
2.65878198860244));
#248029=CARTESIAN_POINT('Ctrl Pts',(-53.9240892607409,-23.8071866393156,
2.63872492669793));
#248030=CARTESIAN_POINT('Ctrl Pts',(-53.9378509529598,-23.8635355386145,
2.69532212015263));
#248031=CARTESIAN_POINT('Ctrl Pts',(-53.9937257232526,-23.915575084618,
2.68176836726614));
#248032=CARTESIAN_POINT('Ctrl Pts',(-54.0330064121712,-23.7392497560572,
2.75442176402219));
#248033=CARTESIAN_POINT('Ctrl Pts',(-54.0187512923758,-23.8300830854579,
2.7920317992011));
#248034=CARTESIAN_POINT('Ctrl Pts',(-54.0845104630311,-23.8883623535217,
2.7488531074816));
#248035=CARTESIAN_POINT('Ctrl Pts',(-54.086059454542,-23.7337507958622,
2.82866089558392));
#248036=CARTESIAN_POINT('Ctrl Pts',(-54.0553500291286,-23.8418399747428,
2.85316563119167));
#248037=CARTESIAN_POINT('Ctrl Pts',(-54.1330265677737,-23.8930480394869,
2.79189751796623));
#248038=CARTESIAN_POINT('Ctrl Pts',(-54.1275498658872,-23.752222950883,
2.90134173516006));
#248039=CARTESIAN_POINT('Ctrl Pts',(-54.0765745253534,-23.8679139708571,
2.90103711553212));
#248040=CARTESIAN_POINT('Ctrl Pts',(-54.1745185419758,-23.9115214566117,
2.83404198860244));
#248041=CARTESIAN_POINT('Origin',(-54.2261740956464,-23.7955011834911,2.83404198860245));
#248042=CARTESIAN_POINT('Origin',(-56.242823936856,-24.6933715410275,3.56647653971793));
#248043=CARTESIAN_POINT('Origin',(-56.1680608984276,-24.6600848917114,3.42473028058466));
#248044=CARTESIAN_POINT('Origin',(-54.3889216310586,-23.8679610547533,3.11913648168129));
#248045=CARTESIAN_POINT('Origin',(-54.5516691663893,-23.9404209259123,3.40423097483293));
#248046=CARTESIAN_POINT('Ctrl Pts',(-55.8666273273831,-24.5258780191674,
3.36123028058464));
#248047=CARTESIAN_POINT('Ctrl Pts',(-55.8149717737125,-24.641898292288,
3.36123028058463));
#248048=CARTESIAN_POINT('Ctrl Pts',(-55.8149717737125,-24.641898292288,
3.23423028058464));
#248049=CARTESIAN_POINT('Ctrl Pts',(-55.9487607347574,-24.5627025231282,
3.36123028058464));
#248050=CARTESIAN_POINT('Ctrl Pts',(-55.897123215877,-24.678474470879,3.36099641108452));
#248051=CARTESIAN_POINT('Ctrl Pts',(-55.9383132588146,-24.696813459544,
3.23423043688322));
#248052=CARTESIAN_POINT('Ctrl Pts',(-56.0264248009273,-24.5975211960728,
3.41054258905264));
#248053=CARTESIAN_POINT('Ctrl Pts',(-55.9751910510473,-24.7132325104972,
3.41008815825997));
#248054=CARTESIAN_POINT('Ctrl Pts',(-56.0549414076416,-24.7487396569162,
3.30819867304297));
#248055=CARTESIAN_POINT('Ctrl Pts',(-56.0673542004324,-24.6158705164596,
3.48823028058465));
#248056=CARTESIAN_POINT('Ctrl Pts',(-56.0163785451196,-24.7315703643338,
3.48794691941581));
#248057=CARTESIAN_POINT('Ctrl Pts',(-56.116405344757,-24.776105164832,3.42473028058466));
#248058=CARTESIAN_POINT('Origin',(-55.8666273273831,-24.5258780191674,3.23423028058464));
#248059=CARTESIAN_POINT('Ctrl Pts',(-54.4530463244691,-23.8971395307771,
3.47153072139055));
#248060=CARTESIAN_POINT('Ctrl Pts',(-54.401990736535,-24.0130054343462,
3.4712274628506));
#248061=CARTESIAN_POINT('Ctrl Pts',(-54.50016060885,-24.0565064908994,3.40413046676784));
#248062=CARTESIAN_POINT('Ctrl Pts',(-54.5581374230422,-23.9437939758161,
3.65553813457969));
#248063=CARTESIAN_POINT('Ctrl Pts',(-54.5068816478285,-24.0597061770699,
3.65520336072201));
#248064=CARTESIAN_POINT('Ctrl Pts',(-54.5841625982709,-24.0939065860612,
3.55128134519895));
#248065=CARTESIAN_POINT('Ctrl Pts',(-54.7469293531953,-24.0276077026094,
3.77003198860246));
#248066=CARTESIAN_POINT('Ctrl Pts',(-54.6954643138418,-24.1436691352835,
3.76980209314012));
#248067=CARTESIAN_POINT('Ctrl Pts',(-54.7350683949941,-24.161094175271,
3.64284195387423));
#248068=CARTESIAN_POINT('Ctrl Pts',(-54.9452378026827,-24.1156489724279,
3.77003198860246));
#248069=CARTESIAN_POINT('Ctrl Pts',(-54.8935048726349,-24.2318430357369,
3.77003198860246));
#248070=CARTESIAN_POINT('Ctrl Pts',(-54.8935823068775,-24.2316691155806,
3.64284189403811));
#248071=CARTESIAN_POINT('Origin',(-54.9452378026827,-24.1156489724279,3.64303198860245));
#248072=CARTESIAN_POINT('Origin',(50.541702139688,22.8501626153352,3.23423028058498));
#248073=CARTESIAN_POINT('Origin',(-55.7284918401496,-24.4643761377919,3.23423028058464));
#248074=CARTESIAN_POINT('Origin',(50.3447265545023,22.7624634345051,3.64303198860279));
#248075=CARTESIAN_POINT('Origin',(-55.3119205422643,-24.2788510342452,3.642991717218));
#248076=CARTESIAN_POINT('Ctrl Pts',(-55.5277679687681,-24.3743766270216,
3.48823028058463));
#248077=CARTESIAN_POINT('Ctrl Pts',(-55.4763362579872,-24.4911280468229,
3.48852004212241));
#248078=CARTESIAN_POINT('Ctrl Pts',(-55.3754026508173,-24.4461895095991,
3.42473028058463));
#248079=CARTESIAN_POINT('Ctrl Pts',(-55.5688345658074,-24.3927905570406,
3.41028005848388));
#248080=CARTESIAN_POINT('Ctrl Pts',(-55.5172331055236,-24.5093364964831,
3.41074404220487));
#248081=CARTESIAN_POINT('Ctrl Pts',(-55.4370743056943,-24.4736474994208,
3.30780486243963));
#248082=CARTESIAN_POINT('Ctrl Pts',(-55.6466353090192,-24.4276751358089,
3.36123028058464));
#248083=CARTESIAN_POINT('Ctrl Pts',(-55.5948055748745,-24.5438739850307,
3.36146460586237));
#248084=CARTESIAN_POINT('Ctrl Pts',(-55.5539102504896,-24.5256662135188,
3.23423045308347));
#248085=CARTESIAN_POINT('Ctrl Pts',(-55.7284918401496,-24.4643761377919,
3.36123028058464));
#248086=CARTESIAN_POINT('Ctrl Pts',(-55.676836286479,-24.5803964109126,
3.36123028058464));
#248087=CARTESIAN_POINT('Ctrl Pts',(-55.676836286479,-24.5803964109126,
3.23423028058464));
#248088=CARTESIAN_POINT('Origin',(-55.4270582044879,-24.3301692364785,3.42473028058463));
#248089=CARTESIAN_POINT('Origin',(-55.3527410377819,-24.2970811017172,3.56563113524668));
#248090=CARTESIAN_POINT('Origin',(-53.0360596835501,-30.9870007556522,3.56647653909445));
#248091=CARTESIAN_POINT('Origin',(-53.0743345559668,-31.0091584503696,3.64299466007742));
#248092=CARTESIAN_POINT('Origin',(-52.9651856060843,-30.9460815882871,3.42473028058462));
#248093=CARTESIAN_POINT('Ctrl Pts',(-52.8702215132213,-30.8905967158739,
3.48823028058461));
#248094=CARTESIAN_POINT('Ctrl Pts',(-52.9338619179793,-30.7813498801535,
3.48794691941577));
#248095=CARTESIAN_POINT('Ctrl Pts',(-53.0286856060843,-30.8360963620065,
3.42473028058462));
#248096=CARTESIAN_POINT('Ctrl Pts',(-52.8311874403352,-30.8681941459794,
3.41028005925063));
#248097=CARTESIAN_POINT('Ctrl Pts',(-52.8946849835383,-30.7587310665098,
3.40982512230992));
#248098=CARTESIAN_POINT('Ctrl Pts',(-52.9702219582405,-30.802342359186,
3.30780486372843));
#248099=CARTESIAN_POINT('Ctrl Pts',(-52.7572372522459,-30.8257530395509,
3.36123028058459));
#248100=CARTESIAN_POINT('Ctrl Pts',(-52.8205474253439,-30.7159277273265,
3.36099721048426));
#248101=CARTESIAN_POINT('Ctrl Pts',(-52.8594635164569,-30.7383959430072,
3.23423045308352));
#248102=CARTESIAN_POINT('Ctrl Pts',(-52.6794317578285,-30.7811015270746,
3.36123028058459));
#248103=CARTESIAN_POINT('Ctrl Pts',(-52.7429317578285,-30.671116300794,
3.36123028058459));
#248104=CARTESIAN_POINT('Ctrl Pts',(-52.7429317578285,-30.671116300794,
3.23423028058459));
#248105=CARTESIAN_POINT('Origin',(-52.6794317578285,-30.7811015270746,3.23423028058459));
#248106=CARTESIAN_POINT('Origin',(0.158750000000008,-0.274963065701374,
3.64303198860262));
#248107=CARTESIAN_POINT('Origin',(-53.4219427993284,-31.2097904767609,3.6430319886024));
#248108=CARTESIAN_POINT('Origin',(0.158750000000008,-0.274963065701371,
3.23423028058481));
#248109=CARTESIAN_POINT('Origin',(-52.5484816883957,-30.7054974692372,3.23423028058459));
#248110=CARTESIAN_POINT('Ctrl Pts',(-53.8880358395968,-31.4795232016792,
3.47153072139049));
#248111=CARTESIAN_POINT('Ctrl Pts',(-53.9523112176908,-31.369131349158,
3.4718232790264));
#248112=CARTESIAN_POINT('Ctrl Pts',(-53.858399113013,-31.3151318426939,
3.40413028959031));
#248113=CARTESIAN_POINT('Ctrl Pts',(-53.7885171709483,-31.4219316852007,
3.65553807120931));
#248114=CARTESIAN_POINT('Ctrl Pts',(-53.8525966788936,-31.3115614337838,
3.655862754969));
#248115=CARTESIAN_POINT('Ctrl Pts',(-53.7787668993573,-31.269156162554,
3.55128126837173));
#248116=CARTESIAN_POINT('Ctrl Pts',(-53.6097358757349,-31.3184699958134,
3.7700319886024));
#248117=CARTESIAN_POINT('Ctrl Pts',(-53.6736035436603,-31.2082202476924,
3.77025505748431));
#248118=CARTESIAN_POINT('Ctrl Pts',(-53.6357108652121,-31.1865627224613,
3.64284211731183));
#248119=CARTESIAN_POINT('Ctrl Pts',(-53.4219427993284,-31.2097904767609,
3.77003198860241));
#248120=CARTESIAN_POINT('Ctrl Pts',(-53.4855376653836,-31.0996409376526,
3.77003198860241));
#248121=CARTESIAN_POINT('Ctrl Pts',(-53.4854427285714,-31.0998053730349,
3.64284239821726));
#248122=CARTESIAN_POINT('Origin',(-53.7950387249976,-31.4251975098795,3.40423097483288));
#248123=CARTESIAN_POINT('Ctrl Pts',(-52.5484816883957,-30.7054974692372,
3.36123028058459));
#248124=CARTESIAN_POINT('Ctrl Pts',(-52.6119816883957,-30.5955122429565,
3.36123028058459));
#248125=CARTESIAN_POINT('Ctrl Pts',(-52.6119816883957,-30.5955122429565,
3.23423028058459));
#248126=CARTESIAN_POINT('Ctrl Pts',(-52.4704129317469,-30.6606955449592,
3.36123028058459));
#248127=CARTESIAN_POINT('Ctrl Pts',(-52.5339553345213,-30.5504637065434,
3.36146538610071));
#248128=CARTESIAN_POINT('Ctrl Pts',(-52.4950560684224,-30.5280052047898,
3.23423043688392));
#248129=CARTESIAN_POINT('Ctrl Pts',(-52.3965920780926,-30.6183335281981,
3.41054258693078));
#248130=CARTESIAN_POINT('Ctrl Pts',(-52.4605500011258,-30.5080831175488,
3.41100608859706));
#248131=CARTESIAN_POINT('Ctrl Pts',(-52.3844945583554,-30.4641724871906,
3.30819866970773));
#248132=CARTESIAN_POINT('Ctrl Pts',(-52.357688023316,-30.5960088312571,
3.48823028058459));
#248133=CARTESIAN_POINT('Ctrl Pts',(-52.4219111049554,-30.4857749404422,
3.48852004212237));
#248134=CARTESIAN_POINT('Ctrl Pts',(-52.3262277788839,-30.4305321463779,
3.42473028058459));
#248135=CARTESIAN_POINT('Origin',(-52.2627277788839,-30.5405173726585,3.42473028058459));
#248136=CARTESIAN_POINT('Origin',(-53.9493203812227,-31.5142720656061,3.1191364817832));
#248137=CARTESIAN_POINT('Origin',(-54.1036020372436,-31.6033466212668,2.83404198860239));
#248138=CARTESIAN_POINT('Origin',(-52.1922763801639,-30.4998422386361,3.56563113460743));
#248139=CARTESIAN_POINT('Origin',(-52.1535342613171,-30.4775331296743,3.64299171721718));
#248140=CARTESIAN_POINT('Ctrl Pts',(-54.5122556166608,-31.490293248291,
2.59908173516001));
#248141=CARTESIAN_POINT('Ctrl Pts',(-54.4799531854477,-31.4716329851992,
2.65878198860239));
#248142=CARTESIAN_POINT('Ctrl Pts',(-54.4189959163061,-31.4364195775138,
2.65878198860239));
#248143=CARTESIAN_POINT('Ctrl Pts',(-54.4681793099457,-31.5665926662618,
2.59908193475578));
#248144=CARTESIAN_POINT('Ctrl Pts',(-54.447844664727,-31.5272089901454,
2.65878715325339));
#248145=CARTESIAN_POINT('Ctrl Pts',(-54.3934750329619,-31.4805801312535,
2.65878198860239));
#248146=CARTESIAN_POINT('Ctrl Pts',(-54.4058464214485,-31.6244843104274,
2.63878778849827));
#248147=CARTESIAN_POINT('Ctrl Pts',(-54.3982481205271,-31.5668246399999,
2.69564460180128));
#248148=CARTESIAN_POINT('Ctrl Pts',(-54.3482630350909,-31.5088182930364,
2.68180481624867));
#248149=CARTESIAN_POINT('Ctrl Pts',(-54.2895863184074,-31.6805188761699,
2.75443238878644));
#248150=CARTESIAN_POINT('Ctrl Pts',(-54.313947642815,-31.5913182835554,
2.79268340777014));
#248151=CARTESIAN_POINT('Ctrl Pts',(-54.254463650534,-31.5259511417531,
2.7488592683558));
#248152=CARTESIAN_POINT('Ctrl Pts',(-54.2359839591649,-31.6804069909882,
2.82856655361631));
#248153=CARTESIAN_POINT('Ctrl Pts',(-54.2789047974503,-31.5756141966208,
2.85384197230784));
#248154=CARTESIAN_POINT('Ctrl Pts',(-54.2064835118363,-31.5160982999434,
2.79184624278431));
#248155=CARTESIAN_POINT('Ctrl Pts',(-54.1966007261205,-31.6576696180587,
2.90134173516001));
#248156=CARTESIAN_POINT('Ctrl Pts',(-54.260776142598,-31.5474441649286,
2.90163218716368));
#248157=CARTESIAN_POINT('Ctrl Pts',(-54.1671020372436,-31.4933613949861,
2.83404198860239));
#248158=CARTESIAN_POINT('Origin',(-54.4189959163061,-31.4364195775138,2.53178198860238));
#248159=CARTESIAN_POINT('Origin',(0.158750000000008,-0.274963065701374,
3.64303198860262));
#248160=CARTESIAN_POINT('Origin',(-51.8059703131944,-30.2768083268883,3.64303198860241));
#248161=CARTESIAN_POINT('Origin',(1.12590909550281E-16,1.9165987954201E-13,
2.53178198860262));
#248162=CARTESIAN_POINT('Origin',(-54.4342359163061,-31.4100231232064,2.53178198860239));
#248163=CARTESIAN_POINT('Ctrl Pts',(-51.8059703131944,-30.2768083268883,
3.77003198860241));
#248164=CARTESIAN_POINT('Ctrl Pts',(-51.8695654390618,-30.1666583377722,
3.77003198860241));
#248165=CARTESIAN_POINT('Ctrl Pts',(-51.8694702420496,-30.166823223834,
3.64284187937022));
#248166=CARTESIAN_POINT('Ctrl Pts',(-51.6181777324909,-30.1681210939099,
3.77003198860241));
#248167=CARTESIAN_POINT('Ctrl Pts',(-51.6818230251198,-30.0582657983055,
3.7698020896317));
#248168=CARTESIAN_POINT('Ctrl Pts',(-51.7191994478415,-30.0800643400498,
3.64284193928267));
#248169=CARTESIAN_POINT('Ctrl Pts',(-51.439403302349,-30.0646505034507,
3.65553535416564));
#248170=CARTESIAN_POINT('Ctrl Pts',(-51.5030508615839,-29.9550522173035,
3.65520057834208));
#248171=CARTESIAN_POINT('Ctrl Pts',(-51.576144478209,-29.997471514538,3.55127910964202));
#248172=CARTESIAN_POINT('Ctrl Pts',(-51.3398895692694,-30.007053683816,
3.47153072139049));
#248173=CARTESIAN_POINT('Ctrl Pts',(-51.4036173400344,-29.8976445635504,
3.47122746281559));
#248174=CARTESIAN_POINT('Ctrl Pts',(-51.4965132406189,-29.9514963979198,
3.40413045901249));
#248175=CARTESIAN_POINT('Origin',(-51.432874005494,-30.0614010732039,3.40423097483288));
#248176=CARTESIAN_POINT('Ctrl Pts',(-54.5146464769135,-31.1067982185537,
2.90134173516001));
#248177=CARTESIAN_POINT('Ctrl Pts',(-54.451276142598,-31.2174884860868,
2.90163218716369));
#248178=CARTESIAN_POINT('Ctrl Pts',(-54.3576020372436,-31.1634057161443,
2.83404198860239));
#248179=CARTESIAN_POINT('Ctrl Pts',(-54.5540471172212,-31.1295467523333,
2.82853349835327));
#248180=CARTESIAN_POINT('Ctrl Pts',(-54.4847554296815,-31.2191042733508,
2.85381483162341));
#248181=CARTESIAN_POINT('Ctrl Pts',(-54.3970014563935,-31.1861529813964,
2.79182701594247));
#248182=CARTESIAN_POINT('Ctrl Pts',(-54.5807851087094,-31.1758273123591,
2.75468822073627));
#248183=CARTESIAN_POINT('Ctrl Pts',(-54.5157207333386,-31.241605266785,
2.79286913083788));
#248184=CARTESIAN_POINT('Ctrl Pts',(-54.4293656242358,-31.2226915745263,
2.74900763297888));
#248185=CARTESIAN_POINT('Ctrl Pts',(-54.5905870683101,-31.3035520968884,
2.63954450640362));
#248186=CARTESIAN_POINT('Ctrl Pts',(-54.5367490446502,-31.3261415286133,
2.69627684028853));
#248187=CARTESIAN_POINT('Ctrl Pts',(-54.4614280312967,-31.3118587536637,
2.6822435603647));
#248188=CARTESIAN_POINT('Ctrl Pts',(-54.571706714292,-31.3872779850341,
2.59908178706265));
#248189=CARTESIAN_POINT('Ctrl Pts',(-54.5274095677421,-31.3893985541604,
2.658787043214));
#248190=CARTESIAN_POINT('Ctrl Pts',(-54.4598040608989,-31.3656949292516,
2.65878198860239));
#248191=CARTESIAN_POINT('Ctrl Pts',(-54.5275217339717,-31.4638515574743,
2.59908173516001));
#248192=CARTESIAN_POINT('Ctrl Pts',(-54.4952102564863,-31.4452069629856,
2.65878198860239));
#248193=CARTESIAN_POINT('Ctrl Pts',(-54.4342359163061,-31.4100231232064,
2.65878198860239));
#248194=CARTESIAN_POINT('Origin',(-54.4211020372436,-31.0534204898637,2.83404198860239));
#248195=CARTESIAN_POINT('Origin',(-51.2785921372155,-29.9723263949887,3.11913648167081));
#248196=CARTESIAN_POINT('Origin',(-51.1243102687782,-29.8832517167488,2.83404198860241));
#248197=CARTESIAN_POINT('Origin',(-54.2668203811882,-30.9643459342369,3.1191364817751));
#248198=CARTESIAN_POINT('Origin',(-54.1125387249976,-30.8752713784764,3.40423097483288));
#248199=CARTESIAN_POINT('Ctrl Pts',(-51.0313275753406,-29.8289013456888,
2.90134173516002));
#248200=CARTESIAN_POINT('Ctrl Pts',(-51.0949610231999,-29.7196599535395,
2.90103711553208));
#248201=CARTESIAN_POINT('Ctrl Pts',(-51.1878102687782,-29.7732664904682,
2.8340419886024));
#248202=CARTESIAN_POINT('Ctrl Pts',(-50.9919790793208,-29.8061828667728,
2.82862991747939));
#248203=CARTESIAN_POINT('Ctrl Pts',(-51.0613736255811,-29.7178139048422,
2.85314045886485));
#248204=CARTESIAN_POINT('Ctrl Pts',(-51.1484598763123,-29.7505475307853,
2.7918796100002));
#248205=CARTESIAN_POINT('Ctrl Pts',(-50.9654077681504,-29.7601395581529,
2.75470625793304));
#248206=CARTESIAN_POINT('Ctrl Pts',(-51.0305123301025,-29.6951292702709,
2.7922425038188));
#248207=CARTESIAN_POINT('Ctrl Pts',(-51.1163184807715,-29.7141562330556,
2.74901809108243));
#248208=CARTESIAN_POINT('Ctrl Pts',(-50.9561384187038,-29.6330385513049,
2.63947868311676));
#248209=CARTESIAN_POINT('Ctrl Pts',(-51.0099200724111,-29.6107158994149,
2.69595066767886));
#248210=CARTESIAN_POINT('Ctrl Pts',(-51.0849545802165,-29.6253256551033,
2.68220539436034));
#248211=CARTESIAN_POINT('Ctrl Pts',(-50.9753486645696,-29.5497635830446,
2.59908178585031));
#248212=CARTESIAN_POINT('Ctrl Pts',(-51.0195754864256,-29.5477758465712,
2.6587767094479));
#248213=CARTESIAN_POINT('Ctrl Pts',(-51.0870396576419,-29.5717132339806,
2.6587819886024));
#248214=CARTESIAN_POINT('Ctrl Pts',(-51.0193480105325,-29.473599835734,
2.59908173516002));
#248215=CARTESIAN_POINT('Ctrl Pts',(-51.0516501490683,-29.4922606054649,
2.65878198860241));
#248216=CARTESIAN_POINT('Ctrl Pts',(-51.1126068659044,-29.5274749692187,
2.65878198860241));
#248217=CARTESIAN_POINT('Origin',(-51.1126068659044,-29.5274749692187,2.5317819886024));
#248218=CARTESIAN_POINT('Ctrl Pts',(-53.7394427993284,-30.6598643453577,
3.77003198860241));
#248219=CARTESIAN_POINT('Ctrl Pts',(-53.6758479277942,-30.7700138939557,
3.77003198860241));
#248220=CARTESIAN_POINT('Ctrl Pts',(-53.6759428700935,-30.7698494490696,
3.64284238727575));
#248221=CARTESIAN_POINT('Ctrl Pts',(-53.9274614872879,-30.7681598456274,
3.77003198860241));
#248222=CARTESIAN_POINT('Ctrl Pts',(-53.8639162380511,-30.8785957589619,
3.77025506105773));
#248223=CARTESIAN_POINT('Ctrl Pts',(-53.8262133418081,-30.8566081460789,
3.64284210641871));
#248224=CARTESIAN_POINT('Ctrl Pts',(-54.1064511722692,-30.8712573299212,
3.6555352798781));
#248225=CARTESIAN_POINT('Ctrl Pts',(-54.0429074791724,-30.9819369489465,
3.65585996533168));
#248226=CARTESIAN_POINT('Ctrl Pts',(-53.9692682429961,-30.9392009315189,
3.55127902710165));
#248227=CARTESIAN_POINT('Ctrl Pts',(-54.2060847114739,-30.9286463962981,
3.4715307213905));
#248228=CARTESIAN_POINT('Ctrl Pts',(-54.1426202463871,-31.0395064423978,
3.47182327905166));
#248229=CARTESIAN_POINT('Ctrl Pts',(-54.0488992470932,-30.9851759130206,
3.40413028377964));
#248230=CARTESIAN_POINT('Origin',(-53.7394427993284,-30.6598643453577,3.64303198860241));
#248231=CARTESIAN_POINT('Origin',(3.61170357355341E-16,1.91548106122166E-13,
2.53178198860262));
#248232=CARTESIAN_POINT('Origin',(-51.1278468659044,-29.5010785149114,2.53178198860241));
#248233=CARTESIAN_POINT('Origin',(46.5080917980719,27.2180767400487,3.64303198860282));
#248234=CARTESIAN_POINT('Origin',(-53.3918862459814,-30.4591427892374,3.64299466007567));
#248235=CARTESIAN_POINT('Ctrl Pts',(-51.0345602039884,-29.4472515437738,
2.59908173516002));
#248236=CARTESIAN_POINT('Ctrl Pts',(-51.0668719738975,-29.465895631477,
2.65878198860241));
#248237=CARTESIAN_POINT('Ctrl Pts',(-51.1278468659044,-29.5010785149114,
2.65878198860241));
#248238=CARTESIAN_POINT('Ctrl Pts',(-51.0783704650301,-29.3713249278647,
2.59908193199787));
#248239=CARTESIAN_POINT('Ctrl Pts',(-51.0987866273839,-29.410578440836,
2.65877685806612));
#248240=CARTESIAN_POINT('Ctrl Pts',(-51.1532877451685,-29.4569685172213,
2.6587819886024));
#248241=CARTESIAN_POINT('Ctrl Pts',(-51.140158823466,-29.3133705634514,
2.63872492669767));
#248242=CARTESIAN_POINT('Ctrl Pts',(-51.1479550638444,-29.3708492661236,
2.69532212015257));
#248243=CARTESIAN_POINT('Ctrl Pts',(-51.1980841325264,-29.4284442379233,
2.68176836726614));
#248244=CARTESIAN_POINT('Ctrl Pts',(-51.2555806533509,-29.2571907880104,
2.75442176402237));
#248245=CARTESIAN_POINT('Ctrl Pts',(-51.2319089562576,-29.3460364571628,
2.79203179920106));
#248246=CARTESIAN_POINT('Ctrl Pts',(-51.2912160489644,-29.4108701703526,
2.74885310748152));
#248247=CARTESIAN_POINT('Ctrl Pts',(-51.3089178634634,-29.2572675046851,
2.82866089558372));
#248248=CARTESIAN_POINT('Ctrl Pts',(-51.2670782717316,-29.361554550688,
2.85316563119145));
#248249=CARTESIAN_POINT('Ctrl Pts',(-51.3389765898555,-29.4206015015121,
2.79189751796623));
#248250=CARTESIAN_POINT('Ctrl Pts',(-51.3482501200163,-29.2799753962465,
2.90134173516001));
#248251=CARTESIAN_POINT('Ctrl Pts',(-51.2854610231999,-29.3897042746976,
2.90103711553208));
#248252=CARTESIAN_POINT('Ctrl Pts',(-51.3783102687782,-29.4433108116264,
2.8340419886024));
#248253=CARTESIAN_POINT('Origin',(-51.4418102687782,-29.3333255853457,2.8340419886024));
#248254=CARTESIAN_POINT('Origin',(-53.3535596824664,-30.4370746239676,3.56647653971759));
#248255=CARTESIAN_POINT('Origin',(-53.2826856060843,-30.396155456884,3.42473028058463));
#248256=CARTESIAN_POINT('Origin',(-51.5960921371733,-29.4224002636277,3.11913648168053));
#248257=CARTESIAN_POINT('Origin',(-51.750374005494,-29.5114749418008,3.4042309748329));
#248258=CARTESIAN_POINT('Ctrl Pts',(-52.9969317578285,-30.2311753956715,
3.3612302805846));
#248259=CARTESIAN_POINT('Ctrl Pts',(-52.9334317578285,-30.3411606219521,
3.3612302805846));
#248260=CARTESIAN_POINT('Ctrl Pts',(-52.9334317578285,-30.3411606219521,
3.23423028058459));
#248261=CARTESIAN_POINT('Ctrl Pts',(-53.0747660209934,-30.276383450003,
3.36123028058459));
#248262=CARTESIAN_POINT('Ctrl Pts',(-53.0113099140563,-30.3861235964148,
3.36099641108464));
#248263=CARTESIAN_POINT('Ctrl Pts',(-53.0503573673265,-30.4086676540709,
3.23423043688365));
#248264=CARTESIAN_POINT('Ctrl Pts',(-53.1483650929069,-30.3191294881018,
3.41054258905263));
#248265=CARTESIAN_POINT('Ctrl Pts',(-53.0853168809897,-30.4288515386974,
3.41008815825976));
#248266=CARTESIAN_POINT('Ctrl Pts',(-53.1609188493365,-30.4725003554714,
3.30819867304261));
#248267=CARTESIAN_POINT('Ctrl Pts',(-53.1871522506172,-30.3416565762239,
3.48823028058462));
#248268=CARTESIAN_POINT('Ctrl Pts',(-53.1243619179793,-30.4513942013116,
3.48794691941578));
#248269=CARTESIAN_POINT('Ctrl Pts',(-53.2191856060843,-30.5061406831646,
3.42473028058463));
#248270=CARTESIAN_POINT('Origin',(-52.9969317578285,-30.2311753956715,3.2342302805846));
#248271=CARTESIAN_POINT('Ctrl Pts',(-51.6568155675425,-29.4581217525676,
3.47153072139052));
#248272=CARTESIAN_POINT('Ctrl Pts',(-51.5939283826159,-29.5680161684459,
3.47122746285056));
#248273=CARTESIAN_POINT('Ctrl Pts',(-51.6870133715069,-29.6215404675519,
3.4041304667677));
#248274=CARTESIAN_POINT('Ctrl Pts',(-51.7564542486362,-29.5155056307139,
3.65553813457966));
#248275=CARTESIAN_POINT('Ctrl Pts',(-51.6933631336501,-29.6254251653841,
3.65520336072067));
#248276=CARTESIAN_POINT('Ctrl Pts',(-51.7666458147667,-29.6675162799447,
3.55128134519894));
#248277=CARTESIAN_POINT('Ctrl Pts',(-51.9354510367809,-29.6185943474766,
3.77003198860242));
#248278=CARTESIAN_POINT('Ctrl Pts',(-51.8721362050963,-29.7286404220041,
3.76980209314217));
#248279=CARTESIAN_POINT('Ctrl Pts',(-51.9097019182957,-29.7501097595407,
3.64284195387388));
#248280=CARTESIAN_POINT('Ctrl Pts',(-52.1234703131944,-29.7268821954852,
3.77003198860242));
#248281=CARTESIAN_POINT('Ctrl Pts',(-52.0598751946718,-29.8370321718797,
3.77003198860241));
#248282=CARTESIAN_POINT('Ctrl Pts',(-52.0599703843282,-29.8368672985585,
3.64284189403787));
#248283=CARTESIAN_POINT('Origin',(-52.1234703131944,-29.7268821954852,3.64303198860241));
#248284=CARTESIAN_POINT('Origin',(45.3776874999996,26.5654375142636,3.234230280585));
#248285=CARTESIAN_POINT('Origin',(-52.8659816883957,-30.155571337834,3.2342302805846));
#248286=CARTESIAN_POINT('Origin',(45.2006711678726,26.4632370872591,3.64303198860282));
#248287=CARTESIAN_POINT('Origin',(-52.4710850656381,-29.9275190026066,3.64299171721771));
#248288=CARTESIAN_POINT('Ctrl Pts',(-52.6757649139393,-30.0450834959839,
3.4882302805846));
#248289=CARTESIAN_POINT('Ctrl Pts',(-52.6124111049554,-30.1558192616004,
3.48852004212237));
#248290=CARTESIAN_POINT('Ctrl Pts',(-52.5167277788839,-30.100576467536,
3.42473028058459));
#248291=CARTESIAN_POINT('Ctrl Pts',(-52.7146817640548,-30.067689180849,
3.41028005848386));
#248292=CARTESIAN_POINT('Ctrl Pts',(-52.6511806140149,-30.1782028480951,
3.41074404220263));
#248293=CARTESIAN_POINT('Ctrl Pts',(-52.575191448499,-30.1343304829261,
3.30780486243823));
#248294=CARTESIAN_POINT('Ctrl Pts',(-52.7884098752459,-30.1105150503713,
3.36123028058459));
#248295=CARTESIAN_POINT('Ctrl Pts',(-52.7247179826676,-30.2206596676793,
3.36146460586396));
#248296=CARTESIAN_POINT('Ctrl Pts',(-52.6859499175236,-30.1982769148326,
3.23423045308398));
#248297=CARTESIAN_POINT('Ctrl Pts',(-52.8659816883957,-30.155571337834,
3.3612302805846));
#248298=CARTESIAN_POINT('Ctrl Pts',(-52.8024816883957,-30.2655565641147,
3.3612302805846));
#248299=CARTESIAN_POINT('Ctrl Pts',(-52.8024816883957,-30.2655565641147,
3.23423028058459));
#248300=CARTESIAN_POINT('Origin',(-52.5802277788839,-29.9905912412554,3.42473028058459));
#248301=CARTESIAN_POINT('Origin',(-52.5097763812716,-29.949916107531,3.5656311352473));
#248302=CARTESIAN_POINT('Origin',(-49.5064990290868,-36.3610285397831,3.56647653909432));
#248303=CARTESIAN_POINT('Origin',(-49.5422481179701,-36.3870656659254,3.64299466007706));
#248304=CARTESIAN_POINT('Origin',(-49.4402904249163,-36.3129251734945,3.42473028058458));
#248305=CARTESIAN_POINT('Ctrl Pts',(-49.3516463037382,-36.2478178023253,
3.48823028058457));
#248306=CARTESIAN_POINT('Ctrl Pts',(-49.4263574835548,-36.1458216659127,
3.48794691941574));
#248307=CARTESIAN_POINT('Ctrl Pts',(-49.5149391519574,-36.2101800152089,
3.42473028058459));
#248308=CARTESIAN_POINT('Ctrl Pts',(-49.3151677697923,-36.2214577843982,
3.4102800592506));
#248309=CARTESIAN_POINT('Ctrl Pts',(-49.3897594742869,-36.1192316557419,
3.40982512231162));
#248310=CARTESIAN_POINT('Ctrl Pts',(-49.4603240281359,-36.1704998050803,
3.30780486372868));
#248311=CARTESIAN_POINT('Ctrl Pts',(-49.2460589922059,-36.1715192752712,
3.36123028058456));
#248312=CARTESIAN_POINT('Ctrl Pts',(-49.3205022166689,-36.0689133127038,
3.36099721048352));
#248313=CARTESIAN_POINT('Ctrl Pts',(-49.3568565533029,-36.0953262843488,
3.23423045308384));
#248314=CARTESIAN_POINT('Ctrl Pts',(-49.1733470784084,-36.1189794796885,
3.36123028058455));
#248315=CARTESIAN_POINT('Ctrl Pts',(-49.2479958054496,-36.0162343214029,
3.36123028058456));
#248316=CARTESIAN_POINT('Ctrl Pts',(-49.2479958054496,-36.0162343214029,
3.23423028058455));
#248317=CARTESIAN_POINT('Origin',(-49.1733470784084,-36.1189794796885,3.23423028058455));
#248318=CARTESIAN_POINT('Origin',(0.186621817602868,-0.25686289571386,3.64303198860262));
#248319=CARTESIAN_POINT('Origin',(-49.8669803696023,-36.6229335645812,3.64303198860236));
#248320=CARTESIAN_POINT('Origin',(0.186621817602868,-0.256862895713858,
3.23423028058481));
#248321=CARTESIAN_POINT('Origin',(-49.05101714314,-36.0301015792679,3.23423028058455));
#248322=CARTESIAN_POINT('Ctrl Pts',(-50.3023253561992,-36.9399086546489,
3.47153072139045));
#248323=CARTESIAN_POINT('Ctrl Pts',(-50.3777877177481,-36.8368401467444,
3.47182327902636));
#248324=CARTESIAN_POINT('Ctrl Pts',(-50.2900345588339,-36.7733199672426,
3.40413028959031));
#248325=CARTESIAN_POINT('Ctrl Pts',(-50.2093718139428,-36.8722300970264,
3.65553807120931));
#248326=CARTESIAN_POINT('Ctrl Pts',(-50.2846371204117,-36.7691625978869,
3.6558627549694));
#248327=CARTESIAN_POINT('Ctrl Pts',(-50.2156443459698,-36.7192723137692,
3.55128126837172));
#248328=CARTESIAN_POINT('Ctrl Pts',(-50.0423845927721,-36.7506474475458,
3.77003198860237));
#248329=CARTESIAN_POINT('Ctrl Pts',(-50.1174266236762,-36.6476776482608,
3.77025505748412));
#248330=CARTESIAN_POINT('Ctrl Pts',(-50.0820053531159,-36.6221779017723,
3.64284211731208));
#248331=CARTESIAN_POINT('Ctrl Pts',(-49.8669803696023,-36.6229335645812,
3.77003198860237));
#248332=CARTESIAN_POINT('Ctrl Pts',(-49.9417406183798,-36.5200349097938,
3.77003198860237));
#248333=CARTESIAN_POINT('Ctrl Pts',(-49.9416290134636,-36.5201885207827,
3.64284239821728));
#248334=CARTESIAN_POINT('Origin',(-50.2155162706041,-36.8761597191957,3.40423097483284));
#248335=CARTESIAN_POINT('Ctrl Pts',(-49.05101714314,-36.0301015792679,3.36123028058455));
#248336=CARTESIAN_POINT('Ctrl Pts',(-49.1256658701812,-35.9273564209823,
3.36123028058456));
#248337=CARTESIAN_POINT('Ctrl Pts',(-49.1256658701812,-35.9273564209823,
3.23423028058455));
#248338=CARTESIAN_POINT('Ctrl Pts',(-48.9780591316062,-35.9773846774553,
3.36123028058455));
#248339=CARTESIAN_POINT('Ctrl Pts',(-49.0527758071231,-35.8743986902983,
3.36146538610146));
#248340=CARTESIAN_POINT('Ctrl Pts',(-49.0164371879478,-35.8479971380617,
3.23423043688415));
#248341=CARTESIAN_POINT('Ctrl Pts',(-48.9090707128238,-35.9275383438667,
3.41054258693074));
#248342=CARTESIAN_POINT('Ctrl Pts',(-48.9842025736633,-35.824577319909,
3.41100608859626));
#248343=CARTESIAN_POINT('Ctrl Pts',(-48.9131536812776,-35.7729572780243,
3.30819866970743));
#248344=CARTESIAN_POINT('Ctrl Pts',(-48.872713344794,-35.9012693628907,
3.48823028058455));
#248345=CARTESIAN_POINT('Ctrl Pts',(-48.9481071848794,-35.7983524848938,
3.48852004212234));
#248346=CARTESIAN_POINT('Ctrl Pts',(-48.8587224664497,-35.7334106856009,
3.42473028058455));
#248347=CARTESIAN_POINT('Origin',(-48.7840737394086,-35.8361558438865,3.42473028058455));
#248348=CARTESIAN_POINT('Origin',(-50.3596419293477,-36.9808731396205,3.11913648178297));
#248349=CARTESIAN_POINT('Origin',(-50.5037675878942,-37.0855865599605,2.83404198860235));
#248350=CARTESIAN_POINT('Origin',(-48.7182599900757,-35.7883393560614,3.56563113460791));
#248351=CARTESIAN_POINT('Origin',(-48.682062041486,-35.7621028045853,3.64299171721765));
#248352=CARTESIAN_POINT('Ctrl Pts',(-50.9219998155897,-37.0158684358562,
2.59908173515997));
#248353=CARTESIAN_POINT('Ctrl Pts',(-50.8918248690997,-36.9939338721435,
2.65878198860235));
#248354=CARTESIAN_POINT('Ctrl Pts',(-50.8348823336483,-36.9525415975214,
2.65878198860235));
#248355=CARTESIAN_POINT('Ctrl Pts',(-50.870189502586,-37.0871426490245,
2.5990819347554));
#248356=CARTESIAN_POINT('Ctrl Pts',(-50.8540829678243,-37.0458491715915,
2.65878715325316));
#248357=CARTESIAN_POINT('Ctrl Pts',(-50.8048852215546,-36.9937925764105,
2.65878198860235));
#248358=CARTESIAN_POINT('Ctrl Pts',(-50.8021467555728,-37.1382015956605,
2.63878778849862));
#248359=CARTESIAN_POINT('Ctrl Pts',(-50.8006171556812,-37.0800635522218,
2.69564460180089));
#248360=CARTESIAN_POINT('Ctrl Pts',(-50.7569692080808,-37.0171501059292,
2.68180481624872));
#248361=CARTESIAN_POINT('Ctrl Pts',(-50.6806663304944,-37.1817767082786,
2.754432388786));
#248362=CARTESIAN_POINT('Ctrl Pts',(-50.7142182018863,-37.0956112176472,
2.79268340777063));
#248363=CARTESIAN_POINT('Ctrl Pts',(-50.66189279602,-37.0243843935852,2.74885926835567));
#248364=CARTESIAN_POINT('Ctrl Pts',(-50.6273693057702,-37.1760624637761,
2.82856655361656));
#248365=CARTESIAN_POINT('Ctrl Pts',(-50.6810088489707,-37.0763301845679,
2.8538419723071));
#248366=CARTESIAN_POINT('Ctrl Pts',(-50.6152053999547,-37.0095702365079,
2.79184624278423));
#248367=CARTESIAN_POINT('Ctrl Pts',(-50.5905785208481,-37.1493329797263,
2.90134173515997));
#248368=CARTESIAN_POINT('Ctrl Pts',(-50.665924074908,-37.0464195108255,
2.90163218716364));
#248369=CARTESIAN_POINT('Ctrl Pts',(-50.5784163149354,-36.9828414016749,
2.83404198860235));
#248370=CARTESIAN_POINT('Origin',(-50.8348823336483,-36.9525415975214,2.53178198860235));
#248371=CARTESIAN_POINT('Origin',(0.186621817602868,-0.25686289571386,3.64303198860262));
#248372=CARTESIAN_POINT('Origin',(-48.3573835402116,-35.5261472678868,3.64303198860237));
#248373=CARTESIAN_POINT('Origin',(1.03190816135906E-16,1.91674354416515E-13,
2.53178198860262));
#248374=CARTESIAN_POINT('Origin',(-50.8527980281382,-36.9278827595329,2.53178198860235));
#248375=CARTESIAN_POINT('Ctrl Pts',(-48.3573835402116,-35.5261472678868,
3.77003198860238));
#248376=CARTESIAN_POINT('Ctrl Pts',(-48.4321440944168,-35.4232481927144,
3.77003198860238));
#248377=CARTESIAN_POINT('Ctrl Pts',(-48.4320321836171,-35.4234022247158,
3.64284187937009));
#248378=CARTESIAN_POINT('Ctrl Pts',(-48.1819806163558,-35.3984257650668,
3.77003198860238));
#248379=CARTESIAN_POINT('Ctrl Pts',(-48.2567602586449,-35.2958250128988,
3.76980208962771));
#248380=CARTESIAN_POINT('Ctrl Pts',(-48.2916533613408,-35.3214110399831,
3.64284193928205));
#248381=CARTESIAN_POINT('Ctrl Pts',(-48.0150011530604,-35.2768349808759,
3.65553535416558));
#248382=CARTESIAN_POINT('Ctrl Pts',(-48.0897561847331,-35.1744900671645,
3.65520057834544));
#248383=CARTESIAN_POINT('Ctrl Pts',(-48.1580153629248,-35.2243173504706,
3.55127910964284));
#248384=CARTESIAN_POINT('Ctrl Pts',(-47.9220530736684,-35.209151665053,
3.47153072139047));
#248385=CARTESIAN_POINT('Ctrl Pts',(-47.996868104246,-35.1070032653413,
3.47122746281558));
#248386=CARTESIAN_POINT('Ctrl Pts',(-48.0836260618765,-35.1702703594596,
3.40413045901242));
#248387=CARTESIAN_POINT('Origin',(-48.0088472823269,-35.2729208539817,3.40423097483285));
#248388=CARTESIAN_POINT('Ctrl Pts',(-50.964463724589,-36.6347241449657,
2.90134173515998));
#248389=CARTESIAN_POINT('Ctrl Pts',(-50.8898702560315,-36.7381840359687,
2.90163218716365));
#248390=CARTESIAN_POINT('Ctrl Pts',(-50.8023624960588,-36.674605926818,
2.83404198860236));
#248391=CARTESIAN_POINT('Ctrl Pts',(-51.001270654789,-36.6614665482798,
2.82853349835328));
#248392=CARTESIAN_POINT('Ctrl Pts',(-50.9229972443165,-36.7432905102097,
2.85381483162211));
#248393=CARTESIAN_POINT('Ctrl Pts',(-50.8391683443876,-36.7013469409082,
2.79182701594226));
#248394=CARTESIAN_POINT('Ctrl Pts',(-51.0230245369434,-36.7102884597169,
2.75468822073616));
#248395=CARTESIAN_POINT('Ctrl Pts',(-50.9514409225354,-36.768904996455,
2.79286913083798));
#248396=CARTESIAN_POINT('Ctrl Pts',(-50.8675358949429,-36.7410683485316,
2.74900763297898));
#248397=CARTESIAN_POINT('Ctrl Pts',(-51.0194219249358,-36.8383381382863,
2.63954450640366));
#248398=CARTESIAN_POINT('Ctrl Pts',(-50.9635175930187,-36.8551762168621,
2.69627684028837));
#248399=CARTESIAN_POINT('Ctrl Pts',(-50.8901021525733,-36.8330984946705,
2.68224356036453));
#248400=CARTESIAN_POINT('Ctrl Pts',(-50.9918932610483,-36.9196318328647,
2.59908178706376));
#248401=CARTESIAN_POINT('Ctrl Pts',(-50.9476171190685,-36.9171104726345,
2.65878704321395));
#248402=CARTESIAN_POINT('Ctrl Pts',(-50.8828596657519,-36.8864699989246,
2.65878198860235));
#248403=CARTESIAN_POINT('Ctrl Pts',(-50.9399462128199,-36.991167339171,
2.59908173515997));
#248404=CARTESIAN_POINT('Ctrl Pts',(-50.9097606317991,-36.9692474126343,
2.65878198860235));
#248405=CARTESIAN_POINT('Ctrl Pts',(-50.8527980281382,-36.9278827595329,
2.65878198860235));
#248406=CARTESIAN_POINT('Origin',(-50.8770112230999,-36.5718607685324,2.83404198860236));
#248407=CARTESIAN_POINT('Origin',(-47.8647214254959,-35.1682072895723,3.11913648167072));
#248408=CARTESIAN_POINT('Origin',(-47.7205955685088,-35.0634937251224,2.83404198860236));
#248409=CARTESIAN_POINT('Origin',(-50.7328855645158,-36.4671473482183,3.11913648177345));
#248410=CARTESIAN_POINT('Origin',(-50.5887599058098,-36.3624339277676,3.40423097483284));
#248411=CARTESIAN_POINT('Ctrl Pts',(-47.6338034047597,-34.9997217530262,
2.90134173515998));
#248412=CARTESIAN_POINT('Ctrl Pts',(-47.7085070967801,-34.8977303031704,
2.90103711553204));
#248413=CARTESIAN_POINT('Ctrl Pts',(-47.7952442955499,-34.9607485668368,
2.83404198860236));
#248414=CARTESIAN_POINT('Ctrl Pts',(-47.5970451916072,-34.9730146904937,
2.82862991747933));
#248415=CARTESIAN_POINT('Ctrl Pts',(-47.6752966590729,-34.8923835282615,
2.85314045886504));
#248416=CARTESIAN_POINT('Ctrl Pts',(-47.7584842465943,-34.9340408279389,
2.7918796099996));
#248417=CARTESIAN_POINT('Ctrl Pts',(-47.5754322771533,-34.9244461536125,
2.75470625793305));
#248418=CARTESIAN_POINT('Ctrl Pts',(-47.6469756149924,-34.8665972787024,
2.79224250381856));
#248419=CARTESIAN_POINT('Ctrl Pts',(-47.7303228514092,-34.8944891948624,
2.74901809108221));
#248420=CARTESIAN_POINT('Ctrl Pts',(-47.5794993790982,-34.797072508526,
2.63947868311669));
#248421=CARTESIAN_POINT('Ctrl Pts',(-47.635319763777,-34.7804938560724,
2.69595066767899));
#248422=CARTESIAN_POINT('Ctrl Pts',(-47.708416089387,-34.8028668197835,
2.68220539436048));
#248423=CARTESIAN_POINT('Ctrl Pts',(-47.6073089936882,-34.716261746734,
2.59908178585007));
#248424=CARTESIAN_POINT('Ctrl Pts',(-47.6515013114247,-34.7189078610122,
2.65877670944894));
#248425=CARTESIAN_POINT('Ctrl Pts',(-47.7160937685324,-34.7497660430522,
2.65878198860237));
#248426=CARTESIAN_POINT('Ctrl Pts',(-47.6590285860933,-34.6451144164188,
2.59908173515998));
#248427=CARTESIAN_POINT('Ctrl Pts',(-47.689203188551,-34.667049453402,2.65878198860237));
#248428=CARTESIAN_POINT('Ctrl Pts',(-47.7461450747862,-34.7084426211234,
2.65878198860237));
#248429=CARTESIAN_POINT('Origin',(-47.7461450747862,-34.7084426211234,2.53178198860237));
#248430=CARTESIAN_POINT('Ctrl Pts',(-50.240224004808,-36.1092077731531,
3.77003198860237));
#248431=CARTESIAN_POINT('Ctrl Pts',(-50.1654637495897,-36.2121064368053,
3.77003198860237));
#248432=CARTESIAN_POINT('Ctrl Pts',(-50.1655753609562,-36.2119528169383,
3.64284238727604));
#248433=CARTESIAN_POINT('Ctrl Pts',(-50.4158927445031,-36.2365633238551,
3.77003198860237));
#248434=CARTESIAN_POINT('Ctrl Pts',(-50.3411519064815,-36.3397519704547,
3.77025506105981));
#248435=CARTESIAN_POINT('Ctrl Pts',(-50.3059538820319,-36.3139437822118,
3.64284210641911));
#248436=CARTESIAN_POINT('Ctrl Pts',(-50.5831252836602,-36.357805546057,
3.65553527987808));
#248437=CARTESIAN_POINT('Ctrl Pts',(-50.5083605190661,-36.4612367259577,
3.65585996532878));
#248438=CARTESIAN_POINT('Ctrl Pts',(-50.4395918165605,-36.4110374247129,
3.55127902710112));
#248439=CARTESIAN_POINT('Ctrl Pts',(-50.6762142289945,-36.4252947698681,
3.47153072139046));
#248440=CARTESIAN_POINT('Ctrl Pts',(-50.6015093986315,-36.5289136700279,
3.47182327905162));
#248441=CARTESIAN_POINT('Ctrl Pts',(-50.5139808995222,-36.4650842569436,
3.40413028377978));
#248442=CARTESIAN_POINT('Origin',(-50.240224004808,-36.1092077731531,3.64303198860237));
#248443=CARTESIAN_POINT('Origin',(3.64514313700083E-16,1.9154295688095E-13,
2.53178198860262));
#248444=CARTESIAN_POINT('Origin',(-47.764060769276,-34.6837837831348,2.53178198860237));
#248445=CARTESIAN_POINT('Origin',(40.5385041740525,29.8453988870289,3.64303198860284));
#248446=CARTESIAN_POINT('Origin',(-49.9155525184304,-35.873256238299,3.64299466007745));
#248447=CARTESIAN_POINT('Ctrl Pts',(-47.6769115920301,-34.6205005703637,
2.59908173515998));
#248448=CARTESIAN_POINT('Ctrl Pts',(-47.7070975168461,-34.6424200234577,
2.65878198860237));
#248449=CARTESIAN_POINT('Ctrl Pts',(-47.764060769276,-34.6837837831348,
2.65878198860237));
#248450=CARTESIAN_POINT('Ctrl Pts',(-47.7284183483604,-34.5495693076632,
2.59908193199868));
#248451=CARTESIAN_POINT('Ctrl Pts',(-47.7446195594529,-34.5907418558606,
2.65877685806676));
#248452=CARTESIAN_POINT('Ctrl Pts',(-47.7939730310152,-34.6425747206414,
2.65878198860237));
#248453=CARTESIAN_POINT('Ctrl Pts',(-47.7959261043552,-34.4983910654769,
2.63872492669783));
#248454=CARTESIAN_POINT('Ctrl Pts',(-47.7976714756521,-34.5563698228278,
2.69532212015247));
#248455=CARTESIAN_POINT('Ctrl Pts',(-47.8415056181565,-34.61888919786,2.6817683672662));
#248456=CARTESIAN_POINT('Ctrl Pts',(-47.9165880269726,-34.4545839152293,
2.75442176402215));
#248457=CARTESIAN_POINT('Ctrl Pts',(-47.8837591046484,-34.5404685123898,
2.79203179920117));
#248458=CARTESIAN_POINT('Ctrl Pts',(-47.9359643384883,-34.6111463389769,
2.7488531074814));
#248459=CARTESIAN_POINT('Ctrl Pts',(-47.9696250311914,-34.4602354682501,
2.82866089558383));
#248460=CARTESIAN_POINT('Ctrl Pts',(-47.9171136764632,-34.5595777906765,
2.85316563119103));
#248461=CARTESIAN_POINT('Ctrl Pts',(-47.982446041048,-34.6258166968305,
2.79189751796547));
#248462=CARTESIAN_POINT('Ctrl Pts',(-48.0063682005184,-34.4869303039399,
2.90134173515999));
#248463=CARTESIAN_POINT('Ctrl Pts',(-47.9324532779035,-34.5894948283136,
2.90103711553205));
#248464=CARTESIAN_POINT('Ctrl Pts',(-48.0191904766733,-34.6525130919799,
2.83404198860237));
#248465=CARTESIAN_POINT('Origin',(-48.0938392037145,-34.5497679336943,2.83404198860238));
#248466=CARTESIAN_POINT('Origin',(-49.8797426632452,-35.8473027479617,3.56647653971698));
#248467=CARTESIAN_POINT('Origin',(-49.813534060122,-35.7991993820664,3.4247302805846));
#248468=CARTESIAN_POINT('Origin',(-48.2379650606552,-34.6544814981795,3.11913648168121));
#248469=CARTESIAN_POINT('Origin',(-48.3820909175326,-34.7591950625536,3.40423097483285));
#248470=CARTESIAN_POINT('Ctrl Pts',(-49.5465907136142,-35.6052536882604,
3.36123028058456));
#248471=CARTESIAN_POINT('Ctrl Pts',(-49.471941986573,-35.7079988465461,
3.36123028058455));
#248472=CARTESIAN_POINT('Ctrl Pts',(-49.471941986573,-35.7079988465461,
3.23423028058456));
#248473=CARTESIAN_POINT('Ctrl Pts',(-49.6192730640972,-35.6583499840553,
3.36123028058456));
#248474=CARTESIAN_POINT('Ctrl Pts',(-49.5446936074932,-35.7608559931208,
3.36099641108516));
#248475=CARTESIAN_POINT('Ctrl Pts',(-49.5811706590218,-35.7873581223577,
3.23423043688376));
#248476=CARTESIAN_POINT('Ctrl Pts',(-49.688000774921,-35.7085550527694,
3.41054258905262));
#248477=CARTESIAN_POINT('Ctrl Pts',(-49.6138288703661,-35.8110857017866,
3.41008815826032));
#248478=CARTESIAN_POINT('Ctrl Pts',(-49.6844541394795,-35.8623979633506,
3.30819867304285));
#248479=CARTESIAN_POINT('Ctrl Pts',(-49.7242207306172,-35.7350130971392,
3.48823028058459));
#248480=CARTESIAN_POINT('Ctrl Pts',(-49.6503036646782,-35.8375861910559,
3.48794691941575));
#248481=CARTESIAN_POINT('Ctrl Pts',(-49.7388853330808,-35.9019445403521,
3.4247302805846));
#248482=CARTESIAN_POINT('Origin',(-49.5465907136142,-35.6052536882604,3.23423028058456));
#248483=CARTESIAN_POINT('Ctrl Pts',(-48.2946219293743,-34.6963546279287,
3.47153072139047));
#248484=CARTESIAN_POINT('Ctrl Pts',(-48.2205921526131,-34.7990735298991,
3.47122746285052));
#248485=CARTESIAN_POINT('Ctrl Pts',(-48.3075723994628,-34.8620346481362,
3.40413046676745));
#248486=CARTESIAN_POINT('Ctrl Pts',(-48.38771653075,-34.7638392294014,3.6555381345796));
#248487=CARTESIAN_POINT('Ctrl Pts',(-48.313481315449,-34.866561796061,3.65520336072181));
#248488=CARTESIAN_POINT('Ctrl Pts',(-48.3819628268463,-34.9160824571361,
3.55128134519942));
#248489=CARTESIAN_POINT('Ctrl Pts',(-48.5549570506162,-34.8850734745832,
3.77003198860238));
#248490=CARTESIAN_POINT('Ctrl Pts',(-48.480486117148,-34.9878985031425,
3.76980209314177));
#248491=CARTESIAN_POINT('Ctrl Pts',(-48.5156018845791,-35.0131769156757,
3.64284195387375));
#248492=CARTESIAN_POINT('Ctrl Pts',(-48.7306271754173,-35.0124214764587,
3.77003198860238));
#248493=CARTESIAN_POINT('Ctrl Pts',(-48.6558666298463,-35.1153205397472,
3.77003198860238));
#248494=CARTESIAN_POINT('Ctrl Pts',(-48.655978531999,-35.1151665196474,
3.64284189403744));
#248495=CARTESIAN_POINT('Origin',(-48.7306271754173,-35.0124214764587,3.64303198860238));
#248496=CARTESIAN_POINT('Origin',(39.5520252162584,29.1286799712091,3.23423028058503));
#248497=CARTESIAN_POINT('Origin',(-49.4242607783458,-35.5163757878398,3.23423028058456));
#248498=CARTESIAN_POINT('Origin',(39.3975469582344,29.0164449471024,3.64303198860284));
#248499=CARTESIAN_POINT('Origin',(-49.0553654007524,-35.248294810039,3.64299171721698));
#248500=CARTESIAN_POINT('Ctrl Pts',(-49.246635155601,-35.3866101428262,
3.48823028058456));
#248501=CARTESIAN_POINT('Ctrl Pts',(-49.1720533660028,-35.4901170100369,
3.48852004212234));
#248502=CARTESIAN_POINT('Ctrl Pts',(-49.0826686475732,-35.425175210744,
3.42473028058456));
#248503=CARTESIAN_POINT('Ctrl Pts',(-49.2829758776408,-35.4131599099204,
3.41028005848381));
#248504=CARTESIAN_POINT('Ctrl Pts',(-49.2082707697412,-35.5164304941026,
3.41074404220296));
#248505=CARTESIAN_POINT('Ctrl Pts',(-49.1372837917322,-35.4648554356487,
3.30780486243887));
#248506=CARTESIAN_POINT('Ctrl Pts',(-49.3518235761955,-35.4634578610105,
3.36123028058456));
#248507=CARTESIAN_POINT('Ctrl Pts',(-49.2769673468835,-35.5663414789258,
3.36146460586393));
#248508=CARTESIAN_POINT('Ctrl Pts',(-49.2407512920142,-35.54002897487,3.23423045308351));
#248509=CARTESIAN_POINT('Ctrl Pts',(-49.4242607783458,-35.5163757878398,
3.36123028058456));
#248510=CARTESIAN_POINT('Ctrl Pts',(-49.3496120513046,-35.6191209461254,
3.36123028058456));
#248511=CARTESIAN_POINT('Ctrl Pts',(-49.3496120513046,-35.6191209461254,
3.23423028058456));
#248512=CARTESIAN_POINT('Origin',(-49.1573173746143,-35.3224300524584,3.42473028058456));
#248513=CARTESIAN_POINT('Origin',(-49.0915036263505,-35.2746135650452,3.56563113524708));
#248514=CARTESIAN_POINT('Origin',(-45.4345348113615,-41.336677286195,3.56647653909452));
#248515=CARTESIAN_POINT('Origin',(-45.4673664422113,-41.3663085755598,3.64299466007842));
#248516=CARTESIAN_POINT('Origin',(-45.3737170758069,-41.281916751533,3.42473028058454));
#248517=CARTESIAN_POINT('Ctrl Pts',(-45.2923641298554,-41.2079002115909,
3.48823028058455));
#248518=CARTESIAN_POINT('Ctrl Pts',(-45.3773275334102,-41.1142722655008,
3.48794691941571));
#248519=CARTESIAN_POINT('Ctrl Pts',(-45.4586966628145,-41.1875373586974,
3.42473028058456));
#248520=CARTESIAN_POINT('Ctrl Pts',(-45.2588408013024,-41.1778715515028,
3.41028005925058));
#248521=CARTESIAN_POINT('Ctrl Pts',(-45.3437094247774,-41.0840023845226,
3.40982512230884));
#248522=CARTESIAN_POINT('Ctrl Pts',(-45.4085284377449,-41.1423656859495,
3.30780486372779));
#248523=CARTESIAN_POINT('Ctrl Pts',(-45.1953306044449,-41.1209827764374,
3.36123028058452));
#248524=CARTESIAN_POINT('Ctrl Pts',(-45.2800912647189,-41.0267203359189,
3.36099721048419));
#248525=CARTESIAN_POINT('Ctrl Pts',(-45.3134855411615,-41.056788677484,
3.23423045308386));
#248526=CARTESIAN_POINT('Ctrl Pts',(-45.1285089182129,-41.0611303347406,
3.36123028058452));
#248527=CARTESIAN_POINT('Ctrl Pts',(-45.2134885052205,-40.966750941905,
3.36123028058452));
#248528=CARTESIAN_POINT('Ctrl Pts',(-45.2134885052205,-40.966750941905,
3.23423028058452));
#248529=CARTESIAN_POINT('Origin',(-45.1285089182129,-41.0611303347406,3.23423028058452));
#248530=CARTESIAN_POINT('Origin',(0.212448967518945,-0.235948482088887,
3.64303198860262));
#248531=CARTESIAN_POINT('Origin',(-45.7656648676103,-41.6348281284264,3.64303198860233));
#248532=CARTESIAN_POINT('Origin',(0.212448967518945,-0.235948482088884,
3.23423028058481));
#248533=CARTESIAN_POINT('Origin',(-45.016139389479,-40.9599523566127,3.23423028058452));
#248534=CARTESIAN_POINT('Ctrl Pts',(-46.1654920697608,-41.9955727382253,
3.47153072139041));
#248535=CARTESIAN_POINT('Ctrl Pts',(-46.2513146333399,-41.9009568150787,
3.47182327902632));
#248536=CARTESIAN_POINT('Ctrl Pts',(-46.1706818621619,-41.8286119029182,
3.40413028959029));
#248537=CARTESIAN_POINT('Ctrl Pts',(-46.0801220723621,-41.9185486398924,
3.65553807120923));
#248538=CARTESIAN_POINT('Ctrl Pts',(-46.1657485549025,-41.8239131221215,
3.65586275496807));
#248539=CARTESIAN_POINT('Ctrl Pts',(-46.102348684828,-41.7670844335126,
3.55128126837167));
#248540=CARTESIAN_POINT('Ctrl Pts',(-45.9267584721685,-41.7801771152759,
3.77003198860233));
#248541=CARTESIAN_POINT('Ctrl Pts',(-46.0121526898594,-41.685615423495,
3.77025505748548));
#248542=CARTESIAN_POINT('Ctrl Pts',(-45.9795909100381,-41.6565528363085,
3.64284211731204));
#248543=CARTESIAN_POINT('Ctrl Pts',(-45.7656648676103,-41.6348281284264,
3.77003198860233));
#248544=CARTESIAN_POINT('Ctrl Pts',(-45.8507714101799,-41.5403077371547,
3.77003198860233));
#248545=CARTESIAN_POINT('Ctrl Pts',(-45.8506443599266,-41.5404488407561,
3.64284239821729));
#248546=CARTESIAN_POINT('Origin',(-46.0858221116775,-41.9230990057957,3.4042309748328));
#248547=CARTESIAN_POINT('Ctrl Pts',(-45.016139389479,-40.9599523566127,
3.36123028058452));
#248548=CARTESIAN_POINT('Ctrl Pts',(-45.1011189764865,-40.865572963777,
3.36123028058452));
#248549=CARTESIAN_POINT('Ctrl Pts',(-45.1011189764865,-40.865572963777,
3.23423028058452));
#248550=CARTESIAN_POINT('Ctrl Pts',(-44.9490914663004,-40.8998980546758,
3.36123028058452));
#248551=CARTESIAN_POINT('Ctrl Pts',(-45.0341638030252,-40.8052862548027,
3.36146538610245));
#248552=CARTESIAN_POINT('Ctrl Pts',(-45.000783964292,-40.7752309130124,
3.23423043688429));
#248553=CARTESIAN_POINT('Ctrl Pts',(-44.8856913339429,-40.8431135311207,
3.41054258693071));
#248554=CARTESIAN_POINT('Ctrl Pts',(-44.9711739721998,-40.7485699563836,
3.41100608859617));
#248555=CARTESIAN_POINT('Ctrl Pts',(-44.9059100567337,-40.6898060629486,
3.3081986697077));
#248556=CARTESIAN_POINT('Ctrl Pts',(-44.8522789915938,-40.8131880745608,
3.48823028058452));
#248557=CARTESIAN_POINT('Ctrl Pts',(-44.9380175594359,-40.7187157882339,
3.48852004212231));
#248558=CARTESIAN_POINT('Ctrl Pts',(-44.8559107663282,-40.6447864996554,
3.42473028058453));
#248559=CARTESIAN_POINT('Origin',(-44.7709311793206,-40.7391658924911,3.42473028058452));
#248560=CARTESIAN_POINT('Origin',(-46.2182127020609,-42.0423040287734,3.11913648178265));
#248561=CARTESIAN_POINT('Origin',(-46.3506032922591,-42.1615090516454,2.83404198860231));
#248562=CARTESIAN_POINT('Origin',(-44.7104761485856,-40.6847319383086,3.56563113460817));
#248563=CARTESIAN_POINT('Origin',(-44.677218962551,-40.6548553974684,3.64299171721742));
#248564=CARTESIAN_POINT('Ctrl Pts',(-46.7738319284254,-42.1358900227697,
2.59908173515993));
#248565=CARTESIAN_POINT('Ctrl Pts',(-46.7461150696869,-42.1109214781063,
2.65878198860232));
#248566=CARTESIAN_POINT('Ctrl Pts',(-46.6938111422601,-42.0638038389702,
2.65878198860231));
#248567=CARTESIAN_POINT('Ctrl Pts',(-46.7148552537641,-42.2013581359414,
2.59908193475522));
#248568=CARTESIAN_POINT('Ctrl Pts',(-46.7031532960248,-42.1586072771714,
2.65878715325297));
#248569=CARTESIAN_POINT('Ctrl Pts',(-46.6596664560544,-42.1016932886521,
2.65878198860231));
#248570=CARTESIAN_POINT('Ctrl Pts',(-46.6418481388112,-42.2450249725429,
2.63878778849834));
#248571=CARTESIAN_POINT('Ctrl Pts',(-46.6464039985654,-42.1870455286632,
2.69564460180072));
#248572=CARTESIAN_POINT('Ctrl Pts',(-46.6095714048488,-42.1199142759248,
2.68180481624859));
#248573=CARTESIAN_POINT('Ctrl Pts',(-46.5164783566524,-42.2756632139847,
2.75443238878623));
#248574=CARTESIAN_POINT('Ctrl Pts',(-46.5588531737051,-42.1934768724829,
2.79268340777076));
#248575=CARTESIAN_POINT('Ctrl Pts',(-46.5142596423497,-42.1171707421505,
2.74885926835574));
#248576=CARTESIAN_POINT('Ctrl Pts',(-46.4640705998029,-42.2644092166206,
2.82856655361634));
#248577=CARTESIAN_POINT('Ctrl Pts',(-46.5278411618559,-42.1708301402943,
2.85384197230709));
#248578=CARTESIAN_POINT('Ctrl Pts',(-46.4693765057988,-42.0975575768108,
2.79184624278386));
#248579=CARTESIAN_POINT('Ctrl Pts',(-46.4302753505421,-42.2339804752703,
2.90134173515994));
#248580=CARTESIAN_POINT('Ctrl Pts',(-46.5159655405271,-42.1395065321001,
2.90163218716362));
#248581=CARTESIAN_POINT('Ctrl Pts',(-46.4355828792667,-42.0671296588098,
2.83404198860232));
#248582=CARTESIAN_POINT('Origin',(-46.6938111422601,-42.0638038389702,2.53178198860231));
#248583=CARTESIAN_POINT('Origin',(0.212448967518945,-0.235948482088887,
3.64303198860262));
#248584=CARTESIAN_POINT('Origin',(-44.3789831537292,-40.386254305094,3.64303198860234));
#248585=CARTESIAN_POINT('Origin',(9.23291810287646E-17,1.91687767418825E-13,
2.53178198860262));
#248586=CARTESIAN_POINT('Origin',(-46.7142062431419,-42.0411527846897,2.53178198860231));
#248587=CARTESIAN_POINT('Ctrl Pts',(-44.3789831537292,-40.386254305094,
3.77003198860234));
#248588=CARTESIAN_POINT('Ctrl Pts',(-44.4640900439955,-40.2917335276661,
3.77003198860234));
#248589=CARTESIAN_POINT('Ctrl Pts',(-44.4639626455265,-40.2918750180001,
3.64284187937013));
#248590=CARTESIAN_POINT('Ctrl Pts',(-44.2178916378589,-40.2408978759471,
3.77003198860235));
#248591=CARTESIAN_POINT('Ctrl Pts',(-44.3029863283988,-40.1466757825268,
3.76980208963012));
#248592=CARTESIAN_POINT('Ctrl Pts',(-44.3350138149328,-40.1757689690801,
3.64284193928242));
#248593=CARTESIAN_POINT('Ctrl Pts',(-44.0645366033553,-40.1025190720971,
3.65553535416554));
#248594=CARTESIAN_POINT('Ctrl Pts',(-44.1495800756938,-40.0085488431143,
3.65520057834386));
#248595=CARTESIAN_POINT('Ctrl Pts',(-44.2122569536148,-40.0652381943513,
3.55127910964213));
#248596=CARTESIAN_POINT('Ctrl Pts',(-43.9791725362579,-40.025490812659,
3.47153072139044));
#248597=CARTESIAN_POINT('Ctrl Pts',(-44.0642551375171,-39.9317222927446,
3.47122746281554));
#248598=CARTESIAN_POINT('Ctrl Pts',(-44.1439246138545,-40.0037114790888,
3.40413045901242));
#248599=CARTESIAN_POINT('Origin',(-44.0588255818374,-40.0979831325501,3.40423097483281));
#248600=CARTESIAN_POINT('Ctrl Pts',(-46.8559036426982,-41.7612723673365,
2.90134173515993));
#248601=CARTESIAN_POINT('Ctrl Pts',(-46.7709043015499,-41.8563683535932,
2.90163218716361));
#248602=CARTESIAN_POINT('Ctrl Pts',(-46.6905216402894,-41.7839914803029,
2.83404198860232));
#248603=CARTESIAN_POINT('Ctrl Pts',(-46.88971359836,-41.7917156448197,2.82853349835316));
#248604=CARTESIAN_POINT('Ctrl Pts',(-46.8033160448221,-41.8649095672151,
2.85381483162259));
#248605=CARTESIAN_POINT('Ctrl Pts',(-46.7243306652208,-41.8144332630849,
2.79182701594156));
#248606=CARTESIAN_POINT('Ctrl Pts',(-46.9062450310964,-41.8425440045881,
2.75468822073627));
#248607=CARTESIAN_POINT('Ctrl Pts',(-46.8289264627106,-41.8933569085959,
2.79286913083846));
#248608=CARTESIAN_POINT('Ctrl Pts',(-46.7483907976678,-41.8569022891471,
2.74900763297884));
#248609=CARTESIAN_POINT('Ctrl Pts',(-46.8892773184516,-41.9695156381235,
2.63954450640348));
#248610=CARTESIAN_POINT('Ctrl Pts',(-46.8319191778362,-41.9804178820373,
2.69627684028798));
#248611=CARTESIAN_POINT('Ctrl Pts',(-46.7612136652288,-41.9507871007489,
2.6822435603646));
#248612=CARTESIAN_POINT('Ctrl Pts',(-46.8534019544977,-42.0474864684051,
2.59908178706348));
#248613=CARTESIAN_POINT('Ctrl Pts',(-46.8096319157674,-42.0403508033706,
2.65878704321515));
#248614=CARTESIAN_POINT('Ctrl Pts',(-46.7484320121849,-42.0031091842998,
2.65878198860231));
#248615=CARTESIAN_POINT('Ctrl Pts',(-46.7942619810913,-42.1132001506003,
2.59908173515993));
#248616=CARTESIAN_POINT('Ctrl Pts',(-46.7665330160776,-42.0882450513177,
2.65878198860232));
#248617=CARTESIAN_POINT('Ctrl Pts',(-46.7142062431419,-42.0411527846897,
2.65878198860231));
#248618=CARTESIAN_POINT('Origin',(-46.7755012272969,-41.6896120874673,2.83404198860232));
#248619=CARTESIAN_POINT('Origin',(-43.9264348094997,-39.9787779456716,3.11913648167122));
#248620=CARTESIAN_POINT('Origin',(-43.7940440370141,-39.8595727587357,2.83404198860234));
#248621=CARTESIAN_POINT('Origin',(-46.6431106370605,-41.5704070646241,3.11913648177693));
#248622=CARTESIAN_POINT('Origin',(-46.5107200467153,-41.4512020416176,3.40423097483281));
#248623=CARTESIAN_POINT('Ctrl Pts',(-43.714393316062,-39.7870778846749,
2.90134173515995));
#248624=CARTESIAN_POINT('Ctrl Pts',(-43.799348782961,-39.6934538167802,
2.90103711553201));
#248625=CARTESIAN_POINT('Ctrl Pts',(-43.8790236240217,-39.7651933659001,
2.83404198860233));
#248626=CARTESIAN_POINT('Ctrl Pts',(-43.6806281164518,-39.7566748466924,
2.82862991747931));
#248627=CARTESIAN_POINT('Ctrl Pts',(-43.7668791656725,-39.6846648960484,
2.8531404588637));
#248628=CARTESIAN_POINT('Ctrl Pts',(-43.8452566693654,-39.7347894633639,
2.79187960999875));
#248629=CARTESIAN_POINT('Ctrl Pts',(-43.6642103943283,-39.7061132086032,
2.75470625793302));
#248630=CARTESIAN_POINT('Ctrl Pts',(-43.7414086642727,-39.6560595510441,
2.79224250381861));
#248631=CARTESIAN_POINT('Ctrl Pts',(-43.8213838166742,-39.6925108309091,
2.74901809108232));
#248632=CARTESIAN_POINT('Ctrl Pts',(-43.681569387645,-39.5798624575878,
2.63947868311666));
#248633=CARTESIAN_POINT('Ctrl Pts',(-43.7388169234803,-39.5692094437565,
2.6959506676789));
#248634=CARTESIAN_POINT('Ctrl Pts',(-43.8091742082548,-39.5991004926181,
2.68220539436031));
#248635=CARTESIAN_POINT('Ctrl Pts',(-43.7176736830019,-39.5024012818816,
2.59908178584979));
#248636=CARTESIAN_POINT('Ctrl Pts',(-43.7613473163388,-39.5096522555304,
2.65877670944783));
#248637=CARTESIAN_POINT('Ctrl Pts',(-43.8223603708607,-39.5470931435008,
2.65878198860234));
#248638=CARTESIAN_POINT('Ctrl Pts',(-43.7765468711719,-39.437049873601,
2.59908173515995));
#248639=CARTESIAN_POINT('Ctrl Pts',(-43.8042633382926,-39.4620188529811,
2.65878198860233));
#248640=CARTESIAN_POINT('Ctrl Pts',(-43.8565665267053,-39.5091373124624,
2.65878198860234));
#248641=CARTESIAN_POINT('Origin',(-43.8565665267053,-39.5091373124624,2.53178198860234));
#248642=CARTESIAN_POINT('Ctrl Pts',(-46.1905628026481,-41.1629311642483,
3.77003198860234));
#248643=CARTESIAN_POINT('Ctrl Pts',(-46.1054562527463,-41.2574515636632,
3.77003198860234));
#248644=CARTESIAN_POINT('Ctrl Pts',(-46.1055833103428,-41.2573104519064,
3.64284238727582));
#248645=CARTESIAN_POINT('Ctrl Pts',(-46.3519569305998,-41.3079514313262,
3.77003198860233));
#248646=CARTESIAN_POINT('Ctrl Pts',(-46.2668393800555,-41.4027622547786,
3.77025506105675));
#248647=CARTESIAN_POINT('Ctrl Pts',(-46.2345318643239,-41.3734162510837,
3.64284210641889));
#248648=CARTESIAN_POINT('Ctrl Pts',(-46.5056000892412,-41.446010036274,
3.65553527987799));
#248649=CARTESIAN_POINT('Ctrl Pts',(-46.4204333915659,-41.5410595633948,
3.65585996533104));
#248650=CARTESIAN_POINT('Ctrl Pts',(-46.3572886670225,-41.4839469723842,
3.55127902710129));
#248651=CARTESIAN_POINT('Ctrl Pts',(-46.5911245387426,-41.5228599914565,
3.47153072139041));
#248652=CARTESIAN_POINT('Ctrl Pts',(-46.5059978248575,-41.618102475323,
3.47182327905158));
#248653=CARTESIAN_POINT('Ctrl Pts',(-46.4256208064856,-41.5454735069379,
3.40413028377964));
#248654=CARTESIAN_POINT('Origin',(-46.1905628026481,-41.1629311642483,3.64303198860234));
#248655=CARTESIAN_POINT('Origin',(3.68378193773366E-16,1.91538185386435E-13,
2.53178198860262));
#248656=CARTESIAN_POINT('Origin',(-43.8769616275871,-39.4864862581819,2.53178198860234));
#248657=CARTESIAN_POINT('Origin',(34.1507877370002,31.1767457860028,3.64303198860284));
#248658=CARTESIAN_POINT('Origin',(-45.8923335519908,-40.8943347850523,3.64299466007333));
#248659=CARTESIAN_POINT('Ctrl Pts',(-43.7969047596343,-39.4144401478991,
2.59908173515995));
#248660=CARTESIAN_POINT('Ctrl Pts',(-43.8246341160482,-39.439394812269,
2.65878198860234));
#248661=CARTESIAN_POINT('Ctrl Pts',(-43.8769616275871,-39.4864862581818,
2.65878198860234));
#248662=CARTESIAN_POINT('Ctrl Pts',(-43.8555436924519,-39.3492813761644,
2.59908193199843));
#248663=CARTESIAN_POINT('Ctrl Pts',(-43.867352448422,-39.3919218645326,
2.6587768580655));
#248664=CARTESIAN_POINT('Ctrl Pts',(-43.9110175468015,-39.4486296259964,
2.65878198860234));
#248665=CARTESIAN_POINT('Ctrl Pts',(-43.9280312169042,-39.3054399757366,
2.63872492669765));
#248666=CARTESIAN_POINT('Ctrl Pts',(-43.9237065964666,-39.3632835603679,
2.69532212015234));
#248667=CARTESIAN_POINT('Ctrl Pts',(-43.9607655567554,-39.430042363277,
2.68176836726587));
#248668=CARTESIAN_POINT('Ctrl Pts',(-44.0526112349803,-39.2744854109877,
2.75442176402225));
#248669=CARTESIAN_POINT('Ctrl Pts',(-44.0109847679678,-39.3564679665374,
2.79203179920121));
#248670=CARTESIAN_POINT('Ctrl Pts',(-44.0555161714741,-39.4322155454628,
2.74885310748166));
#248671=CARTESIAN_POINT('Ctrl Pts',(-44.1047669487885,-39.2856498807566,
2.82866089558368));
#248672=CARTESIAN_POINT('Ctrl Pts',(-44.0421591564523,-39.3789590643314,
2.8531656311927));
#248673=CARTESIAN_POINT('Ctrl Pts',(-44.1002097724412,-39.4516641984997,
2.79189751796617));
#248674=CARTESIAN_POINT('Ctrl Pts',(-44.1385184650372,-39.3160391863692,
2.90134173515995));
#248675=CARTESIAN_POINT('Ctrl Pts',(-44.0542875439837,-39.4103156382733,
2.90103711553201));
#248676=CARTESIAN_POINT('Ctrl Pts',(-44.1339623850444,-39.4820551873932,
2.83404198860233));
#248677=CARTESIAN_POINT('Origin',(-44.218941972052,-39.3876757945576,2.83404198860233));
#248678=CARTESIAN_POINT('Origin',(-45.8594327453962,-40.864780321517,3.56647653971802));
#248679=CARTESIAN_POINT('Origin',(-45.7986150108448,-40.8100197873549,3.42473028058455));
#248680=CARTESIAN_POINT('Origin',(-44.3513327444876,-39.5068809815272,3.1191364816803));
#248681=CARTESIAN_POINT('Origin',(-44.4837235168753,-39.6260861683719,3.40423097483282));
#248682=CARTESIAN_POINT('Ctrl Pts',(-45.5534068532508,-40.5892333705625,
3.36123028058452));
#248683=CARTESIAN_POINT('Ctrl Pts',(-45.4684272662432,-40.6836127633981,
3.36123028058452));
#248684=CARTESIAN_POINT('Ctrl Pts',(-45.4684272662432,-40.6836127633981,
3.23423028058452));
#248685=CARTESIAN_POINT('Ctrl Pts',(-45.6201409680082,-40.6496361736963,
3.36123028058452));
#248686=CARTESIAN_POINT('Ctrl Pts',(-45.535255269862,-40.7437849681278,
3.36099641108599));
#248687=CARTESIAN_POINT('Ctrl Pts',(-45.5687622694476,-40.7739548060679,
3.23423043688381));
#248688=CARTESIAN_POINT('Ctrl Pts',(-45.6832443225589,-40.7067502157885,
3.41054258905255));
#248689=CARTESIAN_POINT('Ctrl Pts',(-45.5987613682843,-40.8009661159843,
3.41008815825802));
#248690=CARTESIAN_POINT('Ctrl Pts',(-45.6636361529328,-40.8593796344563,
3.30819867304212));
#248691=CARTESIAN_POINT('Ctrl Pts',(-45.7165002428303,-40.7368493365299,
3.48823028058454));
#248692=CARTESIAN_POINT('Ctrl Pts',(-45.6322662944329,-40.8311340869939,
3.4879469194157));
#248693=CARTESIAN_POINT('Ctrl Pts',(-45.7136354238372,-40.9043991801905,
3.42473028058455));
#248694=CARTESIAN_POINT('Origin',(-45.5534068532508,-40.5892333705625,3.23423028058452));
#248695=CARTESIAN_POINT('Ctrl Pts',(-44.4033023070486,-39.5544469813073,
3.47153072139044));
#248696=CARTESIAN_POINT('Ctrl Pts',(-44.3189410241786,-39.6488649595844,
3.47122746285048));
#248697=CARTESIAN_POINT('Ctrl Pts',(-44.3988635552007,-39.7205730817658,
3.40413046676722));
#248698=CARTESIAN_POINT('Ctrl Pts',(-44.4888328647701,-39.6312929306934,
3.65553813457959));
#248699=CARTESIAN_POINT('Ctrl Pts',(-44.404266885707,-39.7256930794079,
3.65520336072389));
#248700=CARTESIAN_POINT('Ctrl Pts',(-44.4671969296202,-39.7821007282677,
3.55128134520005));
#248701=CARTESIAN_POINT('Ctrl Pts',(-44.642484794226,-39.7693444365323,
3.77003198860235));
#248702=CARTESIAN_POINT('Ctrl Pts',(-44.5576736781029,-39.8638218465962,
3.76980209314011));
#248703=CARTESIAN_POINT('Ctrl Pts',(-44.5899547640713,-39.892632378544,
3.64284195387283));
#248704=CARTESIAN_POINT('Ctrl Pts',(-44.8038810887671,-39.9143573409159,
3.77003198860235));
#248705=CARTESIAN_POINT('Ctrl Pts',(-44.7187742083296,-40.0088781074279,
3.77003198860235));
#248706=CARTESIAN_POINT('Ctrl Pts',(-44.7189015969551,-40.0087366280261,
3.64284189403704));
#248707=CARTESIAN_POINT('Origin',(-44.8038810887671,-39.9143573409159,3.64303198860235));
#248708=CARTESIAN_POINT('Origin',(33.3184119221863,30.4272712359686,3.23423028058503));
#248709=CARTESIAN_POINT('Origin',(-45.4410373245168,-40.4880553924345,3.23423028058452));
#248710=CARTESIAN_POINT('Origin',(33.1880655373213,30.3099068238766,3.64303198860284));
#248711=CARTESIAN_POINT('Origin',(-45.1021848870407,-40.1828829233542,3.64299171721751));
#248712=CARTESIAN_POINT('Ctrl Pts',(-45.2779489569769,-40.3404336838194,
3.48823028058452));
#248713=CARTESIAN_POINT('Ctrl Pts',(-45.1929563204586,-40.435577609727,
3.4885200421223));
#248714=CARTESIAN_POINT('Ctrl Pts',(-45.1108495273509,-40.3616483211486,
3.42473028058452));
#248715=CARTESIAN_POINT('Ctrl Pts',(-45.3113153943823,-40.3706366483428,
3.41028005848378));
#248716=CARTESIAN_POINT('Ctrl Pts',(-45.2262248134149,-40.4655326953357,
3.41074404220353));
#248717=CARTESIAN_POINT('Ctrl Pts',(-45.1610177711069,-40.4068200107218,
3.30780486243963));
#248718=CARTESIAN_POINT('Ctrl Pts',(-45.374528370508,-40.4278556061233,
3.36123028058453));
#248719=CARTESIAN_POINT('Ctrl Pts',(-45.2893279449758,-40.5223510101973,
3.36146460586381));
#248720=CARTESIAN_POINT('Ctrl Pts',(-45.2560606910588,-40.4923970402283,
3.23423045308356));
#248721=CARTESIAN_POINT('Ctrl Pts',(-45.4410373245168,-40.4880553924345,
3.36123028058453));
#248722=CARTESIAN_POINT('Ctrl Pts',(-45.3560577375092,-40.5824347852702,
3.36123028058453));
#248723=CARTESIAN_POINT('Ctrl Pts',(-45.3560577375093,-40.5824347852702,
3.23423028058453));
#248724=CARTESIAN_POINT('Origin',(-45.1958291143585,-40.2672689283129,3.42473028058452));
#248725=CARTESIAN_POINT('Origin',(-45.1353740846429,-40.2128349746541,3.56563113524785));
#248726=CARTESIAN_POINT('Origin',(-40.8647803224533,-45.8594327460074,3.56647653909403));
#248727=CARTESIAN_POINT('Origin',(-40.8943347850521,-45.8923335519892,3.64299466007529));
#248728=CARTESIAN_POINT('Origin',(-40.8100197873543,-45.7986150108453,3.42473028058451));
#248729=CARTESIAN_POINT('Ctrl Pts',(-40.7368493365293,-45.7165002428309,
3.48823028058451));
#248730=CARTESIAN_POINT('Ctrl Pts',(-40.8311340869933,-45.6322662944334,
3.48794691941567));
#248731=CARTESIAN_POINT('Ctrl Pts',(-40.9043991801899,-45.7136354238377,
3.42473028058452));
#248732=CARTESIAN_POINT('Ctrl Pts',(-40.7066485019706,-45.6831319408675,
3.41028005925053));
#248733=CARTESIAN_POINT('Ctrl Pts',(-40.800864206014,-45.5986481857962,
3.40982512230997));
#248734=CARTESIAN_POINT('Ctrl Pts',(-40.8592275074395,-45.6634671987653,
3.30780486372868));
#248735=CARTESIAN_POINT('Ctrl Pts',(-40.649432716852,-45.6199161851844,
3.36123028058449));
#248736=CARTESIAN_POINT('Ctrl Pts',(-40.743582157414,-45.535030025744,3.36099721048404));
#248737=CARTESIAN_POINT('Ctrl Pts',(-40.7736504989785,-45.5684243021869,
3.23423045308392));
#248738=CARTESIAN_POINT('Ctrl Pts',(-40.5892333705618,-45.5534068532513,
3.36123028058449));
#248739=CARTESIAN_POINT('Ctrl Pts',(-40.6836127633975,-45.4684272662438,
3.36123028058449));
#248740=CARTESIAN_POINT('Ctrl Pts',(-40.6836127633975,-45.4684272662438,
3.23423028058449));
#248741=CARTESIAN_POINT('Origin',(-40.5892333705618,-45.5534068532513,3.23423028058449));
#248742=CARTESIAN_POINT('Origin',(0.23594848208908,-0.212448967518752,3.64303198860262));
#248743=CARTESIAN_POINT('Origin',(-41.1629311642476,-46.1905628026487,3.6430319886023));
#248744=CARTESIAN_POINT('Origin',(0.23594848208908,-0.212448967518749,3.23423028058481));
#248745=CARTESIAN_POINT('Origin',(-40.4880553924339,-45.4410373245173,3.23423028058449));
#248746=CARTESIAN_POINT('Ctrl Pts',(-41.5228599914559,-46.5911245387432,
3.47153072139039));
#248747=CARTESIAN_POINT('Ctrl Pts',(-41.6181024670993,-46.5059978322077,
3.47182327902629));
#248748=CARTESIAN_POINT('Ctrl Pts',(-41.5454735131715,-46.4256208133854,
3.40413028959007));
#248749=CARTESIAN_POINT('Ctrl Pts',(-41.4460088704661,-46.505598791845,
3.65553807120923));
#248750=CARTESIAN_POINT('Ctrl Pts',(-41.5410583874213,-46.4204321019767,
3.65586275496799));
#248751=CARTESIAN_POINT('Ctrl Pts',(-41.4839460439596,-46.3572876358792,
3.5512812683718));
#248752=CARTESIAN_POINT('Ctrl Pts',(-41.3079491749513,-46.3519544194672,
3.7700319886023));
#248753=CARTESIAN_POINT('Ctrl Pts',(-41.4027599825085,-46.2668368728742,
3.77025505748597));
#248754=CARTESIAN_POINT('Ctrl Pts',(-41.3734144471009,-46.2345298607748,
3.64284211731165));
#248755=CARTESIAN_POINT('Ctrl Pts',(-41.1629311642476,-46.1905628026487,
3.7700319886023));
#248756=CARTESIAN_POINT('Ctrl Pts',(-41.2574515555196,-46.1054562600788,
3.7700319886023));
#248757=CARTESIAN_POINT('Ctrl Pts',(-41.2573104519179,-46.1055833103324,
3.64284239821689));
#248758=CARTESIAN_POINT('Origin',(-41.451202041617,-46.5107200467159,3.40423097483277));
#248759=CARTESIAN_POINT('Ctrl Pts',(-40.4880553924339,-45.4410373245173,
3.36123028058449));
#248760=CARTESIAN_POINT('Ctrl Pts',(-40.5824347852696,-45.3560577375098,
3.36123028058449));
#248761=CARTESIAN_POINT('Ctrl Pts',(-40.5824347852696,-45.3560577375098,
3.23423028058449));
#248762=CARTESIAN_POINT('Ctrl Pts',(-40.4276521486877,-45.3743035899551,
3.36123028058449));
#248763=CARTESIAN_POINT('Ctrl Pts',(-40.5221480762965,-45.2891025640463,
3.36146538610272));
#248764=CARTESIAN_POINT('Ctrl Pts',(-40.4920927345057,-45.255722725316,
3.23423043688376));
#248765=CARTESIAN_POINT('Ctrl Pts',(-40.3705349278737,-45.3112030195552,
3.41054258693066));
#248766=CARTESIAN_POINT('Ctrl Pts',(-40.4654317778761,-45.2261127332245,
3.41100608859622));
#248767=CARTESIAN_POINT('Ctrl Pts',(-40.4066678844402,-45.1608488177559,
3.30819866970767));
#248768=CARTESIAN_POINT('Ctrl Pts',(-40.3404336838189,-45.2779489569774,
3.48823028058449));
#248769=CARTESIAN_POINT('Ctrl Pts',(-40.4355776097265,-45.1929563204591,
3.48852004212226));
#248770=CARTESIAN_POINT('Ctrl Pts',(-40.361648321148,-45.1108495273514,
3.42473028058448));
#248771=CARTESIAN_POINT('Origin',(-40.2672689283123,-45.195829114359,3.42473028058447));
#248772=CARTESIAN_POINT('Origin',(-41.5704070646284,-46.6431106370687,3.1191364817825));
#248773=CARTESIAN_POINT('Origin',(-41.6896120874666,-46.7755012272975,2.83404198860228));
#248774=CARTESIAN_POINT('Origin',(-40.2128349741381,-45.1353740836141,3.56563113460706));
#248775=CARTESIAN_POINT('Origin',(-40.1828829233539,-45.1021848870412,3.64299171721761));
#248776=CARTESIAN_POINT('Ctrl Pts',(-42.1132001505997,-46.7942619810919,
2.5990817351599));
#248777=CARTESIAN_POINT('Ctrl Pts',(-42.0882450513171,-46.7665330160781,
2.65878198860228));
#248778=CARTESIAN_POINT('Ctrl Pts',(-42.0411527846891,-46.7142062431424,
2.65878198860228));
#248779=CARTESIAN_POINT('Ctrl Pts',(-42.0477032750703,-46.853206711919,
2.59908193475449));
#248780=CARTESIAN_POINT('Ctrl Pts',(-42.0405341034508,-46.8094668591673,
2.65878715325307));
#248781=CARTESIAN_POINT('Ctrl Pts',(-42.0032346206989,-46.748319038878,
2.65878198860228));
#248782=CARTESIAN_POINT('Ctrl Pts',(-41.9705316734061,-46.8890030154864,
2.63878778849854));
#248783=CARTESIAN_POINT('Ctrl Pts',(-41.9811230778539,-46.8318174060855,
2.69564460180075));
#248784=CARTESIAN_POINT('Ctrl Pts',(-41.9515093836253,-46.7612038509546,
2.6818048162485));
#248785=CARTESIAN_POINT('Ctrl Pts',(-41.8426461117364,-46.906368706767,
2.75443238878597));
#248786=CARTESIAN_POINT('Ctrl Pts',(-41.8933796070862,-46.8290619651513,
2.79268340777068));
#248787=CARTESIAN_POINT('Ctrl Pts',(-41.8570065263032,-46.7485125544803,
2.74885926835577));
#248788=CARTESIAN_POINT('Ctrl Pts',(-41.7917018131134,-46.8896982576902,
2.82856655361648));
#248789=CARTESIAN_POINT('Ctrl Pts',(-41.8649047103987,-46.8032976561885,
2.8538419723072));
#248790=CARTESIAN_POINT('Ctrl Pts',(-41.8144193983033,-46.724315266822,
2.79184624278382));
#248791=CARTESIAN_POINT('Ctrl Pts',(-41.7612723673359,-46.8559036426987,
2.90134173515991));
#248792=CARTESIAN_POINT('Ctrl Pts',(-41.8563683535926,-46.7709043015504,
2.90163218716358));
#248793=CARTESIAN_POINT('Ctrl Pts',(-41.7839914803023,-46.6905216402899,
2.83404198860229));
#248794=CARTESIAN_POINT('Origin',(-42.0411527846891,-46.7142062431424,2.53178198860228));
#248795=CARTESIAN_POINT('Origin',(0.23594848208908,-0.212448967518752,3.64303198860262));
#248796=CARTESIAN_POINT('Origin',(-39.9143573409153,-44.8038810887676,3.64303198860231));
#248797=CARTESIAN_POINT('Origin',(8.0125006576031E-17,1.91699971593277E-13,
2.53178198860262));
#248798=CARTESIAN_POINT('Origin',(-42.0638038389696,-46.6938111422606,2.53178198860228));
#248799=CARTESIAN_POINT('Ctrl Pts',(-39.9143573409153,-44.8038810887676,
3.77003198860231));
#248800=CARTESIAN_POINT('Ctrl Pts',(-40.0088781183433,-44.7187741985013,
3.77003198860231));
#248801=CARTESIAN_POINT('Ctrl Pts',(-40.0087366280092,-44.7189015969703,
3.64284187937008));
#248802=CARTESIAN_POINT('Ctrl Pts',(-39.7693421853875,-44.6424822887503,
3.77003198860232));
#248803=CARTESIAN_POINT('Ctrl Pts',(-39.8638196089375,-44.5576711710521,
3.76980208962971));
#248804=CARTESIAN_POINT('Ctrl Pts',(-39.8926305794713,-44.5899527660326,
3.64284193928275));
#248805=CARTESIAN_POINT('Ctrl Pts',(-39.6312917695244,-44.4888315723753,
3.65553535416554));
#248806=CARTESIAN_POINT('Ctrl Pts',(-39.7256919284553,-44.4042655856119,
3.6552005783438));
#248807=CARTESIAN_POINT('Ctrl Pts',(-39.7820998051101,-44.4671959043835,
3.55127910964178));
#248808=CARTESIAN_POINT('Ctrl Pts',(-39.5544469813067,-44.4033023070491,
3.47153072139042));
#248809=CARTESIAN_POINT('Ctrl Pts',(-39.6488649704634,-44.3189410144583,
3.47122746281552));
#248810=CARTESIAN_POINT('Ctrl Pts',(-39.720573090053,-44.3988635644383,
3.40413045901239));
#248811=CARTESIAN_POINT('Origin',(-39.6260861683714,-44.4837235168758,3.40423097483279));
#248812=CARTESIAN_POINT('Ctrl Pts',(-42.2339804752697,-46.4302753505427,
2.90134173515991));
#248813=CARTESIAN_POINT('Ctrl Pts',(-42.1395065320995,-46.5159655405277,
2.90163218716358));
#248814=CARTESIAN_POINT('Ctrl Pts',(-42.0671296588092,-46.4355828792672,
2.83404198860229));
#248815=CARTESIAN_POINT('Ctrl Pts',(-42.2644230274465,-46.4640859592732,
2.8285334983533));
#248816=CARTESIAN_POINT('Ctrl Pts',(-42.1708479205188,-46.5278479142023,
2.85381483162399));
#248817=CARTESIAN_POINT('Ctrl Pts',(-42.0975714415919,-46.4693919041993,
2.79182701594314));
#248818=CARTESIAN_POINT('Ctrl Pts',(-42.2755508889259,-46.5163638812299,
2.754688220736));
#248819=CARTESIAN_POINT('Ctrl Pts',(-42.1933444849776,-46.5588164356978,
2.79286913083808));
#248820=CARTESIAN_POINT('Ctrl Pts',(-42.1170605480848,-46.5141432491637,
2.74900763297869));
#248821=CARTESIAN_POINT('Ctrl Pts',(-42.2454039774542,-46.6408663419435,
2.63954450640368));
#248822=CARTESIAN_POINT('Ctrl Pts',(-42.187220455932,-46.6457133039298,
2.69627684028821));
#248823=CARTESIAN_POINT('Ctrl Pts',(-42.119999535554,-46.6088541045839,
2.68224356036468));
#248824=CARTESIAN_POINT('Ctrl Pts',(-42.201574971429,-46.7146600431956,
2.5990817870629));
#248825=CARTESIAN_POINT('Ctrl Pts',(-42.1587905896506,-46.7029882531948,
2.65878704321527));
#248826=CARTESIAN_POINT('Ctrl Pts',(-42.1018187547554,-46.6595535157374,
2.65878198860228));
#248827=CARTESIAN_POINT('Ctrl Pts',(-42.1358900227691,-46.7738319284259,
2.5990817351599));
#248828=CARTESIAN_POINT('Ctrl Pts',(-42.1109214781057,-46.7461150696874,
2.65878198860228));
#248829=CARTESIAN_POINT('Ctrl Pts',(-42.0638038389696,-46.6938111422606,
2.65878198860228));
#248830=CARTESIAN_POINT('Origin',(-42.1615090516448,-46.3506032922596,2.83404198860229));
#248831=CARTESIAN_POINT('Origin',(-39.506880981537,-44.3513327445029,3.11913648166909));
#248832=CARTESIAN_POINT('Origin',(-39.387675794557,-44.2189419720524,2.8340419886023));
#248833=CARTESIAN_POINT('Origin',(-42.0423040287658,-46.2182127020492,3.11913648177404));
#248834=CARTESIAN_POINT('Origin',(-41.9230990057951,-46.085822111678,3.40423097483277));
#248835=CARTESIAN_POINT('Ctrl Pts',(-39.3160391863686,-44.1385184650377,
2.90134173515992));
#248836=CARTESIAN_POINT('Ctrl Pts',(-39.4103156382728,-44.0542875439842,
2.90103711553198));
#248837=CARTESIAN_POINT('Ctrl Pts',(-39.4820551873926,-44.1339623850449,
2.8340419886023));
#248838=CARTESIAN_POINT('Ctrl Pts',(-39.2856369388931,-44.1047525536517,
2.82862991747916));
#248839=CARTESIAN_POINT('Ctrl Pts',(-39.3789425853224,-44.0421527706803,
2.85314045886441));
#248840=CARTESIAN_POINT('Ctrl Pts',(-39.4516512848559,-44.1001954303879,
2.79187960999956));
#248841=CARTESIAN_POINT('Ctrl Pts',(-39.2745942850996,-44.0527517782421,
2.75470625793312));
#248842=CARTESIAN_POINT('Ctrl Pts',(-39.3566016867493,-44.0110417363802,
2.79224250381888));
#248843=CARTESIAN_POINT('Ctrl Pts',(-39.4323285306297,-44.0556530121005,
2.74901809108238));
#248844=CARTESIAN_POINT('Ctrl Pts',(-39.3050549810248,-43.9290071509455,
2.63947868311649));
#248845=CARTESIAN_POINT('Ctrl Pts',(-39.3631024520339,-43.9243964923857,
2.69595066767864));
#248846=CARTESIAN_POINT('Ctrl Pts',(-39.4299498468376,-43.961478133811,
2.68220539436019));
#248847=CARTESIAN_POINT('Ctrl Pts',(-39.3490583909334,-43.8557442421761,
2.59908178584995));
#248848=CARTESIAN_POINT('Ctrl Pts',(-39.3917348424044,-43.8675206320103,
2.65877670944855));
#248849=CARTESIAN_POINT('Ctrl Pts',(-39.4485000225466,-43.9111340157071,
2.6587819886023));
#248850=CARTESIAN_POINT('Ctrl Pts',(-39.4144401478986,-43.7969047596348,
2.59908173515992));
#248851=CARTESIAN_POINT('Ctrl Pts',(-39.4393948122684,-43.8246341160487,
2.6587819886023));
#248852=CARTESIAN_POINT('Ctrl Pts',(-39.4864862581813,-43.8769616275876,
2.6587819886023));
#248853=CARTESIAN_POINT('Origin',(-39.4864862581813,-43.8769616275876,2.5317819886023));
#248854=CARTESIAN_POINT('Ctrl Pts',(-41.6348281284258,-45.7656648676108,
3.77003198860231));
#248855=CARTESIAN_POINT('Ctrl Pts',(-41.5403077290109,-45.8507714175126,
3.77003198860231));
#248856=CARTESIAN_POINT('Ctrl Pts',(-41.5404488407676,-45.8506443599161,
3.64284238727582));
#248857=CARTESIAN_POINT('Ctrl Pts',(-41.7801793767998,-45.926760978665,
3.7700319886023));
#248858=CARTESIAN_POINT('Ctrl Pts',(-41.6856176794272,-46.0121552117509,
3.77025506105692));
#248859=CARTESIAN_POINT('Ctrl Pts',(-41.6565546403142,-45.9795929135662,
3.64284210641874));
#248860=CARTESIAN_POINT('Ctrl Pts',(-41.9185498083229,-46.0801233673968,
3.65553527987801));
#248861=CARTESIAN_POINT('Ctrl Pts',(-41.8239142817198,-46.1657498592366,
3.65585996533074));
#248862=CARTESIAN_POINT('Ctrl Pts',(-41.7670853619603,-46.1023497159504,
3.55127902710108));
#248863=CARTESIAN_POINT('Ctrl Pts',(-41.9955727382247,-46.1654920697614,
3.47153072139039));
#248864=CARTESIAN_POINT('Ctrl Pts',(-41.9009568069089,-46.2513146407504,
3.47182327905155));
#248865=CARTESIAN_POINT('Ctrl Pts',(-41.8286118967076,-46.1706818552411,
3.40413028377963));
#248866=CARTESIAN_POINT('Origin',(-41.6348281284258,-45.7656648676108,3.64303198860231));
#248867=CARTESIAN_POINT('Origin',(3.72719664096538E-16,1.91533843916112E-13,
2.53178198860262));
#248868=CARTESIAN_POINT('Origin',(-39.5091373124618,-43.8565665267058,2.53178198860231));
#248869=CARTESIAN_POINT('Origin',(27.6232705441538,31.1532462714326,3.64303198860284));
#248870=CARTESIAN_POINT('Origin',(-41.3663085755616,-45.4673664422114,3.64299466007618));
#248871=CARTESIAN_POINT('Ctrl Pts',(-39.4370498736004,-43.7765468711724,
2.59908173515992));
#248872=CARTESIAN_POINT('Ctrl Pts',(-39.4620188529806,-43.8042633382931,
2.65878198860231));
#248873=CARTESIAN_POINT('Ctrl Pts',(-39.5091373124618,-43.8565665267058,
2.6587819886023));
#248874=CARTESIAN_POINT('Ctrl Pts',(-39.502178522486,-43.7178744835419,
2.599081931998));
#248875=CARTESIAN_POINT('Ctrl Pts',(-39.5094654441324,-43.7615157339664,
2.65877685806551));
#248876=CARTESIAN_POINT('Ctrl Pts',(-39.5469637653732,-43.8224770900121,
2.6587819886023));
#248877=CARTESIAN_POINT('Ctrl Pts',(-39.5788516269098,-43.6818502604298,
2.63872492669776));
#248878=CARTESIAN_POINT('Ctrl Pts',(-39.5685043961835,-43.7389249259238,
2.69532212015268));
#248879=CARTESIAN_POINT('Ctrl Pts',(-39.5983821485328,-43.8091917332945,
2.68176836726603));
#248880=CARTESIAN_POINT('Ctrl Pts',(-39.7059848156955,-43.6640874258691,
2.75442176402208));
#248881=CARTESIAN_POINT('Ctrl Pts',(-39.656016872279,-43.7412697217733,
2.79203179920073));
#248882=CARTESIAN_POINT('Ctrl Pts',(-39.692386550076,-43.8212571467117,
2.74885310748143));
#248883=CARTESIAN_POINT('Ctrl Pts',(-39.7566878101782,-43.6806424921196,
2.82866089558376));
#248884=CARTESIAN_POINT('Ctrl Pts',(-39.684669524313,-43.7668962219026,
2.85316563119219));
#248885=CARTESIAN_POINT('Ctrl Pts',(-39.7348023770063,-43.8452710114193,
2.79189751796567));
#248886=CARTESIAN_POINT('Ctrl Pts',(-39.7870778846743,-43.7143933160625,
2.90134173515992));
#248887=CARTESIAN_POINT('Ctrl Pts',(-39.6934538167797,-43.7993487829614,
2.90103711553198));
#248888=CARTESIAN_POINT('Ctrl Pts',(-39.7651933658995,-43.8790236240221,
2.8340419886023));
#248889=CARTESIAN_POINT('Origin',(-39.8595727587351,-43.7940440370146,2.83404198860231));
#248890=CARTESIAN_POINT('Origin',(-41.3366772856885,-45.4345348103665,3.56647653971706));
#248891=CARTESIAN_POINT('Origin',(-41.2819167515325,-45.3737170758074,3.42473028058453));
#248892=CARTESIAN_POINT('Origin',(-39.9787779456587,-43.9264348094898,3.11913648168119));
#248893=CARTESIAN_POINT('Origin',(-40.0979831325495,-44.0588255818379,3.40423097483279));
#248894=CARTESIAN_POINT('Ctrl Pts',(-41.06113033474,-45.1285089182134,3.36123028058449));
#248895=CARTESIAN_POINT('Ctrl Pts',(-40.9667509419044,-45.213488505221,
3.36123028058449));
#248896=CARTESIAN_POINT('Ctrl Pts',(-40.9667509419044,-45.213488505221,
3.23423028058449));
#248897=CARTESIAN_POINT('Ctrl Pts',(-41.1211850608429,-45.1955564429372,
3.36123028058449));
#248898=CARTESIAN_POINT('Ctrl Pts',(-41.0269231466364,-45.2803165088395,
3.36099641108397));
#248899=CARTESIAN_POINT('Ctrl Pts',(-41.0570929845757,-45.313823508427,
3.23423043688387));
#248900=CARTESIAN_POINT('Ctrl Pts',(-41.1779726855657,-45.2589537050075,
3.41054258905252));
#248901=CARTESIAN_POINT('Ctrl Pts',(-41.0841042944903,-45.34382260726,3.41008815825996));
#248902=CARTESIAN_POINT('Ctrl Pts',(-41.1425178129606,-45.4086973919085,
3.3081986730428));
#248903=CARTESIAN_POINT('Ctrl Pts',(-41.2079002115903,-45.2923641298559,
3.48823028058451));
#248904=CARTESIAN_POINT('Ctrl Pts',(-41.1142722655002,-45.3773275334107,
3.48794691941567));
#248905=CARTESIAN_POINT('Ctrl Pts',(-41.1875373586968,-45.458696662815,
3.42473028058452));
#248906=CARTESIAN_POINT('Origin',(-41.06113033474,-45.1285089182134,3.23423028058449));
#248907=CARTESIAN_POINT('Ctrl Pts',(-40.0254908126584,-43.9791725362584,
3.47153072139041));
#248908=CARTESIAN_POINT('Ctrl Pts',(-39.9317223035493,-44.0642551277132,
3.47122746285046));
#248909=CARTESIAN_POINT('Ctrl Pts',(-40.0037114707675,-44.1439246046466,
3.40413046676764));
#248910=CARTESIAN_POINT('Ctrl Pts',(-40.1025202360401,-44.0645378932523,
3.65553813457955));
#248911=CARTESIAN_POINT('Ctrl Pts',(-40.0085500157875,-44.1495813562431,
3.65520336072111));
#248912=CARTESIAN_POINT('Ctrl Pts',(-40.0652391174783,-44.2122579788851,
3.5512813451992));
#248913=CARTESIAN_POINT('Ctrl Pts',(-40.2409001323891,-44.2178941385649,
3.77003198860231));
#248914=CARTESIAN_POINT('Ctrl Pts',(-40.1466780419446,-44.3029888158489,
3.76980209314098));
#248915=CARTESIAN_POINT('Ctrl Pts',(-40.1757707681163,-44.3350158129988,
3.64284195387372));
#248916=CARTESIAN_POINT('Ctrl Pts',(-40.3862543050934,-44.3789831537297,
3.77003198860232));
#248917=CARTESIAN_POINT('Ctrl Pts',(-40.2917335385821,-44.4640900341667,
3.77003198860231));
#248918=CARTESIAN_POINT('Ctrl Pts',(-40.2918750179832,-44.4639626455417,
3.64284189403786));
#248919=CARTESIAN_POINT('Origin',(-40.3862543050934,-44.3789831537297,3.64303198860232));
#248920=CARTESIAN_POINT('Origin',(26.9484406282047,30.4037717213984,3.23423028058503));
#248921=CARTESIAN_POINT('Origin',(-40.9599523566121,-45.0161393894795,3.23423028058449));
#248922=CARTESIAN_POINT('Origin',(26.8427652369004,30.2864073093063,3.64303198860284));
#248923=CARTESIAN_POINT('Origin',(-40.6548553974682,-44.6772189625504,3.64299171721637));
#248924=CARTESIAN_POINT('Ctrl Pts',(-40.8131880745603,-44.8522789915943,
3.48823028058449));
#248925=CARTESIAN_POINT('Ctrl Pts',(-40.7187157882333,-44.9380175594364,
3.48852004212228));
#248926=CARTESIAN_POINT('Ctrl Pts',(-40.6447864996549,-44.8559107663287,
3.42473028058449));
#248927=CARTESIAN_POINT('Ctrl Pts',(-40.8432146576644,-44.8858042435429,
3.41028005848375));
#248928=CARTESIAN_POINT('Ctrl Pts',(-40.748670873839,-44.9712860523923,
3.41074404220453));
#248929=CARTESIAN_POINT('Ctrl Pts',(-40.6899581892261,-44.9060790100825,
3.30780486243839));
#248930=CARTESIAN_POINT('Ctrl Pts',(-40.900100336765,-44.9493173051398,
3.36123028058449));
#248931=CARTESIAN_POINT('Ctrl Pts',(-40.8054891887065,-45.0343891839532,
3.36146460586165));
#248932=CARTESIAN_POINT('Ctrl Pts',(-40.7755352187361,-45.0011219300382,
3.2342304530842));
#248933=CARTESIAN_POINT('Ctrl Pts',(-40.9599523566121,-45.0161393894795,
3.36123028058449));
#248934=CARTESIAN_POINT('Ctrl Pts',(-40.8655729637765,-45.101118976487,
3.3612302805845));
#248935=CARTESIAN_POINT('Ctrl Pts',(-40.8655729637765,-45.1011189764871,
3.23423028058449));
#248936=CARTESIAN_POINT('Origin',(-40.7391658924905,-44.7709311793211,3.42473028058448));
#248937=CARTESIAN_POINT('Origin',(-40.6847319392787,-44.7104761492006,3.56563113524681));
#248938=CARTESIAN_POINT('Origin',(-35.8473027488272,-49.8797426639491,3.5664765390944));
#248939=CARTESIAN_POINT('Origin',(-35.8732562382983,-49.9155525184326,3.64299466007498));
#248940=CARTESIAN_POINT('Origin',(-35.7991993820658,-49.8135340601224,3.42473028058448));
#248941=CARTESIAN_POINT('Ctrl Pts',(-35.7350130971385,-49.7242207306176,
3.48823028058448));
#248942=CARTESIAN_POINT('Ctrl Pts',(-35.8375861910552,-49.6503036646787,
3.48794691941564));
#248943=CARTESIAN_POINT('Ctrl Pts',(-35.9019445403514,-49.7388853330813,
3.42473028058449));
#248944=CARTESIAN_POINT('Ctrl Pts',(-35.7084656432366,-49.6878783768787,
3.41028005925051));
#248945=CARTESIAN_POINT('Ctrl Pts',(-35.8109961808822,-49.6137056554105,
3.40982512230884));
#248946=CARTESIAN_POINT('Ctrl Pts',(-35.8622643302221,-49.6842702092588,
3.30780486372859));
#248947=CARTESIAN_POINT('Ctrl Pts',(-35.6581711379697,-49.6190282456277,
3.36123028058446));
#248948=CARTESIAN_POINT('Ctrl Pts',(-35.7606778378488,-49.5444483977922,
3.36099721048756));
#248949=CARTESIAN_POINT('Ctrl Pts',(-35.7870908094917,-49.5808027344274,
3.23423045308409));
#248950=CARTESIAN_POINT('Ctrl Pts',(-35.6052536882598,-49.5465907136146,
3.36123028058446));
#248951=CARTESIAN_POINT('Ctrl Pts',(-35.7079988465454,-49.4719419865735,
3.36123028058446));
#248952=CARTESIAN_POINT('Ctrl Pts',(-35.7079988465454,-49.4719419865735,
3.23423028058446));
#248953=CARTESIAN_POINT('Origin',(-35.6052536882598,-49.5465907136146,3.23423028058446));
#248954=CARTESIAN_POINT('Origin',(0.256862895714053,-0.186621817602674,
3.64303198860262));
#248955=CARTESIAN_POINT('Origin',(-36.1092077731524,-50.2402240048084,3.64303198860227));
#248956=CARTESIAN_POINT('Origin',(0.256862895714053,-0.186621817602671,
3.23423028058481));
#248957=CARTESIAN_POINT('Origin',(-35.5163757878391,-49.4242607783462,3.23423028058446));
#248958=CARTESIAN_POINT('Ctrl Pts',(-36.4252947698674,-50.676214228995,
3.47153072139035));
#248959=CARTESIAN_POINT('Ctrl Pts',(-36.5289136610807,-50.601509405082,
3.47182327902626));
#248960=CARTESIAN_POINT('Ctrl Pts',(-36.4650842624219,-50.5139809070359,
3.4041302895903));
#248961=CARTESIAN_POINT('Ctrl Pts',(-36.357804522255,-50.5831238715078,
3.6555380712092));
#248962=CARTESIAN_POINT('Ctrl Pts',(-36.461235691223,-50.5083591136197,
3.65586275496875));
#248963=CARTESIAN_POINT('Ctrl Pts',(-36.4110366091574,-50.4395906940183,
3.5512812683713));
#248964=CARTESIAN_POINT('Ctrl Pts',(-36.2365613423289,-50.4158900112688,
3.77003198860227));
#248965=CARTESIAN_POINT('Ctrl Pts',(-36.3397499727028,-50.3411491755192,
3.77025505748459));
#248966=CARTESIAN_POINT('Ctrl Pts',(-36.3139421975399,-50.3059517008918,
3.64284211731228));
#248967=CARTESIAN_POINT('Ctrl Pts',(-36.1092077731524,-50.2402240048084,
3.77003198860227));
#248968=CARTESIAN_POINT('Ctrl Pts',(-36.2121064279396,-50.165463756031,
3.77003198860227));
#248969=CARTESIAN_POINT('Ctrl Pts',(-36.2119528169509,-50.1655753609471,
3.64284239821737));
#248970=CARTESIAN_POINT('Origin',(-36.3624339277669,-50.5887599058102,3.40423097483274));
#248971=CARTESIAN_POINT('Ctrl Pts',(-35.5163757878391,-49.4242607783462,
3.36123028058446));
#248972=CARTESIAN_POINT('Ctrl Pts',(-35.6191209461248,-49.3496120513051,
3.36123028058446));
#248973=CARTESIAN_POINT('Ctrl Pts',(-35.6191209461248,-49.3496120513051,
3.23423028058446));
#248974=CARTESIAN_POINT('Ctrl Pts',(-35.4632790141045,-49.351578759919,
3.36123028058446));
#248975=CARTESIAN_POINT('Ctrl Pts',(-35.5661632154437,-49.276721988246,
3.36146538609945));
#248976=CARTESIAN_POINT('Ctrl Pts',(-35.5397616632048,-49.2403833690725,
3.23423043688379));
#248977=CARTESIAN_POINT('Ctrl Pts',(-35.4130704930567,-49.2828534857288,
3.41054258693064));
#248978=CARTESIAN_POINT('Ctrl Pts',(-35.51634184505,-49.2081487547866,3.41100608859729));
#248979=CARTESIAN_POINT('Ctrl Pts',(-35.464721803166,-49.1370998624003,
3.30819866970716));
#248980=CARTESIAN_POINT('Ctrl Pts',(-35.3866101428255,-49.2466351556014,
3.48823028058446));
#248981=CARTESIAN_POINT('Ctrl Pts',(-35.4901170100363,-49.1720533660032,
3.48852004212224));
#248982=CARTESIAN_POINT('Ctrl Pts',(-35.4251752107434,-49.0826686475736,
3.42473028058446));
#248983=CARTESIAN_POINT('Origin',(-35.3224300524577,-49.1573173746147,3.42473028058445));
#248984=CARTESIAN_POINT('Origin',(-36.4671473482312,-50.7328855645266,3.1191364817836));
#248985=CARTESIAN_POINT('Origin',(-36.5718607685317,-50.8770112231004,2.83404198860225));
#248986=CARTESIAN_POINT('Origin',(-35.2746135646431,-49.0915036252753,3.56563113460834));
#248987=CARTESIAN_POINT('Origin',(-35.2482948100394,-49.0553654007527,3.64299171721764));
#248988=CARTESIAN_POINT('Ctrl Pts',(-36.9911673391703,-50.9399462128203,
2.59908173515987));
#248989=CARTESIAN_POINT('Ctrl Pts',(-36.9692474126336,-50.9097606317995,
2.65878198860225));
#248990=CARTESIAN_POINT('Ctrl Pts',(-36.9278827595322,-50.8527980281386,
2.65878198860226));
#248991=CARTESIAN_POINT('Ctrl Pts',(-36.9198678602467,-50.9917217504956,
2.59908193475606));
#248992=CARTESIAN_POINT('Ctrl Pts',(-36.9173100216886,-50.947472126738,
2.65878715325367));
#248993=CARTESIAN_POINT('Ctrl Pts',(-36.886606557094,-50.8827604229954,
2.65878198860226));
#248994=CARTESIAN_POINT('Ctrl Pts',(-36.8393772800886,-51.0192553292379,
2.63878778849838));
#248995=CARTESIAN_POINT('Ctrl Pts',(-36.8558881875863,-50.9634900918198,
2.6956446018007));
#248996=CARTESIAN_POINT('Ctrl Pts',(-36.8338178466772,-50.8901678911825,
2.6818048162485));
#248997=CARTESIAN_POINT('Ctrl Pts',(-36.7103770798839,-51.0231582082089,
2.75443238878605));
#248998=CARTESIAN_POINT('Ctrl Pts',(-36.7689134067392,-50.9515780553173,
2.79268340777063));
#248999=CARTESIAN_POINT('Ctrl Pts',(-36.7411592876128,-50.8676678805078,
2.74885926835571));
#249000=CARTESIAN_POINT('Ctrl Pts',(-36.6614543958819,-51.0012539523501,
2.82856655361637));
#249001=CARTESIAN_POINT('Ctrl Pts',(-36.7432876021361,-50.9229784487439,
2.8538419723075));
#249002=CARTESIAN_POINT('Ctrl Pts',(-36.7013347616504,-50.8391515810786,
2.79184624278418));
#249003=CARTESIAN_POINT('Ctrl Pts',(-36.634724144965,-50.9644637245894,
2.90134173515988));
#249004=CARTESIAN_POINT('Ctrl Pts',(-36.738184035968,-50.8898702560319,
2.90163218716355));
#249005=CARTESIAN_POINT('Ctrl Pts',(-36.6746059268174,-50.8023624960592,
2.83404198860226));
#249006=CARTESIAN_POINT('Origin',(-36.9278827595322,-50.8527980281386,2.53178198860225));
#249007=CARTESIAN_POINT('Origin',(0.256862895714053,-0.186621817602674,
3.64303198860262));
#249008=CARTESIAN_POINT('Origin',(-35.0124214764581,-48.7306271754178,3.64303198860228));
#249009=CARTESIAN_POINT('Origin',(6.67120042669018E-17,1.91710833228385E-13,
2.53178198860262));
#249010=CARTESIAN_POINT('Origin',(-36.9525415975208,-50.8348823336487,2.53178198860226));
#249011=CARTESIAN_POINT('Ctrl Pts',(-35.0124214764581,-48.7306271754178,
3.77003198860228));
#249012=CARTESIAN_POINT('Ctrl Pts',(-35.1153205516304,-48.6558666212126,
3.77003198860228));
#249013=CARTESIAN_POINT('Ctrl Pts',(-35.115166519629,-48.6559785320123,
3.64284187937004));
#249014=CARTESIAN_POINT('Ctrl Pts',(-34.8850714976646,-48.5549543235565,
3.77003198860229));
#249015=CARTESIAN_POINT('Ctrl Pts',(-34.9878965398059,-48.4804833899309,
3.7698020896304));
#249016=CARTESIAN_POINT('Ctrl Pts',(-35.0131753353115,-48.5155997094328,
3.6428419392829));
#249017=CARTESIAN_POINT('Ctrl Pts',(-34.7638382096868,-48.3877151240588,
3.65553535416552));
#249018=CARTESIAN_POINT('Ctrl Pts',(-34.8665607873097,-48.3134799021651,
3.65520057834337));
#249019=CARTESIAN_POINT('Ctrl Pts',(-34.916081646201,-48.3819617107285,
3.5512791096416));
#249020=CARTESIAN_POINT('Ctrl Pts',(-34.6963546279281,-48.2946219293748,
3.47153072139038));
#249021=CARTESIAN_POINT('Ctrl Pts',(-34.7990735417348,-48.220592144083,
3.47122746281549));
#249022=CARTESIAN_POINT('Ctrl Pts',(-34.8620346554126,-48.3075724095163,
3.40413045901235));
#249023=CARTESIAN_POINT('Origin',(-34.759195062553,-48.3820909175331,3.40423097483276));
#249024=CARTESIAN_POINT('Ctrl Pts',(-37.1493329797256,-50.5905785208486,
2.90134173515987));
#249025=CARTESIAN_POINT('Ctrl Pts',(-37.0464195108248,-50.6659240749085,
2.90163218716355));
#249026=CARTESIAN_POINT('Ctrl Pts',(-36.9828414016742,-50.5784163149358,
2.83404198860226));
#249027=CARTESIAN_POINT('Ctrl Pts',(-37.1760745934433,-50.627386024724,
2.82853349835321));
#249028=CARTESIAN_POINT('Ctrl Pts',(-37.0763471615781,-50.6810174228632,
2.85381483162248));
#249029=CARTESIAN_POINT('Ctrl Pts',(-37.0095824157651,-50.6152221632656,
2.79182701594302));
#249030=CARTESIAN_POINT('Ctrl Pts',(-37.1816769644888,-50.6805407410137,
2.75468822073603));
#249031=CARTESIAN_POINT('Ctrl Pts',(-37.0954833955417,-50.7141678268703,
2.79286913083843));
#249032=CARTESIAN_POINT('Ctrl Pts',(-37.0242869695748,-50.6617655220312,
2.74900763297875));
#249033=CARTESIAN_POINT('Ctrl Pts',(-37.1386811500604,-50.8012099538927,
2.63954450640359));
#249034=CARTESIAN_POINT('Ctrl Pts',(-37.0803097184697,-50.7999485296222,
2.69627684028798));
#249035=CARTESIAN_POINT('Ctrl Pts',(-37.0173098767917,-50.7562647493203,
2.68224356036455));
#249036=CARTESIAN_POINT('Ctrl Pts',(-37.087378701726,-50.8700180268815,
2.59908178706274));
#249037=CARTESIAN_POINT('Ctrl Pts',(-37.0460487315398,-50.8539379904884,
2.6587870432159));
#249038=CARTESIAN_POINT('Ctrl Pts',(-36.9939291606759,-50.8047860147162,
2.65878198860226));
#249039=CARTESIAN_POINT('Ctrl Pts',(-37.0158684358555,-50.9219998155901,
2.59908173515987));
#249040=CARTESIAN_POINT('Ctrl Pts',(-36.9939338721428,-50.8918248691002,
2.65878198860226));
#249041=CARTESIAN_POINT('Ctrl Pts',(-36.9525415975208,-50.8348823336487,
2.65878198860226));
#249042=CARTESIAN_POINT('Origin',(-37.0855865599598,-50.5037675878947,2.83404198860224));
#249043=CARTESIAN_POINT('Origin',(-34.6544814981908,-48.2379650606661,3.11913648167141));
#249044=CARTESIAN_POINT('Origin',(-34.5497679336937,-48.0938392037149,2.83404198860227));
#249045=CARTESIAN_POINT('Origin',(-36.980873139615,-50.3596419293362,3.11913648177507));
#249046=CARTESIAN_POINT('Origin',(-36.876159719195,-50.2155162706045,3.40423097483274));
#249047=CARTESIAN_POINT('Ctrl Pts',(-34.4869303039392,-48.0063682005188,
2.9013417351599));
#249048=CARTESIAN_POINT('Ctrl Pts',(-34.5894948283129,-47.9324532779039,
2.90103711553196));
#249049=CARTESIAN_POINT('Ctrl Pts',(-34.6525130919793,-48.0191904766737,
2.83404198860228));
#249050=CARTESIAN_POINT('Ctrl Pts',(-34.4602241019853,-47.9696093621193,
2.82862991747919));
#249051=CARTESIAN_POINT('Ctrl Pts',(-34.5595620694338,-47.917105603145,
2.85314045886478));
#249052=CARTESIAN_POINT('Ctrl Pts',(-34.6258053530815,-47.9824304277182,
2.79187960999922));
#249053=CARTESIAN_POINT('Ctrl Pts',(-34.4546775021463,-47.9167391807672,
2.75470625793305));
#249054=CARTESIAN_POINT('Ctrl Pts',(-34.5405955452481,-47.8838297385507,
2.79224250381847));
#249055=CARTESIAN_POINT('Ctrl Pts',(-34.6112444014586,-47.9361122396533,
2.74901809108231));
#249056=CARTESIAN_POINT('Ctrl Pts',(-34.4979061669206,-47.7968564492221,
2.63947868311651));
#249057=CARTESIAN_POINT('Ctrl Pts',(-34.5561175928638,-47.7983386612727,
2.69595066767887));
#249058=CARTESIAN_POINT('Ctrl Pts',(-34.618722703651,-47.8422046210391,
2.68220539436021));
#249059=CARTESIAN_POINT('Ctrl Pts',(-34.5493265808144,-47.7285944911487,
2.59908178585036));
#249060=CARTESIAN_POINT('Ctrl Pts',(-34.5905382782873,-47.7447672725785,
2.65877670944848));
#249061=CARTESIAN_POINT('Ctrl Pts',(-34.6424336528567,-47.7940753146422,
2.65878198860228));
#249062=CARTESIAN_POINT('Ctrl Pts',(-34.620500570363,-47.6769115920305,
2.59908173515989));
#249063=CARTESIAN_POINT('Ctrl Pts',(-34.642420023457,-47.7070975168465,
2.65878198860227));
#249064=CARTESIAN_POINT('Ctrl Pts',(-34.6837837831342,-47.7640607692764,
2.65878198860228));
#249065=CARTESIAN_POINT('Origin',(-34.6837837831342,-47.7640607692764,2.53178198860228));
#249066=CARTESIAN_POINT('Ctrl Pts',(-36.6229335645805,-49.8669803696027,
3.77003198860228));
#249067=CARTESIAN_POINT('Ctrl Pts',(-36.5200349009281,-49.9417406248211,
3.77003198860228));
#249068=CARTESIAN_POINT('Ctrl Pts',(-36.5201885207953,-49.9416290134545,
3.64284238727569));
#249069=CARTESIAN_POINT('Ctrl Pts',(-36.7506494346799,-50.0423873219319,
3.77003198860228));
#249070=CARTESIAN_POINT('Ctrl Pts',(-36.6476796282246,-50.1174293675627,
3.77025506105825));
#249071=CARTESIAN_POINT('Ctrl Pts',(-36.6221794864696,-50.0820075342381,
3.64284210641864));
#249072=CARTESIAN_POINT('Ctrl Pts',(-36.8722311236871,-50.2093732240182,
3.65553527987796));
#249073=CARTESIAN_POINT('Ctrl Pts',(-36.7691636147942,-50.2846385388097,
3.65585996532967));
#249074=CARTESIAN_POINT('Ctrl Pts',(-36.7192731293494,-50.215645468493,
3.55127902710114));
#249075=CARTESIAN_POINT('Ctrl Pts',(-36.9399086546482,-50.3023253561997,
3.47153072139036));
#249076=CARTESIAN_POINT('Ctrl Pts',(-36.8368401378447,-50.3777877242641,
3.47182327905152));
#249077=CARTESIAN_POINT('Ctrl Pts',(-36.7733199617894,-50.2900345513018,
3.40413028377955));
#249078=CARTESIAN_POINT('Origin',(-36.6229335645805,-49.8669803696027,3.64303198860228));
#249079=CARTESIAN_POINT('Origin',(3.77491158612227E-16,1.91529980036038E-13,
2.53178198860262));
#249080=CARTESIAN_POINT('Origin',(-34.7084426211227,-47.7461450747866,2.53178198860228));
#249081=CARTESIAN_POINT('Origin',(21.2404668433927,29.7751578089173,3.64303198860283));
#249082=CARTESIAN_POINT('Origin',(-36.3870656659267,-49.5422481179708,3.6429946600742));
#249083=CARTESIAN_POINT('Ctrl Pts',(-34.6451144164181,-47.6590285860937,
2.59908173515989));
#249084=CARTESIAN_POINT('Ctrl Pts',(-34.6670494534013,-47.6892031885514,
2.65878198860228));
#249085=CARTESIAN_POINT('Ctrl Pts',(-34.7084426211227,-47.7461450747866,
2.65878198860228));
#249086=CARTESIAN_POINT('Ctrl Pts',(-34.7160192182659,-47.6074854095243,
2.59908193199792));
#249087=CARTESIAN_POINT('Ctrl Pts',(-34.7187044685505,-47.651649279334,
2.65877685806575));
#249088=CARTESIAN_POINT('Ctrl Pts',(-34.7496251731986,-47.7161963245879,
2.65878198860228));
#249089=CARTESIAN_POINT('Ctrl Pts',(-34.7960378560834,-47.5796730526552,
2.63872492669777));
#249090=CARTESIAN_POINT('Ctrl Pts',(-34.7797813814944,-47.6353534770325,
2.69532212015245));
#249091=CARTESIAN_POINT('Ctrl Pts',(-34.8021505789967,-47.7083584310193,
2.68176836726607));
#249092=CARTESIAN_POINT('Ctrl Pts',(-34.9243313177589,-47.5752965616147,
2.75442176402202));
#249093=CARTESIAN_POINT('Ctrl Pts',(-34.866569357182,-47.6468329724886,
2.79203179920103));
#249094=CARTESIAN_POINT('Ctrl Pts',(-34.8943788354693,-47.7301838844736,
2.74885310748134));
#249095=CARTESIAN_POINT('Ctrl Pts',(-34.9730260802976,-47.5970608435769,
2.82866089558375));
#249096=CARTESIAN_POINT('Ctrl Pts',(-34.8923863483133,-47.6753141056557,
2.85316563119084));
#249097=CARTESIAN_POINT('Ctrl Pts',(-34.9340521716866,-47.7584998599248,
2.79189751796537));
#249098=CARTESIAN_POINT('Ctrl Pts',(-34.9997217530256,-47.6338034047601,
2.9013417351599));
#249099=CARTESIAN_POINT('Ctrl Pts',(-34.8977303031698,-47.7085070967804,
2.90103711553195));
#249100=CARTESIAN_POINT('Ctrl Pts',(-34.9607485668361,-47.7952442955503,
2.83404198860228));
#249101=CARTESIAN_POINT('Origin',(-35.0634937251217,-47.7205955685092,2.83404198860228));
#249102=CARTESIAN_POINT('Origin',(-36.3610285393798,-49.5064990280447,3.56647653971786));
#249103=CARTESIAN_POINT('Origin',(-36.3129251734939,-49.4402904249167,3.42473028058449));
#249104=CARTESIAN_POINT('Origin',(-35.1682072895631,-47.8647214254838,3.11913648168009));
#249105=CARTESIAN_POINT('Origin',(-35.2729208539811,-48.0088472823273,3.40423097483276));
#249106=CARTESIAN_POINT('Ctrl Pts',(-36.1189794796879,-49.1733470784089,
3.36123028058446));
#249107=CARTESIAN_POINT('Ctrl Pts',(-36.0162343214022,-49.24799580545,3.36123028058446));
#249108=CARTESIAN_POINT('Ctrl Pts',(-36.0162343214022,-49.24799580545,3.23423028058446));
#249109=CARTESIAN_POINT('Ctrl Pts',(-36.1716968449929,-49.2463047380079,
3.36123028058446));
#249110=CARTESIAN_POINT('Ctrl Pts',(-36.0690914679796,-49.3207474263659,
3.36099641108385));
#249111=CARTESIAN_POINT('Ctrl Pts',(-36.0955935972142,-49.3572244778993,
3.23423043688384));
#249112=CARTESIAN_POINT('Ctrl Pts',(-36.2215465627843,-49.3152906263895,
3.41054258905249));
#249113=CARTESIAN_POINT('Ctrl Pts',(-36.1193211766459,-49.389882689244,
3.41008815826051));
#249114=CARTESIAN_POINT('Ctrl Pts',(-36.1706334382063,-49.4605079583558,
3.30819867304284));
#249115=CARTESIAN_POINT('Ctrl Pts',(-36.2478178023246,-49.3516463037386,
3.48823028058448));
#249116=CARTESIAN_POINT('Ctrl Pts',(-36.1458216659121,-49.4263574835552,
3.48794691941564));
#249117=CARTESIAN_POINT('Ctrl Pts',(-36.2101800152082,-49.5149391519578,
3.42473028058449));
#249118=CARTESIAN_POINT('Origin',(-36.1189794796879,-49.1733470784089,3.23423028058446));
#249119=CARTESIAN_POINT('Ctrl Pts',(-35.2091516650524,-47.9220530736688,
3.47153072139038));
#249120=CARTESIAN_POINT('Ctrl Pts',(-35.1070032771115,-47.9968680956253,
3.47122746285042));
#249121=CARTESIAN_POINT('Ctrl Pts',(-35.1702703521465,-48.0836260518494,
3.40413046676746));
#249122=CARTESIAN_POINT('Ctrl Pts',(-35.2768360036062,-48.0150025575606,
3.65553813457951));
#249123=CARTESIAN_POINT('Ctrl Pts',(-35.1744910995522,-48.0897575808483,
3.65520336072128));
#249124=CARTESIAN_POINT('Ctrl Pts',(-35.2243181613713,-48.1580164790724,
3.55128134519897));
#249125=CARTESIAN_POINT('Ctrl Pts',(-35.3984277477544,-48.1819833392239,
3.77003198860228));
#249126=CARTESIAN_POINT('Ctrl Pts',(-35.295826999928,-48.256762968645,3.76980209314088));
#249127=CARTESIAN_POINT('Ctrl Pts',(-35.3214126203088,-48.2916555365112,
3.64284195387367));
#249128=CARTESIAN_POINT('Ctrl Pts',(-35.5261472678861,-48.357383540212,
3.77003198860229));
#249129=CARTESIAN_POINT('Ctrl Pts',(-35.4232482045978,-48.4321440857829,
3.77003198860229));
#249130=CARTESIAN_POINT('Ctrl Pts',(-35.4234022246974,-48.4320321836304,
3.64284189403754));
#249131=CARTESIAN_POINT('Origin',(-35.5261472678861,-48.357383540212,3.64303198860229));
#249132=CARTESIAN_POINT('Origin',(20.7197400704237,29.0584388930976,3.23423028058502));
#249133=CARTESIAN_POINT('Origin',(-36.0301015792672,-49.0510171431405,3.23423028058446));
#249134=CARTESIAN_POINT('Origin',(20.6381965522785,28.9462038689909,3.64303198860283));
#249135=CARTESIAN_POINT('Origin',(-35.7621028045849,-48.6820620414858,3.64299171721696));
#249136=CARTESIAN_POINT('Ctrl Pts',(-35.90126936289,-48.8727133447945,3.48823028058447));
#249137=CARTESIAN_POINT('Ctrl Pts',(-35.7983524848931,-48.9481071848798,
3.48852004212224));
#249138=CARTESIAN_POINT('Ctrl Pts',(-35.7334106856002,-48.8587224664502,
3.42473028058446));
#249139=CARTESIAN_POINT('Ctrl Pts',(-35.9276271141657,-48.9091935744924,
3.41028005848374));
#249140=CARTESIAN_POINT('Ctrl Pts',(-35.8246659689643,-48.9843245886148,
3.41074404220222));
#249141=CARTESIAN_POINT('Ctrl Pts',(-35.7730909105047,-48.913337610609,
3.30780486243807));
#249142=CARTESIAN_POINT('Ctrl Pts',(-35.9775622448362,-48.9783048775121,
3.36123028058446));
#249143=CARTESIAN_POINT('Ctrl Pts',(-35.874576953785,-49.053021165758,3.36146460586494));
#249144=CARTESIAN_POINT('Ctrl Pts',(-35.8482644497263,-49.0168051108914,
3.23423045308429));
#249145=CARTESIAN_POINT('Ctrl Pts',(-36.0301015792672,-49.0510171431405,
3.36123028058446));
#249146=CARTESIAN_POINT('Ctrl Pts',(-35.9273564209816,-49.1256658701816,
3.36123028058446));
#249147=CARTESIAN_POINT('Ctrl Pts',(-35.9273564209816,-49.1256658701816,
3.23423028058446));
#249148=CARTESIAN_POINT('Origin',(-35.8361558438858,-48.784073739409,3.42473028058446));
#249149=CARTESIAN_POINT('Origin',(-35.7883393569603,-48.7182599907927,3.56563113524784));
#249150=CARTESIAN_POINT('Origin',(-30.4370746247564,-53.3535596832574,3.56647653909417));
#249151=CARTESIAN_POINT('Origin',(-30.4591427892363,-53.3918862459817,3.64299466007604));
#249152=CARTESIAN_POINT('Origin',(-30.3961554568832,-53.2826856060847,3.42473028058446));
#249153=CARTESIAN_POINT('Ctrl Pts',(-30.3416565762231,-53.1871522506176,
3.48823028058445));
#249154=CARTESIAN_POINT('Ctrl Pts',(-30.4513942013108,-53.1243619179796,
3.48794691941561));
#249155=CARTESIAN_POINT('Ctrl Pts',(-30.5061406831638,-53.2191856060847,
3.42473028058447));
#249156=CARTESIAN_POINT('Ctrl Pts',(-30.3190533624379,-53.1482340195357,
3.41028005925049));
#249157=CARTESIAN_POINT('Ctrl Pts',(-30.4287753876662,-53.0851849835423,
3.40982512230914));
#249158=CARTESIAN_POINT('Ctrl Pts',(-30.4723866803434,-53.1607219582409,
3.30780486372757));
#249159=CARTESIAN_POINT('Ctrl Pts',(-30.2762311741516,-53.0745038491597,
3.36123028058444));
#249160=CARTESIAN_POINT('Ctrl Pts',(-30.385972048483,-53.0110474253425,
3.36099721048402));
#249161=CARTESIAN_POINT('Ctrl Pts',(-30.4084402641646,-53.0499635164572,
3.23423045308424));
#249162=CARTESIAN_POINT('Ctrl Pts',(-30.2311753956707,-52.9969317578288,
3.36123028058444));
#249163=CARTESIAN_POINT('Ctrl Pts',(-30.3411606219514,-52.9334317578288,
3.36123028058444));
#249164=CARTESIAN_POINT('Ctrl Pts',(-30.3411606219514,-52.9334317578288,
3.23423028058444));
#249165=CARTESIAN_POINT('Origin',(-30.2311753956707,-52.9969317578288,3.23423028058444));
#249166=CARTESIAN_POINT('Origin',(0.274963065701566,-0.158749999999814,
3.64303198860263));
#249167=CARTESIAN_POINT('Origin',(-30.659864345357,-53.7394427993287,3.64303198860224));
#249168=CARTESIAN_POINT('Origin',(0.274963065701566,-0.158749999999811,
3.23423028058481));
#249169=CARTESIAN_POINT('Origin',(-30.1555713378333,-52.865981688396,3.23423028058444));
#249170=CARTESIAN_POINT('Ctrl Pts',(-30.9286463962973,-54.2060847114743,
3.47153072139033));
#249171=CARTESIAN_POINT('Ctrl Pts',(-31.0395064328255,-54.1426202518669,
3.47182327902624));
#249172=CARTESIAN_POINT('Ctrl Pts',(-30.9851759176833,-54.0488992551382,
3.40413028958997));
#249173=CARTESIAN_POINT('Ctrl Pts',(-30.8712564593353,-54.1064496608376,
3.65553807120916));
#249174=CARTESIAN_POINT('Ctrl Pts',(-30.981936066786,-54.0429059732603,
3.65586275496826));
#249175=CARTESIAN_POINT('Ctrl Pts',(-30.939200237769,-53.9692670413548,
3.55128126837159));
#249176=CARTESIAN_POINT('Ctrl Pts',(-30.7681581606549,-53.9274585619019,
3.77003198860224));
#249177=CARTESIAN_POINT('Ctrl Pts',(-30.8785940576193,-53.8639133132318,
3.77025505748453));
#249178=CARTESIAN_POINT('Ctrl Pts',(-30.856606798079,-53.8262110069728,
3.64284211731175));
#249179=CARTESIAN_POINT('Ctrl Pts',(-30.659864345357,-53.7394427993288,
3.77003198860225));
#249180=CARTESIAN_POINT('Ctrl Pts',(-30.7700138844655,-53.6758479332734,
3.77003198860225));
#249181=CARTESIAN_POINT('Ctrl Pts',(-30.769849449083,-53.6759428700857,
3.64284239821677));
#249182=CARTESIAN_POINT('Origin',(-30.8752713784757,-54.112538724998,3.40423097483272));
#249183=CARTESIAN_POINT('Ctrl Pts',(-30.1555713378333,-52.865981688396,
3.36123028058444));
#249184=CARTESIAN_POINT('Ctrl Pts',(-30.2655565641139,-52.802481688396,
3.36123028058444));
#249185=CARTESIAN_POINT('Ctrl Pts',(-30.2655565641139,-52.802481688396,
3.23423028058444));
#249186=CARTESIAN_POINT('Ctrl Pts',(-30.1103627734743,-52.7881477055076,
3.36123028058443));
#249187=CARTESIAN_POINT('Ctrl Pts',(-30.2205080277004,-52.7244553345187,
3.36146538610102));
#249188=CARTESIAN_POINT('Ctrl Pts',(-30.1980495259463,-52.6855560684212,
3.23423043688476));
#249189=CARTESIAN_POINT('Ctrl Pts',(-30.067613047258,-52.7145506960115,
3.41054258693063));
#249190=CARTESIAN_POINT('Ctrl Pts',(-30.1781274387062,-52.6510500011304,
3.4110060885975));
#249191=CARTESIAN_POINT('Ctrl Pts',(-30.1342168083493,-52.5749945583579,
3.30819866970748));
#249192=CARTESIAN_POINT('Ctrl Pts',(-30.0450834959832,-52.6757649139397,
3.48823028058443));
#249193=CARTESIAN_POINT('Ctrl Pts',(-30.1558192615997,-52.6124111049557,
3.48852004212222));
#249194=CARTESIAN_POINT('Ctrl Pts',(-30.1005764675353,-52.5167277788842,
3.42473028058443));
#249195=CARTESIAN_POINT('Origin',(-29.9905912412547,-52.5802277788842,3.42473028058442));
#249196=CARTESIAN_POINT('Origin',(-30.9643459342445,-54.266820381201,3.1191364817843));
#249197=CARTESIAN_POINT('Origin',(-31.0534204898629,-54.4211020372439,2.83404198860223));
#249198=CARTESIAN_POINT('Origin',(-29.9499161072439,-52.5097763801598,3.56563113460837));
#249199=CARTESIAN_POINT('Origin',(-29.927519002606,-52.4710850656384,3.64299171721757));
#249200=CARTESIAN_POINT('Ctrl Pts',(-31.4638515574735,-54.527521733972,
2.59908173515985));
#249201=CARTESIAN_POINT('Ctrl Pts',(-31.4452069629848,-54.4952102564866,
2.65878198860223));
#249202=CARTESIAN_POINT('Ctrl Pts',(-31.4100231232056,-54.4342359163064,
2.65878198860223));
#249203=CARTESIAN_POINT('Ctrl Pts',(-31.387530647168,-54.5715608148715,
2.59908193475496));
#249204=CARTESIAN_POINT('Ctrl Pts',(-31.3896121658904,-54.5272862282526,
2.65878715325321));
#249205=CARTESIAN_POINT('Ctrl Pts',(-31.365841113034,-54.4597196360206,
2.65878198860223));
#249206=CARTESIAN_POINT('Ctrl Pts',(-31.3046029601553,-54.5905300051367,
2.63878778849819));
#249207=CARTESIAN_POINT('Ctrl Pts',(-31.3268524737459,-54.536796115312,
2.69564460180095));
#249208=CARTESIAN_POINT('Ctrl Pts',(-31.3125672934291,-54.4615686025426,
2.68180481624847));
#249209=CARTESIAN_POINT('Ctrl Pts',(-31.1759014746037,-54.5809273110394,
2.7544323887862));
#249210=CARTESIAN_POINT('Ctrl Pts',(-31.2415992967173,-54.5158579940063,
2.79268340777024));
#249211=CARTESIAN_POINT('Ctrl Pts',(-31.2227682191853,-54.4295063924925,
2.74885926835569));
#249212=CARTESIAN_POINT('Ctrl Pts',(-31.129536412388,-54.5540292360083,
2.82856655361619));
#249213=CARTESIAN_POINT('Ctrl Pts',(-31.219103345881,-54.4847364330974,
2.85384197230905));
#249214=CARTESIAN_POINT('Ctrl Pts',(-31.1861426211013,-54.3969835118377,
2.79184624278558));
#249215=CARTESIAN_POINT('Ctrl Pts',(-31.106798218553,-54.5146464769139,
2.90134173515985));
#249216=CARTESIAN_POINT('Ctrl Pts',(-31.217488486086,-54.4512761425984,
2.90163218716352));
#249217=CARTESIAN_POINT('Ctrl Pts',(-31.1634057161435,-54.3576020372439,
2.83404198860223));
#249218=CARTESIAN_POINT('Origin',(-31.4100231232056,-54.4342359163064,2.53178198860222));
#249219=CARTESIAN_POINT('Origin',(0.274963065701566,-0.158749999999814,
3.64303198860263));
#249220=CARTESIAN_POINT('Origin',(-29.7268821954845,-52.1234703131947,3.64303198860225));
#249221=CARTESIAN_POINT('Origin',(5.22371297615222E-17,1.91720233321799E-13,
2.53178198860262));
#249222=CARTESIAN_POINT('Origin',(-31.436419577513,-54.4189959163064,2.53178198860223));
#249223=CARTESIAN_POINT('Ctrl Pts',(-29.7268821954845,-52.1234703131947,
3.77003198860226));
#249224=CARTESIAN_POINT('Ctrl Pts',(-29.8370321846009,-52.0598751873271,
3.77003198860226));
#249225=CARTESIAN_POINT('Ctrl Pts',(-29.8368672985388,-52.0599703843395,
3.64284187936975));
#249226=CARTESIAN_POINT('Ctrl Pts',(-29.6185926664433,-51.935448118016,
3.77003198860226));
#249227=CARTESIAN_POINT('Ctrl Pts',(-29.7286387544941,-51.8721332875992,
3.76980208963075));
#249228=CARTESIAN_POINT('Ctrl Pts',(-29.7501084152009,-51.9096995898763,
3.64284193928295));
#249229=CARTESIAN_POINT('Ctrl Pts',(-29.5155047636237,-51.7564527430624,
3.65553535416548));
#249230=CARTESIAN_POINT('Ctrl Pts',(-29.6254243098809,-51.693361622663,
3.65520057834344));
#249231=CARTESIAN_POINT('Ctrl Pts',(-29.667515590115,-51.7666446199922,
3.55127910964187));
#249232=CARTESIAN_POINT('Ctrl Pts',(-29.4581217525669,-51.6568155675428,
3.47153072139035));
#249233=CARTESIAN_POINT('Ctrl Pts',(-29.568016181109,-51.5939283753694,
3.47122746281545));
#249234=CARTESIAN_POINT('Ctrl Pts',(-29.6215404737378,-51.6870133822664,
3.40413045901218));
#249235=CARTESIAN_POINT('Origin',(-29.5114749418,-51.7503740054944,3.40423097483273));
#249236=CARTESIAN_POINT('Ctrl Pts',(-31.6576696180579,-54.1966007261208,
2.90134173515985));
#249237=CARTESIAN_POINT('Ctrl Pts',(-31.5474441649278,-54.2607761425984,
2.90163218716353));
#249238=CARTESIAN_POINT('Ctrl Pts',(-31.4933613949854,-54.1671020372439,
2.83404198860223));
#249239=CARTESIAN_POINT('Ctrl Pts',(-31.6804173065999,-54.2360018544267,
2.82853349835301));
#249240=CARTESIAN_POINT('Ctrl Pts',(-31.5756301844116,-54.2789150989582,
2.85381483162341));
#249241=CARTESIAN_POINT('Ctrl Pts',(-31.5161086602377,-54.2065014563942,
2.7918270159426));
#249242=CARTESIAN_POINT('Ctrl Pts',(-31.680432806462,-54.2894509908544,
2.75468822073627));
#249243=CARTESIAN_POINT('Ctrl Pts',(-31.591196427296,-54.3138841827109,
2.79286913083811));
#249244=CARTESIAN_POINT('Ctrl Pts',(-31.5258675551964,-54.254326890184,
2.7490076329788));
#249245=CARTESIAN_POINT('Ctrl Pts',(-31.6250591602186,-54.4049648787501,
2.63954450640331));
#249246=CARTESIAN_POINT('Ctrl Pts',(-31.5671393481776,-54.3976088886508,
2.69627684028808));
#249247=CARTESIAN_POINT('Ctrl Pts',(-31.5090508246488,-54.3475791360313,
2.68224356036447));
#249248=CARTESIAN_POINT('Ctrl Pts',(-31.5668453499334,-54.4680334478294,
2.59908178706285));
#249249=CARTESIAN_POINT('Ctrl Pts',(-31.5274226111427,-54.4477213412889,
2.6587870432146));
#249250=CARTESIAN_POINT('Ctrl Pts',(-31.4807263372346,-54.3933906465327,
2.65878198860223));
#249251=CARTESIAN_POINT('Ctrl Pts',(-31.4902932482903,-54.5122556166612,
2.59908173515985));
#249252=CARTESIAN_POINT('Ctrl Pts',(-31.4716329851984,-54.479953185448,
2.65878198860223));
#249253=CARTESIAN_POINT('Ctrl Pts',(-31.436419577513,-54.4189959163064,
2.65878198860223));
#249254=CARTESIAN_POINT('Origin',(-31.603346621266,-54.1036020372439,2.83404198860223));
#249255=CARTESIAN_POINT('Origin',(-29.4224002636363,-51.5960921371862,3.11913648167068));
#249256=CARTESIAN_POINT('Origin',(-29.333325585345,-51.4418102687786,2.83404198860225));
#249257=CARTESIAN_POINT('Origin',(-31.5142720655983,-53.9493203812114,3.11913648177452));
#249258=CARTESIAN_POINT('Origin',(-31.4251975098788,-53.795038724998,3.40423097483272));
#249259=CARTESIAN_POINT('Ctrl Pts',(-29.2799753962458,-51.3482501200166,
2.90134173515987));
#249260=CARTESIAN_POINT('Ctrl Pts',(-29.3897042746969,-51.2854610232002,
2.90103711553193));
#249261=CARTESIAN_POINT('Ctrl Pts',(-29.4433108116256,-51.3783102687786,
2.83404198860225));
#249262=CARTESIAN_POINT('Ctrl Pts',(-29.2572578385499,-51.3089010921301,
2.82862991747923));
#249263=CARTESIAN_POINT('Ctrl Pts',(-29.3615397594608,-51.2670685993225,
2.85314045886427));
#249264=CARTESIAN_POINT('Ctrl Pts',(-29.4205918519427,-51.3389598763126,
2.79187960999989));
#249265=CARTESIAN_POINT('Ctrl Pts',(-29.2572680623745,-51.2557407616057,
2.7547062579329));
#249266=CARTESIAN_POINT('Ctrl Pts',(-29.3461554108687,-51.2319924817692,
2.7922425038188));
#249267=CARTESIAN_POINT('Ctrl Pts',(-29.4109522357565,-51.2913733902318,
2.74901809108211));
#249268=CARTESIAN_POINT('Ctrl Pts',(-29.3127910737009,-51.1410333861057,
2.63947868311662));
#249269=CARTESIAN_POINT('Ctrl Pts',(-29.3705286780137,-51.1485922293422,
2.69595066767867));
#249270=CARTESIAN_POINT('Ctrl Pts',(-29.4282055900896,-51.1987619028143,
2.68220539436036));
#249271=CARTESIAN_POINT('Ctrl Pts',(-29.3710651187642,-51.078520271026,
2.59908178585069));
#249272=CARTESIAN_POINT('Ctrl Pts',(-29.4103605382565,-51.0989122516714,
2.65877670944823));
#249273=CARTESIAN_POINT('Ctrl Pts',(-29.4568175306708,-51.1533747228769,
2.65878198860225));
#249274=CARTESIAN_POINT('Ctrl Pts',(-29.4472515437731,-51.0345602039887,
2.59908173515987));
#249275=CARTESIAN_POINT('Ctrl Pts',(-29.4658956314762,-51.0668719738978,
2.65878198860225));
#249276=CARTESIAN_POINT('Ctrl Pts',(-29.5010785149107,-51.1278468659048,
2.65878198860225));
#249277=CARTESIAN_POINT('Origin',(-29.5010785149107,-51.1278468659048,2.53178198860225));
#249278=CARTESIAN_POINT('Ctrl Pts',(-31.2097904767601,-53.4219427993288,
3.77003198860225));
#249279=CARTESIAN_POINT('Ctrl Pts',(-31.099640928162,-53.485537670863,3.77003198860225));
#249280=CARTESIAN_POINT('Ctrl Pts',(-31.0998053730483,-53.4854427285636,
3.64284238727554));
#249281=CARTESIAN_POINT('Ctrl Pts',(-31.318471686786,-53.6097387976566,
3.77003198860225));
#249282=CARTESIAN_POINT('Ctrl Pts',(-31.2082219299925,-53.6736064794804,
3.77025506105671));
#249283=CARTESIAN_POINT('Ctrl Pts',(-31.1865640704875,-53.6357132000308,
3.64284210641846));
#249284=CARTESIAN_POINT('Ctrl Pts',(-31.4219325588451,-53.7885186806138,
3.65553527987794));
#249285=CARTESIAN_POINT('Ctrl Pts',(-31.3115622968593,-53.8525981958153,
3.65585996533033));
#249286=CARTESIAN_POINT('Ctrl Pts',(-31.2691568563313,-53.7787681009838,
3.55127902710127));
#249287=CARTESIAN_POINT('Ctrl Pts',(-31.4795232016785,-53.8880358395971,
3.47153072139033));
#249288=CARTESIAN_POINT('Ctrl Pts',(-31.3691313396259,-53.9523112232408,
3.47182327905149));
#249289=CARTESIAN_POINT('Ctrl Pts',(-31.3151318380579,-53.8583991049521,
3.40413028377945));
#249290=CARTESIAN_POINT('Origin',(-31.2097904767601,-53.4219427993288,3.64303198860225));
#249291=CARTESIAN_POINT('Origin',(3.82640399828021E-16,1.91526636079694E-13,
2.53178198860262));
#249292=CARTESIAN_POINT('Origin',(-29.527474969218,-51.1126068659048,2.53178198860225));
#249293=CARTESIAN_POINT('Origin',(15.2806508669887,27.1018636743466,3.64303198860282));
#249294=CARTESIAN_POINT('Origin',(-31.0091584503713,-53.0743345559678,3.64299466007412));
#249295=CARTESIAN_POINT('Ctrl Pts',(-29.4735998357333,-51.0193480105328,
2.59908173515987));
#249296=CARTESIAN_POINT('Ctrl Pts',(-29.4922606054642,-51.0516501490687,
2.65878198860225));
#249297=CARTESIAN_POINT('Ctrl Pts',(-29.527474969218,-51.1126068659048,
2.65878198860225));
#249298=CARTESIAN_POINT('Ctrl Pts',(-29.5495039426967,-50.9754987628538,
2.59908193199895));
#249299=CARTESIAN_POINT('Ctrl Pts',(-29.5475581014577,-51.0197013834522,
2.65877685806689));
#249300=CARTESIAN_POINT('Ctrl Pts',(-29.5715624158009,-51.0871269269774,
2.65878198860225));
#249301=CARTESIAN_POINT('Ctrl Pts',(-29.6319914129668,-50.9562029902289,
2.63872492669762));
#249302=CARTESIAN_POINT('Ctrl Pts',(-29.6100038038521,-51.0098791271087,
2.69532212015239));
#249303=CARTESIAN_POINT('Ctrl Pts',(-29.6246193648992,-51.0848223701587,
2.68176836726606));
#249304=CARTESIAN_POINT('Ctrl Pts',(-29.7600395375186,-50.9652607924606,
2.75442176402213));
#249305=CARTESIAN_POINT('Ctrl Pts',(-29.6951164119093,-51.0303675504162,
2.792031799201));
#249306=CARTESIAN_POINT('Ctrl Pts',(-29.7140610042227,-51.1161687394135,
2.74885310748131));
#249307=CARTESIAN_POINT('Ctrl Pts',(-29.8061925581062,-50.9919958361057,
2.82866089558362));
#249308=CARTESIAN_POINT('Ctrl Pts',(-29.7178148857801,-51.0613912713637,
2.85316563119169));
#249309=CARTESIAN_POINT('Ctrl Pts',(-29.7505571803534,-51.1484765898561,
2.7918975179659));
#249310=CARTESIAN_POINT('Ctrl Pts',(-29.8289013456881,-51.031327575341,
2.90134173515987));
#249311=CARTESIAN_POINT('Ctrl Pts',(-29.7196599535388,-51.0949610232002,
2.90103711553193));
#249312=CARTESIAN_POINT('Ctrl Pts',(-29.7732664904675,-51.1878102687786,
2.83404198860225));
#249313=CARTESIAN_POINT('Origin',(-29.8832517167481,-51.1243102687786,2.83404198860226));
#249314=CARTESIAN_POINT('Origin',(-30.9870007553597,-53.0360596824716,3.56647653971798));
#249315=CARTESIAN_POINT('Origin',(-30.9460815882863,-52.9651856060847,3.42473028058447));
#249316=CARTESIAN_POINT('Origin',(-29.9723263949767,-51.2785921372,3.1191364816828));
#249317=CARTESIAN_POINT('Origin',(-30.0614010732032,-51.4328740054944,3.40423097483274));
#249318=CARTESIAN_POINT('Ctrl Pts',(-30.7811015270739,-52.6794317578288,
3.36123028058444));
#249319=CARTESIAN_POINT('Ctrl Pts',(-30.6711163007932,-52.7429317578288,
3.36123028058444));
#249320=CARTESIAN_POINT('Ctrl Pts',(-30.6711163007932,-52.7429317578288,
3.23423028058444));
#249321=CARTESIAN_POINT('Ctrl Pts',(-30.8259039490958,-52.7575002129169,
3.36123028058444));
#249322=CARTESIAN_POINT('Ctrl Pts',(-30.7160792752587,-52.820809914056,
3.36099641108435));
#249323=CARTESIAN_POINT('Ctrl Pts',(-30.738623332913,-52.8598573673285,
3.2342304368839));
#249324=CARTESIAN_POINT('Ctrl Pts',(-30.8682695960177,-52.8313189037788,
3.41054258905248));
#249325=CARTESIAN_POINT('Ctrl Pts',(-30.7588072175379,-52.8948168809893,
3.41008815825996));
#249326=CARTESIAN_POINT('Ctrl Pts',(-30.8024560343113,-52.9704188493347,
3.3081986730428));
#249327=CARTESIAN_POINT('Ctrl Pts',(-30.8905967158731,-52.8702215132217,
3.48823028058445));
#249328=CARTESIAN_POINT('Ctrl Pts',(-30.7813498801527,-52.9338619179796,
3.48794691941561));
#249329=CARTESIAN_POINT('Ctrl Pts',(-30.8360963620057,-53.0286856060847,
3.42473028058446));
#249330=CARTESIAN_POINT('Origin',(-30.7811015270739,-52.6794317578288,3.23423028058444));
#249331=CARTESIAN_POINT('Ctrl Pts',(-30.0070536838153,-51.3398895692698,
3.47153072139036));
#249332=CARTESIAN_POINT('Ctrl Pts',(-29.8976445761569,-51.4036173326914,
3.4712274628504));
#249333=CARTESIAN_POINT('Ctrl Pts',(-29.951496391695,-51.4965132298825,
3.40413046676735));
#249334=CARTESIAN_POINT('Ctrl Pts',(-30.0646513737701,-51.4394048060584,
3.65553813457952));
#249335=CARTESIAN_POINT('Ctrl Pts',(-29.9550530981038,-51.5030523579586,
3.65520336072241));
#249336=CARTESIAN_POINT('Ctrl Pts',(-29.9974722043253,-51.5761456730011,
3.55128134519924));
#249337=CARTESIAN_POINT('Ctrl Pts',(-30.1681227811166,-51.6181806476914,
3.77003198860227));
#249338=CARTESIAN_POINT('Ctrl Pts',(-30.058267491178,-51.6818259279789,
3.7698020931406));
#249339=CARTESIAN_POINT('Ctrl Pts',(-30.0800656843527,-51.7192017762878,
3.64284195387371));
#249340=CARTESIAN_POINT('Ctrl Pts',(-30.2768083268876,-51.8059703131947,
3.77003198860226));
#249341=CARTESIAN_POINT('Ctrl Pts',(-30.1666583504928,-51.8695654317175,
3.77003198860226));
#249342=CARTESIAN_POINT('Ctrl Pts',(-30.1668232238143,-51.8694702420609,
3.64284189403736));
#249343=CARTESIAN_POINT('Origin',(-30.2768083268876,-51.8059703131947,3.64303198860226));
#249344=CARTESIAN_POINT('Origin',(14.903849434298,26.4492244485615,3.234230280585));
#249345=CARTESIAN_POINT('Origin',(-30.7054974692364,-52.548481688396,3.23423028058444));
#249346=CARTESIAN_POINT('Origin',(14.8448439902557,26.347024021557,3.64303198860281));
#249347=CARTESIAN_POINT('Origin',(-30.4775331296734,-52.1535342613179,3.64299171721737));
#249348=CARTESIAN_POINT('Ctrl Pts',(-30.5960088312564,-52.3576880233163,
3.48823028058444));
#249349=CARTESIAN_POINT('Ctrl Pts',(-30.4857749404415,-52.4219111049557,
3.48852004212222));
#249350=CARTESIAN_POINT('Ctrl Pts',(-30.4305321463772,-52.3262277788842,
3.42473028058444));
#249351=CARTESIAN_POINT('Ctrl Pts',(-30.6184089696598,-52.3967235457368,
3.41028005848368));
#249352=CARTESIAN_POINT('Ctrl Pts',(-30.5081585269343,-52.4606806140151,
3.41074404220138));
#249353=CARTESIAN_POINT('Ctrl Pts',(-30.4642861617676,-52.3846914484999,
3.30780486243784));
#249354=CARTESIAN_POINT('Ctrl Pts',(-30.6608464521623,-52.4706758922782,
3.36123028058443));
#249355=CARTESIAN_POINT('Ctrl Pts',(-30.5506153465215,-52.5342179826684,
3.36146460586488));
#249356=CARTESIAN_POINT('Ctrl Pts',(-30.5282325936734,-52.4954499175236,
3.23423045308435));
#249357=CARTESIAN_POINT('Ctrl Pts',(-30.7054974692364,-52.548481688396,
3.36123028058444));
#249358=CARTESIAN_POINT('Ctrl Pts',(-30.5955122429558,-52.611981688396,
3.36123028058444));
#249359=CARTESIAN_POINT('Ctrl Pts',(-30.5955122429558,-52.611981688396,
3.23423028058444));
#249360=CARTESIAN_POINT('Origin',(-30.5405173726578,-52.2627277788842,3.42473028058445));
#249361=CARTESIAN_POINT('Origin',(-30.4998422394557,-52.1922763809715,3.56563113524769));
#249362=CARTESIAN_POINT('Origin',(-24.6933715417282,-56.2428239377255,3.5664765390945));
#249363=CARTESIAN_POINT('Origin',(-24.7113125977909,-56.2832472948495,3.6429946600762));
#249364=CARTESIAN_POINT('Origin',(-24.6600848917106,-56.1680608984278,3.42473028058445));
#249365=CARTESIAN_POINT('Ctrl Pts',(-24.6158705164589,-56.0673542004326,
3.48823028058444));
#249366=CARTESIAN_POINT('Ctrl Pts',(-24.731570364333,-56.0163785451198,
3.4879469194156));
#249367=CARTESIAN_POINT('Ctrl Pts',(-24.7761051648312,-56.1164053447572,
3.42473028058445));
#249368=CARTESIAN_POINT('Ctrl Pts',(-24.5974591883325,-56.0262864882906,
3.41028005925047));
#249369=CARTESIAN_POINT('Ctrl Pts',(-24.7131705636669,-55.9750519161889,
3.40982512230921));
#249370=CARTESIAN_POINT('Ctrl Pts',(-24.7486471852345,-56.0547337128459,
3.30780486372833));
#249371=CARTESIAN_POINT('Ctrl Pts',(-24.5625784858793,-55.9484840819673,
3.36123028058441));
#249372=CARTESIAN_POINT('Ctrl Pts',(-24.6783511906883,-55.896846324036,
3.36099721048678));
#249373=CARTESIAN_POINT('Ctrl Pts',(-24.6966284839307,-55.9378977967869,
3.23423045308457));
#249374=CARTESIAN_POINT('Ctrl Pts',(-24.5258780191666,-55.8666273273833,
3.36123028058441));
#249375=CARTESIAN_POINT('Ctrl Pts',(-24.6418982922872,-55.8149717737127,
3.36123028058442));
#249376=CARTESIAN_POINT('Ctrl Pts',(-24.6418982922872,-55.8149717737127,
3.23423028058442));
#249377=CARTESIAN_POINT('Origin',(-24.5258780191666,-55.8666273273833,3.23423028058441));
#249378=CARTESIAN_POINT('Origin',(0.290050682801532,-0.12913888417638,3.64303198860263));
#249379=CARTESIAN_POINT('Origin',(-24.8746050278048,-56.6498810128382,3.64303198860222));
#249380=CARTESIAN_POINT('Origin',(0.290050682801533,-0.129138884176377,
3.23423028058481));
#249381=CARTESIAN_POINT('Origin',(-24.4643761377912,-55.7284918401498,3.23423028058442));
#249382=CARTESIAN_POINT('Ctrl Pts',(-25.0931373005741,-57.1420619865022,
3.47153072139031));
#249383=CARTESIAN_POINT('Ctrl Pts',(-25.2100238766575,-57.0905332211011,
3.47182327902622));
#249384=CARTESIAN_POINT('Ctrl Pts',(-25.165787501526,-56.9916465525423,
3.40413028959));
#249385=CARTESIAN_POINT('Ctrl Pts',(-25.0464764504208,-57.0369738651809,
3.65553807120914));
#249386=CARTESIAN_POINT('Ctrl Pts',(-25.1631918674157,-56.9853474458577,
3.65586275496877));
#249387=CARTESIAN_POINT('Ctrl Pts',(-25.1283875141298,-56.9076448051882,
3.55128126837116));
#249388=CARTESIAN_POINT('Ctrl Pts',(-24.9626525995183,-56.8481865914866,
3.77003198860223));
#249389=CARTESIAN_POINT('Ctrl Pts',(-25.0791258042765,-56.7965331449336,
3.77025505748508));
#249390=CARTESIAN_POINT('Ctrl Pts',(-25.06119995738,-56.7567390814052,3.64284211731215));
#249391=CARTESIAN_POINT('Ctrl Pts',(-24.8746050278048,-56.6498810128382,
3.77003198860223));
#249392=CARTESIAN_POINT('Ctrl Pts',(-24.9907986298333,-56.5981482881658,
3.77003198860223));
#249393=CARTESIAN_POINT('Ctrl Pts',(-24.990625171646,-56.5982255167265,
3.64284239821683));
#249394=CARTESIAN_POINT('Origin',(-25.049832894896,-57.0434492461379,3.40423097483269));
#249395=CARTESIAN_POINT('Ctrl Pts',(-24.4643761377912,-55.7284918401498,
3.36123028058442));
#249396=CARTESIAN_POINT('Ctrl Pts',(-24.5803964109118,-55.6768362864792,
3.36123028058442));
#249397=CARTESIAN_POINT('Ctrl Pts',(-24.5803964109118,-55.6768362864792,
3.23423028058442));
#249398=CARTESIAN_POINT('Ctrl Pts',(-24.4275510972983,-55.646358658205,
3.36123028058442));
#249399=CARTESIAN_POINT('Ctrl Pts',(-24.5437506299586,-55.5945285148511,
3.36146538610141));
#249400=CARTESIAN_POINT('Ctrl Pts',(-24.5254812387364,-55.553494790328,
3.23423043688428));
#249401=CARTESIAN_POINT('Ctrl Pts',(-24.3927285408595,-55.5686962576408,
3.41054258693061));
#249402=CARTESIAN_POINT('Ctrl Pts',(-24.5092751529597,-55.5170953257151,
3.41100608859654));
#249403=CARTESIAN_POINT('Ctrl Pts',(-24.473555028186,-55.4368666119022,
3.3081986697068));
#249404=CARTESIAN_POINT('Ctrl Pts',(-24.3743766270209,-55.5277679687683,
3.48823028058443));
#249405=CARTESIAN_POINT('Ctrl Pts',(-24.4911280468221,-55.4763362579875,
3.48852004212221));
#249406=CARTESIAN_POINT('Ctrl Pts',(-24.4461895095984,-55.3754026508175,
3.42473028058443));
#249407=CARTESIAN_POINT('Origin',(-24.3301692364778,-55.4270582044881,3.42473028058442));
#249408=CARTESIAN_POINT('Origin',(-25.1222926664907,-57.2061965577157,3.11913648178284));
#249409=CARTESIAN_POINT('Origin',(-25.1947524379611,-57.3689438691196,2.83404198860221));
#249410=CARTESIAN_POINT('Origin',(-24.2970811015497,-55.3527410366453,3.56563113460771));
#249411=CARTESIAN_POINT('Origin',(-24.2788510342437,-55.3119205422645,3.64299171721722));
#249412=CARTESIAN_POINT('Ctrl Pts',(-25.5918112338789,-57.5176823163889,
2.59908173515983));
#249413=CARTESIAN_POINT('Ctrl Pts',(-25.5766462455171,-57.4835989537478,
2.65878198860221));
#249414=CARTESIAN_POINT('Ctrl Pts',(-25.5480287005713,-57.4192809246789,
2.65878198860221));
#249415=CARTESIAN_POINT('Ctrl Pts',(-25.5113050800554,-57.5535024391256,
2.5990819347554));
#249416=CARTESIAN_POINT('Ctrl Pts',(-25.5180031505012,-57.5096879712772,
2.6587871532528));
#249417=CARTESIAN_POINT('Ctrl Pts',(-25.5014249500136,-57.4400067642813,
2.65878198860221));
#249418=CARTESIAN_POINT('Ctrl Pts',(-25.4268488592811,-57.5636994104961,
2.6387877884984));
#249419=CARTESIAN_POINT('Ctrl Pts',(-25.4545932086367,-57.5125855880056,
2.69564460180084));
#249420=CARTESIAN_POINT('Ctrl Pts',(-25.4482497003378,-57.4362769714768,
2.68180481624847));
#249421=CARTESIAN_POINT('Ctrl Pts',(-25.2998561687911,-57.540696352457,
2.75443238878594));
#249422=CARTESIAN_POINT('Ctrl Pts',(-25.3719956870767,-57.4828507843371,
2.79268340777035));
#249423=CARTESIAN_POINT('Ctrl Pts',(-25.3622939683644,-57.395003842335,
2.74885926835564));
#249424=CARTESIAN_POINT('Ctrl Pts',(-25.2565567136853,-57.5090991591924,
2.82856655361635));
#249425=CARTESIAN_POINT('Ctrl Pts',(-25.3528760603488,-57.4495482434215,
2.85384197230768));
#249426=CARTESIAN_POINT('Ctrl Pts',(-25.3292685758742,-57.3588307079379,
2.79184624278448));
#249427=CARTESIAN_POINT('Ctrl Pts',(-25.2380597013425,-57.4675553545141,
2.90134173515982));
#249428=CARTESIAN_POINT('Ctrl Pts',(-25.354767599671,-57.4161024530844,
2.9016321871635));
#249429=CARTESIAN_POINT('Ctrl Pts',(-25.3107727110817,-57.317288315449,
2.83404198860221));
#249430=CARTESIAN_POINT('Origin',(-25.5480287005713,-57.4192809246789,2.5317819886022));
#249431=CARTESIAN_POINT('Origin',(0.290050682801532,-0.12913888417638,3.64303198860263));
#249432=CARTESIAN_POINT('Origin',(-24.1156489724272,-54.9452378026829,3.64303198860223));
#249433=CARTESIAN_POINT('Origin',(3.68589728140376E-17,1.9172806888413E-13,
2.53178198860262));
#249434=CARTESIAN_POINT('Origin',(-25.5758735661203,-57.406883591798,2.53178198860221));
#249435=CARTESIAN_POINT('Ctrl Pts',(-24.1156489724272,-54.9452378026829,
3.77003198860224));
#249436=CARTESIAN_POINT('Ctrl Pts',(-24.2318430491567,-54.89350486666,3.77003198860224));
#249437=CARTESIAN_POINT('Ctrl Pts',(-24.2316691155599,-54.8935823068866,
3.64284187936935));
#249438=CARTESIAN_POINT('Ctrl Pts',(-24.0276063358797,-54.7469262747035,
3.77003198860224));
#249439=CARTESIAN_POINT('Ctrl Pts',(-24.1436677818743,-54.6954612380258,
3.7698020896313));
#249440=CARTESIAN_POINT('Ctrl Pts',(-24.1610930816824,-54.7350659388095,
3.64284193928315));
#249441=CARTESIAN_POINT('Ctrl Pts',(-23.9437932708537,-54.5581358350793,
3.65553535416546));
#249442=CARTESIAN_POINT('Ctrl Pts',(-24.059705484196,-54.5068800556895,
3.65520057834371));
#249443=CARTESIAN_POINT('Ctrl Pts',(-24.093906024898,-54.5841613379333,
3.55127910964144));
#249444=CARTESIAN_POINT('Ctrl Pts',(-23.8971395307763,-54.4530463244693,
3.47153072139034));
#249445=CARTESIAN_POINT('Ctrl Pts',(-24.0130054476979,-54.4019907306516,
3.47122746281544));
#249446=CARTESIAN_POINT('Ctrl Pts',(-24.0565064959269,-54.5001606201976,
3.40413045901197));
#249447=CARTESIAN_POINT('Origin',(-23.9404209259116,-54.5516691663895,3.40423097483271));
#249448=CARTESIAN_POINT('Ctrl Pts',(-25.8191582032616,-57.2088336324699,
2.90134173515983));
#249449=CARTESIAN_POINT('Ctrl Pts',(-25.7028284190329,-57.2611357920725,
2.90163218716351));
#249450=CARTESIAN_POINT('Ctrl Pts',(-25.6588335304436,-57.1623216544371,
2.83404198860221));
#249451=CARTESIAN_POINT('Ctrl Pts',(-25.8376627381934,-57.250396698198,
2.82853349835328));
#249452=CARTESIAN_POINT('Ctrl Pts',(-25.7289639953181,-57.2821216226324,
2.85381483162255));
#249453=CARTESIAN_POINT('Ctrl Pts',(-25.6773378230589,-57.2038829761261,
2.7918270159416));
#249454=CARTESIAN_POINT('Ctrl Pts',(-25.8320911970514,-57.3035546548413,
2.75468822073581));
#249455=CARTESIAN_POINT('Ctrl Pts',(-25.7407897001103,-57.3185262575348,
2.7928691308381));
#249456=CARTESIAN_POINT('Ctrl Pts',(-25.6820441386713,-57.2524664994803,
2.74900763297875));
#249457=CARTESIAN_POINT('Ctrl Pts',(-25.7649464042477,-57.4126476234249,
2.63954450640372));
#249458=CARTESIAN_POINT('Ctrl Pts',(-25.708112793338,-57.3992776612634,
2.69627684028807));
#249459=CARTESIAN_POINT('Ctrl Pts',(-25.6555720179783,-57.3434500727657,
2.68224356036447));
#249460=CARTESIAN_POINT('Ctrl Pts',(-25.7004590347002,-57.469285696154,
2.59908178706275));
#249461=CARTESIAN_POINT('Ctrl Pts',(-25.66337545108,-57.4449640631546,2.65878704321414));
#249462=CARTESIAN_POINT('Ctrl Pts',(-25.6226140882778,-57.3860499078787,
2.65878198860221));
#249463=CARTESIAN_POINT('Ctrl Pts',(-25.6197038181293,-57.5052637377732,
2.59908173515983));
#249464=CARTESIAN_POINT('Ctrl Pts',(-25.6045223014057,-57.4711877340329,
2.65878198860221));
#249465=CARTESIAN_POINT('Ctrl Pts',(-25.5758735661203,-57.406883591798,
2.65878198860221));
#249466=CARTESIAN_POINT('Origin',(-25.7748538035642,-57.1106661007665,2.83404198860221));
#249467=CARTESIAN_POINT('Origin',(-23.8679610547591,-54.3889216310751,3.11913648167016));
#249468=CARTESIAN_POINT('Origin',(-23.7955011834904,-54.2261740956466,2.83404198860223));
#249469=CARTESIAN_POINT('Origin',(-25.7023940320488,-56.9479187893697,3.11913648177552));
#249470=CARTESIAN_POINT('Origin',(-25.629934260499,-56.7851714777848,3.4042309748327));
#249471=CARTESIAN_POINT('Ctrl Pts',(-23.7522229508823,-54.1275498658874,
2.90134173515985));
#249472=CARTESIAN_POINT('Ctrl Pts',(-23.8679139708563,-54.0765745253536,
2.90103711553191));
#249473=CARTESIAN_POINT('Ctrl Pts',(-23.911521456611,-54.174518541976,2.83404198860223));
#249474=CARTESIAN_POINT('Ctrl Pts',(-23.73374293576,-54.0860417646979,2.82862991747925));
#249475=CARTESIAN_POINT('Ctrl Pts',(-23.8418262755854,-54.0553388636017,
2.85314045886441));
#249476=CARTESIAN_POINT('Ctrl Pts',(-23.8930401898202,-54.1330089371356,
2.79187960999867));
#249477=CARTESIAN_POINT('Ctrl Pts',(-23.7393098712345,-54.0331737207068,
2.75470625793287));
#249478=CARTESIAN_POINT('Ctrl Pts',(-23.8301926567295,-54.0188467943739,
2.79224250381887));
#249479=CARTESIAN_POINT('Ctrl Pts',(-23.8884275227218,-54.0846755205371,
2.7490180910822));
#249480=CARTESIAN_POINT('Ctrl Pts',(-23.8065189073819,-53.9248984592617,
2.63947868311661));
#249481=CARTESIAN_POINT('Ctrl Pts',(-23.8631501047896,-53.9384511174159,
2.69595066767855));
#249482=CARTESIAN_POINT('Ctrl Pts',(-23.9152668978356,-53.9943748351526,
2.68220539436023));
#249483=CARTESIAN_POINT('Ctrl Pts',(-23.8710081209823,-53.8688190939459,
2.59908178585036));
#249484=CARTESIAN_POINT('Ctrl Pts',(-23.9079567336557,-53.8932068550021,
2.6587767094497));
#249485=CARTESIAN_POINT('Ctrl Pts',(-23.9484663513835,-53.9522270531161,
2.65878198860223));
#249486=CARTESIAN_POINT('Ctrl Pts',(-23.951372267036,-53.8330634946838,
2.59908173515985));
#249487=CARTESIAN_POINT('Ctrl Pts',(-23.9665367208219,-53.8671470951731,
2.65878198860223));
#249488=CARTESIAN_POINT('Ctrl Pts',(-23.9951532569802,-53.9314655730804,
2.65878198860223));
#249489=CARTESIAN_POINT('Origin',(-23.9951532569802,-53.9314655730804,2.53178198860223));
#249490=CARTESIAN_POINT('Ctrl Pts',(-25.4547063934078,-56.3916032444851,
3.77003198860223));
#249491=CARTESIAN_POINT('Ctrl Pts',(-25.3385127813687,-56.4433359736145,
3.77003198860223));
#249492=CARTESIAN_POINT('Ctrl Pts',(-25.3386862495815,-56.4432587405902,
3.64284238727522));
#249493=CARTESIAN_POINT('Ctrl Pts',(-25.5431622092807,-56.5897307565548,
3.77003198860223));
#249494=CARTESIAN_POINT('Ctrl Pts',(-25.4268404215552,-56.6417243268781,
3.77025506105786));
#249495=CARTESIAN_POINT('Ctrl Pts',(-25.4092621323408,-56.6017747680085,
3.64284210641837));
#249496=CARTESIAN_POINT('Ctrl Pts',(-25.6273687254301,-56.7783458705711,
3.6555352798779));
#249497=CARTESIAN_POINT('Ctrl Pts',(-25.510904950036,-56.830537517614,3.65585996533093));
#249498=CARTESIAN_POINT('Ctrl Pts',(-25.4764491573039,-56.7526792962306,
3.55127902710141));
#249499=CARTESIAN_POINT('Ctrl Pts',(-25.6742415049975,-56.8833377255395,
3.4715307213903));
#249500=CARTESIAN_POINT('Ctrl Pts',(-25.5577357740372,-56.9357219102088,
3.47182327905146));
#249501=CARTESIAN_POINT('Ctrl Pts',(-25.513848576796,-56.8366797674138,
3.40413028377926));
#249502=CARTESIAN_POINT('Origin',(-25.4547063934078,-56.3916032444851,3.64303198860223));
#249503=CARTESIAN_POINT('Origin',(3.88110971579612E-16,1.91523848684163E-13,
2.53178198860262));
#249504=CARTESIAN_POINT('Origin',(-24.0229981225292,-53.9190682401995,2.53178198860224));
#249505=CARTESIAN_POINT('Origin',(10.0037024164483,23.2492868865828,3.64303198860279));
#249506=CARTESIAN_POINT('Origin',(-25.2915084057487,-56.0249274780514,3.64299466007511));
#249507=CARTESIAN_POINT('Ctrl Pts',(-23.9791663275009,-53.8206887816836,
2.59908173515985));
#249508=CARTESIAN_POINT('Ctrl Pts',(-23.9943483786813,-53.8547645473081,
2.65878198860223));
#249509=CARTESIAN_POINT('Ctrl Pts',(-24.0229981225292,-53.9190682401995,
2.65878198860223));
#249510=CARTESIAN_POINT('Ctrl Pts',(-24.0592381182998,-53.7850138844282,
2.59908193199934));
#249511=CARTESIAN_POINT('Ctrl Pts',(-24.0526825045791,-53.8287709626517,
2.65877685806671));
#249512=CARTESIAN_POINT('Ctrl Pts',(-24.0695074323269,-53.8983362760839,
2.65878198860223));
#249513=CARTESIAN_POINT('Ctrl Pts',(-24.1432906710369,-53.7744461045705,
2.63872492669742));
#249514=CARTESIAN_POINT('Ctrl Pts',(-24.1158128282434,-53.8255298669644,
2.69532212015236));
#249515=CARTESIAN_POINT('Ctrl Pts',(-24.1225146216894,-53.9015903052238,
2.68176836726598));
#249516=CARTESIAN_POINT('Ctrl Pts',(-24.2696905364167,-53.7968389608978,
2.75442176402227));
#249517=CARTESIAN_POINT('Ctrl Pts',(-24.1983175571249,-53.8548027426707,
2.7920317992009));
#249518=CARTESIAN_POINT('Ctrl Pts',(-24.2081897025472,-53.9421141528987,
2.74885310748134));
#249519=CARTESIAN_POINT('Ctrl Pts',(-24.3127961529001,-53.8282518514938,
2.82866089558347));
#249520=CARTESIAN_POINT('Ctrl Pts',(-24.2176488245043,-53.8880291490203,
2.85316563119182));
#249521=CARTESIAN_POINT('Ctrl Pts',(-24.2411088588481,-53.9780599067624,
2.79189751796557));
#249522=CARTESIAN_POINT('Ctrl Pts',(-24.3312692531083,-53.8697418420145,
2.90134173515984));
#249523=CARTESIAN_POINT('Ctrl Pts',(-24.2159747902182,-53.9216078643417,
2.90103711553191));
#249524=CARTESIAN_POINT('Ctrl Pts',(-24.2595822759728,-54.0195518809641,
2.83404198860223));
#249525=CARTESIAN_POINT('Origin',(-24.3756025490934,-53.9678963272935,2.83404198860223));
#249526=CARTESIAN_POINT('Origin',(-25.2734729066191,-55.9845461685084,3.56647653971746));
#249527=CARTESIAN_POINT('Origin',(-25.2401862573137,-55.9097831300747,3.42473028058445));
#249528=CARTESIAN_POINT('Origin',(-24.4480624203037,-54.1306438627319,3.11913648167933));
#249529=CARTESIAN_POINT('Origin',(-24.5205222915147,-54.2933913980364,3.40423097483272));
#249530=CARTESIAN_POINT('Ctrl Pts',(-25.1059793847697,-55.6083495590302,
3.36123028058442));
#249531=CARTESIAN_POINT('Ctrl Pts',(-24.9899591116491,-55.6600051127008,
3.36123028058442));
#249532=CARTESIAN_POINT('Ctrl Pts',(-24.9899591116491,-55.6600051127008,
3.23423028058442));
#249533=CARTESIAN_POINT('Ctrl Pts',(-25.142375998794,-55.6906734752784,
3.36123028058442));
#249534=CARTESIAN_POINT('Ctrl Pts',(-25.0265352902408,-55.7421565548675,
3.36099641108454));
#249535=CARTESIAN_POINT('Ctrl Pts',(-25.0448742789057,-55.7833465978043,
3.23423043688414));
#249536=CARTESIAN_POINT('Ctrl Pts',(-25.1767934079555,-55.7685161955949,
3.41054258905245));
#249537=CARTESIAN_POINT('Ctrl Pts',(-25.0612933298577,-55.8202243900326,
3.4100881582604));
#249538=CARTESIAN_POINT('Ctrl Pts',(-25.0968004762765,-55.8999747466282,
3.30819867304245));
#249539=CARTESIAN_POINT('Ctrl Pts',(-25.1949317875296,-55.8095395120007,
3.48823028058443));
#249540=CARTESIAN_POINT('Ctrl Pts',(-25.0796311836949,-55.8614118841079,
3.48794691941559));
#249541=CARTESIAN_POINT('Ctrl Pts',(-25.1241659841931,-55.9614386837453,
3.42473028058444));
#249542=CARTESIAN_POINT('Origin',(-25.1059793847697,-55.6083495590302,3.23423028058442));
#249543=CARTESIAN_POINT('Ctrl Pts',(-24.4761921430387,-54.1952354911872,
3.47153072139034));
#249544=CARTESIAN_POINT('Ctrl Pts',(-24.3607210247419,-54.2471777813618,
3.47122746285039));
#249545=CARTESIAN_POINT('Ctrl Pts',(-24.4045675690225,-54.3451938326306,
3.40413046676736));
#249546=CARTESIAN_POINT('Ctrl Pts',(-24.5230721320493,-54.3002261711145,
3.6555381345795));
#249547=CARTESIAN_POINT('Ctrl Pts',(-24.4074212664117,-54.3520689157374,
3.65520336072156));
#249548=CARTESIAN_POINT('Ctrl Pts',(-24.4419676644359,-54.4291958219368,
3.55128134519859));
#249549=CARTESIAN_POINT('Ctrl Pts',(-24.6072895482028,-54.4888383671844,
3.77003198860224));
#249550=CARTESIAN_POINT('Ctrl Pts',(-24.491383313694,-54.5406519873259,
3.76980209314076));
#249551=CARTESIAN_POINT('Ctrl Pts',(-24.5091552540991,-54.5801016184624,
3.64284195387403));
#249552=CARTESIAN_POINT('Ctrl Pts',(-24.6957503380303,-54.6869600343298,
3.77003198860224));
#249553=CARTESIAN_POINT('Ctrl Pts',(-24.5795562747208,-54.7386929643777,
3.77003198860224));
#249554=CARTESIAN_POINT('Ctrl Pts',(-24.5797301948775,-54.738615530135,
3.64284189403738));
#249555=CARTESIAN_POINT('Origin',(-24.6957503380303,-54.6869600343298,3.64303198860224));
#249556=CARTESIAN_POINT('Origin',(9.75435829333325,22.6892508167096,3.23423028058497));
#249557=CARTESIAN_POINT('Origin',(-25.0444775033943,-55.4702140717967,3.23423028058442));
#249558=CARTESIAN_POINT('Origin',(9.71531210234964,22.6015516358795,3.64303198860278));
#249559=CARTESIAN_POINT('Origin',(-24.8590452239598,-55.0536014459536,3.64299171721715));
#249560=CARTESIAN_POINT('Ctrl Pts',(-24.955532024241,-55.2690209153041,
3.48823028058442));
#249561=CARTESIAN_POINT('Ctrl Pts',(-24.839188866184,-55.3213695969756,
3.4885200421222));
#249562=CARTESIAN_POINT('Ctrl Pts',(-24.7942503289602,-55.2204359898057,
3.42473028058442));
#249563=CARTESIAN_POINT('Ctrl Pts',(-24.9737291291726,-55.3101840490919,
3.4102800584837));
#249564=CARTESIAN_POINT('Ctrl Pts',(-24.8573973158458,-55.3622664445036,
3.41074404220123));
#249565=CARTESIAN_POINT('Ctrl Pts',(-24.8217083187803,-55.2821076446789,
3.30780486243738));
#249566=CARTESIAN_POINT('Ctrl Pts',(-25.0082040095655,-55.3881672017728,
3.36123028058442));
#249567=CARTESIAN_POINT('Ctrl Pts',(-24.8919348043947,-55.4398389138674,
3.36146460586436));
#249568=CARTESIAN_POINT('Ctrl Pts',(-24.8737270328811,-55.3989435894807,
3.23423045308459));
#249569=CARTESIAN_POINT('Ctrl Pts',(-25.0444775033943,-55.4702140717967,
3.36123028058442));
#249570=CARTESIAN_POINT('Ctrl Pts',(-24.9284572302736,-55.5218696254673,
3.36123028058442));
#249571=CARTESIAN_POINT('Ctrl Pts',(-24.9284572302736,-55.5218696254673,
3.23423028058442));
#249572=CARTESIAN_POINT('Origin',(-24.9102706020808,-55.168780436135,3.42473028058442));
#249573=CARTESIAN_POINT('Origin',(-24.8771824678731,-55.0944632691829,3.56563113524668));
#249574=CARTESIAN_POINT('Origin',(-18.6791227126679,-58.515880043567,3.56647653909354));
#249575=CARTESIAN_POINT('Origin',(-18.6927400943479,-58.5579573083303,3.64299466007364));
#249576=CARTESIAN_POINT('Origin',(-18.6538332760099,-58.4380471616454,3.42473028058443));
#249577=CARTESIAN_POINT('Ctrl Pts',(-18.6203878281142,-58.3332704847796,
3.48823028058443));
#249578=CARTESIAN_POINT('Ctrl Pts',(-18.7407822670297,-58.2946680067388,
3.48794691941559));
#249579=CARTESIAN_POINT('Ctrl Pts',(-18.7746174535794,-58.3988020033598,
3.42473028058444));
#249580=CARTESIAN_POINT('Ctrl Pts',(-18.6063701040098,-58.2905032380258,
3.41028005925046));
#249581=CARTESIAN_POINT('Ctrl Pts',(-18.7268030714104,-58.2516444665209,
3.40982512231077));
#249582=CARTESIAN_POINT('Ctrl Pts',(-18.7537563325793,-58.3345980746911,
3.30780486372911));
#249583=CARTESIAN_POINT('Ctrl Pts',(-18.5798130476659,-58.2094810151999,
3.36123028058441));
#249584=CARTESIAN_POINT('Ctrl Pts',(-18.7003491529659,-58.1702276772295,
3.3609972104835));
#249585=CARTESIAN_POINT('Ctrl Pts',(-18.7142352739232,-58.2129647630934,
3.2342304530829));
#249586=CARTESIAN_POINT('Ctrl Pts',(-18.5518699907145,-58.1242364370956,
3.36123028058441));
#249587=CARTESIAN_POINT('Ctrl Pts',(-18.672654168284,-58.08499127881,3.36123028058441));
#249588=CARTESIAN_POINT('Ctrl Pts',(-18.672654168284,-58.08499127881,3.23423028058441));
#249589=CARTESIAN_POINT('Origin',(-18.5518699907145,-58.1242364370956,3.2342302805844));
#249590=CARTESIAN_POINT('Origin',(0.301960443923718,-0.0981128957138591,
3.64303198860263));
#249591=CARTESIAN_POINT('Origin',(-18.8168143322221,-58.9396512752213,3.64303198860221));
#249592=CARTESIAN_POINT('Origin',(0.301960443923718,-0.0981128957138562,
3.23423028058481));
#249593=CARTESIAN_POINT('Origin',(-18.5051441132836,-57.9804289733664,3.2342302805844));
#249594=CARTESIAN_POINT('Ctrl Pts',(-18.9827025415091,-59.4519788726608,
3.4715307213903));
#249595=CARTESIAN_POINT('Ctrl Pts',(-19.1043350233605,-59.4129503614026,
3.4718232790262));
#249596=CARTESIAN_POINT('Ctrl Pts',(-19.0706774512222,-59.3099814440477,
3.4041302895898));
#249597=CARTESIAN_POINT('Ctrl Pts',(-18.9472820042061,-59.3425890481018,
3.65553807120915));
#249598=CARTESIAN_POINT('Ctrl Pts',(-19.0687544722125,-59.3034455268842,
3.65586275496877));
#249599=CARTESIAN_POINT('Ctrl Pts',(-19.0422629184335,-59.2225305038481,
3.55128126837106));
#249600=CARTESIAN_POINT('Ctrl Pts',(-18.8836509927323,-59.1460739925262,
3.77003198860221));
#249601=CARTESIAN_POINT('Ctrl Pts',(-19.0048854004781,-59.1068782740624,
3.77025505748552));
#249602=CARTESIAN_POINT('Ctrl Pts',(-18.9912173655538,-59.0654284453484,
3.64284211731235));
#249603=CARTESIAN_POINT('Ctrl Pts',(-18.8168143322221,-58.9396512752213,
3.77003198860221));
#249604=CARTESIAN_POINT('Ctrl Pts',(-18.9377789557522,-58.900347486489,
3.77003198860221));
#249605=CARTESIAN_POINT('Ctrl Pts',(-18.9375983752039,-58.9004061606659,
3.64284239821646));
#249606=CARTESIAN_POINT('Origin',(-18.9499432001052,-59.349379800228,3.40423097483268));
#249607=CARTESIAN_POINT('Ctrl Pts',(-18.5051441132836,-57.9804289733663,
3.36123028058441));
#249608=CARTESIAN_POINT('Ctrl Pts',(-18.6259282908531,-57.9411838150807,
3.36123028058441));
#249609=CARTESIAN_POINT('Ctrl Pts',(-18.6259282908531,-57.9411838150807,
3.23423028058441));
#249610=CARTESIAN_POINT('Ctrl Pts',(-18.4771060595073,-57.8948964606935,
3.3612302805844));
#249611=CARTESIAN_POINT('Ctrl Pts',(-18.5980867642066,-57.8554964068691,
3.36146538610072));
#249612=CARTESIAN_POINT('Ctrl Pts',(-18.5842066467866,-57.8127777979935,
3.23423043688339));
#249613=CARTESIAN_POINT('Ctrl Pts',(-18.4505921960623,-57.8140195545735,
3.41054258693058));
#249614=CARTESIAN_POINT('Ctrl Pts',(-18.5718941197427,-57.7748837362142,
3.41100608859698));
#249615=CARTESIAN_POINT('Ctrl Pts',(-18.5447558577151,-57.6913607539395,
3.30819866970735));
#249616=CARTESIAN_POINT('Ctrl Pts',(-18.4366189870667,-57.7713971777987,
3.48823028058441));
#249617=CARTESIAN_POINT('Ctrl Pts',(-18.5581069080655,-57.732451061807,
3.48852004212219));
#249618=CARTESIAN_POINT('Ctrl Pts',(-18.5239649837002,-57.6273730232605,
3.42473028058441));
#249619=CARTESIAN_POINT('Origin',(-18.4031808061308,-57.6666181815461,3.4247302805844));
#249620=CARTESIAN_POINT('Origin',(-19.0049943031114,-59.5188096735787,3.11913648178371));
#249621=CARTESIAN_POINT('Origin',(-19.0600454060081,-59.688239546742,2.83404198860219));
#249622=CARTESIAN_POINT('Origin',(-18.3780421908164,-57.5892494790284,3.56563113460774));
#249623=CARTESIAN_POINT('Origin',(-18.3641788932745,-57.546747042666,3.64299171721713));
#249624=CARTESIAN_POINT('Ctrl Pts',(-19.4393816709751,-59.8776671349985,
2.59908173515981));
#249625=CARTESIAN_POINT('Ctrl Pts',(-19.4278624395261,-59.8421853116552,
2.65878198860219));
#249626=CARTESIAN_POINT('Ctrl Pts',(-19.4061247292248,-59.7752282754837,
2.65878198860219));
#249627=CARTESIAN_POINT('Ctrl Pts',(-19.3555723159018,-59.904875846812,
2.59908193475578));
#249628=CARTESIAN_POINT('Ctrl Pts',(-19.3668135526093,-59.8620015382112,
2.65878715325416));
#249629=CARTESIAN_POINT('Ctrl Pts',(-19.3576098387249,-59.7909691583389,
2.65878198860219));
#249630=CARTESIAN_POINT('Ctrl Pts',(-19.2705128813947,-59.9061888791358,
2.63878778849821));
#249631=CARTESIAN_POINT('Ctrl Pts',(-19.3034480936183,-59.8582551377157,
2.69564460180079));
#249632=CARTESIAN_POINT('Ctrl Pts',(-19.3051157581414,-59.7817014705981,
2.68180481624832));
#249633=CARTESIAN_POINT('Ctrl Pts',(-19.1466203444576,-59.8700374834722,
2.7544323887861));
#249634=CARTESIAN_POINT('Ctrl Pts',(-19.2244111832563,-59.820049432414,
2.79268340777034));
#249635=CARTESIAN_POINT('Ctrl Pts',(-19.2239451174245,-59.7316696194039,
2.74885926835576));
#249636=CARTESIAN_POINT('Ctrl Pts',(-19.1068608943535,-59.8340873574358,
2.82856655361622));
#249637=CARTESIAN_POINT('Ctrl Pts',(-19.2088773592695,-59.7849307811032,
2.85384197230818));
#249638=CARTESIAN_POINT('Ctrl Pts',(-19.1948817636402,-59.6922425516965,
2.79184624278462));
#249639=CARTESIAN_POINT('Ctrl Pts',(-19.0928077206406,-59.7908376697911,
2.90134173515981));
#249640=CARTESIAN_POINT('Ctrl Pts',(-19.2142545736078,-59.7518659300026,
2.90163218716348));
#249641=CARTESIAN_POINT('Ctrl Pts',(-19.1808295835776,-59.6489943884564,
2.83404198860219));
#249642=CARTESIAN_POINT('Origin',(-19.4061247292248,-59.7752282754837,2.53178198860219));
#249643=CARTESIAN_POINT('Origin',(0.301960443923718,-0.0981128957138591,
3.64303198860263));
#249644=CARTESIAN_POINT('Origin',(-18.240199652704,-57.1650137687747,3.64303198860222));
#249645=CARTESIAN_POINT('Origin',(2.07460197300492E-17,1.91734254067317E-13,
2.53178198860262));
#249646=CARTESIAN_POINT('Origin',(-19.4351129318415,-59.7658094374951,2.53178198860219));
#249647=CARTESIAN_POINT('Ctrl Pts',(-18.240199652704,-57.1650137687747,
3.77003198860223));
#249648=CARTESIAN_POINT('Ctrl Pts',(-18.3611647704261,-57.1257098194697,
3.77003198860223));
#249649=CARTESIAN_POINT('Ctrl Pts',(-18.3609836949481,-57.125768654459,
3.64284187936962));
#249650=CARTESIAN_POINT('Ctrl Pts',(-18.1733685221984,-56.9585856505952,
3.77003198860223));
#249651=CARTESIAN_POINT('Ctrl Pts',(-18.2941737326415,-56.919534269366,
3.76980208962944));
#249652=CARTESIAN_POINT('Ctrl Pts',(-18.3073637563264,-56.9607434512666,
3.6428419392832));
#249653=CARTESIAN_POINT('Ctrl Pts',(-18.1097485684455,-56.7620685738639,
3.65553535416544));
#249654=CARTESIAN_POINT('Ctrl Pts',(-18.2303834904097,-56.7232097045342,
3.65520057834419));
#249655=CARTESIAN_POINT('Ctrl Pts',(-18.256318583299,-56.8036425617875,
3.5512791096416));
#249656=CARTESIAN_POINT('Ctrl Pts',(-18.0743352474886,-56.6526781108323,
3.47153072139033));
#249657=CARTESIAN_POINT('Ctrl Pts',(-18.1949032015567,-56.6140134911406,
3.47122746281543));
#249658=CARTESIAN_POINT('Ctrl Pts',(-18.2279043987987,-56.7161926934816,
3.4041304590121));
#249659=CARTESIAN_POINT('Origin',(-18.1070706485037,-56.755284824227,3.40423097483271));
#249660=CARTESIAN_POINT('Ctrl Pts',(-19.697766688184,-59.5942745858236,
2.90134173515982));
#249661=CARTESIAN_POINT('Ctrl Pts',(-19.5766071063163,-59.6341304551457,
2.90163218716349));
#249662=CARTESIAN_POINT('Ctrl Pts',(-19.5431821162861,-59.5312589135995,
2.8340419886022));
#249663=CARTESIAN_POINT('Ctrl Pts',(-19.7118253299473,-59.637544215329,
2.82853349835315));
#249664=CARTESIAN_POINT('Ctrl Pts',(-19.6004058925606,-59.6577332347569,
2.85381483162282));
#249665=CARTESIAN_POINT('Ctrl Pts',(-19.5572406993628,-59.5745267832909,
2.79182701594181));
#249666=CARTESIAN_POINT('Ctrl Pts',(-19.7007277907732,-59.6898285824897,
2.754688220736));
#249667=CARTESIAN_POINT('Ctrl Pts',(-19.6083614943627,-59.695174564008,
2.79286913083796));
#249668=CARTESIAN_POINT('Ctrl Pts',(-19.5568428722495,-59.623336104959,
2.74900763297877));
#249669=CARTESIAN_POINT('Ctrl Pts',(-19.6225475038103,-59.791305386369,
2.63954450640351));
#249670=CARTESIAN_POINT('Ctrl Pts',(-19.5674227749668,-59.7720679362487,
2.69627684028815));
#249671=CARTESIAN_POINT('Ctrl Pts',(-19.5210053955053,-59.7110541706149,
2.68224356036443));
#249672=CARTESIAN_POINT('Ctrl Pts',(-19.5524931121159,-59.8408924241697,
2.59908178706384));
#249673=CARTESIAN_POINT('Ctrl Pts',(-19.5181549791675,-59.8128277376105,
2.6587870432151));
#249674=CARTESIAN_POINT('Ctrl Pts',(-19.4837751174913,-59.7499755976261,
2.65878198860219));
#249675=CARTESIAN_POINT('Ctrl Pts',(-19.4684195516691,-59.8682321556242,
2.59908173515981));
#249676=CARTESIAN_POINT('Ctrl Pts',(-19.4568831131878,-59.8327559231846,
2.65878198860219));
#249677=CARTESIAN_POINT('Ctrl Pts',(-19.4351129318415,-59.7658094374951,
2.65878198860219));
#249678=CARTESIAN_POINT('Origin',(-19.6639662938556,-59.4920137553139,2.83404198860219));
#249679=CARTESIAN_POINT('Origin',(-18.0520194698746,-56.585854717958,3.1191364816709));
#249680=CARTESIAN_POINT('Origin',(-17.9969682911406,-56.4164246115663,2.83404198860222));
#249681=CARTESIAN_POINT('Origin',(-19.6089151909114,-59.3225838821508,3.11913648177464));
#249682=CARTESIAN_POINT('Origin',(-19.5538640879527,-59.1531540087999,3.40423097483268));
#249683=CARTESIAN_POINT('Ctrl Pts',(-17.9642361803967,-56.3138168485095,
2.90134173515983));
#249684=CARTESIAN_POINT('Ctrl Pts',(-18.084621806869,-56.2752137607566,
2.9010371155319));
#249685=CARTESIAN_POINT('Ctrl Pts',(-18.1177524687101,-56.3771794532807,
2.83404198860222));
#249686=CARTESIAN_POINT('Ctrl Pts',(-17.9501961787623,-56.2706044454591,
2.82862991747923));
#249687=CARTESIAN_POINT('Ctrl Pts',(-18.0608967538119,-56.2513675234857,
2.85314045886425));
#249688=CARTESIAN_POINT('Ctrl Pts',(-18.1037113794371,-56.3339654239813,
2.79187960999962));
#249689=CARTESIAN_POINT('Ctrl Pts',(-17.9612588333752,-56.2186079213553,
2.75470625793283));
#249690=CARTESIAN_POINT('Ctrl Pts',(-18.0531413250547,-56.2138593173286,
2.79224250381846));
#249691=CARTESIAN_POINT('Ctrl Pts',(-18.1041761987734,-56.2854146278933,
2.74901809108221));
#249692=CARTESIAN_POINT('Ctrl Pts',(-18.0394175380791,-56.1179510603876,
2.63947868311662));
#249693=CARTESIAN_POINT('Ctrl Pts',(-18.0943218653323,-56.1373490477008,
2.69595066767879));
#249694=CARTESIAN_POINT('Ctrl Pts',(-18.1403075368575,-56.1984140977476,
2.68220539436019));
#249695=CARTESIAN_POINT('Ctrl Pts',(-18.1094153628973,-56.0689198620977,
2.59908178585038));
#249696=CARTESIAN_POINT('Ctrl Pts',(-18.1436123520185,-56.097036206149,
2.65877670944869));
#249697=CARTESIAN_POINT('Ctrl Pts',(-18.1777307632111,-56.1599674935309,
2.65878198860222));
#249698=CARTESIAN_POINT('Ctrl Pts',(-18.1930767435944,-56.0417604764383,
2.59908173515984));
#249699=CARTESIAN_POINT('Ctrl Pts',(-18.204595418534,-56.0772424804484,
2.65878198860222));
#249700=CARTESIAN_POINT('Ctrl Pts',(-18.2263320786577,-56.1441998575527,
2.65878198860222));
#249701=CARTESIAN_POINT('Origin',(-18.2263320786577,-56.1441998575527,2.53178198860222));
#249702=CARTESIAN_POINT('Ctrl Pts',(-19.4207352200695,-58.7434254837932,
3.77003198860222));
#249703=CARTESIAN_POINT('Ctrl Pts',(-19.2997705861185,-58.7827292759115,
3.77003198860222));
#249704=CARTESIAN_POINT('Ctrl Pts',(-19.2999511771033,-58.7826705983436,
3.6428423872756));
#249705=CARTESIAN_POINT('Ctrl Pts',(-19.4879965013596,-58.9497137831218,
3.77003198860221));
#249706=CARTESIAN_POINT('Ctrl Pts',(-19.3668771285525,-58.9892635895145,
3.77025506105811));
#249707=CARTESIAN_POINT('Ctrl Pts',(-19.3535710010437,-58.9476954469487,
3.6428421064192));
#249708=CARTESIAN_POINT('Ctrl Pts',(-19.5520260773863,-59.1460976215385,
3.65553527987787));
#249709=CARTESIAN_POINT('Ctrl Pts',(-19.4307447900758,-59.1858295778062,
3.65585996532951));
#249710=CARTESIAN_POINT('Ctrl Pts',(-19.4046161500175,-59.1047962608419,
3.55127902710053));
#249711=CARTESIAN_POINT('Ctrl Pts',(-19.5876674457073,-59.2554138597571,
3.47153072139031));
#249712=CARTESIAN_POINT('Ctrl Pts',(-19.4663243070087,-59.2953329133625,
3.47182327905147));
#249713=CARTESIAN_POINT('Ctrl Pts',(-19.4330302514108,-59.1922458725044,
3.40413028377948));
#249714=CARTESIAN_POINT('Origin',(-19.4207352200695,-58.7434254837932,3.64303198860222));
#249715=CARTESIAN_POINT('Origin',(3.93842937138094E-16,1.91521648388735E-13,
2.53178198860262));
#249716=CARTESIAN_POINT('Origin',(-18.2553202812744,-56.1347810195642,2.53178198860222));
#249717=CARTESIAN_POINT('Origin',(5.6397553624924,18.3848338156956,3.64303198860275));
#249718=CARTESIAN_POINT('Origin',(-19.296759302444,-58.361699570715,3.64299466007636));
#249719=CARTESIAN_POINT('Ctrl Pts',(-18.2220120550212,-56.0323588238391,
2.59908173515984));
#249720=CARTESIAN_POINT('Ctrl Pts',(-18.2335490499213,-56.0678348753332,
2.65878198860222));
#249721=CARTESIAN_POINT('Ctrl Pts',(-18.2553202812744,-56.1347810195642,
2.65878198860222));
#249722=CARTESIAN_POINT('Ctrl Pts',(-18.3053742463593,-56.0052491386464,
2.59908193199861));
#249723=CARTESIAN_POINT('Ctrl Pts',(-18.294280684832,-56.0480812627868,
2.65877685806598));
#249724=CARTESIAN_POINT('Ctrl Pts',(-18.3037418885556,-56.1190241739963,
2.65878198860222));
#249725=CARTESIAN_POINT('Ctrl Pts',(-18.3900709842066,-56.0035251343644,
2.63872492669767));
#249726=CARTESIAN_POINT('Ctrl Pts',(-18.3574039607303,-56.0514568378823,
2.69532212015237));
#249727=CARTESIAN_POINT('Ctrl Pts',(-18.3561185603237,-56.1278011372721,
2.68176836726598));
#249728=CARTESIAN_POINT('Ctrl Pts',(-18.5134377270385,-56.0390077039668,
2.75442176402201));
#249729=CARTESIAN_POINT('Ctrl Pts',(-18.4363968713611,-56.0891934462338,
2.79203179920095));
#249730=CARTESIAN_POINT('Ctrl Pts',(-18.437088408601,-56.1770584756116,
2.74885310748131));
#249731=CARTESIAN_POINT('Ctrl Pts',(-18.5530236652639,-56.0747542753108,
2.82866089558367));
#249732=CARTESIAN_POINT('Ctrl Pts',(-18.4521491348405,-56.1242585025262,
2.85316563119173));
#249733=CARTESIAN_POINT('Ctrl Pts',(-18.466069875907,-56.2162483036947,
2.79189751796582));
#249734=CARTESIAN_POINT('Ctrl Pts',(-18.567058682946,-56.1179479440988,
2.90134173515983));
#249735=CARTESIAN_POINT('Ctrl Pts',(-18.4469743395774,-56.1574782858997,
2.90103711553189));
#249736=CARTESIAN_POINT('Ctrl Pts',(-18.4801050014185,-56.2594439784239,
2.83404198860221));
#249737=CARTESIAN_POINT('Origin',(-18.600889178988,-56.2201988201382,2.83404198860222));
#249738=CARTESIAN_POINT('Origin',(-19.2830435998987,-58.3196542512035,3.56647653971717));
#249739=CARTESIAN_POINT('Origin',(-19.2577541638573,-58.2418213702174,3.42473028058445));
#249740=CARTESIAN_POINT('Origin',(-18.6559403576599,-56.389628926534,3.11913648168046));
#249741=CARTESIAN_POINT('Origin',(-18.7109915363512,-56.5590590327989,3.40423097483271));
#249742=CARTESIAN_POINT('Ctrl Pts',(-19.155790878562,-57.9280106456676,
3.36123028058441));
#249743=CARTESIAN_POINT('Ctrl Pts',(-19.0350067009925,-57.9672558039532,
3.36123028058441));
#249744=CARTESIAN_POINT('Ctrl Pts',(-19.0350067009925,-57.9672558039532,
3.23423028058441));
#249745=CARTESIAN_POINT('Ctrl Pts',(-19.1833829156714,-58.0136880650208,
3.36123028058441));
#249746=CARTESIAN_POINT('Ctrl Pts',(-19.0627953474467,-58.0527804636634,
3.36099641108351));
#249747=CARTESIAN_POINT('Ctrl Pts',(-19.0767283413222,-58.0956618095401,
3.23423043688317));
#249748=CARTESIAN_POINT('Ctrl Pts',(-19.209475002731,-58.0947019536606,
3.41054258905243));
#249749=CARTESIAN_POINT('Ctrl Pts',(-19.0892026680443,-58.1340538395287,
3.41008815826083));
#249750=CARTESIAN_POINT('Ctrl Pts',(-19.1161791203798,-58.2170788227743,
3.30819867304341));
#249751=CARTESIAN_POINT('Ctrl Pts',(-19.2232259141434,-58.1373965169893,
3.48823028058443));
#249752=CARTESIAN_POINT('Ctrl Pts',(-19.1031347997382,-58.1769325318819,
3.48794691941559));
#249753=CARTESIAN_POINT('Ctrl Pts',(-19.1369699862878,-58.281066528503,
3.42473028058444));
#249754=CARTESIAN_POINT('Origin',(-19.155790878562,-57.9280106456676,3.23423028058441));
#249755=CARTESIAN_POINT('Ctrl Pts',(-18.6771643191705,-56.4568070719811,
3.47153072139033));
#249756=CARTESIAN_POINT('Ctrl Pts',(-18.5568963159709,-56.496394798308,
3.47122746285037));
#249757=CARTESIAN_POINT('Ctrl Pts',(-18.5902571970797,-56.5984571192857,
3.40413046676725));
#249758=CARTESIAN_POINT('Ctrl Pts',(-18.7128129802646,-56.566122895188,
3.65553813457947));
#249759=CARTESIAN_POINT('Ctrl Pts',(-18.5923766197452,-56.6055928325687,
3.65520336072065));
#249760=CARTESIAN_POINT('Ctrl Pts',(-18.6186718120033,-56.6859083114039,
3.55128134519815));
#249761=CARTESIAN_POINT('Ctrl Pts',(-18.7768537015919,-56.7625049710039,
3.77003198860223));
#249762=CARTESIAN_POINT('Ctrl Pts',(-18.6561664154738,-56.8019192501375,
3.76980209314237));
#249763=CARTESIAN_POINT('Ctrl Pts',(-18.6697173900119,-56.8430104456862,
3.64284195387455));
#249764=CARTESIAN_POINT('Ctrl Pts',(-18.8441205405514,-56.9687879773466,
3.77003198860223));
#249765=CARTESIAN_POINT('Ctrl Pts',(-18.7231554367999,-57.0080919221123,
3.77003198860222));
#249766=CARTESIAN_POINT('Ctrl Pts',(-18.7233364982864,-57.0080330916691,
3.64284189403718));
#249767=CARTESIAN_POINT('Origin',(-18.8441205405514,-56.9687879773466,3.64303198860223));
#249768=CARTESIAN_POINT('Origin',(5.49583002221419,17.9418771653391,3.23423028058494));
#249769=CARTESIAN_POINT('Origin',(-19.109065001131,-57.7842031819383,3.23423028058441));
#249770=CARTESIAN_POINT('Origin',(5.4732919481113,17.872512105713,3.64303198860275));
#249771=CARTESIAN_POINT('Origin',(-18.968196416682,-57.3504898524417,3.64299171721817));
#249772=CARTESIAN_POINT('Ctrl Pts',(-19.0416371860872,-57.5748148483576,
3.4882302805844));
#249773=CARTESIAN_POINT('Ctrl Pts',(-18.920459440774,-57.6147155869502,
3.48852004212219));
#249774=CARTESIAN_POINT('Ctrl Pts',(-18.8863175164087,-57.5096375484037,
3.4247302805844));
#249775=CARTESIAN_POINT('Ctrl Pts',(-19.0554318862552,-57.6176546016062,
3.41028005848365));
#249776=CARTESIAN_POINT('Ctrl Pts',(-18.9342932580178,-57.6572916985361,
3.41074404220394));
#249777=CARTESIAN_POINT('Ctrl Pts',(-18.9071786451771,-57.5738415009809,
3.30780486243911));
#249778=CARTESIAN_POINT('Ctrl Pts',(-19.0815664505355,-57.698814160686,
3.36123028058441));
#249779=CARTESIAN_POINT('Ctrl Pts',(-18.9605330155747,-57.7380493683895,
3.36146460586264));
#249780=CARTESIAN_POINT('Ctrl Pts',(-18.9466997135536,-57.6954748424952,
3.23423045308292));
#249781=CARTESIAN_POINT('Ctrl Pts',(-19.109065001131,-57.7842031819383,
3.36123028058441));
#249782=CARTESIAN_POINT('Ctrl Pts',(-18.9882808235615,-57.8234483402239,
3.36123028058441));
#249783=CARTESIAN_POINT('Ctrl Pts',(-18.9882808235615,-57.8234483402239,
3.23423028058441));
#249784=CARTESIAN_POINT('Origin',(-19.0071016939782,-57.4703923901181,3.4247302805844));
#249785=CARTESIAN_POINT('Origin',(-18.9819630792877,-57.393023688563,3.56563113524764));
#249786=CARTESIAN_POINT('Origin',(-12.4602215063104,-60.147823922414,3.56647653909347));
#249787=CARTESIAN_POINT('Origin',(-12.4693660187251,-60.1910940874988,3.64299466007341));
#249788=CARTESIAN_POINT('Origin',(-12.4432063593716,-60.0677739512125,3.42473028058441));
#249789=CARTESIAN_POINT('Ctrl Pts',(-12.420896274158,-59.9600752506736,
3.48823028058442));
#249790=CARTESIAN_POINT('Ctrl Pts',(-12.544666237448,-59.9342688867324,
3.48794691941558));
#249791=CARTESIAN_POINT('Ctrl Pts',(-12.5674311046648,-60.0413691664787,
3.42473028058443));
#249792=CARTESIAN_POINT('Ctrl Pts',(-12.411425735194,-59.9160770362134,
3.41028005925045));
#249793=CARTESIAN_POINT('Ctrl Pts',(-12.5352608058697,-59.8900198101355,
3.40982512230985));
#249794=CARTESIAN_POINT('Ctrl Pts',(-12.5533954010684,-59.9753363727311,
3.30780486372844));
#249795=CARTESIAN_POINT('Ctrl Pts',(-12.3934832896268,-59.8327226933128,
3.36123028058439));
#249796=CARTESIAN_POINT('Ctrl Pts',(-12.5174621766265,-59.8062838430886,
3.36099721048398));
#249797=CARTESIAN_POINT('Ctrl Pts',(-12.5268049860493,-59.8502383056088,
3.23423045308289));
#249798=CARTESIAN_POINT('Ctrl Pts',(-12.3746037924158,-59.7450242491247,
3.3612302805844));
#249799=CARTESIAN_POINT('Ctrl Pts',(-12.498828537709,-59.7186194643909,
3.3612302805844));
#249800=CARTESIAN_POINT('Ctrl Pts',(-12.498828537709,-59.7186194643908,
3.2342302805844));
#249801=CARTESIAN_POINT('Origin',(-12.3746037924158,-59.7450242491247,3.23423028058439));
#249802=CARTESIAN_POINT('Origin',(0.31056186323299,-0.0660119618344516,
3.64303198860263));
#249803=CARTESIAN_POINT('Origin',(-12.5528626811441,-60.5836663843181,3.6430319886022));
#249804=CARTESIAN_POINT('Origin',(0.31056186323299,-0.0660119618344487,
3.23423028058481));
#249805=CARTESIAN_POINT('Origin',(-12.3431658574205,-59.5971203935659,3.2342302805844));
#249806=CARTESIAN_POINT('Ctrl Pts',(-12.6642893210135,-61.1105274371641,
3.47153072139029));
#249807=CARTESIAN_POINT('Ctrl Pts',(-12.7893350777076,-61.0844267845856,
3.4718232790262));
#249808=CARTESIAN_POINT('Ctrl Pts',(-12.7666250679672,-60.9785037674412,
3.4041302895901));
#249809=CARTESIAN_POINT('Ctrl Pts',(-12.6404971713776,-60.9980344071774,
3.65553807120914));
#249810=CARTESIAN_POINT('Ctrl Pts',(-12.7653958126107,-60.9718026486701,
3.65586275496848));
#249811=CARTESIAN_POINT('Ctrl Pts',(-12.7475073053521,-60.8885617651934,
3.55128126837233));
#249812=CARTESIAN_POINT('Ctrl Pts',(-12.5977561540113,-60.7959446297924,
3.77003198860221));
#249813=CARTESIAN_POINT('Ctrl Pts',(-12.7224234952042,-60.7696360759163,
3.77025505748393));
#249814=CARTESIAN_POINT('Ctrl Pts',(-12.713163022104,-60.7269846150119,
3.64284211731113));
#249815=CARTESIAN_POINT('Ctrl Pts',(-12.5528626811441,-60.5836663843181,
3.77003198860221));
#249816=CARTESIAN_POINT('Ctrl Pts',(-12.6772730124459,-60.5572221520603,
3.77003198860221));
#249817=CARTESIAN_POINT('Ctrl Pts',(-12.6770872880158,-60.5572616290067,
3.64284239821705));
#249818=CARTESIAN_POINT('Origin',(-12.6424339620836,-61.0050661295706,3.40423097483267));
#249819=CARTESIAN_POINT('Ctrl Pts',(-12.3431658574205,-59.5971203935659,
3.3612302805844));
#249820=CARTESIAN_POINT('Ctrl Pts',(-12.4673906027137,-59.570715608832,
3.3612302805844));
#249821=CARTESIAN_POINT('Ctrl Pts',(-12.4673906027137,-59.570715608832,
3.2342302805844));
#249822=CARTESIAN_POINT('Ctrl Pts',(-12.324221981146,-59.5091256622725,
3.3612302805844));
#249823=CARTESIAN_POINT('Ctrl Pts',(-12.448658367964,-59.4825873732123,
3.36146538610033));
#249824=CARTESIAN_POINT('Ctrl Pts',(-12.4393195978191,-59.4386519140016,
3.23423043688338));
#249825=CARTESIAN_POINT('Ctrl Pts',(-12.3063073021285,-59.4259203549056,
3.41054258693058));
#249826=CARTESIAN_POINT('Ctrl Pts',(-12.4310355281328,-59.3996784303283,
3.41100608859746));
#249827=CARTESIAN_POINT('Ctrl Pts',(-12.4127764613278,-59.3137762748647,
3.30819866970766));
#249828=CARTESIAN_POINT('Ctrl Pts',(-12.2968658913797,-59.382070869907,
3.4882302805844));
#249829=CARTESIAN_POINT('Ctrl Pts',(-12.4217592664906,-59.3560370505013,
3.48852004212218));
#249830=CARTESIAN_POINT('Ctrl Pts',(-12.3987880210518,-59.2479658375576,
3.4247302805844));
#249831=CARTESIAN_POINT('Origin',(-12.2745632757586,-59.2743706222914,3.4247302805844));
#249832=CARTESIAN_POINT('Origin',(-12.6794732450934,-61.1793222555458,3.11913648178362));
#249833=CARTESIAN_POINT('Origin',(-12.716512528016,-61.3535783813231,2.83404198860219));
#249834=CARTESIAN_POINT('Origin',(-12.2576496039901,-59.1947980527941,3.56563113460808));
#249835=CARTESIAN_POINT('Origin',(-12.2483049653994,-59.1510793400372,3.64299171721742));
#249836=CARTESIAN_POINT('Ctrl Pts',(-13.0739701745318,-61.5816197022697,
2.59908173515981));
#249837=CARTESIAN_POINT('Ctrl Pts',(-13.066222907106,-61.5451281645059,
2.65878198860219));
#249838=CARTESIAN_POINT('Ctrl Pts',(-13.0516031943522,-61.4762657165315,
2.65878198860219));
#249839=CARTESIAN_POINT('Ctrl Pts',(-12.9877758510414,-61.5999188988202,
2.599081934755));
#249840=CARTESIAN_POINT('Ctrl Pts',(-13.0034370926704,-61.5584544893689,
2.65878715325401));
#249841=CARTESIAN_POINT('Ctrl Pts',(-13.0017087032037,-61.4868491822356,
2.65878198860219));
#249842=CARTESIAN_POINT('Ctrl Pts',(-12.9030451317656,-61.5923336062394,
2.63878778849841));
#249843=CARTESIAN_POINT('Ctrl Pts',(-12.9408103617796,-61.5481051179913,
2.69564460180071));
#249844=CARTESIAN_POINT('Ctrl Pts',(-12.9504709278433,-61.4721451382821,
2.68180481624841));
#249845=CARTESIAN_POINT('Ctrl Pts',(-12.7836101409423,-61.5434299552079,
2.7544323887859));
#249846=CARTESIAN_POINT('Ctrl Pts',(-12.8662000075459,-61.5018471007598,
2.79268340777052));
#249847=CARTESIAN_POINT('Ctrl Pts',(-12.8749747009093,-61.4139027244673,
2.74885926835568));
#249848=CARTESIAN_POINT('Ctrl Pts',(-12.7478263086951,-61.5035207735034,
2.82856655361638));
#249849=CARTESIAN_POINT('Ctrl Pts',(-12.8544221781245,-61.4652971063435,
2.85384197230746));
#249850=CARTESIAN_POINT('Ctrl Pts',(-12.8501918100164,-61.3716536946534,
2.79184624278466));
#249851=CARTESIAN_POINT('Ctrl Pts',(-12.7383709431244,-61.4590390555208,
2.9013417351598));
#249852=CARTESIAN_POINT('Ctrl Pts',(-12.8632261535949,-61.4329754599098,
2.90163218716348));
#249853=CARTESIAN_POINT('Ctrl Pts',(-12.8407372733092,-61.3271735965893,
2.83404198860219));
#249854=CARTESIAN_POINT('Origin',(-13.0516031943522,-61.4762657165315,2.53178198860219));
#249855=CARTESIAN_POINT('Origin',(0.31056186323299,-0.0660119618344516,
3.64303198860263));
#249856=CARTESIAN_POINT('Origin',(-12.1649068885786,-58.7584778814676,3.64303198860222));
#249857=CARTESIAN_POINT('Origin',(4.07480739539809E-18,1.91738721105199E-13,
2.53178198860262));
#249858=CARTESIAN_POINT('Origin',(-13.0814171332226,-61.4699285681954,2.53178198860219));
#249859=CARTESIAN_POINT('Ctrl Pts',(-12.1649068885786,-58.7584778814676,
3.77003198860222));
#249860=CARTESIAN_POINT('Ctrl Pts',(-12.2893177281503,-58.7320335411737,
3.77003198860222));
#249861=CARTESIAN_POINT('Ctrl Pts',(-12.2891314946916,-58.7320731263174,
3.64284187936946));
#249862=CARTESIAN_POINT('Ctrl Pts',(-12.1200194799674,-58.5461948427481,
3.77003198860222));
#249863=CARTESIAN_POINT('Ctrl Pts',(-12.2442448876971,-58.519984972077,
3.76980208962876));
#249864=CARTESIAN_POINT('Ctrl Pts',(-12.2530551225943,-58.5623471386713,
3.64284193928119));
#249865=CARTESIAN_POINT('Ctrl Pts',(-12.0772896710141,-58.3441042111263,
3.65553535416544));
#249866=CARTESIAN_POINT('Ctrl Pts',(-12.2013256001494,-58.3180679977531,
3.65520057834594));
#249867=CARTESIAN_POINT('Ctrl Pts',(-12.2187110949205,-58.4007711908067,
3.55127910964318));
#249868=CARTESIAN_POINT('Ctrl Pts',(-12.0535047649316,-58.2316113004781,
3.47153072139032));
#249869=CARTESIAN_POINT('Ctrl Pts',(-12.1774537884114,-58.2057612725766,
3.47122746281542));
#249870=CARTESIAN_POINT('Ctrl Pts',(-12.1995935666432,-58.3108302909898,
3.40413045901201));
#249871=CARTESIAN_POINT('Origin',(-12.0753355159227,-58.3370777047234,3.40423097483269));
#249872=CARTESIAN_POINT('Ctrl Pts',(-13.360562319248,-61.3267881959112,
2.9013417351598));
#249873=CARTESIAN_POINT('Ctrl Pts',(-13.2359003894744,-61.3537611057082,
2.90163218716348));
#249874=CARTESIAN_POINT('Ctrl Pts',(-13.2134115091888,-61.2479592423877,
2.83404198860219));
#249875=CARTESIAN_POINT('Ctrl Pts',(-13.3700210384231,-61.3712903180778,
2.82853349835321));
#249876=CARTESIAN_POINT('Ctrl Pts',(-13.2571016411964,-61.3797222373777,
2.85381483162357));
#249877=CARTESIAN_POINT('Ctrl Pts',(-13.2228703539488,-61.2924596082469,
2.79182701594243));
#249878=CARTESIAN_POINT('Ctrl Pts',(-13.3535190881765,-61.422128257289,
2.75468822073589));
#249879=CARTESIAN_POINT('Ctrl Pts',(-13.2610999767698,-61.4177900459396,
2.79286913083762));
#249880=CARTESIAN_POINT('Ctrl Pts',(-13.2173727427868,-61.3409599630867,
2.74900763297863));
#249881=CARTESIAN_POINT('Ctrl Pts',(-13.2651598666396,-61.5148770953647,
2.6395445064036));
#249882=CARTESIAN_POINT('Ctrl Pts',(-13.2123479779263,-61.489982926815,
2.69627684028835));
#249883=CARTESIAN_POINT('Ctrl Pts',(-13.1725625528863,-61.4244514636292,
2.68224356036456));
#249884=CARTESIAN_POINT('Ctrl Pts',(-13.1903059833729,-61.5568698122753,
2.59908178706352));
#249885=CARTESIAN_POINT('Ctrl Pts',(-13.1590895168687,-61.5253695547398,
2.65878704321494));
#249886=CARTESIAN_POINT('Ctrl Pts',(-13.1314678292773,-61.4592680512454,
2.65878198860219));
#249887=CARTESIAN_POINT('Ctrl Pts',(-13.1038352065721,-61.5752716937451,
2.5990817351598));
#249888=CARTESIAN_POINT('Ctrl Pts',(-13.0960702419674,-61.5387839176327,
2.65878198860219));
#249889=CARTESIAN_POINT('Ctrl Pts',(-13.0814171332226,-61.4699285681954,
2.65878198860219));
#249890=CARTESIAN_POINT('Origin',(-13.3376362544819,-61.2215544576539,2.83404198860219));
#249891=CARTESIAN_POINT('Origin',(-12.0382961820466,-58.1628213392038,3.11913648166968));
#249892=CARTESIAN_POINT('Origin',(-12.0012568480854,-57.9885649735459,2.83404198860222));
#249893=CARTESIAN_POINT('Origin',(-13.3005969715109,-61.0472983318743,3.11913648177593));
#249894=CARTESIAN_POINT('Origin',(-13.2635576885496,-60.8730422059013,3.40423097483267));
#249895=CARTESIAN_POINT('Ctrl Pts',(-11.9794294790606,-57.8830978693155,
2.90134173515983));
#249896=CARTESIAN_POINT('Ctrl Pts',(-12.1031907419151,-57.8572899778511,
2.90103711553189));
#249897=CARTESIAN_POINT('Ctrl Pts',(-12.1254815933786,-57.962160188812,
2.83404198860222));
#249898=CARTESIAN_POINT('Ctrl Pts',(-11.9699833161087,-57.8386546085354,
2.82862991747918));
#249899=CARTESIAN_POINT('Ctrl Pts',(-12.0820882677177,-57.8310944294256,
2.85314045886411));
#249900=CARTESIAN_POINT('Ctrl Pts',(-12.1160345187361,-57.9177151970025,
2.79187960999948));
#249901=CARTESIAN_POINT('Ctrl Pts',(-11.9864204851024,-57.7880992891174,
2.75470625793289));
#249902=CARTESIAN_POINT('Ctrl Pts',(-12.0782959991606,-57.7929810340974,
2.79224250381867));
#249903=CARTESIAN_POINT('Ctrl Pts',(-12.1215717318489,-57.8694789541062,
2.74901809108219));
#249904=CARTESIAN_POINT('Ctrl Pts',(-12.0746725352384,-57.6961636462596,
2.63947868311656));
#249905=CARTESIAN_POINT('Ctrl Pts',(-12.1272484490374,-57.7211944343228,
2.69595066767865));
#249906=CARTESIAN_POINT('Ctrl Pts',(-12.166599170402,-57.7867317752134,
2.68220539436021));
#249907=CARTESIAN_POINT('Ctrl Pts',(-12.1494120604575,-57.6547178110644,
2.59908178585008));
#249908=CARTESIAN_POINT('Ctrl Pts',(-12.1804827566579,-57.6862546895615,
2.658776709448));
#249909=CARTESIAN_POINT('Ctrl Pts',(-12.2078361528628,-57.7524075778592,
2.65878198860222));
#249910=CARTESIAN_POINT('Ctrl Pts',(-12.2354540642039,-57.6364522029206,
2.59908173515984));
#249911=CARTESIAN_POINT('Ctrl Pts',(-12.2432007592841,-57.6729438621905,
2.65878198860222));
#249912=CARTESIAN_POINT('Ctrl Pts',(-12.2578193919762,-57.7418065394565,
2.65878198860222));
#249913=CARTESIAN_POINT('Origin',(-12.2578193919762,-57.7418065394565,2.53178198860222));
#249914=CARTESIAN_POINT('Ctrl Pts',(-13.1739864076101,-60.4516424606488,
3.77003198860221));
#249915=CARTESIAN_POINT('Ctrl Pts',(-13.04957606559,-60.4780866951848,3.77003198860221));
#249916=CARTESIAN_POINT('Ctrl Pts',(-13.0497618007544,-60.4780472159569,
3.64284238727576));
#249917=CARTESIAN_POINT('Ctrl Pts',(-13.2193162256439,-60.6638314094602,
3.77003198860221));
#249918=CARTESIAN_POINT('Ctrl Pts',(-13.0947262769508,-60.6905041359643,
3.77025506105674));
#249919=CARTESIAN_POINT('Ctrl Pts',(-13.0858380958633,-60.6477728389722,
3.64284210641834));
#249920=CARTESIAN_POINT('Ctrl Pts',(-13.2624673401146,-60.8658323498475,
3.65553527987789));
#249921=CARTESIAN_POINT('Ctrl Pts',(-13.1376973240572,-60.8926693037143,
3.65585996533023));
#249922=CARTESIAN_POINT('Ctrl Pts',(-13.1201821075155,-60.8093487091476,
3.55127902710125));
#249923=CARTESIAN_POINT('Ctrl Pts',(-13.2864868028989,-60.9782752797347,
3.47153072139028));
#249924=CARTESIAN_POINT('Ctrl Pts',(-13.1616357172822,-61.0052918407714,
3.47182327905145));
#249925=CARTESIAN_POINT('Ctrl Pts',(-13.1392995799681,-60.8992893450418,
3.40413028377954));
#249926=CARTESIAN_POINT('Origin',(-13.1739864076101,-60.4516424606488,3.64303198860221));
#249927=CARTESIAN_POINT('Origin',(3.9977349588932E-16,1.91520059300307E-13,
2.53178198860262));
#249928=CARTESIAN_POINT('Origin',(-12.2876333308465,-57.7354693911204,2.53178198860221));
#249929=CARTESIAN_POINT('Origin',(2.37914510404509,12.7200883457658,3.64303198860271));
#249930=CARTESIAN_POINT('Origin',(-13.090590866118,-60.0590486699122,3.64299466007532));
#249931=CARTESIAN_POINT('Ctrl Pts',(-12.2652136052655,-57.6301266171957,
2.59908173515984));
#249932=CARTESIAN_POINT('Ctrl Pts',(-12.2729791421549,-57.6666142715154,
2.65878198860222));
#249933=CARTESIAN_POINT('Ctrl Pts',(-12.2876333308465,-57.7354693911204,
2.65878198860222));
#249934=CARTESIAN_POINT('Ctrl Pts',(-12.3509528635299,-57.6118791634495,
2.59908193199748));
#249935=CARTESIAN_POINT('Ctrl Pts',(-12.3354428975789,-57.653317055794,
2.65877685806514));
#249936=CARTESIAN_POINT('Ctrl Pts',(-12.3374367183498,-57.7248602993992,
2.65878198860222));
#249937=CARTESIAN_POINT('Ctrl Pts',(-12.4353658313036,-57.6190178232951,
2.63872492669765));
#249938=CARTESIAN_POINT('Ctrl Pts',(-12.3978675338889,-57.6632723181626,
2.69532212015252));
#249939=CARTESIAN_POINT('Ctrl Pts',(-12.3886090227463,-57.739064034563,
2.68176836726592));
#249940=CARTESIAN_POINT('Ctrl Pts',(-12.554347819737,-57.6672013517151,
2.75442176402202));
#249941=CARTESIAN_POINT('Ctrl Pts',(-12.4724831634112,-57.7090592089818,
2.79203179920068));
#249942=CARTESIAN_POINT('Ctrl Pts',(-12.4639865158415,-57.7965151898604,
2.74885310748137));
#249943=CARTESIAN_POINT('Ctrl Pts',(-12.589980367881,-57.7068899568908,
2.82866089558366));
#249944=CARTESIAN_POINT('Ctrl Pts',(-12.484483837892,-57.7455787351216,
2.85316563119178));
#249945=CARTESIAN_POINT('Ctrl Pts',(-12.4887127671318,-57.838519720205,
2.79189751796654));
#249946=CARTESIAN_POINT('Ctrl Pts',(-12.5994235324466,-57.7513140650719,
2.90134173515982));
#249947=CARTESIAN_POINT('Ctrl Pts',(-12.4758649777947,-57.7780756236495,
2.90103711553188));
#249948=CARTESIAN_POINT('Ctrl Pts',(-12.4981558292581,-57.8829458346105,
2.83404198860221));
#249949=CARTESIAN_POINT('Origin',(-12.6223805745513,-57.8565410498766,2.83404198860222));
#249950=CARTESIAN_POINT('Origin',(-13.0813452322602,-60.0157999977489,3.56647653971779));
#249951=CARTESIAN_POINT('Origin',(-13.0643300858376,-59.9357500275433,3.42473028058443));
#249952=CARTESIAN_POINT('Origin',(-12.6594199084529,-58.0307974155289,3.11913648168081));
#249953=CARTESIAN_POINT('Origin',(-12.6964592423886,-58.2050537810541,3.4042309748327));
#249954=CARTESIAN_POINT('Ctrl Pts',(-12.9957275188818,-59.6130003254554,
3.3612302805844));
#249955=CARTESIAN_POINT('Ctrl Pts',(-12.8715027735886,-59.6394051101893,
3.3612302805844));
#249956=CARTESIAN_POINT('Ctrl Pts',(-12.8715027735886,-59.6394051101893,
3.2342302805844));
#249957=CARTESIAN_POINT('Ctrl Pts',(-13.0142126749438,-59.7010925481782,
3.3612302805844));
#249958=CARTESIAN_POINT('Ctrl Pts',(-12.8901994296792,-59.7273659613761,
3.36099641108416));
#249959=CARTESIAN_POINT('Ctrl Pts',(-12.8995737759689,-59.771468793191,
3.23423043688307));
#249960=CARTESIAN_POINT('Ctrl Pts',(-13.0316935695386,-59.784390000023,
3.41054258905243));
#249961=CARTESIAN_POINT('Ctrl Pts',(-12.9079667071275,-59.8109544298234,
3.41008815826071));
#249962=CARTESIAN_POINT('Ctrl Pts',(-12.926116905723,-59.8963444006322,
3.3081986730435));
#249963=CARTESIAN_POINT('Ctrl Pts',(-13.0409063549232,-59.8282880397054,
3.48823028058442));
#249964=CARTESIAN_POINT('Ctrl Pts',(-12.9173404733276,-59.8550545325309,
3.48794691941558));
#249965=CARTESIAN_POINT('Ctrl Pts',(-12.9401053405444,-59.9621548122771,
3.42473028058443));
#249966=CARTESIAN_POINT('Origin',(-12.9957275188818,-59.6130003254554,3.2342302805844));
#249967=CARTESIAN_POINT('Ctrl Pts',(-12.6735055745735,-58.0998260601479,
3.47153072139031));
#249968=CARTESIAN_POINT('Ctrl Pts',(-12.5497583678824,-58.126625491213,
3.47122746285036));
#249969=CARTESIAN_POINT('Ctrl Pts',(-12.5722680770241,-58.2316158657528,
3.40413046676745));
#249970=CARTESIAN_POINT('Ctrl Pts',(-12.6975323335627,-58.2122693395989,
3.65553813457946));
#249971=CARTESIAN_POINT('Ctrl Pts',(-12.573630004124,-58.2389340288467,
3.65520336072208));
#249972=CARTESIAN_POINT('Ctrl Pts',(-12.5913858949914,-58.3215581271244,
3.55128134519942));
#249973=CARTESIAN_POINT('Ctrl Pts',(-12.7406947165199,-58.4142696920425,
3.77003198860223));
#249974=CARTESIAN_POINT('Ctrl Pts',(-12.6165486539538,-58.4408527990774,
3.7698020931406));
#249975=CARTESIAN_POINT('Ctrl Pts',(-12.6257301953095,-58.4831353553004,
3.64284195387302));
#249976=CARTESIAN_POINT('Ctrl Pts',(-12.7860306150445,-58.6264539577983,
3.77003198860222));
#249977=CARTESIAN_POINT('Ctrl Pts',(-12.6616197898419,-58.6528982950379,
3.77003198860222));
#249978=CARTESIAN_POINT('Ctrl Pts',(-12.66180600891,-58.6528587129531,3.64284189403758));
#249979=CARTESIAN_POINT('Origin',(-12.7860306150445,-58.6264539577983,3.64303198860222));
#249980=CARTESIAN_POINT('Origin',(2.31399271319931,12.4135704460883,3.2342302805849));
#249981=CARTESIAN_POINT('Origin',(-12.9642895838864,-59.4650964698966,3.2342302805844));
#249982=CARTESIAN_POINT('Origin',(2.30379013587677,12.3655710936223,3.64303198860271));
#249983=CARTESIAN_POINT('Origin',(-12.8695280801138,-59.0190342907437,3.64299171721762));
#249984=CARTESIAN_POINT('Ctrl Pts',(-12.9191181862039,-59.2498070616279,
3.48823028058439));
#249985=CARTESIAN_POINT('Ctrl Pts',(-12.7944335023702,-59.2768226962998,
3.48852004212217));
#249986=CARTESIAN_POINT('Ctrl Pts',(-12.7714622569314,-59.168751483356,
3.42473028058439));
#249987=CARTESIAN_POINT('Ctrl Pts',(-12.9283593439864,-59.2938540730358,
3.41028005848365));
#249988=CARTESIAN_POINT('Ctrl Pts',(-12.8037411209987,-59.320611599147,
3.41074404220263));
#249989=CARTESIAN_POINT('Ctrl Pts',(-12.785497965755,-59.2347843016954,
3.30780486243861));
#249990=CARTESIAN_POINT('Ctrl Pts',(-12.9458672564,-59.3773008374012,3.3612302805844));
#249991=CARTESIAN_POINT('Ctrl Pts',(-12.8213956592928,-59.4036696715731,
3.36146460586352));
#249992=CARTESIAN_POINT('Ctrl Pts',(-12.8120883873133,-59.3598823995823,
3.23423045308352));
#249993=CARTESIAN_POINT('Ctrl Pts',(-12.9642895838864,-59.4650964698966,
3.3612302805844));
#249994=CARTESIAN_POINT('Ctrl Pts',(-12.8400648385932,-59.4915012546304,
3.3612302805844));
#249995=CARTESIAN_POINT('Ctrl Pts',(-12.8400648385932,-59.4915012546304,
3.2342302805844));
#249996=CARTESIAN_POINT('Origin',(-12.8956870022246,-59.1423466986221,3.42473028058439));
#249997=CARTESIAN_POINT('Origin',(-12.878773330973,-59.0627741301476,3.56563113524774));
#249998=CARTESIAN_POINT('Origin',(-6.10480350566428,-61.1207756556235,3.56647653909442));
#249999=CARTESIAN_POINT('Origin',(-6.1093749596214,-61.164764644046,3.64299466007773));
#250000=CARTESIAN_POINT('Origin',(-6.09624906995176,-61.0393856393803,3.42473028058441));
#250001=CARTESIAN_POINT('Ctrl Pts',(-6.08531878138258,-60.9299448846689,
3.48823028058441));
#250002=CARTESIAN_POINT('Ctrl Pts',(-6.21110821942873,-60.9172173747509,
3.48794691941557));
#250003=CARTESIAN_POINT('Ctrl Pts',(-6.22255335066354,-61.0261105245453,
3.42473028058442));
#250004=CARTESIAN_POINT('Ctrl Pts',(-6.08049918876651,-60.8851977561468,
3.41028005925044));
#250005=CARTESIAN_POINT('Ctrl Pts',(-6.20637959976652,-60.8722275639157,
3.40982512230997));
#250006=CARTESIAN_POINT('Ctrl Pts',(-6.21549684257552,-60.9589723348217,
3.30780486372864));
#250007=CARTESIAN_POINT('Ctrl Pts',(-6.0713679351627,-60.8004245407958,
3.36123028058439));
#250008=CARTESIAN_POINT('Ctrl Pts',(-6.19743126523164,-60.7870898478956,
3.36099721048403));
#250009=CARTESIAN_POINT('Ctrl Pts',(-6.20212840134644,-60.8317801127834,
3.23423045308315));
#250010=CARTESIAN_POINT('Ctrl Pts',(-6.06175884541508,-60.7112330730303,
3.36123028058439));
#250011=CARTESIAN_POINT('Ctrl Pts',(-6.18806312612685,-60.6979579581953,
3.36123028058439));
#250012=CARTESIAN_POINT('Ctrl Pts',(-6.18806312612685,-60.6979579581953,
3.23423028058439));
#250013=CARTESIAN_POINT('Origin',(-6.06175884541508,-60.7112330730303,3.23423028058438));
#250014=CARTESIAN_POINT('Origin',(0.315760701779433,-0.033187787087293,
3.64303198860263));
#250015=CARTESIAN_POINT('Origin',(-6.15137923967613,-61.5639141665611,3.64303198860219));
#250016=CARTESIAN_POINT('Origin',(0.315760701779433,-0.0331877870872902,
3.23423028058481));
#250017=CARTESIAN_POINT('Origin',(-6.04595329344999,-60.5608532912342,3.23423028058439));
#250018=CARTESIAN_POINT('Ctrl Pts',(-6.207123496544,-62.0995362748658,3.47153072139028));
#250019=CARTESIAN_POINT('Ctrl Pts',(-6.33421250060393,-62.0866494451784,
3.47182327902618));
#250020=CARTESIAN_POINT('Ctrl Pts',(-6.32269886887934,-61.9789328429855,
3.40413028958983));
#250021=CARTESIAN_POINT('Ctrl Pts',(-6.1952204063465,-61.9851725366284,
3.65553807120912));
#250022=CARTESIAN_POINT('Ctrl Pts',(-6.32217680516108,-61.9721399414743,
3.65586275496892));
#250023=CARTESIAN_POINT('Ctrl Pts',(-6.31308733464666,-61.8874852020919,
3.55128126837237));
#250024=CARTESIAN_POINT('Ctrl Pts',(-6.17383766261641,-61.7797221753252,
3.7700319886022));
#250025=CARTESIAN_POINT('Ctrl Pts',(-6.30057205577816,-61.7665890280522,
3.77025505748452));
#250026=CARTESIAN_POINT('Ctrl Pts',(-6.29582060418285,-61.7232032332915,
3.64284211731086));
#250027=CARTESIAN_POINT('Ctrl Pts',(-6.15137923967613,-61.5639141665611,
3.7700319886022));
#250028=CARTESIAN_POINT('Ctrl Pts',(-6.27787221312652,-61.5506192193201,
3.7700319886022));
#250029=CARTESIAN_POINT('Ctrl Pts',(-6.27768337964921,-61.5506390665183,
3.64284239821655));
#250030=CARTESIAN_POINT('Origin',(-6.19641157197401,-61.9923681882668,3.40423097483266));
#250031=CARTESIAN_POINT('Ctrl Pts',(-6.04595329344999,-60.5608532912342,
3.36123028058439));
#250032=CARTESIAN_POINT('Ctrl Pts',(-6.17225757416176,-60.5475781763992,
3.36123028058439));
#250033=CARTESIAN_POINT('Ctrl Pts',(-6.17225757416176,-60.5475781763992,
3.23423028058439));
#250034=CARTESIAN_POINT('Ctrl Pts',(-6.03631114774991,-60.4713604300107,
3.36123028058439));
#250035=CARTESIAN_POINT('Ctrl Pts',(-6.16283986559452,-60.4579746647647,
3.36146538610082));
#250036=CARTESIAN_POINT('Ctrl Pts',(-6.15814476024311,-60.4133037213026,
3.23423043688355));
#250037=CARTESIAN_POINT('Ctrl Pts',(-6.02719193013319,-60.3867383361557,
3.4105425869306));
#250038=CARTESIAN_POINT('Ctrl Pts',(-6.15397990991512,-60.3736778173753,
3.4110060885966));
#250039=CARTESIAN_POINT('Ctrl Pts',(-6.14480008848946,-60.2863376507164,
3.30819866970773));
#250040=CARTESIAN_POINT('Ctrl Pts',(-6.02238575970214,-60.3421421670674,
3.48823028058439));
#250041=CARTESIAN_POINT('Ctrl Pts',(-6.14931623097185,-60.329305876221,
3.48852004212216));
#250042=CARTESIAN_POINT('Ctrl Pts',(-6.13776734223154,-60.2194255397044,
3.42473028058438));
#250043=CARTESIAN_POINT('Origin',(-6.01146306151977,-60.2327006545394,3.42473028058439));
#250044=CARTESIAN_POINT('Origin',(-6.21503322485571,-62.1695413802865,3.11913648178484));
#250045=CARTESIAN_POINT('Origin',(-6.23365487766561,-62.3467145720968,2.83404198860218));
#250046=CARTESIAN_POINT('Origin',(-6.00295964302102,-60.1517960317838,3.56563113460705));
#250047=CARTESIAN_POINT('Origin',(-5.99823604520072,-60.1073400339997,3.64299171721757));
#250048=CARTESIAN_POINT('Ctrl Pts',(-6.56531752495238,-62.6108711573004,
2.5990817351598));
#250049=CARTESIAN_POINT('Ctrl Pts',(-6.56142710223288,-62.5737697140401,
2.65878198860218));
#250050=CARTESIAN_POINT('Ctrl Pts',(-6.55408556365882,-62.5037563256533,
2.65878198860218));
#250051=CARTESIAN_POINT('Ctrl Pts',(-6.4776825960902,-62.6200603487605,
2.59908193475532));
#250052=CARTESIAN_POINT('Ctrl Pts',(-6.49759225479898,-62.5804601312021,
2.65878715325233));
#250053=CARTESIAN_POINT('Ctrl Pts',(-6.50335812634735,-62.5090664195404,
2.65878198860218));
#250054=CARTESIAN_POINT('Ctrl Pts',(-6.39420891953701,-62.6036598373287,
2.63878778849862));
#250055=CARTESIAN_POINT('Ctrl Pts',(-6.43639040357881,-62.5636211788246,
2.69564460180056));
#250056=CARTESIAN_POINT('Ctrl Pts',(-6.45393802799965,-62.4890871199576,
2.68180481624838));
#250057=CARTESIAN_POINT('Ctrl Pts',(-6.28054002958074,-62.5425397295635,
2.75443238878567));
#250058=CARTESIAN_POINT('Ctrl Pts',(-6.36702405212719,-62.5098176621811,
2.79268340777068));
#250059=CARTESIAN_POINT('Ctrl Pts',(-6.38494336730917,-62.4232722595961,
2.74885926835567));
#250060=CARTESIAN_POINT('Ctrl Pts',(-6.24912387034406,-62.4991087455373,
2.82856655361656));
#250061=CARTESIAN_POINT('Ctrl Pts',(-6.35913125763714,-62.4722367740483,
2.85384197230787));
#250062=CARTESIAN_POINT('Ctrl Pts',(-6.36471246584659,-62.3786641568868,
2.79184624278385));
#250063=CARTESIAN_POINT('Ctrl Pts',(-6.24436990787996,-62.4538823482274,
2.90134173515979));
#250064=CARTESIAN_POINT('Ctrl Pts',(-6.37126553604007,-62.4410124550017,
2.90163218716347));
#250065=CARTESIAN_POINT('Ctrl Pts',(-6.35995915837738,-62.3334394572618,
2.83404198860218));
#250066=CARTESIAN_POINT('Origin',(-6.55408556365882,-62.5037563256533,2.53178198860217));
#250067=CARTESIAN_POINT('Origin',(0.315760701779433,-0.033187787087293,
3.64303198860263));
#250068=CARTESIAN_POINT('Origin',(-5.9563328589115,-59.7081718144891,3.64303198860221));
#250069=CARTESIAN_POINT('Origin',(-1.29720108988958E-17,1.91741421055974E-13,
2.53178198860262));
#250070=CARTESIAN_POINT('Origin',(-6.58439859102965,-62.5005702980929,2.53178198860218));
#250071=CARTESIAN_POINT('Ctrl Pts',(-5.9563328589115,-59.7081718144891,
3.77003198860222));
#250072=CARTESIAN_POINT('Ctrl Pts',(-6.08282634913932,-59.6948768129326,
3.77003198860221));
#250073=CARTESIAN_POINT('Ctrl Pts',(-6.08263699811322,-59.6948967145274,
3.64284187936994));
#250074=CARTESIAN_POINT('Ctrl Pts',(-5.9338809680361,-59.4923596726252,
3.77003198860222));
#250075=CARTESIAN_POINT('Ctrl Pts',(-6.06016553348731,-59.4792784733341,
3.76980208962856));
#250076=CARTESIAN_POINT('Ctrl Pts',(-6.06449945282193,-59.5223294958618,
3.64284193928205));
#250077=CARTESIAN_POINT('Ctrl Pts',(-5.91250946061122,-59.2869096333628,
3.65553535416543));
#250078=CARTESIAN_POINT('Ctrl Pts',(-6.03858743332082,-59.2739813341569,
3.6552005783451));
#250079=CARTESIAN_POINT('Ctrl Pts',(-6.04723285085718,-59.3580487495168,
3.55127910964222));
#250080=CARTESIAN_POINT('Ctrl Pts',(-5.90061356181196,-59.1725467709676,
3.47153072139032));
#250081=CARTESIAN_POINT('Ctrl Pts',(-6.02658564326364,-59.1597945531716,
3.47122746281542));
#250082=CARTESIAN_POINT('Ctrl Pts',(-6.03762143444245,-59.2666022295036,
3.40413045901226));
#250083=CARTESIAN_POINT('Origin',(-5.91130048050282,-59.2797173540685,3.40423097483269));
#250084=CARTESIAN_POINT('Ctrl Pts',(-6.87697683366501,-62.387392681069,
2.9013417351598));
#250085=CARTESIAN_POINT('Ctrl Pts',(-6.75017837817539,-62.4011871104967,
2.90163218716347));
#250086=CARTESIAN_POINT('Ctrl Pts',(-6.7388720005127,-62.2936141127568,
2.83404198860218));
#250087=CARTESIAN_POINT('Ctrl Pts',(-6.88173199854423,-62.432639721334,
2.82853349835313));
#250088=CARTESIAN_POINT('Ctrl Pts',(-6.76854981002423,-62.4292221586326,
2.85381483162327));
#250089=CARTESIAN_POINT('Ctrl Pts',(-6.74362747387351,-62.3388594194639,
2.79182701594337));
#250090=CARTESIAN_POINT('Ctrl Pts',(-6.86000643604651,-62.4814742414945,
2.75468822073597));
#250091=CARTESIAN_POINT('Ctrl Pts',(-6.76854707276773,-62.467499367628,
2.79286913083797));
#250092=CARTESIAN_POINT('Ctrl Pts',(-6.73309031164111,-62.3865194274372,
2.74900763297861));
#250093=CARTESIAN_POINT('Ctrl Pts',(-6.76243636205652,-62.5644789380881,
2.63954450640351));
#250094=CARTESIAN_POINT('Ctrl Pts',(-6.71251593157837,-62.5342007968298,
2.69627684028813));
#250095=CARTESIAN_POINT('Ctrl Pts',(-6.67979835840198,-62.4648696125157,
2.68224356036455));
#250096=CARTESIAN_POINT('Ctrl Pts',(-6.68360310202745,-62.5984172531152,
2.59908178706191));
#250097=CARTESIAN_POINT('Ctrl Pts',(-6.6558503161057,-62.5638265480139,
2.65878704321527));
#250098=CARTESIAN_POINT('Ctrl Pts',(-6.63528943158894,-62.4951999029145,
2.65878198860218));
#250099=CARTESIAN_POINT('Ctrl Pts',(-6.59568250079822,-62.6076796697353,
2.5990817351598));
#250100=CARTESIAN_POINT('Ctrl Pts',(-6.5917740846471,-62.5705801176608,
2.65878198860217));
#250101=CARTESIAN_POINT('Ctrl Pts',(-6.58439859102965,-62.500570298093,
2.65878198860218));
#250102=CARTESIAN_POINT('Origin',(-6.86517628122447,-62.2803389979218,2.83404198860218));
#250103=CARTESIAN_POINT('Origin',(-5.89267880207724,-59.102543918501,3.11913648166976));
#250104=CARTESIAN_POINT('Origin',(-5.87405712357809,-58.9253704827879,2.83404198860221));
#250105=CARTESIAN_POINT('Origin',(-6.84655462836752,-62.1031658060995,3.11913648177431));
#250106=CARTESIAN_POINT('Origin',(-6.82793297553286,-61.9259926140918,3.40423097483267));
#250107=CARTESIAN_POINT('Ctrl Pts',(-5.8633736414952,-58.8181995570483,
2.90134173515982));
#250108=CARTESIAN_POINT('Ctrl Pts',(-5.98915458643734,-58.8054696185319,
2.90103711553188));
#250109=CARTESIAN_POINT('Ctrl Pts',(-6.00036140428986,-58.9120953679529,
2.8340419886022));
#250110=CARTESIAN_POINT('Ctrl Pts',(-5.85862481136399,-58.7730123682038,
2.82862991747912));
#250111=CARTESIAN_POINT('Ctrl Pts',(-5.97090589422232,-58.7772117628634,
2.85314045886394));
#250112=CARTESIAN_POINT('Ctrl Pts',(-5.99561184840453,-58.8669063622641,
2.79187960999894));
#250113=CARTESIAN_POINT('Ctrl Pts',(-5.8802564056751,-58.7244521481308,
2.75470625793301));
#250114=CARTESIAN_POINT('Ctrl Pts',(-5.9711183347532,-58.7389107566975,
2.79224250381853));
#250115=CARTESIAN_POINT('Ctrl Pts',(-6.00616078842832,-58.8195131589315,
2.7490180910822));
#250116=CARTESIAN_POINT('Ctrl Pts',(-5.97763489331392,-58.6422449895247,
2.63947868311641));
#250117=CARTESIAN_POINT('Ctrl Pts',(-6.02730636094564,-58.6726343357861,
2.69595066767874));
#250118=CARTESIAN_POINT('Ctrl Pts',(-6.05959099741106,-58.7419259266983,
2.68220539436018));
#250119=CARTESIAN_POINT('Ctrl Pts',(-6.05629725705559,-58.6088386066676,
2.59908178584968));
#250120=CARTESIAN_POINT('Ctrl Pts',(-6.0839012432855,-58.6434504949714,
2.65877670944779));
#250121=CARTESIAN_POINT('Ctrl Pts',(-6.10418993496956,-58.7121001992951,
2.65878198860221));
#250122=CARTESIAN_POINT('Ctrl Pts',(-6.14377718965262,-58.5996668978647,
2.59908173515982));
#250123=CARTESIAN_POINT('Ctrl Pts',(-6.14766703046111,-58.6367684021391,
2.6587819886022));
#250124=CARTESIAN_POINT('Ctrl Pts',(-6.15500747092256,-58.7067819056642,
2.65878198860221));
#250125=CARTESIAN_POINT('Origin',(-6.15500747092256,-58.7067819056642,2.53178198860221));
#250126=CARTESIAN_POINT('Ctrl Pts',(-6.78290064323498,-61.4975385923861,
3.7700319886022));
#250127=CARTESIAN_POINT('Ctrl Pts',(-6.65640765888756,-61.5108335407724,
3.7700319886022));
#250128=CARTESIAN_POINT('Ctrl Pts',(-6.65659650327814,-61.5108136924271,
3.64284238727587));
#250129=CARTESIAN_POINT('Ctrl Pts',(-6.80580235504166,-61.7133034041534,
3.7700319886022));
#250130=CARTESIAN_POINT('Ctrl Pts',(-6.6791068640111,-61.7268068187958,
3.77025506105741));
#250131=CARTESIAN_POINT('Ctrl Pts',(-6.67473401011684,-61.6833805404091,
3.64284210641856));
#250132=CARTESIAN_POINT('Ctrl Pts',(-6.82760223531332,-61.9187082819377,
3.65553527987789));
#250133=CARTESIAN_POINT('Ctrl Pts',(-6.70071049690984,-61.9323562021225,
3.65585996532953));
#250134=CARTESIAN_POINT('Ctrl Pts',(-6.69200060426915,-61.8476612078223,
3.55127902710129));
#250135=CARTESIAN_POINT('Ctrl Pts',(-6.83973663030197,-62.0330459552231,
3.47153072139028));
#250136=CARTESIAN_POINT('Ctrl Pts',(-6.71274549238784,-62.0468640245948,
3.47182327905145));
#250137=CARTESIAN_POINT('Ctrl Pts',(-6.701611992752,-61.9391074595194,3.40413028377961));
#250138=CARTESIAN_POINT('Origin',(-6.78290064323498,-61.4975385923861,3.6430319886022));
#250139=CARTESIAN_POINT('Origin',(4.0583767139057E-16,1.91519098829264E-13,
2.53178198860262));
#250140=CARTESIAN_POINT('Origin',(-6.18532049829339,-58.7035958781038,2.53178198860221));
#250141=CARTESIAN_POINT('Origin',(0.364094271196318,6.50157577599512,3.64303198860267));
#250142=CARTESIAN_POINT('Origin',(-6.74099917687787,-61.0983782637168,3.64299466007654));
#250143=CARTESIAN_POINT('Ctrl Pts',(-6.17403490858961,-58.5964866834549,
2.59908173515982));
#250144=CARTESIAN_POINT('Ctrl Pts',(-6.17794390662112,-58.633586174224,
2.65878198860221));
#250145=CARTESIAN_POINT('Ctrl Pts',(-6.18532049829339,-58.7035958781038,
2.65878198860221));
#250146=CARTESIAN_POINT('Ctrl Pts',(-6.26121185652487,-58.5873013840782,
2.59908193199824));
#250147=CARTESIAN_POINT('Ctrl Pts',(-6.24145541658238,-58.6268910424079,
2.65877685806558));
#250148=CARTESIAN_POINT('Ctrl Pts',(-6.23596000968332,-58.6982507756597,
2.65878198860221));
#250149=CARTESIAN_POINT('Ctrl Pts',(-6.34441620808539,-58.603224495399,
2.63872492669768));
#250150=CARTESIAN_POINT('Ctrl Pts',(-6.30249747592639,-58.6433169201092,
2.69532212015256));
#250151=CARTESIAN_POINT('Ctrl Pts',(-6.28536729223259,-58.7177256636151,
2.68176836726592));
#250152=CARTESIAN_POINT('Ctrl Pts',(-6.45770985055622,-58.6635810738162,
2.75442176402197));
#250153=CARTESIAN_POINT('Ctrl Pts',(-6.37191831988748,-58.6966524426395,
2.79203179920061));
#250154=CARTESIAN_POINT('Ctrl Pts',(-6.35432657855756,-58.7827411889909,
2.74885310748135));
#250155=CARTESIAN_POINT('Ctrl Pts',(-6.48899861096488,-58.7067768761599,
2.82866089558365));
#250156=CARTESIAN_POINT('Ctrl Pts',(-6.38003592347285,-58.7342263230564,
2.85316563119164));
#250157=CARTESIAN_POINT('Ctrl Pts',(-6.37452670784893,-58.827100211173,
2.79189751796643));
#250158=CARTESIAN_POINT('Ctrl Pts',(-6.49374646112681,-58.7519447039087,
2.90134173515981));
#250159=CARTESIAN_POINT('Ctrl Pts',(-6.36806742857265,-58.7656442740269,
2.90103711553188));
#250160=CARTESIAN_POINT('Ctrl Pts',(-6.37927424642518,-58.8722700234479,
2.8340419886022));
#250161=CARTESIAN_POINT('Origin',(-6.50557852713695,-58.8589949086129,2.8340419886022));
#250162=CARTESIAN_POINT('Origin',(-6.73632490881102,-61.0544000804069,3.56647653971742));
#250163=CARTESIAN_POINT('Origin',(-6.72777047351062,-60.9730100652053,3.42473028058442));
#250164=CARTESIAN_POINT('Origin',(-6.52420020557653,-59.036168344315,3.1191364816805));
#250165=CARTESIAN_POINT('Origin',(-6.54282188406168,-59.2133417798935,3.40423097483269));
#250166=CARTESIAN_POINT('Ctrl Pts',(-6.69328024897394,-60.6448574988553,
3.36123028058439));
#250167=CARTESIAN_POINT('Ctrl Pts',(-6.56697596826216,-60.6581326136903,
3.36123028058439));
#250168=CARTESIAN_POINT('Ctrl Pts',(-6.56697596826216,-60.6581326136903,
3.23423028058439));
#250169=CARTESIAN_POINT('Ctrl Pts',(-6.70245599674927,-60.7343993681212,
3.36123028058439));
#250170=CARTESIAN_POINT('Ctrl Pts',(-6.57637578951115,-60.7475659388581,
3.36099641108384));
#250171=CARTESIAN_POINT('Ctrl Pts',(-6.58108878091658,-60.7924070567586,
3.23423043688315));
#250172=CARTESIAN_POINT('Ctrl Pts',(-6.71113417453891,-60.8190677588578,
3.41054258905242));
#250173=CARTESIAN_POINT('Ctrl Pts',(-6.58530836180298,-60.8325536871424,
3.41008815826015));
#250174=CARTESIAN_POINT('Ctrl Pts',(-6.5944334492835,-60.9193730951222,
3.30819867304306));
#250175=CARTESIAN_POINT('Ctrl Pts',(-6.71570789669348,-60.8636883187843,
3.48823028058441));
#250176=CARTESIAN_POINT('Ctrl Pts',(-6.59002106156404,-60.8773920302459,
3.48794691941557));
#250177=CARTESIAN_POINT('Ctrl Pts',(-6.60146619279885,-60.9862851800403,
3.42473028058442));
#250178=CARTESIAN_POINT('Origin',(-6.69328024897394,-60.6448574988553,3.23423028058439));
#250179=CARTESIAN_POINT('Ctrl Pts',(-6.53099325079995,-59.1062911958295,
3.47153072139031));
#250180=CARTESIAN_POINT('Ctrl Pts',(-6.4051226409094,-59.1200087114581,
3.47122746285036));
#250181=CARTESIAN_POINT('Ctrl Pts',(-6.41653455700065,-59.2267768430459,
3.40413046676746));
#250182=CARTESIAN_POINT('Ctrl Pts',(-6.54313486548254,-59.2206299794251,
3.65553813457947));
#250183=CARTESIAN_POINT('Ctrl Pts',(-6.4171240669808,-59.234197276625,3.65520336072176));
#250184=CARTESIAN_POINT('Ctrl Pts',(-6.42614611919671,-59.3182247474317,
3.55128134519943));
#250185=CARTESIAN_POINT('Ctrl Pts',(-6.56494601396971,-59.4260354503638,
3.77003198860222));
#250186=CARTESIAN_POINT('Ctrl Pts',(-6.43870134519636,-59.4394961352151,
3.76980209314032));
#250187=CARTESIAN_POINT('Ctrl Pts',(-6.44341285848396,-59.4825067955806,
3.64284195387329));
#250188=CARTESIAN_POINT('Ctrl Pts',(-6.58785426247035,-59.6417962403142,
3.77003198860222));
#250189=CARTESIAN_POINT('Ctrl Pts',(-6.46136078685173,-59.6550912403352,
3.77003198860222));
#250190=CARTESIAN_POINT('Ctrl Pts',(-6.46155012324679,-59.6550713402781,
3.64284189403761));
#250191=CARTESIAN_POINT('Origin',(-6.58785426247035,-59.6417962403142,3.64303198860221));
#250192=CARTESIAN_POINT('Origin',(0.347626240493858,6.34489293004856,3.23423028058486));
#250193=CARTESIAN_POINT('Origin',(-6.67747469700884,-60.4944777170593,3.23423028058439));
#250194=CARTESIAN_POINT('Origin',(0.345047419449677,6.32035708677198,3.64303198860267));
#250195=CARTESIAN_POINT('Origin',(-6.62985850077779,-60.0409538388296,3.6429917172174));
#250196=CARTESIAN_POINT('Ctrl Pts',(-6.65505462397334,-60.2756459899118,
3.48823028058439));
#250197=CARTESIAN_POINT('Ctrl Pts',(-6.52822907310716,-60.2894805317161,
3.48852004212217));
#250198=CARTESIAN_POINT('Ctrl Pts',(-6.51668018436685,-60.1796001951994,
3.42473028058438));
#250199=CARTESIAN_POINT('Ctrl Pts',(-6.65964099131231,-60.3204176712043,
3.41028005848362));
#250200=CARTESIAN_POINT('Ctrl Pts',(-6.53290851690239,-60.3340024654432,
3.4107440422026));
#250201=CARTESIAN_POINT('Ctrl Pts',(-6.52373669508263,-60.2467384099245,
3.30780486243842));
#250202=CARTESIAN_POINT('Ctrl Pts',(-6.66833043150598,-60.405237380643,
3.36123028058439));
#250203=CARTESIAN_POINT('Ctrl Pts',(-6.54178440911728,-60.4184509388167,
3.36146460586334));
#250204=CARTESIAN_POINT('Ctrl Pts',(-6.53710513959971,-60.373930663246,
3.23423045308357));
#250205=CARTESIAN_POINT('Ctrl Pts',(-6.67747469700884,-60.4944777170593,
3.36123028058439));
#250206=CARTESIAN_POINT('Ctrl Pts',(-6.55117041629707,-60.5077528318942,
3.36123028058439));
#250207=CARTESIAN_POINT('Ctrl Pts',(-6.55117041629707,-60.5077528318942,
3.23423028058439));
#250208=CARTESIAN_POINT('Origin',(-6.64298446507862,-60.1663250803644,3.42473028058439));
#250209=CARTESIAN_POINT('Origin',(-6.63448104699066,-60.0854204586806,3.56563113524721));
#250210=CARTESIAN_POINT('Origin',(0.317499999706111,-61.4240753804082,3.5664765390942));
#250211=CARTESIAN_POINT('Origin',(0.317551690013291,-61.4683012396067,3.64299466007677));
#250212=CARTESIAN_POINT('Origin',(0.317500000000648,-61.3422370451704,3.42473028058441));
#250213=CARTESIAN_POINT('Ctrl Pts',(0.316930737396561,-61.2322532920971,
3.48823028058441));
#250214=CARTESIAN_POINT('Ctrl Pts',(0.190500000000648,-61.2327440814644,
3.48794691941557));
#250215=CARTESIAN_POINT('Ctrl Pts',(0.190500000000648,-61.3422370451704,
3.42473028058442));
#250216=CARTESIAN_POINT('Ctrl Pts',(0.317046579200287,-61.1872475084172,
3.41028005925046));
#250217=CARTESIAN_POINT('Ctrl Pts',(0.190500000000573,-61.1875064541747,
3.40982512230936));
#250218=CARTESIAN_POINT('Ctrl Pts',(0.190500000000647,-61.2747290395307,
3.30780486372771));
#250219=CARTESIAN_POINT('Ctrl Pts',(0.31726659691415,-61.101984213703,3.36123028058439));
#250220=CARTESIAN_POINT('Ctrl Pts',(0.190500000000765,-61.1018997758113,
3.36099721048437));
#250221=CARTESIAN_POINT('Ctrl Pts',(0.190500000000646,-61.146836207171,
3.23423045308358));
#250222=CARTESIAN_POINT('Ctrl Pts',(0.317500000000645,-61.0122769227454,
3.36123028058439));
#250223=CARTESIAN_POINT('Ctrl Pts',(0.190500000000645,-61.0122769227454,
3.36123028058439));
#250224=CARTESIAN_POINT('Ctrl Pts',(0.190500000000645,-61.0122769227454,
3.23423028058439));
#250225=CARTESIAN_POINT('Origin',(0.317500000000645,-61.0122769227454,3.23423028058439));
#250226=CARTESIAN_POINT('Origin',(0.317500000000006,1.87143253445273E-13,
3.64303198860263));
#250227=CARTESIAN_POINT('Origin',(0.317500000000654,-61.8696548221179,3.64303198860219));
#250228=CARTESIAN_POINT('Origin',(0.317500000000006,1.89997900514936E-13,
3.23423028058481));
#250229=CARTESIAN_POINT('Origin',(0.317500000000643,-60.8610688070705,3.23423028058439));
#250230=CARTESIAN_POINT('Ctrl Pts',(0.318048871877788,-62.4081695979766,
3.47153072139028));
#250231=CARTESIAN_POINT('Ctrl Pts',(0.190309034176441,-62.4086377819833,
3.47182327902618));
#250232=CARTESIAN_POINT('Ctrl Pts',(0.190500142125711,-62.3003077603773,
3.40413028959004));
#250233=CARTESIAN_POINT('Ctrl Pts',(0.317932489890643,-62.2931881445369,
3.65553807120917));
#250234=CARTESIAN_POINT('Ctrl Pts',(0.190309294367224,-62.293497500569,
3.65586275496757));
#250235=CARTESIAN_POINT('Ctrl Pts',(0.190500141996126,-62.2083564003226,
3.55128126837138));
#250236=CARTESIAN_POINT('Ctrl Pts',(0.317722686168063,-62.0866281564671,
3.7700319886022));
#250237=CARTESIAN_POINT('Ctrl Pts',(0.190309769570757,-62.086814305312,
3.77025505748501));
#250238=CARTESIAN_POINT('Ctrl Pts',(0.190500141762521,-62.0431695205407,
3.64284211731181));
#250239=CARTESIAN_POINT('Ctrl Pts',(0.317500000000654,-61.8696548221179,
3.7700319886022));
#250240=CARTESIAN_POINT('Ctrl Pts',(0.190310267890066,-61.8696548221179,
3.7700319886022));
#250241=CARTESIAN_POINT('Ctrl Pts',(0.190500141514568,-61.8696548221179,
3.64284239821694));
#250242=CARTESIAN_POINT('Origin',(0.317500000000658,-62.3004688883553,3.40423097483266));
#250243=CARTESIAN_POINT('Ctrl Pts',(0.317500000000643,-60.8610688070705,
3.36123028058439));
#250244=CARTESIAN_POINT('Ctrl Pts',(0.190500000000643,-60.8610688070705,
3.36123028058439));
#250245=CARTESIAN_POINT('Ctrl Pts',(0.190500000000643,-60.8610688070705,
3.23423028058439));
#250246=CARTESIAN_POINT('Ctrl Pts',(0.31773477376092,-60.7710583184318,
3.36123028058438));
#250247=CARTESIAN_POINT('Ctrl Pts',(0.190500000000766,-60.7709717342426,
3.36146538610139));
#250248=CARTESIAN_POINT('Ctrl Pts',(0.190500000000642,-60.7260547307369,
3.2342304368841));
#250249=CARTESIAN_POINT('Ctrl Pts',(0.317958617919681,-60.6859465754576,
3.41054258693055));
#250250=CARTESIAN_POINT('Ctrl Pts',(0.190500000000172,-60.686210556255,
3.41100608859671));
#250251=CARTESIAN_POINT('Ctrl Pts',(0.19050000000064,-60.598389295539,3.30819866970735));
#250252=CARTESIAN_POINT('Ctrl Pts',(0.318076890624007,-60.6410923272403,
3.48823028058439));
#250253=CARTESIAN_POINT('Ctrl Pts',(0.190500000000634,-60.641594202042,
3.48852004212217));
#250254=CARTESIAN_POINT('Ctrl Pts',(0.19050000000064,-60.5311086139133,
3.42473028058439));
#250255=CARTESIAN_POINT('Origin',(0.317500000000639,-60.5311086139133,3.42473028058439));
#250256=CARTESIAN_POINT('Origin',(0.317499999979056,-62.4786179998463,3.11913648178229));
#250257=CARTESIAN_POINT('Origin',(0.317500000000662,-62.6567671111297,2.83404198860217));
#250258=CARTESIAN_POINT('Origin',(0.317499999994423,-60.4497583458796,3.56563113460789));
#250259=CARTESIAN_POINT('Origin',(0.31755080432116,-60.4050521322801,3.64299171721745));
#250260=CARTESIAN_POINT('Ctrl Pts',(0.0152661173115319,-62.9541448057646,
2.59908173515979));
#250261=CARTESIAN_POINT('Ctrl Pts',(0.0152570710392988,-62.9168399481841,
2.65878198860218));
#250262=CARTESIAN_POINT('Ctrl Pts',(0.0152400000006639,-62.8464427007194,
2.65878198860218));
#250263=CARTESIAN_POINT('Ctrl Pts',(0.10338150492588,-62.9541233134301,
2.59908193475501));
#250264=CARTESIAN_POINT('Ctrl Pts',(0.0794415635241914,-62.9168211560388,
2.65878715325371));
#250265=CARTESIAN_POINT('Ctrl Pts',(0.0662446030566008,-62.8464212442879,
2.65878198860218));
#250266=CARTESIAN_POINT('Ctrl Pts',(0.184683583688456,-62.9290872705826,
2.63878778849821));
#250267=CARTESIAN_POINT('Ctrl Pts',(0.138547994785007,-62.8936771137452,
2.69564460180082));
#250268=CARTESIAN_POINT('Ctrl Pts',(0.113305567452228,-62.8213855864653,
2.68180481624846));
#250269=CARTESIAN_POINT('Ctrl Pts',(0.291340992632371,-62.8564203507738,
2.75443238878607));
#250270=CARTESIAN_POINT('Ctrl Pts',(0.201910351191927,-62.8329175802734,
2.7926834077703));
#250271=CARTESIAN_POINT('Ctrl Pts',(0.1750427419585,-62.7487193609387,2.74885926835559));
#250272=CARTESIAN_POINT('Ctrl Pts',(0.318045276843287,-62.8099434033761,
2.82856655361622));
#250273=CARTESIAN_POINT('Ctrl Pts',(0.205831635643734,-62.7947175424999,
2.85384197230742));
#250274=CARTESIAN_POINT('Ctrl Pts',(0.190500000000664,-62.7022409210439,
2.79184624278408));
#250275=CARTESIAN_POINT('Ctrl Pts',(0.318045750793708,-62.7644678366117,
2.90134173515981));
#250276=CARTESIAN_POINT('Ctrl Pts',(0.190500000000659,-62.7649326510147,
2.90163218716348));
#250277=CARTESIAN_POINT('Ctrl Pts',(0.190500000000662,-62.6567671111297,
2.83404198860219));
#250278=CARTESIAN_POINT('Origin',(0.317500000000006,1.87143253445273E-13,
3.64303198860263));
#250279=CARTESIAN_POINT('Origin',(0.317500000000634,-60.0036905223729,3.64303198860221));
#250280=CARTESIAN_POINT('Ctrl Pts',(0.317500000000634,-60.0036905223729,
3.77003198860221));
#250281=CARTESIAN_POINT('Ctrl Pts',(0.190309748265596,-60.0036905223729,
3.77003198860221));
#250282=CARTESIAN_POINT('Ctrl Pts',(0.190500142290163,-60.0036905223729,
3.64284187936986));
#250283=CARTESIAN_POINT('Ctrl Pts',(0.31727038552505,-59.7867137603522,
3.77003198860222));
#250284=CARTESIAN_POINT('Ctrl Pts',(0.190310262476818,-59.7869045527981,
3.76980208962897));
#250285=CARTESIAN_POINT('Ctrl Pts',(0.190500142033094,-59.8301727552505,
3.6428419392825));
#250286=CARTESIAN_POINT('Ctrl Pts',(0.317049440714242,-59.5801552670726,
3.65553535416542));
#250287=CARTESIAN_POINT('Ctrl Pts',(0.190310761082648,-59.580476527185,
3.65520057834388));
#250288=CARTESIAN_POINT('Ctrl Pts',(0.190500141785736,-59.6649871046535,
3.55127910964184));
#250289=CARTESIAN_POINT('Ctrl Pts',(0.316925998273675,-59.465175436383,
3.4715307213903));
#250290=CARTESIAN_POINT('Ctrl Pts',(0.190311035335334,-59.4656607446592,
3.47122746281541));
#250291=CARTESIAN_POINT('Ctrl Pts',(0.190500141647532,-59.5730368716577,
3.40413045901222));
#250292=CARTESIAN_POINT('Origin',(0.31750000000063,-59.572876015004,3.40423097483268));
#250293=CARTESIAN_POINT('Ctrl Pts',(-0.318045750792382,-62.7644678366118,
2.9013417351598));
#250294=CARTESIAN_POINT('Ctrl Pts',(-0.190499999999336,-62.7649326510147,
2.90163218716347));
#250295=CARTESIAN_POINT('Ctrl Pts',(-0.190499999999338,-62.6567671111297,
2.83404198860218));
#250296=CARTESIAN_POINT('Ctrl Pts',(-0.318045262794514,-62.8099640589333,
2.82853349835311));
#250297=CARTESIAN_POINT('Ctrl Pts',(-0.205840330723024,-62.7947344577603,
2.85381483162217));
#250298=CARTESIAN_POINT('Ctrl Pts',(-0.190499999999339,-62.7022616416329,
2.79182701594121));
#250299=CARTESIAN_POINT('Ctrl Pts',(-0.291334117854884,-62.8562601188212,
2.75468822073599));
#250300=CARTESIAN_POINT('Ctrl Pts',(-0.201836550627177,-62.8328016940823,
2.79286913083821));
#250301=CARTESIAN_POINT('Ctrl Pts',(-0.175038734051574,-62.748559129723,
2.7490076329788));
#250302=CARTESIAN_POINT('Ctrl Pts',(-0.185622189559593,-62.9286112571069,
2.63954450640348));
#250303=CARTESIAN_POINT('Ctrl Pts',(-0.139140155999356,-62.8932808767897,
2.69627684028793));
#250304=CARTESIAN_POINT('Ctrl Pts',(-0.113848895264975,-62.8209095783123,
2.68224356036436));
#250305=CARTESIAN_POINT('Ctrl Pts',(-0.103673266462265,-62.9541233349672,
2.59908178706312));
#250306=CARTESIAN_POINT('Ctrl Pts',(-0.0796882264530914,-62.916821165302,
2.65878704321472));
#250307=CARTESIAN_POINT('Ctrl Pts',(-0.0664134143645206,-62.8464212664861,
2.65878198860218));
#250308=CARTESIAN_POINT('Ctrl Pts',(-0.0152661173102017,-62.9541448057646,
2.59908173515979));
#250309=CARTESIAN_POINT('Ctrl Pts',(-0.0152570710379694,-62.9168399481841,
2.65878198860218));
#250310=CARTESIAN_POINT('Ctrl Pts',(-0.015239999999336,-62.8464427007194,
2.65878198860218));
#250311=CARTESIAN_POINT('Origin',(-0.317499999999338,-62.6567671111297,
2.83404198860218));
#250312=CARTESIAN_POINT('Origin',(0.317499999972213,-59.3947266586248,3.11913648167007));
#250313=CARTESIAN_POINT('Origin',(0.317500000000626,-59.2165773020939,2.83404198860221));
#250314=CARTESIAN_POINT('Origin',(-0.317499999976278,-62.4786179998357,
3.11913648177568));
#250315=CARTESIAN_POINT('Origin',(-0.317499999999342,-62.3004688883553,
3.40423097483267));
#250316=CARTESIAN_POINT('Ctrl Pts',(0.316922544676314,-59.1088767419346,
2.90134173515982));
#250317=CARTESIAN_POINT('Ctrl Pts',(0.190500000000626,-59.1093642282365,
2.90103711553188));
#250318=CARTESIAN_POINT('Ctrl Pts',(0.190500000000626,-59.2165773020939,
2.8340419886022));
#250319=CARTESIAN_POINT('Ctrl Pts',(0.316922012809783,-59.0634407053228,
2.82862991747926));
#250320=CARTESIAN_POINT('Ctrl Pts',(0.205694973741507,-59.0793536643042,
2.85314045886381));
#250321=CARTESIAN_POINT('Ctrl Pts',(0.190500000000625,-59.171139382729,
2.79187960999897));
#250322=CARTESIAN_POINT('Ctrl Pts',(0.290332993455545,-59.0174076205273,
2.75470625793277));
#250323=CARTESIAN_POINT('Ctrl Pts',(0.201480151666442,-59.0412846811393,
2.79224250381859));
#250324=CARTESIAN_POINT('Ctrl Pts',(0.175054909460322,-59.1251084688119,
2.74901809108218));
#250325=CARTESIAN_POINT('Ctrl Pts',(0.184894967402272,-58.9458296250061,
2.63947868311665));
#250326=CARTESIAN_POINT('Ctrl Pts',(0.138672156931882,-58.981244577429,
2.69595066767869));
#250327=CARTESIAN_POINT('Ctrl Pts',(0.113807322598413,-59.0535312451932,
2.6822053943602));
#250328=CARTESIAN_POINT('Ctrl Pts',(0.1031716064563,-58.9208287018089,2.59908178585043));
#250329=CARTESIAN_POINT('Ctrl Pts',(0.0793367652463939,-58.958136384828,
2.65877670944839));
#250330=CARTESIAN_POINT('Ctrl Pts',(0.066335065234977,-59.0285307646514,
2.6587819886022));
#250331=CARTESIAN_POINT('Ctrl Pts',(0.015212193456543,-58.9208513795071,
2.59908173515982));
#250332=CARTESIAN_POINT('Ctrl Pts',(0.0152218248297303,-58.9581562369412,
2.65878198860221));
#250333=CARTESIAN_POINT('Ctrl Pts',(0.0152400000006241,-59.0285534841294,
2.6587819886022));
#250334=CARTESIAN_POINT('Ctrl Pts',(-0.317499999999346,-61.8696548221179,
3.7700319886022));
#250335=CARTESIAN_POINT('Ctrl Pts',(-0.190310256930768,-61.8696548221179,
3.7700319886022));
#250336=CARTESIAN_POINT('Ctrl Pts',(-0.190500141529595,-61.8696548221179,
3.64284238727532));
#250337=CARTESIAN_POINT('Ctrl Pts',(-0.317722689631596,-62.0866315324119,
3.7700319886022));
#250338=CARTESIAN_POINT('Ctrl Pts',(-0.190309758574985,-62.0868176889516,
3.77025506105797));
#250339=CARTESIAN_POINT('Ctrl Pts',(-0.190500141777577,-62.0431722165658,
3.64284210641847));
#250340=CARTESIAN_POINT('Ctrl Pts',(-0.317932491655028,-62.2931898887679,
3.6555352798779));
#250341=CARTESIAN_POINT('Ctrl Pts',(-0.190309283349165,-62.2934992458067,
3.65585996533061));
#250342=CARTESIAN_POINT('Ctrl Pts',(-0.190500142011202,-62.208357787851,
3.55127902710123));
#250343=CARTESIAN_POINT('Ctrl Pts',(-0.31804887187647,-62.4081695979766,
3.47153072139028));
#250344=CARTESIAN_POINT('Ctrl Pts',(-0.190309023145839,-62.4086377820237,
3.47182327905144));
#250345=CARTESIAN_POINT('Ctrl Pts',(-0.1905001421408,-62.3003077510783,
3.40413028377931));
#250346=CARTESIAN_POINT('Origin',(-0.317499999999346,-61.8696548221179,
3.6430319886022));
#250347=CARTESIAN_POINT('Origin',(-0.317499999999998,-4.7125364762808E-13,
3.64303198860263));
#250348=CARTESIAN_POINT('Origin',(-0.317551690011254,-61.4683012396059,
3.64299466007809));
#250349=CARTESIAN_POINT('Ctrl Pts',(-0.015212193455297,-58.9208513795071,
2.59908173515982));
#250350=CARTESIAN_POINT('Ctrl Pts',(-0.0152218248284836,-58.9581562369412,
2.6587819886022));
#250351=CARTESIAN_POINT('Ctrl Pts',(-0.0152399999993761,-59.0285534841294,
2.6587819886022));
#250352=CARTESIAN_POINT('Ctrl Pts',(-0.102871702176794,-58.9208288705613,
2.59908193199802));
#250353=CARTESIAN_POINT('Ctrl Pts',(-0.0790852439328077,-58.9581365422923,
2.65877685806533));
#250354=CARTESIAN_POINT('Ctrl Pts',(-0.0661608181919111,-59.0285309330207,
2.6587819886022));
#250355=CARTESIAN_POINT('Ctrl Pts',(-0.183955833236869,-58.9453619764181,
2.63872492669755));
#250356=CARTESIAN_POINT('Ctrl Pts',(-0.138075936735338,-58.9808530699759,
2.69532212015228));
#250357=CARTESIAN_POINT('Ctrl Pts',(-0.113261762367514,-59.0530636028224,
2.68176836726592));
#250358=CARTESIAN_POINT('Ctrl Pts',(-0.290319860890052,-59.0172303255292,
2.75442176402209));
#250359=CARTESIAN_POINT('Ctrl Pts',(-0.201541405841324,-59.041152869072,
2.79203179920101));
#250360=CARTESIAN_POINT('Ctrl Pts',(-0.175047309550586,-59.1249311745755,
2.74885310748134));
#250361=CARTESIAN_POINT('Ctrl Pts',(-0.316922027356719,-59.063460062791,
2.82866089558356));
#250362=CARTESIAN_POINT('Ctrl Pts',(-0.20568700036596,-59.0793694364685,
2.85316563119101));
#250363=CARTESIAN_POINT('Ctrl Pts',(-0.190499999999374,-59.1711586818657,
2.79189751796571));
#250364=CARTESIAN_POINT('Ctrl Pts',(-0.316922544675064,-59.1088767419346,
2.90134173515982));
#250365=CARTESIAN_POINT('Ctrl Pts',(-0.190499999999374,-59.1093642282365,
2.90103711553188));
#250366=CARTESIAN_POINT('Ctrl Pts',(-0.190499999999374,-59.2165773020939,
2.8340419886022));
#250367=CARTESIAN_POINT('Origin',(-0.317499999999374,-59.2165773020939,
2.8340419886022));
#250368=CARTESIAN_POINT('Origin',(-0.317499999993643,-61.4240753793289,
3.56647653971734));
#250369=CARTESIAN_POINT('Origin',(-0.317499999999352,-61.3422370451704,
3.42473028058442));
#250370=CARTESIAN_POINT('Origin',(-0.317499999969443,-59.3947266586082,
3.11913648168042));
#250371=CARTESIAN_POINT('Origin',(-0.31749999999937,-59.572876015004,3.40423097483268));
#250372=CARTESIAN_POINT('Ctrl Pts',(-0.317499999999355,-61.0122769227454,
3.36123028058439));
#250373=CARTESIAN_POINT('Ctrl Pts',(-0.190499999999355,-61.0122769227454,
3.36123028058439));
#250374=CARTESIAN_POINT('Ctrl Pts',(-0.190499999999355,-61.0122769227454,
3.23423028058439));
#250375=CARTESIAN_POINT('Ctrl Pts',(-0.317265808075734,-61.1022873990969,
3.36123028058439));
#250376=CARTESIAN_POINT('Ctrl Pts',(-0.190499999999337,-61.1022028716725,
3.36099641108441));
#250377=CARTESIAN_POINT('Ctrl Pts',(-0.190499999999354,-61.1472909869853,
3.2342304368835));
#250378=CARTESIAN_POINT('Ctrl Pts',(-0.317046189128469,-61.1873990841183,
3.41054258905241));
#250379=CARTESIAN_POINT('Ctrl Pts',(-0.190499999999407,-61.1876587562293,
3.41008815826042));
#250380=CARTESIAN_POINT('Ctrl Pts',(-0.190499999999353,-61.274956389781,
3.30819867304318));
#250381=CARTESIAN_POINT('Ctrl Pts',(-0.316930737395267,-61.2322532920971,
3.48823028058441));
#250382=CARTESIAN_POINT('Ctrl Pts',(-0.190499999999352,-61.2327440814644,
3.48794691941557));
#250383=CARTESIAN_POINT('Ctrl Pts',(-0.190499999999352,-61.3422370451704,
3.42473028058442));
#250384=CARTESIAN_POINT('Origin',(-0.317499999999355,-61.0122769227454,
3.23423028058439));
#250385=CARTESIAN_POINT('Ctrl Pts',(-0.316925998272419,-59.465175436383,
3.47153072139031));
#250386=CARTESIAN_POINT('Ctrl Pts',(-0.19031104992418,-59.4656607446032,
3.47122746285036));
#250387=CARTESIAN_POINT('Ctrl Pts',(-0.190500141624417,-59.5730368592471,
3.40413046676735));
#250388=CARTESIAN_POINT('Ctrl Pts',(-0.317049442578568,-59.5801570044829,
3.65553813457941));
#250389=CARTESIAN_POINT('Ctrl Pts',(-0.190310775687915,-59.5804782634818,
3.65520336072243));
#250390=CARTESIAN_POINT('Ctrl Pts',(-0.190500141762601,-59.6649884842686,
3.5512813451993));
#250391=CARTESIAN_POINT('Ctrl Pts',(-0.317270389088207,-59.7867171285934,
3.77003198860222));
#250392=CARTESIAN_POINT('Ctrl Pts',(-0.190310277117269,-59.7869079131857,
3.76980209314134));
#250393=CARTESIAN_POINT('Ctrl Pts',(-0.190500142009918,-59.8301754438947,
3.64284195387351));
#250394=CARTESIAN_POINT('Ctrl Pts',(-0.317499999999366,-60.0036905223729,
3.77003198860221));
#250395=CARTESIAN_POINT('Ctrl Pts',(-0.190309762953857,-60.0036905223729,
3.77003198860221));
#250396=CARTESIAN_POINT('Ctrl Pts',(-0.19050014226694,-60.0036905223729,
3.64284189403738));
#250397=CARTESIAN_POINT('Origin',(-0.317499999999366,-60.0036905223729,
3.64303198860221));
#250398=CARTESIAN_POINT('Origin',(-0.317499999999991,-4.52611858510147E-13,
3.23423028058481));
#250399=CARTESIAN_POINT('Origin',(-0.317499999999357,-60.8610688070705,
3.23423028058439));
#250400=CARTESIAN_POINT('Origin',(-0.317499999999991,-4.52994308698643E-13,
3.64303198860263));
#250401=CARTESIAN_POINT('Origin',(-0.317550804320116,-60.4050521322799,
3.64299171721719));
#250402=CARTESIAN_POINT('Ctrl Pts',(-0.318076890622726,-60.6410923272403,
3.48823028058439));
#250403=CARTESIAN_POINT('Ctrl Pts',(-0.19049999999936,-60.641594202042,
3.48852004212217));
#250404=CARTESIAN_POINT('Ctrl Pts',(-0.19049999999936,-60.5311086139133,
3.42473028058439));
#250405=CARTESIAN_POINT('Ctrl Pts',(-0.317958218318119,-60.6860981505082,
3.41028005848366));
#250406=CARTESIAN_POINT('Ctrl Pts',(-0.190499999999408,-60.6863613750271,
3.41074404220247));
#250407=CARTESIAN_POINT('Ctrl Pts',(-0.19049999999936,-60.5986166446941,
3.30780486243807));
#250408=CARTESIAN_POINT('Ctrl Pts',(-0.317733982966898,-60.7713615025338,
3.36123028058439));
#250409=CARTESIAN_POINT('Ctrl Pts',(-0.190499999999476,-60.7712750141999,
3.36146460586369));
#250410=CARTESIAN_POINT('Ctrl Pts',(-0.190499999999358,-60.7265095085059,
3.23423045308392));
#250411=CARTESIAN_POINT('Ctrl Pts',(-0.317499999999357,-60.8610688070705,
3.36123028058439));
#250412=CARTESIAN_POINT('Ctrl Pts',(-0.190499999999357,-60.8610688070705,
3.36123028058439));
#250413=CARTESIAN_POINT('Ctrl Pts',(-0.190499999999357,-60.8610688070705,
3.23423028058439));
#250414=CARTESIAN_POINT('Origin',(-0.31749999999936,-60.5311086139133,3.42473028058439));
#250415=CARTESIAN_POINT('Origin',(-0.317500000300995,-60.4497583469871,
3.5656311352473));
#250416=CARTESIAN_POINT('Origin',(6.7363249086388,-61.0544000815102,3.56647653909427));
#250417=CARTESIAN_POINT('Origin',(6.74099917687956,-61.098378263717,3.64299466007584));
#250418=CARTESIAN_POINT('Origin',(6.72777047351185,-60.9730100652052,3.42473028058441));
#250419=CARTESIAN_POINT('Ctrl Pts',(6.71570789669471,-60.8636883187842,
3.48823028058441));
#250420=CARTESIAN_POINT('Ctrl Pts',(6.59002106156527,-60.8773920302458,
3.48794691941557));
#250421=CARTESIAN_POINT('Ctrl Pts',(6.60146619280008,-60.9862851800402,
3.42473028058442));
#250422=CARTESIAN_POINT('Ctrl Pts',(6.71111871849912,-60.8189169727306,
3.41028005925045));
#250423=CARTESIAN_POINT('Ctrl Pts',(6.58529244190302,-60.8324022194098,
3.40982512231001));
#250424=CARTESIAN_POINT('Ctrl Pts',(6.59440968471205,-60.9191469903165,
3.30780486372833));
#250425=CARTESIAN_POINT('Ctrl Pts',(6.70242508976298,-60.7340977611526,
3.36123028058439));
#250426=CARTESIAN_POINT('Ctrl Pts',(6.57634410736829,-60.7472645033911,
3.36099721048417));
#250427=CARTESIAN_POINT('Ctrl Pts',(6.58104124348299,-60.7919547682783,
3.23423045308359));
#250428=CARTESIAN_POINT('Ctrl Pts',(6.69328024897516,-60.6448574988552,
3.36123028058439));
#250429=CARTESIAN_POINT('Ctrl Pts',(6.56697596826339,-60.6581326136902,
3.36123028058439));
#250430=CARTESIAN_POINT('Ctrl Pts',(6.56697596826339,-60.6581326136902,
3.23423028058439));
#250431=CARTESIAN_POINT('Origin',(6.69328024897516,-60.6448574988552,3.23423028058439));
#250432=CARTESIAN_POINT('Origin',(0.315760701779432,0.033187787087667,3.64303198860263));
#250433=CARTESIAN_POINT('Origin',(6.78290064323623,-61.497538592386,3.64303198860219));
#250434=CARTESIAN_POINT('Origin',(0.315760701779432,0.0331877870876699,
3.23423028058481));
#250435=CARTESIAN_POINT('Origin',(6.67747469701007,-60.4944777170591,3.23423028058439));
#250436=CARTESIAN_POINT('Ctrl Pts',(6.83973663030323,-62.033045955223,3.47153072139027));
#250437=CARTESIAN_POINT('Ctrl Pts',(6.71274550335325,-62.0468640234017,
3.47182327902618));
#250438=CARTESIAN_POINT('Ctrl Pts',(6.7016119937089,-61.9391074687686,3.40413028959007));
#250439=CARTESIAN_POINT('Ctrl Pts',(6.827602051236,-61.9187065474463,3.6555380712091));
#250440=CARTESIAN_POINT('Ctrl Pts',(6.70071032544549,-61.9323544652987,
3.65586275496805));
#250441=CARTESIAN_POINT('Ctrl Pts',(6.69200045921809,-61.8476598278984,
3.55128126837131));
#250442=CARTESIAN_POINT('Ctrl Pts',(6.80580199871532,-61.7133000470643,
3.7700319886022));
#250443=CARTESIAN_POINT('Ctrl Pts',(6.67910652125957,-61.7268034525388,
3.77025505748433));
#250444=CARTESIAN_POINT('Ctrl Pts',(6.67473372829026,-61.6833778591529,
3.64284211731188));
#250445=CARTESIAN_POINT('Ctrl Pts',(6.78290064323623,-61.497538592386,3.7700319886022));
#250446=CARTESIAN_POINT('Ctrl Pts',(6.65640766978628,-61.5108335396269,
3.7700319886022));
#250447=CARTESIAN_POINT('Ctrl Pts',(6.65659650326314,-61.5108136924287,
3.64284239821701));
#250448=CARTESIAN_POINT('Origin',(6.82793297553411,-61.9259926140917,3.40423097483266));
#250449=CARTESIAN_POINT('Ctrl Pts',(6.67747469701007,-60.4944777170591,
3.36123028058439));
#250450=CARTESIAN_POINT('Ctrl Pts',(6.5511704162983,-60.5077528318941,3.36123028058439));
#250451=CARTESIAN_POINT('Ctrl Pts',(6.5511704162983,-60.5077528318941,3.23423028058439));
#250452=CARTESIAN_POINT('Ctrl Pts',(6.66829952659989,-60.4049357747548,
3.36123028058439));
#250453=CARTESIAN_POINT('Ctrl Pts',(6.54175270773107,-60.4181493202578,
3.36146538610129));
#250454=CARTESIAN_POINT('Ctrl Pts',(6.5370576023796,-60.373478376797,3.2342304368841));
#250455=CARTESIAN_POINT('Ctrl Pts',(6.65962554481757,-60.320266884728,3.41054258693058));
#250456=CARTESIAN_POINT('Ctrl Pts',(6.53289275205065,-60.3338524728728,
3.41100608859687));
#250457=CARTESIAN_POINT('Ctrl Pts',(6.52371293062606,-60.2465123062119,
3.30819866970745));
#250458=CARTESIAN_POINT('Ctrl Pts',(6.65505462397456,-60.2756459899116,
3.48823028058439));
#250459=CARTESIAN_POINT('Ctrl Pts',(6.52822907310839,-60.2894805317159,
3.48852004212217));
#250460=CARTESIAN_POINT('Ctrl Pts',(6.51668018436807,-60.1796001951993,
3.42473028058438));
#250461=CARTESIAN_POINT('Origin',(6.64298446507984,-60.1663250803643,3.42473028058439));
#250462=CARTESIAN_POINT('Origin',(6.84655462836866,-62.1031658061142,3.11913648178355));
#250463=CARTESIAN_POINT('Origin',(6.86517628122572,-62.2803389979217,2.83404198860218));
#250464=CARTESIAN_POINT('Origin',(6.63448104656917,-60.0854204576119,3.56563113460814));
#250465=CARTESIAN_POINT('Origin',(6.62985850077906,-60.0409538388293,3.64299171721731));
#250466=CARTESIAN_POINT('Ctrl Pts',(6.59568250079948,-62.6076796697352,
2.5990817351598));
#250467=CARTESIAN_POINT('Ctrl Pts',(6.59177408464837,-62.5705801176607,
2.65878198860218));
#250468=CARTESIAN_POINT('Ctrl Pts',(6.58439859103091,-62.5005702980928,
2.65878198860218));
#250469=CARTESIAN_POINT('Ctrl Pts',(6.68331293653995,-62.5984477290791,
2.59908193475685));
#250470=CARTESIAN_POINT('Ctrl Pts',(6.65560500345326,-62.5638523220913,
2.65878715325371));
#250471=CARTESIAN_POINT('Ctrl Pts',(6.63512154272684,-62.4952175264254,
2.65878198860218));
#250472=CARTESIAN_POINT('Ctrl Pts',(6.76155265492332,-62.5650504549415,
2.63878778849831));
#250473=CARTESIAN_POINT('Ctrl Pts',(6.71196843232464,-62.5346567608584,
2.69564460180095));
#250474=CARTESIAN_POINT('Ctrl Pts',(6.67930776339634,-62.4653998062673,
2.68180481624849));
#250475=CARTESIAN_POINT('Ctrl Pts',(6.86003002196326,-62.4816328770698,
2.754432388786));
#250476=CARTESIAN_POINT('Ctrl Pts',(6.76863258245117,-62.4676069047241,
2.79268340777016));
#250477=CARTESIAN_POINT('Ctrl Pts',(6.73311104631516,-62.3866783619493,
2.74885926835558));
#250478=CARTESIAN_POINT('Ctrl Pts',(6.88172985342223,-62.4326191774616,
2.82856655361629));
#250479=CARTESIAN_POINT('Ctrl Pts',(6.76853939445093,-62.4292062449167,
2.85384197230755));
#250480=CARTESIAN_POINT('Ctrl Pts',(6.74362530798327,-62.3388388123827,
2.79184624278459));
#250481=CARTESIAN_POINT('Ctrl Pts',(6.87697683366627,-62.3873926810689,
2.90134173515981));
#250482=CARTESIAN_POINT('Ctrl Pts',(6.75017837817664,-62.4011871104966,
2.90163218716348));
#250483=CARTESIAN_POINT('Ctrl Pts',(6.73887200051396,-62.2936141127567,
2.83404198860219));
#250484=CARTESIAN_POINT('Origin',(6.58439859103091,-62.5005702980928,2.53178198860218));
#250485=CARTESIAN_POINT('Origin',(0.315760701779432,0.033187787087667,3.64303198860263));
#250486=CARTESIAN_POINT('Origin',(6.58785426247156,-59.641796240314,3.64303198860221));
#250487=CARTESIAN_POINT('Origin',(5.64744126194171E-15,1.86046536471642E-13,
2.53178198860262));
#250488=CARTESIAN_POINT('Origin',(6.55408556366009,-62.5037563256532,2.53178198860218));
#250489=CARTESIAN_POINT('Ctrl Pts',(6.58785426247156,-59.641796240314,3.77003198860222));
#250490=CARTESIAN_POINT('Ctrl Pts',(6.46136077224366,-59.6550912418705,
3.77003198860221));
#250491=CARTESIAN_POINT('Ctrl Pts',(6.46155012326984,-59.6550713402757,
3.64284187936987));
#250492=CARTESIAN_POINT('Ctrl Pts',(6.56494565834935,-59.4260321009466,
3.77003198860222));
#250493=CARTESIAN_POINT('Ctrl Pts',(6.43870097938032,-59.4394927947704,
3.76980208962893));
#250494=CARTESIAN_POINT('Ctrl Pts',(6.44341257746724,-59.482504121664,3.64284193928254));
#250495=CARTESIAN_POINT('Ctrl Pts',(6.54313468201992,-59.2206282517274,
3.65553535416544));
#250496=CARTESIAN_POINT('Ctrl Pts',(6.41712387096409,-59.2341955513611,
3.65520057834401));
#250497=CARTESIAN_POINT('Ctrl Pts',(6.42614597501047,-59.3182233753705,
3.55127910964182));
#250498=CARTESIAN_POINT('Ctrl Pts',(6.53099325080115,-59.1062911958294,
3.47153072139032));
#250499=CARTESIAN_POINT('Ctrl Pts',(6.40512262640605,-59.1200087130387,
3.47122746281542));
#250500=CARTESIAN_POINT('Ctrl Pts',(6.41653455832087,-59.2267768553863,
3.40413045901223));
#250501=CARTESIAN_POINT('Origin',(6.54282188406287,-59.2133417798934,3.40423097483269));
#250502=CARTESIAN_POINT('Ctrl Pts',(6.24436990788122,-62.4538823482273,
2.90134173515981));
#250503=CARTESIAN_POINT('Ctrl Pts',(6.37126553604134,-62.4410124550016,
2.90163218716348));
#250504=CARTESIAN_POINT('Ctrl Pts',(6.35995915837864,-62.3334394572616,
2.83404198860219));
#250505=CARTESIAN_POINT('Ctrl Pts',(6.24912604340991,-62.4991292864729,
2.82853349835311));
#250506=CARTESIAN_POINT('Ctrl Pts',(6.3591243783167,-62.4722545055298,2.853814831623));
#250507=CARTESIAN_POINT('Ctrl Pts',(6.36471463173932,-62.3786847639674,
2.79182701594183));
#250508=CARTESIAN_POINT('Ctrl Pts',(6.28053011789794,-62.5423796567681,
2.75468822073602));
#250509=CARTESIAN_POINT('Ctrl Pts',(6.36708533499931,-62.5096946965654,
2.79286913083812));
#250510=CARTESIAN_POINT('Ctrl Pts',(6.38493060453764,-62.4231124872026,
2.74900763297871));
#250511=CARTESIAN_POINT('Ctrl Pts',(6.39322569848958,-62.6032845425343,
2.63954450640347));
#250512=CARTESIAN_POINT('Ctrl Pts',(6.4357600682454,-62.5632890101999,2.69627684028802));
#250513=CARTESIAN_POINT('Ctrl Pts',(6.45334792019265,-62.4886705126493,
2.68224356036447));
#250514=CARTESIAN_POINT('Ctrl Pts',(6.47739243510548,-62.6200908675648,
2.59908178706328));
#250515=CARTESIAN_POINT('Ctrl Pts',(6.49734694408407,-62.5804859237133,
2.65878704321479));
#250516=CARTESIAN_POINT('Ctrl Pts',(6.50319024212579,-62.509084087203,2.65878198860219));
#250517=CARTESIAN_POINT('Ctrl Pts',(6.56531752495365,-62.6108711573003,
2.5990817351598));
#250518=CARTESIAN_POINT('Ctrl Pts',(6.56142710223415,-62.5737697140399,
2.65878198860219));
#250519=CARTESIAN_POINT('Ctrl Pts',(6.55408556366009,-62.5037563256532,
2.65878198860219));
#250520=CARTESIAN_POINT('Origin',(6.23365487766687,-62.3467145720966,2.83404198860219));
#250521=CARTESIAN_POINT('Origin',(6.52420020557853,-59.0361683443313,3.11913648167029));
#250522=CARTESIAN_POINT('Origin',(6.50557852713814,-58.8589949086128,2.83404198860221));
#250523=CARTESIAN_POINT('Origin',(6.21503322485436,-62.1695413802703,3.11913648177471));
#250524=CARTESIAN_POINT('Origin',(6.19641157197526,-61.9923681882667,3.40423097483267));
#250525=CARTESIAN_POINT('Ctrl Pts',(6.493746461128,-58.7519447039086,2.90134173515983));
#250526=CARTESIAN_POINT('Ctrl Pts',(6.36806742857384,-58.7656442740268,
2.90103711553189));
#250527=CARTESIAN_POINT('Ctrl Pts',(6.37927424642637,-58.8722700234478,
2.83404198860221));
#250528=CARTESIAN_POINT('Ctrl Pts',(6.48899657309107,-58.7067576262544,
2.82862991747911));
#250529=CARTESIAN_POINT('Ctrl Pts',(6.38004220453002,-58.7342098038494,
2.853140458864));
#250530=CARTESIAN_POINT('Ctrl Pts',(6.37452469054107,-58.8270810177594,
2.7918796099985));
#250531=CARTESIAN_POINT('Ctrl Pts',(6.45774144355372,-58.6637560248471,
2.75470625793298));
#250532=CARTESIAN_POINT('Ctrl Pts',(6.37187117938199,-58.696789935432,2.79224250381849));
#250533=CARTESIAN_POINT('Ctrl Pts',(6.35435266912825,-58.7829167175849,
2.74901809108212));
#250534=CARTESIAN_POINT('Ctrl Pts',(6.34539908016383,-58.6035914159078,
2.63947868311645));
#250535=CARTESIAN_POINT('Ctrl Pts',(6.30313135363891,-58.6436439608621,
2.69595066767878));
#250536=CARTESIAN_POINT('Ctrl Pts',(6.28595874576574,-58.7181337176186,
2.68220539436026));
#250537=CARTESIAN_POINT('Ctrl Pts',(6.26151010025776,-58.5872698677163,
2.59908178584991));
#250538=CARTESIAN_POINT('Ctrl Pts',(6.2417055435759,-58.6268645946668,2.65877670944829));
#250539=CARTESIAN_POINT('Ctrl Pts',(6.23613328458309,-58.6982323944341,
2.65878198860221));
#250540=CARTESIAN_POINT('Ctrl Pts',(6.17403490859079,-58.5964866834548,
2.59908173515983));
#250541=CARTESIAN_POINT('Ctrl Pts',(6.17794390662231,-58.6335861742239,
2.65878198860221));
#250542=CARTESIAN_POINT('Ctrl Pts',(6.18532049829458,-58.7035958781036,
2.65878198860221));
#250543=CARTESIAN_POINT('Origin',(6.18532049829458,-58.7035958781036,2.53178198860221));
#250544=CARTESIAN_POINT('Ctrl Pts',(6.15137923967737,-61.5639141665609,
3.7700319886022));
#250545=CARTESIAN_POINT('Ctrl Pts',(6.2778722240253,-61.5506192181746,3.7700319886022));
#250546=CARTESIAN_POINT('Ctrl Pts',(6.27768337963421,-61.5506390665199,
3.64284238727536));
#250547=CARTESIAN_POINT('Ctrl Pts',(6.17383801205427,-61.7797255331383,
3.7700319886022));
#250548=CARTESIAN_POINT('Ctrl Pts',(6.30057242040001,-61.7665923920107,
3.77025506105787));
#250549=CARTESIAN_POINT('Ctrl Pts',(6.29582088597947,-61.7232059145518,
3.64284210641839));
#250550=CARTESIAN_POINT('Ctrl Pts',(6.19522058691298,-61.9851742714888,
3.65553527987788));
#250551=CARTESIAN_POINT('Ctrl Pts',(6.32217699854598,-61.9721416759939,
3.6558599653302));
#250552=CARTESIAN_POINT('Ctrl Pts',(6.31308747966748,-61.8874865820176,
3.55127902710128));
#250553=CARTESIAN_POINT('Ctrl Pts',(6.20712349654526,-62.0995362748656,
3.47153072139027));
#250554=CARTESIAN_POINT('Ctrl Pts',(6.33421251157784,-62.0866494440657,
3.47182327905144));
#250555=CARTESIAN_POINT('Ctrl Pts',(6.32269886789231,-61.9789328337394,
3.40413028377933));
#250556=CARTESIAN_POINT('Origin',(6.15137923967737,-61.5639141665609,3.6430319886022));
#250557=CARTESIAN_POINT('Origin',(5.67080826956262E-15,1.86266390934843E-13,
2.53178198860262));
#250558=CARTESIAN_POINT('Origin',(6.15500747092375,-58.706781905664,2.53178198860221));
#250559=CARTESIAN_POINT('Origin',(0.364094271196581,-6.50157577599598,3.64303198860258));
#250560=CARTESIAN_POINT('Origin',(6.10937495962149,-61.1647646440466,3.64299466007637));
#250561=CARTESIAN_POINT('Ctrl Pts',(6.14377718965381,-58.5996668978646,
2.59908173515983));
#250562=CARTESIAN_POINT('Ctrl Pts',(6.1476670304623,-58.636768402139,2.65878198860221));
#250563=CARTESIAN_POINT('Ctrl Pts',(6.15500747092375,-58.706781905664,2.65878198860221));
#250564=CARTESIAN_POINT('Ctrl Pts',(6.05659553606754,-58.6088074259624,
2.59908193199769));
#250565=CARTESIAN_POINT('Ctrl Pts',(6.08415140319859,-58.6434243604371,
2.65877685806616));
#250566=CARTESIAN_POINT('Ctrl Pts',(6.10436324506852,-58.7120821529669,
2.65878198860221));
#250567=CARTESIAN_POINT('Ctrl Pts',(5.97852000021575,-58.6416817365137,
2.63872492669757));
#250568=CARTESIAN_POINT('Ctrl Pts',(6.027858391313,-58.672182651071,2.69532212015236));
#250569=CARTESIAN_POINT('Ctrl Pts',(6.0600846870675,-58.7414038195493,2.68176836726596));
#250570=CARTESIAN_POINT('Ctrl Pts',(5.88025093392532,-58.7242744516461,
2.7544217640221));
#250571=CARTESIAN_POINT('Ctrl Pts',(5.97104363802227,-58.7387860695151,
2.79203179920094));
#250572=CARTESIAN_POINT('Ctrl Pts',(6.00614981441083,-58.8193360415242,
2.74885310748132));
#250573=CARTESIAN_POINT('Ctrl Pts',(5.85862682030309,-58.7730316211505,
2.82866089558359));
#250574=CARTESIAN_POINT('Ctrl Pts',(5.97091547255976,-58.7772266151811,
2.85316563119105));
#250575=CARTESIAN_POINT('Ctrl Pts',(5.99561386571486,-58.8669255556784,
2.79189751796562));
#250576=CARTESIAN_POINT('Ctrl Pts',(5.86337364149639,-58.8181995570482,
2.90134173515983));
#250577=CARTESIAN_POINT('Ctrl Pts',(5.98915458643853,-58.8054696185318,
2.90103711553189));
#250578=CARTESIAN_POINT('Ctrl Pts',(6.00036140429106,-58.9120953679528,
2.83404198860221));
#250579=CARTESIAN_POINT('Origin',(5.87405712357929,-58.9253704827878,2.83404198860221));
#250580=CARTESIAN_POINT('Origin',(6.10480350526334,-61.1207756545813,3.56647653971707));
#250581=CARTESIAN_POINT('Origin',(6.096249069953,-61.0393856393802,3.42473028058442));
#250582=CARTESIAN_POINT('Origin',(5.89267880207835,-59.102543918482,3.11913648168151));
#250583=CARTESIAN_POINT('Origin',(5.91130048050402,-59.2797173540683,3.40423097483269));
#250584=CARTESIAN_POINT('Ctrl Pts',(6.06175884541631,-60.7112330730301,
3.36123028058439));
#250585=CARTESIAN_POINT('Ctrl Pts',(6.18806312612808,-60.6979579581951,
3.36123028058439));
#250586=CARTESIAN_POINT('Ctrl Pts',(6.18806312612808,-60.6979579581951,
3.23423028058439));
#250587=CARTESIAN_POINT('Ctrl Pts',(6.07140041118294,-60.8007259828523,
3.36123028058439));
#250588=CARTESIAN_POINT('Ctrl Pts',(6.19746294737698,-60.7873912833617,
3.36099641108445));
#250589=CARTESIAN_POINT('Ctrl Pts',(6.20217593878228,-60.8322324012614,
3.23423043688341));
#250590=CARTESIAN_POINT('Ctrl Pts',(6.08051542067653,-60.8853484607267,
3.41054258905241));
#250591=CARTESIAN_POINT('Ctrl Pts',(6.20639551966795,-60.872379031649,3.41008815825926));
#250592=CARTESIAN_POINT('Ctrl Pts',(6.21552060714972,-60.9591984396299,
3.30819867304214));
#250593=CARTESIAN_POINT('Ctrl Pts',(6.08531878138382,-60.9299448846688,
3.48823028058441));
#250594=CARTESIAN_POINT('Ctrl Pts',(6.21110821942996,-60.9172173747508,
3.48794691941557));
#250595=CARTESIAN_POINT('Ctrl Pts',(6.22255335066477,-61.0261105245452,
3.42473028058442));
#250596=CARTESIAN_POINT('Origin',(6.06175884541631,-60.7112330730302,3.23423028058439));
#250597=CARTESIAN_POINT('Ctrl Pts',(5.90061356181316,-59.1725467709675,
3.47153072139031));
#250598=CARTESIAN_POINT('Ctrl Pts',(6.02658562874884,-59.159794554641,3.47122746285035));
#250599=CARTESIAN_POINT('Ctrl Pts',(6.03762143316813,-59.2666022171586,
3.40413046676737));
#250600=CARTESIAN_POINT('Ctrl Pts',(5.91250964036529,-59.2869113614503,
3.65553813457948));
#250601=CARTESIAN_POINT('Ctrl Pts',(6.03858760028519,-59.2739830624735,
3.65520336072233));
#250602=CARTESIAN_POINT('Ctrl Pts',(6.04723299508931,-59.358050121573,3.55128134519909));
#250603=CARTESIAN_POINT('Ctrl Pts',(5.93388131656964,-59.4923630227872,
3.77003198860222));
#250604=CARTESIAN_POINT('Ctrl Pts',(6.06016587018304,-59.4792818168401,
3.769802093141));
#250605=CARTESIAN_POINT('Ctrl Pts',(6.06449973388468,-59.5223321697741,
3.64284195387344));
#250606=CARTESIAN_POINT('Ctrl Pts',(5.95633285891271,-59.708171814489,3.77003198860222));
#250607=CARTESIAN_POINT('Ctrl Pts',(6.0828263345315,-59.694876814468,3.77003198860222));
#250608=CARTESIAN_POINT('Ctrl Pts',(6.08263699813626,-59.694896714525,3.64284189403743));
#250609=CARTESIAN_POINT('Origin',(5.95633285891271,-59.708171814489,3.64303198860222));
#250610=CARTESIAN_POINT('Origin',(0.347626240494121,-6.34489293004938,3.23423028058477));
#250611=CARTESIAN_POINT('Origin',(6.04595329345122,-60.5608532912341,3.23423028058439));
#250612=CARTESIAN_POINT('Origin',(0.345047419449927,-6.3203570867728,3.64303198860258));
#250613=CARTESIAN_POINT('Origin',(5.99823604520151,-60.1073400339994,3.64299171721718));
#250614=CARTESIAN_POINT('Ctrl Pts',(6.02238575970336,-60.3421421670673,
3.48823028058439));
#250615=CARTESIAN_POINT('Ctrl Pts',(6.14931623097308,-60.3293058762209,
3.48852004212217));
#250616=CARTESIAN_POINT('Ctrl Pts',(6.13776734223276,-60.2194255397043,
3.42473028058438));
#250617=CARTESIAN_POINT('Ctrl Pts',(6.02720817145293,-60.3868890390925,
3.41028005848367));
#250618=CARTESIAN_POINT('Ctrl Pts',(6.15399567477074,-60.3738278099493,
3.41074404220253));
#250619=CARTESIAN_POINT('Ctrl Pts',(6.14482385294855,-60.2865637544295,
3.30780486243826));
#250620=CARTESIAN_POINT('Ctrl Pts',(6.03634362557981,-60.4716618705779,
3.36123028058439));
#250621=CARTESIAN_POINT('Ctrl Pts',(6.16287156698331,-60.4582762833204,
3.36146460586393));
#250622=CARTESIAN_POINT('Ctrl Pts',(6.15819229746561,-60.4137560077508,
3.23423045308384));
#250623=CARTESIAN_POINT('Ctrl Pts',(6.04595329345122,-60.5608532912341,
3.36123028058439));
#250624=CARTESIAN_POINT('Ctrl Pts',(6.17225757416299,-60.5475781763991,
3.36123028058439));
#250625=CARTESIAN_POINT('Ctrl Pts',(6.17225757416299,-60.5475781763991,
3.23423028058439));
#250626=CARTESIAN_POINT('Origin',(6.01146306152099,-60.2327006545393,3.42473028058439));
#250627=CARTESIAN_POINT('Origin',(6.00295964283261,-60.1517960329186,3.56563113524724));
#250628=CARTESIAN_POINT('Origin',(13.0813452322063,-60.015799998865,3.56647653909396));
#250629=CARTESIAN_POINT('Origin',(13.0905908661208,-60.059048669912,3.64299466007403));
#250630=CARTESIAN_POINT('Origin',(13.0643300858388,-59.935750027543,3.42473028058442));
#250631=CARTESIAN_POINT('Ctrl Pts',(13.0409063549245,-59.8282880397052,
3.48823028058442));
#250632=CARTESIAN_POINT('Ctrl Pts',(12.9173404733289,-59.8550545325306,
3.48794691941558));
#250633=CARTESIAN_POINT('Ctrl Pts',(12.9401053405456,-59.9621548122768,
3.42473028058443));
#250634=CARTESIAN_POINT('Ctrl Pts',(13.0316624367257,-59.7842416555143,
3.41028005925046));
#250635=CARTESIAN_POINT('Ctrl Pts',(12.9079350417485,-59.8108054559342,
3.4098251223098));
#250636=CARTESIAN_POINT('Ctrl Pts',(12.9260696369487,-59.8961220185272,
3.30780486372835));
#250637=CARTESIAN_POINT('Ctrl Pts',(13.0141504107558,-59.700795824104,3.36123028058439));
#250638=CARTESIAN_POINT('Ctrl Pts',(12.8901364125068,-59.7270694888868,
3.36099721048401));
#250639=CARTESIAN_POINT('Ctrl Pts',(12.8994792219305,-59.7710239514086,
3.23423045308377));
#250640=CARTESIAN_POINT('Ctrl Pts',(12.995727518883,-59.6130003254552,3.3612302805844));
#250641=CARTESIAN_POINT('Ctrl Pts',(12.8715027735898,-59.639405110189,3.3612302805844));
#250642=CARTESIAN_POINT('Ctrl Pts',(12.8715027735898,-59.639405110189,3.2342302805844));
#250643=CARTESIAN_POINT('Origin',(12.995727518883,-59.6130003254552,3.2342302805844));
#250644=CARTESIAN_POINT('Origin',(0.310561863232988,0.0660119618348257,
3.64303198860263));
#250645=CARTESIAN_POINT('Origin',(13.1739864076113,-60.4516424606486,3.6430319886022));
#250646=CARTESIAN_POINT('Origin',(0.310561863232988,0.0660119618348286,
3.23423028058481));
#250647=CARTESIAN_POINT('Origin',(12.9642895838877,-59.4650964698963,3.2342302805844));
#250648=CARTESIAN_POINT('Ctrl Pts',(13.2864868029002,-60.9782752797345,
3.47153072139028));
#250649=CARTESIAN_POINT('Ctrl Pts',(13.1616357280628,-61.0052918384386,
3.47182327902619));
#250650=CARTESIAN_POINT('Ctrl Pts',(13.1392995818866,-60.8992893541402,
3.40413028958995));
#250651=CARTESIAN_POINT('Ctrl Pts',(13.2624669757416,-60.8658306440993,
3.65553807120913));
#250652=CARTESIAN_POINT('Ctrl Pts',(13.1376969719827,-60.8926675943312,
3.65586275496889));
#250653=CARTESIAN_POINT('Ctrl Pts',(13.1201818190183,-60.8093473519476,
3.5512812683716));
#250654=CARTESIAN_POINT('Ctrl Pts',(13.219315520358,-60.663828108008,3.77003198860221));
#250655=CARTESIAN_POINT('Ctrl Pts',(13.0947255842068,-60.6905008239732,
3.77025505748452));
#250656=CARTESIAN_POINT('Ctrl Pts',(13.0858375353127,-60.6477702018612,
3.64284211731198));
#250657=CARTESIAN_POINT('Ctrl Pts',(13.1739864076113,-60.4516424606486,
3.77003198860221));
#250658=CARTESIAN_POINT('Ctrl Pts',(13.0495760763092,-60.4780866929064,
3.77003198860221));
#250659=CARTESIAN_POINT('Ctrl Pts',(13.0497618007396,-60.47804721596,3.64284239821677));
#250660=CARTESIAN_POINT('Origin',(13.2635576885508,-60.873042205901,3.40423097483267));
#250661=CARTESIAN_POINT('Ctrl Pts',(12.9642895838877,-59.4650964698963,
3.3612302805844));
#250662=CARTESIAN_POINT('Ctrl Pts',(12.8400648385945,-59.4915012546302,
3.3612302805844));
#250663=CARTESIAN_POINT('Ctrl Pts',(12.8400648385945,-59.4915012546302,
3.2342302805844));
#250664=CARTESIAN_POINT('Ctrl Pts',(12.9458049943944,-59.3770041141839,
3.3612302805844));
#250665=CARTESIAN_POINT('Ctrl Pts',(12.8213326038456,-59.4033730190122,
3.3614653861013));
#250666=CARTESIAN_POINT('Ctrl Pts',(12.8119938336999,-59.3594375597997,
3.23423043688426));
#250667=CARTESIAN_POINT('Ctrl Pts',(12.9283282206303,-59.2937057271821,
3.41054258693058));
#250668=CARTESIAN_POINT('Ctrl Pts',(12.8037097640131,-59.3204640761242,
3.41100608859616));
#250669=CARTESIAN_POINT('Ctrl Pts',(12.7854506972086,-59.2345619206629,
3.30819866970701));
#250670=CARTESIAN_POINT('Ctrl Pts',(12.9191181862052,-59.2498070616276,
3.4882302805844));
#250671=CARTESIAN_POINT('Ctrl Pts',(12.7944335023715,-59.2768226962995,
3.48852004212218));
#250672=CARTESIAN_POINT('Ctrl Pts',(12.7714622569326,-59.1687514833557,
3.4247302805844));
#250673=CARTESIAN_POINT('Origin',(12.8956870022258,-59.1423466986219,3.4247302805844));
#250674=CARTESIAN_POINT('Origin',(13.3005969715165,-61.0472983318859,3.11913648178374));
#250675=CARTESIAN_POINT('Origin',(13.3376362544832,-61.2215544576536,2.8340419886022));
#250676=CARTESIAN_POINT('Origin',(12.878773330444,-59.0627741291263,3.56563113460749));
#250677=CARTESIAN_POINT('Origin',(12.8695280801147,-59.0190342907436,3.64299171721792));
#250678=CARTESIAN_POINT('Ctrl Pts',(13.1038352065734,-61.5752716937448,
2.5990817351598));
#250679=CARTESIAN_POINT('Ctrl Pts',(13.0960702419687,-61.5387839176324,
2.65878198860219));
#250680=CARTESIAN_POINT('Ctrl Pts',(13.0814171332239,-61.4699285681951,
2.65878198860219));
#250681=CARTESIAN_POINT('Ctrl Pts',(13.1900205930485,-61.556930451843,2.59908193475553));
#250682=CARTESIAN_POINT('Ctrl Pts',(13.15884824219,-61.5254208297822,2.65878715325412));
#250683=CARTESIAN_POINT('Ctrl Pts',(13.1313027022866,-61.4593031273778,
2.65878198860219));
#250684=CARTESIAN_POINT('Ctrl Pts',(13.264340740325,-61.5155378539377,2.63878778849826));
#250685=CARTESIAN_POINT('Ctrl Pts',(13.2118511391505,-61.4904936222812,
2.69564460180084));
#250686=CARTESIAN_POINT('Ctrl Pts',(13.1721300657497,-61.4250300340663,
2.68180481624848));
#250687=CARTESIAN_POINT('Ctrl Pts',(13.35355912682,-61.4222835584423,2.75443238878605));
#250688=CARTESIAN_POINT('Ctrl Pts',(13.2611962587093,-61.4178880557397,
2.79268340777032));
#250689=CARTESIAN_POINT('Ctrl Pts',(13.2174099770545,-61.3411158595751,
2.7488592683556));
#250690=CARTESIAN_POINT('Ctrl Pts',(13.3700167576327,-61.3712701109733,
2.82856655361625));
#250691=CARTESIAN_POINT('Ctrl Pts',(13.2570896192444,-61.3797074995629,
2.85384197230744));
#250692=CARTESIAN_POINT('Ctrl Pts',(13.2228660458972,-61.2924393404513,
2.79184624278419));
#250693=CARTESIAN_POINT('Ctrl Pts',(13.3605623192493,-61.326788195911,2.90134173515982));
#250694=CARTESIAN_POINT('Ctrl Pts',(13.2359003894758,-61.353761105708,2.90163218716349));
#250695=CARTESIAN_POINT('Ctrl Pts',(13.21341150919,-61.2479592423874,2.8340419886022));
#250696=CARTESIAN_POINT('Origin',(13.0814171332239,-61.4699285681951,2.53178198860219));
#250697=CARTESIAN_POINT('Origin',(0.310561863232988,0.0660119618348257,
3.64303198860263));
#250698=CARTESIAN_POINT('Origin',(12.7860306150458,-58.626453957798,3.64303198860222));
#250699=CARTESIAN_POINT('Origin',(5.63039444364742E-15,1.86043836520868E-13,
2.53178198860262));
#250700=CARTESIAN_POINT('Origin',(13.0516031943535,-61.4762657165312,2.53178198860219));
#250701=CARTESIAN_POINT('Ctrl Pts',(12.7860306150458,-58.626453957798,3.77003198860222));
#250702=CARTESIAN_POINT('Ctrl Pts',(12.6616197754744,-58.6528982980918,
3.77003198860222));
#250703=CARTESIAN_POINT('Ctrl Pts',(12.6618060089327,-58.6528587129482,
3.64284187936988));
#250704=CARTESIAN_POINT('Ctrl Pts',(12.7406940127384,-58.4142663981462,
3.77003198860222));
#250705=CARTESIAN_POINT('Ctrl Pts',(12.6165479409694,-58.4408495151693,
3.76980208962966));
#250706=CARTESIAN_POINT('Ctrl Pts',(12.6257296363319,-58.4831327254061,
3.64284193928274));
#250707=CARTESIAN_POINT('Ctrl Pts',(12.6975319705104,-58.212267640543,3.65553535416545));
#250708=CARTESIAN_POINT('Ctrl Pts',(12.5736296288425,-58.2389323335247,
3.65520057834348));
#250709=CARTESIAN_POINT('Ctrl Pts',(12.5913856081756,-58.3215567776507,
3.55127910964162));
#250710=CARTESIAN_POINT('Ctrl Pts',(12.6735055745747,-58.0998260601477,
3.47153072139032));
#250711=CARTESIAN_POINT('Ctrl Pts',(12.5497583536238,-58.126625494301,3.47122746281542));
#250712=CARTESIAN_POINT('Ctrl Pts',(12.5722680796271,-58.2316158778875,
3.40413045901224));
#250713=CARTESIAN_POINT('Origin',(12.6964592423899,-58.2050537810539,3.40423097483269));
#250714=CARTESIAN_POINT('Ctrl Pts',(12.7383709431257,-61.4590390555205,
2.90134173515981));
#250715=CARTESIAN_POINT('Ctrl Pts',(12.8632261535962,-61.4329754599095,
2.90163218716349));
#250716=CARTESIAN_POINT('Ctrl Pts',(12.8407372733105,-61.327173596589,2.8340419886022));
#250717=CARTESIAN_POINT('Ctrl Pts',(12.7478306169683,-61.5035409747664,
2.82853349835311));
#250718=CARTESIAN_POINT('Ctrl Pts',(12.8544171899349,-61.465315459776,2.85381483162333));
#250719=CARTESIAN_POINT('Ctrl Pts',(12.8501961180705,-61.3716739624481,
2.79182701594231));
#250720=CARTESIAN_POINT('Ctrl Pts',(12.7835835513937,-61.543271795361,2.75468822073602));
#250721=CARTESIAN_POINT('Ctrl Pts',(12.8662481012973,-61.5017184029583,
2.79286913083775));
#250722=CARTESIAN_POINT('Ctrl Pts',(12.874945307291,-61.4137451613971,2.74900763297864));
#250723=CARTESIAN_POINT('Ctrl Pts',(12.9020280679177,-61.5920631419341,
2.63954450640349));
#250724=CARTESIAN_POINT('Ctrl Pts',(12.9401487584132,-61.5478406570046,
2.69627684028829));
#250725=CARTESIAN_POINT('Ctrl Pts',(12.9498405053868,-61.4717924962539,
2.68224356036456));
#250726=CARTESIAN_POINT('Ctrl Pts',(12.9874904696728,-61.5999795805211,
2.599081787063));
#250727=CARTESIAN_POINT('Ctrl Pts',(13.0031958218449,-61.5585057825381,
2.65878704321566));
#250728=CARTESIAN_POINT('Ctrl Pts',(13.0015435854433,-61.4868843017927,
2.65878198860219));
#250729=CARTESIAN_POINT('Ctrl Pts',(13.0739701745332,-61.5816197022694,
2.59908173515981));
#250730=CARTESIAN_POINT('Ctrl Pts',(13.0662229071073,-61.5451281645056,
2.65878198860219));
#250731=CARTESIAN_POINT('Ctrl Pts',(13.0516031943535,-61.4762657165312,
2.65878198860219));
#250732=CARTESIAN_POINT('Origin',(12.7165125280173,-61.3535783813229,2.8340419886022));
#250733=CARTESIAN_POINT('Origin',(12.6594199084589,-58.0307974155454,3.11913648166996));
#250734=CARTESIAN_POINT('Origin',(12.6223805745526,-57.8565410498763,2.83404198860222));
#250735=CARTESIAN_POINT('Origin',(12.6794732450928,-61.179322255532,3.11913648177509));
#250736=CARTESIAN_POINT('Origin',(12.6424339620849,-61.0050661295703,3.40423097483267));
#250737=CARTESIAN_POINT('Ctrl Pts',(12.5994235324478,-57.7513140650717,
2.90134173515983));
#250738=CARTESIAN_POINT('Ctrl Pts',(12.4758649777959,-57.7780756236492,
2.90103711553189));
#250739=CARTESIAN_POINT('Ctrl Pts',(12.4981558292594,-57.8829458346102,
2.83404198860222));
#250740=CARTESIAN_POINT('Ctrl Pts',(12.5899763290081,-57.7068710254541,
2.82862991747923));
#250741=CARTESIAN_POINT('Ctrl Pts',(12.4844883578133,-57.7455616498585,
2.85314045886428));
#250742=CARTESIAN_POINT('Ctrl Pts',(12.488708754617,-57.8385008428011,2.79187960999885));
#250743=CARTESIAN_POINT('Ctrl Pts',(12.5543975270272,-57.6673720419783,
2.75470625793286));
#250744=CARTESIAN_POINT('Ctrl Pts',(12.4724506530564,-57.7092008760993,
2.79224250381865));
#250745=CARTESIAN_POINT('Ctrl Pts',(12.4640308112195,-57.7966870296826,
2.74901809108221));
#250746=CARTESIAN_POINT('Ctrl Pts',(12.4363816727429,-57.619279995667,2.63947868311658));
#250747=CARTESIAN_POINT('Ctrl Pts',(12.3985321242206,-57.6635313090884,
2.69595066767867));
#250748=CARTESIAN_POINT('Ctrl Pts',(12.3892398894931,-57.7394080294756,
2.68220539436019));
#250749=CARTESIAN_POINT('Ctrl Pts',(12.3512461790957,-57.611816644779,2.59908178585008));
#250750=CARTESIAN_POINT('Ctrl Pts',(12.3356888898096,-57.6532646075507,
2.65877670944881));
#250751=CARTESIAN_POINT('Ctrl Pts',(12.337607122671,-57.724823906712,2.65878198860222));
#250752=CARTESIAN_POINT('Ctrl Pts',(12.2652136052667,-57.6301266171954,
2.59908173515984));
#250753=CARTESIAN_POINT('Ctrl Pts',(12.2729791421561,-57.6666142715152,
2.65878198860222));
#250754=CARTESIAN_POINT('Ctrl Pts',(12.2876333308477,-57.7354693911201,
2.65878198860222));
#250755=CARTESIAN_POINT('Origin',(12.2876333308477,-57.7354693911201,2.53178198860222));
#250756=CARTESIAN_POINT('Ctrl Pts',(12.5528626811454,-60.5836663843179,
3.77003198860221));
#250757=CARTESIAN_POINT('Ctrl Pts',(12.6772730231654,-60.5572221497819,
3.77003198860221));
#250758=CARTESIAN_POINT('Ctrl Pts',(12.6770872880011,-60.5572616290098,
3.64284238727576));
#250759=CARTESIAN_POINT('Ctrl Pts',(12.5977568525211,-60.795947932685,3.77003198860221));
#250760=CARTESIAN_POINT('Ctrl Pts',(12.7224242094588,-60.7696393833344,
3.77025506105822));
#250761=CARTESIAN_POINT('Ctrl Pts',(12.7131635826249,-60.7269872521279,
3.64284210641902));
#250762=CARTESIAN_POINT('Ctrl Pts',(12.6404975322993,-60.9980361136593,
3.65553527987791));
#250763=CARTESIAN_POINT('Ctrl Pts',(12.7653961862437,-60.971804353472,3.65585996532863));
#250764=CARTESIAN_POINT('Ctrl Pts',(12.7475075938202,-60.8885631224013,
3.55127902710092));
#250765=CARTESIAN_POINT('Ctrl Pts',(12.6642893210148,-61.1105274371638,
3.47153072139028));
#250766=CARTESIAN_POINT('Ctrl Pts',(12.7893350885052,-61.0844267823319,
3.47182327905145));
#250767=CARTESIAN_POINT('Ctrl Pts',(12.7666250660191,-60.9785037583489,
3.40413028377955));
#250768=CARTESIAN_POINT('Origin',(12.5528626811454,-60.5836663843179,3.64303198860221));
#250769=CARTESIAN_POINT('Origin',(5.67687244506386E-15,1.86267351405886E-13,
2.53178198860262));
#250770=CARTESIAN_POINT('Origin',(12.2578193919774,-57.7418065394563,2.53178198860222));
#250771=CARTESIAN_POINT('Origin',(2.3791451040456,-12.7200883457667,3.64303198860254));
#250772=CARTESIAN_POINT('Origin',(12.4693660187269,-60.1910940874967,3.64299466007605));
#250773=CARTESIAN_POINT('Ctrl Pts',(12.2354540642051,-57.6364522029204,
2.59908173515984));
#250774=CARTESIAN_POINT('Ctrl Pts',(12.2432007592853,-57.6729438621903,
2.65878198860222));
#250775=CARTESIAN_POINT('Ctrl Pts',(12.2578193919774,-57.7418065394563,
2.65878198860222));
#250776=CARTESIAN_POINT('Ctrl Pts',(12.1497054461947,-57.6546556225238,
2.59908193199844));
#250777=CARTESIAN_POINT('Ctrl Pts',(12.1807288143665,-57.6862025493664,
2.65877685806609));
#250778=CARTESIAN_POINT('Ctrl Pts',(12.208006627196,-57.7523715145525,2.65878198860222));
#250779=CARTESIAN_POINT('Ctrl Pts',(12.0754939174604,-57.6955109599431,
2.63872492669758));
#250780=CARTESIAN_POINT('Ctrl Pts',(12.1277502414159,-57.720687521098,2.69532212015226));
#250781=CARTESIAN_POINT('Ctrl Pts',(12.1670355805169,-57.7861609236004,
2.68176836726595));
#250782=CARTESIAN_POINT('Ctrl Pts',(11.9863964689869,-57.7879231380264,
2.7544217640221));
#250783=CARTESIAN_POINT('Ctrl Pts',(12.0782086782663,-57.7928648378988,
2.7920317992011));
#250784=CARTESIAN_POINT('Ctrl Pts',(12.1215423041379,-57.8693039540642,
2.74885310748135));
#250785=CARTESIAN_POINT('Ctrl Pts',(11.9699873265234,-57.8386735460211,
2.82866089558358));
#250786=CARTESIAN_POINT('Ctrl Pts',(12.0820993460737,-57.8311081991714,
2.85316563119168));
#250787=CARTESIAN_POINT('Ctrl Pts',(12.1160385312535,-57.9177340744066,
2.79189751796608));
#250788=CARTESIAN_POINT('Ctrl Pts',(11.9794294790618,-57.8830978693153,
2.90134173515983));
#250789=CARTESIAN_POINT('Ctrl Pts',(12.1031907419163,-57.8572899778508,
2.90103711553189));
#250790=CARTESIAN_POINT('Ctrl Pts',(12.1254815933798,-57.9621601888118,
2.83404198860222));
#250791=CARTESIAN_POINT('Origin',(12.0012568480866,-57.9885649735456,2.83404198860222));
#250792=CARTESIAN_POINT('Origin',(12.4602215058074,-60.1478239214154,3.56647653971778));
#250793=CARTESIAN_POINT('Origin',(12.4432063593729,-60.0677739512123,3.42473028058443));
#250794=CARTESIAN_POINT('Origin',(12.038296182044,-58.1628213391881,3.11913648167957));
#250795=CARTESIAN_POINT('Origin',(12.0753355159239,-58.3370777047231,3.40423097483269));
#250796=CARTESIAN_POINT('Ctrl Pts',(12.3746037924171,-59.7450242491244,
3.3612302805844));
#250797=CARTESIAN_POINT('Ctrl Pts',(12.4988285377103,-59.7186194643906,
3.3612302805844));
#250798=CARTESIAN_POINT('Ctrl Pts',(12.4988285377102,-59.7186194643906,
3.2342302805844));
#250799=CARTESIAN_POINT('Ctrl Pts',(12.3935470970153,-59.8330190893696,
3.3612302805844));
#250800=CARTESIAN_POINT('Ctrl Pts',(12.5175251937999,-59.8065803155745,
3.36099641108498));
#250801=CARTESIAN_POINT('Ctrl Pts',(12.5268995400903,-59.8506831473911,
3.2342304368836));
#250802=CARTESIAN_POINT('Ctrl Pts',(12.411457631102,-59.9162252185213,3.41054258905242));
#250803=CARTESIAN_POINT('Ctrl Pts',(12.5352924712508,-59.8901687840285,
3.41008815825911));
#250804=CARTESIAN_POINT('Ctrl Pts',(12.5534426698451,-59.9755587548351,
3.30819867304268));
#250805=CARTESIAN_POINT('Ctrl Pts',(12.4208962741593,-59.9600752506734,
3.48823028058442));
#250806=CARTESIAN_POINT('Ctrl Pts',(12.5446662374493,-59.9342688867322,
3.48794691941558));
#250807=CARTESIAN_POINT('Ctrl Pts',(12.5674311046661,-60.0413691664784,
3.42473028058443));
#250808=CARTESIAN_POINT('Origin',(12.3746037924171,-59.7450242491244,3.2342302805844));
#250809=CARTESIAN_POINT('Ctrl Pts',(12.0535047649328,-58.2316113004778,
3.47153072139032));
#250810=CARTESIAN_POINT('Ctrl Pts',(12.1774537741291,-58.2057612755552,
3.47122746285037));
#250811=CARTESIAN_POINT('Ctrl Pts',(12.1995935640854,-58.310830278845,3.40413046676749));
#250812=CARTESIAN_POINT('Ctrl Pts',(12.0772900304182,-58.3441059109576,
3.65553813457945));
#250813=CARTESIAN_POINT('Ctrl Pts',(12.201325946859,-58.3180696991554,3.65520336072166));
#250814=CARTESIAN_POINT('Ctrl Pts',(12.2187113817825,-58.4007725402752,
3.5512813451987));
#250815=CARTESIAN_POINT('Ctrl Pts',(12.120020176778,-58.5461981381262,3.77003198860223));
#250816=CARTESIAN_POINT('Ctrl Pts',(12.2442455720369,-58.5199882620684,
3.76980209314081));
#250817=CARTESIAN_POINT('Ctrl Pts',(12.2530556816164,-58.5623497685522,
3.64284195387377));
#250818=CARTESIAN_POINT('Ctrl Pts',(12.1649068885798,-58.7584778814673,
3.77003198860222));
#250819=CARTESIAN_POINT('Ctrl Pts',(12.2893177137824,-58.7320335442277,
3.77003198860222));
#250820=CARTESIAN_POINT('Ctrl Pts',(12.2891314947143,-58.7320731263126,
3.64284189403764));
#250821=CARTESIAN_POINT('Origin',(12.1649068885798,-58.7584778814673,3.64303198860222));
#250822=CARTESIAN_POINT('Origin',(2.31399271319982,-12.413570446089,3.23423028058473));
#250823=CARTESIAN_POINT('Origin',(12.3431658574217,-59.5971203935656,3.2342302805844));
#250824=CARTESIAN_POINT('Origin',(2.30379013587727,-12.3655710936231,3.64303198860254));
#250825=CARTESIAN_POINT('Origin',(12.2483049654011,-59.1510793400371,3.64299171721781));
#250826=CARTESIAN_POINT('Ctrl Pts',(12.296865891381,-59.3820708699068,3.4882302805844));
#250827=CARTESIAN_POINT('Ctrl Pts',(12.4217592664919,-59.3560370505011,
3.48852004212218));
#250828=CARTESIAN_POINT('Ctrl Pts',(12.398788021053,-59.2479658375573,3.4247302805844));
#250829=CARTESIAN_POINT('Ctrl Pts',(12.3063392072239,-59.4260685345956,
3.41028005848365));
#250830=CARTESIAN_POINT('Ctrl Pts',(12.4310668851223,-59.3998259533497,
3.41074404220255));
#250831=CARTESIAN_POINT('Ctrl Pts',(12.4128237298763,-59.3139986558953,
3.30780486243784));
#250832=CARTESIAN_POINT('Ctrl Pts',(12.3242857901785,-59.5094220566591,
3.36123028058439));
#250833=CARTESIAN_POINT('Ctrl Pts',(12.4487214234139,-59.4828840257732,
3.36146460586428));
#250834=CARTESIAN_POINT('Ctrl Pts',(12.4394141514352,-59.4390967537847,
3.23423045308405));
#250835=CARTESIAN_POINT('Ctrl Pts',(12.3431658574217,-59.5971203935656,
3.3612302805844));
#250836=CARTESIAN_POINT('Ctrl Pts',(12.4673906027149,-59.5707156088318,
3.3612302805844));
#250837=CARTESIAN_POINT('Ctrl Pts',(12.4673906027149,-59.5707156088318,
3.2342302805844));
#250838=CARTESIAN_POINT('Origin',(12.2745632757598,-59.2743706222912,3.4247302805844));
#250839=CARTESIAN_POINT('Origin',(12.2576496039196,-59.194798053941,3.56563113524728));
#250840=CARTESIAN_POINT('Origin',(19.2830435999592,-58.3196542523186,3.56647653909411));
#250841=CARTESIAN_POINT('Origin',(19.2967593024467,-58.3616995707152,3.64299466007486));
#250842=CARTESIAN_POINT('Origin',(19.2577541638585,-58.241821370217,3.42473028058443));
#250843=CARTESIAN_POINT('Ctrl Pts',(19.2232259141446,-58.137396516989,3.48823028058443));
#250844=CARTESIAN_POINT('Ctrl Pts',(19.1031347997394,-58.1769325318816,
3.48794691941559));
#250845=CARTESIAN_POINT('Ctrl Pts',(19.136969986289,-58.2810665285026,3.42473028058444));
#250846=CARTESIAN_POINT('Ctrl Pts',(19.2094285342441,-58.0945576760634,
3.41028005925047));
#250847=CARTESIAN_POINT('Ctrl Pts',(19.0891556041198,-58.1339089916623,
3.40982512230991));
#250848=CARTESIAN_POINT('Ctrl Pts',(19.116108865289,-58.2168625998338,3.30780486372806));
#250849=CARTESIAN_POINT('Ctrl Pts',(19.1832899764622,-58.0133994748118,
3.36123028058441));
#250850=CARTESIAN_POINT('Ctrl Pts',(19.0627016856762,-58.0524922023731,
3.36099721048509));
#250851=CARTESIAN_POINT('Ctrl Pts',(19.0765878066329,-58.0952292882361,
3.2342304530843));
#250852=CARTESIAN_POINT('Ctrl Pts',(19.1557908785631,-57.9280106456672,
3.36123028058441));
#250853=CARTESIAN_POINT('Ctrl Pts',(19.0350067009936,-57.9672558039528,
3.36123028058441));
#250854=CARTESIAN_POINT('Ctrl Pts',(19.0350067009936,-57.9672558039528,
3.23423028058441));
#250855=CARTESIAN_POINT('Origin',(19.1557908785631,-57.9280106456672,3.23423028058441));
#250856=CARTESIAN_POINT('Origin',(0.301960443923716,0.0981128957142328,
3.64303198860263));
#250857=CARTESIAN_POINT('Origin',(19.4207352200707,-58.7434254837928,3.64303198860222));
#250858=CARTESIAN_POINT('Origin',(0.301960443923716,0.0981128957142356,
3.23423028058481));
#250859=CARTESIAN_POINT('Origin',(19.1090650011322,-57.7842031819379,3.23423028058441));
#250860=CARTESIAN_POINT('Ctrl Pts',(19.5876674457085,-59.2554138597567,
3.4715307213903));
#250861=CARTESIAN_POINT('Ctrl Pts',(19.4663243174868,-59.2953329099155,
3.47182327902621));
#250862=CARTESIAN_POINT('Ctrl Pts',(19.4330302542699,-59.1922458813528,
3.40413028959015));
#250863=CARTESIAN_POINT('Ctrl Pts',(19.5520255367122,-59.1460959632211,
3.65553807120917));
#250864=CARTESIAN_POINT('Ctrl Pts',(19.4307442612537,-59.1858279145837,
3.65586275496688));
#250865=CARTESIAN_POINT('Ctrl Pts',(19.4046157212338,-59.1047949412303,
3.55128126837138));
#250866=CARTESIAN_POINT('Ctrl Pts',(19.4879954548421,-58.9497105734776,
3.77003198860222));
#250867=CARTESIAN_POINT('Ctrl Pts',(19.366876093408,-58.989260368081,3.77025505748598));
#250868=CARTESIAN_POINT('Ctrl Pts',(19.3535701679114,-58.9476928828799,
3.64284211731211));
#250869=CARTESIAN_POINT('Ctrl Pts',(19.4207352200707,-58.7434254837929,
3.77003198860222));
#250870=CARTESIAN_POINT('Ctrl Pts',(19.2997705965413,-58.782729272525,3.77003198860222));
#250871=CARTESIAN_POINT('Ctrl Pts',(19.299951177089,-58.7826705983483,3.64284239821712));
#250872=CARTESIAN_POINT('Origin',(19.5538640879539,-59.1531540087995,3.40423097483269));
#250873=CARTESIAN_POINT('Ctrl Pts',(19.1090650011322,-57.7842031819379,
3.36123028058441));
#250874=CARTESIAN_POINT('Ctrl Pts',(18.9882808235627,-57.8234483402235,
3.36123028058441));
#250875=CARTESIAN_POINT('Ctrl Pts',(18.9882808235627,-57.8234483402235,
3.23423028058441));
#250876=CARTESIAN_POINT('Ctrl Pts',(19.0814735135864,-57.6985255711011,
3.36123028058441));
#250877=CARTESIAN_POINT('Ctrl Pts',(18.960439296918,-57.7377609320114,3.36146538610076));
#250878=CARTESIAN_POINT('Ctrl Pts',(18.9465591794957,-57.6950423231348,
3.234230436884));
#250879=CARTESIAN_POINT('Ctrl Pts',(19.0553854270324,-57.617510321683,3.41054258693058));
#250880=CARTESIAN_POINT('Ctrl Pts',(18.9342466524541,-57.6571482613564,
3.41100608859694));
#250881=CARTESIAN_POINT('Ctrl Pts',(18.9071083904254,-57.5736252790843,
3.30819866970748));
#250882=CARTESIAN_POINT('Ctrl Pts',(19.0416371860884,-57.5748148483572,
3.4882302805844));
#250883=CARTESIAN_POINT('Ctrl Pts',(18.9204594407751,-57.6147155869498,
3.48852004212217));
#250884=CARTESIAN_POINT('Ctrl Pts',(18.8863175164099,-57.5096375484033,
3.42473028058439));
#250885=CARTESIAN_POINT('Origin',(19.0071016939793,-57.4703923901177,3.42473028058439));
#250886=CARTESIAN_POINT('Origin',(19.6089151909164,-59.3225838821625,3.11913648178257));
#250887=CARTESIAN_POINT('Origin',(19.6639662938568,-59.4920137553135,2.83404198860221));
#250888=CARTESIAN_POINT('Origin',(18.9819630786536,-57.3930236876037,3.56563113460773));
#250889=CARTESIAN_POINT('Origin',(18.9681964166838,-57.3504898524406,3.6429917172174));
#250890=CARTESIAN_POINT('Ctrl Pts',(19.4684195516703,-59.8682321556238,
2.59908173515982));
#250891=CARTESIAN_POINT('Ctrl Pts',(19.456883113189,-59.8327559231842,2.6587819886022));
#250892=CARTESIAN_POINT('Ctrl Pts',(19.4351129318427,-59.7658094374947,
2.6587819886022));
#250893=CARTESIAN_POINT('Ctrl Pts',(19.5522156237501,-59.8409825629596,
2.59908193475582));
#250894=CARTESIAN_POINT('Ctrl Pts',(19.5179203859187,-59.8129039518359,
2.6587871532548));
#250895=CARTESIAN_POINT('Ctrl Pts',(19.4836145615382,-59.7500277420804,
2.6587819886022));
#250896=CARTESIAN_POINT('Ctrl Pts',(19.6218019328337,-59.792048147252,2.63878778849858));
#250897=CARTESIAN_POINT('Ctrl Pts',(19.5669820401377,-59.7726277678648,
2.69564460180074));
#250898=CARTESIAN_POINT('Ctrl Pts',(19.5206357546569,-59.7116747787975,
2.68180481624849));
#250899=CARTESIAN_POINT('Ctrl Pts',(19.7007838434716,-59.6899788477095,
2.75443238878576));
#250900=CARTESIAN_POINT('Ctrl Pts',(19.6084674936738,-59.6952619726976,
2.79268340777048));
#250901=CARTESIAN_POINT('Ctrl Pts',(19.5568961981644,-59.6234872553901,
2.74885926835562));
#250902=CARTESIAN_POINT('Ctrl Pts',(19.7118189603907,-59.6375245663852,
2.82856655361648));
#250903=CARTESIAN_POINT('Ctrl Pts',(19.6003923959456,-59.6577198343142,
2.85384197230767));
#250904=CARTESIAN_POINT('Ctrl Pts',(19.5572342963498,-59.5745070768389,
2.79184624278477));
#250905=CARTESIAN_POINT('Ctrl Pts',(19.6977666881852,-59.5942745858232,
2.90134173515983));
#250906=CARTESIAN_POINT('Ctrl Pts',(19.5766071063175,-59.6341304551453,
2.9016321871635));
#250907=CARTESIAN_POINT('Ctrl Pts',(19.5431821162873,-59.5312589135992,
2.83404198860221));
#250908=CARTESIAN_POINT('Origin',(19.4351129318427,-59.7658094374947,2.5317819886022));
#250909=CARTESIAN_POINT('Origin',(0.301960443923716,0.0981128957142328,
3.64303198860263));
#250910=CARTESIAN_POINT('Origin',(18.8441205405526,-56.9687879773462,3.64303198860223));
#250911=CARTESIAN_POINT('Origin',(5.61372323131277E-15,1.86039369482986E-13,
2.53178198860262));
#250912=CARTESIAN_POINT('Origin',(19.406124729226,-59.7752282754833,2.5317819886022));
#250913=CARTESIAN_POINT('Ctrl Pts',(18.8441205405526,-56.9687879773462,
3.77003198860223));
#250914=CARTESIAN_POINT('Ctrl Pts',(18.7231554228308,-57.0080919266512,
3.77003198860223));
#250915=CARTESIAN_POINT('Ctrl Pts',(18.7233364983084,-57.008033091662,3.64284187936999));
#250916=CARTESIAN_POINT('Ctrl Pts',(18.7768526573602,-56.7625017687171,
3.77003198860224));
#250917=CARTESIAN_POINT('Ctrl Pts',(18.6561653631336,-56.8019160587494,
3.7698020896296));
#250918=CARTESIAN_POINT('Ctrl Pts',(18.6697165591971,-56.8430078886266,
3.64284193928345));
#250919=CARTESIAN_POINT('Ctrl Pts',(18.7128124416033,-56.5661212433884,
3.65553535416544));
#250920=CARTESIAN_POINT('Ctrl Pts',(18.5923760693075,-56.6055911857578,
3.6552005783447));
#250921=CARTESIAN_POINT('Ctrl Pts',(18.6186713857005,-56.6859069993044,
3.55127910964129));
#250922=CARTESIAN_POINT('Ctrl Pts',(18.6771643191716,-56.4568070719807,
3.47153072139033));
#250923=CARTESIAN_POINT('Ctrl Pts',(18.5568963021136,-56.4963948028693,
3.47122746281543));
#250924=CARTESIAN_POINT('Ctrl Pts',(18.5902572009366,-56.5984571310815,
3.4041304590123));
#250925=CARTESIAN_POINT('Origin',(18.7109915363523,-56.5590590327986,3.40423097483271));
#250926=CARTESIAN_POINT('Ctrl Pts',(19.0928077206418,-59.7908376697907,
2.90134173515982));
#250927=CARTESIAN_POINT('Ctrl Pts',(19.214254573609,-59.7518659300022,2.9016321871635));
#250928=CARTESIAN_POINT('Ctrl Pts',(19.1808295835788,-59.648994388456,2.83404198860221));
#250929=CARTESIAN_POINT('Ctrl Pts',(19.1068672906319,-59.834106997697,2.82853349835317));
#250930=CARTESIAN_POINT('Ctrl Pts',(19.2088743168603,-59.7849495553994,
2.85381483162279));
#250931=CARTESIAN_POINT('Ctrl Pts',(19.1948881666555,-59.6922622581471,
2.79182701594138));
#250932=CARTESIAN_POINT('Ctrl Pts',(19.1465773683633,-59.8698829694065,
2.75468822073595));
#250933=CARTESIAN_POINT('Ctrl Pts',(19.224445560962,-59.8199164124669,2.79286913083809));
#250934=CARTESIAN_POINT('Ctrl Pts',(19.223899415002,-59.7315159919503,2.74900763297869));
#250935=CARTESIAN_POINT('Ctrl Pts',(19.2694731179109,-59.9060262085831,
2.63954450640357));
#250936=CARTESIAN_POINT('Ctrl Pts',(19.3027624708834,-59.8580612818569,
2.6962768402881));
#250937=CARTESIAN_POINT('Ctrl Pts',(19.3044519280757,-59.7814166574705,
2.68224356036452));
#250938=CARTESIAN_POINT('Ctrl Pts',(19.355294840847,-59.9049660265686,2.59908178706304));
#250939=CARTESIAN_POINT('Ctrl Pts',(19.3665789650884,-59.8620777700647,
2.65878704321362));
#250940=CARTESIAN_POINT('Ctrl Pts',(19.3574492964907,-59.791021345015,2.65878198860221));
#250941=CARTESIAN_POINT('Ctrl Pts',(19.4393816709763,-59.8776671349981,
2.59908173515982));
#250942=CARTESIAN_POINT('Ctrl Pts',(19.4278624395273,-59.8421853116549,
2.65878198860221));
#250943=CARTESIAN_POINT('Ctrl Pts',(19.406124729226,-59.7752282754833,2.65878198860221));
#250944=CARTESIAN_POINT('Origin',(19.0600454060093,-59.6882395467416,2.83404198860221));
#250945=CARTESIAN_POINT('Origin',(18.6559403576674,-56.3896289265479,3.11913648167074));
#250946=CARTESIAN_POINT('Origin',(18.6008891789892,-56.2201988201379,2.83404198860223));
#250947=CARTESIAN_POINT('Origin',(19.0049943031093,-59.5188096735662,3.11913648177587));
#250948=CARTESIAN_POINT('Origin',(18.9499432001064,-59.3493798002276,3.40423097483269));
#250949=CARTESIAN_POINT('Ctrl Pts',(18.5670586829472,-56.1179479440984,
2.90134173515985));
#250950=CARTESIAN_POINT('Ctrl Pts',(18.4469743395785,-56.1574782858993,
2.90103711553191));
#250951=CARTESIAN_POINT('Ctrl Pts',(18.4801050014197,-56.2594439784235,
2.83404198860223));
#250952=CARTESIAN_POINT('Ctrl Pts',(18.553017669642,-56.0747358697598,2.82862991747918));
#250953=CARTESIAN_POINT('Ctrl Pts',(18.4521518441045,-56.124241038398,2.85314045886448));
#250954=CARTESIAN_POINT('Ctrl Pts',(18.4660639121469,-56.2162299491246,
2.79187960999894));
#250955=CARTESIAN_POINT('Ctrl Pts',(18.513505004018,-56.0391722633443,2.7547062579329));
#250956=CARTESIAN_POINT('Ctrl Pts',(18.4363793473478,-56.0893377355405,
2.79224250381869));
#250957=CARTESIAN_POINT('Ctrl Pts',(18.4371504234768,-56.1772247439493,
2.74901809108223));
#250958=CARTESIAN_POINT('Ctrl Pts',(18.3911086652352,-56.0036796861842,
2.63947868311657));
#250959=CARTESIAN_POINT('Ctrl Pts',(18.3580919822896,-56.0516449414235,
2.69595066767864));
#250960=CARTESIAN_POINT('Ctrl Pts',(18.356781928376,-56.1280773042132,2.6822053943602));
#250961=CARTESIAN_POINT('Ctrl Pts',(18.305659420131,-56.0051563026337,2.59908178585011));
#250962=CARTESIAN_POINT('Ctrl Pts',(18.2945198471568,-56.048003388668,2.658776709449));
#250963=CARTESIAN_POINT('Ctrl Pts',(18.3039075553122,-56.1189701685695,
2.65878198860223));
#250964=CARTESIAN_POINT('Ctrl Pts',(18.2220120550223,-56.0323588238387,
2.59908173515985));
#250965=CARTESIAN_POINT('Ctrl Pts',(18.2335490499224,-56.0678348753329,
2.65878198860223));
#250966=CARTESIAN_POINT('Ctrl Pts',(18.2553202812755,-56.1347810195638,
2.65878198860223));
#250967=CARTESIAN_POINT('Origin',(18.2553202812755,-56.1347810195638,2.53178198860223));
#250968=CARTESIAN_POINT('Ctrl Pts',(18.8168143322233,-58.9396512752209,
3.77003198860222));
#250969=CARTESIAN_POINT('Ctrl Pts',(18.9377789661745,-58.9003474831026,
3.77003198860222));
#250970=CARTESIAN_POINT('Ctrl Pts',(18.9375983751895,-58.9004061606706,
3.64284238727543));
#250971=CARTESIAN_POINT('Ctrl Pts',(18.8836520326624,-59.146077204311,3.77003198860222));
#250972=CARTESIAN_POINT('Ctrl Pts',(19.0048864565391,-59.1068814887043,
3.77025506105808));
#250973=CARTESIAN_POINT('Ctrl Pts',(18.9912181986578,-59.0654310094276,
3.6428421064193));
#250974=CARTESIAN_POINT('Ctrl Pts',(18.9472825415249,-59.3425907075094,
3.6555352798779));
#250975=CARTESIAN_POINT('Ctrl Pts',(19.0687550219954,-59.3034471832903,
3.65585996532954));
#250976=CARTESIAN_POINT('Ctrl Pts',(19.0422633471882,-59.2225318234682,
3.55127902710076));
#250977=CARTESIAN_POINT('Ctrl Pts',(18.9827025415103,-59.4519788726604,
3.47153072139031));
#250978=CARTESIAN_POINT('Ctrl Pts',(19.1043350338631,-59.4129503580326,
3.47182327905148));
#250979=CARTESIAN_POINT('Ctrl Pts',(19.0706774483344,-59.3099814352089,
3.4041302837794));
#250980=CARTESIAN_POINT('Origin',(18.8168143322233,-58.9396512752209,3.64303198860222));
#250981=CARTESIAN_POINT('Origin',(5.68280300381509E-15,1.86268940494314E-13,
2.53178198860262));
#250982=CARTESIAN_POINT('Origin',(18.2263320786588,-56.1441998575524,2.53178198860223));
#250983=CARTESIAN_POINT('Origin',(5.63975536249314,-18.3848338156963,3.6430319886025));
#250984=CARTESIAN_POINT('Origin',(18.6927400943504,-58.5579573083282,3.64299466007569));
#250985=CARTESIAN_POINT('Ctrl Pts',(18.1930767435955,-56.0417604764379,
2.59908173515985));
#250986=CARTESIAN_POINT('Ctrl Pts',(18.2045954185351,-56.077242480448,2.65878198860223));
#250987=CARTESIAN_POINT('Ctrl Pts',(18.2263320786588,-56.1441998575524,
2.65878198860223));
#250988=CARTESIAN_POINT('Ctrl Pts',(18.1097006409639,-56.0688273470718,
2.59908193199789));
#250989=CARTESIAN_POINT('Ctrl Pts',(18.1438516116622,-56.0969586315467,
2.6587768580669));
#250990=CARTESIAN_POINT('Ctrl Pts',(18.1778965340258,-56.159913808362,2.65878198860223));
#250991=CARTESIAN_POINT('Ctrl Pts',(18.0401661963857,-56.1172160917337,
2.6387249266977));
#250992=CARTESIAN_POINT('Ctrl Pts',(18.0947679219786,-56.136792459813,2.69532212015243));
#250993=CARTESIAN_POINT('Ctrl Pts',(18.1406818860302,-56.197800756041,2.68176836726596));
#250994=CARTESIAN_POINT('Ctrl Pts',(17.9612165360197,-56.218435245606,2.75442176402201));
#250995=CARTESIAN_POINT('Ctrl Pts',(18.0530423367039,-56.2137528851844,
2.7920317992009));
#250996=CARTESIAN_POINT('Ctrl Pts',(18.104128639785,-56.2852436625531,2.74885310748136));
#250997=CARTESIAN_POINT('Ctrl Pts',(17.9502021467132,-56.270622860001,2.82866089558369));
#250998=CARTESIAN_POINT('Ctrl Pts',(18.0609092108095,-56.2513800597957,
2.85316563119182));
#250999=CARTESIAN_POINT('Ctrl Pts',(18.1037173431996,-56.3339837785512,
2.79189751796588));
#251000=CARTESIAN_POINT('Ctrl Pts',(17.9642361803979,-56.3138168485091,
2.90134173515985));
#251001=CARTESIAN_POINT('Ctrl Pts',(18.0846218068701,-56.2752137607562,
2.90103711553191));
#251002=CARTESIAN_POINT('Ctrl Pts',(18.1177524687112,-56.3771794532803,
2.83404198860223));
#251003=CARTESIAN_POINT('Origin',(17.9969682911417,-56.416424611566,2.83404198860223));
#251004=CARTESIAN_POINT('Origin',(18.6791227120631,-58.5158800426264,3.56647653971792));
#251005=CARTESIAN_POINT('Origin',(18.6538332760111,-58.4380471616451,3.42473028058444));
#251006=CARTESIAN_POINT('Origin',(18.0520194698712,-56.5858547179415,3.1191364816814));
#251007=CARTESIAN_POINT('Origin',(18.1070706485049,-56.7552848242267,3.40423097483271));
#251008=CARTESIAN_POINT('Ctrl Pts',(18.5518699907157,-58.1242364370953,
3.36123028058441));
#251009=CARTESIAN_POINT('Ctrl Pts',(18.6726541682852,-58.0849912788096,
3.36123028058441));
#251010=CARTESIAN_POINT('Ctrl Pts',(18.6726541682852,-58.0849912788097,
3.23423028058441));
#251011=CARTESIAN_POINT('Ctrl Pts',(18.5799074873355,-58.2097691178797,
3.36123028058441));
#251012=CARTESIAN_POINT('Ctrl Pts',(18.7004428147392,-58.1705159385204,
3.36099641108505));
#251013=CARTESIAN_POINT('Ctrl Pts',(18.714375808615,-58.2133972843966,3.23423043688396));
#251014=CARTESIAN_POINT('Ctrl Pts',(18.6064173144584,-58.2906472745451,
3.41054258905244));
#251015=CARTESIAN_POINT('Ctrl Pts',(18.7268501353368,-58.2517893143846,
3.41008815825988));
#251016=CARTESIAN_POINT('Ctrl Pts',(18.7538265876725,-58.3348142976307,
3.30819867304288));
#251017=CARTESIAN_POINT('Ctrl Pts',(18.6203878281154,-58.3332704847792,
3.48823028058442));
#251018=CARTESIAN_POINT('Ctrl Pts',(18.7407822670309,-58.2946680067384,
3.48794691941558));
#251019=CARTESIAN_POINT('Ctrl Pts',(18.7746174535806,-58.3988020033595,
3.42473028058443));
#251020=CARTESIAN_POINT('Origin',(18.5518699907157,-58.1242364370953,3.23423028058441));
#251021=CARTESIAN_POINT('Ctrl Pts',(18.0743352474898,-56.652678110832,3.47153072139033));
#251022=CARTESIAN_POINT('Ctrl Pts',(18.1949031876642,-56.6140134955958,
3.47122746285038));
#251023=CARTESIAN_POINT('Ctrl Pts',(18.2279043949855,-56.716192681671,3.4041304667674));
#251024=CARTESIAN_POINT('Ctrl Pts',(18.1097491035614,-56.7620702268155,
3.6555381345795));
#251025=CARTESIAN_POINT('Ctrl Pts',(18.2303840130647,-56.723211360369,3.65520336072128));
#251026=CARTESIAN_POINT('Ctrl Pts',(18.2563190096467,-56.8036438738762,
3.55128134519865));
#251027=CARTESIAN_POINT('Ctrl Pts',(18.1733695596544,-56.9585888550836,
3.77003198860224));
#251028=CARTESIAN_POINT('Ctrl Pts',(18.2941747571344,-56.9195374698047,
3.76980209314177));
#251029=CARTESIAN_POINT('Ctrl Pts',(18.307364587184,-56.9607460083088,3.64284195387389));
#251030=CARTESIAN_POINT('Ctrl Pts',(18.2401996527051,-57.1650137687743,
3.77003198860223));
#251031=CARTESIAN_POINT('Ctrl Pts',(18.3611647564563,-57.1257098240087,
3.77003198860223));
#251032=CARTESIAN_POINT('Ctrl Pts',(18.3609836949701,-57.1257686544518,
3.64284189403747));
#251033=CARTESIAN_POINT('Origin',(18.2401996527051,-57.1650137687743,3.64303198860223));
#251034=CARTESIAN_POINT('Origin',(5.49583002221492,-17.9418771653397,3.23423028058469));
#251035=CARTESIAN_POINT('Origin',(18.5051441132848,-57.980428973366,3.23423028058441));
#251036=CARTESIAN_POINT('Origin',(5.47329194811203,-17.8725121057136,3.6430319886025));
#251037=CARTESIAN_POINT('Origin',(18.3641788932763,-57.5467470426658,3.64299171721758));
#251038=CARTESIAN_POINT('Ctrl Pts',(18.4366189870679,-57.7713971777983,
3.48823028058441));
#251039=CARTESIAN_POINT('Ctrl Pts',(18.5581069080667,-57.7324510618066,
3.48852004212219));
#251040=CARTESIAN_POINT('Ctrl Pts',(18.5239649837014,-57.6273730232601,
3.42473028058441));
#251041=CARTESIAN_POINT('Ctrl Pts',(18.4506394153723,-57.8141635875295,
3.41028005848366));
#251042=CARTESIAN_POINT('Ctrl Pts',(18.57194072531,-57.7750271733914,3.41074404220208));
#251043=CARTESIAN_POINT('Ctrl Pts',(18.5448261124699,-57.6915769758378,
3.30780486243811));
#251044=CARTESIAN_POINT('Ctrl Pts',(18.477200500637,-57.8951845615406,3.36123028058441));
#251045=CARTESIAN_POINT('Ctrl Pts',(18.5981804828674,-57.8557848432471,
3.36146460586471));
#251046=CARTESIAN_POINT('Ctrl Pts',(18.5843471808463,-57.8132103173514,
3.23423045308441));
#251047=CARTESIAN_POINT('Ctrl Pts',(18.5051441132848,-57.980428973366,3.36123028058441));
#251048=CARTESIAN_POINT('Ctrl Pts',(18.6259282908542,-57.9411838150804,
3.36123028058441));
#251049=CARTESIAN_POINT('Ctrl Pts',(18.6259282908542,-57.9411838150804,
3.23423028058441));
#251050=CARTESIAN_POINT('Origin',(18.4031808061319,-57.6666181815458,3.4247302805844));
#251051=CARTESIAN_POINT('Origin',(18.3780421908689,-57.5892494801764,3.56563113524746));
#251052=CARTESIAN_POINT('Origin',(25.2734729067949,-55.9845461696113,3.56647653909447));
#251053=CARTESIAN_POINT('Origin',(25.2915084057465,-56.0249274780504,3.64299466007821));
#251054=CARTESIAN_POINT('Origin',(25.2401862573148,-55.9097831300742,3.42473028058445));
#251055=CARTESIAN_POINT('Ctrl Pts',(25.1949317875307,-55.8095395120002,
3.48823028058445));
#251056=CARTESIAN_POINT('Ctrl Pts',(25.079631183696,-55.8614118841074,3.48794691941561));
#251057=CARTESIAN_POINT('Ctrl Pts',(25.1241659841942,-55.9614386837448,
3.42473028058446));
#251058=CARTESIAN_POINT('Ctrl Pts',(25.176732112911,-55.7683775656457,3.41028005925051));
#251059=CARTESIAN_POINT('Ctrl Pts',(25.0612313830316,-55.8200852551801,
3.40982512230935));
#251060=CARTESIAN_POINT('Ctrl Pts',(25.0967080045986,-55.899767051836,3.30780486372789));
#251061=CARTESIAN_POINT('Ctrl Pts',(25.1422534028254,-55.690396180789,3.36123028058443));
#251062=CARTESIAN_POINT('Ctrl Pts',(25.0264120100495,-55.7418796630212,
3.36099721048522));
#251063=CARTESIAN_POINT('Ctrl Pts',(25.0446893032929,-55.7829311357726,
3.23423045308423));
#251064=CARTESIAN_POINT('Ctrl Pts',(25.1059793847708,-55.6083495590297,
3.36123028058442));
#251065=CARTESIAN_POINT('Ctrl Pts',(24.9899591116502,-55.6600051127003,
3.36123028058442));
#251066=CARTESIAN_POINT('Ctrl Pts',(24.9899591116502,-55.6600051127003,
3.23423028058442));
#251067=CARTESIAN_POINT('Origin',(25.1059793847708,-55.6083495590297,3.23423028058442));
#251068=CARTESIAN_POINT('Origin',(0.29005068280153,0.129138884176754,3.64303198860263));
#251069=CARTESIAN_POINT('Origin',(25.454706393409,-56.3916032444846,3.64303198860224));
#251070=CARTESIAN_POINT('Origin',(0.29005068280153,0.129138884176756,3.23423028058481));
#251071=CARTESIAN_POINT('Origin',(25.0444775033954,-55.4702140717962,3.23423028058442));
#251072=CARTESIAN_POINT('Ctrl Pts',(25.6742415049986,-56.883337725539,3.47153072139032));
#251073=CARTESIAN_POINT('Ctrl Pts',(25.5577357840975,-56.9357219056855,
3.47182327902622));
#251074=CARTESIAN_POINT('Ctrl Pts',(25.5138485805643,-56.8366797759148,
3.40413028958989));
#251075=CARTESIAN_POINT('Ctrl Pts',(25.6273680143751,-56.7783442778547,
3.65553807120917));
#251076=CARTESIAN_POINT('Ctrl Pts',(25.5109042502509,-56.8305359187808,
3.65586275497006));
#251077=CARTESIAN_POINT('Ctrl Pts',(25.476448592932,-56.7526780286678,3.55128126837173));
#251078=CARTESIAN_POINT('Ctrl Pts',(25.5431608329964,-56.5897276738843,
3.77003198860224));
#251079=CARTESIAN_POINT('Ctrl Pts',(25.4268390553482,-56.6417212312958,
3.7702550574829));
#251080=CARTESIAN_POINT('Ctrl Pts',(25.4092610357543,-56.6017723050721,
3.64284211731164));
#251081=CARTESIAN_POINT('Ctrl Pts',(25.454706393409,-56.3916032444846,3.77003198860224));
#251082=CARTESIAN_POINT('Ctrl Pts',(25.3385127913802,-56.4433359691571,
3.77003198860224));
#251083=CARTESIAN_POINT('Ctrl Pts',(25.3386862495677,-56.4432587405963,
3.64284239821661));
#251084=CARTESIAN_POINT('Origin',(25.6299342605002,-56.7851714777843,3.40423097483271));
#251085=CARTESIAN_POINT('Ctrl Pts',(25.0444775033954,-55.4702140717962,
3.36123028058442));
#251086=CARTESIAN_POINT('Ctrl Pts',(24.9284572302748,-55.5218696254668,
3.36123028058442));
#251087=CARTESIAN_POINT('Ctrl Pts',(24.9284572302748,-55.5218696254668,
3.23423028058442));
#251088=CARTESIAN_POINT('Ctrl Pts',(25.0080814159075,-55.3878899076689,
3.36123028058442));
#251089=CARTESIAN_POINT('Ctrl Pts',(24.891811449322,-55.4395618538377,3.36146538610203));
#251090=CARTESIAN_POINT('Ctrl Pts',(24.8735420580991,-55.3985281293151,
3.23423043688475));
#251091=CARTESIAN_POINT('Ctrl Pts',(24.9736678430987,-55.3100454158608,
3.41054258693061));
#251092=CARTESIAN_POINT('Ctrl Pts',(24.8573359723247,-55.362128664703,3.41100608859636));
#251093=CARTESIAN_POINT('Ctrl Pts',(24.8216158475492,-55.2818999508905,
3.30819866970666));
#251094=CARTESIAN_POINT('Ctrl Pts',(24.9555320242421,-55.2690209153036,
3.48823028058443));
#251095=CARTESIAN_POINT('Ctrl Pts',(24.8391888661851,-55.3213695969751,
3.48852004212221));
#251096=CARTESIAN_POINT('Ctrl Pts',(24.7942503289613,-55.2204359898052,
3.42473028058442));
#251097=CARTESIAN_POINT('Origin',(24.910270602082,-55.1687804361345,3.42473028058442));
#251098=CARTESIAN_POINT('Origin',(25.7023940320527,-56.9479187893833,3.11913648178429));
#251099=CARTESIAN_POINT('Origin',(25.7748538035653,-57.110666100766,2.83404198860222));
#251100=CARTESIAN_POINT('Origin',(24.8771824671431,-55.0944632682972,3.56563113460811));
#251101=CARTESIAN_POINT('Origin',(24.859045223961,-55.053601445953,3.64299171721715));
#251102=CARTESIAN_POINT('Ctrl Pts',(25.6197038181304,-57.5052637377727,
2.59908173515983));
#251103=CARTESIAN_POINT('Ctrl Pts',(25.6045223014068,-57.4711877340324,
2.65878198860222));
#251104=CARTESIAN_POINT('Ctrl Pts',(25.5758735661215,-57.4068835917975,
2.65878198860222));
#251105=CARTESIAN_POINT('Ctrl Pts',(25.7001924885135,-57.4694043465856,
2.59908193475659));
#251106=CARTESIAN_POINT('Ctrl Pts',(25.6631501095112,-57.4450643815374,
2.65878715325396));
#251107=CARTESIAN_POINT('Ctrl Pts',(25.622459862445,-57.3861185493431,2.65878198860222));
#251108=CARTESIAN_POINT('Ctrl Pts',(25.7642825572407,-57.413464248775,2.63878778849814));
#251109=CARTESIAN_POINT('Ctrl Pts',(25.7077329912393,-57.3998804953988,
2.69564460180077));
#251110=CARTESIAN_POINT('Ctrl Pts',(25.6552692732812,-57.3441059191827,
2.68180481624851));
#251111=CARTESIAN_POINT('Ctrl Pts',(25.8321626496797,-57.3036982377896,
2.75443238878623));
#251112=CARTESIAN_POINT('Ctrl Pts',(25.7409042554415,-57.3186021074444,
2.79268340777047));
#251113=CARTESIAN_POINT('Ctrl Pts',(25.6821129719831,-57.2526112478166,
2.74885926835563));
#251114=CARTESIAN_POINT('Ctrl Pts',(25.8376543496551,-57.2503778226938,
2.82856655361616));
#251115=CARTESIAN_POINT('Ctrl Pts',(25.7289491719118,-57.2821097063799,
2.85384197230757));
#251116=CARTESIAN_POINT('Ctrl Pts',(25.6773293952372,-57.2038640469257,
2.79184624278425));
#251117=CARTESIAN_POINT('Ctrl Pts',(25.8191582032627,-57.2088336324694,
2.90134173515984));
#251118=CARTESIAN_POINT('Ctrl Pts',(25.702828419034,-57.261135792072,2.90163218716352));
#251119=CARTESIAN_POINT('Ctrl Pts',(25.6588335304447,-57.1623216544366,
2.83404198860222));
#251120=CARTESIAN_POINT('Origin',(25.5758735661215,-57.4068835917975,2.53178198860222));
#251121=CARTESIAN_POINT('Origin',(0.29005068280153,0.129138884176754,3.64303198860263));
#251122=CARTESIAN_POINT('Origin',(24.6957503380314,-54.6869600343293,3.64303198860224));
#251123=CARTESIAN_POINT('Origin',(5.59761027822878E-15,1.86033184299798E-13,
2.53178198860262));
#251124=CARTESIAN_POINT('Origin',(25.5480287005725,-57.4192809246784,2.53178198860222));
#251125=CARTESIAN_POINT('Ctrl Pts',(24.6957503380314,-54.6869600343293,
3.77003198860225));
#251126=CARTESIAN_POINT('Ctrl Pts',(24.5795562613022,-54.738692970352,3.77003198860225));
#251127=CARTESIAN_POINT('Ctrl Pts',(24.5797301948987,-54.7386155301255,
3.64284187936967));
#251128=CARTESIAN_POINT('Ctrl Pts',(24.60728817496,-54.4888352915925,3.77003198860225));
#251129=CARTESIAN_POINT('Ctrl Pts',(24.491381933528,-54.5406489234203,3.76980208962834));
#251130=CARTESIAN_POINT('Ctrl Pts',(24.5091541605509,-54.5800991622562,
3.64284193928303));
#251131=CARTESIAN_POINT('Ctrl Pts',(24.5230714236772,-54.3002245846698,
3.65553535416549));
#251132=CARTESIAN_POINT('Ctrl Pts',(24.4074205468504,-54.352067335484,3.65520057834545));
#251133=CARTESIAN_POINT('Ctrl Pts',(24.4419671033159,-54.4291945615841,
3.55127910964149));
#251134=CARTESIAN_POINT('Ctrl Pts',(24.4761921430398,-54.1952354911867,
3.47153072139034));
#251135=CARTESIAN_POINT('Ctrl Pts',(24.3607210114368,-54.2471777873468,
3.47122746281544));
#251136=CARTESIAN_POINT('Ctrl Pts',(24.4045675740915,-54.345193843959,3.40413045901214));
#251137=CARTESIAN_POINT('Origin',(24.5205222915158,-54.2933913980359,3.40423097483272));
#251138=CARTESIAN_POINT('Ctrl Pts',(25.2380597013437,-57.4675553545136,
2.90134173515984));
#251139=CARTESIAN_POINT('Ctrl Pts',(25.3547675996722,-57.4161024530839,
2.90163218716352));
#251140=CARTESIAN_POINT('Ctrl Pts',(25.3107727110829,-57.3172883154485,
2.83404198860222));
#251141=CARTESIAN_POINT('Ctrl Pts',(25.2565651278916,-57.5091180232687,
2.82853349835314));
#251142=CARTESIAN_POINT('Ctrl Pts',(25.3528749970549,-57.449567232889,2.85381483162242));
#251143=CARTESIAN_POINT('Ctrl Pts',(25.3292770036983,-57.3588496371378,
2.79182701594165));
#251144=CARTESIAN_POINT('Ctrl Pts',(25.2997972770064,-57.5405471770605,
2.75468822073607));
#251145=CARTESIAN_POINT('Ctrl Pts',(25.3720159720866,-57.4827148996383,
2.79286913083821));
#251146=CARTESIAN_POINT('Ctrl Pts',(25.3622324578626,-57.3948558336725,
2.7490076329787));
#251147=CARTESIAN_POINT('Ctrl Pts',(25.4257977880276,-57.563646315949,2.63954450640349));
#251148=CARTESIAN_POINT('Ctrl Pts',(25.4538910783603,-57.5124644612005,
2.69627684028803));
#251149=CARTESIAN_POINT('Ctrl Pts',(25.4475597357244,-57.4360631077222,
2.68224356036454));
#251150=CARTESIAN_POINT('Ctrl Pts',(25.511038551389,-57.5536211289084,2.59908178706398));
#251151=CARTESIAN_POINT('Ctrl Pts',(25.5177778164713,-57.5097883065927,
2.65878704321368));
#251152=CARTESIAN_POINT('Ctrl Pts',(25.5012707422386,-57.4400754463043,
2.65878198860223));
#251153=CARTESIAN_POINT('Ctrl Pts',(25.5918112338801,-57.5176823163884,
2.59908173515984));
#251154=CARTESIAN_POINT('Ctrl Pts',(25.5766462455183,-57.4835989537473,
2.65878198860223));
#251155=CARTESIAN_POINT('Ctrl Pts',(25.5480287005725,-57.4192809246784,
2.65878198860223));
#251156=CARTESIAN_POINT('Origin',(25.1947524379623,-57.3689438691191,2.83404198860222));
#251157=CARTESIAN_POINT('Origin',(24.4480624203097,-54.1306438627461,3.11913648166974));
#251158=CARTESIAN_POINT('Origin',(24.3756025490945,-53.967896327293,2.83404198860224));
#251159=CARTESIAN_POINT('Origin',(25.122292666488,-57.2061965577009,3.11913648177378));
#251160=CARTESIAN_POINT('Origin',(25.0498328948971,-57.0434492461374,3.4042309748327));
#251161=CARTESIAN_POINT('Ctrl Pts',(24.3312692531094,-53.869741842014,2.90134173515986));
#251162=CARTESIAN_POINT('Ctrl Pts',(24.2159747902193,-53.9216078643412,
2.90103711553192));
#251163=CARTESIAN_POINT('Ctrl Pts',(24.2595822759739,-54.0195518809636,
2.83404198860224));
#251164=CARTESIAN_POINT('Ctrl Pts',(24.3127882662185,-53.8282341734838,
2.82862991747925));
#251165=CARTESIAN_POINT('Ctrl Pts',(24.2176496934273,-53.8880114973697,
2.8531404588629));
#251166=CARTESIAN_POINT('Ctrl Pts',(24.2411010091831,-53.9780422761232,
2.79187960999868));
#251167=CARTESIAN_POINT('Ctrl Pts',(24.2697746459847,-53.7969955864423,
2.7547062579329));
#251168=CARTESIAN_POINT('Ctrl Pts',(24.1983152114494,-53.8549480733037,
2.79224250381878));
#251169=CARTESIAN_POINT('Ctrl Pts',(24.2082687574728,-53.9422730280817,
2.74901809108215));
#251170=CARTESIAN_POINT('Ctrl Pts',(24.1443388226044,-53.7744913425361,
2.63947868311661));
#251171=CARTESIAN_POINT('Ctrl Pts',(24.116516742923,-53.8256450222186,2.69595066767865));
#251172=CARTESIAN_POINT('Ctrl Pts',(24.123203223048,-53.9017956184501,2.68220539436032));
#251173=CARTESIAN_POINT('Ctrl Pts',(24.0595120258539,-53.7848917482044,
2.59908178585034));
#251174=CARTESIAN_POINT('Ctrl Pts',(24.0529122166844,-53.8286685158623,
2.65877670944859));
#251175=CARTESIAN_POINT('Ctrl Pts',(24.0696665464389,-53.8982652496122,
2.65878198860225));
#251176=CARTESIAN_POINT('Ctrl Pts',(23.979166327502,-53.8206887816831,2.59908173515986));
#251177=CARTESIAN_POINT('Ctrl Pts',(23.9943483786823,-53.8547645473076,
2.65878198860225));
#251178=CARTESIAN_POINT('Ctrl Pts',(24.0229981225303,-53.919068240199,2.65878198860225));
#251179=CARTESIAN_POINT('Origin',(24.0229981225303,-53.919068240199,2.53178198860225));
#251180=CARTESIAN_POINT('Ctrl Pts',(24.8746050278059,-56.6498810128377,
3.77003198860224));
#251181=CARTESIAN_POINT('Ctrl Pts',(24.9907986398452,-56.5981482837082,
3.77003198860224));
#251182=CARTESIAN_POINT('Ctrl Pts',(24.9906251716322,-56.5982255167326,
3.64284238727508));
#251183=CARTESIAN_POINT('Ctrl Pts',(24.962653969475,-56.8481896769742,3.77003198860223));
#251184=CARTESIAN_POINT('Ctrl Pts',(25.079127190573,-56.7965362315712,3.77025506105937));
#251185=CARTESIAN_POINT('Ctrl Pts',(25.0612010539381,-56.7567415443521,
3.64284210641882));
#251186=CARTESIAN_POINT('Ctrl Pts',(25.0464771582534,-57.036975459332,3.65553527987793));
#251187=CARTESIAN_POINT('Ctrl Pts',(25.163192587334,-56.9853490357273,3.65585996533029));
#251188=CARTESIAN_POINT('Ctrl Pts',(25.1283880784749,-56.9076460727654,
3.55127902710107));
#251189=CARTESIAN_POINT('Ctrl Pts',(25.0931373005752,-57.1420619865017,
3.47153072139031));
#251190=CARTESIAN_POINT('Ctrl Pts',(25.210023886751,-57.0905332166514,3.47182327905148));
#251191=CARTESIAN_POINT('Ctrl Pts',(25.1657874977299,-56.9916465440533,
3.4041302837792));
#251192=CARTESIAN_POINT('Origin',(24.8746050278059,-56.6498810128377,3.64303198860224));
#251193=CARTESIAN_POINT('Origin',(5.68853496937358E-15,1.86271140789742E-13,
2.53178198860262));
#251194=CARTESIAN_POINT('Origin',(23.9951532569813,-53.93146557308,2.53178198860225));
#251195=CARTESIAN_POINT('Origin',(10.0037024164492,-23.2492868865832,3.64303198860246));
#251196=CARTESIAN_POINT('Origin',(24.7113125977916,-56.2832472948501,3.64299466007465));
#251197=CARTESIAN_POINT('Ctrl Pts',(23.9513722670371,-53.8330634946833,
2.59908173515986));
#251198=CARTESIAN_POINT('Ctrl Pts',(23.966536720823,-53.8671470951726,2.65878198860225));
#251199=CARTESIAN_POINT('Ctrl Pts',(23.9951532569813,-53.93146557308,2.65878198860225));
#251200=CARTESIAN_POINT('Ctrl Pts',(23.8712821658127,-53.8686972660496,
2.59908193199887));
#251201=CARTESIAN_POINT('Ctrl Pts',(23.9081865738555,-53.8931046959176,
2.6587768580666));
#251202=CARTESIAN_POINT('Ctrl Pts',(23.9486256024606,-53.9521563342727,
2.65878198860225));
#251203=CARTESIAN_POINT('Ctrl Pts',(23.8071866393159,-53.9240892607408,
2.63872492669778));
#251204=CARTESIAN_POINT('Ctrl Pts',(23.8635355386147,-53.9378509529596,
2.69532212015233));
#251205=CARTESIAN_POINT('Ctrl Pts',(23.9155750846182,-53.9937257232522,
2.68176836726611));
#251206=CARTESIAN_POINT('Ctrl Pts',(23.7392497560577,-54.0330064121708,
2.75442176402196));
#251207=CARTESIAN_POINT('Ctrl Pts',(23.8300830854584,-54.0187512923756,
2.7920317992011));
#251208=CARTESIAN_POINT('Ctrl Pts',(23.8883623535223,-54.0845104630309,
2.74885310748125));
#251209=CARTESIAN_POINT('Ctrl Pts',(23.7337507958623,-54.0860594545419,
2.82866089558375));
#251210=CARTESIAN_POINT('Ctrl Pts',(23.8418399747441,-54.055350029128,2.85316563119103));
#251211=CARTESIAN_POINT('Ctrl Pts',(23.8930480394875,-54.133026567774,2.79189751796542));
#251212=CARTESIAN_POINT('Ctrl Pts',(23.7522229508834,-54.1275498658869,
2.90134173515987));
#251213=CARTESIAN_POINT('Ctrl Pts',(23.8679139708575,-54.0765745253531,
2.90103711553193));
#251214=CARTESIAN_POINT('Ctrl Pts',(23.9115214566121,-54.1745185419755,
2.83404198860225));
#251215=CARTESIAN_POINT('Origin',(23.7955011834915,-54.2261740956461,2.83404198860224));
#251216=CARTESIAN_POINT('Origin',(24.6933715410278,-56.2428239368551,3.56647653971807));
#251217=CARTESIAN_POINT('Origin',(24.6600848917118,-56.1680608984273,3.42473028058445));
#251218=CARTESIAN_POINT('Origin',(23.8679610547535,-54.388921631058,3.11913648168137));
#251219=CARTESIAN_POINT('Origin',(23.9404209259127,-54.551669166389,3.40423097483273));
#251220=CARTESIAN_POINT('Ctrl Pts',(24.5258780191677,-55.8666273273828,
3.36123028058442));
#251221=CARTESIAN_POINT('Ctrl Pts',(24.6418982922884,-55.8149717737122,
3.36123028058442));
#251222=CARTESIAN_POINT('Ctrl Pts',(24.6418982922884,-55.8149717737122,
3.23423028058442));
#251223=CARTESIAN_POINT('Ctrl Pts',(24.5627025231306,-55.9487607347562,
3.36123028058442));
#251224=CARTESIAN_POINT('Ctrl Pts',(24.678474470882,-55.8971232158784,3.36099641108666));
#251225=CARTESIAN_POINT('Ctrl Pts',(24.6968134595452,-55.9383132588163,
3.2342304368845));
#251226=CARTESIAN_POINT('Ctrl Pts',(24.5975211960739,-56.0264248009268,
3.41054258905248));
#251227=CARTESIAN_POINT('Ctrl Pts',(24.7132325104969,-55.9751910510436,
3.41008815825889));
#251228=CARTESIAN_POINT('Ctrl Pts',(24.7487396569155,-56.0549414076388,
3.30819867304241));
#251229=CARTESIAN_POINT('Ctrl Pts',(24.61587051646,-56.0673542004321,3.48823028058444));
#251230=CARTESIAN_POINT('Ctrl Pts',(24.7315703643342,-56.0163785451193,
3.48794691941561));
#251231=CARTESIAN_POINT('Ctrl Pts',(24.7761051648324,-56.1164053447567,
3.42473028058445));
#251232=CARTESIAN_POINT('Origin',(24.5258780191677,-55.8666273273828,3.23423028058442));
#251233=CARTESIAN_POINT('Ctrl Pts',(23.8971395307774,-54.4530463244688,
3.47153072139034));
#251234=CARTESIAN_POINT('Ctrl Pts',(24.0130054343472,-54.4019907365345,
3.47122746285038));
#251235=CARTESIAN_POINT('Ctrl Pts',(24.0565064909,-54.5001606088503,3.40413046676726));
#251236=CARTESIAN_POINT('Ctrl Pts',(23.9437939758159,-54.5581374230422,
3.6555381345795));
#251237=CARTESIAN_POINT('Ctrl Pts',(24.0597061770684,-54.5068816478246,
3.65520336072068));
#251238=CARTESIAN_POINT('Ctrl Pts',(24.0939065860604,-54.5841625982679,
3.55128134519838));
#251239=CARTESIAN_POINT('Ctrl Pts',(24.0276077026114,-54.7469293531943,
3.77003198860224));
#251240=CARTESIAN_POINT('Ctrl Pts',(24.1436691352879,-54.6954643138432,
3.76980209314288));
#251241=CARTESIAN_POINT('Ctrl Pts',(24.1610941752726,-54.7350683949964,
3.64284195387434));
#251242=CARTESIAN_POINT('Ctrl Pts',(24.1156489724283,-54.9452378026824,
3.77003198860225));
#251243=CARTESIAN_POINT('Ctrl Pts',(24.2318430357379,-54.8935048726344,
3.77003198860225));
#251244=CARTESIAN_POINT('Ctrl Pts',(24.231669115581,-54.8935823068772,3.6428418940372));
#251245=CARTESIAN_POINT('Origin',(24.1156489724283,-54.9452378026824,3.64303198860225));
#251246=CARTESIAN_POINT('Origin',(9.75435829333415,-22.68925081671,3.23423028058465));
#251247=CARTESIAN_POINT('Origin',(24.4643761377923,-55.7284918401493,3.23423028058442));
#251248=CARTESIAN_POINT('Origin',(9.71531210235053,-22.6015516358799,3.64303198860247));
#251249=CARTESIAN_POINT('Origin',(24.2788510342453,-55.311920542264,3.64299171721759));
#251250=CARTESIAN_POINT('Ctrl Pts',(24.374376627022,-55.5277679687678,3.48823028058443));
#251251=CARTESIAN_POINT('Ctrl Pts',(24.4911280468232,-55.476336257987,3.48852004212221));
#251252=CARTESIAN_POINT('Ctrl Pts',(24.4461895095995,-55.375402650817,3.42473028058442));
#251253=CARTESIAN_POINT('Ctrl Pts',(24.3927905570419,-55.5688345658067,
3.41028005848369));
#251254=CARTESIAN_POINT('Ctrl Pts',(24.5093364964853,-55.5172331055173,
3.41074404220213));
#251255=CARTESIAN_POINT('Ctrl Pts',(24.47364749942,-55.4370743056914,3.30780486243795));
#251256=CARTESIAN_POINT('Ctrl Pts',(24.4276751358093,-55.6466353090189,
3.36123028058442));
#251257=CARTESIAN_POINT('Ctrl Pts',(24.5438739850335,-55.5948055748771,
3.36146460586399));
#251258=CARTESIAN_POINT('Ctrl Pts',(24.5256662135201,-55.5539102504913,
3.23423045308425));
#251259=CARTESIAN_POINT('Ctrl Pts',(24.4643761377923,-55.7284918401493,
3.36123028058442));
#251260=CARTESIAN_POINT('Ctrl Pts',(24.5803964109129,-55.6768362864787,
3.36123028058442));
#251261=CARTESIAN_POINT('Ctrl Pts',(24.5803964109129,-55.6768362864787,
3.23423028058443));
#251262=CARTESIAN_POINT('Origin',(24.3301692364789,-55.4270582044877,3.42473028058442));
#251263=CARTESIAN_POINT('Origin',(24.2970811017196,-55.3527410377814,3.56563113524687));
#251264=CARTESIAN_POINT('Origin',(30.9870007556499,-53.036059683551,3.56647653909447));
#251265=CARTESIAN_POINT('Origin',(31.009158450368,-53.074334555967,3.64299466007827));
#251266=CARTESIAN_POINT('Origin',(30.9460815882875,-52.965185606084,3.42473028058447));
#251267=CARTESIAN_POINT('Ctrl Pts',(30.8905967158742,-52.870221513221,3.48823028058448));
#251268=CARTESIAN_POINT('Ctrl Pts',(30.7813498801538,-52.933861917979,3.48794691941564));
#251269=CARTESIAN_POINT('Ctrl Pts',(30.8360963620068,-53.028685606084,3.42473028058449));
#251270=CARTESIAN_POINT('Ctrl Pts',(30.8681941459792,-52.8311874403352,
3.41028005925052));
#251271=CARTESIAN_POINT('Ctrl Pts',(30.7587310665085,-52.8946849835364,
3.40982512230918));
#251272=CARTESIAN_POINT('Ctrl Pts',(30.8023423591864,-52.9702219582401,
3.30780486372862));
#251273=CARTESIAN_POINT('Ctrl Pts',(30.8257530395519,-52.7572372522452,
3.36123028058445));
#251274=CARTESIAN_POINT('Ctrl Pts',(30.7159277273276,-52.8205474253451,
3.36099721048575));
#251275=CARTESIAN_POINT('Ctrl Pts',(30.7383959430076,-52.8594635164567,
3.23423045308295));
#251276=CARTESIAN_POINT('Ctrl Pts',(30.781101527075,-52.6794317578282,3.36123028058445));
#251277=CARTESIAN_POINT('Ctrl Pts',(30.6711163007943,-52.7429317578282,
3.36123028058445));
#251278=CARTESIAN_POINT('Ctrl Pts',(30.6711163007943,-52.7429317578282,
3.23423028058445));
#251279=CARTESIAN_POINT('Origin',(30.781101527075,-52.6794317578282,3.23423028058445));
#251280=CARTESIAN_POINT('Origin',(0.274963065701563,0.158750000000187,3.64303198860263));
#251281=CARTESIAN_POINT('Origin',(31.2097904767612,-53.4219427993281,3.64303198860226));
#251282=CARTESIAN_POINT('Origin',(0.274963065701563,0.15875000000019,3.23423028058481));
#251283=CARTESIAN_POINT('Origin',(30.7054974692375,-52.5484816883954,3.23423028058445));
#251284=CARTESIAN_POINT('Ctrl Pts',(31.4795232016796,-53.8880358395965,
3.47153072139034));
#251285=CARTESIAN_POINT('Ctrl Pts',(31.3691313491582,-53.9523112176906,
3.47182327902625));
#251286=CARTESIAN_POINT('Ctrl Pts',(31.3151318426942,-53.8583991130125,
3.40413028959004));
#251287=CARTESIAN_POINT('Ctrl Pts',(31.4219316852033,-53.7885171709467,
3.65553807120918));
#251288=CARTESIAN_POINT('Ctrl Pts',(31.3115614337847,-53.8525966788944,
3.65586275496689));
#251289=CARTESIAN_POINT('Ctrl Pts',(31.2691561625549,-53.778766899358,3.55128126837125));
#251290=CARTESIAN_POINT('Ctrl Pts',(31.3184699958148,-53.609735875734,3.77003198860225));
#251291=CARTESIAN_POINT('Ctrl Pts',(31.2082202476924,-53.6736035436592,
3.77025505748722));
#251292=CARTESIAN_POINT('Ctrl Pts',(31.1865627224611,-53.6357108652109,
3.64284211731213));
#251293=CARTESIAN_POINT('Ctrl Pts',(31.2097904767612,-53.4219427993281,
3.77003198860226));
#251294=CARTESIAN_POINT('Ctrl Pts',(31.0996409376528,-53.4855376653835,
3.77003198860226));
#251295=CARTESIAN_POINT('Ctrl Pts',(31.0998053730353,-53.4854427285712,
3.64284239821688));
#251296=CARTESIAN_POINT('Origin',(31.4251975098799,-53.7950387249973,3.40423097483273));
#251297=CARTESIAN_POINT('Ctrl Pts',(30.7054974692375,-52.5484816883954,
3.36123028058445));
#251298=CARTESIAN_POINT('Ctrl Pts',(30.5955122429569,-52.6119816883954,
3.36123028058445));
#251299=CARTESIAN_POINT('Ctrl Pts',(30.5955122429569,-52.6119816883954,
3.23423028058445));
#251300=CARTESIAN_POINT('Ctrl Pts',(30.6606955449581,-52.4704129317475,
3.36123028058446));
#251301=CARTESIAN_POINT('Ctrl Pts',(30.5504637065427,-52.5339553345204,
3.36146538610016));
#251302=CARTESIAN_POINT('Ctrl Pts',(30.5280052047897,-52.4950560684212,
3.23423043688334));
#251303=CARTESIAN_POINT('Ctrl Pts',(30.6183335281992,-52.3965920780919,
3.41054258693063));
#251304=CARTESIAN_POINT('Ctrl Pts',(30.5080831175497,-52.4605500011269,
3.41100608859759));
#251305=CARTESIAN_POINT('Ctrl Pts',(30.4641724871917,-52.3844945583564,
3.30819866970833));
#251306=CARTESIAN_POINT('Ctrl Pts',(30.5960088312575,-52.3576880233157,
3.48823028058444));
#251307=CARTESIAN_POINT('Ctrl Pts',(30.4857749404426,-52.4219111049551,
3.48852004212222));
#251308=CARTESIAN_POINT('Ctrl Pts',(30.4305321463783,-52.3262277788836,
3.42473028058444));
#251309=CARTESIAN_POINT('Origin',(30.5405173726589,-52.2627277788836,3.42473028058445));
#251310=CARTESIAN_POINT('Origin',(31.5142720656055,-53.9493203812242,3.11913648178368));
#251311=CARTESIAN_POINT('Origin',(31.6033466212672,-54.1036020372433,2.83404198860224));
#251312=CARTESIAN_POINT('Origin',(30.4998422386366,-52.1922763801639,3.56563113460745));
#251313=CARTESIAN_POINT('Origin',(30.4775331296742,-52.1535342613178,3.64299171721798));
#251314=CARTESIAN_POINT('Ctrl Pts',(31.4902932482914,-54.5122556166605,
2.59908173515985));
#251315=CARTESIAN_POINT('Ctrl Pts',(31.4716329851996,-54.4799531854473,
2.65878198860224));
#251316=CARTESIAN_POINT('Ctrl Pts',(31.4364195775141,-54.4189959163058,
2.65878198860224));
#251317=CARTESIAN_POINT('Ctrl Pts',(31.566592666262,-54.4681793099452,2.59908193475597));
#251318=CARTESIAN_POINT('Ctrl Pts',(31.5272089901453,-54.4478446647263,
2.65878715325333));
#251319=CARTESIAN_POINT('Ctrl Pts',(31.4805801312541,-54.393475032962,2.65878198860224));
#251320=CARTESIAN_POINT('Ctrl Pts',(31.6244843104278,-54.4058464214479,
2.63878778849855));
#251321=CARTESIAN_POINT('Ctrl Pts',(31.5668246400003,-54.3982481205262,
2.69564460180097));
#251322=CARTESIAN_POINT('Ctrl Pts',(31.5088182930364,-54.3482630350898,
2.68180481624859));
#251323=CARTESIAN_POINT('Ctrl Pts',(31.6805188761703,-54.2895863184074,
2.75443238878586));
#251324=CARTESIAN_POINT('Ctrl Pts',(31.5913182835558,-54.3139476428153,
2.79268340777021));
#251325=CARTESIAN_POINT('Ctrl Pts',(31.5259511417539,-54.2544636505346,
2.74885926835559));
#251326=CARTESIAN_POINT('Ctrl Pts',(31.6804069909882,-54.2359839591646,
2.82856655361648));
#251327=CARTESIAN_POINT('Ctrl Pts',(31.5756141966219,-54.2789047974527,
2.85384197230916));
#251328=CARTESIAN_POINT('Ctrl Pts',(31.5160982999442,-54.2064835118368,
2.7918462427859));
#251329=CARTESIAN_POINT('Ctrl Pts',(31.6576696180591,-54.1966007261202,
2.90134173515986));
#251330=CARTESIAN_POINT('Ctrl Pts',(31.547444164929,-54.2607761425977,2.90163218716353));
#251331=CARTESIAN_POINT('Ctrl Pts',(31.4933613949865,-54.1671020372433,
2.83404198860224));
#251332=CARTESIAN_POINT('Origin',(31.4364195775141,-54.4189959163058,2.53178198860223));
#251333=CARTESIAN_POINT('Origin',(0.274963065701563,0.158750000000187,3.64303198860263));
#251334=CARTESIAN_POINT('Origin',(30.2768083268887,-51.8059703131941,3.64303198860226));
#251335=CARTESIAN_POINT('Origin',(5.58223212128129E-15,1.86025348737467E-13,
2.53178198860262));
#251336=CARTESIAN_POINT('Origin',(31.4100231232068,-54.4342359163058,2.53178198860224));
#251337=CARTESIAN_POINT('Ctrl Pts',(30.2768083268887,-51.8059703131941,
3.77003198860227));
#251338=CARTESIAN_POINT('Ctrl Pts',(30.1666583377722,-51.8695654390617,
3.77003198860227));
#251339=CARTESIAN_POINT('Ctrl Pts',(30.1668232238344,-51.8694702420493,
3.64284187936972));
#251340=CARTESIAN_POINT('Ctrl Pts',(30.1681210939109,-51.6181777324902,
3.77003198860227));
#251341=CARTESIAN_POINT('Ctrl Pts',(30.0582657983058,-51.6818230251218,
3.76980208963099));
#251342=CARTESIAN_POINT('Ctrl Pts',(30.080064340051,-51.7191994478426,3.64284193928307));
#251343=CARTESIAN_POINT('Ctrl Pts',(30.0646505034496,-51.4394033023496,
3.65553535416551));
#251344=CARTESIAN_POINT('Ctrl Pts',(29.9550522173029,-51.5030508615811,
3.6552005783431));
#251345=CARTESIAN_POINT('Ctrl Pts',(29.9974715145375,-51.5761444782072,
3.55127910964149));
#251346=CARTESIAN_POINT('Ctrl Pts',(30.0070536838164,-51.3398895692692,
3.47153072139037));
#251347=CARTESIAN_POINT('Ctrl Pts',(29.8976445635505,-51.4036173400343,
3.47122746281548));
#251348=CARTESIAN_POINT('Ctrl Pts',(29.9514963979204,-51.4965132406189,
3.40413045901218));
#251349=CARTESIAN_POINT('Origin',(30.0614010732043,-51.4328740054938,3.40423097483275));
#251350=CARTESIAN_POINT('Ctrl Pts',(31.1067982185541,-54.5146464769132,
2.90134173515986));
#251351=CARTESIAN_POINT('Ctrl Pts',(31.2174884860871,-54.4512761425977,
2.90163218716353));
#251352=CARTESIAN_POINT('Ctrl Pts',(31.1634057161447,-54.3576020372433,
2.83404198860224));
#251353=CARTESIAN_POINT('Ctrl Pts',(31.1295467523329,-54.5540471172212,
2.82853349835322));
#251354=CARTESIAN_POINT('Ctrl Pts',(31.2191042733523,-54.4847554296808,
2.85381483162266));
#251355=CARTESIAN_POINT('Ctrl Pts',(31.1861529813967,-54.397001456393,2.79182701594234));
#251356=CARTESIAN_POINT('Ctrl Pts',(31.1758273123594,-54.5807851087093,
2.75468822073598));
#251357=CARTESIAN_POINT('Ctrl Pts',(31.241605266786,-54.515720733338,2.792869130838));
#251358=CARTESIAN_POINT('Ctrl Pts',(31.2226915745269,-54.4293656242359,
2.74900763297872));
#251359=CARTESIAN_POINT('Ctrl Pts',(31.3035520968889,-54.5905870683097,
2.63954450640362));
#251360=CARTESIAN_POINT('Ctrl Pts',(31.326141528613,-54.5367490446502,2.69627684028817));
#251361=CARTESIAN_POINT('Ctrl Pts',(31.3118587536639,-54.4614280312961,
2.68224356036457));
#251362=CARTESIAN_POINT('Ctrl Pts',(31.3872779850338,-54.5717067142908,
2.59908178706425));
#251363=CARTESIAN_POINT('Ctrl Pts',(31.3893985541607,-54.5274095677407,
2.6587870432139));
#251364=CARTESIAN_POINT('Ctrl Pts',(31.3656949292504,-54.4598040608957,
2.65878198860224));
#251365=CARTESIAN_POINT('Ctrl Pts',(31.4638515574747,-54.5275217339714,
2.59908173515985));
#251366=CARTESIAN_POINT('Ctrl Pts',(31.445206962986,-54.495210256486,2.65878198860224));
#251367=CARTESIAN_POINT('Ctrl Pts',(31.4100231232068,-54.4342359163058,
2.65878198860224));
#251368=CARTESIAN_POINT('Origin',(31.053420489864,-54.4211020372433,2.83404198860224));
#251369=CARTESIAN_POINT('Origin',(29.9723263949905,-51.2785921372162,3.11913648166973));
#251370=CARTESIAN_POINT('Origin',(29.8832517167492,-51.1243102687779,2.83404198860226));
#251371=CARTESIAN_POINT('Origin',(30.9643459342406,-54.2668203811894,3.1191364817768));
#251372=CARTESIAN_POINT('Origin',(30.8752713784768,-54.1125387249973,3.40423097483274));
#251373=CARTESIAN_POINT('Ctrl Pts',(29.8289013456892,-51.0313275753403,
2.90134173515988));
#251374=CARTESIAN_POINT('Ctrl Pts',(29.7196599535399,-51.0949610231996,
2.90103711553193));
#251375=CARTESIAN_POINT('Ctrl Pts',(29.7732664904686,-51.1878102687779,
2.83404198860226));
#251376=CARTESIAN_POINT('Ctrl Pts',(29.8061828667731,-50.9919790793205,
2.82862991747924));
#251377=CARTESIAN_POINT('Ctrl Pts',(29.7178139048437,-51.0613736255825,
2.85314045886342));
#251378=CARTESIAN_POINT('Ctrl Pts',(29.7505475307862,-51.1484598763129,
2.79187960999871));
#251379=CARTESIAN_POINT('Ctrl Pts',(29.760139558153,-50.9654077681503,2.75470625793292));
#251380=CARTESIAN_POINT('Ctrl Pts',(29.6951292702716,-51.0305123301026,
2.79224250381854));
#251381=CARTESIAN_POINT('Ctrl Pts',(29.7141562330561,-51.1163184807715,
2.74901809108226));
#251382=CARTESIAN_POINT('Ctrl Pts',(29.6330385513056,-50.9561384187033,
2.63947868311661));
#251383=CARTESIAN_POINT('Ctrl Pts',(29.610715899415,-51.0099200724105,2.69595066767883));
#251384=CARTESIAN_POINT('Ctrl Pts',(29.6253256551035,-51.0849545802159,
2.68220539436023));
#251385=CARTESIAN_POINT('Ctrl Pts',(29.5497635830447,-50.9753486645692,
2.59908178584971));
#251386=CARTESIAN_POINT('Ctrl Pts',(29.5477758465698,-51.019575486422,2.65877670944804));
#251387=CARTESIAN_POINT('Ctrl Pts',(29.5717132339802,-51.0870396576403,
2.65878198860226));
#251388=CARTESIAN_POINT('Ctrl Pts',(29.4735998357344,-51.0193480105322,
2.59908173515988));
#251389=CARTESIAN_POINT('Ctrl Pts',(29.4922606054652,-51.0516501490681,
2.65878198860226));
#251390=CARTESIAN_POINT('Ctrl Pts',(29.5274749692191,-51.1126068659042,
2.65878198860226));
#251391=CARTESIAN_POINT('Origin',(29.5274749692191,-51.1126068659042,2.53178198860226));
#251392=CARTESIAN_POINT('Ctrl Pts',(30.6598643453581,-53.7394427993281,
3.77003198860226));
#251393=CARTESIAN_POINT('Ctrl Pts',(30.7700138939561,-53.6758479277939,
3.77003198860225));
#251394=CARTESIAN_POINT('Ctrl Pts',(30.7698494490699,-53.6759428700932,
3.64284238727559));
#251395=CARTESIAN_POINT('Ctrl Pts',(30.7681598456276,-53.9274614872877,
3.77003198860225));
#251396=CARTESIAN_POINT('Ctrl Pts',(30.878595758964,-53.8639162380547,3.77025506105976));
#251397=CARTESIAN_POINT('Ctrl Pts',(30.8566081460799,-53.8262133418089,
3.6428421064193));
#251398=CARTESIAN_POINT('Ctrl Pts',(30.8712573299226,-54.1064511722683,
3.65553527987797));
#251399=CARTESIAN_POINT('Ctrl Pts',(30.9819369489464,-54.0429074791658,
3.65585996532834));
#251400=CARTESIAN_POINT('Ctrl Pts',(30.9392009315185,-53.9692682429945,
3.55127902710052));
#251401=CARTESIAN_POINT('Ctrl Pts',(30.9286463962985,-54.2060847114736,
3.47153072139035));
#251402=CARTESIAN_POINT('Ctrl Pts',(31.0395064423981,-54.1426202463868,
3.47182327905151));
#251403=CARTESIAN_POINT('Ctrl Pts',(30.9851759130209,-54.0488992470929,
3.4041302837795));
#251404=CARTESIAN_POINT('Origin',(30.6598643453581,-53.7394427993281,3.64303198860226));
#251405=CARTESIAN_POINT('Origin',(5.69400554112517E-15,1.86273928185272E-13,
2.53178198860262));
#251406=CARTESIAN_POINT('Origin',(29.5010785149117,-51.1278468659042,2.53178198860227));
#251407=CARTESIAN_POINT('Origin',(15.2806508669898,-27.1018636743469,3.64303198860243));
#251408=CARTESIAN_POINT('Origin',(30.4591427892377,-53.3918862459826,3.64299466007281));
#251409=CARTESIAN_POINT('Ctrl Pts',(29.4472515437741,-51.0345602039881,
2.59908173515988));
#251410=CARTESIAN_POINT('Ctrl Pts',(29.4658956314773,-51.0668719738972,
2.65878198860226));
#251411=CARTESIAN_POINT('Ctrl Pts',(29.5010785149117,-51.1278468659042,
2.65878198860226));
#251412=CARTESIAN_POINT('Ctrl Pts',(29.3713249278652,-51.0783704650302,
2.59908193199828));
#251413=CARTESIAN_POINT('Ctrl Pts',(29.4105784408362,-51.0987866273834,
2.65877685806608));
#251414=CARTESIAN_POINT('Ctrl Pts',(29.4569685172211,-51.1532877451673,
2.65878198860226));
#251415=CARTESIAN_POINT('Ctrl Pts',(29.3133705634518,-51.1401588234658,
2.63872492669764));
#251416=CARTESIAN_POINT('Ctrl Pts',(29.3708492661241,-51.1479550638445,
2.69532212015224));
#251417=CARTESIAN_POINT('Ctrl Pts',(29.4284442379237,-51.1980841325261,
2.68176836726597));
#251418=CARTESIAN_POINT('Ctrl Pts',(29.2571907880108,-51.2555806533506,
2.75442176402212));
#251419=CARTESIAN_POINT('Ctrl Pts',(29.346036457163,-51.2319089562571,2.79203179920123));
#251420=CARTESIAN_POINT('Ctrl Pts',(29.410870170353,-51.2912160489642,2.74885310748141));
#251421=CARTESIAN_POINT('Ctrl Pts',(29.2572675046856,-51.308917863463,2.82866089558365));
#251422=CARTESIAN_POINT('Ctrl Pts',(29.3615545506894,-51.2670782717299,
2.85316563119133));
#251423=CARTESIAN_POINT('Ctrl Pts',(29.420601501513,-51.3389765898561,2.79189751796506));
#251424=CARTESIAN_POINT('Ctrl Pts',(29.2799753962468,-51.348250120016,2.90134173515988));
#251425=CARTESIAN_POINT('Ctrl Pts',(29.389704274698,-51.2854610231996,2.90103711553194));
#251426=CARTESIAN_POINT('Ctrl Pts',(29.4433108116267,-51.3783102687779,
2.83404198860226));
#251427=CARTESIAN_POINT('Origin',(29.3333255853461,-51.441810268778,2.83404198860226));
#251428=CARTESIAN_POINT('Origin',(30.4370746239673,-53.3535596824661,3.56647653971762));
#251429=CARTESIAN_POINT('Origin',(30.3961554568843,-53.282685606084,3.42473028058449));
#251430=CARTESIAN_POINT('Origin',(29.4224002636298,-51.5960921371717,3.11913648168056));
#251431=CARTESIAN_POINT('Origin',(29.5114749418011,-51.7503740054938,3.40423097483275));
#251432=CARTESIAN_POINT('Ctrl Pts',(30.2311753956719,-52.9969317578282,
3.36123028058445));
#251433=CARTESIAN_POINT('Ctrl Pts',(30.3411606219525,-52.9334317578282,
3.36123028058445));
#251434=CARTESIAN_POINT('Ctrl Pts',(30.3411606219525,-52.9334317578282,
3.23423028058445));
#251435=CARTESIAN_POINT('Ctrl Pts',(30.2763834500047,-53.0747660209923,
3.36123028058445));
#251436=CARTESIAN_POINT('Ctrl Pts',(30.3861235964177,-53.0113099140571,
3.36099641108313));
#251437=CARTESIAN_POINT('Ctrl Pts',(30.4086676540725,-53.0503573673283,
3.23423043688312));
#251438=CARTESIAN_POINT('Ctrl Pts',(30.3191294881016,-53.148365092907,3.41054258905248));
#251439=CARTESIAN_POINT('Ctrl Pts',(30.4288515386959,-53.0853168809873,
3.41008815826136));
#251440=CARTESIAN_POINT('Ctrl Pts',(30.4725003554702,-53.1609188493334,
3.30819867304359));
#251441=CARTESIAN_POINT('Ctrl Pts',(30.3416565762243,-53.187152250617,3.48823028058447));
#251442=CARTESIAN_POINT('Ctrl Pts',(30.451394201312,-53.124361917979,3.48794691941563));
#251443=CARTESIAN_POINT('Ctrl Pts',(30.506140683165,-53.219185606084,3.42473028058448));
#251444=CARTESIAN_POINT('Origin',(30.2311753956718,-52.9969317578282,3.23423028058445));
#251445=CARTESIAN_POINT('Ctrl Pts',(29.458121752568,-51.6568155675422,3.47153072139037));
#251446=CARTESIAN_POINT('Ctrl Pts',(29.5680161684463,-51.5939283826156,
3.47122746285042));
#251447=CARTESIAN_POINT('Ctrl Pts',(29.6215404675523,-51.6870133715067,
3.40413046676754));
#251448=CARTESIAN_POINT('Ctrl Pts',(29.5155056307128,-51.7564542486368,
3.65553813457951));
#251449=CARTESIAN_POINT('Ctrl Pts',(29.6254251653831,-51.6933631336489,
3.65520336072092));
#251450=CARTESIAN_POINT('Ctrl Pts',(29.6675162799448,-51.766645814766,3.55128134519813));
#251451=CARTESIAN_POINT('Ctrl Pts',(29.6185943474811,-51.9354510367783,
3.77003198860227));
#251452=CARTESIAN_POINT('Ctrl Pts',(29.728640422008,-51.8721362050952,3.76980209314207));
#251453=CARTESIAN_POINT('Ctrl Pts',(29.7501097595413,-51.9097019182958,
3.64284195387483));
#251454=CARTESIAN_POINT('Ctrl Pts',(29.7268821954856,-52.1234703131941,
3.77003198860227));
#251455=CARTESIAN_POINT('Ctrl Pts',(29.8370321718801,-52.0598751946715,
3.77003198860227));
#251456=CARTESIAN_POINT('Ctrl Pts',(29.8368672985589,-52.0599703843279,
3.64284189403769));
#251457=CARTESIAN_POINT('Origin',(29.7268821954856,-52.1234703131941,3.64303198860227));
#251458=CARTESIAN_POINT('Origin',(14.9038494342991,-26.4492244485618,3.23423028058463));
#251459=CARTESIAN_POINT('Origin',(30.1555713378344,-52.8659816883954,3.23423028058444));
#251460=CARTESIAN_POINT('Origin',(14.8448439902567,-26.3470240215573,3.64303198860244));
#251461=CARTESIAN_POINT('Origin',(29.9275190026069,-52.4710850656378,3.64299171721745));
#251462=CARTESIAN_POINT('Ctrl Pts',(30.0450834959843,-52.675764913939,3.48823028058445));
#251463=CARTESIAN_POINT('Ctrl Pts',(30.1558192616008,-52.6124111049551,
3.48852004212223));
#251464=CARTESIAN_POINT('Ctrl Pts',(30.1005764675364,-52.5167277788836,
3.42473028058445));
#251465=CARTESIAN_POINT('Ctrl Pts',(30.0676891808495,-52.7146817640545,
3.41028005848372));
#251466=CARTESIAN_POINT('Ctrl Pts',(30.1782028480957,-52.6511806140151,
3.41074404220182));
#251467=CARTESIAN_POINT('Ctrl Pts',(30.1343304829266,-52.5751914484988,
3.3078048624383));
#251468=CARTESIAN_POINT('Ctrl Pts',(30.1105150503728,-52.7884098752449,
3.36123028058445));
#251469=CARTESIAN_POINT('Ctrl Pts',(30.2206596676797,-52.7247179826669,
3.36146460586487));
#251470=CARTESIAN_POINT('Ctrl Pts',(30.1982769148329,-52.6859499175233,
3.23423045308358));
#251471=CARTESIAN_POINT('Ctrl Pts',(30.1555713378344,-52.8659816883954,
3.36123028058445));
#251472=CARTESIAN_POINT('Ctrl Pts',(30.265556564115,-52.8024816883954,3.36123028058445));
#251473=CARTESIAN_POINT('Ctrl Pts',(30.265556564115,-52.8024816883954,3.23423028058445));
#251474=CARTESIAN_POINT('Origin',(29.9905912412558,-52.5802277788836,3.42473028058445));
#251475=CARTESIAN_POINT('Origin',(29.9499161075317,-52.5097763812719,3.56563113524751));
#251476=CARTESIAN_POINT('Origin',(36.3610285397826,-49.5064990290875,3.56647653909407));
#251477=CARTESIAN_POINT('Origin',(36.3870656659267,-49.5422481179701,3.64299466007515));
#251478=CARTESIAN_POINT('Origin',(36.3129251734949,-49.440290424916,3.4247302805845));
#251479=CARTESIAN_POINT('Ctrl Pts',(36.2478178023256,-49.3516463037379,
3.4882302805845));
#251480=CARTESIAN_POINT('Ctrl Pts',(36.1458216659131,-49.4263574835545,
3.48794691941566));
#251481=CARTESIAN_POINT('Ctrl Pts',(36.2101800152093,-49.5149391519571,
3.42473028058451));
#251482=CARTESIAN_POINT('Ctrl Pts',(36.2214577844001,-49.3151677697908,
3.41028005925053));
#251483=CARTESIAN_POINT('Ctrl Pts',(36.1192316557429,-49.389759474289,3.4098251223104));
#251484=CARTESIAN_POINT('Ctrl Pts',(36.1704998050817,-49.460324028137,3.30780486372858));
#251485=CARTESIAN_POINT('Ctrl Pts',(36.1715192752725,-49.2460589922049,
3.36123028058448));
#251486=CARTESIAN_POINT('Ctrl Pts',(36.0689133127053,-49.3205022166655,
3.36099721048417));
#251487=CARTESIAN_POINT('Ctrl Pts',(36.0953262843484,-49.3568565533015,
3.23423045308315));
#251488=CARTESIAN_POINT('Ctrl Pts',(36.1189794796889,-49.1733470784082,
3.36123028058448));
#251489=CARTESIAN_POINT('Ctrl Pts',(36.0162343214032,-49.2479958054493,
3.36123028058448));
#251490=CARTESIAN_POINT('Ctrl Pts',(36.0162343214032,-49.2479958054493,
3.23423028058448));
#251491=CARTESIAN_POINT('Origin',(36.1189794796889,-49.1733470784082,3.23423028058447));
#251492=CARTESIAN_POINT('Origin',(0.256862895714049,0.186621817603047,3.64303198860263));
#251493=CARTESIAN_POINT('Origin',(36.6229335645815,-49.866980369602,3.64303198860229));
#251494=CARTESIAN_POINT('Origin',(0.256862895714049,0.18662181760305,3.23423028058482));
#251495=CARTESIAN_POINT('Origin',(36.0301015792682,-49.0510171431398,3.23423028058447));
#251496=CARTESIAN_POINT('Ctrl Pts',(36.9399086546492,-50.3023253561989,
3.47153072139037));
#251497=CARTESIAN_POINT('Ctrl Pts',(36.8368401467443,-50.3777877177481,
3.47182327902627));
#251498=CARTESIAN_POINT('Ctrl Pts',(36.7733199672426,-50.2900345588333,
3.40413028958994));
#251499=CARTESIAN_POINT('Ctrl Pts',(36.8722300970264,-50.2093718139428,
3.65553807120923));
#251500=CARTESIAN_POINT('Ctrl Pts',(36.7691625978881,-50.2846371204149,
3.65586275497175));
#251501=CARTESIAN_POINT('Ctrl Pts',(36.7192723137713,-50.2156443459719,
3.5512812683729));
#251502=CARTESIAN_POINT('Ctrl Pts',(36.7506474475462,-50.0423845927719,
3.7700319886023));
#251503=CARTESIAN_POINT('Ctrl Pts',(36.6476776482602,-50.1174266236734,
3.77025505748201));
#251504=CARTESIAN_POINT('Ctrl Pts',(36.6221779017711,-50.0820053531135,
3.64284211731047));
#251505=CARTESIAN_POINT('Ctrl Pts',(36.6229335645815,-49.866980369602,3.77003198860229));
#251506=CARTESIAN_POINT('Ctrl Pts',(36.5200349097938,-49.9417406183798,
3.7700319886023));
#251507=CARTESIAN_POINT('Ctrl Pts',(36.5201885207831,-49.9416290134633,
3.64284239821669));
#251508=CARTESIAN_POINT('Origin',(36.876159719196,-50.2155162706038,3.40423097483275));
#251509=CARTESIAN_POINT('Ctrl Pts',(36.0301015792682,-49.0510171431398,
3.36123028058448));
#251510=CARTESIAN_POINT('Ctrl Pts',(35.9273564209826,-49.1256658701809,
3.36123028058448));
#251511=CARTESIAN_POINT('Ctrl Pts',(35.9273564209826,-49.1256658701809,
3.23423028058448));
#251512=CARTESIAN_POINT('Ctrl Pts',(35.9773846774571,-48.9780591316049,
3.36123028058447));
#251513=CARTESIAN_POINT('Ctrl Pts',(35.874398690302,-49.052775807121,3.36146538610047));
#251514=CARTESIAN_POINT('Ctrl Pts',(35.8479971380629,-49.0164371879487,
3.23423043688354));
#251515=CARTESIAN_POINT('Ctrl Pts',(35.9275383438695,-48.9090707128217,
3.41054258693067));
#251516=CARTESIAN_POINT('Ctrl Pts',(35.8245773199107,-48.9842025736611,
3.4110060885967));
#251517=CARTESIAN_POINT('Ctrl Pts',(35.7729572780235,-48.9131536812757,
3.30819866970723));
#251518=CARTESIAN_POINT('Ctrl Pts',(35.901269362891,-48.8727133447938,3.48823028058448));
#251519=CARTESIAN_POINT('Ctrl Pts',(35.7983524848941,-48.9481071848791,
3.48852004212226));
#251520=CARTESIAN_POINT('Ctrl Pts',(35.7334106856012,-48.8587224664495,
3.42473028058448));
#251521=CARTESIAN_POINT('Origin',(35.8361558438868,-48.7840737394083,3.42473028058447));
#251522=CARTESIAN_POINT('Origin',(36.9808731396208,-50.3596419293476,3.11913648178302));
#251523=CARTESIAN_POINT('Origin',(37.0855865599608,-50.5037675878939,2.83404198860227));
#251524=CARTESIAN_POINT('Origin',(35.7883393560615,-48.7182599900757,3.5656311346079));
#251525=CARTESIAN_POINT('Origin',(35.7621028045857,-48.6820620414853,3.64299171721735));
#251526=CARTESIAN_POINT('Ctrl Pts',(37.0158684358566,-50.9219998155894,
2.59908173515989));
#251527=CARTESIAN_POINT('Ctrl Pts',(36.9939338721439,-50.8918248690994,
2.65878198860227));
#251528=CARTESIAN_POINT('Ctrl Pts',(36.9525415975218,-50.834882333648,2.65878198860227));
#251529=CARTESIAN_POINT('Ctrl Pts',(37.087142649025,-50.8701895025855,2.59908193475562));
#251530=CARTESIAN_POINT('Ctrl Pts',(37.0458491715916,-50.8540829678232,
2.65878715325282));
#251531=CARTESIAN_POINT('Ctrl Pts',(36.993792576411,-50.8048852215544,2.65878198860227));
#251532=CARTESIAN_POINT('Ctrl Pts',(37.1382015956606,-50.8021467555728,
2.63878778849844));
#251533=CARTESIAN_POINT('Ctrl Pts',(37.0800635522222,-50.8006171556816,
2.69564460180099));
#251534=CARTESIAN_POINT('Ctrl Pts',(37.0171501059297,-50.756969208081,2.68180481624857));
#251535=CARTESIAN_POINT('Ctrl Pts',(37.1817767082792,-50.6806663304938,
2.75443238878602));
#251536=CARTESIAN_POINT('Ctrl Pts',(37.0956112176475,-50.7142182018854,
2.79268340777035));
#251537=CARTESIAN_POINT('Ctrl Pts',(37.0243843935853,-50.6618927960193,
2.74885926835567));
#251538=CARTESIAN_POINT('Ctrl Pts',(37.1760624637765,-50.6273693057699,
2.8285665536164));
#251539=CARTESIAN_POINT('Ctrl Pts',(37.0763301845694,-50.681008848973,2.8538419723086));
#251540=CARTESIAN_POINT('Ctrl Pts',(37.0095702365092,-50.6152053999558,
2.79184624278548));
#251541=CARTESIAN_POINT('Ctrl Pts',(37.1493329797266,-50.5905785208478,
2.90134173515986));
#251542=CARTESIAN_POINT('Ctrl Pts',(37.0464195108259,-50.6659240749077,
2.90163218716354));
#251543=CARTESIAN_POINT('Ctrl Pts',(36.9828414016752,-50.5784163149351,
2.83404198860226));
#251544=CARTESIAN_POINT('Origin',(36.9525415975218,-50.834882333648,2.53178198860226));
#251545=CARTESIAN_POINT('Origin',(0.256862895714049,0.186621817603047,3.64303198860263));
#251546=CARTESIAN_POINT('Origin',(35.5261472678871,-48.3573835402113,3.64303198860229));
#251547=CARTESIAN_POINT('Origin',(5.56775724677591E-15,1.86015948644053E-13,
2.53178198860263));
#251548=CARTESIAN_POINT('Origin',(36.9278827595332,-50.8527980281379,2.53178198860227));
#251549=CARTESIAN_POINT('Ctrl Pts',(35.5261472678871,-48.3573835402113,
3.7700319886023));
#251550=CARTESIAN_POINT('Ctrl Pts',(35.4232481927143,-48.4321440944168,
3.7700319886023));
#251551=CARTESIAN_POINT('Ctrl Pts',(35.4234022247162,-48.4320321836168,
3.64284187936949));
#251552=CARTESIAN_POINT('Ctrl Pts',(35.3984257650692,-48.181980616354,3.7700319886023));
#251553=CARTESIAN_POINT('Ctrl Pts',(35.2958250129008,-48.2567602586468,
3.76980208963083));
#251554=CARTESIAN_POINT('Ctrl Pts',(35.3214110399847,-48.2916533613424,
3.64284193928292));
#251555=CARTESIAN_POINT('Ctrl Pts',(35.2768349808773,-48.0150011530595,
3.65553535416552));
#251556=CARTESIAN_POINT('Ctrl Pts',(35.1744900671632,-48.0897561847294,
3.65520057834393));
#251557=CARTESIAN_POINT('Ctrl Pts',(35.2243173504695,-48.1580153629225,
3.55127910964204));
#251558=CARTESIAN_POINT('Ctrl Pts',(35.2091516650533,-47.9220530736681,
3.47153072139038));
#251559=CARTESIAN_POINT('Ctrl Pts',(35.1070032653413,-47.996868104246,3.47122746281548));
#251560=CARTESIAN_POINT('Ctrl Pts',(35.1702703594602,-48.0836260618766,
3.40413045901206));
#251561=CARTESIAN_POINT('Origin',(35.272920853982,-48.0088472823266,3.40423097483277));
#251562=CARTESIAN_POINT('Ctrl Pts',(36.634724144966,-50.9644637245887,2.90134173515988));
#251563=CARTESIAN_POINT('Ctrl Pts',(36.738184035969,-50.8898702560312,2.90163218716356));
#251564=CARTESIAN_POINT('Ctrl Pts',(36.6746059268184,-50.8023624960585,
2.83404198860226));
#251565=CARTESIAN_POINT('Ctrl Pts',(36.6614665482797,-51.0012706547892,
2.82853349835304));
#251566=CARTESIAN_POINT('Ctrl Pts',(36.7432905102111,-50.9229972443175,
2.85381483162273));
#251567=CARTESIAN_POINT('Ctrl Pts',(36.7013469409089,-50.8391683443877,
2.79182701594243));
#251568=CARTESIAN_POINT('Ctrl Pts',(36.7102884597173,-51.023024536943,2.75468822073628));
#251569=CARTESIAN_POINT('Ctrl Pts',(36.7689049964556,-50.9514409225348,
2.79286913083826));
#251570=CARTESIAN_POINT('Ctrl Pts',(36.7410683485318,-50.8675358949422,
2.74900763297879));
#251571=CARTESIAN_POINT('Ctrl Pts',(36.8383381382866,-51.0194219249358,
2.63954450640335));
#251572=CARTESIAN_POINT('Ctrl Pts',(36.8551762168621,-50.9635175930187,
2.69627684028801));
#251573=CARTESIAN_POINT('Ctrl Pts',(36.8330984946711,-50.8901021525735,
2.68224356036454));
#251574=CARTESIAN_POINT('Ctrl Pts',(36.9196318328649,-50.9918932610477,
2.5990817870642));
#251575=CARTESIAN_POINT('Ctrl Pts',(36.9171104726345,-50.9476171190672,
2.65878704321513));
#251576=CARTESIAN_POINT('Ctrl Pts',(36.8864699989244,-50.8828596657507,
2.65878198860226));
#251577=CARTESIAN_POINT('Ctrl Pts',(36.9911673391713,-50.9399462128196,
2.59908173515988));
#251578=CARTESIAN_POINT('Ctrl Pts',(36.9692474126346,-50.9097606317988,
2.65878198860226));
#251579=CARTESIAN_POINT('Ctrl Pts',(36.9278827595333,-50.8527980281379,
2.65878198860226));
#251580=CARTESIAN_POINT('Origin',(36.5718607685328,-50.8770112230996,2.83404198860226));
#251581=CARTESIAN_POINT('Origin',(35.1682072895751,-47.864721425496,3.11913648166955));
#251582=CARTESIAN_POINT('Origin',(35.0634937251227,-47.7205955685085,2.8340419886023));
#251583=CARTESIAN_POINT('Origin',(36.4671473482233,-50.7328855645155,3.11913648177506));
#251584=CARTESIAN_POINT('Origin',(36.3624339277679,-50.5887599058095,3.40423097483275));
#251585=CARTESIAN_POINT('Ctrl Pts',(34.9997217530266,-47.6338034047594,
2.90134173515991));
#251586=CARTESIAN_POINT('Ctrl Pts',(34.8977303031707,-47.7085070967798,
2.90103711553197));
#251587=CARTESIAN_POINT('Ctrl Pts',(34.9607485668371,-47.7952442955496,
2.83404198860229));
#251588=CARTESIAN_POINT('Ctrl Pts',(34.9730146904946,-47.5970451916065,
2.82862991747929));
#251589=CARTESIAN_POINT('Ctrl Pts',(34.8923835282618,-47.6752966590726,
2.85314045886503));
#251590=CARTESIAN_POINT('Ctrl Pts',(34.9340408279393,-47.758484246594,2.79187960999928));
#251591=CARTESIAN_POINT('Ctrl Pts',(34.924446153613,-47.5754322771529,2.75470625793294));
#251592=CARTESIAN_POINT('Ctrl Pts',(34.8665972787031,-47.6469756149918,
2.79224250381878));
#251593=CARTESIAN_POINT('Ctrl Pts',(34.894489194863,-47.730322851409,2.74901809108229));
#251594=CARTESIAN_POINT('Ctrl Pts',(34.7970725085262,-47.579499379098,2.63947868311666));
#251595=CARTESIAN_POINT('Ctrl Pts',(34.7804938560725,-47.635319763777,2.69595066767873));
#251596=CARTESIAN_POINT('Ctrl Pts',(34.8028668197836,-47.7084160893866,
2.68220539436026));
#251597=CARTESIAN_POINT('Ctrl Pts',(34.7162617467346,-47.6073089936879,
2.59908178585027));
#251598=CARTESIAN_POINT('Ctrl Pts',(34.7189078610127,-47.651501311424,2.65877670944819));
#251599=CARTESIAN_POINT('Ctrl Pts',(34.7497660430528,-47.7160937685323,
2.65878198860229));
#251600=CARTESIAN_POINT('Ctrl Pts',(34.6451144164191,-47.659028586093,2.59908173515991));
#251601=CARTESIAN_POINT('Ctrl Pts',(34.6670494534023,-47.6892031885508,
2.65878198860229));
#251602=CARTESIAN_POINT('Ctrl Pts',(34.7084426211237,-47.7461450747859,
2.65878198860229));
#251603=CARTESIAN_POINT('Origin',(34.7084426211237,-47.7461450747859,2.53178198860229));
#251604=CARTESIAN_POINT('Ctrl Pts',(36.1092077731534,-50.2402240048077,
3.77003198860229));
#251605=CARTESIAN_POINT('Ctrl Pts',(36.212106436806,-50.1654637495892,3.77003198860229));
#251606=CARTESIAN_POINT('Ctrl Pts',(36.2119528169387,-50.165575360956,3.64284238727548));
#251607=CARTESIAN_POINT('Ctrl Pts',(36.2365633238593,-50.4158927445,3.77003198860229));
#251608=CARTESIAN_POINT('Ctrl Pts',(36.3397519704552,-50.3411519064793,
3.77025506105769));
#251609=CARTESIAN_POINT('Ctrl Pts',(36.3139437822108,-50.3059538820299,
3.64284210641761));
#251610=CARTESIAN_POINT('Ctrl Pts',(36.3578055460617,-50.5831252836568,
3.65553527987796));
#251611=CARTESIAN_POINT('Ctrl Pts',(36.4612367259639,-50.508360519064,3.65585996533066));
#251612=CARTESIAN_POINT('Ctrl Pts',(36.4110374247146,-50.4395918165622,
3.5512790271021));
#251613=CARTESIAN_POINT('Ctrl Pts',(36.4252947698684,-50.6762142289942,
3.47153072139036));
#251614=CARTESIAN_POINT('Ctrl Pts',(36.5289136700286,-50.6015093986309,
3.47182327905153));
#251615=CARTESIAN_POINT('Ctrl Pts',(36.4650842569437,-50.5139808995216,
3.40413028377944));
#251616=CARTESIAN_POINT('Origin',(36.1092077731534,-50.2402240048077,3.64303198860229));
#251617=CARTESIAN_POINT('Origin',(5.69915478234096E-15,1.86277272141617E-13,
2.53178198860262));
#251618=CARTESIAN_POINT('Origin',(34.6837837831351,-47.7640607692757,2.53178198860229));
#251619=CARTESIAN_POINT('Origin',(21.2404668433939,-29.7751578089174,3.64303198860242));
#251620=CARTESIAN_POINT('Origin',(35.8732562382986,-49.9155525184321,3.64299466007537));
#251621=CARTESIAN_POINT('Ctrl Pts',(34.620500570364,-47.6769115920298,2.59908173515991));
#251622=CARTESIAN_POINT('Ctrl Pts',(34.642420023458,-47.7070975168458,2.6587819886023));
#251623=CARTESIAN_POINT('Ctrl Pts',(34.6837837831352,-47.7640607692757,
2.65878198860229));
#251624=CARTESIAN_POINT('Ctrl Pts',(34.5495693076631,-47.7284183483594,
2.59908193199727));
#251625=CARTESIAN_POINT('Ctrl Pts',(34.590741855859,-47.74461955945,2.65877685806571));
#251626=CARTESIAN_POINT('Ctrl Pts',(34.6425747206412,-47.7939730310143,
2.65878198860229));
#251627=CARTESIAN_POINT('Ctrl Pts',(34.4983910654773,-47.795926104355,2.63872492669799));
#251628=CARTESIAN_POINT('Ctrl Pts',(34.5563698228284,-47.7976714756521,
2.69532212015248));
#251629=CARTESIAN_POINT('Ctrl Pts',(34.6188891978605,-47.8415056181566,
2.68176836726613));
#251630=CARTESIAN_POINT('Ctrl Pts',(34.4545839152295,-47.9165880269722,
2.7544217640218));
#251631=CARTESIAN_POINT('Ctrl Pts',(34.5404685123898,-47.8837591046478,
2.79203179920099));
#251632=CARTESIAN_POINT('Ctrl Pts',(34.611146338977,-47.9359643384876,2.74885310748129));
#251633=CARTESIAN_POINT('Ctrl Pts',(34.4602354682506,-47.9696250311911,
2.82866089558392));
#251634=CARTESIAN_POINT('Ctrl Pts',(34.5595777906771,-47.9171136764618,
2.85316563119149));
#251635=CARTESIAN_POINT('Ctrl Pts',(34.6258166968309,-47.9824460410477,
2.79189751796571));
#251636=CARTESIAN_POINT('Ctrl Pts',(34.4869303039402,-48.0063682005181,
2.90134173515989));
#251637=CARTESIAN_POINT('Ctrl Pts',(34.5894948283139,-47.9324532779032,
2.90103711553195));
#251638=CARTESIAN_POINT('Ctrl Pts',(34.6525130919802,-48.0191904766731,
2.83404198860228));
#251639=CARTESIAN_POINT('Origin',(34.5497679336946,-48.0938392037142,2.83404198860228));
#251640=CARTESIAN_POINT('Origin',(35.8473027479624,-49.8797426632419,3.56647653971822));
#251641=CARTESIAN_POINT('Origin',(35.7991993820668,-49.8135340601217,3.42473028058451));
#251642=CARTESIAN_POINT('Origin',(34.6544814981831,-48.2379650606531,3.1191364816809));
#251643=CARTESIAN_POINT('Origin',(34.759195062554,-48.3820909175324,3.40423097483277));
#251644=CARTESIAN_POINT('Ctrl Pts',(35.6052536882608,-49.5465907136139,
3.36123028058447));
#251645=CARTESIAN_POINT('Ctrl Pts',(35.7079988465464,-49.4719419865727,
3.36123028058447));
#251646=CARTESIAN_POINT('Ctrl Pts',(35.7079988465464,-49.4719419865727,
3.23423028058447));
#251647=CARTESIAN_POINT('Ctrl Pts',(35.6583499840581,-49.6192730640951,
3.36123028058448));
#251648=CARTESIAN_POINT('Ctrl Pts',(35.7608559931245,-49.5446936074928,
3.36099641108458));
#251649=CARTESIAN_POINT('Ctrl Pts',(35.7873581223586,-49.5811706590224,
3.23423043688335));
#251650=CARTESIAN_POINT('Ctrl Pts',(35.7085550527735,-49.688000774918,3.41054258905246));
#251651=CARTESIAN_POINT('Ctrl Pts',(35.8110857017877,-49.6138288703623,
3.41008815826126));
#251652=CARTESIAN_POINT('Ctrl Pts',(35.86239796335,-49.684454139478,3.30819867304337));
#251653=CARTESIAN_POINT('Ctrl Pts',(35.7350130971395,-49.7242207306169,
3.4882302805845));
#251654=CARTESIAN_POINT('Ctrl Pts',(35.8375861910562,-49.6503036646779,
3.48794691941566));
#251655=CARTESIAN_POINT('Ctrl Pts',(35.9019445403524,-49.7388853330806,
3.42473028058451));
#251656=CARTESIAN_POINT('Origin',(35.6052536882608,-49.5465907136139,3.23423028058447));
#251657=CARTESIAN_POINT('Ctrl Pts',(34.6963546279291,-48.2946219293741,
3.4715307213904));
#251658=CARTESIAN_POINT('Ctrl Pts',(34.7990735298992,-48.220592152613,3.47122746285045));
#251659=CARTESIAN_POINT('Ctrl Pts',(34.8620346481364,-48.3075723994623,
3.40413046676756));
#251660=CARTESIAN_POINT('Ctrl Pts',(34.7638392294046,-48.3877165307476,
3.65553813457952));
#251661=CARTESIAN_POINT('Ctrl Pts',(34.866561796066,-48.3134813154519,3.6552033607186));
#251662=CARTESIAN_POINT('Ctrl Pts',(34.9160824571381,-48.3819628268483,
3.55128134519815));
#251663=CARTESIAN_POINT('Ctrl Pts',(34.8850734745852,-48.5549570506147,
3.77003198860229));
#251664=CARTESIAN_POINT('Ctrl Pts',(34.9878985031443,-48.4804861171417,
3.7698020931439));
#251665=CARTESIAN_POINT('Ctrl Pts',(35.0131769156747,-48.5156018845769,
3.64284195387484));
#251666=CARTESIAN_POINT('Ctrl Pts',(35.012421476459,-48.7306271754171,3.77003198860229));
#251667=CARTESIAN_POINT('Ctrl Pts',(35.1153205397472,-48.6558666298463,
3.77003198860229));
#251668=CARTESIAN_POINT('Ctrl Pts',(35.1151665196478,-48.6559785319987,
3.6428418940377));
#251669=CARTESIAN_POINT('Origin',(35.012421476459,-48.7306271754171,3.64303198860229));
#251670=CARTESIAN_POINT('Origin',(20.7197400704249,-29.0584388930976,3.23423028058461));
#251671=CARTESIAN_POINT('Origin',(35.5163757878401,-49.4242607783455,3.23423028058447));
#251672=CARTESIAN_POINT('Origin',(20.6381965522797,-28.9462038689909,3.64303198860242));
#251673=CARTESIAN_POINT('Origin',(35.2482948100404,-49.055365400752,3.64299171721771));
#251674=CARTESIAN_POINT('Ctrl Pts',(35.3866101428265,-49.2466351556007,
3.48823028058447));
#251675=CARTESIAN_POINT('Ctrl Pts',(35.4901170100372,-49.1720533660025,
3.48852004212225));
#251676=CARTESIAN_POINT('Ctrl Pts',(35.4251752107443,-49.0826686475729,
3.42473028058447));
#251677=CARTESIAN_POINT('Ctrl Pts',(35.4131599099223,-49.2829758776394,
3.41028005848372));
#251678=CARTESIAN_POINT('Ctrl Pts',(35.5164304941053,-49.2082707697372,
3.41074404220328));
#251679=CARTESIAN_POINT('Ctrl Pts',(35.4648554356498,-49.137283791733,3.30780486243949));
#251680=CARTESIAN_POINT('Ctrl Pts',(35.4634578610136,-49.3518235761932,
3.36123028058447));
#251681=CARTESIAN_POINT('Ctrl Pts',(35.5663414789302,-49.2769673468818,
3.36146460586282));
#251682=CARTESIAN_POINT('Ctrl Pts',(35.5400289748697,-49.2407512920131,
3.23423045308296));
#251683=CARTESIAN_POINT('Ctrl Pts',(35.5163757878401,-49.4242607783455,
3.36123028058448));
#251684=CARTESIAN_POINT('Ctrl Pts',(35.6191209461258,-49.3496120513043,
3.36123028058447));
#251685=CARTESIAN_POINT('Ctrl Pts',(35.6191209461258,-49.3496120513043,
3.23423028058448));
#251686=CARTESIAN_POINT('Origin',(35.3224300524587,-49.157317374614,3.42473028058447));
#251687=CARTESIAN_POINT('Origin',(35.2746135650482,-49.0915036263505,3.56563113524804));
#251688=CARTESIAN_POINT('Origin',(41.3366772861966,-45.4345348113606,3.56647653909422));
#251689=CARTESIAN_POINT('Origin',(41.3663085755626,-45.4673664422105,3.64299466007593));
#251690=CARTESIAN_POINT('Origin',(41.2819167515334,-45.3737170758066,3.42473028058452));
#251691=CARTESIAN_POINT('Ctrl Pts',(41.2079002115913,-45.292364129855,3.48823028058452));
#251692=CARTESIAN_POINT('Ctrl Pts',(41.1142722655012,-45.3773275334099,
3.48794691941568));
#251693=CARTESIAN_POINT('Ctrl Pts',(41.1875373586978,-45.4586966628142,
3.42473028058454));
#251694=CARTESIAN_POINT('Ctrl Pts',(41.1778715515046,-45.2588408013008,
3.41028005925054));
#251695=CARTESIAN_POINT('Ctrl Pts',(41.0840023845213,-45.3437094247702,
3.40982512231053));
#251696=CARTESIAN_POINT('Ctrl Pts',(41.1423656859475,-45.408528437742,3.30780486372896));
#251697=CARTESIAN_POINT('Ctrl Pts',(41.1209827764392,-45.1953306044433,
3.36123028058451));
#251698=CARTESIAN_POINT('Ctrl Pts',(41.0267203359238,-45.2800912647208,
3.36099721048405));
#251699=CARTESIAN_POINT('Ctrl Pts',(41.0567886774861,-45.3134855411631,
3.23423045308344));
#251700=CARTESIAN_POINT('Ctrl Pts',(41.0611303347409,-45.1285089182126,
3.3612302805845));
#251701=CARTESIAN_POINT('Ctrl Pts',(40.9667509419053,-45.2134885052202,
3.3612302805845));
#251702=CARTESIAN_POINT('Ctrl Pts',(40.9667509419053,-45.2134885052202,
3.2342302805845));
#251703=CARTESIAN_POINT('Origin',(41.0611303347409,-45.1285089182126,3.2342302805845));
#251704=CARTESIAN_POINT('Origin',(0.235948482089076,0.212448967519124,3.64303198860263));
#251705=CARTESIAN_POINT('Origin',(41.6348281284267,-45.7656648676099,3.64303198860231));
#251706=CARTESIAN_POINT('Origin',(0.235948482089076,0.212448967519127,3.23423028058482));
#251707=CARTESIAN_POINT('Origin',(40.959952356613,-45.0161393894786,3.2342302805845));
#251708=CARTESIAN_POINT('Ctrl Pts',(41.9955727382256,-46.1654920697605,
3.4715307213904));
#251709=CARTESIAN_POINT('Ctrl Pts',(41.900956815079,-46.2513146333396,3.47182327902631));
#251710=CARTESIAN_POINT('Ctrl Pts',(41.8286119029185,-46.1706818621616,
3.40413028959028));
#251711=CARTESIAN_POINT('Ctrl Pts',(41.9185486398946,-46.0801220723601,
3.65553807120925));
#251712=CARTESIAN_POINT('Ctrl Pts',(41.82391312212,-46.1657485548994,3.65586275496646));
#251713=CARTESIAN_POINT('Ctrl Pts',(41.7670844335132,-46.1023486848279,
3.55128126837224));
#251714=CARTESIAN_POINT('Ctrl Pts',(41.7801771152784,-45.9267584721662,
3.77003198860231));
#251715=CARTESIAN_POINT('Ctrl Pts',(41.6856154235002,-46.0121526898581,
3.77025505748641));
#251716=CARTESIAN_POINT('Ctrl Pts',(41.6565528363087,-45.9795909100377,
3.64284211731136));
#251717=CARTESIAN_POINT('Ctrl Pts',(41.6348281284267,-45.76566486761,3.77003198860232));
#251718=CARTESIAN_POINT('Ctrl Pts',(41.5403077371551,-45.8507714101796,
3.77003198860231));
#251719=CARTESIAN_POINT('Ctrl Pts',(41.5404488407565,-45.8506443599262,
3.64284239821728));
#251720=CARTESIAN_POINT('Origin',(41.9230990057961,-46.0858221116771,3.40423097483278));
#251721=CARTESIAN_POINT('Ctrl Pts',(40.959952356613,-45.0161393894786,3.3612302805845));
#251722=CARTESIAN_POINT('Ctrl Pts',(40.8655729637774,-45.1011189764862,
3.3612302805845));
#251723=CARTESIAN_POINT('Ctrl Pts',(40.8655729637774,-45.1011189764862,
3.2342302805845));
#251724=CARTESIAN_POINT('Ctrl Pts',(40.8998980546775,-44.9490914662989,
3.3612302805845));
#251725=CARTESIAN_POINT('Ctrl Pts',(40.8052862548063,-45.0341638030259,
3.36146538610179));
#251726=CARTESIAN_POINT('Ctrl Pts',(40.7752309130136,-45.0007839642926,
3.23423043688384));
#251727=CARTESIAN_POINT('Ctrl Pts',(40.8431135311204,-44.8856913339431,
3.41054258693068));
#251728=CARTESIAN_POINT('Ctrl Pts',(40.7485699563807,-44.9711739721972,
3.41100608859567));
#251729=CARTESIAN_POINT('Ctrl Pts',(40.6898060629479,-44.9059100567322,
3.30819866970758));
#251730=CARTESIAN_POINT('Ctrl Pts',(40.8131880745612,-44.8522789915935,
3.48823028058449));
#251731=CARTESIAN_POINT('Ctrl Pts',(40.7187157882343,-44.9380175594356,
3.48852004212228));
#251732=CARTESIAN_POINT('Ctrl Pts',(40.6447864996558,-44.8559107663279,
3.42473028058449));
#251733=CARTESIAN_POINT('Origin',(40.7391658924914,-44.7709311793203,3.4247302805845));
#251734=CARTESIAN_POINT('Origin',(42.0423040287741,-46.2182127020635,3.11913648178416));
#251735=CARTESIAN_POINT('Origin',(42.1615090516458,-46.3506032922587,2.8340419886023));
#251736=CARTESIAN_POINT('Origin',(40.6847319383109,-44.7104761485832,3.56563113460798));
#251737=CARTESIAN_POINT('Origin',(40.6548553974687,-44.6772189625509,3.64299171721763));
#251738=CARTESIAN_POINT('Ctrl Pts',(42.1358900227701,-46.773831928425,2.59908173515991));
#251739=CARTESIAN_POINT('Ctrl Pts',(42.1109214781067,-46.7461150696865,
2.6587819886023));
#251740=CARTESIAN_POINT('Ctrl Pts',(42.0638038389706,-46.6938111422597,
2.6587819886023));
#251741=CARTESIAN_POINT('Ctrl Pts',(42.2013581359414,-46.7148552537627,
2.59908193475685));
#251742=CARTESIAN_POINT('Ctrl Pts',(42.1586072771697,-46.7031532960215,
2.65878715325369));
#251743=CARTESIAN_POINT('Ctrl Pts',(42.1016932886505,-46.6596664560516,
2.6587819886023));
#251744=CARTESIAN_POINT('Ctrl Pts',(42.2450249725429,-46.6418481388113,
2.63878778849814));
#251745=CARTESIAN_POINT('Ctrl Pts',(42.1870455286633,-46.6464039985657,
2.69564460180075));
#251746=CARTESIAN_POINT('Ctrl Pts',(42.1199142759252,-46.609571404849,2.68180481624819));
#251747=CARTESIAN_POINT('Ctrl Pts',(42.2756632139855,-46.5164783566515,
2.7544323887864));
#251748=CARTESIAN_POINT('Ctrl Pts',(42.1934768724835,-46.5588531737041,
2.79268340777068));
#251749=CARTESIAN_POINT('Ctrl Pts',(42.1171707421508,-46.5142596423488,
2.74885926835611));
#251750=CARTESIAN_POINT('Ctrl Pts',(42.2644092166197,-46.4640705998039,
2.82856655361619));
#251751=CARTESIAN_POINT('Ctrl Pts',(42.1708301402948,-46.5278411618555,
2.85384197230716));
#251752=CARTESIAN_POINT('Ctrl Pts',(42.097557576812,-46.4693765057994,2.79184624278455));
#251753=CARTESIAN_POINT('Ctrl Pts',(42.2339804752707,-46.4302753505418,
2.90134173515992));
#251754=CARTESIAN_POINT('Ctrl Pts',(42.1395065321005,-46.5159655405268,
2.9016321871636));
#251755=CARTESIAN_POINT('Ctrl Pts',(42.0671296588101,-46.4355828792663,
2.8340419886023));
#251756=CARTESIAN_POINT('Origin',(42.0638038389706,-46.6938111422597,2.53178198860229));
#251757=CARTESIAN_POINT('Origin',(0.235948482089076,0.212448967519124,3.64303198860263));
#251758=CARTESIAN_POINT('Origin',(40.3862543050944,-44.3789831537289,3.64303198860232));
#251759=CARTESIAN_POINT('Origin',(5.55434424446678E-15,1.86005087008946E-13,
2.53178198860262));
#251760=CARTESIAN_POINT('Origin',(42.0411527846901,-46.7142062431416,2.5317819886023));
#251761=CARTESIAN_POINT('Ctrl Pts',(40.3862543050944,-44.3789831537289,
3.77003198860233));
#251762=CARTESIAN_POINT('Ctrl Pts',(40.2917335276661,-44.4640900439955,
3.77003198860233));
#251763=CARTESIAN_POINT('Ctrl Pts',(40.2918750180005,-44.4639626455262,
3.64284187936968));
#251764=CARTESIAN_POINT('Ctrl Pts',(40.2408978759506,-44.2178916378556,
3.77003198860233));
#251765=CARTESIAN_POINT('Ctrl Pts',(40.1466757825319,-44.3029863283953,
3.76980208962652));
#251766=CARTESIAN_POINT('Ctrl Pts',(40.1757689690827,-44.335013814935,3.64284193928157));
#251767=CARTESIAN_POINT('Ctrl Pts',(40.1025190720993,-44.0645366033533,
3.65553535416555));
#251768=CARTESIAN_POINT('Ctrl Pts',(40.0085488431155,-44.1495800756913,
3.65520057834686));
#251769=CARTESIAN_POINT('Ctrl Pts',(40.0652381943489,-44.2122569536115,
3.55127910964328));
#251770=CARTESIAN_POINT('Ctrl Pts',(40.0254908126594,-43.9791725362576,
3.47153072139041));
#251771=CARTESIAN_POINT('Ctrl Pts',(39.9317222927446,-44.0642551375171,
3.47122746281551));
#251772=CARTESIAN_POINT('Ctrl Pts',(40.0037114790894,-44.1439246138544,
3.40413045901217));
#251773=CARTESIAN_POINT('Origin',(40.0979831325504,-44.0588255818371,3.4042309748328));
#251774=CARTESIAN_POINT('Ctrl Pts',(41.7612723673368,-46.8559036426978,
2.90134173515992));
#251775=CARTESIAN_POINT('Ctrl Pts',(41.8563683535936,-46.7709043015495,
2.90163218716359));
#251776=CARTESIAN_POINT('Ctrl Pts',(41.7839914803032,-46.690521640289,2.8340419886023));
#251777=CARTESIAN_POINT('Ctrl Pts',(41.7917156448195,-46.88971359836,2.82853349835323));
#251778=CARTESIAN_POINT('Ctrl Pts',(41.8649095672158,-46.8033160448216,
2.85381483162249));
#251779=CARTESIAN_POINT('Ctrl Pts',(41.814433263085,-46.7243306652201,2.79182701594126));
#251780=CARTESIAN_POINT('Ctrl Pts',(41.8425440045886,-46.906245031096,2.75468822073613));
#251781=CARTESIAN_POINT('Ctrl Pts',(41.8933569085963,-46.8289264627099,
2.79286913083832));
#251782=CARTESIAN_POINT('Ctrl Pts',(41.8569022891478,-46.7483907976675,
2.74900763297862));
#251783=CARTESIAN_POINT('Ctrl Pts',(41.9695156381237,-46.8892773184513,
2.63954450640359));
#251784=CARTESIAN_POINT('Ctrl Pts',(41.9804178820376,-46.8319191778361,
2.6962768402881));
#251785=CARTESIAN_POINT('Ctrl Pts',(41.950787100749,-46.7612136652285,2.68224356036478));
#251786=CARTESIAN_POINT('Ctrl Pts',(42.0474864684055,-46.8534019544972,
2.59908178706358));
#251787=CARTESIAN_POINT('Ctrl Pts',(42.0403508033704,-46.8096319157664,
2.65878704321398));
#251788=CARTESIAN_POINT('Ctrl Pts',(42.0031091843002,-46.7484320121843,
2.6587819886023));
#251789=CARTESIAN_POINT('Ctrl Pts',(42.1132001506006,-46.794261981091,2.59908173515991));
#251790=CARTESIAN_POINT('Ctrl Pts',(42.0882450513181,-46.7665330160772,
2.6587819886023));
#251791=CARTESIAN_POINT('Ctrl Pts',(42.0411527846901,-46.7142062431416,
2.6587819886023));
#251792=CARTESIAN_POINT('Origin',(41.6896120874676,-46.7755012272966,2.8340419886023));
#251793=CARTESIAN_POINT('Origin',(39.9787779456782,-43.9264348094998,3.11913648166838));
#251794=CARTESIAN_POINT('Origin',(39.859572758736,-43.7940440370138,2.83404198860232));
#251795=CARTESIAN_POINT('Origin',(41.5704070646248,-46.6431106370586,3.11913648177637));
#251796=CARTESIAN_POINT('Origin',(41.451202041618,-46.510720046715,3.40423097483279));
#251797=CARTESIAN_POINT('Ctrl Pts',(39.7870778846752,-43.7143933160617,
2.90134173515993));
#251798=CARTESIAN_POINT('Ctrl Pts',(39.6934538167806,-43.7993487829606,
2.90103711553199));
#251799=CARTESIAN_POINT('Ctrl Pts',(39.7651933659004,-43.8790236240213,
2.83404198860232));
#251800=CARTESIAN_POINT('Ctrl Pts',(39.7566748466929,-43.6806281164514,
2.82862991747937));
#251801=CARTESIAN_POINT('Ctrl Pts',(39.6846648960488,-43.766879165672,2.85314045886381));
#251802=CARTESIAN_POINT('Ctrl Pts',(39.7347894633642,-43.845256669365,2.79187960999885));
#251803=CARTESIAN_POINT('Ctrl Pts',(39.7061132086036,-43.6642103943278,
2.75470625793291));
#251804=CARTESIAN_POINT('Ctrl Pts',(39.6560595510445,-43.7414086642724,
2.79224250381877));
#251805=CARTESIAN_POINT('Ctrl Pts',(39.6925108309095,-43.8213838166739,
2.74901809108231));
#251806=CARTESIAN_POINT('Ctrl Pts',(39.579862457588,-43.6815693876449,2.63947868311675));
#251807=CARTESIAN_POINT('Ctrl Pts',(39.5692094437569,-43.73881692348,2.69595066767879));
#251808=CARTESIAN_POINT('Ctrl Pts',(39.5991004926185,-43.8091742082544,
2.68220539436029));
#251809=CARTESIAN_POINT('Ctrl Pts',(39.5024012818823,-43.7176736830018,
2.59908178585043));
#251810=CARTESIAN_POINT('Ctrl Pts',(39.5096522555313,-43.7613473163391,
2.65877670944801));
#251811=CARTESIAN_POINT('Ctrl Pts',(39.5470931435013,-43.8223603708606,
2.65878198860232));
#251812=CARTESIAN_POINT('Ctrl Pts',(39.4370498736014,-43.7765468711716,
2.59908173515994));
#251813=CARTESIAN_POINT('Ctrl Pts',(39.4620188529815,-43.8042633382923,
2.65878198860232));
#251814=CARTESIAN_POINT('Ctrl Pts',(39.5091373124628,-43.856566526705,2.65878198860232));
#251815=CARTESIAN_POINT('Origin',(39.5091373124628,-43.856566526705,2.53178198860232));
#251816=CARTESIAN_POINT('Ctrl Pts',(41.1629311642486,-46.1905628026478,
3.77003198860232));
#251817=CARTESIAN_POINT('Ctrl Pts',(41.2574515636633,-46.1054562527462,
3.77003198860232));
#251818=CARTESIAN_POINT('Ctrl Pts',(41.2573104519068,-46.1055833103425,
3.64284238727614));
#251819=CARTESIAN_POINT('Ctrl Pts',(41.307951431325,-46.351956930601,3.77003198860231));
#251820=CARTESIAN_POINT('Ctrl Pts',(41.4027622547794,-46.2668393800552,
3.770255061059));
#251821=CARTESIAN_POINT('Ctrl Pts',(41.3734162510852,-46.2345318643249,
3.64284210641861));
#251822=CARTESIAN_POINT('Ctrl Pts',(41.4460100362753,-46.5056000892401,
3.65553527987802));
#251823=CARTESIAN_POINT('Ctrl Pts',(41.541059563395,-46.4204333915652,3.65585996532922));
#251824=CARTESIAN_POINT('Ctrl Pts',(41.4839469723832,-46.3572886670207,
3.55127902710143));
#251825=CARTESIAN_POINT('Ctrl Pts',(41.5228599914568,-46.5911245387423,
3.4715307213904));
#251826=CARTESIAN_POINT('Ctrl Pts',(41.6181024753231,-46.5059978248575,
3.47182327905157));
#251827=CARTESIAN_POINT('Ctrl Pts',(41.5454735069385,-46.4256208064855,
3.40413028377981));
#251828=CARTESIAN_POINT('Origin',(41.1629311642486,-46.1905628026478,3.64303198860232));
#251829=CARTESIAN_POINT('Origin',(5.70392627685665E-15,1.86281136021691E-13,
2.53178198860262));
#251830=CARTESIAN_POINT('Origin',(39.4864862581822,-43.8769616275868,2.53178198860232));
#251831=CARTESIAN_POINT('Origin',(27.6232705441551,-31.1532462714323,3.64303198860241));
#251832=CARTESIAN_POINT('Origin',(40.8943347850531,-45.8923335519892,3.64299466007435));
#251833=CARTESIAN_POINT('Ctrl Pts',(39.4144401478995,-43.796904759634,2.59908173515994));
#251834=CARTESIAN_POINT('Ctrl Pts',(39.4393948122693,-43.8246341160479,
2.65878198860232));
#251835=CARTESIAN_POINT('Ctrl Pts',(39.4864862581822,-43.8769616275868,
2.65878198860232));
#251836=CARTESIAN_POINT('Ctrl Pts',(39.3492813761644,-43.8555436924512,
2.5990819319977));
#251837=CARTESIAN_POINT('Ctrl Pts',(39.391921864532,-43.8673524484207,2.65877685806562));
#251838=CARTESIAN_POINT('Ctrl Pts',(39.4486296259959,-43.9110175468,2.65878198860232));
#251839=CARTESIAN_POINT('Ctrl Pts',(39.305439975737,-43.9280312169039,2.63872492669775));
#251840=CARTESIAN_POINT('Ctrl Pts',(39.3632835603683,-43.9237065964663,
2.69532212015237));
#251841=CARTESIAN_POINT('Ctrl Pts',(39.4300423632771,-43.9607655567551,
2.68176836726605));
#251842=CARTESIAN_POINT('Ctrl Pts',(39.274485410988,-44.0526112349799,2.75442176402213));
#251843=CARTESIAN_POINT('Ctrl Pts',(39.3564679665378,-44.0109847679675,
2.79203179920121));
#251844=CARTESIAN_POINT('Ctrl Pts',(39.4322155454634,-44.0555161714738,
2.74885310748144));
#251845=CARTESIAN_POINT('Ctrl Pts',(39.2856498807585,-44.1047669487868,
2.82866089558373));
#251846=CARTESIAN_POINT('Ctrl Pts',(39.3789590643336,-44.0421591564527,
2.85316563119135));
#251847=CARTESIAN_POINT('Ctrl Pts',(39.4516641985005,-44.1002097724414,
2.79189751796553));
#251848=CARTESIAN_POINT('Ctrl Pts',(39.3160391863695,-44.1385184650369,
2.90134173515994));
#251849=CARTESIAN_POINT('Ctrl Pts',(39.4103156382737,-44.0542875439834,
2.901037115532));
#251850=CARTESIAN_POINT('Ctrl Pts',(39.4820551873935,-44.1339623850441,
2.83404198860232));
#251851=CARTESIAN_POINT('Origin',(39.3876757945579,-44.2189419720517,2.83404198860232));
#251852=CARTESIAN_POINT('Origin',(40.8647803215176,-45.8594327453962,3.56647653971777));
#251853=CARTESIAN_POINT('Origin',(40.8100197873553,-45.7986150108445,3.42473028058453));
#251854=CARTESIAN_POINT('Origin',(39.5068809815269,-44.3513327444847,3.11913648168179));
#251855=CARTESIAN_POINT('Origin',(39.6260861683723,-44.483723516875,3.40423097483281));
#251856=CARTESIAN_POINT('Ctrl Pts',(40.5892333705628,-45.5534068532505,
3.3612302805845));
#251857=CARTESIAN_POINT('Ctrl Pts',(40.6836127633984,-45.4684272662429,
3.3612302805845));
#251858=CARTESIAN_POINT('Ctrl Pts',(40.6836127633984,-45.4684272662429,
3.2342302805845));
#251859=CARTESIAN_POINT('Ctrl Pts',(40.6496361736987,-45.620140968006,3.3612302805845));
#251860=CARTESIAN_POINT('Ctrl Pts',(40.7437849681316,-45.5352552698632,
3.36099641108314));
#251861=CARTESIAN_POINT('Ctrl Pts',(40.7739548060703,-45.5687622694495,
3.23423043688344));
#251862=CARTESIAN_POINT('Ctrl Pts',(40.7067502157884,-45.683244322559,3.41054258905254));
#251863=CARTESIAN_POINT('Ctrl Pts',(40.8009661159811,-45.5987613682809,
3.41008815826137));
#251864=CARTESIAN_POINT('Ctrl Pts',(40.8593796344539,-45.6636361529295,
3.30819867304344));
#251865=CARTESIAN_POINT('Ctrl Pts',(40.7368493365303,-45.71650024283,3.48823028058452));
#251866=CARTESIAN_POINT('Ctrl Pts',(40.8311340869943,-45.6322662944326,
3.48794691941568));
#251867=CARTESIAN_POINT('Ctrl Pts',(40.9043991801909,-45.7136354238369,
3.42473028058453));
#251868=CARTESIAN_POINT('Origin',(40.5892333705628,-45.5534068532505,3.2342302805845));
#251869=CARTESIAN_POINT('Ctrl Pts',(39.5544469813076,-44.4033023070483,
3.47153072139043));
#251870=CARTESIAN_POINT('Ctrl Pts',(39.648864959584,-44.3189410241789,3.47122746285048));
#251871=CARTESIAN_POINT('Ctrl Pts',(39.7205730817656,-44.3988635551997,
3.40413046676773));
#251872=CARTESIAN_POINT('Ctrl Pts',(39.6312929306927,-44.4888328647708,
3.65553813457958));
#251873=CARTESIAN_POINT('Ctrl Pts',(39.7256930794106,-44.404266885713,3.65520336072251));
#251874=CARTESIAN_POINT('Ctrl Pts',(39.7821007282716,-44.4671969296237,
3.55128134519942));
#251875=CARTESIAN_POINT('Ctrl Pts',(39.7693444365344,-44.6424847942241,
3.77003198860233));
#251876=CARTESIAN_POINT('Ctrl Pts',(39.8638218465944,-44.5576736780981,
3.7698020931396));
#251877=CARTESIAN_POINT('Ctrl Pts',(39.8926323785411,-44.5899547640674,
3.64284195387346));
#251878=CARTESIAN_POINT('Ctrl Pts',(39.9143573409162,-44.8038810887668,
3.77003198860233));
#251879=CARTESIAN_POINT('Ctrl Pts',(40.0088781074275,-44.7187742083299,
3.77003198860233));
#251880=CARTESIAN_POINT('Ctrl Pts',(40.0087366280265,-44.7189015969548,
3.64284189403801));
#251881=CARTESIAN_POINT('Origin',(39.9143573409162,-44.8038810887668,3.64303198860232));
#251882=CARTESIAN_POINT('Origin',(26.948440628206,-30.4037717213981,3.2342302805846));
#251883=CARTESIAN_POINT('Origin',(40.4880553924349,-45.4410373245165,3.2342302805845));
#251884=CARTESIAN_POINT('Origin',(26.8427652369017,-30.2864073093061,3.64303198860241));
#251885=CARTESIAN_POINT('Origin',(40.1828829233546,-45.1021848870404,3.64299171721753));
#251886=CARTESIAN_POINT('Ctrl Pts',(40.3404336838198,-45.2779489569766,
3.4882302805845));
#251887=CARTESIAN_POINT('Ctrl Pts',(40.4355776097274,-45.1929563204583,
3.48852004212227));
#251888=CARTESIAN_POINT('Ctrl Pts',(40.3616483211489,-45.1108495273506,
3.42473028058449));
#251889=CARTESIAN_POINT('Ctrl Pts',(40.3706366483421,-45.311315394383,3.41028005848376));
#251890=CARTESIAN_POINT('Ctrl Pts',(40.4655326953337,-45.2262248134145,
3.410744042204));
#251891=CARTESIAN_POINT('Ctrl Pts',(40.4068200107205,-45.1610177711048,
3.30780486243926));
#251892=CARTESIAN_POINT('Ctrl Pts',(40.4278556061251,-45.3745283705064,
3.3612302805845));
#251893=CARTESIAN_POINT('Ctrl Pts',(40.5223510102001,-45.2893279449748,
3.36146460586259));
#251894=CARTESIAN_POINT('Ctrl Pts',(40.4923970402299,-45.2560606910598,
3.23423045308319));
#251895=CARTESIAN_POINT('Ctrl Pts',(40.4880553924349,-45.4410373245165,
3.3612302805845));
#251896=CARTESIAN_POINT('Ctrl Pts',(40.5824347852705,-45.3560577375089,
3.3612302805845));
#251897=CARTESIAN_POINT('Ctrl Pts',(40.5824347852705,-45.3560577375089,
3.23423028058451));
#251898=CARTESIAN_POINT('Origin',(40.2672689283133,-45.1958291143582,3.4247302805845));
#251899=CARTESIAN_POINT('Origin',(40.2128349746532,-45.1353740846434,3.56563113524767));
#251900=CARTESIAN_POINT('Origin',(45.8594327460075,-40.8647803224525,3.56647653909432));
#251901=CARTESIAN_POINT('Origin',(45.8923335519901,-40.8943347850511,3.64299466007529));
#251902=CARTESIAN_POINT('Origin',(45.7986150108456,-40.810019787354,3.42473028058456));
#251903=CARTESIAN_POINT('Ctrl Pts',(45.7165002428312,-40.736849336529,3.48823028058456));
#251904=CARTESIAN_POINT('Ctrl Pts',(45.6322662944337,-40.831134086993,3.48794691941572));
#251905=CARTESIAN_POINT('Ctrl Pts',(45.7136354238381,-40.9043991801896,
3.42473028058457));
#251906=CARTESIAN_POINT('Ctrl Pts',(45.6831319408685,-40.7066485019696,
3.41028005925058));
#251907=CARTESIAN_POINT('Ctrl Pts',(45.5986481857988,-40.8008642060155,
3.4098251223095));
#251908=CARTESIAN_POINT('Ctrl Pts',(45.6634671987668,-40.8592275074402,
3.30780486372854));
#251909=CARTESIAN_POINT('Ctrl Pts',(45.6199161851861,-40.6494327168502,
3.36123028058454));
#251910=CARTESIAN_POINT('Ctrl Pts',(45.535030025744,-40.7435821574108,3.36099721048374));
#251911=CARTESIAN_POINT('Ctrl Pts',(45.5684243021863,-40.7736504989773,
3.23423045308361));
#251912=CARTESIAN_POINT('Ctrl Pts',(45.5534068532516,-40.5892333705615,
3.36123028058454));
#251913=CARTESIAN_POINT('Ctrl Pts',(45.468427266244,-40.6836127633972,3.36123028058454));
#251914=CARTESIAN_POINT('Ctrl Pts',(45.4684272662441,-40.6836127633972,
3.23423028058454));
#251915=CARTESIAN_POINT('Origin',(45.5534068532516,-40.5892333705615,3.23423028058454));
#251916=CARTESIAN_POINT('Origin',(0.21244896751894,0.235948482089259,3.64303198860263));
#251917=CARTESIAN_POINT('Origin',(46.190562802649,-41.1629311642473,3.64303198860234));
#251918=CARTESIAN_POINT('Origin',(0.21244896751894,0.235948482089262,3.23423028058482));
#251919=CARTESIAN_POINT('Origin',(45.4410373245177,-40.4880553924336,3.23423028058454));
#251920=CARTESIAN_POINT('Ctrl Pts',(46.5911245387435,-41.5228599914555,
3.47153072139043));
#251921=CARTESIAN_POINT('Ctrl Pts',(46.5059978322082,-41.6181024670989,
3.47182327902633));
#251922=CARTESIAN_POINT('Ctrl Pts',(46.4256208133858,-41.5454735131712,
3.40413028959021));
#251923=CARTESIAN_POINT('Ctrl Pts',(46.5055987918451,-41.4460088704661,
3.65553807120927));
#251924=CARTESIAN_POINT('Ctrl Pts',(46.4204321019755,-41.5410583874223,
3.65586275497085));
#251925=CARTESIAN_POINT('Ctrl Pts',(46.3572876358795,-41.4839460439592,
3.55128126837205));
#251926=CARTESIAN_POINT('Ctrl Pts',(46.3519544194676,-41.3079491749508,
3.77003198860234));
#251927=CARTESIAN_POINT('Ctrl Pts',(46.2668368728761,-41.4027599825067,
3.77025505748214));
#251928=CARTESIAN_POINT('Ctrl Pts',(46.2345298607754,-41.3734144471008,
3.6428421173117));
#251929=CARTESIAN_POINT('Ctrl Pts',(46.190562802649,-41.1629311642473,3.77003198860235));
#251930=CARTESIAN_POINT('Ctrl Pts',(46.1054562600792,-41.2574515555191,
3.77003198860235));
#251931=CARTESIAN_POINT('Ctrl Pts',(46.1055833103327,-41.2573104519176,
3.64284239821712));
#251932=CARTESIAN_POINT('Origin',(46.5107200467162,-41.4512020416167,3.40423097483282));
#251933=CARTESIAN_POINT('Ctrl Pts',(45.4410373245177,-40.4880553924336,
3.36123028058454));
#251934=CARTESIAN_POINT('Ctrl Pts',(45.3560577375101,-40.5824347852693,
3.36123028058454));
#251935=CARTESIAN_POINT('Ctrl Pts',(45.3560577375101,-40.5824347852693,
3.23423028058454));
#251936=CARTESIAN_POINT('Ctrl Pts',(45.3743035899565,-40.4276521486862,
3.36123028058454));
#251937=CARTESIAN_POINT('Ctrl Pts',(45.289102564049,-40.5221480762958,3.36146538610066));
#251938=CARTESIAN_POINT('Ctrl Pts',(45.2557227253168,-40.4920927345057,
3.23423043688334));
#251939=CARTESIAN_POINT('Ctrl Pts',(45.3112030195546,-40.3705349278744,
3.4105425869307));
#251940=CARTESIAN_POINT('Ctrl Pts',(45.226112733224,-40.4654317778737,3.4110060885973));
#251941=CARTESIAN_POINT('Ctrl Pts',(45.1608488177557,-40.4066678844394,
3.30819866970787));
#251942=CARTESIAN_POINT('Ctrl Pts',(45.2779489569777,-40.3404336838185,
3.48823028058454));
#251943=CARTESIAN_POINT('Ctrl Pts',(45.1929563204594,-40.4355776097261,
3.48852004212231));
#251944=CARTESIAN_POINT('Ctrl Pts',(45.1108495273517,-40.3616483211477,
3.42473028058453));
#251945=CARTESIAN_POINT('Origin',(45.1958291143593,-40.267268928312,3.42473028058454));
#251946=CARTESIAN_POINT('Origin',(46.6431106370702,-41.5704070646301,3.11913648178396));
#251947=CARTESIAN_POINT('Origin',(46.7755012272978,-41.6896120874663,2.83404198860233));
#251948=CARTESIAN_POINT('Origin',(45.1353740836147,-40.2128349741379,3.56563113460728));
#251949=CARTESIAN_POINT('Origin',(45.1021848870414,-40.1828829233538,3.64299171721789));
#251950=CARTESIAN_POINT('Ctrl Pts',(46.7942619810922,-42.1132001505994,
2.59908173515994));
#251951=CARTESIAN_POINT('Ctrl Pts',(46.7665330160784,-42.0882450513168,
2.65878198860233));
#251952=CARTESIAN_POINT('Ctrl Pts',(46.7142062431428,-42.0411527846888,
2.65878198860233));
#251953=CARTESIAN_POINT('Ctrl Pts',(46.8532067119187,-42.0477032750696,
2.59908193475573));
#251954=CARTESIAN_POINT('Ctrl Pts',(46.8094668591649,-42.0405341034483,
2.65878715325369));
#251955=CARTESIAN_POINT('Ctrl Pts',(46.7483190388757,-42.0032346206964,
2.65878198860233));
#251956=CARTESIAN_POINT('Ctrl Pts',(46.8890030154869,-41.9705316734057,
2.63878778849843));
#251957=CARTESIAN_POINT('Ctrl Pts',(46.8318174060861,-41.9811230778535,
2.69564460180073));
#251958=CARTESIAN_POINT('Ctrl Pts',(46.7612038509551,-41.9515093836251,
2.6818048162486));
#251959=CARTESIAN_POINT('Ctrl Pts',(46.9063687067671,-41.8426461117362,
2.75443238878615));
#251960=CARTESIAN_POINT('Ctrl Pts',(46.8290619651513,-41.8933796070859,
2.79268340777078));
#251961=CARTESIAN_POINT('Ctrl Pts',(46.7485125544804,-41.8570065263028,
2.74885926835575));
#251962=CARTESIAN_POINT('Ctrl Pts',(46.8896982576905,-41.7917018131132,
2.82856655361643));
#251963=CARTESIAN_POINT('Ctrl Pts',(46.8032976561896,-41.8649047103977,
2.85384197230743));
#251964=CARTESIAN_POINT('Ctrl Pts',(46.7243152668226,-41.8144193983031,
2.7918462427841));
#251965=CARTESIAN_POINT('Ctrl Pts',(46.855903642699,-41.7612723673355,2.90134173515995));
#251966=CARTESIAN_POINT('Ctrl Pts',(46.7709043015507,-41.8563683535923,
2.90163218716363));
#251967=CARTESIAN_POINT('Ctrl Pts',(46.6905216402902,-41.7839914803019,
2.83404198860233));
#251968=CARTESIAN_POINT('Origin',(46.7142062431428,-42.0411527846888,2.53178198860233));
#251969=CARTESIAN_POINT('Origin',(0.21244896751894,0.235948482089259,3.64303198860263));
#251970=CARTESIAN_POINT('Origin',(44.8038810887679,-39.914357340915,3.64303198860235));
#251971=CARTESIAN_POINT('Origin',(5.54214007001405E-15,1.85992882834493E-13,
2.53178198860262));
#251972=CARTESIAN_POINT('Origin',(46.6938111422609,-42.0638038389693,2.53178198860233));
#251973=CARTESIAN_POINT('Ctrl Pts',(44.8038810887679,-39.914357340915,3.77003198860236));
#251974=CARTESIAN_POINT('Ctrl Pts',(44.7187741985015,-40.0088781183431,
3.77003198860237));
#251975=CARTESIAN_POINT('Ctrl Pts',(44.7189015969706,-40.0087366280089,
3.64284187936997));
#251976=CARTESIAN_POINT('Ctrl Pts',(44.6424822887504,-39.7693421853875,
3.77003198860237));
#251977=CARTESIAN_POINT('Ctrl Pts',(44.5576711710536,-39.8638196089392,
3.76980208962785));
#251978=CARTESIAN_POINT('Ctrl Pts',(44.5899527660337,-39.8926305794717,
3.64284193928197));
#251979=CARTESIAN_POINT('Ctrl Pts',(44.4888315723767,-39.6312917695228,
3.65553535416558));
#251980=CARTESIAN_POINT('Ctrl Pts',(44.4042655856122,-39.7256919284505,
3.65520057834616));
#251981=CARTESIAN_POINT('Ctrl Pts',(44.4671959043829,-39.7820998051089,
3.55127910964262));
#251982=CARTESIAN_POINT('Ctrl Pts',(44.4033023070494,-39.5544469813064,
3.47153072139045));
#251983=CARTESIAN_POINT('Ctrl Pts',(44.3189410144585,-39.6488649704632,
3.47122746281555));
#251984=CARTESIAN_POINT('Ctrl Pts',(44.3988635644387,-39.7205730900528,
3.40413045901234));
#251985=CARTESIAN_POINT('Origin',(44.4837235168761,-39.6260861683711,3.40423097483283));
#251986=CARTESIAN_POINT('Ctrl Pts',(46.430275350543,-42.2339804752694,2.90134173515995));
#251987=CARTESIAN_POINT('Ctrl Pts',(46.515965540528,-42.1395065320992,2.90163218716363));
#251988=CARTESIAN_POINT('Ctrl Pts',(46.4355828792675,-42.0671296588088,
2.83404198860233));
#251989=CARTESIAN_POINT('Ctrl Pts',(46.464085959275,-42.2644230274446,2.82853349835333));
#251990=CARTESIAN_POINT('Ctrl Pts',(46.5278479142045,-42.1708479205175,
2.85381483162383));
#251991=CARTESIAN_POINT('Ctrl Pts',(46.4693919041987,-42.0975714415906,
2.79182701594139));
#251992=CARTESIAN_POINT('Ctrl Pts',(46.5163638812304,-42.2755508889254,
2.75468822073606));
#251993=CARTESIAN_POINT('Ctrl Pts',(46.5588164356978,-42.193344484977,2.79286913083796));
#251994=CARTESIAN_POINT('Ctrl Pts',(46.5141432491637,-42.1170605480842,
2.74900763297871));
#251995=CARTESIAN_POINT('Ctrl Pts',(46.6408663419436,-42.245403977454,2.63954450640372));
#251996=CARTESIAN_POINT('Ctrl Pts',(46.6457133039304,-42.187220455932,2.69627684028839));
#251997=CARTESIAN_POINT('Ctrl Pts',(46.6088541045845,-42.119999535554,2.68224356036476));
#251998=CARTESIAN_POINT('Ctrl Pts',(46.714660043196,-42.2015749714284,2.59908178706311));
#251999=CARTESIAN_POINT('Ctrl Pts',(46.7029882531952,-42.1587905896503,
2.65878704321522));
#252000=CARTESIAN_POINT('Ctrl Pts',(46.6595535157378,-42.1018187547551,
2.65878198860233));
#252001=CARTESIAN_POINT('Ctrl Pts',(46.7738319284262,-42.1358900227688,
2.59908173515994));
#252002=CARTESIAN_POINT('Ctrl Pts',(46.7461150696877,-42.1109214781054,
2.65878198860233));
#252003=CARTESIAN_POINT('Ctrl Pts',(46.6938111422609,-42.0638038389693,
2.65878198860233));
#252004=CARTESIAN_POINT('Origin',(46.3506032922599,-42.1615090516445,2.83404198860233));
#252005=CARTESIAN_POINT('Origin',(44.3513327445038,-39.5068809815363,3.11913648166901));
#252006=CARTESIAN_POINT('Origin',(44.2189419720528,-39.3876757945567,2.83404198860235));
#252007=CARTESIAN_POINT('Origin',(46.2182127020562,-42.0423040287639,3.11913648177653));
#252008=CARTESIAN_POINT('Origin',(46.0858221116783,-41.9230990057948,3.4042309748328));
#252009=CARTESIAN_POINT('Ctrl Pts',(44.1385184650381,-39.3160391863683,
2.90134173515997));
#252010=CARTESIAN_POINT('Ctrl Pts',(44.0542875439845,-39.4103156382725,
2.90103711553202));
#252011=CARTESIAN_POINT('Ctrl Pts',(44.1339623850452,-39.4820551873923,
2.83404198860235));
#252012=CARTESIAN_POINT('Ctrl Pts',(44.1047525536511,-39.285636938894,2.82862991747939));
#252013=CARTESIAN_POINT('Ctrl Pts',(44.0421527706791,-39.3789425853225,
2.85314045886471));
#252014=CARTESIAN_POINT('Ctrl Pts',(44.1001954303881,-39.4516512848555,
2.79187960999985));
#252015=CARTESIAN_POINT('Ctrl Pts',(44.0527517782421,-39.2745942850993,
2.75470625793293));
#252016=CARTESIAN_POINT('Ctrl Pts',(44.0110417363805,-39.356601686749,2.79224250381871));
#252017=CARTESIAN_POINT('Ctrl Pts',(44.0556530121008,-39.4323285306294,
2.74901809108237));
#252018=CARTESIAN_POINT('Ctrl Pts',(43.9290071509461,-39.3050549810244,
2.63947868311676));
#252019=CARTESIAN_POINT('Ctrl Pts',(43.924396492386,-39.3631024520336,2.69595066767885));
#252020=CARTESIAN_POINT('Ctrl Pts',(43.9614781338114,-39.4299498468373,
2.68220539436029));
#252021=CARTESIAN_POINT('Ctrl Pts',(43.8557442421761,-39.3490583909331,
2.5990817858497));
#252022=CARTESIAN_POINT('Ctrl Pts',(43.8675206320095,-39.3917348424031,
2.65877670944714));
#252023=CARTESIAN_POINT('Ctrl Pts',(43.9111340157069,-39.4485000225459,
2.65878198860235));
#252024=CARTESIAN_POINT('Ctrl Pts',(43.7969047596351,-39.4144401478983,
2.59908173515997));
#252025=CARTESIAN_POINT('Ctrl Pts',(43.824634116049,-39.4393948122681,2.65878198860235));
#252026=CARTESIAN_POINT('Ctrl Pts',(43.8769616275879,-39.486486258181,2.65878198860235));
#252027=CARTESIAN_POINT('Origin',(43.8769616275879,-39.486486258181,2.53178198860235));
#252028=CARTESIAN_POINT('Ctrl Pts',(45.7656648676111,-41.6348281284255,
3.77003198860235));
#252029=CARTESIAN_POINT('Ctrl Pts',(45.8507714175131,-41.5403077290104,
3.77003198860235));
#252030=CARTESIAN_POINT('Ctrl Pts',(45.8506443599165,-41.5404488407673,
3.64284238727559));
#252031=CARTESIAN_POINT('Ctrl Pts',(45.9267609786678,-41.7801793767969,
3.77003198860235));
#252032=CARTESIAN_POINT('Ctrl Pts',(46.0121552117538,-41.6856176794247,
3.77025506105598));
#252033=CARTESIAN_POINT('Ctrl Pts',(45.9795929135651,-41.6565546403126,
3.6428421064184));
#252034=CARTESIAN_POINT('Ctrl Pts',(46.0801233673988,-41.9185498083207,
3.65553527987807));
#252035=CARTESIAN_POINT('Ctrl Pts',(46.1657498592337,-41.823914281722,3.65585996533128));
#252036=CARTESIAN_POINT('Ctrl Pts',(46.1023497159522,-41.7670853619614,
3.55127902710157));
#252037=CARTESIAN_POINT('Ctrl Pts',(46.1654920697617,-41.9955727382244,
3.47153072139041));
#252038=CARTESIAN_POINT('Ctrl Pts',(46.2513146407509,-41.9009568069084,
3.47182327905159));
#252039=CARTESIAN_POINT('Ctrl Pts',(46.1706818552412,-41.8286118967071,
3.40413028377952));
#252040=CARTESIAN_POINT('Origin',(45.7656648676111,-41.6348281284255,3.64303198860235));
#252041=CARTESIAN_POINT('Origin',(5.70826774717982E-15,1.86285477492014E-13,
2.53178198860262));
#252042=CARTESIAN_POINT('Origin',(43.8565665267061,-39.5091373124615,2.53178198860235));
#252043=CARTESIAN_POINT('Origin',(34.1507877370015,-31.1767457860023,3.64303198860241));
#252044=CARTESIAN_POINT('Origin',(45.4673664422113,-41.3663085755614,3.64299466007682));
#252045=CARTESIAN_POINT('Ctrl Pts',(43.7765468711727,-39.4370498736001,
2.59908173515997));
#252046=CARTESIAN_POINT('Ctrl Pts',(43.8042633382934,-39.4620188529802,
2.65878198860235));
#252047=CARTESIAN_POINT('Ctrl Pts',(43.8565665267061,-39.5091373124615,
2.65878198860235));
#252048=CARTESIAN_POINT('Ctrl Pts',(43.7178744835421,-39.5021785224855,
2.59908193199766));
#252049=CARTESIAN_POINT('Ctrl Pts',(43.7615157339677,-39.5094654441323,
2.65877685806628));
#252050=CARTESIAN_POINT('Ctrl Pts',(43.8224770900131,-39.5469637653733,
2.65878198860235));
#252051=CARTESIAN_POINT('Ctrl Pts',(43.6818502604301,-39.5788516269094,
2.63872492669768));
#252052=CARTESIAN_POINT('Ctrl Pts',(43.7389249259235,-39.5685043961835,
2.69532212015245));
#252053=CARTESIAN_POINT('Ctrl Pts',(43.8091917332947,-39.5983821485326,
2.68176836726621));
#252054=CARTESIAN_POINT('Ctrl Pts',(43.6640874258695,-39.7059848156952,
2.75442176402224));
#252055=CARTESIAN_POINT('Ctrl Pts',(43.7412697217743,-39.6560168722784,
2.79203179920111));
#252056=CARTESIAN_POINT('Ctrl Pts',(43.8212571467122,-39.6923865500756,
2.74885310748133));
#252057=CARTESIAN_POINT('Ctrl Pts',(43.6806424921203,-39.7566878101774,
2.82866089558371));
#252058=CARTESIAN_POINT('Ctrl Pts',(43.7668962219034,-39.6846695243133,
2.85316563119134));
#252059=CARTESIAN_POINT('Ctrl Pts',(43.8452710114196,-39.734802377006,2.79189751796581));
#252060=CARTESIAN_POINT('Ctrl Pts',(43.7143933160628,-39.787077884674,2.90134173515996));
#252061=CARTESIAN_POINT('Ctrl Pts',(43.7993487829618,-39.6934538167793,
2.90103711553202));
#252062=CARTESIAN_POINT('Ctrl Pts',(43.8790236240225,-39.7651933658992,
2.83404198860234));
#252063=CARTESIAN_POINT('Origin',(43.7940440370149,-39.8595727587348,2.83404198860235));
#252064=CARTESIAN_POINT('Origin',(45.434534810367,-41.3366772856856,3.56647653971801));
#252065=CARTESIAN_POINT('Origin',(45.3737170758078,-41.2819167515321,3.42473028058456));
#252066=CARTESIAN_POINT('Origin',(43.9264348094903,-39.9787779456548,3.11913648168266));
#252067=CARTESIAN_POINT('Origin',(44.0588255818383,-40.0979831325492,3.40423097483283));
#252068=CARTESIAN_POINT('Ctrl Pts',(45.1285089182138,-41.0611303347397,
3.36123028058453));
#252069=CARTESIAN_POINT('Ctrl Pts',(45.2134885052213,-40.9667509419041,
3.36123028058454));
#252070=CARTESIAN_POINT('Ctrl Pts',(45.2134885052213,-40.9667509419041,
3.23423028058453));
#252071=CARTESIAN_POINT('Ctrl Pts',(45.195556442937,-41.1211850608431,3.36123028058453));
#252072=CARTESIAN_POINT('Ctrl Pts',(45.2803165088406,-41.0269231466347,
3.36099641108291));
#252073=CARTESIAN_POINT('Ctrl Pts',(45.3138235084273,-41.0570929845754,
3.23423043688364));
#252074=CARTESIAN_POINT('Ctrl Pts',(45.2589537050094,-41.1779726855636,
3.41054258905254));
#252075=CARTESIAN_POINT('Ctrl Pts',(45.3438226072621,-41.0841042944886,
3.41008815826071));
#252076=CARTESIAN_POINT('Ctrl Pts',(45.4086973919088,-41.1425178129604,
3.308198673043));
#252077=CARTESIAN_POINT('Ctrl Pts',(45.2923641298562,-41.20790021159,3.48823028058455));
#252078=CARTESIAN_POINT('Ctrl Pts',(45.377327533411,-41.1142722654999,3.48794691941571));
#252079=CARTESIAN_POINT('Ctrl Pts',(45.4586966628153,-41.1875373586965,
3.42473028058456));
#252080=CARTESIAN_POINT('Origin',(45.1285089182138,-41.0611303347397,3.23423028058453));
#252081=CARTESIAN_POINT('Ctrl Pts',(43.9791725362587,-40.0254908126581,
3.47153072139045));
#252082=CARTESIAN_POINT('Ctrl Pts',(44.0642551277136,-39.9317223035489,
3.4712274628505));
#252083=CARTESIAN_POINT('Ctrl Pts',(44.143924604647,-40.0037114707673,3.4041304667676));
#252084=CARTESIAN_POINT('Ctrl Pts',(44.0645378932532,-40.1025202360392,
3.65553813457958));
#252085=CARTESIAN_POINT('Ctrl Pts',(44.1495813562435,-40.008550015784,3.65520336072267));
#252086=CARTESIAN_POINT('Ctrl Pts',(44.2122579788845,-40.0652391174772,
3.55128134519978));
#252087=CARTESIAN_POINT('Ctrl Pts',(44.217894138565,-40.240900132389,3.77003198860236));
#252088=CARTESIAN_POINT('Ctrl Pts',(44.3029888158522,-40.1466780419433,
3.76980209313978));
#252089=CARTESIAN_POINT('Ctrl Pts',(44.3350158129998,-40.1757707681167,
3.6428419538732));
#252090=CARTESIAN_POINT('Ctrl Pts',(44.37898315373,-40.3862543050931,3.77003198860236));
#252091=CARTESIAN_POINT('Ctrl Pts',(44.4640900341671,-40.2917335385817,
3.77003198860236));
#252092=CARTESIAN_POINT('Ctrl Pts',(44.463962645542,-40.2918750179829,3.64284189403775));
#252093=CARTESIAN_POINT('Origin',(44.37898315373,-40.3862543050931,3.64303198860235));
#252094=CARTESIAN_POINT('Origin',(33.3184119221875,-30.4272712359681,3.2342302805846));
#252095=CARTESIAN_POINT('Origin',(45.0161393894798,-40.9599523566118,3.23423028058453));
#252096=CARTESIAN_POINT('Origin',(33.1880655373225,-30.3099068238761,3.64303198860241));
#252097=CARTESIAN_POINT('Origin',(44.677218962552,-40.6548553974674,3.6429917172175));
#252098=CARTESIAN_POINT('Ctrl Pts',(44.8522789915946,-40.8131880745599,
3.48823028058453));
#252099=CARTESIAN_POINT('Ctrl Pts',(44.9380175594367,-40.718715788233,3.48852004212231));
#252100=CARTESIAN_POINT('Ctrl Pts',(44.855910766329,-40.6447864996546,3.42473028058453));
#252101=CARTESIAN_POINT('Ctrl Pts',(44.8858042435448,-40.8432146576624,
3.4102800584838));
#252102=CARTESIAN_POINT('Ctrl Pts',(44.9712860523949,-40.7486708738375,
3.41074404220322));
#252103=CARTESIAN_POINT('Ctrl Pts',(44.9060790100844,-40.6899581892272,
3.30780486243906));
#252104=CARTESIAN_POINT('Ctrl Pts',(44.9493173051415,-40.9001003367632,
3.36123028058453));
#252105=CARTESIAN_POINT('Ctrl Pts',(45.0343891839554,-40.8054891887032,
3.36146460586378));
#252106=CARTESIAN_POINT('Ctrl Pts',(45.0011219300373,-40.7755352187347,
3.2342304530841));
#252107=CARTESIAN_POINT('Ctrl Pts',(45.0161393894798,-40.9599523566118,
3.36123028058453));
#252108=CARTESIAN_POINT('Ctrl Pts',(45.1011189764874,-40.8655729637762,
3.36123028058453));
#252109=CARTESIAN_POINT('Ctrl Pts',(45.1011189764874,-40.8655729637762,
3.23423028058453));
#252110=CARTESIAN_POINT('Origin',(44.7709311793215,-40.7391658924902,3.42473028058453));
#252111=CARTESIAN_POINT('Origin',(44.7104761492018,-40.6847319392787,3.56563113524736));
#252112=CARTESIAN_POINT('Origin',(49.8797426639505,-35.8473027488283,3.56647653909349));
#252113=CARTESIAN_POINT('Origin',(49.9155525184332,-35.8732562382981,3.64299466007415));
#252114=CARTESIAN_POINT('Origin',(49.8135340601227,-35.7991993820654,3.42473028058459));
#252115=CARTESIAN_POINT('Ctrl Pts',(49.7242207306179,-35.7350130971381,
3.4882302805846));
#252116=CARTESIAN_POINT('Ctrl Pts',(49.650303664679,-35.8375861910549,3.48794691941576));
#252117=CARTESIAN_POINT('Ctrl Pts',(49.7388853330816,-35.9019445403511,
3.42473028058461));
#252118=CARTESIAN_POINT('Ctrl Pts',(49.6878783768803,-35.7084656432344,
3.41028005925061));
#252119=CARTESIAN_POINT('Ctrl Pts',(49.6137056554155,-35.8109961808836,
3.40982512231138));
#252120=CARTESIAN_POINT('Ctrl Pts',(49.6842702092623,-35.862264330224,3.307804863728));
#252121=CARTESIAN_POINT('Ctrl Pts',(49.6190282456271,-35.6581711379706,
3.36123028058457));
#252122=CARTESIAN_POINT('Ctrl Pts',(49.5444483977905,-35.7606778378451,
3.3609972104828));
#252123=CARTESIAN_POINT('Ctrl Pts',(49.5808027344254,-35.7870908094897,
3.23423045308385));
#252124=CARTESIAN_POINT('Ctrl Pts',(49.5465907136149,-35.6052536882594,
3.36123028058457));
#252125=CARTESIAN_POINT('Ctrl Pts',(49.4719419865738,-35.707998846545,3.36123028058457));
#252126=CARTESIAN_POINT('Ctrl Pts',(49.4719419865738,-35.707998846545,3.23423028058457));
#252127=CARTESIAN_POINT('Origin',(49.5465907136149,-35.6052536882594,3.23423028058457));
#252128=CARTESIAN_POINT('Origin',(0.186621817602863,0.256862895714232,3.64303198860263));
#252129=CARTESIAN_POINT('Origin',(50.2402240048087,-36.1092077731521,3.64303198860238));
#252130=CARTESIAN_POINT('Origin',(0.186621817602863,0.256862895714235,3.23423028058482));
#252131=CARTESIAN_POINT('Origin',(49.4242607783465,-35.5163757878388,3.23423028058457));
#252132=CARTESIAN_POINT('Ctrl Pts',(50.6762142289952,-36.4252947698671,
3.47153072139047));
#252133=CARTESIAN_POINT('Ctrl Pts',(50.6015094050819,-36.5289136610809,
3.47182327902638));
#252134=CARTESIAN_POINT('Ctrl Pts',(50.5139809070358,-36.4650842624213,
3.40413028959007));
#252135=CARTESIAN_POINT('Ctrl Pts',(50.583123871509,-36.3578045222534,3.65553807120933));
#252136=CARTESIAN_POINT('Ctrl Pts',(50.5083591136191,-36.4612356912204,
3.65586275496775));
#252137=CARTESIAN_POINT('Ctrl Pts',(50.4395906940212,-36.411036609159,3.55128126837191));
#252138=CARTESIAN_POINT('Ctrl Pts',(50.4158900112693,-36.2365613423283,
3.77003198860238));
#252139=CARTESIAN_POINT('Ctrl Pts',(50.3411491755206,-36.3397499727037,
3.77025505748543));
#252140=CARTESIAN_POINT('Ctrl Pts',(50.3059517008897,-36.3139421975378,
3.64284211731174));
#252141=CARTESIAN_POINT('Ctrl Pts',(50.2402240048087,-36.1092077731521,
3.77003198860239));
#252142=CARTESIAN_POINT('Ctrl Pts',(50.1654637560309,-36.2121064279398,
3.77003198860239));
#252143=CARTESIAN_POINT('Ctrl Pts',(50.1655753609474,-36.2119528169505,
3.64284239821683));
#252144=CARTESIAN_POINT('Origin',(50.5887599058106,-36.3624339277665,3.40423097483285));
#252145=CARTESIAN_POINT('Ctrl Pts',(49.4242607783465,-35.5163757878388,
3.36123028058457));
#252146=CARTESIAN_POINT('Ctrl Pts',(49.3496120513053,-35.6191209461244,
3.36123028058457));
#252147=CARTESIAN_POINT('Ctrl Pts',(49.3496120513054,-35.6191209461244,
3.23423028058457));
#252148=CARTESIAN_POINT('Ctrl Pts',(49.3515787599213,-35.4632790141014,
3.36123028058457));
#252149=CARTESIAN_POINT('Ctrl Pts',(49.2767219882466,-35.5661632154394,
3.36146538610215));
#252150=CARTESIAN_POINT('Ctrl Pts',(49.2403833690726,-35.5397616632044,
3.23423043688358));
#252151=CARTESIAN_POINT('Ctrl Pts',(49.2828534857282,-35.4130704930576,
3.41054258693075));
#252152=CARTESIAN_POINT('Ctrl Pts',(49.2081487547888,-35.5163418450519,
3.41100608859616));
#252153=CARTESIAN_POINT('Ctrl Pts',(49.1370998624009,-35.4647218031658,
3.30819866970762));
#252154=CARTESIAN_POINT('Ctrl Pts',(49.2466351556017,-35.3866101428252,
3.48823028058457));
#252155=CARTESIAN_POINT('Ctrl Pts',(49.1720533660035,-35.4901170100359,
3.48852004212235));
#252156=CARTESIAN_POINT('Ctrl Pts',(49.0826686475739,-35.425175210743,3.42473028058457));
#252157=CARTESIAN_POINT('Origin',(49.1573173746151,-35.3224300524574,3.42473028058457));
#252158=CARTESIAN_POINT('Origin',(50.7328855645279,-36.4671473482298,3.11913648178386));
#252159=CARTESIAN_POINT('Origin',(50.8770112231007,-36.5718607685314,2.83404198860237));
#252160=CARTESIAN_POINT('Origin',(49.0915036252748,-35.2746135646418,3.56563113460774));
#252161=CARTESIAN_POINT('Origin',(49.0553654007531,-35.2482948100387,3.64299171721751));
#252162=CARTESIAN_POINT('Ctrl Pts',(50.9399462128206,-36.99116733917,2.59908173515998));
#252163=CARTESIAN_POINT('Ctrl Pts',(50.9097606317998,-36.9692474126332,
2.65878198860237));
#252164=CARTESIAN_POINT('Ctrl Pts',(50.8527980281389,-36.9278827595319,
2.65878198860237));
#252165=CARTESIAN_POINT('Ctrl Pts',(50.9917217504968,-36.9198678602466,
2.59908193475485));
#252166=CARTESIAN_POINT('Ctrl Pts',(50.9474721267433,-36.9173100216915,
2.6587871532533));
#252167=CARTESIAN_POINT('Ctrl Pts',(50.8827604229973,-36.8866065570947,
2.65878198860237));
#252168=CARTESIAN_POINT('Ctrl Pts',(51.019255329238,-36.8393772800886,2.63878778849845));
#252169=CARTESIAN_POINT('Ctrl Pts',(50.9634900918198,-36.8558881875862,
2.69564460180069));
#252170=CARTESIAN_POINT('Ctrl Pts',(50.8901678911829,-36.833817846677,2.68180481624849));
#252171=CARTESIAN_POINT('Ctrl Pts',(51.0231582082094,-36.7103770798832,
2.7544323887862));
#252172=CARTESIAN_POINT('Ctrl Pts',(50.951578055318,-36.7689134067385,2.79268340777093));
#252173=CARTESIAN_POINT('Ctrl Pts',(50.8676678805081,-36.7411592876123,
2.74885926835594));
#252174=CARTESIAN_POINT('Ctrl Pts',(51.0012539523504,-36.6614543958815,
2.82856655361644));
#252175=CARTESIAN_POINT('Ctrl Pts',(50.9229784487449,-36.7432876021357,
2.85384197230816));
#252176=CARTESIAN_POINT('Ctrl Pts',(50.8391515810791,-36.7013347616501,
2.79184624278423));
#252177=CARTESIAN_POINT('Ctrl Pts',(50.9644637245897,-36.6347241449646,
2.90134173515999));
#252178=CARTESIAN_POINT('Ctrl Pts',(50.8898702560322,-36.7381840359676,
2.90163218716366));
#252179=CARTESIAN_POINT('Ctrl Pts',(50.8023624960595,-36.674605926817,2.83404198860237));
#252180=CARTESIAN_POINT('Origin',(50.8527980281389,-36.9278827595319,2.53178198860236));
#252181=CARTESIAN_POINT('Origin',(0.186621817602863,0.256862895714232,3.64303198860263));
#252182=CARTESIAN_POINT('Origin',(48.7306271754181,-35.0124214764577,3.64303198860239));
#252183=CARTESIAN_POINT('Origin',(5.53127843490691E-15,1.85979469832184E-13,
2.53178198860262));
#252184=CARTESIAN_POINT('Origin',(50.8348823336491,-36.9525415975204,2.53178198860237));
#252185=CARTESIAN_POINT('Ctrl Pts',(48.7306271754181,-35.0124214764577,
3.77003198860239));
#252186=CARTESIAN_POINT('Ctrl Pts',(48.6558666212128,-35.1153205516302,
3.77003198860239));
#252187=CARTESIAN_POINT('Ctrl Pts',(48.6559785320126,-35.1151665196287,
3.64284187937003));
#252188=CARTESIAN_POINT('Ctrl Pts',(48.5549543235587,-34.8850714976616,
3.77003198860239));
#252189=CARTESIAN_POINT('Ctrl Pts',(48.4804833899324,-34.9878965398032,
3.76980208963104));
#252190=CARTESIAN_POINT('Ctrl Pts',(48.5155997094336,-35.0131753353115,
3.64284193928289));
#252191=CARTESIAN_POINT('Ctrl Pts',(48.3877151240604,-34.7638382096847,
3.65553535416562));
#252192=CARTESIAN_POINT('Ctrl Pts',(48.3134799021691,-34.8665607873053,
3.65520057834284));
#252193=CARTESIAN_POINT('Ctrl Pts',(48.3819617107282,-34.9160816462002,
3.55127910964184));
#252194=CARTESIAN_POINT('Ctrl Pts',(48.2946219293751,-34.6963546279277,
3.47153072139048));
#252195=CARTESIAN_POINT('Ctrl Pts',(48.2205921440833,-34.7990735417346,
3.47122746281559));
#252196=CARTESIAN_POINT('Ctrl Pts',(48.3075724095167,-34.8620346554123,
3.40413045901239));
#252197=CARTESIAN_POINT('Origin',(48.3820909175334,-34.7591950625526,3.40423097483286));
#252198=CARTESIAN_POINT('Ctrl Pts',(50.5905785208489,-37.1493329797253,
2.90134173515998));
#252199=CARTESIAN_POINT('Ctrl Pts',(50.6659240749088,-37.0464195108245,
2.90163218716366));
#252200=CARTESIAN_POINT('Ctrl Pts',(50.5784163149361,-36.9828414016739,
2.83404198860236));
#252201=CARTESIAN_POINT('Ctrl Pts',(50.6273860247248,-37.1760745934425,
2.82853349835314));
#252202=CARTESIAN_POINT('Ctrl Pts',(50.6810174228652,-37.0763471615757,
2.85381483162217));
#252203=CARTESIAN_POINT('Ctrl Pts',(50.6152221632645,-37.0095824157637,
2.79182701594132));
#252204=CARTESIAN_POINT('Ctrl Pts',(50.680540741014,-37.1816769644883,2.75468822073637));
#252205=CARTESIAN_POINT('Ctrl Pts',(50.7141678268704,-37.095483395542,2.79286913083809));
#252206=CARTESIAN_POINT('Ctrl Pts',(50.6617655220316,-37.0242869695744,
2.74900763297886));
#252207=CARTESIAN_POINT('Ctrl Pts',(50.8012099538931,-37.1386811500602,
2.63954450640347));
#252208=CARTESIAN_POINT('Ctrl Pts',(50.7999485296229,-37.0803097184688,
2.69627684028837));
#252209=CARTESIAN_POINT('Ctrl Pts',(50.7562647493206,-37.0173098767914,
2.68224356036466));
#252210=CARTESIAN_POINT('Ctrl Pts',(50.8700180268814,-37.0873787017253,
2.59908178706366));
#252211=CARTESIAN_POINT('Ctrl Pts',(50.8539379904877,-37.0460487315392,
2.65878704321445));
#252212=CARTESIAN_POINT('Ctrl Pts',(50.8047860147157,-36.9939291606749,
2.65878198860237));
#252213=CARTESIAN_POINT('Ctrl Pts',(50.9219998155904,-37.0158684358552,
2.59908173515998));
#252214=CARTESIAN_POINT('Ctrl Pts',(50.8918248691005,-36.9939338721425,
2.65878198860237));
#252215=CARTESIAN_POINT('Ctrl Pts',(50.8348823336491,-36.9525415975204,
2.65878198860237));
#252216=CARTESIAN_POINT('Origin',(50.503767587895,-37.0855865599595,2.83404198860236));
#252217=CARTESIAN_POINT('Origin',(48.2379650606707,-34.6544814981893,3.11913648166982));
#252218=CARTESIAN_POINT('Origin',(48.0938392037152,-34.5497679336933,2.83404198860239));
#252219=CARTESIAN_POINT('Origin',(50.3596419293386,-36.9808731396133,3.11913648177573));
#252220=CARTESIAN_POINT('Origin',(50.2155162706049,-36.8761597191946,3.40423097483285));
#252221=CARTESIAN_POINT('Ctrl Pts',(48.0063682005191,-34.4869303039389,
2.90134173516));
#252222=CARTESIAN_POINT('Ctrl Pts',(47.9324532779042,-34.5894948283126,
2.90103711553205));
#252223=CARTESIAN_POINT('Ctrl Pts',(48.019190476674,-34.6525130919789,2.83404198860238));
#252224=CARTESIAN_POINT('Ctrl Pts',(47.9696093621204,-34.4602241019842,
2.82862991747951));
#252225=CARTESIAN_POINT('Ctrl Pts',(47.9171056031461,-34.5595620694339,
2.85314045886484));
#252226=CARTESIAN_POINT('Ctrl Pts',(47.9824304277188,-34.6258053530814,
2.79187960999931));
#252227=CARTESIAN_POINT('Ctrl Pts',(47.9167391807674,-34.4546775021458,
2.75470625793289));
#252228=CARTESIAN_POINT('Ctrl Pts',(47.88382973855,-34.5405955452474,2.79224250381846));
#252229=CARTESIAN_POINT('Ctrl Pts',(47.9361122396532,-34.611244401458,2.74901809108239));
#252230=CARTESIAN_POINT('Ctrl Pts',(47.7968564492225,-34.4979061669204,
2.63947868311689));
#252231=CARTESIAN_POINT('Ctrl Pts',(47.7983386612738,-34.5561175928637,
2.69595066767908));
#252232=CARTESIAN_POINT('Ctrl Pts',(47.8422046210398,-34.6187227036509,
2.68220539436033));
#252233=CARTESIAN_POINT('Ctrl Pts',(47.728594491149,-34.5493265808139,2.59908178585035));
#252234=CARTESIAN_POINT('Ctrl Pts',(47.7447672725775,-34.5905382782863,
2.65877670944851));
#252235=CARTESIAN_POINT('Ctrl Pts',(47.7940753146426,-34.6424336528564,
2.65878198860238));
#252236=CARTESIAN_POINT('Ctrl Pts',(47.6769115920308,-34.6205005703627,
2.59908173516));
#252237=CARTESIAN_POINT('Ctrl Pts',(47.7070975168468,-34.6424200234567,
2.65878198860238));
#252238=CARTESIAN_POINT('Ctrl Pts',(47.7640607692767,-34.6837837831338,
2.65878198860238));
#252239=CARTESIAN_POINT('Origin',(47.7640607692768,-34.6837837831338,2.53178198860238));
#252240=CARTESIAN_POINT('Ctrl Pts',(49.866980369603,-36.6229335645802,3.77003198860238));
#252241=CARTESIAN_POINT('Ctrl Pts',(49.9417406248217,-36.5200349009273,
3.77003198860239));
#252242=CARTESIAN_POINT('Ctrl Pts',(49.9416290134548,-36.5201885207949,
3.64284238727527));
#252243=CARTESIAN_POINT('Ctrl Pts',(50.0423873219322,-36.7506494346797,
3.77003198860238));
#252244=CARTESIAN_POINT('Ctrl Pts',(50.1174293675628,-36.6476796282212,
3.77025506105767));
#252245=CARTESIAN_POINT('Ctrl Pts',(50.082007534236,-36.6221794864674,3.6428421064183));
#252246=CARTESIAN_POINT('Ctrl Pts',(50.20937322402,-36.8722311236847,3.65553527987809));
#252247=CARTESIAN_POINT('Ctrl Pts',(50.2846385388137,-36.7691636147932,
3.655859965331));
#252248=CARTESIAN_POINT('Ctrl Pts',(50.2156454684962,-36.719273129351,3.55127902710179));
#252249=CARTESIAN_POINT('Ctrl Pts',(50.3023253562,-36.9399086546478,3.47153072139046));
#252250=CARTESIAN_POINT('Ctrl Pts',(50.3777877242647,-36.8368401378439,
3.47182327905163));
#252251=CARTESIAN_POINT('Ctrl Pts',(50.2900345513017,-36.7733199617888,
3.40413028377937));
#252252=CARTESIAN_POINT('Origin',(49.866980369603,-36.6229335645802,3.64303198860238));
#252253=CARTESIAN_POINT('Origin',(5.7121316272531E-15,1.86290248986529E-13,
2.53178198860262));
#252254=CARTESIAN_POINT('Origin',(47.7461450747869,-34.7084426211224,2.53178198860239));
#252255=CARTESIAN_POINT('Origin',(40.5385041740537,-29.8453988870281,3.64303198860242));
#252256=CARTESIAN_POINT('Origin',(49.5422481179707,-36.3870656659206,3.64299466008053));
#252257=CARTESIAN_POINT('Ctrl Pts',(47.659028586094,-34.6451144164178,2.59908173516));
#252258=CARTESIAN_POINT('Ctrl Pts',(47.6892031885518,-34.667049453401,2.65878198860238));
#252259=CARTESIAN_POINT('Ctrl Pts',(47.7461450747869,-34.7084426211224,
2.65878198860238));
#252260=CARTESIAN_POINT('Ctrl Pts',(47.6074854095242,-34.7160192182654,
2.59908193199744));
#252261=CARTESIAN_POINT('Ctrl Pts',(47.6516492793336,-34.7187044685494,
2.65877685806567));
#252262=CARTESIAN_POINT('Ctrl Pts',(47.7161963245873,-34.7496251731977,
2.65878198860238));
#252263=CARTESIAN_POINT('Ctrl Pts',(47.5796730526556,-34.796037856083,2.63872492669789));
#252264=CARTESIAN_POINT('Ctrl Pts',(47.6353534770334,-34.7797813814947,
2.69532212015227));
#252265=CARTESIAN_POINT('Ctrl Pts',(47.7083584310204,-34.8021505789967,
2.68176836726608));
#252266=CARTESIAN_POINT('Ctrl Pts',(47.575296561615,-34.9243313177586,2.75442176402211));
#252267=CARTESIAN_POINT('Ctrl Pts',(47.6468329724883,-34.866569357181,2.79203179920141));
#252268=CARTESIAN_POINT('Ctrl Pts',(47.7301838844732,-34.8943788354686,
2.74885310748154));
#252269=CARTESIAN_POINT('Ctrl Pts',(47.5970608435775,-34.9730260802968,
2.82866089558384));
#252270=CARTESIAN_POINT('Ctrl Pts',(47.6753141056553,-34.8923863483122,
2.85316563119167));
#252271=CARTESIAN_POINT('Ctrl Pts',(47.7584998599249,-34.9340521716862,
2.79189751796622));
#252272=CARTESIAN_POINT('Ctrl Pts',(47.6338034047604,-34.9997217530253,
2.90134173515999));
#252273=CARTESIAN_POINT('Ctrl Pts',(47.7085070967808,-34.8977303031694,
2.90103711553205));
#252274=CARTESIAN_POINT('Ctrl Pts',(47.7952442955506,-34.9607485668358,
2.83404198860238));
#252275=CARTESIAN_POINT('Origin',(47.7205955685095,-35.0634937251214,2.83404198860238));
#252276=CARTESIAN_POINT('Origin',(49.5064990280468,-36.3610285393803,3.56647653971683));
#252277=CARTESIAN_POINT('Origin',(49.440290424917,-36.3129251734935,3.42473028058461));
#252278=CARTESIAN_POINT('Origin',(47.8647214254841,-35.1682072895556,3.11913648168284));
#252279=CARTESIAN_POINT('Origin',(48.0088472823277,-35.2729208539807,3.40423097483287));
#252280=CARTESIAN_POINT('Ctrl Pts',(49.1733470784092,-36.1189794796875,
3.36123028058457));
#252281=CARTESIAN_POINT('Ctrl Pts',(49.2479958054503,-36.0162343214019,
3.36123028058457));
#252282=CARTESIAN_POINT('Ctrl Pts',(49.2479958054503,-36.0162343214019,
3.23423028058457));
#252283=CARTESIAN_POINT('Ctrl Pts',(49.2463047380091,-36.1716968449913,
3.36123028058457));
#252284=CARTESIAN_POINT('Ctrl Pts',(49.3207474263657,-36.0690914679756,
3.36099641108531));
#252285=CARTESIAN_POINT('Ctrl Pts',(49.3572244778989,-36.0955935972133,
3.23423043688377));
#252286=CARTESIAN_POINT('Ctrl Pts',(49.3152906263894,-36.2215465627845,
3.4105425890526));
#252287=CARTESIAN_POINT('Ctrl Pts',(49.3898826892475,-36.1193211766471,
3.41008815825869));
#252288=CARTESIAN_POINT('Ctrl Pts',(49.4605079583572,-36.1706334382067,
3.30819867304271));
#252289=CARTESIAN_POINT('Ctrl Pts',(49.3516463037389,-36.2478178023243,
3.48823028058459));
#252290=CARTESIAN_POINT('Ctrl Pts',(49.4263574835555,-36.1458216659117,
3.48794691941576));
#252291=CARTESIAN_POINT('Ctrl Pts',(49.5149391519582,-36.2101800152079,
3.42473028058461));
#252292=CARTESIAN_POINT('Origin',(49.1733470784092,-36.1189794796875,3.23423028058457));
#252293=CARTESIAN_POINT('Ctrl Pts',(47.9220530736691,-35.209151665052,3.47153072139048));
#252294=CARTESIAN_POINT('Ctrl Pts',(47.9968680956257,-35.1070032771111,
3.47122746285053));
#252295=CARTESIAN_POINT('Ctrl Pts',(48.0836260518497,-35.1702703521461,
3.40413046676755));
#252296=CARTESIAN_POINT('Ctrl Pts',(48.0150025575607,-35.2768360036061,
3.65553813457965));
#252297=CARTESIAN_POINT('Ctrl Pts',(48.0897575808475,-35.1744910995543,
3.65520336072245));
#252298=CARTESIAN_POINT('Ctrl Pts',(48.1580164790723,-35.2243181613706,
3.55128134519974));
#252299=CARTESIAN_POINT('Ctrl Pts',(48.1819833392254,-35.3984277477525,
3.7700319886024));
#252300=CARTESIAN_POINT('Ctrl Pts',(48.256762968645,-35.2958269999273,3.76980209313948));
#252301=CARTESIAN_POINT('Ctrl Pts',(48.2916555365119,-35.3214126203087,
3.64284195387307));
#252302=CARTESIAN_POINT('Ctrl Pts',(48.3573835402124,-35.5261472678858,
3.77003198860239));
#252303=CARTESIAN_POINT('Ctrl Pts',(48.4321440857833,-35.4232482045974,
3.77003198860239));
#252304=CARTESIAN_POINT('Ctrl Pts',(48.4320321836307,-35.4234022246971,
3.64284189403762));
#252305=CARTESIAN_POINT('Origin',(48.3573835402124,-35.5261472678858,3.64303198860239));
#252306=CARTESIAN_POINT('Origin',(39.5520252162596,-29.1286799712083,3.23423028058462));
#252307=CARTESIAN_POINT('Origin',(49.0510171431408,-36.0301015792669,3.23423028058457));
#252308=CARTESIAN_POINT('Origin',(39.3975469582356,-29.0164449471017,3.64303198860243));
#252309=CARTESIAN_POINT('Origin',(48.6820620414868,-35.7621028045843,3.64299171721786));
#252310=CARTESIAN_POINT('Ctrl Pts',(48.8727133447948,-35.9012693628897,
3.48823028058456));
#252311=CARTESIAN_POINT('Ctrl Pts',(48.9481071848801,-35.7983524848928,
3.48852004212234));
#252312=CARTESIAN_POINT('Ctrl Pts',(48.8587224664505,-35.7334106855999,
3.42473028058456));
#252313=CARTESIAN_POINT('Ctrl Pts',(48.9091935744948,-35.9276271141626,
3.41028005848382));
#252314=CARTESIAN_POINT('Ctrl Pts',(48.9843245886205,-35.8246659689611,
3.41074404220299));
#252315=CARTESIAN_POINT('Ctrl Pts',(48.9133376106103,-35.7730909105051,
3.3078048624387));
#252316=CARTESIAN_POINT('Ctrl Pts',(48.9783048775129,-35.9775622448352,
3.36123028058457));
#252317=CARTESIAN_POINT('Ctrl Pts',(49.0530211657563,-35.8745769537839,
3.36146460586502));
#252318=CARTESIAN_POINT('Ctrl Pts',(49.0168051108909,-35.8482644497254,
3.2342304530841));
#252319=CARTESIAN_POINT('Ctrl Pts',(49.0510171431408,-36.0301015792669,
3.36123028058457));
#252320=CARTESIAN_POINT('Ctrl Pts',(49.1256658701819,-35.9273564209813,
3.36123028058457));
#252321=CARTESIAN_POINT('Ctrl Pts',(49.1256658701819,-35.9273564209813,
3.23423028058457));
#252322=CARTESIAN_POINT('Origin',(48.7840737394093,-35.8361558438855,3.42473028058457));
#252323=CARTESIAN_POINT('Origin',(48.7182599907917,-35.7883393569593,3.56563113524709));
#252324=CARTESIAN_POINT('Origin',(53.3535596832581,-30.4370746247553,3.56647653909434));
#252325=CARTESIAN_POINT('Origin',(53.3918862459827,-30.4591427892358,3.64299466007485));
#252326=CARTESIAN_POINT('Origin',(53.282685606085,-30.3961554568828,3.42473028058463));
#252327=CARTESIAN_POINT('Ctrl Pts',(53.1871522506179,-30.3416565762228,
3.48823028058463));
#252328=CARTESIAN_POINT('Ctrl Pts',(53.1243619179799,-30.4513942013105,
3.48794691941579));
#252329=CARTESIAN_POINT('Ctrl Pts',(53.219185606085,-30.5061406831635,3.42473028058464));
#252330=CARTESIAN_POINT('Ctrl Pts',(53.1482340195355,-30.3190533624386,
3.41028005925068));
#252331=CARTESIAN_POINT('Ctrl Pts',(53.0851849835374,-30.4287753876651,
3.40982512231055));
#252332=CARTESIAN_POINT('Ctrl Pts',(53.1607219582391,-30.4723866803419,
3.30780486372884));
#252333=CARTESIAN_POINT('Ctrl Pts',(53.0745038491597,-30.2762311741517,
3.36123028058461));
#252334=CARTESIAN_POINT('Ctrl Pts',(53.0110474253457,-30.3859720484848,
3.36099721048422));
#252335=CARTESIAN_POINT('Ctrl Pts',(53.0499635164591,-30.4084402641652,
3.23423045308377));
#252336=CARTESIAN_POINT('Ctrl Pts',(52.9969317578291,-30.2311753956704,
3.36123028058461));
#252337=CARTESIAN_POINT('Ctrl Pts',(52.9334317578291,-30.341160621951,3.36123028058461));
#252338=CARTESIAN_POINT('Ctrl Pts',(52.9334317578291,-30.341160621951,3.23423028058461));
#252339=CARTESIAN_POINT('Origin',(52.9969317578291,-30.2311753956704,3.23423028058461));
#252340=CARTESIAN_POINT('Origin',(0.158750000000002,0.274963065701745,3.64303198860263));
#252341=CARTESIAN_POINT('Origin',(53.739442799329,-30.6598643453566,3.64303198860242));
#252342=CARTESIAN_POINT('Origin',(0.158750000000002,0.274963065701748,3.23423028058482));
#252343=CARTESIAN_POINT('Origin',(52.8659816883963,-30.1555713378329,3.23423028058461));
#252344=CARTESIAN_POINT('Ctrl Pts',(54.2060847114746,-30.9286463962969,
3.47153072139051));
#252345=CARTESIAN_POINT('Ctrl Pts',(54.1426202518673,-31.0395064328251,
3.47182327902642));
#252346=CARTESIAN_POINT('Ctrl Pts',(54.0488992551386,-30.985175917683,3.4041302895902));
#252347=CARTESIAN_POINT('Ctrl Pts',(54.1064496608375,-30.8712564593356,
3.65553807120937));
#252348=CARTESIAN_POINT('Ctrl Pts',(54.042905973262,-30.9819360667859,3.65586275496656));
#252349=CARTESIAN_POINT('Ctrl Pts',(53.9692670413556,-30.9392002377689,
3.55128126837208));
#252350=CARTESIAN_POINT('Ctrl Pts',(53.9274585619027,-30.7681581606536,
3.77003198860242));
#252351=CARTESIAN_POINT('Ctrl Pts',(53.8639133132313,-30.8785940576183,
3.77025505748772));
#252352=CARTESIAN_POINT('Ctrl Pts',(53.8262110069728,-30.8566067980785,
3.64284211731191));
#252353=CARTESIAN_POINT('Ctrl Pts',(53.7394427993291,-30.6598643453566,
3.77003198860242));
#252354=CARTESIAN_POINT('Ctrl Pts',(53.6758479332737,-30.770013884465,3.77003198860242));
#252355=CARTESIAN_POINT('Ctrl Pts',(53.675942870086,-30.7698494490826,3.64284239821704));
#252356=CARTESIAN_POINT('Origin',(54.1125387249983,-30.8752713784753,3.40423097483289));
#252357=CARTESIAN_POINT('Ctrl Pts',(52.8659816883963,-30.1555713378329,
3.36123028058461));
#252358=CARTESIAN_POINT('Ctrl Pts',(52.8024816883963,-30.2655565641136,
3.36123028058461));
#252359=CARTESIAN_POINT('Ctrl Pts',(52.8024816883963,-30.2655565641135,
3.23423028058461));
#252360=CARTESIAN_POINT('Ctrl Pts',(52.788147705508,-30.1103627734736,3.36123028058462));
#252361=CARTESIAN_POINT('Ctrl Pts',(52.7244553345199,-30.2205080276993,
3.36146538610119));
#252362=CARTESIAN_POINT('Ctrl Pts',(52.6855560684225,-30.1980495259465,
3.2342304368842));
#252363=CARTESIAN_POINT('Ctrl Pts',(52.7145506960115,-30.0676130472582,
3.4105425869308));
#252364=CARTESIAN_POINT('Ctrl Pts',(52.6510500011306,-30.1781274387051,
3.41100608859755));
#252365=CARTESIAN_POINT('Ctrl Pts',(52.5749945583568,-30.1342168083481,
3.30819866970778));
#252366=CARTESIAN_POINT('Ctrl Pts',(52.67576491394,-30.0450834959828,3.4882302805846));
#252367=CARTESIAN_POINT('Ctrl Pts',(52.612411104956,-30.1558192615993,3.48852004212238));
#252368=CARTESIAN_POINT('Ctrl Pts',(52.5167277788845,-30.1005764675349,
3.4247302805846));
#252369=CARTESIAN_POINT('Origin',(52.5802277788845,-29.9905912412543,3.42473028058461));
#252370=CARTESIAN_POINT('Origin',(54.2668203812008,-30.9643459342411,3.11913648178328));
#252371=CARTESIAN_POINT('Origin',(54.4211020372442,-31.0534204898625,2.8340419886024));
#252372=CARTESIAN_POINT('Origin',(52.5097763801598,-29.9499161072436,3.56563113460845));
#252373=CARTESIAN_POINT('Origin',(52.4710850656387,-29.927519002605,3.64299171721728));
#252374=CARTESIAN_POINT('Ctrl Pts',(54.5275217339724,-31.4638515574732,
2.59908173516002));
#252375=CARTESIAN_POINT('Ctrl Pts',(54.4952102564869,-31.4452069629845,
2.65878198860241));
#252376=CARTESIAN_POINT('Ctrl Pts',(54.4342359163067,-31.4100231232053,
2.65878198860241));
#252377=CARTESIAN_POINT('Ctrl Pts',(54.5715608148713,-31.3875306471672,
2.59908193475617));
#252378=CARTESIAN_POINT('Ctrl Pts',(54.5272862282495,-31.389612165888,2.65878715325355));
#252379=CARTESIAN_POINT('Ctrl Pts',(54.4597196360186,-31.3658411130322,
2.65878198860241));
#252380=CARTESIAN_POINT('Ctrl Pts',(54.5905300051368,-31.304602960155,2.63878778849852));
#252381=CARTESIAN_POINT('Ctrl Pts',(54.5367961153114,-31.3268524737452,
2.69564460180104));
#252382=CARTESIAN_POINT('Ctrl Pts',(54.4615686025424,-31.3125672934286,
2.68180481624844));
#252383=CARTESIAN_POINT('Ctrl Pts',(54.5809273110399,-31.1759014746032,
2.75443238878622));
#252384=CARTESIAN_POINT('Ctrl Pts',(54.5158579940075,-31.2415992967173,
2.79268340777048));
#252385=CARTESIAN_POINT('Ctrl Pts',(54.4295063924933,-31.222768219185,2.74885926835607));
#252386=CARTESIAN_POINT('Ctrl Pts',(54.5540292360083,-31.129536412388,2.82856655361651));
#252387=CARTESIAN_POINT('Ctrl Pts',(54.4847364330952,-31.2191033458799,
2.8538419723079));
#252388=CARTESIAN_POINT('Ctrl Pts',(54.3969835118378,-31.1861426211008,
2.79184624278575));
#252389=CARTESIAN_POINT('Ctrl Pts',(54.5146464769142,-31.1067982185526,
2.90134173516003));
#252390=CARTESIAN_POINT('Ctrl Pts',(54.4512761425986,-31.2174884860856,
2.9016321871637));
#252391=CARTESIAN_POINT('Ctrl Pts',(54.3576020372442,-31.1634057161431,
2.83404198860241));
#252392=CARTESIAN_POINT('Origin',(54.4342359163067,-31.4100231232053,2.5317819886024));
#252393=CARTESIAN_POINT('Origin',(0.158750000000002,0.274963065701745,3.64303198860263));
#252394=CARTESIAN_POINT('Origin',(52.123470313195,-29.7268821954841,3.64303198860242));
#252395=CARTESIAN_POINT('Origin',(5.52187834149254E-15,1.85964994957679E-13,
2.53178198860262));
#252396=CARTESIAN_POINT('Origin',(54.4189959163067,-31.4364195775126,2.5317819886024));
#252397=CARTESIAN_POINT('Ctrl Pts',(52.123470313195,-29.7268821954841,3.77003198860243));
#252398=CARTESIAN_POINT('Ctrl Pts',(52.0598751873275,-29.8370321846005,
3.77003198860243));
#252399=CARTESIAN_POINT('Ctrl Pts',(52.0599703843398,-29.8368672985384,
3.64284187937001));
#252400=CARTESIAN_POINT('Ctrl Pts',(51.9354481180157,-29.6185926664438,
3.77003198860243));
#252401=CARTESIAN_POINT('Ctrl Pts',(51.8721332876,-29.7286387544935,3.7698020896278));
#252402=CARTESIAN_POINT('Ctrl Pts',(51.9096995898758,-29.7501084152001,
3.64284193928265));
#252403=CARTESIAN_POINT('Ctrl Pts',(51.7564527430631,-29.5155047636227,
3.65553535416569));
#252404=CARTESIAN_POINT('Ctrl Pts',(51.6933616226623,-29.6254243098814,
3.65520057834603));
#252405=CARTESIAN_POINT('Ctrl Pts',(51.7666446199934,-29.6675155901152,
3.55127910964215));
#252406=CARTESIAN_POINT('Ctrl Pts',(51.6568155675431,-29.4581217525665,
3.47153072139052));
#252407=CARTESIAN_POINT('Ctrl Pts',(51.5939283753698,-29.5680161811085,
3.47122746281562));
#252408=CARTESIAN_POINT('Ctrl Pts',(51.6870133822666,-29.6215404737374,
3.4041304590124));
#252409=CARTESIAN_POINT('Origin',(51.7503740054947,-29.5114749417997,3.4042309748329));
#252410=CARTESIAN_POINT('Ctrl Pts',(54.1966007261211,-31.6576696180576,
2.90134173516003));
#252411=CARTESIAN_POINT('Ctrl Pts',(54.2607761425987,-31.5474441649275,
2.9016321871637));
#252412=CARTESIAN_POINT('Ctrl Pts',(54.1671020372442,-31.493361394985,2.83404198860241));
#252413=CARTESIAN_POINT('Ctrl Pts',(54.2360018544271,-31.6804173065994,
2.82853349835321));
#252414=CARTESIAN_POINT('Ctrl Pts',(54.2789150989581,-31.5756301844087,
2.8538148316222));
#252415=CARTESIAN_POINT('Ctrl Pts',(54.2065014563936,-31.5161086602368,
2.79182701594168));
#252416=CARTESIAN_POINT('Ctrl Pts',(54.2894509908547,-31.6804328064616,
2.75468822073639));
#252417=CARTESIAN_POINT('Ctrl Pts',(54.3138841827112,-31.5911964272959,
2.79286913083789));
#252418=CARTESIAN_POINT('Ctrl Pts',(54.2543268901844,-31.525867555196,2.74900763297894));
#252419=CARTESIAN_POINT('Ctrl Pts',(54.4049648787504,-31.6250591602182,
2.63954450640354));
#252420=CARTESIAN_POINT('Ctrl Pts',(54.3976088886511,-31.5671393481769,
2.69627684028851));
#252421=CARTESIAN_POINT('Ctrl Pts',(54.3475791360316,-31.5090508246484,
2.68224356036467));
#252422=CARTESIAN_POINT('Ctrl Pts',(54.4680334478301,-31.5668453499332,
2.59908178706226));
#252423=CARTESIAN_POINT('Ctrl Pts',(54.4477213412894,-31.5274226111426,
2.65878704321479));
#252424=CARTESIAN_POINT('Ctrl Pts',(54.3933906465336,-31.4807263372346,
2.6587819886024));
#252425=CARTESIAN_POINT('Ctrl Pts',(54.5122556166615,-31.4902932482899,
2.59908173516002));
#252426=CARTESIAN_POINT('Ctrl Pts',(54.4799531854483,-31.4716329851981,
2.6587819886024));
#252427=CARTESIAN_POINT('Ctrl Pts',(54.4189959163067,-31.4364195775126,
2.65878198860241));
#252428=CARTESIAN_POINT('Origin',(54.1036020372442,-31.6033466212656,2.8340419886024));
#252429=CARTESIAN_POINT('Origin',(51.5960921371869,-29.4224002636341,3.1191364816712));
#252430=CARTESIAN_POINT('Origin',(51.4418102687789,-29.3333255853447,2.83404198860242));
#252431=CARTESIAN_POINT('Origin',(53.9493203812085,-31.5142720655992,3.11913648177336));
#252432=CARTESIAN_POINT('Origin',(53.7950387249983,-31.4251975098784,3.40423097483289));
#252433=CARTESIAN_POINT('Ctrl Pts',(51.3482501200169,-29.2799753962454,
2.90134173516004));
#252434=CARTESIAN_POINT('Ctrl Pts',(51.2854610232005,-29.3897042746966,
2.90103711553209));
#252435=CARTESIAN_POINT('Ctrl Pts',(51.3783102687789,-29.4433108116253,
2.83404198860242));
#252436=CARTESIAN_POINT('Ctrl Pts',(51.3089010921307,-29.257257838549,2.82862991747938));
#252437=CARTESIAN_POINT('Ctrl Pts',(51.2670685993222,-29.36153975946,2.85314045886519));
#252438=CARTESIAN_POINT('Ctrl Pts',(51.3389598763133,-29.4205918519426,
2.79187960999965));
#252439=CARTESIAN_POINT('Ctrl Pts',(51.2557407616061,-29.2572680623741,
2.7547062579331));
#252440=CARTESIAN_POINT('Ctrl Pts',(51.2319924817695,-29.3461554108679,
2.7922425038186));
#252441=CARTESIAN_POINT('Ctrl Pts',(51.2913733902321,-29.4109522357559,
2.74901809108242));
#252442=CARTESIAN_POINT('Ctrl Pts',(51.1410333861059,-29.3127910737007,
2.63947868311675));
#252443=CARTESIAN_POINT('Ctrl Pts',(51.1485922293425,-29.3705286780138,
2.69595066767904));
#252444=CARTESIAN_POINT('Ctrl Pts',(51.1987619028147,-29.4282055900894,
2.68220539436038));
#252445=CARTESIAN_POINT('Ctrl Pts',(51.0785202710263,-29.3710651187638,
2.59908178585086));
#252446=CARTESIAN_POINT('Ctrl Pts',(51.0989122516733,-29.4103605382568,
2.65877670944826));
#252447=CARTESIAN_POINT('Ctrl Pts',(51.1533747228781,-29.4568175306709,
2.65878198860242));
#252448=CARTESIAN_POINT('Ctrl Pts',(51.0345602039891,-29.4472515437727,
2.59908173516004));
#252449=CARTESIAN_POINT('Ctrl Pts',(51.0668719738981,-29.4658956314759,
2.65878198860242));
#252450=CARTESIAN_POINT('Ctrl Pts',(51.1278468659051,-29.5010785149103,
2.65878198860242));
#252451=CARTESIAN_POINT('Origin',(51.1278468659051,-29.5010785149103,2.53178198860242));
#252452=CARTESIAN_POINT('Ctrl Pts',(53.421942799329,-31.2097904767597,3.77003198860242));
#252453=CARTESIAN_POINT('Ctrl Pts',(53.4855376708633,-31.0996409281616,
3.77003198860242));
#252454=CARTESIAN_POINT('Ctrl Pts',(53.4854427285639,-31.0998053730479,
3.64284238727567));
#252455=CARTESIAN_POINT('Ctrl Pts',(53.6097387976563,-31.3184716867866,
3.77003198860243));
#252456=CARTESIAN_POINT('Ctrl Pts',(53.6736064794785,-31.2082219299917,
3.77025506105756));
#252457=CARTESIAN_POINT('Ctrl Pts',(53.6357132000301,-31.1865640704865,
3.6428421064187));
#252458=CARTESIAN_POINT('Ctrl Pts',(53.7885186806147,-31.4219325588438,
3.65553527987807));
#252459=CARTESIAN_POINT('Ctrl Pts',(53.8525981958198,-31.3115622968576,
3.65585996533081));
#252460=CARTESIAN_POINT('Ctrl Pts',(53.7787681009854,-31.2691568563317,
3.55127902710171));
#252461=CARTESIAN_POINT('Ctrl Pts',(53.8880358395974,-31.4795232016781,
3.47153072139051));
#252462=CARTESIAN_POINT('Ctrl Pts',(53.9523112232411,-31.3691313396255,
3.47182327905167));
#252463=CARTESIAN_POINT('Ctrl Pts',(53.8583991049523,-31.3151318380575,
3.40413028377961));
#252464=CARTESIAN_POINT('Origin',(53.421942799329,-31.2097904767597,3.64303198860242));
#252465=CARTESIAN_POINT('Origin',(5.71547558359784E-15,1.86295398227745E-13,
2.53178198860262));
#252466=CARTESIAN_POINT('Origin',(51.1126068659051,-29.5274749692176,2.53178198860242));
#252467=CARTESIAN_POINT('Origin',(46.508091798073,-27.2180767400477,3.64303198860244));
#252468=CARTESIAN_POINT('Origin',(53.074334555967,-31.0091584503641,3.6429946600813));
#252469=CARTESIAN_POINT('Ctrl Pts',(51.0193480105331,-29.4735998357329,
2.59908173516004));
#252470=CARTESIAN_POINT('Ctrl Pts',(51.051650149069,-29.4922606054638,2.65878198860242));
#252471=CARTESIAN_POINT('Ctrl Pts',(51.1126068659051,-29.5274749692176,
2.65878198860242));
#252472=CARTESIAN_POINT('Ctrl Pts',(50.9754987628539,-29.5495039426962,
2.59908193199881));
#252473=CARTESIAN_POINT('Ctrl Pts',(51.0197013834523,-29.5475581014572,
2.6587768580658));
#252474=CARTESIAN_POINT('Ctrl Pts',(51.0871269269774,-29.5715624158004,
2.65878198860242));
#252475=CARTESIAN_POINT('Ctrl Pts',(50.9562029902293,-29.6319914129664,
2.63872492669796));
#252476=CARTESIAN_POINT('Ctrl Pts',(51.0098791271093,-29.6100038038521,
2.69532212015255));
#252477=CARTESIAN_POINT('Ctrl Pts',(51.084822370159,-29.6246193648988,2.68176836726625));
#252478=CARTESIAN_POINT('Ctrl Pts',(50.9652607924608,-29.7600395375182,
2.75442176402211));
#252479=CARTESIAN_POINT('Ctrl Pts',(51.0303675504162,-29.6951164119086,
2.7920317992012));
#252480=CARTESIAN_POINT('Ctrl Pts',(51.1161687394138,-29.7140610042223,
2.74885310748144));
#252481=CARTESIAN_POINT('Ctrl Pts',(50.9919958361066,-29.806192558105,2.82866089558394));
#252482=CARTESIAN_POINT('Ctrl Pts',(51.0613912713634,-29.7178148857786,
2.85316563119245));
#252483=CARTESIAN_POINT('Ctrl Pts',(51.1484765898563,-29.750557180353,2.79189751796625));
#252484=CARTESIAN_POINT('Ctrl Pts',(51.0313275753413,-29.8289013456877,
2.90134173516004));
#252485=CARTESIAN_POINT('Ctrl Pts',(51.0949610232005,-29.7196599535384,
2.9010371155321));
#252486=CARTESIAN_POINT('Ctrl Pts',(51.1878102687789,-29.7732664904672,
2.83404198860242));
#252487=CARTESIAN_POINT('Origin',(51.1243102687789,-29.8832517167478,2.83404198860241));
#252488=CARTESIAN_POINT('Origin',(53.0360596824734,-30.9870007553613,3.56647653971681));
#252489=CARTESIAN_POINT('Origin',(52.965185606085,-30.946081588286,3.42473028058464));
#252490=CARTESIAN_POINT('Origin',(51.2785921372034,-29.9723263949827,3.11913648167932));
#252491=CARTESIAN_POINT('Origin',(51.4328740054947,-30.0614010732028,3.4042309748329));
#252492=CARTESIAN_POINT('Ctrl Pts',(52.6794317578291,-30.7811015270735,
3.36123028058461));
#252493=CARTESIAN_POINT('Ctrl Pts',(52.7429317578291,-30.6711163007929,
3.3612302805846));
#252494=CARTESIAN_POINT('Ctrl Pts',(52.7429317578291,-30.6711163007929,
3.23423028058461));
#252495=CARTESIAN_POINT('Ctrl Pts',(52.757500212918,-30.8259039490941,3.3612302805846));
#252496=CARTESIAN_POINT('Ctrl Pts',(52.8208099140591,-30.7160792752576,
3.36099641108556));
#252497=CARTESIAN_POINT('Ctrl Pts',(52.8598573673284,-30.7386233329124,
3.23423043688372));
#252498=CARTESIAN_POINT('Ctrl Pts',(52.8313189037791,-30.8682695960174,
3.41054258905263));
#252499=CARTESIAN_POINT('Ctrl Pts',(52.8948168809884,-30.7588072175341,
3.41008815826004));
#252500=CARTESIAN_POINT('Ctrl Pts',(52.9704188493355,-30.8024560343112,
3.30819867304305));
#252501=CARTESIAN_POINT('Ctrl Pts',(52.870221513222,-30.8905967158728,3.48823028058462));
#252502=CARTESIAN_POINT('Ctrl Pts',(52.93386191798,-30.7813498801524,3.48794691941578));
#252503=CARTESIAN_POINT('Ctrl Pts',(53.028685606085,-30.8360963620053,3.42473028058463));
#252504=CARTESIAN_POINT('Origin',(52.6794317578291,-30.7811015270735,3.23423028058461));
#252505=CARTESIAN_POINT('Ctrl Pts',(51.3398895692701,-30.007053683815,3.47153072139051));
#252506=CARTESIAN_POINT('Ctrl Pts',(51.4036173326914,-29.897644576157,3.47122746285057));
#252507=CARTESIAN_POINT('Ctrl Pts',(51.4965132298824,-29.9514963916944,
3.40413046676775));
#252508=CARTESIAN_POINT('Ctrl Pts',(51.4394048060587,-30.0646513737697,
3.65553813457968));
#252509=CARTESIAN_POINT('Ctrl Pts',(51.5030523579664,-29.9550530981058,
3.65520336072045));
#252510=CARTESIAN_POINT('Ctrl Pts',(51.5761456730037,-29.9974722043263,
3.55128134519916));
#252511=CARTESIAN_POINT('Ctrl Pts',(51.6181806476918,-30.1681227811162,
3.77003198860243));
#252512=CARTESIAN_POINT('Ctrl Pts',(51.6818259279743,-30.0582674911749,
3.76980209314072));
#252513=CARTESIAN_POINT('Ctrl Pts',(51.7192017762861,-30.0800656843512,
3.64284195387399));
#252514=CARTESIAN_POINT('Ctrl Pts',(51.805970313195,-30.2768083268872,3.77003198860243));
#252515=CARTESIAN_POINT('Ctrl Pts',(51.8695654317176,-30.1666583504928,
3.77003198860243));
#252516=CARTESIAN_POINT('Ctrl Pts',(51.8694702420612,-30.166823223814,3.64284189403797));
#252517=CARTESIAN_POINT('Origin',(51.805970313195,-30.2768083268872,3.64303198860243));
#252518=CARTESIAN_POINT('Origin',(45.3776875000007,-26.5654375142626,3.23423028058464));
#252519=CARTESIAN_POINT('Origin',(52.5484816883963,-30.7054974692361,3.23423028058461));
#252520=CARTESIAN_POINT('Origin',(45.2006711678738,-26.4632370872581,3.64303198860245));
#252521=CARTESIAN_POINT('Origin',(52.1535342613181,-30.4775331296731,3.64299171721757));
#252522=CARTESIAN_POINT('Ctrl Pts',(52.3576880233166,-30.596008831256,3.48823028058461));
#252523=CARTESIAN_POINT('Ctrl Pts',(52.421911104956,-30.4857749404412,3.48852004212238));
#252524=CARTESIAN_POINT('Ctrl Pts',(52.3262277788845,-30.4305321463768,
3.42473028058461));
#252525=CARTESIAN_POINT('Ctrl Pts',(52.3967235457363,-30.6184089696608,
3.41028005848386));
#252526=CARTESIAN_POINT('Ctrl Pts',(52.4606806140205,-30.5081585269362,
3.41074404220357));
#252527=CARTESIAN_POINT('Ctrl Pts',(52.3846914485018,-30.4642861617681,
3.30780486243881));
#252528=CARTESIAN_POINT('Ctrl Pts',(52.4706758922786,-30.6608464521619,
3.3612302805846));
#252529=CARTESIAN_POINT('Ctrl Pts',(52.5342179826651,-30.5506153465188,
3.36146460586421));
#252530=CARTESIAN_POINT('Ctrl Pts',(52.4954499175227,-30.5282325936724,
3.23423045308408));
#252531=CARTESIAN_POINT('Ctrl Pts',(52.5484816883963,-30.7054974692361,
3.36123028058461));
#252532=CARTESIAN_POINT('Ctrl Pts',(52.6119816883963,-30.5955122429554,
3.36123028058461));
#252533=CARTESIAN_POINT('Ctrl Pts',(52.6119816883963,-30.5955122429554,
3.23423028058461));
#252534=CARTESIAN_POINT('Origin',(52.2627277788845,-30.5405173726574,3.42473028058461));
#252535=CARTESIAN_POINT('Origin',(52.1922763809705,-30.499842239456,3.56563113524742));
#252536=CARTESIAN_POINT('Origin',(56.2428239377254,-24.6933715417288,3.56647653909471));
#252537=CARTESIAN_POINT('Origin',(56.2832472948485,-24.7113125977914,3.64299466007753));
#252538=CARTESIAN_POINT('Origin',(56.1680608984281,-24.6600848917102,3.42473028058467));
#252539=CARTESIAN_POINT('Ctrl Pts',(56.0673542004329,-24.6158705164585,
3.48823028058467));
#252540=CARTESIAN_POINT('Ctrl Pts',(56.0163785451201,-24.7315703643327,
3.48794691941584));
#252541=CARTESIAN_POINT('Ctrl Pts',(56.1164053447575,-24.7761051648309,
3.42473028058468));
#252542=CARTESIAN_POINT('Ctrl Pts',(56.0262864882909,-24.5974591883322,
3.41028005925072));
#252543=CARTESIAN_POINT('Ctrl Pts',(55.9750519161938,-24.7131705636673,
3.40982512231105));
#252544=CARTESIAN_POINT('Ctrl Pts',(56.0547337128485,-24.7486471852352,
3.30780486372883));
#252545=CARTESIAN_POINT('Ctrl Pts',(55.948484081967,-24.5625784858803,3.36123028058465));
#252546=CARTESIAN_POINT('Ctrl Pts',(55.8968463240332,-24.6783511906867,
3.36099721048324));
#252547=CARTESIAN_POINT('Ctrl Pts',(55.9378977967854,-24.6966284839296,
3.23423045308358));
#252548=CARTESIAN_POINT('Ctrl Pts',(55.8666273273836,-24.5258780191662,
3.36123028058465));
#252549=CARTESIAN_POINT('Ctrl Pts',(55.814971773713,-24.6418982922869,3.36123028058465));
#252550=CARTESIAN_POINT('Ctrl Pts',(55.814971773713,-24.6418982922869,3.23423028058465));
#252551=CARTESIAN_POINT('Origin',(55.8666273273836,-24.5258780191662,3.23423028058465));
#252552=CARTESIAN_POINT('Origin',(0.129138884176568,0.290050682801711,3.64303198860263));
#252553=CARTESIAN_POINT('Origin',(56.6498810128385,-24.8746050278044,3.64303198860246));
#252554=CARTESIAN_POINT('Origin',(0.129138884176569,0.290050682801714,3.23423028058482));
#252555=CARTESIAN_POINT('Origin',(55.7284918401501,-24.4643761377908,3.23423028058465));
#252556=CARTESIAN_POINT('Ctrl Pts',(57.1420619865024,-25.0931373005737,
3.47153072139055));
#252557=CARTESIAN_POINT('Ctrl Pts',(57.0905332211013,-25.2100238766573,
3.47182327902645));
#252558=CARTESIAN_POINT('Ctrl Pts',(56.9916465525425,-25.1657875015256,
3.40413028959015));
#252559=CARTESIAN_POINT('Ctrl Pts',(57.0369738651809,-25.0464764504209,
3.6555380712094));
#252560=CARTESIAN_POINT('Ctrl Pts',(56.9853474458565,-25.1631918674164,
3.65586275496893));
#252561=CARTESIAN_POINT('Ctrl Pts',(56.9076448051899,-25.12838751413,3.55128126837223));
#252562=CARTESIAN_POINT('Ctrl Pts',(56.8481865914866,-24.9626525995187,
3.77003198860246));
#252563=CARTESIAN_POINT('Ctrl Pts',(56.7965331449348,-25.0791258042758,
3.77025505748516));
#252564=CARTESIAN_POINT('Ctrl Pts',(56.7567390814043,-25.0611999573791,
3.64284211731155));
#252565=CARTESIAN_POINT('Ctrl Pts',(56.6498810128385,-24.8746050278044,
3.77003198860247));
#252566=CARTESIAN_POINT('Ctrl Pts',(56.598148288166,-24.9907986298331,3.77003198860246));
#252567=CARTESIAN_POINT('Ctrl Pts',(56.5982255167268,-24.9906251716456,
3.64284239821691));
#252568=CARTESIAN_POINT('Origin',(57.0434492461382,-25.0498328948956,3.40423097483293));
#252569=CARTESIAN_POINT('Ctrl Pts',(55.7284918401501,-24.4643761377908,
3.36123028058465));
#252570=CARTESIAN_POINT('Ctrl Pts',(55.6768362864795,-24.5803964109114,
3.36123028058465));
#252571=CARTESIAN_POINT('Ctrl Pts',(55.6768362864795,-24.5803964109114,
3.23423028058465));
#252572=CARTESIAN_POINT('Ctrl Pts',(55.6463586582049,-24.427551097299,3.36123028058465));
#252573=CARTESIAN_POINT('Ctrl Pts',(55.5945285148506,-24.5437506299597,
3.3614653861003));
#252574=CARTESIAN_POINT('Ctrl Pts',(55.5534947903272,-24.5254812387356,
3.23423043688401));
#252575=CARTESIAN_POINT('Ctrl Pts',(55.5686962576401,-24.3927285408613,
3.41054258693087));
#252576=CARTESIAN_POINT('Ctrl Pts',(55.5170953257145,-24.5092751529617,
3.41100608859777));
#252577=CARTESIAN_POINT('Ctrl Pts',(55.4368666119039,-24.4735550281863,
3.30819866970782));
#252578=CARTESIAN_POINT('Ctrl Pts',(55.5277679687686,-24.3743766270205,
3.48823028058464));
#252579=CARTESIAN_POINT('Ctrl Pts',(55.4763362579878,-24.4911280468217,
3.48852004212242));
#252580=CARTESIAN_POINT('Ctrl Pts',(55.3754026508178,-24.446189509598,3.42473028058464));
#252581=CARTESIAN_POINT('Origin',(55.4270582044884,-24.3301692364774,3.42473028058465));
#252582=CARTESIAN_POINT('Origin',(57.2061965577156,-25.1222926664934,3.11913648178368));
#252583=CARTESIAN_POINT('Origin',(57.3689438691199,-25.1947524379607,2.83404198860245));
#252584=CARTESIAN_POINT('Origin',(55.3527410366456,-24.2970811015507,3.56563113460828));
#252585=CARTESIAN_POINT('Origin',(55.3119205422648,-24.2788510342438,3.64299171721779));
#252586=CARTESIAN_POINT('Ctrl Pts',(57.5176823163891,-25.5918112338785,
2.59908173516006));
#252587=CARTESIAN_POINT('Ctrl Pts',(57.4835989537481,-25.5766462455167,
2.65878198860245));
#252588=CARTESIAN_POINT('Ctrl Pts',(57.4192809246792,-25.548028700571,2.65878198860245));
#252589=CARTESIAN_POINT('Ctrl Pts',(57.5535024391265,-25.5113050800553,
2.59908193475448));
#252590=CARTESIAN_POINT('Ctrl Pts',(57.5096879712795,-25.5180031505018,
2.65878715325302));
#252591=CARTESIAN_POINT('Ctrl Pts',(57.4400067642838,-25.5014249500142,
2.65878198860245));
#252592=CARTESIAN_POINT('Ctrl Pts',(57.5636994104965,-25.4268488592806,
2.63878778849858));
#252593=CARTESIAN_POINT('Ctrl Pts',(57.5125855880062,-25.4545932086363,
2.69564460180114));
#252594=CARTESIAN_POINT('Ctrl Pts',(57.4362769714773,-25.4482497003375,
2.68180481624879));
#252595=CARTESIAN_POINT('Ctrl Pts',(57.5406963524572,-25.2998561687908,
2.75443238878624));
#252596=CARTESIAN_POINT('Ctrl Pts',(57.4828507843371,-25.3719956870763,
2.79268340777054));
#252597=CARTESIAN_POINT('Ctrl Pts',(57.395003842335,-25.362293968364,2.7488592683558));
#252598=CARTESIAN_POINT('Ctrl Pts',(57.5090991591925,-25.2565567136854,
2.82856655361656));
#252599=CARTESIAN_POINT('Ctrl Pts',(57.449548243422,-25.3528760603466,2.85384197230804));
#252600=CARTESIAN_POINT('Ctrl Pts',(57.3588307079382,-25.3292685758738,
2.79184624278452));
#252601=CARTESIAN_POINT('Ctrl Pts',(57.4675553545144,-25.2380597013421,
2.90134173516007));
#252602=CARTESIAN_POINT('Ctrl Pts',(57.4161024530847,-25.3547675996707,
2.90163218716375));
#252603=CARTESIAN_POINT('Ctrl Pts',(57.3172883154493,-25.3107727110814,
2.83404198860245));
#252604=CARTESIAN_POINT('Origin',(57.4192809246792,-25.548028700571,2.53178198860245));
#252605=CARTESIAN_POINT('Origin',(0.129138884176568,0.290050682801711,3.64303198860263));
#252606=CARTESIAN_POINT('Origin',(54.9452378026832,-24.1156489724268,3.64303198860246));
#252607=CARTESIAN_POINT('Origin',(5.51404277916147E-15,1.85949616800731E-13,
2.53178198860262));
#252608=CARTESIAN_POINT('Origin',(57.4068835917983,-25.5758735661199,2.53178198860245));
#252609=CARTESIAN_POINT('Ctrl Pts',(54.9452378026832,-24.1156489724268,
3.77003198860247));
#252610=CARTESIAN_POINT('Ctrl Pts',(54.8935048666605,-24.2318430491558,
3.77003198860247));
#252611=CARTESIAN_POINT('Ctrl Pts',(54.8935823068869,-24.2316691155595,
3.64284187937011));
#252612=CARTESIAN_POINT('Ctrl Pts',(54.7469262747042,-24.0276063358784,
3.77003198860247));
#252613=CARTESIAN_POINT('Ctrl Pts',(54.6954612380244,-24.1436677818705,
3.76980208962837));
#252614=CARTESIAN_POINT('Ctrl Pts',(54.7350659388075,-24.161093081681,3.64284193928309));
#252615=CARTESIAN_POINT('Ctrl Pts',(54.5581358350803,-23.9437932708517,
3.65553535416566));
#252616=CARTESIAN_POINT('Ctrl Pts',(54.5068800556933,-24.0597054841975,
3.65520057834521));
#252617=CARTESIAN_POINT('Ctrl Pts',(54.5841613379362,-24.0939060248988,
3.5512791096418));
#252618=CARTESIAN_POINT('Ctrl Pts',(54.4530463244696,-23.897139530776,3.47153072139058));
#252619=CARTESIAN_POINT('Ctrl Pts',(54.4019907306521,-24.013005447697,3.47122746281568));
#252620=CARTESIAN_POINT('Ctrl Pts',(54.5001606201974,-24.0565064959263,
3.40413045901248));
#252621=CARTESIAN_POINT('Origin',(54.5516691663898,-23.9404209259113,3.40423097483294));
#252622=CARTESIAN_POINT('Ctrl Pts',(57.2088336324702,-25.8191582032612,
2.90134173516006));
#252623=CARTESIAN_POINT('Ctrl Pts',(57.2611357920728,-25.7028284190325,
2.90163218716374));
#252624=CARTESIAN_POINT('Ctrl Pts',(57.1623216544374,-25.6588335304432,
2.83404198860244));
#252625=CARTESIAN_POINT('Ctrl Pts',(57.2503966981986,-25.8376627381925,
2.82853349835341));
#252626=CARTESIAN_POINT('Ctrl Pts',(57.2821216226329,-25.7289639953169,
2.85381483162237));
#252627=CARTESIAN_POINT('Ctrl Pts',(57.2038829761265,-25.6773378230585,
2.79182701594191));
#252628=CARTESIAN_POINT('Ctrl Pts',(57.3035546548416,-25.8320911970508,
2.75468822073622));
#252629=CARTESIAN_POINT('Ctrl Pts',(57.3185262575352,-25.7407897001096,
2.79286913083823));
#252630=CARTESIAN_POINT('Ctrl Pts',(57.2524664994805,-25.6820441386708,
2.74900763297889));
#252631=CARTESIAN_POINT('Ctrl Pts',(57.4126476234253,-25.7649464042475,
2.63954450640378));
#252632=CARTESIAN_POINT('Ctrl Pts',(57.3992776612637,-25.7081127933379,
2.69627684028836));
#252633=CARTESIAN_POINT('Ctrl Pts',(57.3434500727661,-25.655572017978,2.6822435603648));
#252634=CARTESIAN_POINT('Ctrl Pts',(57.4692856961539,-25.7004590346995,
2.59908178706388));
#252635=CARTESIAN_POINT('Ctrl Pts',(57.4449640631521,-25.6633754510781,
2.65878704321472));
#252636=CARTESIAN_POINT('Ctrl Pts',(57.3860499078766,-25.6226140882763,
2.65878198860245));
#252637=CARTESIAN_POINT('Ctrl Pts',(57.5052637377735,-25.6197038181289,
2.59908173516006));
#252638=CARTESIAN_POINT('Ctrl Pts',(57.4711877340332,-25.6045223014053,
2.65878198860245));
#252639=CARTESIAN_POINT('Ctrl Pts',(57.4068835917983,-25.5758735661199,
2.65878198860245));
#252640=CARTESIAN_POINT('Origin',(57.1106661007668,-25.7748538035638,2.83404198860243));
#252641=CARTESIAN_POINT('Origin',(54.3889216310736,-23.8679610547589,3.11913648167135));
#252642=CARTESIAN_POINT('Origin',(54.2261740956469,-23.79550118349,2.83404198860246));
#252643=CARTESIAN_POINT('Origin',(56.9479187893679,-25.7023940320471,3.11913648177421));
#252644=CARTESIAN_POINT('Origin',(56.7851714777851,-25.6299342604987,3.40423097483294));
#252645=CARTESIAN_POINT('Ctrl Pts',(54.1275498658877,-23.7522229508819,
2.90134173516007));
#252646=CARTESIAN_POINT('Ctrl Pts',(54.0765745253539,-23.867913970856,2.90103711553213));
#252647=CARTESIAN_POINT('Ctrl Pts',(54.1745185419763,-23.9115214566106,
2.83404198860246));
#252648=CARTESIAN_POINT('Ctrl Pts',(54.0860417646978,-23.7337429357604,
2.82862991747948));
#252649=CARTESIAN_POINT('Ctrl Pts',(54.0553388636012,-23.8418262755861,
2.85314045886458));
#252650=CARTESIAN_POINT('Ctrl Pts',(54.1330089371354,-23.8930401898196,
2.79187960999956));
#252651=CARTESIAN_POINT('Ctrl Pts',(54.0331737207071,-23.7393098712341,
2.75470625793307));
#252652=CARTESIAN_POINT('Ctrl Pts',(54.0188467943739,-23.8301926567292,
2.79224250381902));
#252653=CARTESIAN_POINT('Ctrl Pts',(54.0846755205374,-23.8884275227215,
2.74901809108241));
#252654=CARTESIAN_POINT('Ctrl Pts',(53.924898459262,-23.8065189073815,2.63947868311686));
#252655=CARTESIAN_POINT('Ctrl Pts',(53.9384511174164,-23.8631501047892,
2.69595066767885));
#252656=CARTESIAN_POINT('Ctrl Pts',(53.9943748351528,-23.9152668978352,
2.68220539436047));
#252657=CARTESIAN_POINT('Ctrl Pts',(53.8688190939462,-23.8710081209819,
2.59908178585057));
#252658=CARTESIAN_POINT('Ctrl Pts',(53.8932068550021,-23.9079567336553,
2.65877670944882));
#252659=CARTESIAN_POINT('Ctrl Pts',(53.9522270531172,-23.9484663513835,
2.65878198860246));
#252660=CARTESIAN_POINT('Ctrl Pts',(53.8330634946841,-23.9513722670356,
2.59908173516008));
#252661=CARTESIAN_POINT('Ctrl Pts',(53.8671470951733,-23.9665367208216,
2.65878198860246));
#252662=CARTESIAN_POINT('Ctrl Pts',(53.9314655730807,-23.9951532569799,
2.65878198860246));
#252663=CARTESIAN_POINT('Origin',(53.9314655730807,-23.9951532569799,2.53178198860246));
#252664=CARTESIAN_POINT('Ctrl Pts',(56.3916032444854,-25.4547063934074,
3.77003198860246));
#252665=CARTESIAN_POINT('Ctrl Pts',(56.4433359736148,-25.3385127813683,
3.77003198860246));
#252666=CARTESIAN_POINT('Ctrl Pts',(56.4432587405904,-25.3386862495811,
3.64284238727551));
#252667=CARTESIAN_POINT('Ctrl Pts',(56.5897307565554,-25.5431622092796,
3.77003198860246));
#252668=CARTESIAN_POINT('Ctrl Pts',(56.6417243268775,-25.4268404215536,
3.77025506105722));
#252669=CARTESIAN_POINT('Ctrl Pts',(56.6017747680082,-25.4092621323401,
3.64284210641832));
#252670=CARTESIAN_POINT('Ctrl Pts',(56.7783458705709,-25.6273687254308,
3.65553527987814));
#252671=CARTESIAN_POINT('Ctrl Pts',(56.8305375176153,-25.5109049500375,
3.65585996533227));
#252672=CARTESIAN_POINT('Ctrl Pts',(56.7526792962317,-25.4764491573039,
3.55127902710219));
#252673=CARTESIAN_POINT('Ctrl Pts',(56.8833377255397,-25.6742415049971,
3.47153072139053));
#252674=CARTESIAN_POINT('Ctrl Pts',(56.9357219102091,-25.5577357740369,
3.4718232790517));
#252675=CARTESIAN_POINT('Ctrl Pts',(56.8366797674141,-25.5138485767956,
3.40413028377953));
#252676=CARTESIAN_POINT('Origin',(56.3916032444854,-25.4547063934074,3.64303198860246));
#252677=CARTESIAN_POINT('Origin',(5.71826297912856E-15,1.86300868799497E-13,
2.53178198860262));
#252678=CARTESIAN_POINT('Origin',(53.9190682401998,-24.0229981225288,2.53178198860246));
#252679=CARTESIAN_POINT('Origin',(51.7995637473369,-23.4101986852072,3.64303198860247));
#252680=CARTESIAN_POINT('Origin',(56.0249274780508,-25.2915084057469,3.64299466007761));
#252681=CARTESIAN_POINT('Ctrl Pts',(53.8206887816839,-23.9791663275005,
2.59908173516008));
#252682=CARTESIAN_POINT('Ctrl Pts',(53.8547645473084,-23.9943483786809,
2.65878198860246));
#252683=CARTESIAN_POINT('Ctrl Pts',(53.9190682401998,-24.0229981225288,
2.65878198860246));
#252684=CARTESIAN_POINT('Ctrl Pts',(53.7850138844277,-24.0592381182992,
2.59908193199829));
#252685=CARTESIAN_POINT('Ctrl Pts',(53.828770962649,-24.0526825045776,2.65877685806568));
#252686=CARTESIAN_POINT('Ctrl Pts',(53.8983362760826,-24.0695074323258,
2.65878198860246));
#252687=CARTESIAN_POINT('Ctrl Pts',(53.7744461045709,-24.1432906710364,
2.63872492669783));
#252688=CARTESIAN_POINT('Ctrl Pts',(53.8255298669653,-24.115812828243,2.69532212015263));
#252689=CARTESIAN_POINT('Ctrl Pts',(53.901590305224,-24.1225146216889,2.6817683672662));
#252690=CARTESIAN_POINT('Ctrl Pts',(53.7968389608979,-24.2696905364164,
2.75442176402232));
#252691=CARTESIAN_POINT('Ctrl Pts',(53.8548027426704,-24.1983175571245,
2.79203179920113));
#252692=CARTESIAN_POINT('Ctrl Pts',(53.9421141528991,-24.2081897025468,
2.74885310748157));
#252693=CARTESIAN_POINT('Ctrl Pts',(53.8282518514941,-24.3127961528999,
2.82866089558383));
#252694=CARTESIAN_POINT('Ctrl Pts',(53.88802914902,-24.2176488245055,2.85316563119282));
#252695=CARTESIAN_POINT('Ctrl Pts',(53.9780599067619,-24.2411088588474,
2.79189751796672));
#252696=CARTESIAN_POINT('Ctrl Pts',(53.8697418420148,-24.331269253108,2.90134173516007));
#252697=CARTESIAN_POINT('Ctrl Pts',(53.921607864342,-24.2159747902178,2.90103711553213));
#252698=CARTESIAN_POINT('Ctrl Pts',(54.0195518809644,-24.2595822759724,
2.83404198860245));
#252699=CARTESIAN_POINT('Origin',(53.9678963272938,-24.3756025490931,2.83404198860246));
#252700=CARTESIAN_POINT('Origin',(55.9845461685093,-25.2734729066188,3.56647653971734));
#252701=CARTESIAN_POINT('Origin',(55.909783130075,-25.2401862573133,3.42473028058468));
#252702=CARTESIAN_POINT('Origin',(54.1306438627319,-24.4480624203046,3.11913648167937));
#252703=CARTESIAN_POINT('Origin',(54.2933913980367,-24.5205222915143,3.40423097483294));
#252704=CARTESIAN_POINT('Ctrl Pts',(55.6083495590305,-25.1059793847693,
3.36123028058464));
#252705=CARTESIAN_POINT('Ctrl Pts',(55.6600051127011,-24.9899591116487,
3.36123028058465));
#252706=CARTESIAN_POINT('Ctrl Pts',(55.6600051127011,-24.9899591116487,
3.23423028058464));
#252707=CARTESIAN_POINT('Ctrl Pts',(55.6906734752784,-25.1423759987942,
3.36123028058464));
#252708=CARTESIAN_POINT('Ctrl Pts',(55.7421565548644,-25.0265352902396,
3.36099641108402));
#252709=CARTESIAN_POINT('Ctrl Pts',(55.783346597804,-25.044874278905,3.23423043688411));
#252710=CARTESIAN_POINT('Ctrl Pts',(55.7685161955956,-25.1767934079542,
3.41054258905266));
#252711=CARTESIAN_POINT('Ctrl Pts',(55.8202243900373,-25.0612933298588,
3.41008815825996));
#252712=CARTESIAN_POINT('Ctrl Pts',(55.8999747466293,-25.0968004762765,
3.3081986730426));
#252713=CARTESIAN_POINT('Ctrl Pts',(55.809539512001,-25.1949317875292,3.48823028058467));
#252714=CARTESIAN_POINT('Ctrl Pts',(55.8614118841082,-25.0796311836945,
3.48794691941583));
#252715=CARTESIAN_POINT('Ctrl Pts',(55.9614386837456,-25.1241659841927,
3.42473028058468));
#252716=CARTESIAN_POINT('Origin',(55.6083495590305,-25.1059793847693,3.23423028058464));
#252717=CARTESIAN_POINT('Ctrl Pts',(54.1952354911875,-24.4761921430384,
3.47153072139056));
#252718=CARTESIAN_POINT('Ctrl Pts',(54.247177781362,-24.3607210247417,3.4712274628506));
#252719=CARTESIAN_POINT('Ctrl Pts',(54.3451938326307,-24.404567569022,3.40413046676767));
#252720=CARTESIAN_POINT('Ctrl Pts',(54.3002261711144,-24.5230721320496,
3.6555381345797));
#252721=CARTESIAN_POINT('Ctrl Pts',(54.3520689157398,-24.4074212664147,
3.65520336071996));
#252722=CARTESIAN_POINT('Ctrl Pts',(54.429195821938,-24.4419676644359,3.55128134519888));
#252723=CARTESIAN_POINT('Ctrl Pts',(54.4888383671849,-24.607289548202,3.77003198860246));
#252724=CARTESIAN_POINT('Ctrl Pts',(54.5406519873245,-24.4913833136915,
3.76980209314211));
#252725=CARTESIAN_POINT('Ctrl Pts',(54.5801016184618,-24.5091552540984,
3.64284195387413));
#252726=CARTESIAN_POINT('Ctrl Pts',(54.68696003433,-24.6957503380299,3.77003198860247));
#252727=CARTESIAN_POINT('Ctrl Pts',(54.7386929643779,-24.5795562747206,
3.77003198860246));
#252728=CARTESIAN_POINT('Ctrl Pts',(54.7386155301352,-24.5797301948772,
3.64284189403778));
#252729=CARTESIAN_POINT('Origin',(54.68696003433,-24.6957503380299,3.64303198860247));
#252730=CARTESIAN_POINT('Origin',(50.5417021396889,-22.850162615334,3.23423028058466));
#252731=CARTESIAN_POINT('Origin',(55.470214071797,-25.0444775033939,3.23423028058464));
#252732=CARTESIAN_POINT('Origin',(50.3447265545032,-22.7624634345039,3.64303198860247));
#252733=CARTESIAN_POINT('Origin',(55.0536014459536,-24.8590452239597,3.64299171721713));
#252734=CARTESIAN_POINT('Ctrl Pts',(55.2690209153043,-24.9555320242407,
3.48823028058464));
#252735=CARTESIAN_POINT('Ctrl Pts',(55.3213695969759,-24.8391888661836,
3.48852004212242));
#252736=CARTESIAN_POINT('Ctrl Pts',(55.2204359898059,-24.7942503289599,
3.42473028058464));
#252737=CARTESIAN_POINT('Ctrl Pts',(55.3101840490924,-24.9737291291718,
3.41028005848391));
#252738=CARTESIAN_POINT('Ctrl Pts',(55.3622664445107,-24.8573973158451,
3.41074404220333));
#252739=CARTESIAN_POINT('Ctrl Pts',(55.2821076446827,-24.8217083187814,
3.30780486243885));
#252740=CARTESIAN_POINT('Ctrl Pts',(55.3881672017731,-25.0082040095651,
3.36123028058464));
#252741=CARTESIAN_POINT('Ctrl Pts',(55.4398389138644,-24.8919348043903,
3.36146460586422));
#252742=CARTESIAN_POINT('Ctrl Pts',(55.3989435894784,-24.8737270328796,
3.23423045308444));
#252743=CARTESIAN_POINT('Ctrl Pts',(55.470214071797,-25.0444775033939,3.36123028058464));
#252744=CARTESIAN_POINT('Ctrl Pts',(55.5218696254676,-24.9284572302733,
3.36123028058465));
#252745=CARTESIAN_POINT('Ctrl Pts',(55.5218696254676,-24.9284572302733,
3.23423028058464));
#252746=CARTESIAN_POINT('Origin',(55.1687804361353,-24.9102706020805,3.42473028058464));
#252747=CARTESIAN_POINT('Origin',(55.0944632691836,-24.8771824678734,3.56563113524731));
#252748=CARTESIAN_POINT('Origin',(58.5158800435648,-18.6791227126686,3.56647653909498));
#252749=CARTESIAN_POINT('Origin',(58.5579573083276,-18.6927400943491,3.64299466007739));
#252750=CARTESIAN_POINT('Origin',(58.4380471616457,-18.6538332760095,3.42473028058472));
#252751=CARTESIAN_POINT('Ctrl Pts',(58.3332704847798,-18.6203878281138,
3.48823028058472));
#252752=CARTESIAN_POINT('Ctrl Pts',(58.2946680067391,-18.7407822670293,
3.48794691941588));
#252753=CARTESIAN_POINT('Ctrl Pts',(58.3988020033601,-18.774617453579,3.42473028058473));
#252754=CARTESIAN_POINT('Ctrl Pts',(58.2905032380258,-18.6063701040103,
3.41028005925071));
#252755=CARTESIAN_POINT('Ctrl Pts',(58.2516444665228,-18.7268030714126,
3.40982512231002));
#252756=CARTESIAN_POINT('Ctrl Pts',(58.3345980746932,-18.7537563325796,
3.30780486372849));
#252757=CARTESIAN_POINT('Ctrl Pts',(58.2094810151999,-18.5798130476665,
3.36123028058469));
#252758=CARTESIAN_POINT('Ctrl Pts',(58.170227677228,-18.7003491529652,3.36099721048435));
#252759=CARTESIAN_POINT('Ctrl Pts',(58.2129647630923,-18.7142352739224,
3.23423045308368));
#252760=CARTESIAN_POINT('Ctrl Pts',(58.1242364370959,-18.5518699907141,
3.36123028058469));
#252761=CARTESIAN_POINT('Ctrl Pts',(58.0849912788103,-18.6726541682836,
3.36123028058469));
#252762=CARTESIAN_POINT('Ctrl Pts',(58.0849912788103,-18.6726541682836,
3.23423028058469));
#252763=CARTESIAN_POINT('Origin',(58.1242364370959,-18.5518699907141,3.23423028058469));
#252764=CARTESIAN_POINT('Origin',(0.0981128957140474,0.301960443923896,
3.64303198860263));
#252765=CARTESIAN_POINT('Origin',(58.9396512752216,-18.8168143322217,3.6430319886025));
#252766=CARTESIAN_POINT('Origin',(0.0981128957140474,0.301960443923899,
3.23423028058482));
#252767=CARTESIAN_POINT('Origin',(57.9804289733666,-18.5051441132832,3.23423028058469));
#252768=CARTESIAN_POINT('Ctrl Pts',(59.451978872661,-18.9827025415087,3.47153072139059));
#252769=CARTESIAN_POINT('Ctrl Pts',(59.4129503614029,-19.1043350233598,
3.47182327902649));
#252770=CARTESIAN_POINT('Ctrl Pts',(59.3099814440481,-19.0706774512219,
3.40413028959026));
#252771=CARTESIAN_POINT('Ctrl Pts',(59.3425890481019,-18.9472820042064,
3.65553807120945));
#252772=CARTESIAN_POINT('Ctrl Pts',(59.3034455268839,-19.068754472212,3.65586275496921));
#252773=CARTESIAN_POINT('Ctrl Pts',(59.2225305038479,-19.042262918433,3.55128126837209));
#252774=CARTESIAN_POINT('Ctrl Pts',(59.1460739925266,-18.8836509927319,
3.77003198860251));
#252775=CARTESIAN_POINT('Ctrl Pts',(59.1068782740635,-19.0048854004768,
3.77025505748546));
#252776=CARTESIAN_POINT('Ctrl Pts',(59.0654284453493,-18.9912173655537,
3.64284211731207));
#252777=CARTESIAN_POINT('Ctrl Pts',(58.9396512752216,-18.8168143322217,
3.77003198860251));
#252778=CARTESIAN_POINT('Ctrl Pts',(58.9003474864893,-18.9377789557515,
3.7700319886025));
#252779=CARTESIAN_POINT('Ctrl Pts',(58.9004061606662,-18.9375983752035,
3.64284239821709));
#252780=CARTESIAN_POINT('Origin',(59.3493798002282,-18.9499432001048,3.40423097483297));
#252781=CARTESIAN_POINT('Ctrl Pts',(57.9804289733666,-18.5051441132832,
3.36123028058469));
#252782=CARTESIAN_POINT('Ctrl Pts',(57.941183815081,-18.6259282908527,3.36123028058469));
#252783=CARTESIAN_POINT('Ctrl Pts',(57.941183815081,-18.6259282908527,3.23423028058469));
#252784=CARTESIAN_POINT('Ctrl Pts',(57.8948964606934,-18.477106059508,3.36123028058469));
#252785=CARTESIAN_POINT('Ctrl Pts',(57.8554964068672,-18.5980867642055,
3.36146538610131));
#252786=CARTESIAN_POINT('Ctrl Pts',(57.8127777979909,-18.5842066467853,
3.23423043688402));
#252787=CARTESIAN_POINT('Ctrl Pts',(57.8140195545736,-18.4505921960624,
3.41054258693088));
#252788=CARTESIAN_POINT('Ctrl Pts',(57.7748837362169,-18.5718941197448,
3.41100608859783));
#252789=CARTESIAN_POINT('Ctrl Pts',(57.6913607539435,-18.5447558577159,
3.30819866970838));
#252790=CARTESIAN_POINT('Ctrl Pts',(57.7713971777989,-18.4366189870663,
3.48823028058468));
#252791=CARTESIAN_POINT('Ctrl Pts',(57.7324510618073,-18.5581069080651,
3.48852004212246));
#252792=CARTESIAN_POINT('Ctrl Pts',(57.6273730232608,-18.5239649836999,
3.42473028058468));
#252793=CARTESIAN_POINT('Origin',(57.6666181815464,-18.4031808061304,3.42473028058467));
#252794=CARTESIAN_POINT('Origin',(59.5188096735783,-19.0049943031106,3.11913648178355));
#252795=CARTESIAN_POINT('Origin',(59.6882395467423,-19.0600454060077,2.83404198860249));
#252796=CARTESIAN_POINT('Origin',(57.5892494790284,-18.3780421908168,3.565631134608));
#252797=CARTESIAN_POINT('Origin',(57.5467470426663,-18.3641788932745,3.64299171721775));
#252798=CARTESIAN_POINT('Ctrl Pts',(59.8776671349988,-19.4393816709747,
2.5990817351601));
#252799=CARTESIAN_POINT('Ctrl Pts',(59.8421853116555,-19.4278624395257,
2.65878198860249));
#252800=CARTESIAN_POINT('Ctrl Pts',(59.7752282754839,-19.4061247292244,
2.65878198860249));
#252801=CARTESIAN_POINT('Ctrl Pts',(59.9048758468124,-19.3555723159015,
2.59908193475575));
#252802=CARTESIAN_POINT('Ctrl Pts',(59.8620015382143,-19.3668135526099,
2.65878715325339));
#252803=CARTESIAN_POINT('Ctrl Pts',(59.79096915834,-19.3576098387249,2.65878198860249));
#252804=CARTESIAN_POINT('Ctrl Pts',(59.9061888791359,-19.2705128813942,
2.63878778849882));
#252805=CARTESIAN_POINT('Ctrl Pts',(59.858255137716,-19.3034480936178,2.69564460180118));
#252806=CARTESIAN_POINT('Ctrl Pts',(59.7817014705984,-19.3051157581409,
2.68180481624877));
#252807=CARTESIAN_POINT('Ctrl Pts',(59.8700374834726,-19.1466203444573,
2.75443238878609));
#252808=CARTESIAN_POINT('Ctrl Pts',(59.8200494324143,-19.2244111832561,
2.79268340777058));
#252809=CARTESIAN_POINT('Ctrl Pts',(59.7316696194041,-19.2239451174243,
2.7488592683559));
#252810=CARTESIAN_POINT('Ctrl Pts',(59.834087357436,-19.1068608943528,2.82856655361674));
#252811=CARTESIAN_POINT('Ctrl Pts',(59.7849307811011,-19.2088773592685,
2.85384197230705));
#252812=CARTESIAN_POINT('Ctrl Pts',(59.692242551696,-19.1948817636396,2.79184624278417));
#252813=CARTESIAN_POINT('Ctrl Pts',(59.7908376697914,-19.0928077206402,
2.90134173516011));
#252814=CARTESIAN_POINT('Ctrl Pts',(59.7518659300028,-19.2142545736074,
2.90163218716379));
#252815=CARTESIAN_POINT('Ctrl Pts',(59.6489943884567,-19.1808295835772,
2.83404198860249));
#252816=CARTESIAN_POINT('Origin',(59.7752282754839,-19.4061247292244,2.53178198860248));
#252817=CARTESIAN_POINT('Origin',(0.0981128957140474,0.301960443923896,
3.64303198860263));
#252818=CARTESIAN_POINT('Origin',(57.1650137687749,-18.2401996527036,3.6430319886025));
#252819=CARTESIAN_POINT('Origin',(5.50785759597432E-15,1.85933503847647E-13,
2.53178198860262));
#252820=CARTESIAN_POINT('Origin',(59.7658094374954,-19.4351129318411,2.53178198860249));
#252821=CARTESIAN_POINT('Ctrl Pts',(57.1650137687749,-18.2401996527036,
3.77003198860251));
#252822=CARTESIAN_POINT('Ctrl Pts',(57.1257098194699,-18.3611647704256,
3.77003198860251));
#252823=CARTESIAN_POINT('Ctrl Pts',(57.1257686544592,-18.3609836949477,
3.64284187936996));
#252824=CARTESIAN_POINT('Ctrl Pts',(56.9585856505954,-18.1733685221983,
3.77003198860251));
#252825=CARTESIAN_POINT('Ctrl Pts',(56.9195342693675,-18.2941737326421,
3.76980208962942));
#252826=CARTESIAN_POINT('Ctrl Pts',(56.9607434512668,-18.307363756326,3.64284193928297));
#252827=CARTESIAN_POINT('Ctrl Pts',(56.7620685738644,-18.1097485684444,
3.65553535416572));
#252828=CARTESIAN_POINT('Ctrl Pts',(56.723209704532,-18.2303834904104,3.65520057834524));
#252829=CARTESIAN_POINT('Ctrl Pts',(56.8036425617878,-18.2563185832986,
3.55127910964233));
#252830=CARTESIAN_POINT('Ctrl Pts',(56.6526781108326,-18.0743352474882,
3.4715307213906));
#252831=CARTESIAN_POINT('Ctrl Pts',(56.6140134911409,-18.1949032015562,
3.4712274628157));
#252832=CARTESIAN_POINT('Ctrl Pts',(56.7161926934818,-18.2279043987983,
3.40413045901241));
#252833=CARTESIAN_POINT('Origin',(56.7552848242273,-18.1070706485033,3.40423097483298));
#252834=CARTESIAN_POINT('Ctrl Pts',(59.5942745858238,-19.6977666881836,
2.90134173516011));
#252835=CARTESIAN_POINT('Ctrl Pts',(59.634130455146,-19.5766071063159,2.90163218716378));
#252836=CARTESIAN_POINT('Ctrl Pts',(59.5312589135998,-19.5431821162857,
2.83404198860249));
#252837=CARTESIAN_POINT('Ctrl Pts',(59.6375442153293,-19.7118253299472,
2.82853349835334));
#252838=CARTESIAN_POINT('Ctrl Pts',(59.6577332347555,-19.6004058925603,
2.8538148316221));
#252839=CARTESIAN_POINT('Ctrl Pts',(59.5745267832902,-19.5572406993621,
2.79182701594097));
#252840=CARTESIAN_POINT('Ctrl Pts',(59.6898285824899,-19.7007277907727,
2.75468822073638));
#252841=CARTESIAN_POINT('Ctrl Pts',(59.6951745640079,-19.6083614943623,
2.79286913083837));
#252842=CARTESIAN_POINT('Ctrl Pts',(59.6233361049592,-19.5568428722491,
2.74900763297906));
#252843=CARTESIAN_POINT('Ctrl Pts',(59.7913053863693,-19.62254750381,2.63954450640372));
#252844=CARTESIAN_POINT('Ctrl Pts',(59.7720679362492,-19.5674227749664,
2.69627684028835));
#252845=CARTESIAN_POINT('Ctrl Pts',(59.7110541706152,-19.521005395505,2.68224356036472));
#252846=CARTESIAN_POINT('Ctrl Pts',(59.8408924241701,-19.5524931121154,
2.59908178706399));
#252847=CARTESIAN_POINT('Ctrl Pts',(59.8128277376106,-19.5181549791671,
2.65878704321576));
#252848=CARTESIAN_POINT('Ctrl Pts',(59.7499755976266,-19.4837751174909,
2.65878198860249));
#252849=CARTESIAN_POINT('Ctrl Pts',(59.8682321556244,-19.4684195516687,
2.5990817351601));
#252850=CARTESIAN_POINT('Ctrl Pts',(59.8327559231849,-19.4568831131874,
2.65878198860249));
#252851=CARTESIAN_POINT('Ctrl Pts',(59.7658094374954,-19.4351129318411,
2.65878198860249));
#252852=CARTESIAN_POINT('Origin',(59.4920137553142,-19.6639662938552,2.83404198860249));
#252853=CARTESIAN_POINT('Origin',(56.5858547179611,-18.0520194698708,3.11913648167016));
#252854=CARTESIAN_POINT('Origin',(56.4164246115666,-17.9969682911402,2.8340419886025));
#252855=CARTESIAN_POINT('Origin',(59.3225838821516,-19.6089151909087,3.11913648177479));
#252856=CARTESIAN_POINT('Origin',(59.1531540088002,-19.5538640879523,3.40423097483297));
#252857=CARTESIAN_POINT('Ctrl Pts',(56.3138168485097,-17.9642361803963,
2.90134173516011));
#252858=CARTESIAN_POINT('Ctrl Pts',(56.2752137607568,-18.0846218068686,
2.90103711553218));
#252859=CARTESIAN_POINT('Ctrl Pts',(56.377179453281,-18.1177524687097,2.8340419886025));
#252860=CARTESIAN_POINT('Ctrl Pts',(56.2706044454597,-17.9501961787611,
2.82862991747954));
#252861=CARTESIAN_POINT('Ctrl Pts',(56.2513675234866,-18.0608967538108,
2.85314045886436));
#252862=CARTESIAN_POINT('Ctrl Pts',(56.3339654239813,-18.1037113794367,
2.79187961000014));
#252863=CARTESIAN_POINT('Ctrl Pts',(56.2186079213555,-17.961258833375,2.75470625793309));
#252864=CARTESIAN_POINT('Ctrl Pts',(56.2138593173292,-18.0531413250546,
2.79224250381889));
#252865=CARTESIAN_POINT('Ctrl Pts',(56.2854146278936,-18.1041761987731,
2.74901809108242));
#252866=CARTESIAN_POINT('Ctrl Pts',(56.1179510603879,-18.0394175380786,
2.63947868311692));
#252867=CARTESIAN_POINT('Ctrl Pts',(56.1373490477008,-18.0943218653316,
2.69595066767899));
#252868=CARTESIAN_POINT('Ctrl Pts',(56.1984140977479,-18.140307536857,2.68220539436054));
#252869=CARTESIAN_POINT('Ctrl Pts',(56.0689198620976,-18.1094153628969,
2.59908178585011));
#252870=CARTESIAN_POINT('Ctrl Pts',(56.0970362061477,-18.1436123520177,
2.65877670944876));
#252871=CARTESIAN_POINT('Ctrl Pts',(56.1599674935302,-18.1777307632104,
2.6587819886025));
#252872=CARTESIAN_POINT('Ctrl Pts',(56.0417604764386,-18.193076743594,2.59908173516011));
#252873=CARTESIAN_POINT('Ctrl Pts',(56.0772424804487,-18.2045954185336,
2.65878198860249));
#252874=CARTESIAN_POINT('Ctrl Pts',(56.144199857553,-18.2263320786573,2.6587819886025));
#252875=CARTESIAN_POINT('Origin',(56.144199857553,-18.2263320786573,2.5317819886025));
#252876=CARTESIAN_POINT('Ctrl Pts',(58.7434254837935,-19.4207352200692,
3.7700319886025));
#252877=CARTESIAN_POINT('Ctrl Pts',(58.7827292759118,-19.2997705861182,
3.7700319886025));
#252878=CARTESIAN_POINT('Ctrl Pts',(58.7826705983438,-19.2999511771029,
3.64284238727591));
#252879=CARTESIAN_POINT('Ctrl Pts',(58.9497137831223,-19.4879965013582,
3.7700319886025));
#252880=CARTESIAN_POINT('Ctrl Pts',(58.9892635895157,-19.3668771285514,
3.77025506105836));
#252881=CARTESIAN_POINT('Ctrl Pts',(58.9476954469482,-19.3535710010431,
3.64284210641898));
#252882=CARTESIAN_POINT('Ctrl Pts',(59.1460976215392,-19.5520260773845,
3.65553527987819));
#252883=CARTESIAN_POINT('Ctrl Pts',(59.1858295778045,-19.4307447900781,
3.65585996532955));
#252884=CARTESIAN_POINT('Ctrl Pts',(59.1047962608433,-19.4046161500175,
3.55127902710157));
#252885=CARTESIAN_POINT('Ctrl Pts',(59.2554138597574,-19.5876674457069,
3.47153072139058));
#252886=CARTESIAN_POINT('Ctrl Pts',(59.2953329133628,-19.4663243070084,
3.47182327905175));
#252887=CARTESIAN_POINT('Ctrl Pts',(59.1922458725046,-19.4330302514104,
3.40413028377977));
#252888=CARTESIAN_POINT('Origin',(58.7434254837935,-19.4207352200692,3.6430319886025));
#252889=CARTESIAN_POINT('Origin',(5.72046327455653E-15,1.86306600765055E-13,
2.53178198860262));
#252890=CARTESIAN_POINT('Origin',(56.1347810195644,-18.255320281274,2.5317819886025));
#252891=CARTESIAN_POINT('Origin',(56.182627028633,-18.5886813639048,3.6430319886025));
#252892=CARTESIAN_POINT('Origin',(58.3616995707162,-19.2967593024467,3.64299466007407));
#252893=CARTESIAN_POINT('Ctrl Pts',(56.0323588238394,-18.2220120550208,
2.59908173516011));
#252894=CARTESIAN_POINT('Ctrl Pts',(56.0678348753335,-18.2335490499209,
2.6587819886025));
#252895=CARTESIAN_POINT('Ctrl Pts',(56.1347810195644,-18.255320281274,2.6587819886025));
#252896=CARTESIAN_POINT('Ctrl Pts',(56.0052491386467,-18.3053742463591,
2.59908193199903));
#252897=CARTESIAN_POINT('Ctrl Pts',(56.0480812627891,-18.2942806848325,
2.6587768580666));
#252898=CARTESIAN_POINT('Ctrl Pts',(56.1190241739986,-18.3037418885559,
2.6587819886025));
#252899=CARTESIAN_POINT('Ctrl Pts',(56.0035251343647,-18.3900709842061,
2.63872492669787));
#252900=CARTESIAN_POINT('Ctrl Pts',(56.0514568378825,-18.3574039607296,
2.69532212015265));
#252901=CARTESIAN_POINT('Ctrl Pts',(56.1278011372723,-18.3561185603232,
2.68176836726616));
#252902=CARTESIAN_POINT('Ctrl Pts',(56.0390077039671,-18.5134377270383,
2.75442176402236));
#252903=CARTESIAN_POINT('Ctrl Pts',(56.089193446234,-18.436396871361,2.79203179920119));
#252904=CARTESIAN_POINT('Ctrl Pts',(56.1770584756119,-18.4370884086007,
2.74885310748169));
#252905=CARTESIAN_POINT('Ctrl Pts',(56.0747542753112,-18.5530236652629,
2.82866089558387));
#252906=CARTESIAN_POINT('Ctrl Pts',(56.1242585025264,-18.4521491348405,
2.85316563119207));
#252907=CARTESIAN_POINT('Ctrl Pts',(56.2162483036943,-18.4660698759064,
2.79189751796673));
#252908=CARTESIAN_POINT('Ctrl Pts',(56.1179479440991,-18.5670586829457,
2.90134173516011));
#252909=CARTESIAN_POINT('Ctrl Pts',(56.1574782859,-18.446974339577,2.90103711553218));
#252910=CARTESIAN_POINT('Ctrl Pts',(56.2594439784241,-18.4801050014182,
2.83404198860249));
#252911=CARTESIAN_POINT('Origin',(56.2201988201385,-18.6008891789876,2.83404198860249));
#252912=CARTESIAN_POINT('Origin',(58.319654251203,-19.2830435998979,3.56647653971795));
#252913=CARTESIAN_POINT('Origin',(58.2418213702176,-19.2577541638569,3.42473028058473));
#252914=CARTESIAN_POINT('Origin',(56.3896289265337,-18.6559403576597,3.11913648168106));
#252915=CARTESIAN_POINT('Origin',(56.5590590327992,-18.7109915363508,3.40423097483298));
#252916=CARTESIAN_POINT('Ctrl Pts',(57.9280106456678,-19.1557908785616,
3.36123028058469));
#252917=CARTESIAN_POINT('Ctrl Pts',(57.9672558039534,-19.0350067009921,
3.36123028058469));
#252918=CARTESIAN_POINT('Ctrl Pts',(57.9672558039534,-19.0350067009921,
3.23423028058469));
#252919=CARTESIAN_POINT('Ctrl Pts',(58.0136880650216,-19.1833829156693,
3.36123028058469));
#252920=CARTESIAN_POINT('Ctrl Pts',(58.0527804636641,-19.0627953474444,
3.36099641108448));
#252921=CARTESIAN_POINT('Ctrl Pts',(58.0956618095406,-19.0767283413219,
3.23423043688424));
#252922=CARTESIAN_POINT('Ctrl Pts',(58.0947019536606,-19.2094750027314,
3.4105425890527));
#252923=CARTESIAN_POINT('Ctrl Pts',(58.1340538395294,-19.0892026680431,
3.41008815826056));
#252924=CARTESIAN_POINT('Ctrl Pts',(58.2170788227743,-19.1161791203793,
3.30819867304324));
#252925=CARTESIAN_POINT('Ctrl Pts',(58.1373965169896,-19.223225914143,3.4882302805847));
#252926=CARTESIAN_POINT('Ctrl Pts',(58.1769325318822,-19.1031347997378,
3.48794691941587));
#252927=CARTESIAN_POINT('Ctrl Pts',(58.2810665285032,-19.1369699862874,
3.42473028058472));
#252928=CARTESIAN_POINT('Origin',(57.9280106456678,-19.1557908785616,3.23423028058468));
#252929=CARTESIAN_POINT('Ctrl Pts',(56.4568070719814,-18.6771643191701,
3.4715307213906));
#252930=CARTESIAN_POINT('Ctrl Pts',(56.496394798308,-18.556896315971,3.47122746285065));
#252931=CARTESIAN_POINT('Ctrl Pts',(56.5984571192855,-18.5902571970792,
3.4041304667678));
#252932=CARTESIAN_POINT('Ctrl Pts',(56.5661228951883,-18.712812980264,3.65553813457972));
#252933=CARTESIAN_POINT('Ctrl Pts',(56.605592832572,-18.5923766197432,3.65520336071961));
#252934=CARTESIAN_POINT('Ctrl Pts',(56.6859083114068,-18.6186718120037,
3.55128134519882));
#252935=CARTESIAN_POINT('Ctrl Pts',(56.7625049710036,-18.7768537015936,
3.77003198860251));
#252936=CARTESIAN_POINT('Ctrl Pts',(56.8019192501362,-18.6561664154725,
3.76980209314348));
#252937=CARTESIAN_POINT('Ctrl Pts',(56.8430104456841,-18.6697173900107,
3.64284195387422));
#252938=CARTESIAN_POINT('Ctrl Pts',(56.9687879773469,-18.844120540551,3.77003198860251));
#252939=CARTESIAN_POINT('Ctrl Pts',(57.0080919221124,-18.7231554368001,
3.77003198860251));
#252940=CARTESIAN_POINT('Ctrl Pts',(57.0080330916694,-18.723336498286,3.64284189403798));
#252941=CARTESIAN_POINT('Origin',(56.9687879773468,-18.844120540551,3.64303198860251));
#252942=CARTESIAN_POINT('Origin',(54.8193466381482,-18.1457247135482,3.23423028058469));
#252943=CARTESIAN_POINT('Origin',(57.7842031819385,-19.1090650011306,3.23423028058468));
#252944=CARTESIAN_POINT('Origin',(54.6058629360818,-18.0763596539221,3.6430319886025));
#252945=CARTESIAN_POINT('Origin',(57.3504898524411,-18.9681964166824,3.64299171721744));
#252946=CARTESIAN_POINT('Ctrl Pts',(57.5748148483578,-19.0416371860869,
3.48823028058469));
#252947=CARTESIAN_POINT('Ctrl Pts',(57.6147155869504,-18.9204594407736,
3.48852004212247));
#252948=CARTESIAN_POINT('Ctrl Pts',(57.5096375484039,-18.8863175164083,
3.42473028058469));
#252949=CARTESIAN_POINT('Ctrl Pts',(57.617654601607,-19.0554318862532,3.41028005848393));
#252950=CARTESIAN_POINT('Ctrl Pts',(57.6572916985368,-18.9342932580147,
3.41074404220321));
#252951=CARTESIAN_POINT('Ctrl Pts',(57.5738415009809,-18.9071786451766,
3.30780486243826));
#252952=CARTESIAN_POINT('Ctrl Pts',(57.6988141606862,-19.0815664505351,
3.36123028058469));
#252953=CARTESIAN_POINT('Ctrl Pts',(57.7380493683904,-18.9605330155737,
3.36146460586412));
#252954=CARTESIAN_POINT('Ctrl Pts',(57.6954748424956,-18.9466997135533,
3.2342304530846));
#252955=CARTESIAN_POINT('Ctrl Pts',(57.7842031819385,-19.1090650011306,
3.36123028058469));
#252956=CARTESIAN_POINT('Ctrl Pts',(57.8234483402241,-18.9882808235611,
3.36123028058469));
#252957=CARTESIAN_POINT('Ctrl Pts',(57.8234483402241,-18.9882808235611,
3.23423028058469));
#252958=CARTESIAN_POINT('Origin',(57.4703923901183,-19.0071016939778,3.42473028058468));
#252959=CARTESIAN_POINT('Origin',(57.393023688562,-18.9819630792874,3.56563113524724));
#252960=CARTESIAN_POINT('Origin',(60.1478239224126,-12.4602215063111,3.56647653909461));
#252961=CARTESIAN_POINT('Origin',(60.1910940874961,-12.4693660187264,3.64299466007801));
#252962=CARTESIAN_POINT('Origin',(60.0677739512127,-12.4432063593713,3.42473028058476));
#252963=CARTESIAN_POINT('Ctrl Pts',(59.9600752506739,-12.4208962741577,
3.48823028058476));
#252964=CARTESIAN_POINT('Ctrl Pts',(59.9342688867327,-12.5446662374477,
3.48794691941592));
#252965=CARTESIAN_POINT('Ctrl Pts',(60.0413691664789,-12.5674311046645,
3.42473028058477));
#252966=CARTESIAN_POINT('Ctrl Pts',(59.9160770362136,-12.4114257351938,
3.4102800592508));
#252967=CARTESIAN_POINT('Ctrl Pts',(59.8900198101331,-12.5352608058688,
3.4098251223104));
#252968=CARTESIAN_POINT('Ctrl Pts',(59.9753363727289,-12.5533954010675,
3.30780486372877));
#252969=CARTESIAN_POINT('Ctrl Pts',(59.832722693313,-12.3934832896264,3.36123028058473));
#252970=CARTESIAN_POINT('Ctrl Pts',(59.8062838430907,-12.5174621766265,
3.36099721048495));
#252971=CARTESIAN_POINT('Ctrl Pts',(59.8502383056108,-12.5268049860493,
3.2342304530841));
#252972=CARTESIAN_POINT('Ctrl Pts',(59.7450242491249,-12.3746037924155,
3.36123028058473));
#252973=CARTESIAN_POINT('Ctrl Pts',(59.7186194643911,-12.4988285377087,
3.36123028058473));
#252974=CARTESIAN_POINT('Ctrl Pts',(59.7186194643911,-12.4988285377087,
3.23423028058473));
#252975=CARTESIAN_POINT('Origin',(59.7450242491249,-12.3746037924155,3.23423028058473));
#252976=CARTESIAN_POINT('Origin',(0.0660119618346401,0.310561863233168,
3.64303198860263));
#252977=CARTESIAN_POINT('Origin',(60.5836663843183,-12.5528626811438,3.64303198860255));
#252978=CARTESIAN_POINT('Origin',(0.0660119618346402,0.310561863233171,
3.23423028058482));
#252979=CARTESIAN_POINT('Origin',(59.5971203935661,-12.3431658574201,3.23423028058473));
#252980=CARTESIAN_POINT('Ctrl Pts',(61.1105274371643,-12.6642893210132,
3.47153072139064));
#252981=CARTESIAN_POINT('Ctrl Pts',(61.0844267845858,-12.7893350777074,
3.47182327902655));
#252982=CARTESIAN_POINT('Ctrl Pts',(60.9785037674413,-12.7666250679668,
3.40413028959037));
#252983=CARTESIAN_POINT('Ctrl Pts',(60.9980344071775,-12.6404971713779,
3.65553807120949));
#252984=CARTESIAN_POINT('Ctrl Pts',(60.9718026486699,-12.7653958126134,
3.65586275496802));
#252985=CARTESIAN_POINT('Ctrl Pts',(60.8885617651942,-12.7475073053519,
3.55128126837234));
#252986=CARTESIAN_POINT('Ctrl Pts',(60.7959446297928,-12.5977561540099,
3.77003198860255));
#252987=CARTESIAN_POINT('Ctrl Pts',(60.7696360759166,-12.7224234952028,
3.77025505748547));
#252988=CARTESIAN_POINT('Ctrl Pts',(60.7269846150115,-12.7131630221035,
3.64284211731188));
#252989=CARTESIAN_POINT('Ctrl Pts',(60.5836663843183,-12.5528626811438,
3.77003198860255));
#252990=CARTESIAN_POINT('Ctrl Pts',(60.5572221520605,-12.6772730124458,
3.77003198860255));
#252991=CARTESIAN_POINT('Ctrl Pts',(60.5572616290069,-12.6770872880155,
3.64284239821724));
#252992=CARTESIAN_POINT('Origin',(61.0050661295708,-12.6424339620832,3.40423097483302));
#252993=CARTESIAN_POINT('Ctrl Pts',(59.5971203935661,-12.3431658574201,
3.36123028058473));
#252994=CARTESIAN_POINT('Ctrl Pts',(59.5707156088322,-12.4673906027133,
3.36123028058473));
#252995=CARTESIAN_POINT('Ctrl Pts',(59.5707156088322,-12.4673906027133,
3.23423028058473));
#252996=CARTESIAN_POINT('Ctrl Pts',(59.5091256622726,-12.3242219811463,
3.36123028058473));
#252997=CARTESIAN_POINT('Ctrl Pts',(59.4825873732129,-12.4486583679648,
3.36146538610098));
#252998=CARTESIAN_POINT('Ctrl Pts',(59.4386519140007,-12.4393195978185,
3.23423043688441));
#252999=CARTESIAN_POINT('Ctrl Pts',(59.4259203549056,-12.3063073021292,
3.41054258693093));
#253000=CARTESIAN_POINT('Ctrl Pts',(59.3996784303277,-12.4310355281323,
3.41100608859737));
#253001=CARTESIAN_POINT('Ctrl Pts',(59.3137762748664,-12.4127764613278,
3.30819866970788));
#253002=CARTESIAN_POINT('Ctrl Pts',(59.3820708699072,-12.2968658913794,
3.48823028058473));
#253003=CARTESIAN_POINT('Ctrl Pts',(59.3560370505015,-12.4217592664903,
3.48852004212251));
#253004=CARTESIAN_POINT('Ctrl Pts',(59.2479658375578,-12.3987880210515,
3.42473028058472));
#253005=CARTESIAN_POINT('Origin',(59.2743706222916,-12.2745632757583,3.42473028058472));
#253006=CARTESIAN_POINT('Origin',(61.1793222555443,-12.6794732450919,3.11913648178272));
#253007=CARTESIAN_POINT('Origin',(61.3535783813234,-12.7165125280156,2.83404198860254));
#253008=CARTESIAN_POINT('Origin',(59.1947980527949,-12.2576496039896,3.5656311346087));
#253009=CARTESIAN_POINT('Origin',(59.1510793400374,-12.2483049653993,3.64299171721794));
#253010=CARTESIAN_POINT('Ctrl Pts',(61.5816197022699,-13.0739701745315,
2.59908173516015));
#253011=CARTESIAN_POINT('Ctrl Pts',(61.5451281645061,-13.0662229071057,
2.65878198860253));
#253012=CARTESIAN_POINT('Ctrl Pts',(61.4762657165317,-13.0516031943519,
2.65878198860253));
#253013=CARTESIAN_POINT('Ctrl Pts',(61.5999188988205,-12.9877758510411,
2.59908193475527));
#253014=CARTESIAN_POINT('Ctrl Pts',(61.5584544893694,-13.0034370926701,
2.6587871532546));
#253015=CARTESIAN_POINT('Ctrl Pts',(61.4868491822362,-13.0017087032035,
2.65878198860253));
#253016=CARTESIAN_POINT('Ctrl Pts',(61.5923336062396,-12.9030451317651,
2.63878778849883));
#253017=CARTESIAN_POINT('Ctrl Pts',(61.5481051179915,-12.9408103617793,
2.6956446018011));
#253018=CARTESIAN_POINT('Ctrl Pts',(61.4721451382823,-12.9504709278429,
2.68180481624881));
#253019=CARTESIAN_POINT('Ctrl Pts',(61.5434299552081,-12.7836101409421,
2.75443238878618));
#253020=CARTESIAN_POINT('Ctrl Pts',(61.50184710076,-12.8662000075455,2.7926834077708));
#253021=CARTESIAN_POINT('Ctrl Pts',(61.4139027244675,-12.874974700909,2.74885926835596));
#253022=CARTESIAN_POINT('Ctrl Pts',(61.5035207735037,-12.7478263086944,
2.82856655361677));
#253023=CARTESIAN_POINT('Ctrl Pts',(61.4652971063428,-12.8544221781242,
2.85384197230719));
#253024=CARTESIAN_POINT('Ctrl Pts',(61.371653694653,-12.850191810016,2.79184624278435));
#253025=CARTESIAN_POINT('Ctrl Pts',(61.459039055521,-12.7383709431241,2.90134173516017));
#253026=CARTESIAN_POINT('Ctrl Pts',(61.43297545991,-12.8632261535945,2.90163218716384));
#253027=CARTESIAN_POINT('Ctrl Pts',(61.3271735965895,-12.8407372733088,
2.83404198860254));
#253028=CARTESIAN_POINT('Origin',(61.4762657165317,-13.0516031943519,2.53178198860253));
#253029=CARTESIAN_POINT('Origin',(0.0660119618346401,0.310561863233168,
3.64303198860263));
#253030=CARTESIAN_POINT('Origin',(58.7584778814678,-12.1649068885782,3.64303198860255));
#253031=CARTESIAN_POINT('Origin',(5.5033905580924E-15,1.85916832635312E-13,
2.53178198860262));
#253032=CARTESIAN_POINT('Origin',(61.4699285681956,-13.0814171332223,2.53178198860253));
#253033=CARTESIAN_POINT('Ctrl Pts',(58.7584778814678,-12.1649068885782,
3.77003198860255));
#253034=CARTESIAN_POINT('Ctrl Pts',(58.7320335411741,-12.289317728149,3.77003198860255));
#253035=CARTESIAN_POINT('Ctrl Pts',(58.7320731263176,-12.2891314946913,
3.64284187937075));
#253036=CARTESIAN_POINT('Ctrl Pts',(58.5461948427484,-12.120019479967,3.77003198860255));
#253037=CARTESIAN_POINT('Ctrl Pts',(58.519984972071,-12.2442448876948,3.76980208963029));
#253038=CARTESIAN_POINT('Ctrl Pts',(58.5623471386662,-12.2530551225928,
3.64284193928396));
#253039=CARTESIAN_POINT('Ctrl Pts',(58.3441042111266,-12.0772896710132,
3.6555353541658));
#253040=CARTESIAN_POINT('Ctrl Pts',(58.3180679977625,-12.2013256001478,
3.65520057834298));
#253041=CARTESIAN_POINT('Ctrl Pts',(58.4007711908129,-12.2187110949215,
3.55127910964131));
#253042=CARTESIAN_POINT('Ctrl Pts',(58.2316113004783,-12.0535047649312,
3.47153072139065));
#253043=CARTESIAN_POINT('Ctrl Pts',(58.205761272577,-12.1774537884101,3.47122746281575));
#253044=CARTESIAN_POINT('Ctrl Pts',(58.3108302909892,-12.1995935666427,
3.40413045901286));
#253045=CARTESIAN_POINT('Origin',(58.3370777047236,-12.0753355159223,3.40423097483302));
#253046=CARTESIAN_POINT('Ctrl Pts',(61.3267881959115,-13.3605623192477,
2.90134173516014));
#253047=CARTESIAN_POINT('Ctrl Pts',(61.3537611057085,-13.2359003894741,
2.90163218716382));
#253048=CARTESIAN_POINT('Ctrl Pts',(61.2479592423879,-13.2134115091884,
2.83404198860253));
#253049=CARTESIAN_POINT('Ctrl Pts',(61.3712903180781,-13.3700210384226,
2.82853349835354));
#253050=CARTESIAN_POINT('Ctrl Pts',(61.3797222373783,-13.2571016411963,
2.85381483162401));
#253051=CARTESIAN_POINT('Ctrl Pts',(61.2924596082476,-13.2228703539486,
2.79182701594302));
#253052=CARTESIAN_POINT('Ctrl Pts',(61.4221282572892,-13.3535190881762,
2.75468822073622));
#253053=CARTESIAN_POINT('Ctrl Pts',(61.4177900459398,-13.2610999767694,
2.79286913083837));
#253054=CARTESIAN_POINT('Ctrl Pts',(61.3409599630866,-13.2173727427864,
2.74900763297898));
#253055=CARTESIAN_POINT('Ctrl Pts',(61.5148770953649,-13.2651598666392,
2.63954450640396));
#253056=CARTESIAN_POINT('Ctrl Pts',(61.4899829268152,-13.2123479779261,
2.69627684028846));
#253057=CARTESIAN_POINT('Ctrl Pts',(61.4244514636298,-13.172562552886,2.68224356036489));
#253058=CARTESIAN_POINT('Ctrl Pts',(61.5568698122757,-13.1903059833726,
2.59908178706355));
#253059=CARTESIAN_POINT('Ctrl Pts',(61.5253695547391,-13.1590895168681,
2.65878704321485));
#253060=CARTESIAN_POINT('Ctrl Pts',(61.4592680512448,-13.1314678292768,
2.65878198860253));
#253061=CARTESIAN_POINT('Ctrl Pts',(61.5752716937453,-13.1038352065718,
2.59908173516015));
#253062=CARTESIAN_POINT('Ctrl Pts',(61.5387839176329,-13.096070241967,2.65878198860254));
#253063=CARTESIAN_POINT('Ctrl Pts',(61.4699285681956,-13.0814171332223,
2.65878198860253));
#253064=CARTESIAN_POINT('Origin',(61.2215544576541,-13.3376362544816,2.83404198860253));
#253065=CARTESIAN_POINT('Origin',(58.1628213392036,-12.038296182048,3.11913648167005));
#253066=CARTESIAN_POINT('Origin',(57.9885649735461,-12.001256848085,2.83404198860254));
#253067=CARTESIAN_POINT('Origin',(61.0472983318751,-13.3005969715094,3.11913648177645));
#253068=CARTESIAN_POINT('Origin',(60.8730422059015,-13.2635576885492,3.40423097483301));
#253069=CARTESIAN_POINT('Ctrl Pts',(57.8830978693157,-11.9794294790603,
2.90134173516016));
#253070=CARTESIAN_POINT('Ctrl Pts',(57.8572899778513,-12.1031907419147,
2.90103711553221));
#253071=CARTESIAN_POINT('Ctrl Pts',(57.9621601888122,-12.1254815933782,
2.83404198860254));
#253072=CARTESIAN_POINT('Ctrl Pts',(57.8386546085358,-11.9699833161078,
2.82862991747953));
#253073=CARTESIAN_POINT('Ctrl Pts',(57.8310944294269,-12.0820882677168,
2.85314045886447));
#253074=CARTESIAN_POINT('Ctrl Pts',(57.9177151970033,-12.1160345187358,
2.79187960999923));
#253075=CARTESIAN_POINT('Ctrl Pts',(57.7880992891176,-11.9864204851021,
2.75470625793319));
#253076=CARTESIAN_POINT('Ctrl Pts',(57.7929810340972,-12.07829599916,2.79224250381855));
#253077=CARTESIAN_POINT('Ctrl Pts',(57.8694789541064,-12.1215717318486,
2.74901809108248));
#253078=CARTESIAN_POINT('Ctrl Pts',(57.6961636462599,-12.074672535238,2.6394786831169));
#253079=CARTESIAN_POINT('Ctrl Pts',(57.7211944343233,-12.1272484490374,
2.69595066767926));
#253080=CARTESIAN_POINT('Ctrl Pts',(57.7867317752137,-12.1665991704016,
2.68220539436057));
#253081=CARTESIAN_POINT('Ctrl Pts',(57.6547178110648,-12.1494120604573,
2.5990817858507));
#253082=CARTESIAN_POINT('Ctrl Pts',(57.6862546895616,-12.1804827566574,
2.65877670944855));
#253083=CARTESIAN_POINT('Ctrl Pts',(57.7524075778583,-12.2078361528622,
2.65878198860254));
#253084=CARTESIAN_POINT('Ctrl Pts',(57.6364522029208,-12.2354540642035,
2.59908173516015));
#253085=CARTESIAN_POINT('Ctrl Pts',(57.6729438621908,-12.2432007592838,
2.65878198860254));
#253086=CARTESIAN_POINT('Ctrl Pts',(57.7418065394567,-12.2578193919758,
2.65878198860254));
#253087=CARTESIAN_POINT('Origin',(57.7418065394567,-12.2578193919758,2.53178198860254));
#253088=CARTESIAN_POINT('Ctrl Pts',(60.4516424606491,-13.1739864076097,
3.77003198860255));
#253089=CARTESIAN_POINT('Ctrl Pts',(60.4780866951851,-13.0495760655895,
3.77003198860255));
#253090=CARTESIAN_POINT('Ctrl Pts',(60.4780472159571,-13.049761800754,3.64284238727587));
#253091=CARTESIAN_POINT('Ctrl Pts',(60.6638314094604,-13.219316225644,3.77003198860254));
#253092=CARTESIAN_POINT('Ctrl Pts',(60.6905041359622,-13.0947262769503,
3.77025506105806));
#253093=CARTESIAN_POINT('Ctrl Pts',(60.6477728389708,-13.0858380958626,
3.64284210641946));
#253094=CARTESIAN_POINT('Ctrl Pts',(60.8658323498483,-13.2624673401118,
3.65553527987824));
#253095=CARTESIAN_POINT('Ctrl Pts',(60.8926693037177,-13.137697324057,3.65585996533074));
#253096=CARTESIAN_POINT('Ctrl Pts',(60.8093487091498,-13.1201821075156,
3.55127902710124));
#253097=CARTESIAN_POINT('Ctrl Pts',(60.978275279735,-13.2864868028986,3.47153072139063));
#253098=CARTESIAN_POINT('Ctrl Pts',(61.0052918407717,-13.1616357172817,
3.4718232790518));
#253099=CARTESIAN_POINT('Ctrl Pts',(60.8992893450419,-13.1392995799677,
3.40413028377977));
#253100=CARTESIAN_POINT('Origin',(60.4516424606491,-13.1739864076097,3.64303198860255));
#253101=CARTESIAN_POINT('Origin',(5.72205236298458E-15,1.86312531323806E-13,
2.53178198860262));
#253102=CARTESIAN_POINT('Origin',(57.7354693911206,-12.2876333308462,2.53178198860254));
#253103=CARTESIAN_POINT('Origin',(59.4667368016504,-12.9646382471637,3.64303198860254));
#253104=CARTESIAN_POINT('Origin',(60.0590486699125,-13.090590866118,3.64299466007516));
#253105=CARTESIAN_POINT('Ctrl Pts',(57.6301266171959,-12.2652136052652,
2.59908173516015));
#253106=CARTESIAN_POINT('Ctrl Pts',(57.6666142715157,-12.2729791421546,
2.65878198860254));
#253107=CARTESIAN_POINT('Ctrl Pts',(57.7354693911206,-12.2876333308462,
2.65878198860254));
#253108=CARTESIAN_POINT('Ctrl Pts',(57.6118791634504,-12.3509528635296,
2.59908193199891));
#253109=CARTESIAN_POINT('Ctrl Pts',(57.653317055794,-12.3354428975783,2.65877685806589));
#253110=CARTESIAN_POINT('Ctrl Pts',(57.7248602994012,-12.3374367183498,
2.65878198860254));
#253111=CARTESIAN_POINT('Ctrl Pts',(57.6190178232952,-12.4353658313034,
2.63872492669782));
#253112=CARTESIAN_POINT('Ctrl Pts',(57.6632723181622,-12.3978675338889,
2.69532212015261));
#253113=CARTESIAN_POINT('Ctrl Pts',(57.7390640345626,-12.3886090227458,
2.68176836726626));
#253114=CARTESIAN_POINT('Ctrl Pts',(57.6672013517154,-12.5543478197365,
2.75442176402249));
#253115=CARTESIAN_POINT('Ctrl Pts',(57.7090592089827,-12.4724831634106,
2.79203179920134));
#253116=CARTESIAN_POINT('Ctrl Pts',(57.7965151898612,-12.4639865158412,
2.74885310748168));
#253117=CARTESIAN_POINT('Ctrl Pts',(57.706889956891,-12.5899803678805,2.82866089558387));
#253118=CARTESIAN_POINT('Ctrl Pts',(57.7455787351224,-12.4844838378922,
2.85316563119125));
#253119=CARTESIAN_POINT('Ctrl Pts',(57.8385197202051,-12.4887127671314,
2.79189751796652));
#253120=CARTESIAN_POINT('Ctrl Pts',(57.7513140650722,-12.5994235324462,
2.90134173516015));
#253121=CARTESIAN_POINT('Ctrl Pts',(57.7780756236497,-12.4758649777943,
2.90103711553221));
#253122=CARTESIAN_POINT('Ctrl Pts',(57.8829458346107,-12.4981558292578,
2.83404198860253));
#253123=CARTESIAN_POINT('Origin',(57.8565410498768,-12.622380574551,2.83404198860254));
#253124=CARTESIAN_POINT('Origin',(60.0157999977487,-13.0813452322597,3.56647653971841));
#253125=CARTESIAN_POINT('Origin',(59.9357500275435,-13.0643300858372,3.42473028058477));
#253126=CARTESIAN_POINT('Origin',(58.0307974155295,-12.6594199084515,3.11913648168104));
#253127=CARTESIAN_POINT('Origin',(58.2050537810543,-12.6964592423883,3.40423097483303));
#253128=CARTESIAN_POINT('Ctrl Pts',(59.6130003254557,-12.9957275188814,
3.36123028058473));
#253129=CARTESIAN_POINT('Ctrl Pts',(59.6394051101895,-12.8715027735882,
3.36123028058473));
#253130=CARTESIAN_POINT('Ctrl Pts',(59.6394051101895,-12.8715027735882,
3.23423028058473));
#253131=CARTESIAN_POINT('Ctrl Pts',(59.7010925481785,-13.0142126749434,
3.36123028058473));
#253132=CARTESIAN_POINT('Ctrl Pts',(59.7273659613752,-12.8901994296784,
3.36099641108421));
#253133=CARTESIAN_POINT('Ctrl Pts',(59.7714687931899,-12.8995737759683,
3.23423043688393));
#253134=CARTESIAN_POINT('Ctrl Pts',(59.7843900000233,-13.0316935695379,
3.41054258905273));
#253135=CARTESIAN_POINT('Ctrl Pts',(59.8109544298256,-12.9079667071259,
3.41008815826081));
#253136=CARTESIAN_POINT('Ctrl Pts',(59.8963444006342,-12.9261169057231,
3.30819867304296));
#253137=CARTESIAN_POINT('Ctrl Pts',(59.8282880397057,-13.0409063549229,
3.48823028058476));
#253138=CARTESIAN_POINT('Ctrl Pts',(59.8550545325311,-12.9173404733273,
3.48794691941592));
#253139=CARTESIAN_POINT('Ctrl Pts',(59.9621548122773,-12.940105340544,3.42473028058477));
#253140=CARTESIAN_POINT('Origin',(59.6130003254557,-12.9957275188814,3.23423028058473));
#253141=CARTESIAN_POINT('Ctrl Pts',(58.0998260601482,-12.6735055745731,
3.47153072139064));
#253142=CARTESIAN_POINT('Ctrl Pts',(58.1266254912132,-12.5497583678821,
3.47122746285069));
#253143=CARTESIAN_POINT('Ctrl Pts',(58.2316158657529,-12.5722680770238,
3.4041304667678));
#253144=CARTESIAN_POINT('Ctrl Pts',(58.2122693395992,-12.6975323335619,
3.65553813457982));
#253145=CARTESIAN_POINT('Ctrl Pts',(58.238934028847,-12.5736300041233,3.65520336072198));
#253146=CARTESIAN_POINT('Ctrl Pts',(58.3215581271246,-12.5913858949911,
3.55128134519905));
#253147=CARTESIAN_POINT('Ctrl Pts',(58.4142696920429,-12.7406947165187,
3.77003198860255));
#253148=CARTESIAN_POINT('Ctrl Pts',(58.4408527990778,-12.6165486539527,
3.76980209314141));
#253149=CARTESIAN_POINT('Ctrl Pts',(58.4831353553006,-12.6257301953092,
3.64284195387441));
#253150=CARTESIAN_POINT('Ctrl Pts',(58.6264539577985,-12.7860306150442,
3.77003198860255));
#253151=CARTESIAN_POINT('Ctrl Pts',(58.6528982950381,-12.6616197898416,
3.77003198860255));
#253152=CARTESIAN_POINT('Ctrl Pts',(58.6528587129533,-12.6618060089097,
3.64284189403795));
#253153=CARTESIAN_POINT('Origin',(58.6264539577985,-12.7860306150442,3.64303198860255));
#253154=CARTESIAN_POINT('Origin',(58.0246834617332,-12.6581203474861,3.23423028058473));
#253155=CARTESIAN_POINT('Origin',(59.4650964698968,-12.9642895838861,3.23423028058473));
#253156=CARTESIAN_POINT('Origin',(57.7988642628865,-12.6101209950202,3.64303198860255));
#253157=CARTESIAN_POINT('Origin',(59.0190342907436,-12.8695280801137,3.64299171721763));
#253158=CARTESIAN_POINT('Ctrl Pts',(59.2498070616281,-12.9191181862036,
3.48823028058473));
#253159=CARTESIAN_POINT('Ctrl Pts',(59.2768226963,-12.7944335023699,3.48852004212251));
#253160=CARTESIAN_POINT('Ctrl Pts',(59.1687514833562,-12.771462256931,3.42473028058473));
#253161=CARTESIAN_POINT('Ctrl Pts',(59.2938540730361,-12.9283593439856,
3.41028005848398));
#253162=CARTESIAN_POINT('Ctrl Pts',(59.3206115991478,-12.8037411209985,
3.4107440422032));
#253163=CARTESIAN_POINT('Ctrl Pts',(59.2347843016956,-12.7854979657546,
3.30780486243868));
#253164=CARTESIAN_POINT('Ctrl Pts',(59.3773008374014,-12.9458672564,3.36123028058473));
#253165=CARTESIAN_POINT('Ctrl Pts',(59.4036696715728,-12.8213956592925,
3.36146460586378));
#253166=CARTESIAN_POINT('Ctrl Pts',(59.3598823995826,-12.812088387313,3.23423045308421));
#253167=CARTESIAN_POINT('Ctrl Pts',(59.4650964698968,-12.9642895838861,
3.36123028058473));
#253168=CARTESIAN_POINT('Ctrl Pts',(59.4915012546307,-12.8400648385929,
3.36123028058473));
#253169=CARTESIAN_POINT('Ctrl Pts',(59.4915012546306,-12.8400648385929,
3.23423028058473));
#253170=CARTESIAN_POINT('Origin',(59.1423466986224,-12.8956870022242,3.42473028058473));
#253171=CARTESIAN_POINT('Origin',(59.062774130148,-12.8787733309731,3.56563113524819));
#253172=CARTESIAN_POINT('Origin',(61.1207756556244,-6.10480350566308,3.56647653909447));
#253173=CARTESIAN_POINT('Origin',(61.1647646440465,-6.10937495962015,3.64299466007748));
#253174=CARTESIAN_POINT('Origin',(61.0393856393805,-6.09624906995137,3.4247302805848));
#253175=CARTESIAN_POINT('Ctrl Pts',(60.9299448846691,-6.08531878138219,
3.48823028058481));
#253176=CARTESIAN_POINT('Ctrl Pts',(60.9172173747511,-6.21110821942835,
3.48794691941597));
#253177=CARTESIAN_POINT('Ctrl Pts',(61.0261105245455,-6.22255335066314,
3.42473028058482));
#253178=CARTESIAN_POINT('Ctrl Pts',(60.8851977561471,-6.0804991887655,3.41028005925085));
#253179=CARTESIAN_POINT('Ctrl Pts',(60.8722275639199,-6.2063795997648,3.40982512230922));
#253180=CARTESIAN_POINT('Ctrl Pts',(60.9589723348255,-6.2154968425755,3.30780486372776));
#253181=CARTESIAN_POINT('Ctrl Pts',(60.800424540796,-6.07136793516245,3.36123028058478));
#253182=CARTESIAN_POINT('Ctrl Pts',(60.787089847893,-6.19743126523058,3.36099721048457));
#253183=CARTESIAN_POINT('Ctrl Pts',(60.8317801127809,-6.20212840134576,
3.23423045308397));
#253184=CARTESIAN_POINT('Ctrl Pts',(60.7112330730305,-6.06175884541469,
3.36123028058478));
#253185=CARTESIAN_POINT('Ctrl Pts',(60.6979579581955,-6.18806312612646,
3.36123028058478));
#253186=CARTESIAN_POINT('Ctrl Pts',(60.6979579581955,-6.18806312612646,
3.23423028058478));
#253187=CARTESIAN_POINT('Origin',(60.7112330730305,-6.06175884541469,3.23423028058478));
#253188=CARTESIAN_POINT('Origin',(0.0331877870874813,0.315760701779611,
3.64303198860263));
#253189=CARTESIAN_POINT('Origin',(61.5639141665613,-6.15137923967573,3.64303198860259));
#253190=CARTESIAN_POINT('Origin',(0.0331877870874813,0.315760701779614,
3.23423028058482));
#253191=CARTESIAN_POINT('Origin',(60.5608532912344,-6.0459532934496,3.23423028058478));
#253192=CARTESIAN_POINT('Ctrl Pts',(62.099536274866,-6.20712349654361,3.47153072139067));
#253193=CARTESIAN_POINT('Ctrl Pts',(62.0866494451786,-6.33421250060399,
3.47182327902658));
#253194=CARTESIAN_POINT('Ctrl Pts',(61.9789328429853,-6.3226988688789,3.40413028958998));
#253195=CARTESIAN_POINT('Ctrl Pts',(61.9851725366286,-6.195220406346,3.65553807120954));
#253196=CARTESIAN_POINT('Ctrl Pts',(61.9721399414771,-6.32217680516124,
3.65586275496904));
#253197=CARTESIAN_POINT('Ctrl Pts',(61.8874852020944,-6.31308733464651,
3.55128126837217));
#253198=CARTESIAN_POINT('Ctrl Pts',(61.7797221753255,-6.17383766261601,
3.7700319886026));
#253199=CARTESIAN_POINT('Ctrl Pts',(61.7665890280504,-6.3005720557779,3.77025505748631));
#253200=CARTESIAN_POINT('Ctrl Pts',(61.7232032332896,-6.29582060418223,
3.64284211731207));
#253201=CARTESIAN_POINT('Ctrl Pts',(61.5639141665613,-6.15137923967573,
3.77003198860259));
#253202=CARTESIAN_POINT('Ctrl Pts',(61.5506192193202,-6.27787221312659,
3.77003198860259));
#253203=CARTESIAN_POINT('Ctrl Pts',(61.5506390665185,-6.27768337964882,
3.64284239821648));
#253204=CARTESIAN_POINT('Origin',(61.992368188267,-6.19641157197361,3.40423097483306));
#253205=CARTESIAN_POINT('Ctrl Pts',(60.5608532912344,-6.0459532934496,3.36123028058478));
#253206=CARTESIAN_POINT('Ctrl Pts',(60.5475781763994,-6.17225757416137,
3.36123028058478));
#253207=CARTESIAN_POINT('Ctrl Pts',(60.5475781763994,-6.17225757416137,
3.23423028058478));
#253208=CARTESIAN_POINT('Ctrl Pts',(60.4713604300109,-6.03631114774924,
3.36123028058478));
#253209=CARTESIAN_POINT('Ctrl Pts',(60.457974664764,-6.162839865594,3.36146538610174));
#253210=CARTESIAN_POINT('Ctrl Pts',(60.4133037213019,-6.15814476024263,
3.23423043688428));
#253211=CARTESIAN_POINT('Ctrl Pts',(60.386738336156,-6.02719193013285,3.41054258693097));
#253212=CARTESIAN_POINT('Ctrl Pts',(60.3736778173769,-6.15397990991393,
3.41100608859692));
#253213=CARTESIAN_POINT('Ctrl Pts',(60.2863376507178,-6.1448000884892,3.30819866970818));
#253214=CARTESIAN_POINT('Ctrl Pts',(60.3421421670676,-6.02238575970175,
3.48823028058478));
#253215=CARTESIAN_POINT('Ctrl Pts',(60.3293058762212,-6.14931623097146,
3.48852004212255));
#253216=CARTESIAN_POINT('Ctrl Pts',(60.2194255397046,-6.13776734223115,
3.42473028058477));
#253217=CARTESIAN_POINT('Origin',(60.2327006545396,-6.01146306151938,3.42473028058478));
#253218=CARTESIAN_POINT('Origin',(62.1695413802842,-6.21503322485375,3.11913648178356));
#253219=CARTESIAN_POINT('Origin',(62.346714572097,-6.23365487766521,2.83404198860258));
#253220=CARTESIAN_POINT('Origin',(60.1517960317847,-6.00295964302144,3.56563113460787));
#253221=CARTESIAN_POINT('Origin',(60.1073400339999,-5.99823604520041,3.64299171721801));
#253222=CARTESIAN_POINT('Ctrl Pts',(62.6108711573006,-6.56531752495198,
2.59908173516019));
#253223=CARTESIAN_POINT('Ctrl Pts',(62.5737697140403,-6.56142710223248,
2.65878198860258));
#253224=CARTESIAN_POINT('Ctrl Pts',(62.5037563256536,-6.55408556365842,
2.65878198860258));
#253225=CARTESIAN_POINT('Ctrl Pts',(62.6200603487599,-6.47768259608977,
2.59908193475699));
#253226=CARTESIAN_POINT('Ctrl Pts',(62.5804601311999,-6.49759225479858,
2.65878715325436));
#253227=CARTESIAN_POINT('Ctrl Pts',(62.5090664195357,-6.50335812634647,
2.65878198860258));
#253228=CARTESIAN_POINT('Ctrl Pts',(62.6036598373291,-6.39420891953656,
2.63878778849873));
#253229=CARTESIAN_POINT('Ctrl Pts',(62.563621178826,-6.43639040357826,2.69564460180097));
#253230=CARTESIAN_POINT('Ctrl Pts',(62.4890871199578,-6.45393802799926,
2.68180481624877));
#253231=CARTESIAN_POINT('Ctrl Pts',(62.5425397295636,-6.28054002958038,
2.75443238878635));
#253232=CARTESIAN_POINT('Ctrl Pts',(62.5098176621801,-6.36702405212695,
2.79268340777105));
#253233=CARTESIAN_POINT('Ctrl Pts',(62.4232722595963,-6.38494336730876,
2.74885926835608));
#253234=CARTESIAN_POINT('Ctrl Pts',(62.4991087455377,-6.24912387034354,
2.82856655361668));
#253235=CARTESIAN_POINT('Ctrl Pts',(62.472236774049,-6.35913125763664,2.85384197230803));
#253236=CARTESIAN_POINT('Ctrl Pts',(62.378664156887,-6.36471246584618,2.79184624278429));
#253237=CARTESIAN_POINT('Ctrl Pts',(62.4538823482276,-6.24436990787956,
2.9013417351602));
#253238=CARTESIAN_POINT('Ctrl Pts',(62.4410124550019,-6.37126553603967,
2.90163218716387));
#253239=CARTESIAN_POINT('Ctrl Pts',(62.333439457262,-6.35995915837698,2.83404198860258));
#253240=CARTESIAN_POINT('Origin',(62.5037563256536,-6.55408556365842,2.53178198860258));
#253241=CARTESIAN_POINT('Origin',(0.0331877870874813,0.315760701779611,
3.64303198860263));
#253242=CARTESIAN_POINT('Origin',(59.7081718144893,-5.95633285891111,3.64303198860259));
#253243=CARTESIAN_POINT('Origin',(5.50069060731754E-15,1.85899785817018E-13,
2.53178198860262));
#253244=CARTESIAN_POINT('Origin',(62.5005702980932,-6.58439859102924,2.53178198860258));
#253245=CARTESIAN_POINT('Ctrl Pts',(59.7081718144893,-5.95633285891111,
3.7700319886026));
#253246=CARTESIAN_POINT('Ctrl Pts',(59.6948768129328,-6.08282634913903,
3.7700319886026));
#253247=CARTESIAN_POINT('Ctrl Pts',(59.6948967145276,-6.08263699811283,
3.64284187937022));
#253248=CARTESIAN_POINT('Ctrl Pts',(59.4923596726254,-5.93388096803621,
3.77003198860259));
#253249=CARTESIAN_POINT('Ctrl Pts',(59.4792784733334,-6.06016553348737,
3.76980208962883));
#253250=CARTESIAN_POINT('Ctrl Pts',(59.5223294958632,-6.06449945282166,
3.64284193928313));
#253251=CARTESIAN_POINT('Ctrl Pts',(59.286909633363,-5.91250946061063,3.65553535416583));
#253252=CARTESIAN_POINT('Ctrl Pts',(59.2739813341584,-6.03858743331987,
3.65520057834522));
#253253=CARTESIAN_POINT('Ctrl Pts',(59.3580487495157,-6.04723285085665,
3.55127910964232));
#253254=CARTESIAN_POINT('Ctrl Pts',(59.1725467709678,-5.90061356181158,
3.47153072139069));
#253255=CARTESIAN_POINT('Ctrl Pts',(59.1597945531718,-6.02658564326334,
3.47122746281579));
#253256=CARTESIAN_POINT('Ctrl Pts',(59.266602229504,-6.03762143444208,3.4041304590126));
#253257=CARTESIAN_POINT('Origin',(59.2797173540687,-5.91130048050243,3.40423097483307));
#253258=CARTESIAN_POINT('Ctrl Pts',(62.3873926810692,-6.87697683366461,
2.9013417351602));
#253259=CARTESIAN_POINT('Ctrl Pts',(62.4011871104969,-6.75017837817499,
2.90163218716387));
#253260=CARTESIAN_POINT('Ctrl Pts',(62.293614112757,-6.73887200051229,2.83404198860258));
#253261=CARTESIAN_POINT('Ctrl Pts',(62.4326397213342,-6.88173199854405,
2.82853349835343));
#253262=CARTESIAN_POINT('Ctrl Pts',(62.4292221586327,-6.76854981002352,
2.85381483162388));
#253263=CARTESIAN_POINT('Ctrl Pts',(62.3388594194629,-6.74362747387298,
2.79182701594246));
#253264=CARTESIAN_POINT('Ctrl Pts',(62.4814742414947,-6.86000643604628,
2.7546882207365));
#253265=CARTESIAN_POINT('Ctrl Pts',(62.4674993676295,-6.7685470727674,2.79286913083857));
#253266=CARTESIAN_POINT('Ctrl Pts',(62.3865194274374,-6.73309031164083,
2.74900763297913));
#253267=CARTESIAN_POINT('Ctrl Pts',(62.5644789380884,-6.76243636205594,
2.63954450640377));
#253268=CARTESIAN_POINT('Ctrl Pts',(62.5342007968288,-6.7125159315779,2.69627684028836));
#253269=CARTESIAN_POINT('Ctrl Pts',(62.4648696125159,-6.67979835840146,
2.68224356036483));
#253270=CARTESIAN_POINT('Ctrl Pts',(62.5984172531148,-6.6836031020271,2.59908178706326));
#253271=CARTESIAN_POINT('Ctrl Pts',(62.5638265480141,-6.65585031610526,
2.65878704321495));
#253272=CARTESIAN_POINT('Ctrl Pts',(62.4951999029147,-6.63528943158862,
2.65878198860258));
#253273=CARTESIAN_POINT('Ctrl Pts',(62.6076796697355,-6.59568250079781,
2.59908173516019));
#253274=CARTESIAN_POINT('Ctrl Pts',(62.570580117661,-6.5917740846467,2.65878198860258));
#253275=CARTESIAN_POINT('Ctrl Pts',(62.5005702980932,-6.58439859102924,
2.65878198860258));
#253276=CARTESIAN_POINT('Origin',(62.280338997922,-6.86517628122406,2.83404198860256));
#253277=CARTESIAN_POINT('Origin',(59.1025439185018,-5.89267880207648,3.11913648166983));
#253278=CARTESIAN_POINT('Origin',(58.9253704827881,-5.8740571235777,2.83404198860258));
#253279=CARTESIAN_POINT('Origin',(62.1031658061017,-6.84655462836415,3.11913648177572));
#253280=CARTESIAN_POINT('Origin',(61.925992614092,-6.82793297553246,3.40423097483306));
#253281=CARTESIAN_POINT('Ctrl Pts',(58.8181995570486,-5.86337364149481,
2.9013417351602));
#253282=CARTESIAN_POINT('Ctrl Pts',(58.8054696185321,-5.98915458643695,
2.90103711553225));
#253283=CARTESIAN_POINT('Ctrl Pts',(58.9120953679531,-6.00036140428947,
2.83404198860258));
#253284=CARTESIAN_POINT('Ctrl Pts',(58.7730123682041,-5.85862481136359,
2.82862991747957));
#253285=CARTESIAN_POINT('Ctrl Pts',(58.7772117628632,-5.97090589422296,
2.8531404588642));
#253286=CARTESIAN_POINT('Ctrl Pts',(58.8669063622646,-5.99561184840417,
2.79187960999922));
#253287=CARTESIAN_POINT('Ctrl Pts',(58.7244521481308,-5.88025640567477,
2.75470625793323));
#253288=CARTESIAN_POINT('Ctrl Pts',(58.7389107566974,-5.97111833475291,
2.79224250381903));
#253289=CARTESIAN_POINT('Ctrl Pts',(58.8195131589314,-6.00616078842793,
2.74901809108255));
#253290=CARTESIAN_POINT('Ctrl Pts',(58.642244989525,-5.97763489331347,2.63947868311695));
#253291=CARTESIAN_POINT('Ctrl Pts',(58.6726343357866,-6.02730636094513,
2.69595066767902));
#253292=CARTESIAN_POINT('Ctrl Pts',(58.7419259266988,-6.05959099741067,
2.68220539436058));
#253293=CARTESIAN_POINT('Ctrl Pts',(58.6088386066682,-6.05629725705532,
2.59908178585078));
#253294=CARTESIAN_POINT('Ctrl Pts',(58.6434504949713,-6.08390124328518,
2.65877670944852));
#253295=CARTESIAN_POINT('Ctrl Pts',(58.712100199296,-6.10418993496927,2.65878198860258));
#253296=CARTESIAN_POINT('Ctrl Pts',(58.5996668978649,-6.14377718965223,
2.5990817351602));
#253297=CARTESIAN_POINT('Ctrl Pts',(58.6367684021393,-6.14766703046072,
2.65878198860258));
#253298=CARTESIAN_POINT('Ctrl Pts',(58.7067819056644,-6.15500747092217,
2.65878198860258));
#253299=CARTESIAN_POINT('Origin',(58.7067819056644,-6.15500747092217,2.53178198860258));
#253300=CARTESIAN_POINT('Ctrl Pts',(61.4975385923863,-6.78290064323459,
3.77003198860259));
#253301=CARTESIAN_POINT('Ctrl Pts',(61.5108335407727,-6.65640765888671,
3.77003198860259));
#253302=CARTESIAN_POINT('Ctrl Pts',(61.5108136924274,-6.65659650327775,
3.6428423872758));
#253303=CARTESIAN_POINT('Ctrl Pts',(61.7133034041536,-6.80580235504162,
3.77003198860259));
#253304=CARTESIAN_POINT('Ctrl Pts',(61.7268068187927,-6.67910686401023,
3.7702550610589));
#253305=CARTESIAN_POINT('Ctrl Pts',(61.683380540407,-6.6747340101162,3.64284210641928));
#253306=CARTESIAN_POINT('Ctrl Pts',(61.9187082819379,-6.82760223531246,
3.65553527987827));
#253307=CARTESIAN_POINT('Ctrl Pts',(61.932356202127,-6.70071049691164,3.6558599653304));
#253308=CARTESIAN_POINT('Ctrl Pts',(61.847661207825,-6.69200060426902,3.55127902710152));
#253309=CARTESIAN_POINT('Ctrl Pts',(62.0330459552233,-6.83973663030157,
3.47153072139068));
#253310=CARTESIAN_POINT('Ctrl Pts',(62.0468640245951,-6.71274549238699,
3.47182327905184));
#253311=CARTESIAN_POINT('Ctrl Pts',(61.9391074595192,-6.70161199275156,
3.40413028377976));
#253312=CARTESIAN_POINT('Origin',(61.4975385923863,-6.78290064323459,3.64303198860259));
#253313=CARTESIAN_POINT('Origin',(5.72301283402738E-15,1.86318595499308E-13,
2.53178198860262));
#253314=CARTESIAN_POINT('Origin',(58.703595878104,-6.185320498293,2.53178198860258));
#253315=CARTESIAN_POINT('Origin',(61.5094129706999,-6.78414869068649,3.64303198860258));
#253316=CARTESIAN_POINT('Origin',(61.0983782637173,-6.74099917687762,3.64299466007604));
#253317=CARTESIAN_POINT('Ctrl Pts',(58.5964866834552,-6.17403490858921,
2.5990817351602));
#253318=CARTESIAN_POINT('Ctrl Pts',(58.6335861742243,-6.17794390662073,
2.65878198860258));
#253319=CARTESIAN_POINT('Ctrl Pts',(58.703595878104,-6.185320498293,2.65878198860258));
#253320=CARTESIAN_POINT('Ctrl Pts',(58.5873013840787,-6.26121185652445,
2.5990819319991));
#253321=CARTESIAN_POINT('Ctrl Pts',(58.626891042407,-6.24145541658163,2.65877685806647));
#253322=CARTESIAN_POINT('Ctrl Pts',(58.6982507756596,-6.23596000968288,
2.65878198860258));
#253323=CARTESIAN_POINT('Ctrl Pts',(58.6032244953991,-6.34441620808506,
2.63872492669791));
#253324=CARTESIAN_POINT('Ctrl Pts',(58.6433169201089,-6.30249747592631,
2.69532212015275));
#253325=CARTESIAN_POINT('Ctrl Pts',(58.7177256636153,-6.28536729223223,
2.68176836726633));
#253326=CARTESIAN_POINT('Ctrl Pts',(58.6635810738165,-6.45770985055576,
2.75442176402249));
#253327=CARTESIAN_POINT('Ctrl Pts',(58.6966524426404,-6.37191831988681,
2.79203179920125));
#253328=CARTESIAN_POINT('Ctrl Pts',(58.7827411889911,-6.35432657855714,
2.74885310748169));
#253329=CARTESIAN_POINT('Ctrl Pts',(58.7067768761601,-6.48899861096465,
2.82866089558393));
#253330=CARTESIAN_POINT('Ctrl Pts',(58.7342263230553,-6.38003592347135,
2.85316563119217));
#253331=CARTESIAN_POINT('Ctrl Pts',(58.8271002111739,-6.37452670784861,
2.79189751796605));
#253332=CARTESIAN_POINT('Ctrl Pts',(58.7519447039089,-6.49374646112642,
2.90134173516019));
#253333=CARTESIAN_POINT('Ctrl Pts',(58.7656442740272,-6.36806742857227,
2.90103711553225));
#253334=CARTESIAN_POINT('Ctrl Pts',(58.8722700234481,-6.37927424642479,
2.83404198860258));
#253335=CARTESIAN_POINT('Origin',(58.8589949086131,-6.50557852713656,2.83404198860258));
#253336=CARTESIAN_POINT('Origin',(61.0544000804071,-6.73632490881137,3.56647653971777));
#253337=CARTESIAN_POINT('Origin',(60.9730100652055,-6.72777047351023,3.42473028058482));
#253338=CARTESIAN_POINT('Origin',(59.0361683443145,-6.52420020557606,3.11913648168137));
#253339=CARTESIAN_POINT('Origin',(59.2133417798937,-6.54282188406129,3.40423097483307));
#253340=CARTESIAN_POINT('Ctrl Pts',(60.6448574988555,-6.69328024897354,
3.36123028058478));
#253341=CARTESIAN_POINT('Ctrl Pts',(60.6581326136905,-6.56697596826177,
3.36123028058478));
#253342=CARTESIAN_POINT('Ctrl Pts',(60.6581326136905,-6.56697596826177,
3.23423028058478));
#253343=CARTESIAN_POINT('Ctrl Pts',(60.7343993681214,-6.70245599674913,
3.36123028058477));
#253344=CARTESIAN_POINT('Ctrl Pts',(60.7475659388593,-6.57637578951109,
3.36099641108468));
#253345=CARTESIAN_POINT('Ctrl Pts',(60.7924070567585,-6.58108878091615,
3.23423043688383));
#253346=CARTESIAN_POINT('Ctrl Pts',(60.819067758858,-6.71113417453868,3.41054258905281));
#253347=CARTESIAN_POINT('Ctrl Pts',(60.8325536871411,-6.5853083618035,3.41008815826054));
#253348=CARTESIAN_POINT('Ctrl Pts',(60.9193730951228,-6.59443344928315,
3.30819867304313));
#253349=CARTESIAN_POINT('Ctrl Pts',(60.8636883187846,-6.71570789669309,
3.4882302805848));
#253350=CARTESIAN_POINT('Ctrl Pts',(60.8773920302461,-6.59002106156365,
3.48794691941596));
#253351=CARTESIAN_POINT('Ctrl Pts',(60.9862851800405,-6.60146619279846,
3.42473028058481));
#253352=CARTESIAN_POINT('Origin',(60.6448574988555,-6.69328024897354,3.23423028058478));
#253353=CARTESIAN_POINT('Ctrl Pts',(59.1062911958297,-6.53099325079956,
3.47153072139068));
#253354=CARTESIAN_POINT('Ctrl Pts',(59.1200087114583,-6.40512264090918,
3.47122746285073));
#253355=CARTESIAN_POINT('Ctrl Pts',(59.226776843046,-6.41653455700024,3.40413046676793));
#253356=CARTESIAN_POINT('Ctrl Pts',(59.2206299794252,-6.54313486548251,
3.65553813457982));
#253357=CARTESIAN_POINT('Ctrl Pts',(59.2341972766252,-6.41712406698003,
3.65520336072103));
#253358=CARTESIAN_POINT('Ctrl Pts',(59.3182247474342,-6.42614611919656,
3.55128134519899));
#253359=CARTESIAN_POINT('Ctrl Pts',(59.4260354503639,-6.56494601397015,
3.77003198860259));
#253360=CARTESIAN_POINT('Ctrl Pts',(59.4394961352153,-6.43870134519669,
3.7698020931422));
#253361=CARTESIAN_POINT('Ctrl Pts',(59.482506795579,-6.44341285848338,3.64284195387417));
#253362=CARTESIAN_POINT('Ctrl Pts',(59.6417962403144,-6.58785426246996,
3.77003198860259));
#253363=CARTESIAN_POINT('Ctrl Pts',(59.6550912403353,-6.46136078685152,
3.77003198860259));
#253364=CARTESIAN_POINT('Ctrl Pts',(59.6550713402783,-6.46155012324641,
3.64284189403816));
#253365=CARTESIAN_POINT('Origin',(59.6417962403144,-6.58785426246996,3.64303198860259));
#253366=CARTESIAN_POINT('Origin',(60.0186752706393,-6.62746584473993,3.23423028058478));
#253367=CARTESIAN_POINT('Origin',(60.4944777170595,-6.67747469700845,3.23423028058478));
#253368=CARTESIAN_POINT('Origin',(59.7852323155142,-6.60293000146335,3.64303198860259));
#253369=CARTESIAN_POINT('Origin',(60.04095383883,-6.62985850077703,3.6429917172181));
#253370=CARTESIAN_POINT('Ctrl Pts',(60.275645989912,-6.65505462397295,3.48823028058477));
#253371=CARTESIAN_POINT('Ctrl Pts',(60.2894805317163,-6.52822907310677,
3.48852004212255));
#253372=CARTESIAN_POINT('Ctrl Pts',(60.1796001951996,-6.51668018436646,
3.42473028058477));
#253373=CARTESIAN_POINT('Ctrl Pts',(60.3204176712045,-6.65964099131217,
3.41028005848403));
#253374=CARTESIAN_POINT('Ctrl Pts',(60.3340024654448,-6.53290851690499,
3.41074404220316));
#253375=CARTESIAN_POINT('Ctrl Pts',(60.2467384099257,-6.52373669508235,
3.307804862439));
#253376=CARTESIAN_POINT('Ctrl Pts',(60.4052373806432,-6.66833043150578,
3.36123028058477));
#253377=CARTESIAN_POINT('Ctrl Pts',(60.4184509388157,-6.54178440911694,
3.36146460586406));
#253378=CARTESIAN_POINT('Ctrl Pts',(60.3739306632455,-6.53710513959924,
3.23423045308408));
#253379=CARTESIAN_POINT('Ctrl Pts',(60.4944777170595,-6.67747469700845,
3.36123028058478));
#253380=CARTESIAN_POINT('Ctrl Pts',(60.5077528318945,-6.55117041629668,
3.36123028058478));
#253381=CARTESIAN_POINT('Ctrl Pts',(60.5077528318945,-6.55117041629668,
3.23423028058478));
#253382=CARTESIAN_POINT('Origin',(60.1663250803646,-6.64298446507823,3.42473028058476));
#253383=CARTESIAN_POINT('Origin',(60.0854204586802,-6.63448104699067,3.5656311352473));
#253384=CARTESIAN_POINT('Origin',(0.,0.,41.0845));
#253385=CARTESIAN_POINT('',(-65.254,-7.99131022315614E-15,41.0845));
#253386=CARTESIAN_POINT('Origin',(0.,0.,41.0845));
#253387=CARTESIAN_POINT('',(-65.381,-8.00686323750531E-15,41.2115));
#253388=CARTESIAN_POINT('Origin',(-65.381,-8.00686323750531E-15,41.0845));
#253389=CARTESIAN_POINT('Origin',(0.,0.,41.2115));
#253390=CARTESIAN_POINT('Origin',(-1.38777878078145E-14,-1.38777878078145E-14,
41.3385));
#253391=CARTESIAN_POINT('',(-68.623,-2.22816815376033E-14,41.2115));
#253392=CARTESIAN_POINT('Origin',(-1.38777878078145E-14,-1.38777878078145E-14,
41.2115));
#253393=CARTESIAN_POINT('',(-68.75,-2.22972345519525E-14,41.3385));
#253394=CARTESIAN_POINT('Origin',(-68.623,-2.22816815376033E-14,41.3385));
#253395=CARTESIAN_POINT('Origin',(-1.38777878078145E-14,-1.38777878078145E-14,
41.3385));
#253396=CARTESIAN_POINT('Origin',(-1.38777878078145E-14,-1.38777878078145E-14,
42.3545));
#253397=CARTESIAN_POINT('',(68.877,-2.23127875663017E-14,42.4815));
#253398=CARTESIAN_POINT('Origin',(-1.38777878078145E-14,-1.38777878078145E-14,
42.4815));
#253399=CARTESIAN_POINT('',(68.75,-2.22972345519525E-14,42.3545));
#253400=CARTESIAN_POINT('Origin',(68.877,-2.23127875663017E-14,42.3545));
#253401=CARTESIAN_POINT('',(-68.75,-5.4583410636764E-15,42.3545));
#253402=CARTESIAN_POINT('Origin',(-1.38777878078145E-14,-1.38777878078145E-14,
42.3545));
#253403=CARTESIAN_POINT('Origin',(-1.38777878078145E-14,-1.38777878078145E-14,
42.3545));
#253404=CARTESIAN_POINT('Origin',(0.,0.,17.4625));
#253405=CARTESIAN_POINT('',(-65.254,-7.99131022315614E-15,17.4625));
#253406=CARTESIAN_POINT('Origin',(0.,0.,17.4625));
#253407=CARTESIAN_POINT('',(-65.254,-7.99131022315614E-15,17.4625));
#253408=CARTESIAN_POINT('Origin',(-1.38777878078145E-14,-1.38777878078145E-14,
41.2115));
#253409=CARTESIAN_POINT('',(-68.75,-2.22972345519525E-14,41.2115));
#253410=CARTESIAN_POINT('Origin',(-1.38777878078145E-14,-1.38777878078145E-14,
17.4625));
#253411=CARTESIAN_POINT('',(-72.5300000000001,-2.27601510420302E-14,42.4815));
#253412=CARTESIAN_POINT('Origin',(-1.38777878078145E-14,-1.38777878078145E-14,
42.4815));
#253413=CARTESIAN_POINT('',(-72.5300000000001,-2.27601510420302E-14,17.4625));
#253414=CARTESIAN_POINT('',(-72.5300000000001,-2.27601510420302E-14,17.4625));
#253415=CARTESIAN_POINT('Origin',(-1.38777878078145E-14,-1.38777878078145E-14,
17.4625));
#253416=CARTESIAN_POINT('Origin',(-1.38777878078145E-14,-1.38777878078145E-14,
17.4625));
#253417=CARTESIAN_POINT('Origin',(-1.38777878078145E-14,-1.38777878078145E-14,
42.4815));
#253418=CARTESIAN_POINT('Origin',(-1.38777878078145E-14,-1.38777878078145E-14,
41.2115));
#253419=CARTESIAN_POINT('Origin',(0.,0.,41.1353));
#253420=CARTESIAN_POINT('',(-65.,-7.9602041944578E-15,41.1353));
#253421=CARTESIAN_POINT('Origin',(0.,0.,41.1353));
#253422=CARTESIAN_POINT('',(-65.0762,-7.9695360030673E-15,41.2115));
#253423=CARTESIAN_POINT('Origin',(-65.0762,-7.9695360030673E-15,41.1353));
#253424=CARTESIAN_POINT('Origin',(0.,0.,41.2115));
#253425=CARTESIAN_POINT('Origin',(0.,0.,41.1353));
#253426=CARTESIAN_POINT('',(-65.1778,-7.98197841454664E-15,41.2115));
#253427=CARTESIAN_POINT('Origin',(0.,0.,41.2115));
#253428=CARTESIAN_POINT('',(-65.254,-7.99131022315614E-15,41.1353));
#253429=CARTESIAN_POINT('Origin',(-65.1778,-7.98197841454664E-15,41.1353));
#253430=CARTESIAN_POINT('Origin',(0.,0.,41.1353));
#253431=CARTESIAN_POINT('Origin',(0.,0.,17.4625));
#253432=CARTESIAN_POINT('',(-65.,-7.9602041944578E-15,17.4625));
#253433=CARTESIAN_POINT('Origin',(0.,0.,17.4625));
#253434=CARTESIAN_POINT('',(-65.,-7.9602041944578E-15,17.4625));
#253435=CARTESIAN_POINT('Origin',(0.,0.,17.4625));
#253436=CARTESIAN_POINT('',(-65.254,-7.99131022315614E-15,17.4625));
#253437=CARTESIAN_POINT('',(-65.254,-7.99131022315614E-15,17.4625));
#253438=CARTESIAN_POINT('Origin',(0.,0.,17.4625));
#253439=CARTESIAN_POINT('Origin',(0.,0.,17.4625));
#253440=CARTESIAN_POINT('Origin',(0.,0.,41.2115));
#253441=CARTESIAN_POINT('Origin',(-1.38777878078145E-14,-1.38777878078145E-14,
42.037));
#253442=CARTESIAN_POINT('',(-70.625,-2.25268558267926E-14,42.4815));
#253443=CARTESIAN_POINT('Origin',(0.,0.,42.4815));
#253444=CARTESIAN_POINT('',(-71.3206076480316,-2.26120431947551E-14,42.8625));
#253445=CARTESIAN_POINT('Origin',(-71.3206076480316,-2.26120431947551E-14,
42.037));
#253446=CARTESIAN_POINT('Origin',(-1.38777878078145E-14,-1.38777878078145E-14,
42.8625));
#253447=CARTESIAN_POINT('Origin',(0.,0.,40.3225));
#253448=CARTESIAN_POINT('',(10.8580391950581,76.3872907109282,40.6320481322491));
#253449=CARTESIAN_POINT('',(-10.8580391950582,76.3872907109282,40.6320481322491));
#253450=CARTESIAN_POINT('Origin',(0.,0.,40.6320481322491));
#253451=CARTESIAN_POINT('',(10.5032495111116,73.8913131000538,42.8625));
#253452=CARTESIAN_POINT('Origin',(10.5032495111116,73.8913131000538,40.3225));
#253453=CARTESIAN_POINT('',(-10.5032495111116,73.8913131000538,42.8625));
#253454=CARTESIAN_POINT('Origin',(0.,0.,42.8625));
#253455=CARTESIAN_POINT('Origin',(-10.5032495111116,73.8913131000538,40.3225));
#253456=CARTESIAN_POINT('Origin',(90.,-90.,16.1925));
#253457=CARTESIAN_POINT('',(110.478801107225,-75.6605890912239,16.1925));
#253458=CARTESIAN_POINT('',(75.6605890912239,-110.478801107225,16.1925));
#253459=CARTESIAN_POINT('Origin',(90.,-90.,16.1925));
#253460=CARTESIAN_POINT('',(109.438478010978,-76.3890311653897,17.4625));
#253461=CARTESIAN_POINT('Origin',(109.438478010978,-76.3890311653897,16.1925));
#253462=CARTESIAN_POINT('',(76.3890311653897,-109.438478010978,17.4625));
#253463=CARTESIAN_POINT('Origin',(90.,-90.,17.4625));
#253464=CARTESIAN_POINT('Origin',(76.3890311653897,-109.438478010978,16.1925));
#253465=CARTESIAN_POINT('Origin',(90.,90.,16.1925));
#253466=CARTESIAN_POINT('',(75.6605890912238,110.478801107225,16.1925));
#253467=CARTESIAN_POINT('',(110.478801107225,75.6605890912239,16.1925));
#253468=CARTESIAN_POINT('Origin',(90.,90.,16.1925));
#253469=CARTESIAN_POINT('',(76.3890311653897,109.438478010978,17.4625));
#253470=CARTESIAN_POINT('Origin',(76.3890311653897,109.438478010978,16.1925));
#253471=CARTESIAN_POINT('',(109.438478010978,76.3890311653897,17.4625));
#253472=CARTESIAN_POINT('Origin',(90.,90.,17.4625));
#253473=CARTESIAN_POINT('Origin',(109.438478010978,76.3890311653897,16.1925));
#253474=CARTESIAN_POINT('Ctrl Pts',(-77.8839876917858,25.347849735742,12.3825));
#253475=CARTESIAN_POINT('Ctrl Pts',(-77.7859473914177,25.6490890766241,
12.3825));
#253476=CARTESIAN_POINT('Ctrl Pts',(-77.9676516999077,25.9085897226106,
12.3825));
#253477=CARTESIAN_POINT('Ctrl Pts',(-76.0725110230494,24.758292886385,12.3825));
#253478=CARTESIAN_POINT('Ctrl Pts',(-75.6803498215769,25.9632502499131,
12.3825));
#253479=CARTESIAN_POINT('Ctrl Pts',(-76.4071670555372,27.0012528338594,
12.3825));
#253480=CARTESIAN_POINT('Ctrl Pts',(-76.0725110230494,24.758292886385,14.2875));
#253481=CARTESIAN_POINT('Ctrl Pts',(-75.6803498215769,25.9632502499131,
14.2875));
#253482=CARTESIAN_POINT('Ctrl Pts',(-76.4071670555372,27.0012528338594,
14.2875));
#253483=CARTESIAN_POINT('',(-77.8839876917858,25.347849735742,12.3825));
#253484=CARTESIAN_POINT('',(-77.9676516999077,25.9085897226106,12.3825));
#253485=CARTESIAN_POINT('Origin',(-78.4878132480312,25.5443686855277,12.3825));
#253486=CARTESIAN_POINT('',(-76.0725110230494,24.758292886385,14.2875));
#253487=CARTESIAN_POINT('Origin',(-77.8839876917858,25.347849735742,14.2875));
#253488=CARTESIAN_POINT('',(-76.4071670555372,27.0012528338594,14.2875));
#253489=CARTESIAN_POINT('Origin',(-78.4878132480312,25.5443686855277,14.2875));
#253490=CARTESIAN_POINT('Origin',(-77.9676516999077,25.9085897226106,14.2875));
#253491=CARTESIAN_POINT('Ctrl Pts',(-77.9676516999077,-25.9085897226106,
12.3825));
#253492=CARTESIAN_POINT('Ctrl Pts',(-77.7859473914177,-25.6490890766241,
12.3825));
#253493=CARTESIAN_POINT('Ctrl Pts',(-77.8839876917858,-25.347849735742,
12.3825));
#253494=CARTESIAN_POINT('Ctrl Pts',(-76.4071670555372,-27.0012528338594,
12.3825));
#253495=CARTESIAN_POINT('Ctrl Pts',(-75.6803498215769,-25.9632502499131,
12.3825));
#253496=CARTESIAN_POINT('Ctrl Pts',(-76.0725110230494,-24.758292886385,
12.3825));
#253497=CARTESIAN_POINT('Ctrl Pts',(-76.4071670555372,-27.0012528338594,
14.2875));
#253498=CARTESIAN_POINT('Ctrl Pts',(-75.6803498215769,-25.9632502499131,
14.2875));
#253499=CARTESIAN_POINT('Ctrl Pts',(-76.0725110230494,-24.758292886385,
14.2875));
#253500=CARTESIAN_POINT('',(-77.9676516999077,-25.9085897226106,12.3825));
#253501=CARTESIAN_POINT('',(-77.8839876917858,-25.347849735742,12.3825));
#253502=CARTESIAN_POINT('Origin',(-78.4878132480312,-25.5443686855277,12.3825));
#253503=CARTESIAN_POINT('',(-76.4071670555372,-27.0012528338594,14.2875));
#253504=CARTESIAN_POINT('Origin',(-77.9676516999077,-25.9085897226106,14.2875));
#253505=CARTESIAN_POINT('',(-76.0725110230494,-24.758292886385,14.2875));
#253506=CARTESIAN_POINT('Origin',(-78.4878132480312,-25.5443686855277,14.2875));
#253507=CARTESIAN_POINT('Origin',(-77.8839876917858,-25.347849735742,14.2875));
#253508=CARTESIAN_POINT('Ctrl Pts',(77.8839876917858,-25.3478497357421,
12.3825));
#253509=CARTESIAN_POINT('Ctrl Pts',(77.7859473914177,-25.6490890766241,
12.3825));
#253510=CARTESIAN_POINT('Ctrl Pts',(77.9676516999078,-25.9085897226106,
12.3825));
#253511=CARTESIAN_POINT('Ctrl Pts',(76.0725110230494,-24.758292886385,12.3825));
#253512=CARTESIAN_POINT('Ctrl Pts',(75.6803498215769,-25.9632502499131,
12.3825));
#253513=CARTESIAN_POINT('Ctrl Pts',(76.4071670555372,-27.0012528338594,
12.3825));
#253514=CARTESIAN_POINT('Ctrl Pts',(76.0725110230494,-24.758292886385,14.2875));
#253515=CARTESIAN_POINT('Ctrl Pts',(75.6803498215769,-25.9632502499131,
14.2875));
#253516=CARTESIAN_POINT('Ctrl Pts',(76.4071670555372,-27.0012528338594,
14.2875));
#253517=CARTESIAN_POINT('',(77.8839876917858,-25.3478497357421,12.3825));
#253518=CARTESIAN_POINT('',(77.9676516999077,-25.9085897226107,12.3825));
#253519=CARTESIAN_POINT('Origin',(78.4878132480313,-25.5443686855277,12.3825));
#253520=CARTESIAN_POINT('',(76.0725110230494,-24.758292886385,14.2875));
#253521=CARTESIAN_POINT('Origin',(77.8839876917858,-25.3478497357421,14.2875));
#253522=CARTESIAN_POINT('',(76.4071670555372,-27.0012528338594,14.2875));
#253523=CARTESIAN_POINT('Origin',(78.4878132480313,-25.5443686855277,14.2875));
#253524=CARTESIAN_POINT('Origin',(77.9676516999077,-25.9085897226107,14.2875));
#253525=CARTESIAN_POINT('Origin',(0.,0.,14.2875));
#253526=CARTESIAN_POINT('',(76.0725110230494,24.758292886385,14.2875));
#253527=CARTESIAN_POINT('Origin',(0.,0.,14.2875));
#253528=CARTESIAN_POINT('',(77.8839876917858,25.3478497357421,12.3825));
#253529=CARTESIAN_POINT('Origin',(0.,0.,12.3825));
#253530=CARTESIAN_POINT('Origin',(77.8839876917858,25.3478497357421,14.2875));
#253531=CARTESIAN_POINT('Ctrl Pts',(77.9676516999078,25.9085897226107,12.3825));
#253532=CARTESIAN_POINT('Ctrl Pts',(77.7859473914177,25.6490890766241,12.3825));
#253533=CARTESIAN_POINT('Ctrl Pts',(77.8839876917858,25.3478497357421,12.3825));
#253534=CARTESIAN_POINT('Ctrl Pts',(76.4071670555372,27.0012528338594,12.3825));
#253535=CARTESIAN_POINT('Ctrl Pts',(75.6803498215769,25.9632502499131,12.3825));
#253536=CARTESIAN_POINT('Ctrl Pts',(76.0725110230494,24.758292886385,12.3825));
#253537=CARTESIAN_POINT('Ctrl Pts',(76.4071670555372,27.0012528338594,14.2875));
#253538=CARTESIAN_POINT('Ctrl Pts',(75.6803498215769,25.9632502499131,14.2875));
#253539=CARTESIAN_POINT('Ctrl Pts',(76.0725110230494,24.758292886385,14.2875));
#253540=CARTESIAN_POINT('',(77.9676516999077,25.9085897226107,12.3825));
#253541=CARTESIAN_POINT('Origin',(78.4878132480313,25.5443686855277,12.3825));
#253542=CARTESIAN_POINT('',(76.4071670555372,27.0012528338594,14.2875));
#253543=CARTESIAN_POINT('Origin',(77.9676516999077,25.9085897226107,14.2875));
#253544=CARTESIAN_POINT('Origin',(78.4878132480313,25.5443686855277,14.2875));
#253545=CARTESIAN_POINT('Origin',(-78.4878132480312,25.5443686855277,12.3825));
#253546=CARTESIAN_POINT('',(-76.0725110230494,24.758292886385,17.0741173620445));
#253547=CARTESIAN_POINT('',(-76.0725110230494,24.758292886385,12.3825));
#253548=CARTESIAN_POINT('',(-75.9797434607283,25.1428889948603,17.0741173620445));
#253549=CARTESIAN_POINT('Origin',(-78.4878132480312,25.5443686855277,17.0741173620445));
#253550=CARTESIAN_POINT('',(-75.9478132480312,25.544368685519,16.7790882779809));
#253551=CARTESIAN_POINT('Ctrl Pts',(-75.9797434607283,25.1428889948603,
17.0741173620445));
#253552=CARTESIAN_POINT('Ctrl Pts',(-75.9600903294859,25.2656633862951,
16.9588689369795));
#253553=CARTESIAN_POINT('Ctrl Pts',(-75.9478132480309,25.4015417700709,
16.8637563773694));
#253554=CARTESIAN_POINT('Ctrl Pts',(-75.9478132480312,25.544368685519,16.7790882779809));
#253555=CARTESIAN_POINT('',(-76.4071703643125,27.0012572613409,16.0836464440003));
#253556=CARTESIAN_POINT('Ctrl Pts',(-75.9478132480312,25.544368685519,16.7790882779809));
#253557=CARTESIAN_POINT('Ctrl Pts',(-75.9478132480303,25.6765921306316,
16.7007059383813));
#253558=CARTESIAN_POINT('Ctrl Pts',(-75.9584171366964,25.816334343438,16.6310264783953));
#253559=CARTESIAN_POINT('Ctrl Pts',(-76.0045629689351,26.0968884213634,
16.5063573484839));
#253560=CARTESIAN_POINT('Ctrl Pts',(-76.0396368564122,26.2368139673711,
16.4516393979191));
#253561=CARTESIAN_POINT('Ctrl Pts',(-76.1354463408314,26.5136044910669,
16.3525814751901));
#253562=CARTESIAN_POINT('Ctrl Pts',(-76.1966925113156,26.6511815359268,
16.308172958015));
#253563=CARTESIAN_POINT('Ctrl Pts',(-76.306792867175,26.8483691944594,16.2492604516738));
#253564=CARTESIAN_POINT('Ctrl Pts',(-76.3466590420083,26.9128851528656,
16.2309506379062));
#253565=CARTESIAN_POINT('Ctrl Pts',(-76.4002047884601,26.9913835733178,
16.2087984367714));
#253566=CARTESIAN_POINT('Ctrl Pts',(-76.4110986052641,27.0069745617798,
16.2044315143317));
#253567=CARTESIAN_POINT('Ctrl Pts',(-76.4276519058228,27.0301092948723,
16.1975104106263));
#253568=CARTESIAN_POINT('Ctrl Pts',(-76.4332238412039,27.0378039510364,
16.1952643836651));
#253569=CARTESIAN_POINT('Ctrl Pts',(-76.4442170623447,27.0528119734108,
16.1893033167685));
#253570=CARTESIAN_POINT('Ctrl Pts',(-76.4506141578954,27.0614120539566,
16.1833338857357));
#253571=CARTESIAN_POINT('Ctrl Pts',(-76.4496048710994,27.0600557662765,
16.1636449186976));
#253572=CARTESIAN_POINT('Ctrl Pts',(-76.445847589196,27.0550011412656,16.1552610170204));
#253573=CARTESIAN_POINT('Ctrl Pts',(-76.4389163531081,27.0455867516878,
16.1396560112813));
#253574=CARTESIAN_POINT('Ctrl Pts',(-76.4350958850463,27.0403618512071,
16.1323196149044));
#253575=CARTESIAN_POINT('Ctrl Pts',(-76.4234011422968,27.0242265009732,
16.1108031014866));
#253576=CARTESIAN_POINT('Ctrl Pts',(-76.4152687037725,27.0128231866378,
16.0971732455228));
#253577=CARTESIAN_POINT('Ctrl Pts',(-76.4071670555372,27.0012528338594,
16.0836603564333));
#253578=CARTESIAN_POINT('',(-76.4071670555372,27.0012528338594,17.0741173620445));
#253579=CARTESIAN_POINT('Origin',(-78.4878132480312,-25.5443686855277,12.3825));
#253580=CARTESIAN_POINT('',(-76.4071670555372,-27.0012528338594,16.0836576823356));
#253581=CARTESIAN_POINT('',(-76.4071670555372,-27.0012528338594,12.3825));
#253582=CARTESIAN_POINT('',(-75.9478282514034,-25.544368692031,16.7790882775718));
#253583=CARTESIAN_POINT('Ctrl Pts',(-76.4071670555372,-27.0012528338594,
16.0836576823356));
#253584=CARTESIAN_POINT('Ctrl Pts',(-76.4152523939033,-27.0127999068814,
16.0971460288751));
#253585=CARTESIAN_POINT('Ctrl Pts',(-76.4233804349652,-27.0241972663232,
16.1107708588669));
#253586=CARTESIAN_POINT('Ctrl Pts',(-76.4350405965502,-27.0402858986055,
16.1322149894862));
#253587=CARTESIAN_POINT('Ctrl Pts',(-76.4388439109148,-27.0454878961872,
16.1395118886607));
#253588=CARTESIAN_POINT('Ctrl Pts',(-76.4457808819976,-27.0549109871946,
16.1550922359403));
#253589=CARTESIAN_POINT('Ctrl Pts',(-76.4495262827364,-27.0599501461243,
16.1634279843414));
#253590=CARTESIAN_POINT('Ctrl Pts',(-76.4506693829202,-27.0614862780154,
16.1831233908523));
#253591=CARTESIAN_POINT('Ctrl Pts',(-76.4443470115083,-27.0529879564382,
16.1892139275835));
#253592=CARTESIAN_POINT('Ctrl Pts',(-76.4333625249832,-27.0379946731629,
16.1952076519701));
#253593=CARTESIAN_POINT('Ctrl Pts',(-76.4277817362483,-27.0302892875527,
16.1974549295803));
#253594=CARTESIAN_POINT('Ctrl Pts',(-76.4112309135534,-27.0071623375438,
16.2043785477607));
#253595=CARTESIAN_POINT('Ctrl Pts',(-76.4003361866038,-26.9915731287254,
16.2087447794625));
#253596=CARTESIAN_POINT('Ctrl Pts',(-76.3467821072315,-26.9130777753189,
16.230896934636));
#253597=CARTESIAN_POINT('Ctrl Pts',(-76.3069514286797,-26.8486340830899,
16.2491835660637));
#253598=CARTESIAN_POINT('Ctrl Pts',(-76.1968338030491,-26.6514726518305,
16.3080814902354));
#253599=CARTESIAN_POINT('Ctrl Pts',(-76.1355975399761,-26.5139532715615,
16.3524675745753));
#253600=CARTESIAN_POINT('Ctrl Pts',(-76.0398121713394,-26.2374081758968,
16.4514158583587));
#253601=CARTESIAN_POINT('Ctrl Pts',(-76.0046988236937,-26.0975162379414,
16.5060990022633));
#253602=CARTESIAN_POINT('Ctrl Pts',(-75.9584674534131,-25.816837601813,
16.6307822945995));
#253603=CARTESIAN_POINT('Ctrl Pts',(-75.9478132480311,-25.6771355556999,
16.700383794839));
#253604=CARTESIAN_POINT('Ctrl Pts',(-75.9478132480312,-25.5443686855242,
16.7790882779778));
#253605=CARTESIAN_POINT('',(-75.9797434607283,-25.1428889948604,17.0741173620445));
#253606=CARTESIAN_POINT('Ctrl Pts',(-75.9478432547756,-25.5443686985378,
16.7790882771658));
#253607=CARTESIAN_POINT('Ctrl Pts',(-75.9478592799661,-25.5087358023417,
16.8002117896876));
#253608=CARTESIAN_POINT('Ctrl Pts',(-75.9486271497168,-25.4734339822992,
16.8220725722267));
#253609=CARTESIAN_POINT('Ctrl Pts',(-75.950085661309,-25.4386219982237,
16.8447668373521));
#253610=CARTESIAN_POINT('Ctrl Pts',(-75.950632603156,-25.4255675041953,
16.8532771867742));
#253611=CARTESIAN_POINT('Ctrl Pts',(-75.9512765391559,-25.4125819305939,
16.8619047448722));
#253612=CARTESIAN_POINT('Ctrl Pts',(-75.9520137796523,-25.399673751837,
16.8706545860217));
#253613=CARTESIAN_POINT('Ctrl Pts',(-75.9526588650866,-25.3883790954247,
16.8783106970275));
#253614=CARTESIAN_POINT('Ctrl Pts',(-75.9533753830629,-25.3771436956814,
16.8860604310073));
#253615=CARTESIAN_POINT('Ctrl Pts',(-75.9541607010869,-25.3659732454842,
16.8939071875044));
#253616=CARTESIAN_POINT('Ctrl Pts',(-75.9564237260398,-25.3337837289305,
16.916518925948));
#253617=CARTESIAN_POINT('Ctrl Pts',(-75.9592588897836,-25.3021331439168,
16.939934354713));
#253618=CARTESIAN_POINT('Ctrl Pts',(-75.962596000696,-25.2711588719201,
16.9642401976005));
#253619=CARTESIAN_POINT('Ctrl Pts',(-75.9633120606089,-25.2645125736434,
16.9694556190224));
#253620=CARTESIAN_POINT('Ctrl Pts',(-75.9640511964207,-25.2578973684702,
16.9747118561142));
#253621=CARTESIAN_POINT('Ctrl Pts',(-75.9648126596724,-25.2513145358426,
16.980009460251));
#253622=CARTESIAN_POINT('Ctrl Pts',(-75.9669677451484,-25.2326838705344,
16.9950026850816));
#253623=CARTESIAN_POINT('Ctrl Pts',(-75.9693017197781,-25.2143130480956,
17.0103294780056));
#253624=CARTESIAN_POINT('Ctrl Pts',(-75.9717964668484,-25.1962321628045,
17.0260080558434));
#253625=CARTESIAN_POINT('Ctrl Pts',(-75.9742912139187,-25.1781512775134,
17.0416866336811));
#253626=CARTESIAN_POINT('Ctrl Pts',(-75.9769467318632,-25.1603603423111,
17.0577170011241));
#253627=CARTESIAN_POINT('Ctrl Pts',(-75.9797434607283,-25.1428889948604,
17.0741173620445));
#253628=CARTESIAN_POINT('',(-76.0725110230494,-24.758292886385,17.0741173620445));
#253629=CARTESIAN_POINT('Origin',(-78.4878132480312,-25.5443686855277,17.0741173620445));
#253630=CARTESIAN_POINT('',(-76.0725110230494,-24.758292886385,12.3825));
#253631=CARTESIAN_POINT('Origin',(0.,0.,17.0741173620445));
#253632=CARTESIAN_POINT('',(-76.0424582863717,24.6976449920627,17.8479876922247));
#253633=CARTESIAN_POINT('',(-76.0424582863716,-24.6976449920628,17.847987692225));
#253634=CARTESIAN_POINT('Origin',(0.,0.,17.8479876926672));
#253635=CARTESIAN_POINT('Ctrl Pts',(-76.0424582865173,24.6976449914385,
17.8479876926672));
#253636=CARTESIAN_POINT('Ctrl Pts',(-76.0624207920021,24.737936883604,17.5919904624029));
#253637=CARTESIAN_POINT('Ctrl Pts',(-76.0725110230494,24.758292886385,17.3340474816323));
#253638=CARTESIAN_POINT('Ctrl Pts',(-76.0725110230494,24.758292886385,17.0741173620445));
#253639=CARTESIAN_POINT('Origin',(0.,0.,17.0741173620445));
#253640=CARTESIAN_POINT('Ctrl Pts',(-76.0725110230494,-24.758292886385,
17.0741173620445));
#253641=CARTESIAN_POINT('Ctrl Pts',(-76.0725110230494,-24.758292886385,
17.3340474816323));
#253642=CARTESIAN_POINT('Ctrl Pts',(-76.0624207920021,-24.737936883604,
17.5919904624035));
#253643=CARTESIAN_POINT('Ctrl Pts',(-76.0424582865173,-24.6976449914384,
17.8479876926672));
#253644=CARTESIAN_POINT('Origin',(0.,0.,248.008319357841));
#253645=CARTESIAN_POINT('',(72.53,-8.88236323421576E-15,42.4815));
#253646=CARTESIAN_POINT('Origin',(0.,0.,42.4815));
#253647=CARTESIAN_POINT('',(72.53,-8.88236323421576E-15,8.25499999999998));
#253648=CARTESIAN_POINT('',(72.53,-8.88236323421576E-15,248.008319357841));
#253649=CARTESIAN_POINT('Origin',(0.,0.,8.25499999999998));
#253650=CARTESIAN_POINT('Origin',(-90.,-90.,63.5));
#253651=CARTESIAN_POINT('',(-81.5545,-90.,17.4625));
#253652=CARTESIAN_POINT('Origin',(-90.,-90.,17.4625));
#253653=CARTESIAN_POINT('',(-81.5545,-90.,8.255));
#253654=CARTESIAN_POINT('',(-81.5545,-90.,63.5));
#253655=CARTESIAN_POINT('Origin',(-90.,-90.,8.255));
#253656=CARTESIAN_POINT('Origin',(-90.,90.,63.5));
#253657=CARTESIAN_POINT('',(-81.5545,90.,17.4625));
#253658=CARTESIAN_POINT('Origin',(-90.,90.,17.4625));
#253659=CARTESIAN_POINT('',(-81.5545,90.,8.255));
#253660=CARTESIAN_POINT('',(-81.5545,90.,63.5));
#253661=CARTESIAN_POINT('Origin',(-90.,90.,8.255));
#253662=CARTESIAN_POINT('Origin',(90.,90.,63.5));
#253663=CARTESIAN_POINT('',(98.4455,90.,17.4625));
#253664=CARTESIAN_POINT('Origin',(90.,90.,17.4625));
#253665=CARTESIAN_POINT('',(98.4455,90.,8.255));
#253666=CARTESIAN_POINT('',(98.4455,90.,63.5));
#253667=CARTESIAN_POINT('Origin',(90.,90.,8.255));
#253668=CARTESIAN_POINT('Origin',(90.,-90.,63.5));
#253669=CARTESIAN_POINT('',(98.4455,-90.,17.4625));
#253670=CARTESIAN_POINT('Origin',(90.,-90.,17.4625));
#253671=CARTESIAN_POINT('',(98.4455,-90.,8.255));
#253672=CARTESIAN_POINT('',(98.4455,-90.,63.5));
#253673=CARTESIAN_POINT('Origin',(90.,-90.,8.255));
#253674=CARTESIAN_POINT('Origin',(0.,0.,12.3825));
#253675=CARTESIAN_POINT('',(76.0725110230494,24.758292886385,17.0741173620445));
#253676=CARTESIAN_POINT('',(76.0725110230494,24.758292886385,12.3825));
#253677=CARTESIAN_POINT('',(76.0725110230494,-24.758292886385,17.0741173620445));
#253678=CARTESIAN_POINT('Origin',(0.,0.,17.0741173620445));
#253679=CARTESIAN_POINT('',(76.0725110230494,-24.758292886385,12.3825));
#253680=CARTESIAN_POINT('Origin',(0.,0.,17.4625));
#253681=CARTESIAN_POINT('',(-10.8641498708349,79.2111064053766,17.8479876926672));
#253682=CARTESIAN_POINT('Ctrl Pts',(-10.8580391950582,76.3872907109282,
40.6320481322491));
#253683=CARTESIAN_POINT('Ctrl Pts',(-10.8580660689152,76.3992856302614,
40.5352987690743));
#253684=CARTESIAN_POINT('Ctrl Pts',(-10.8580929305605,76.4112804979204,
40.4385493994896));
#253685=CARTESIAN_POINT('Ctrl Pts',(-10.8581197800107,76.423275313976,40.3418000235038));
#253686=CARTESIAN_POINT('Ctrl Pts',(-10.8590524915919,76.8399581047936,
36.9808647820832));
#253687=CARTESIAN_POINT('Ctrl Pts',(-10.8599704900686,77.256578637456,33.6199218173622));
#253688=CARTESIAN_POINT('Ctrl Pts',(-10.8608744504877,77.6731397785624,
30.2589714884058));
#253689=CARTESIAN_POINT('Ctrl Pts',(-10.861987132648,78.1858836339049,26.1219878400834));
#253690=CARTESIAN_POINT('Ctrl Pts',(-10.8630785478348,78.6985375142473,
21.9849930334727));
#253691=CARTESIAN_POINT('Ctrl Pts',(-10.8641498708349,79.2111064053766,
17.8479876926672));
#253692=CARTESIAN_POINT('',(-24.6976449920629,76.0424582863716,17.847987692225));
#253693=CARTESIAN_POINT('Origin',(0.,0.,17.8479876926672));
#253694=CARTESIAN_POINT('',(-25.1183523255102,75.961488153786,17.4075632995852));
#253695=CARTESIAN_POINT('Ctrl Pts',(-24.6976449919804,76.0424582864102,
17.8479876921334));
#253696=CARTESIAN_POINT('Ctrl Pts',(-24.8421318546264,76.0139038233433,
17.7056692315415));
#253697=CARTESIAN_POINT('Ctrl Pts',(-24.9826881607289,75.9867559935942,
17.5590635300787));
#253698=CARTESIAN_POINT('Ctrl Pts',(-25.1183452685109,75.9614890268762,
17.4075745924918));
#253699=CARTESIAN_POINT('',(-28.7459974181805,74.3634602878983,19.6929518677509));
#253700=CARTESIAN_POINT('Ctrl Pts',(-25.1183716157479,75.9614818429678,
17.4075624145231));
#253701=CARTESIAN_POINT('Ctrl Pts',(-25.1663807403387,75.9292306004122,
17.5341891960434));
#253702=CARTESIAN_POINT('Ctrl Pts',(-25.2225896116214,75.8946388507543,
17.6574709249722));
#253703=CARTESIAN_POINT('Ctrl Pts',(-25.285623436093,75.8583098126767,17.7758260768801));
#253704=CARTESIAN_POINT('Ctrl Pts',(-25.3144603202055,75.8416899063051,
17.8299715111495));
#253705=CARTESIAN_POINT('Ctrl Pts',(-25.3447263486284,75.824706154463,17.8830859081177));
#253706=CARTESIAN_POINT('Ctrl Pts',(-25.3762932265105,75.8074152517247,
17.9350176026268));
#253707=CARTESIAN_POINT('Ctrl Pts',(-25.3987704081996,75.7951032719378,
17.9719955431525));
#253708=CARTESIAN_POINT('Ctrl Pts',(-25.4219292775774,75.7826225663754,
18.0084169806869));
#253709=CARTESIAN_POINT('Ctrl Pts',(-25.4457245653072,75.7699942838142,
18.0442185658015));
#253710=CARTESIAN_POINT('Ctrl Pts',(-25.5176575567036,75.7318190723546,
18.1524465117406));
#253711=CARTESIAN_POINT('Ctrl Pts',(-25.5954180175484,75.6922139916061,
18.2556268052651));
#253712=CARTESIAN_POINT('Ctrl Pts',(-25.6787085180146,75.6512007481018,
18.3538912523495));
#253713=CARTESIAN_POINT('Ctrl Pts',(-25.6911412019917,75.6450787450822,
18.3685590813329));
#253714=CARTESIAN_POINT('Ctrl Pts',(-25.7036970322645,75.6389253810112,
18.383117441432));
#253715=CARTESIAN_POINT('Ctrl Pts',(-25.7163749474321,75.6327407433448,
18.3975668354582));
#253716=CARTESIAN_POINT('Ctrl Pts',(-25.790822604906,75.5964231169445,18.4824170275406));
#253717=CARTESIAN_POINT('Ctrl Pts',(-25.8695946626573,75.5589722614061,
18.5636320093352));
#253718=CARTESIAN_POINT('Ctrl Pts',(-25.9524451451234,75.5204260075582,
18.6412309225863));
#253719=CARTESIAN_POINT('Ctrl Pts',(-26.0094901709642,75.4938857632365,
18.6946600865436));
#253720=CARTESIAN_POINT('Ctrl Pts',(-26.0681509448603,75.4669777563056,
18.746035575097));
#253721=CARTESIAN_POINT('Ctrl Pts',(-26.1282299623944,75.4397648602322,
18.7953196528862));
#253722=CARTESIAN_POINT('Ctrl Pts',(-26.1997874751994,75.4073527596494,
18.8540197810214));
#253723=CARTESIAN_POINT('Ctrl Pts',(-26.2732030109633,75.374575465988,18.909646548187));
#253724=CARTESIAN_POINT('Ctrl Pts',(-26.3483201939313,75.341453311566,18.962331304316));
#253725=CARTESIAN_POINT('Ctrl Pts',(-26.4206512997561,75.3095596493973,
19.0130619962875));
#253726=CARTESIAN_POINT('Ctrl Pts',(-26.4945609623652,75.2773460198525,
19.0610645954997));
#253727=CARTESIAN_POINT('Ctrl Pts',(-26.5699313482712,75.2448262662941,
19.1064165126252));
#253728=CARTESIAN_POINT('Ctrl Pts',(-26.5774516031997,75.2415815325166,
19.1109416052617));
#253729=CARTESIAN_POINT('Ctrl Pts',(-26.5849903403349,75.238332090922,19.1154422462802));
#253730=CARTESIAN_POINT('Ctrl Pts',(-26.5925473515409,75.2350780060009,
19.1199184134199));
#253731=CARTESIAN_POINT('Ctrl Pts',(-26.7154431586983,75.1821584876839,
19.1927120296535));
#253732=CARTESIAN_POINT('Ctrl Pts',(-26.8429293003596,75.1281185031954,
19.2588649121235));
#253733=CARTESIAN_POINT('Ctrl Pts',(-26.9733752019168,75.0735400782349,
19.3179719516907));
#253734=CARTESIAN_POINT('Ctrl Pts',(-27.0676510755531,75.0340951540677,
19.3606897966114));
#253735=CARTESIAN_POINT('Ctrl Pts',(-27.1634716618128,74.9943693681411,
19.3997280200329));
#253736=CARTESIAN_POINT('Ctrl Pts',(-27.2602089524345,74.9545859173702,
19.4349442290443));
#253737=CARTESIAN_POINT('Ctrl Pts',(-27.3823989937776,74.9043349597176,
19.4794262484123));
#253738=CARTESIAN_POINT('Ctrl Pts',(-27.5061040086162,74.85395915675,19.517975099683));
#253739=CARTESIAN_POINT('Ctrl Pts',(-27.6312030307085,74.8034579087233,
19.5507626191466));
#253740=CARTESIAN_POINT('Ctrl Pts',(-27.7301373583959,74.7635190911585,
19.5766925676019));
#253741=CARTESIAN_POINT('Ctrl Pts',(-27.829805833627,74.7235572548823,19.5989868615588));
#253742=CARTESIAN_POINT('Ctrl Pts',(-27.9303548227061,74.6834885518219,
19.61779172406));
#253743=CARTESIAN_POINT('Ctrl Pts',(-27.9505099136077,74.6754567619463,
19.621561167359));
#253744=CARTESIAN_POINT('Ctrl Pts',(-27.9707004214913,74.6674206749929,
19.6251902405012));
#253745=CARTESIAN_POINT('Ctrl Pts',(-27.9909275808283,74.6593796105368,
19.6286798784687));
#253746=CARTESIAN_POINT('Ctrl Pts',(-28.0921856244414,74.6191256904572,
19.6461491586393));
#253747=CARTESIAN_POINT('Ctrl Pts',(-28.1946046459662,74.578657249514,19.6600683967018));
#253748=CARTESIAN_POINT('Ctrl Pts',(-28.2976765638612,74.5381640664798,
19.6704349274694));
#253749=CARTESIAN_POINT('Ctrl Pts',(-28.3951370915022,74.4998753932411,
19.6802370887083));
#253750=CARTESIAN_POINT('Ctrl Pts',(-28.4931826135307,74.4615641517711,
19.6868624470815));
#253751=CARTESIAN_POINT('Ctrl Pts',(-28.5913692277015,74.4233988532873,
19.6902666744795));
#253752=CARTESIAN_POINT('Ctrl Pts',(-28.6428959768779,74.4033703211006,
19.6920531580318));
#253753=CARTESIAN_POINT('Ctrl Pts',(-28.6944612286795,74.3833821576526,
19.6929518677509));
#253754=CARTESIAN_POINT('Ctrl Pts',(-28.7459974181805,74.3634602878983,
19.6929518677509));
#253755=CARTESIAN_POINT('',(-74.3634602878982,28.7459974181806,19.6929518677509));
#253756=CARTESIAN_POINT('Origin',(0.,0.,19.6929518677509));
#253757=CARTESIAN_POINT('',(-75.9614881812303,25.1183521036896,17.4075636545403));
#253758=CARTESIAN_POINT('Ctrl Pts',(-74.3634602878982,28.7459974181806,
19.6929518677509));
#253759=CARTESIAN_POINT('Ctrl Pts',(-74.4304701497097,28.5726485820852,
19.6929518674577));
#253760=CARTESIAN_POINT('Ctrl Pts',(-74.4974864004038,28.4008490217909,
19.6830632277882));
#253761=CARTESIAN_POINT('Ctrl Pts',(-74.5645845522744,28.230491093491,19.6632610083017));
#253762=CARTESIAN_POINT('Ctrl Pts',(-74.5954989334108,28.1520014514031,
19.6541374580476));
#253763=CARTESIAN_POINT('Ctrl Pts',(-74.6264307043179,28.0738178940494,
19.6429087822487));
#253764=CARTESIAN_POINT('Ctrl Pts',(-74.6573872842513,27.9959302213503,
19.6295688156876));
#253765=CARTESIAN_POINT('Ctrl Pts',(-74.7058182219457,27.8740765465654,
19.6086987101799));
#253766=CARTESIAN_POINT('Ctrl Pts',(-74.7545517359242,27.7523615725077,
19.5824195541812));
#253767=CARTESIAN_POINT('Ctrl Pts',(-74.8031494822237,27.6319739934802,
19.5508884666966));
#253768=CARTESIAN_POINT('Ctrl Pts',(-74.8536551827056,27.5068599815951,
19.5181194643944));
#253769=CARTESIAN_POINT('Ctrl Pts',(-74.9040895744662,27.3829937092191,
19.4796267591557));
#253770=CARTESIAN_POINT('Ctrl Pts',(-74.9539558516285,27.2617318168035,
19.4355274341624));
#253771=CARTESIAN_POINT('Ctrl Pts',(-75.0221597822451,27.0958774926508,
19.3752111748938));
#253772=CARTESIAN_POINT('Ctrl Pts',(-75.0893730482371,26.934659238125,19.3046526921904));
#253773=CARTESIAN_POINT('Ctrl Pts',(-75.1556896641871,26.7783260032606,
19.223220896943));
#253774=CARTESIAN_POINT('Ctrl Pts',(-75.1820881660236,26.7160947942557,
19.1908055306641));
#253775=CARTESIAN_POINT('Ctrl Pts',(-75.2083445589399,26.6546378725531,
19.1566666832221));
#253776=CARTESIAN_POINT('Ctrl Pts',(-75.2344646706147,26.5939718531098,
19.120762400072));
#253777=CARTESIAN_POINT('Ctrl Pts',(-75.2368117983606,26.5885204638033,
19.1175360762251));
#253778=CARTESIAN_POINT('Ctrl Pts',(-75.2391574108363,26.5830764322048,
19.1142960456888));
#253779=CARTESIAN_POINT('Ctrl Pts',(-75.2415015097605,26.5776397722412,
19.1110422978748));
#253780=CARTESIAN_POINT('Ctrl Pts',(-75.2885743789447,26.4684638408701,
19.04570237402));
#253781=CARTESIAN_POINT('Ctrl Pts',(-75.3350350763048,26.3622811063522,
18.9747887273505));
#253782=CARTESIAN_POINT('Ctrl Pts',(-75.3808870959315,26.2593455383137,
18.8979255800988));
#253783=CARTESIAN_POINT('Ctrl Pts',(-75.4159393644213,26.1806548896268,
18.839166387017));
#253784=CARTESIAN_POINT('Ctrl Pts',(-75.4508169508407,26.1034760636233,
18.7765523191411));
#253785=CARTESIAN_POINT('Ctrl Pts',(-75.4849716254452,26.0291438153088,
18.7109347212577));
#253786=CARTESIAN_POINT('Ctrl Pts',(-75.4957791231815,26.0056230055015,
18.6901714714594));
#253787=CARTESIAN_POINT('Ctrl Pts',(-75.5065143688567,25.9823868773644,
18.6691073534833));
#253788=CARTESIAN_POINT('Ctrl Pts',(-75.5171603678616,25.959476755343,18.6477689489594));
#253789=CARTESIAN_POINT('Ctrl Pts',(-75.5571222432613,25.8734790541222,
18.5676710020756));
#253790=CARTESIAN_POINT('Ctrl Pts',(-75.5958350863705,25.7920071322344,
18.4838572390432));
#253791=CARTESIAN_POINT('Ctrl Pts',(-75.6333036881582,25.7152212809698,
18.3962512683447));
#253792=CARTESIAN_POINT('Ctrl Pts',(-75.6638282493733,25.6526661199667,
18.3248812761963));
#253793=CARTESIAN_POINT('Ctrl Pts',(-75.6936006486774,25.5930696741659,
18.2508225083577));
#253794=CARTESIAN_POINT('Ctrl Pts',(-75.7225799270827,25.5366139960004,
18.1741082109009));
#253795=CARTESIAN_POINT('Ctrl Pts',(-75.7376547710952,25.5072460962874,
18.1342019008987));
#253796=CARTESIAN_POINT('Ctrl Pts',(-75.7525151457545,25.4787274775003,
18.0935775396257));
#253797=CARTESIAN_POINT('Ctrl Pts',(-75.7671562637947,25.4510796000904,
18.0522434478428));
#253798=CARTESIAN_POINT('Ctrl Pts',(-75.7807604869782,25.4253897658985,
18.0138366671474));
#253799=CARTESIAN_POINT('Ctrl Pts',(-75.7942007247961,25.4004235947553,
17.9746913116853));
#253800=CARTESIAN_POINT('Ctrl Pts',(-75.807444674672,25.3762475819474,17.9349066213656));
#253801=CARTESIAN_POINT('Ctrl Pts',(-75.8430230238117,25.3113015022245,
17.8280296235003));
#253802=CARTESIAN_POINT('Ctrl Pts',(-75.8774043151913,25.2516721229845,
17.7158399467672));
#253803=CARTESIAN_POINT('Ctrl Pts',(-75.9100163344796,25.198659621202,17.5997892951994));
#253804=CARTESIAN_POINT('Ctrl Pts',(-75.9277247353295,25.1698737118314,
17.5367735267276));
#253805=CARTESIAN_POINT('Ctrl Pts',(-75.944911203035,25.1430395031978,17.4726196431217));
#253806=CARTESIAN_POINT('Ctrl Pts',(-75.961482015185,25.1183707693644,17.4075627905746));
#253807=CARTESIAN_POINT('Ctrl Pts',(-75.9614890268773,25.1183452685092,
17.4075745924872));
#253808=CARTESIAN_POINT('Ctrl Pts',(-75.9867559935951,24.9826881607244,
17.5590635300833));
#253809=CARTESIAN_POINT('Ctrl Pts',(-76.0139038233425,24.8421318546272,
17.7056692315459));
#253810=CARTESIAN_POINT('Ctrl Pts',(-76.0424582864102,24.6976449919804,
17.8479876921334));
#253811=CARTESIAN_POINT('',(-75.961488153786,-25.11835232551,17.4075632995853));
#253812=CARTESIAN_POINT('Ctrl Pts',(-76.0424582864102,-24.6976449919803,
17.8479876921334));
#253813=CARTESIAN_POINT('Ctrl Pts',(-76.0139038233691,-24.8421318545712,
17.7056692314804));
#253814=CARTESIAN_POINT('Ctrl Pts',(-75.9867559935943,-24.9826881607289,
17.5590635300785));
#253815=CARTESIAN_POINT('Ctrl Pts',(-75.9614890268762,-25.118345268511,
17.4075745924919));
#253816=CARTESIAN_POINT('',(-74.3634602878982,-28.7459974181806,19.6929518677509));
#253817=CARTESIAN_POINT('Ctrl Pts',(-75.9614818429679,-25.1183716157475,
17.4075624145233));
#253818=CARTESIAN_POINT('Ctrl Pts',(-75.929230600401,-25.166380740355,17.5341891960889));
#253819=CARTESIAN_POINT('Ctrl Pts',(-75.8946388507298,-25.2225896116613,
17.6574709250598));
#253820=CARTESIAN_POINT('Ctrl Pts',(-75.8583098126379,-25.2856234361605,
17.7758260770059));
#253821=CARTESIAN_POINT('Ctrl Pts',(-75.8416899062786,-25.314460320253,
17.8299715112316));
#253822=CARTESIAN_POINT('Ctrl Pts',(-75.8247061544494,-25.3447263486535,
17.8830859081576));
#253823=CARTESIAN_POINT('Ctrl Pts',(-75.8074152517245,-25.376293226511,
17.9350176026265));
#253824=CARTESIAN_POINT('Ctrl Pts',(-75.7951032719375,-25.3987704082004,
17.9719955431528));
#253825=CARTESIAN_POINT('Ctrl Pts',(-75.782622566375,-25.4219292775783,
18.0084169806878));
#253826=CARTESIAN_POINT('Ctrl Pts',(-75.7699942838137,-25.4457245653082,
18.0442185658031));
#253827=CARTESIAN_POINT('Ctrl Pts',(-75.7318190723905,-25.5176575566357,
18.1524465116398));
#253828=CARTESIAN_POINT('Ctrl Pts',(-75.6922139916809,-25.5954180174015,
18.2556268050704));
#253829=CARTESIAN_POINT('Ctrl Pts',(-75.6512007482183,-25.6787085177782,
18.3538912520706));
#253830=CARTESIAN_POINT('Ctrl Pts',(-75.6450787451602,-25.6911412018325,
18.3685590811484));
#253831=CARTESIAN_POINT('Ctrl Pts',(-75.6389253810504,-25.7036970321842,
18.3831174413404));
#253832=CARTESIAN_POINT('Ctrl Pts',(-75.6327407433448,-25.7163749474321,
18.3975668354582));
#253833=CARTESIAN_POINT('Ctrl Pts',(-75.5964231169443,-25.7908226049064,
18.482417027541));
#253834=CARTESIAN_POINT('Ctrl Pts',(-75.5589722614058,-25.8695946626581,
18.5636320093358));
#253835=CARTESIAN_POINT('Ctrl Pts',(-75.5204260075577,-25.9524451451245,
18.6412309225872));
#253836=CARTESIAN_POINT('Ctrl Pts',(-75.4938857632362,-26.009490170965,
18.6946600865442));
#253837=CARTESIAN_POINT('Ctrl Pts',(-75.4669777563054,-26.0681509448607,
18.7460355750973));
#253838=CARTESIAN_POINT('Ctrl Pts',(-75.4397648602322,-26.1282299623944,
18.7953196528863));
#253839=CARTESIAN_POINT('Ctrl Pts',(-75.4073527596456,-26.1997874752078,
18.8540197810283));
#253840=CARTESIAN_POINT('Ctrl Pts',(-75.3745754659803,-26.2732030109805,
18.9096465482));
#253841=CARTESIAN_POINT('Ctrl Pts',(-75.3414533115544,-26.3483201939576,
18.9623313043344));
#253842=CARTESIAN_POINT('Ctrl Pts',(-75.3095596493893,-26.4206512997743,
19.0130619962993));
#253843=CARTESIAN_POINT('Ctrl Pts',(-75.2773460198483,-26.4945609623749,
19.0610645955056));
#253844=CARTESIAN_POINT('Ctrl Pts',(-75.2448262662937,-26.5699313482721,
19.1064165126258));
#253845=CARTESIAN_POINT('Ctrl Pts',(-75.2415815325164,-26.5774516032003,
19.1109416052622));
#253846=CARTESIAN_POINT('Ctrl Pts',(-75.2383320909218,-26.5849903403352,
19.1154422462805));
#253847=CARTESIAN_POINT('Ctrl Pts',(-75.2350780060008,-26.5925473515409,
19.11991841342));
#253848=CARTESIAN_POINT('Ctrl Pts',(-75.1821584877111,-26.715443158635,
19.1927120296162));
#253849=CARTESIAN_POINT('Ctrl Pts',(-75.1281185032508,-26.8429293002287,
19.2588649120556));
#253850=CARTESIAN_POINT('Ctrl Pts',(-75.073540078319,-26.9733752017158,
19.3179719515996));
#253851=CARTESIAN_POINT('Ctrl Pts',(-75.0340951541239,-27.0676510754174,
19.360689796556));
#253852=CARTESIAN_POINT('Ctrl Pts',(-74.994369368169,-27.1634716617447,
19.3997280200081));
#253853=CARTESIAN_POINT('Ctrl Pts',(-74.9545859173699,-27.2602089524353,
19.4349442290446));
#253854=CARTESIAN_POINT('Ctrl Pts',(-74.9043349597174,-27.3823989937779,
19.4794262484125));
#253855=CARTESIAN_POINT('Ctrl Pts',(-74.8539591567499,-27.5061040086164,
19.517975099683));
#253856=CARTESIAN_POINT('Ctrl Pts',(-74.8034579087233,-27.6312030307086,
19.5507626191466));
#253857=CARTESIAN_POINT('Ctrl Pts',(-74.7635190911554,-27.7301373584036,
19.5766925676039));
#253858=CARTESIAN_POINT('Ctrl Pts',(-74.723557254876,-27.8298058336428,
19.5989868615623));
#253859=CARTESIAN_POINT('Ctrl Pts',(-74.6834885518123,-27.9303548227301,
19.6177917240647));
#253860=CARTESIAN_POINT('Ctrl Pts',(-74.6754567619398,-27.9505099136238,
19.6215611673621));
#253861=CARTESIAN_POINT('Ctrl Pts',(-74.6674206749895,-27.9707004214996,
19.6251902405029));
#253862=CARTESIAN_POINT('Ctrl Pts',(-74.6593796105366,-27.9909275808286,
19.6286798784691));
#253863=CARTESIAN_POINT('Ctrl Pts',(-74.6191256904534,-28.0921856244508,
19.6461491586415));
#253864=CARTESIAN_POINT('Ctrl Pts',(-74.5786572495067,-28.1946046459843,
19.6600683967049));
#253865=CARTESIAN_POINT('Ctrl Pts',(-74.5381640664692,-28.2976765638881,
19.6704349274727));
#253866=CARTESIAN_POINT('Ctrl Pts',(-74.4998753932249,-28.3951370915433,
19.6802370887123));
#253867=CARTESIAN_POINT('Ctrl Pts',(-74.4615641517495,-28.4931826135859,
19.6868624470852));
#253868=CARTESIAN_POINT('Ctrl Pts',(-74.4233988532603,-28.5913692277709,
19.690266674482));
#253869=CARTESIAN_POINT('Ctrl Pts',(-74.4033703210826,-28.6428959769242,
19.6920531580326));
#253870=CARTESIAN_POINT('Ctrl Pts',(-74.3833821576437,-28.6944612287026,
19.6929518677509));
#253871=CARTESIAN_POINT('Ctrl Pts',(-74.3634602878982,-28.7459974181806,
19.6929518677509));
#253872=CARTESIAN_POINT('',(-28.7459974181806,-74.3634602878982,19.6929518677509));
#253873=CARTESIAN_POINT('Origin',(0.,0.,19.6929518677509));
#253874=CARTESIAN_POINT('',(-25.1183521036895,-75.9614881812303,17.4075636545405));
#253875=CARTESIAN_POINT('Ctrl Pts',(-28.7459974181806,-74.3634602878982,
19.6929518677509));
#253876=CARTESIAN_POINT('Ctrl Pts',(-28.572648582161,-74.4304701496804,
19.6929518674578));
#253877=CARTESIAN_POINT('Ctrl Pts',(-28.4008490219403,-74.4974864003456,
19.6830632277964));
#253878=CARTESIAN_POINT('Ctrl Pts',(-28.2304910937134,-74.5645845521869,
19.6632610083272));
#253879=CARTESIAN_POINT('Ctrl Pts',(-28.1520014515506,-74.5954989333525,
19.6541374580684));
#253880=CARTESIAN_POINT('Ctrl Pts',(-28.0738178941228,-74.6264307042887,
19.642908782261));
#253881=CARTESIAN_POINT('Ctrl Pts',(-27.9959302213503,-74.6573872842512,
19.6295688156876));
#253882=CARTESIAN_POINT('Ctrl Pts',(-27.8740765465656,-74.7058182219456,
19.6086987101803));
#253883=CARTESIAN_POINT('Ctrl Pts',(-27.752361572508,-74.7545517359241,
19.5824195541813));
#253884=CARTESIAN_POINT('Ctrl Pts',(-27.6319739934803,-74.8031494822237,
19.5508884666964));
#253885=CARTESIAN_POINT('Ctrl Pts',(-27.5068599815953,-74.8536551827056,
19.518119464394));
#253886=CARTESIAN_POINT('Ctrl Pts',(-27.3829937092195,-74.9040895744661,
19.4796267591552));
#253887=CARTESIAN_POINT('Ctrl Pts',(-27.2617318168035,-74.9539558516285,
19.4355274341625));
#253888=CARTESIAN_POINT('Ctrl Pts',(-27.0958774930693,-75.0221597820729,
19.375211175047));
#253889=CARTESIAN_POINT('Ctrl Pts',(-26.9346592389393,-75.0893730478975,
19.3046526925474));
#253890=CARTESIAN_POINT('Ctrl Pts',(-26.7783260044453,-75.1556896636845,
19.2232208975604));
#253891=CARTESIAN_POINT('Ctrl Pts',(-26.7160947950356,-75.1820881656904,
19.1908055310976));
#253892=CARTESIAN_POINT('Ctrl Pts',(-26.654637872938,-75.2083445587741,
19.15666668345));
#253893=CARTESIAN_POINT('Ctrl Pts',(-26.5939718531098,-75.2344646706147,
19.1207624000721));
#253894=CARTESIAN_POINT('Ctrl Pts',(-26.5885204638033,-75.2368117983606,
19.1175360762252));
#253895=CARTESIAN_POINT('Ctrl Pts',(-26.5830764322048,-75.2391574108363,
19.114296045689));
#253896=CARTESIAN_POINT('Ctrl Pts',(-26.5776397722412,-75.2415015097604,
19.1110422978749));
#253897=CARTESIAN_POINT('Ctrl Pts',(-26.4684638408705,-75.2885743789445,
19.0457023740205));
#253898=CARTESIAN_POINT('Ctrl Pts',(-26.3622811063516,-75.3350350763051,
18.9747887273497));
#253899=CARTESIAN_POINT('Ctrl Pts',(-26.2593455383138,-75.3808870959315,
18.8979255800989));
#253900=CARTESIAN_POINT('Ctrl Pts',(-26.1806548896459,-75.4159393644128,
18.8391663870316));
#253901=CARTESIAN_POINT('Ctrl Pts',(-26.1034760636602,-75.450816950824,
18.7765523191711));
#253902=CARTESIAN_POINT('Ctrl Pts',(-26.0291438153621,-75.4849716254206,
18.7109347213048));
#253903=CARTESIAN_POINT('Ctrl Pts',(-26.0056230055367,-75.4957791231653,
18.6901714714912));
#253904=CARTESIAN_POINT('Ctrl Pts',(-25.9823868773818,-75.5065143688487,
18.6691073534994));
#253905=CARTESIAN_POINT('Ctrl Pts',(-25.9594767553431,-75.5171603678615,
18.6477689489594));
#253906=CARTESIAN_POINT('Ctrl Pts',(-25.8734790541225,-75.5571222432612,
18.5676710020758));
#253907=CARTESIAN_POINT('Ctrl Pts',(-25.7920071322347,-75.5958350863704,
18.4838572390434));
#253908=CARTESIAN_POINT('Ctrl Pts',(-25.7152212809698,-75.6333036881581,
18.3962512683447));
#253909=CARTESIAN_POINT('Ctrl Pts',(-25.6526661199683,-75.6638282493725,
18.3248812761982));
#253910=CARTESIAN_POINT('Ctrl Pts',(-25.5930696741688,-75.6936006486759,
18.2508225083616));
#253911=CARTESIAN_POINT('Ctrl Pts',(-25.5366139960046,-75.7225799270805,
18.174108210907));
#253912=CARTESIAN_POINT('Ctrl Pts',(-25.5072460962901,-75.7376547710937,
18.1342019009029));
#253913=CARTESIAN_POINT('Ctrl Pts',(-25.4787274775015,-75.7525151457539,
18.0935775396279));
#253914=CARTESIAN_POINT('Ctrl Pts',(-25.4510796000903,-75.7671562637947,
18.052243447843));
#253915=CARTESIAN_POINT('Ctrl Pts',(-25.4253897658985,-75.7807604869782,
18.0138366671475));
#253916=CARTESIAN_POINT('Ctrl Pts',(-25.4004235947553,-75.7942007247961,
17.9746913116854));
#253917=CARTESIAN_POINT('Ctrl Pts',(-25.3762475819473,-75.807444674672,
17.9349066213656));
#253918=CARTESIAN_POINT('Ctrl Pts',(-25.3113015022286,-75.8430230238094,
17.8280296235075));
#253919=CARTESIAN_POINT('Ctrl Pts',(-25.2516721229916,-75.877404315187,
17.7158399467825));
#253920=CARTESIAN_POINT('Ctrl Pts',(-25.1986596212116,-75.9100163344733,
17.599789295223));
#253921=CARTESIAN_POINT('Ctrl Pts',(-25.1698737118368,-75.9277247353256,
17.5367735267439));
#253922=CARTESIAN_POINT('Ctrl Pts',(-25.1430395031998,-75.9449112030332,
17.4726196431301));
#253923=CARTESIAN_POINT('Ctrl Pts',(-25.1183707693638,-75.9614820151852,
17.4075627905749));
#253924=CARTESIAN_POINT('',(-24.6976449920628,-76.0424582863717,17.8479876922246));
#253925=CARTESIAN_POINT('Ctrl Pts',(-25.1183452685093,-75.9614890268773,
17.4075745924872));
#253926=CARTESIAN_POINT('Ctrl Pts',(-24.9826881607245,-75.9867559935951,
17.5590635300832));
#253927=CARTESIAN_POINT('Ctrl Pts',(-24.8421318546858,-76.0139038233151,
17.7056692316105));
#253928=CARTESIAN_POINT('Ctrl Pts',(-24.6976449919805,-76.0424582864102,
17.8479876921332));
#253929=CARTESIAN_POINT('',(24.6976449920629,-76.0424582863716,17.8479876922249));
#253930=CARTESIAN_POINT('Origin',(0.,0.,17.8479876926671));
#253931=CARTESIAN_POINT('',(25.1183523255102,-75.961488153786,17.4075632995852));
#253932=CARTESIAN_POINT('Ctrl Pts',(24.6976449919804,-76.0424582864102,
17.8479876921333));
#253933=CARTESIAN_POINT('Ctrl Pts',(24.8421318545421,-76.0139038233827,
17.705669231448));
#253934=CARTESIAN_POINT('Ctrl Pts',(24.982688160729,-75.9867559935942,17.5590635300786));
#253935=CARTESIAN_POINT('Ctrl Pts',(25.118345268511,-75.9614890268762,17.4075745924918));
#253936=CARTESIAN_POINT('',(28.7459974181806,-74.3634602878982,19.6929518677509));
#253937=CARTESIAN_POINT('Ctrl Pts',(25.1183716157476,-75.9614818429679,
17.4075624145231));
#253938=CARTESIAN_POINT('Ctrl Pts',(25.1663807403153,-75.9292306004278,
17.5341891959829));
#253939=CARTESIAN_POINT('Ctrl Pts',(25.2225896115677,-75.8946388507875,
17.6574709248538));
#253940=CARTESIAN_POINT('Ctrl Pts',(25.2856234360028,-75.8583098127289,
17.7758260767094));
#253941=CARTESIAN_POINT('Ctrl Pts',(25.3144603201426,-75.8416899063406,
17.8299715110377));
#253942=CARTESIAN_POINT('Ctrl Pts',(25.3447263485959,-75.8247061544809,
17.8830859080628));
#253943=CARTESIAN_POINT('Ctrl Pts',(25.376293226511,-75.8074152517246,17.9350176026264));
#253944=CARTESIAN_POINT('Ctrl Pts',(25.3987704082003,-75.7951032719376,
17.9719955431527));
#253945=CARTESIAN_POINT('Ctrl Pts',(25.4219292775783,-75.7826225663751,
18.0084169806877));
#253946=CARTESIAN_POINT('Ctrl Pts',(25.4457245653082,-75.7699942838137,
18.0442185658029));
#253947=CARTESIAN_POINT('Ctrl Pts',(25.5176575565964,-75.7318190724114,
18.1524465115804));
#253948=CARTESIAN_POINT('Ctrl Pts',(25.5954180173166,-75.6922139917242,
18.2556268049576));
#253949=CARTESIAN_POINT('Ctrl Pts',(25.6787085176417,-75.6512007482855,
18.3538912519095));
#253950=CARTESIAN_POINT('Ctrl Pts',(25.6911412017406,-75.6450787452052,
18.3685590810418));
#253951=CARTESIAN_POINT('Ctrl Pts',(25.7036970321378,-75.638925381073,18.3831174412875));
#253952=CARTESIAN_POINT('Ctrl Pts',(25.7163749474321,-75.6327407433448,
18.3975668354581));
#253953=CARTESIAN_POINT('Ctrl Pts',(25.7908226049063,-75.5964231169443,
18.4824170275409));
#253954=CARTESIAN_POINT('Ctrl Pts',(25.8695946626579,-75.5589722614059,
18.5636320093358));
#253955=CARTESIAN_POINT('Ctrl Pts',(25.9524451451245,-75.5204260075577,
18.6412309225871));
#253956=CARTESIAN_POINT('Ctrl Pts',(26.009490170965,-75.4938857632362,18.6946600865441));
#253957=CARTESIAN_POINT('Ctrl Pts',(26.0681509448606,-75.4669777563054,
18.7460355750972));
#253958=CARTESIAN_POINT('Ctrl Pts',(26.1282299623944,-75.4397648602322,
18.7953196528862));
#253959=CARTESIAN_POINT('Ctrl Pts',(26.1997874752161,-75.4073527596418,
18.8540197810352));
#253960=CARTESIAN_POINT('Ctrl Pts',(26.2732030109977,-75.3745754659727,
18.9096465482131));
#253961=CARTESIAN_POINT('Ctrl Pts',(26.3483201939841,-75.3414533115427,
18.962331304353));
#253962=CARTESIAN_POINT('Ctrl Pts',(26.4206512997923,-75.3095596493815,
19.013061996311));
#253963=CARTESIAN_POINT('Ctrl Pts',(26.4945609623841,-75.2773460198444,
19.061064595511));
#253964=CARTESIAN_POINT('Ctrl Pts',(26.5699313482722,-75.2448262662937,
19.1064165126255));
#253965=CARTESIAN_POINT('Ctrl Pts',(26.5774516032003,-75.2415815325164,
19.1109416052619));
#253966=CARTESIAN_POINT('Ctrl Pts',(26.5849903403353,-75.2383320909218,
19.1154422462802));
#253967=CARTESIAN_POINT('Ctrl Pts',(26.592547351541,-75.2350780060008,19.1199184134197));
#253968=CARTESIAN_POINT('Ctrl Pts',(26.7154431586624,-75.1821584876994,
19.1927120296318));
#253969=CARTESIAN_POINT('Ctrl Pts',(26.8429293002847,-75.1281185032271,
19.2588649120843));
#253970=CARTESIAN_POINT('Ctrl Pts',(26.9733752018017,-75.073540078283,19.3179719516384));
#253971=CARTESIAN_POINT('Ctrl Pts',(27.0676510754753,-75.0340951540999,
19.3606897965796));
#253972=CARTESIAN_POINT('Ctrl Pts',(27.1634716617737,-74.9943693681571,
19.3997280200187));
#253973=CARTESIAN_POINT('Ctrl Pts',(27.2602089524352,-74.9545859173699,
19.4349442290445));
#253974=CARTESIAN_POINT('Ctrl Pts',(27.3823989937782,-74.9043349597173,
19.4794262484125));
#253975=CARTESIAN_POINT('Ctrl Pts',(27.5061040086165,-74.8539591567499,
19.517975099683));
#253976=CARTESIAN_POINT('Ctrl Pts',(27.6312030307086,-74.8034579087233,
19.5507626191466));
#253977=CARTESIAN_POINT('Ctrl Pts',(27.7301373584037,-74.7635190911554,
19.5766925676039));
#253978=CARTESIAN_POINT('Ctrl Pts',(27.829805833643,-74.7235572548759,19.5989868615624));
#253979=CARTESIAN_POINT('Ctrl Pts',(27.9303548227305,-74.6834885518121,
19.6177917240647));
#253980=CARTESIAN_POINT('Ctrl Pts',(27.9505099136241,-74.6754567619397,
19.6215611673621));
#253981=CARTESIAN_POINT('Ctrl Pts',(27.9707004214997,-74.6674206749895,
19.6251902405028));
#253982=CARTESIAN_POINT('Ctrl Pts',(27.9909275808286,-74.6593796105366,
19.628679878469));
#253983=CARTESIAN_POINT('Ctrl Pts',(28.0921856244513,-74.6191256904532,
19.6461491586415));
#253984=CARTESIAN_POINT('Ctrl Pts',(28.1946046459851,-74.5786572495064,
19.6600683967049));
#253985=CARTESIAN_POINT('Ctrl Pts',(28.297676563889,-74.5381640664688,19.6704349274727));
#253986=CARTESIAN_POINT('Ctrl Pts',(28.3951370915476,-74.4998753932232,
19.6802370887127));
#253987=CARTESIAN_POINT('Ctrl Pts',(28.4931826135935,-74.4615641517465,
19.6868624470857));
#253988=CARTESIAN_POINT('Ctrl Pts',(28.5913692277819,-74.423398853256,19.6902666744824));
#253989=CARTESIAN_POINT('Ctrl Pts',(28.6428959769315,-74.4033703210798,
19.6920531580327));
#253990=CARTESIAN_POINT('Ctrl Pts',(28.6944612287063,-74.3833821576423,
19.6929518677509));
#253991=CARTESIAN_POINT('Ctrl Pts',(28.7459974181806,-74.3634602878982,
19.6929518677509));
#253992=CARTESIAN_POINT('',(74.3634602878983,-28.7459974181805,19.6929518677509));
#253993=CARTESIAN_POINT('Origin',(0.,0.,19.6929518677509));
#253994=CARTESIAN_POINT('',(75.9614881812303,-25.1183521036895,17.4075636545405));
#253995=CARTESIAN_POINT('Ctrl Pts',(74.3634602878983,-28.7459974181805,
19.6929518677509));
#253996=CARTESIAN_POINT('Ctrl Pts',(74.4304701497267,-28.5726485820409,
19.6929518674584));
#253997=CARTESIAN_POINT('Ctrl Pts',(74.4974864004376,-28.4008490217041,
19.6830632277838));
#253998=CARTESIAN_POINT('Ctrl Pts',(74.5645845523253,-28.2304910933617,
19.663261008287));
#253999=CARTESIAN_POINT('Ctrl Pts',(74.5954989334447,-28.1520014513173,
19.6541374580355));
#254000=CARTESIAN_POINT('Ctrl Pts',(74.6264307043348,-28.0738178940067,
19.6429087822414));
#254001=CARTESIAN_POINT('Ctrl Pts',(74.6573872842514,-27.9959302213499,
19.6295688156875));
#254002=CARTESIAN_POINT('Ctrl Pts',(74.705818221946,-27.8740765465647,19.6086987101797));
#254003=CARTESIAN_POINT('Ctrl Pts',(74.7545517359244,-27.7523615725074,
19.5824195541808));
#254004=CARTESIAN_POINT('Ctrl Pts',(74.8031494822237,-27.6319739934803,
19.5508884666962));
#254005=CARTESIAN_POINT('Ctrl Pts',(74.8536551827057,-27.5068599815951,
19.5181194643939));
#254006=CARTESIAN_POINT('Ctrl Pts',(74.9040895744663,-27.3829937092191,
19.479626759155));
#254007=CARTESIAN_POINT('Ctrl Pts',(74.9539558516288,-27.2617318168029,
19.4355274341618));
#254008=CARTESIAN_POINT('Ctrl Pts',(75.0221597822634,-27.0958774926063,
19.3752111748775));
#254009=CARTESIAN_POINT('Ctrl Pts',(75.0893730482725,-26.93465923804,19.3046526921532));
#254010=CARTESIAN_POINT('Ctrl Pts',(75.1556896642392,-26.7783260031378,
19.2232208968787));
#254011=CARTESIAN_POINT('Ctrl Pts',(75.1820881660582,-26.7160947941749,
19.1908055306188));
#254012=CARTESIAN_POINT('Ctrl Pts',(75.208344558957,-26.6546378725134,19.156666683198));
#254013=CARTESIAN_POINT('Ctrl Pts',(75.2344646706146,-26.5939718531102,
19.1207624000714));
#254014=CARTESIAN_POINT('Ctrl Pts',(75.2368117983607,-26.5885204638034,
19.1175360762244));
#254015=CARTESIAN_POINT('Ctrl Pts',(75.2391574108366,-26.5830764322045,
19.1142960456879));
#254016=CARTESIAN_POINT('Ctrl Pts',(75.2415015097608,-26.5776397722406,
19.1110422978736));
#254017=CARTESIAN_POINT('Ctrl Pts',(75.2885743789452,-26.4684638408694,
19.0457023740184));
#254018=CARTESIAN_POINT('Ctrl Pts',(75.3350350763051,-26.3622811063518,
18.9747887273492));
#254019=CARTESIAN_POINT('Ctrl Pts',(75.3808870959319,-26.2593455383128,
18.8979255800978));
#254020=CARTESIAN_POINT('Ctrl Pts',(75.415939364422,-26.1806548896252,18.839166387016));
#254021=CARTESIAN_POINT('Ctrl Pts',(75.4508169508416,-26.1034760636214,
18.7765523191393));
#254022=CARTESIAN_POINT('Ctrl Pts',(75.4849716254462,-26.0291438153065,
18.7109347212553));
#254023=CARTESIAN_POINT('Ctrl Pts',(75.4957791231824,-26.0056230054997,
18.6901714714573));
#254024=CARTESIAN_POINT('Ctrl Pts',(75.5065143688574,-25.9823868773631,
18.6691073534816));
#254025=CARTESIAN_POINT('Ctrl Pts',(75.517160367862,-25.9594767553421,18.6477689489581));
#254026=CARTESIAN_POINT('Ctrl Pts',(75.5571222432616,-25.8734790541217,
18.5676710020748));
#254027=CARTESIAN_POINT('Ctrl Pts',(75.5958350863706,-25.7920071322341,
18.4838572390429));
#254028=CARTESIAN_POINT('Ctrl Pts',(75.6333036881581,-25.7152212809698,
18.3962512683448));
#254029=CARTESIAN_POINT('Ctrl Pts',(75.6638282493716,-25.6526661199703,
18.3248812762004));
#254030=CARTESIAN_POINT('Ctrl Pts',(75.693600648674,-25.5930696741725,18.2508225083663));
#254031=CARTESIAN_POINT('Ctrl Pts',(75.7225799270778,-25.5366139960098,
18.1741082109142));
#254032=CARTESIAN_POINT('Ctrl Pts',(75.7376547710921,-25.5072460962931,
18.1342019009073));
#254033=CARTESIAN_POINT('Ctrl Pts',(75.7525151457534,-25.4787274775024,
18.0935775396293));
#254034=CARTESIAN_POINT('Ctrl Pts',(75.7671562637952,-25.4510796000893,
18.0522434478413));
#254035=CARTESIAN_POINT('Ctrl Pts',(75.7807604869785,-25.4253897658979,
18.0138366671463));
#254036=CARTESIAN_POINT('Ctrl Pts',(75.7942007247962,-25.4004235947552,
17.9746913116847));
#254037=CARTESIAN_POINT('Ctrl Pts',(75.8074446746719,-25.3762475819477,
17.9349066213655));
#254038=CARTESIAN_POINT('Ctrl Pts',(75.8430230238029,-25.3113015022408,
17.8280296235264));
#254039=CARTESIAN_POINT('Ctrl Pts',(75.8774043151745,-25.2516721230136,
17.7158399468224));
#254040=CARTESIAN_POINT('Ctrl Pts',(75.9100163344557,-25.1986596212405,
17.599789295285));
#254041=CARTESIAN_POINT('Ctrl Pts',(75.9277247353141,-25.169873711855,17.536773526786));
#254042=CARTESIAN_POINT('Ctrl Pts',(75.9449112030276,-25.1430395032083,
17.4726196431515));
#254043=CARTESIAN_POINT('Ctrl Pts',(75.9614820151851,-25.118370769364,17.4075627905749));
#254044=CARTESIAN_POINT('',(76.0424582863717,-24.6976449920627,17.8479876922247));
#254045=CARTESIAN_POINT('Ctrl Pts',(75.9614890268773,-25.1183452685093,
17.4075745924873));
#254046=CARTESIAN_POINT('Ctrl Pts',(75.9867559935951,-24.9826881607245,
17.5590635300833));
#254047=CARTESIAN_POINT('Ctrl Pts',(76.0139038233338,-24.8421318546458,
17.7056692315664));
#254048=CARTESIAN_POINT('Ctrl Pts',(76.0424582864102,-24.6976449919804,
17.8479876921334));
#254049=CARTESIAN_POINT('',(76.0424582863716,24.6976449920628,17.847987692225));
#254050=CARTESIAN_POINT('Origin',(0.,0.,17.8479876926672));
#254051=CARTESIAN_POINT('',(75.9614886121312,25.1183470986529,17.4075730861852));
#254052=CARTESIAN_POINT('Ctrl Pts',(76.0424582864102,24.6976449919803,17.8479876921334));
#254053=CARTESIAN_POINT('Ctrl Pts',(76.0139038233584,24.842131854594,17.7056692315056));
#254054=CARTESIAN_POINT('Ctrl Pts',(75.9867559935943,24.9826881607288,17.5590635300786));
#254055=CARTESIAN_POINT('Ctrl Pts',(75.9614890268762,25.118345268511,17.4075745924918));
#254056=CARTESIAN_POINT('',(74.3634602878983,28.7459974181805,19.6929518677509));
#254057=CARTESIAN_POINT('Ctrl Pts',(75.9614877926984,25.1183497610148,17.4075725136416));
#254058=CARTESIAN_POINT('Ctrl Pts',(75.9334021721091,25.1601393821171,17.5178916380196));
#254059=CARTESIAN_POINT('Ctrl Pts',(75.9035242097614,25.2082110521886,17.6256433855426));
#254060=CARTESIAN_POINT('Ctrl Pts',(75.8722717148825,25.2615872269752,17.729813441149));
#254061=CARTESIAN_POINT('Ctrl Pts',(75.8512336859029,25.2975181027767,17.7999368875218));
#254062=CARTESIAN_POINT('Ctrl Pts',(75.82957235286,25.3358539579438,17.8684375808773));
#254063=CARTESIAN_POINT('Ctrl Pts',(75.8074111030368,25.376308989996,17.9350062768217));
#254064=CARTESIAN_POINT('Ctrl Pts',(75.7908062731773,25.4066208600191,17.9848844145148));
#254065=CARTESIAN_POINT('Ctrl Pts',(75.7738886212226,25.4381799817096,18.0337776331664));
#254066=CARTESIAN_POINT('Ctrl Pts',(75.7567136591966,25.4708669570284,18.0815237295059));
#254067=CARTESIAN_POINT('Ctrl Pts',(75.7220283060228,25.5368792883161,18.1779484093214));
#254068=CARTESIAN_POINT('Ctrl Pts',(75.6861745408806,25.6076061824442,18.2703348362656));
#254069=CARTESIAN_POINT('Ctrl Pts',(75.6491774008247,25.6828197666451,18.3587322169221));
#254070=CARTESIAN_POINT('Ctrl Pts',(75.6437233302642,25.6939076559987,18.3717636445064));
#254071=CARTESIAN_POINT('Ctrl Pts',(75.6382444253436,25.7050929860443,18.3847084446968));
#254072=CARTESIAN_POINT('Ctrl Pts',(75.6327407805507,25.716374960082,18.3975668402832));
#254073=CARTESIAN_POINT('Ctrl Pts',(75.5926129031196,25.7986334793732,18.4913192791613));
#254074=CARTESIAN_POINT('Ctrl Pts',(75.5511297118698,25.8861084238851,18.5805817736278));
#254075=CARTESIAN_POINT('Ctrl Pts',(75.5083052747818,25.9785568613914,18.6654318615666));
#254076=CARTESIAN_POINT('Ctrl Pts',(75.4856855815722,26.0273877494613,18.7102493323495));
#254077=CARTESIAN_POINT('Ctrl Pts',(75.4628315387299,26.0773070493268,18.7535439863377));
#254078=CARTESIAN_POINT('Ctrl Pts',(75.4397654989299,26.1282310684057,18.7953186220858));
#254079=CARTESIAN_POINT('Ctrl Pts',(75.4062658488513,26.2021898768762,18.855989447761));
#254080=CARTESIAN_POINT('Ctrl Pts',(75.3723921489013,26.2780930526712,18.9133588584959));
#254081=CARTESIAN_POINT('Ctrl Pts',(75.3381414872632,26.355831091728,18.9675999514268));
#254082=CARTESIAN_POINT('Ctrl Pts',(75.304189114822,26.4328921097836,19.021368658387));
#254083=CARTESIAN_POINT('Ctrl Pts',(75.2698661738243,26.5117567910974,19.0720630469863));
#254084=CARTESIAN_POINT('Ctrl Pts',(75.2351662644524,26.5923393889176,19.1198058720703));
#254085=CARTESIAN_POINT('Ctrl Pts',(75.2351370428123,26.5924072494889,19.1198460774678));
#254086=CARTESIAN_POINT('Ctrl Pts',(75.2351078207906,26.5924751115546,19.1198862808855));
#254087=CARTESIAN_POINT('Ctrl Pts',(75.2350785983874,26.5925429751146,19.1199264823231));
#254088=CARTESIAN_POINT('Ctrl Pts',(75.183303568785,26.7127807873402,19.191153705159));
#254089=CARTESIAN_POINT('Ctrl Pts',(75.1304366076855,26.8374586955589,19.2560332970306));
#254090=CARTESIAN_POINT('Ctrl Pts',(75.0770544694664,26.9649752993357,19.3141613796794));
#254091=CARTESIAN_POINT('Ctrl Pts',(75.0342358129132,27.0672583821063,19.3607868332499));
#254092=CARTESIAN_POINT('Ctrl Pts',(74.9910861388835,27.1713664534818,19.4030689498303));
#254093=CARTESIAN_POINT('Ctrl Pts',(74.9479077551293,27.2764562548044,19.4408157537664));
#254094=CARTESIAN_POINT('Ctrl Pts',(74.8999079936204,27.3932805766512,19.4827774352636));
#254095=CARTESIAN_POINT('Ctrl Pts',(74.8517145421664,27.511651646086,19.5194081094312));
#254096=CARTESIAN_POINT('Ctrl Pts',(74.8034459183259,27.631202345934,19.5507462995563));
#254097=CARTESIAN_POINT('Ctrl Pts',(74.7565343276745,27.7473919748717,19.5812034418972));
#254098=CARTESIAN_POINT('Ctrl Pts',(74.7093890816425,27.865081171539,19.6068157552163));
#254099=CARTESIAN_POINT('Ctrl Pts',(74.6621501920651,27.9838718582653,19.6275204329004));
#254100=CARTESIAN_POINT('Ctrl Pts',(74.6123504464618,28.1091022781997,19.6493475268624));
#254101=CARTESIAN_POINT('Ctrl Pts',(74.562446729845,28.2355565734727,19.6657199755857));
#254102=CARTESIAN_POINT('Ctrl Pts',(74.5126081501712,28.3627441365293,19.6766210584599));
#254103=CARTESIAN_POINT('Ctrl Pts',(74.4627695704973,28.4899316995859,19.6875221413342));
#254104=CARTESIAN_POINT('Ctrl Pts',(74.412996284741,28.617851990473,19.6929518677509));
#254105=CARTESIAN_POINT('Ctrl Pts',(74.3634602878983,28.7459974181805,19.6929518677509));
#254106=CARTESIAN_POINT('',(28.7459974181806,74.3634602878982,19.6929518677509));
#254107=CARTESIAN_POINT('Origin',(0.,0.,19.6929518677508));
#254108=CARTESIAN_POINT('',(25.1183521036895,75.9614881812303,17.4075636545405));
#254109=CARTESIAN_POINT('Ctrl Pts',(28.7459974181806,74.3634602878982,19.6929518677509));
#254110=CARTESIAN_POINT('Ctrl Pts',(28.5726485821451,74.4304701496865,19.6929518674579));
#254111=CARTESIAN_POINT('Ctrl Pts',(28.4008490219087,74.4974864003579,19.6830632277949));
#254112=CARTESIAN_POINT('Ctrl Pts',(28.2304910936664,74.5645845522053,19.663261008322));
#254113=CARTESIAN_POINT('Ctrl Pts',(28.1520014515195,74.5954989333648,19.6541374580642));
#254114=CARTESIAN_POINT('Ctrl Pts',(28.0738178941073,74.6264307042949,19.6429087822585));
#254115=CARTESIAN_POINT('Ctrl Pts',(27.9959302213504,74.6573872842512,19.6295688156876));
#254116=CARTESIAN_POINT('Ctrl Pts',(27.8740765465657,74.7058182219455,19.6086987101801));
#254117=CARTESIAN_POINT('Ctrl Pts',(27.752361572508,74.7545517359241,19.5824195541812));
#254118=CARTESIAN_POINT('Ctrl Pts',(27.6319739934803,74.8031494822237,19.5508884666963));
#254119=CARTESIAN_POINT('Ctrl Pts',(27.5068599815954,74.8536551827056,19.5181194643941));
#254120=CARTESIAN_POINT('Ctrl Pts',(27.3829937092194,74.9040895744662,19.4796267591551));
#254121=CARTESIAN_POINT('Ctrl Pts',(27.2617318168037,74.9539558516285,19.435527434162));
#254122=CARTESIAN_POINT('Ctrl Pts',(27.0958774928492,75.0221597821636,19.3752111749656));
#254123=CARTESIAN_POINT('Ctrl Pts',(26.9346592385107,75.0893730480763,19.3046526923589));
#254124=CARTESIAN_POINT('Ctrl Pts',(26.7783260038218,75.1556896639491,19.2232208972347));
#254125=CARTESIAN_POINT('Ctrl Pts',(26.7160947946252,75.1820881658658,19.1908055308687));
#254126=CARTESIAN_POINT('Ctrl Pts',(26.6546378727357,75.2083445588614,19.1566666833293));
#254127=CARTESIAN_POINT('Ctrl Pts',(26.5939718531103,75.2344646706146,19.1207624000712));
#254128=CARTESIAN_POINT('Ctrl Pts',(26.5885204638038,75.2368117983605,19.1175360762244));
#254129=CARTESIAN_POINT('Ctrl Pts',(26.5830764322053,75.2391574108362,19.1142960456881));
#254130=CARTESIAN_POINT('Ctrl Pts',(26.5776397722417,75.2415015097603,19.111042297874));
#254131=CARTESIAN_POINT('Ctrl Pts',(26.4684638408709,75.2885743789445,19.045702374019));
#254132=CARTESIAN_POINT('Ctrl Pts',(26.3622811063523,75.3350350763049,18.9747887273491));
#254133=CARTESIAN_POINT('Ctrl Pts',(26.2593455383141,75.3808870959314,18.8979255800986));
#254134=CARTESIAN_POINT('Ctrl Pts',(26.1806548896519,75.4159393644101,18.8391663870361));
#254135=CARTESIAN_POINT('Ctrl Pts',(26.1034760636718,75.4508169508188,18.7765523191803));
#254136=CARTESIAN_POINT('Ctrl Pts',(26.0291438153788,75.484971625413,18.7109347213192));
#254137=CARTESIAN_POINT('Ctrl Pts',(26.0056230055477,75.4957791231602,18.6901714715009));
#254138=CARTESIAN_POINT('Ctrl Pts',(25.9823868773873,75.5065143688461,18.6691073535043));
#254139=CARTESIAN_POINT('Ctrl Pts',(25.9594767553432,75.5171603678615,18.6477689489594));
#254140=CARTESIAN_POINT('Ctrl Pts',(25.8734790541225,75.5571222432611,18.567671002076));
#254141=CARTESIAN_POINT('Ctrl Pts',(25.7920071322346,75.5958350863704,18.4838572390433));
#254142=CARTESIAN_POINT('Ctrl Pts',(25.7152212809698,75.6333036881581,18.3962512683447));
#254143=CARTESIAN_POINT('Ctrl Pts',(25.6526661199698,75.6638282493718,18.3248812761999));
#254144=CARTESIAN_POINT('Ctrl Pts',(25.5930696741718,75.6936006486744,18.2508225083648));
#254145=CARTESIAN_POINT('Ctrl Pts',(25.5366139960088,75.7225799270784,18.1741082109121));
#254146=CARTESIAN_POINT('Ctrl Pts',(25.5072460962929,75.7376547710924,18.1342019009063));
#254147=CARTESIAN_POINT('Ctrl Pts',(25.4787274775029,75.7525151457532,18.0935775396296));
#254148=CARTESIAN_POINT('Ctrl Pts',(25.4510796000904,75.7671562637946,18.052243447843));
#254149=CARTESIAN_POINT('Ctrl Pts',(25.4253897658984,75.7807604869782,18.0138366671477));
#254150=CARTESIAN_POINT('Ctrl Pts',(25.4004235947551,75.7942007247962,17.9746913116857));
#254151=CARTESIAN_POINT('Ctrl Pts',(25.376247581947,75.8074446746721,17.9349066213659));
#254152=CARTESIAN_POINT('Ctrl Pts',(25.3113015022871,75.8430230237772,17.8280296236051));
#254153=CARTESIAN_POINT('Ctrl Pts',(25.2516721230997,75.8774043151245,17.7158399469868));
#254154=CARTESIAN_POINT('Ctrl Pts',(25.198659621356,75.9100163343844,17.5997892955397));
#254155=CARTESIAN_POINT('Ctrl Pts',(25.1698737119266,75.9277247352681,17.5367735269588));
#254156=CARTESIAN_POINT('Ctrl Pts',(25.1430395032411,75.9449112030055,17.472619643239));
#254157=CARTESIAN_POINT('Ctrl Pts',(25.1183707693638,75.9614820151852,17.4075627905749));
#254158=CARTESIAN_POINT('',(24.6976449920628,76.0424582863717,17.8479876922246));
#254159=CARTESIAN_POINT('Ctrl Pts',(25.1183452685093,75.9614890268773,17.4075745924872));
#254160=CARTESIAN_POINT('Ctrl Pts',(24.9826881607244,75.9867559935951,17.5590635300832));
#254161=CARTESIAN_POINT('Ctrl Pts',(24.8421318546464,76.0139038233335,17.7056692315669));
#254162=CARTESIAN_POINT('Ctrl Pts',(24.6976449919804,76.0424582864102,17.8479876921332));
#254163=CARTESIAN_POINT('',(10.8641498708349,79.2111064053766,17.8479876926671));
#254164=CARTESIAN_POINT('Origin',(0.,0.,17.8479876926671));
#254165=CARTESIAN_POINT('Ctrl Pts',(10.8641498708349,79.2111064053766,17.8479876926671));
#254166=CARTESIAN_POINT('Ctrl Pts',(10.8639322809376,79.1070016560343,18.6882296805948));
#254167=CARTESIAN_POINT('Ctrl Pts',(10.8637138619226,79.0028933995443,19.5284712337854));
#254168=CARTESIAN_POINT('Ctrl Pts',(10.8634946042403,78.8987815953885,20.3687123471684));
#254169=CARTESIAN_POINT('Ctrl Pts',(10.8626175735112,78.4823343787045,23.7296768011912));
#254170=CARTESIAN_POINT('Ctrl Pts',(10.8617271271499,78.0658304123124,27.0906342205866));
#254171=CARTESIAN_POINT('Ctrl Pts',(10.8608226300202,77.6492670005164,30.451584267896));
#254172=CARTESIAN_POINT('Ctrl Pts',(10.8599093742504,77.2286698235283,33.845079860324));
#254173=CARTESIAN_POINT('Ctrl Pts',(10.8589817945603,76.8080120453849,37.2385679384961));
#254174=CARTESIAN_POINT('Ctrl Pts',(10.8580391950581,76.3872907109282,40.6320481322491));
#254175=CARTESIAN_POINT('Origin',(-90.,90.,17.4625));
#254176=CARTESIAN_POINT('',(-110.478801107225,75.6605890912239,16.1925));
#254177=CARTESIAN_POINT('',(-75.6605890912239,110.478801107225,16.1925));
#254178=CARTESIAN_POINT('Origin',(-90.,90.,16.1925));
#254179=CARTESIAN_POINT('',(-75.6605890912239,110.478801107225,12.3825));
#254180=CARTESIAN_POINT('',(-75.6605890912239,110.478801107225,12.3825));
#254181=CARTESIAN_POINT('',(-80.428115389329,113.095,12.3825));
#254182=CARTESIAN_POINT('Origin',(-90.,90.,12.3825));
#254183=CARTESIAN_POINT('',(-90.,115.,10.4775));
#254184=CARTESIAN_POINT('Ctrl Pts',(-80.428115389329,113.095,12.3825));
#254185=CARTESIAN_POINT('Ctrl Pts',(-81.8924546881425,113.701905685175,
12.3825));
#254186=CARTESIAN_POINT('Ctrl Pts',(-83.5138272817594,114.202094699092,
12.1039861530196));
#254187=CARTESIAN_POINT('Ctrl Pts',(-86.8039448109204,114.851492965438,
11.3641723788953));
#254188=CARTESIAN_POINT('Ctrl Pts',(-88.4720214203075,115.,10.8992885166146));
#254189=CARTESIAN_POINT('Ctrl Pts',(-90.,115.,10.4775));
#254190=CARTESIAN_POINT('',(-90.,115.,0.0380999999999992));
#254191=CARTESIAN_POINT('',(-90.,115.,17.4625));
#254192=CARTESIAN_POINT('',(-115.,90.,0.0381));
#254193=CARTESIAN_POINT('Origin',(-90.,90.,0.0381));
#254194=CARTESIAN_POINT('',(-115.,90.,10.4775));
#254195=CARTESIAN_POINT('',(-115.,90.,17.4625));
#254196=CARTESIAN_POINT('',(-111.45976584278,77.1750847966528,14.2875));
#254197=CARTESIAN_POINT('Ctrl Pts',(-115.,90.,10.4775));
#254198=CARTESIAN_POINT('Ctrl Pts',(-115.,89.5656046367595,10.6534234416246));
#254199=CARTESIAN_POINT('Ctrl Pts',(-114.988625660063,89.1307534409601,
10.82954637956));
#254200=CARTESIAN_POINT('Ctrl Pts',(-114.965914947157,88.6961589330913,
11.0044622013578));
#254201=CARTESIAN_POINT('Ctrl Pts',(-114.943409594944,88.2654942282673,
11.1777963539982));
#254202=CARTESIAN_POINT('Ctrl Pts',(-114.909771870929,87.835080885952,11.3499462246594));
#254203=CARTESIAN_POINT('Ctrl Pts',(-114.864988738924,87.4056111020781,
11.5195411430327));
#254204=CARTESIAN_POINT('Ctrl Pts',(-114.841493243082,87.1802895341208,
11.608519214041));
#254205=CARTESIAN_POINT('Ctrl Pts',(-114.814929056248,86.9552277330983,
11.6967938816802));
#254206=CARTESIAN_POINT('Ctrl Pts',(-114.785288831497,86.7305265176408,
11.7841654473661));
#254207=CARTESIAN_POINT('Ctrl Pts',(-114.78477355285,86.726620213312,11.785684352925));
#254208=CARTESIAN_POINT('Ctrl Pts',(-114.784257346139,86.7227140306222,
11.7872029805012));
#254209=CARTESIAN_POINT('Ctrl Pts',(-114.783740211354,86.7188079702431,
11.7887213289904));
#254210=CARTESIAN_POINT('Ctrl Pts',(-114.707687724482,86.1443627503486,
12.0120174245779));
#254211=CARTESIAN_POINT('Ctrl Pts',(-114.611788003437,85.5722301476407,
12.2295806327357));
#254212=CARTESIAN_POINT('Ctrl Pts',(-114.495317720437,85.0015050763843,
12.4383933645731));
#254213=CARTESIAN_POINT('Ctrl Pts',(-114.392569776158,84.4980219018838,
12.6226041210241));
#254214=CARTESIAN_POINT('Ctrl Pts',(-114.273812458388,83.9956342995033,
12.8000049442964));
#254215=CARTESIAN_POINT('Ctrl Pts',(-114.138523507008,83.4937195188485,
12.9685020775533));
#254216=CARTESIAN_POINT('Ctrl Pts',(-114.136898423986,83.4876905476702,
12.9705260553264));
#254217=CARTESIAN_POINT('Ctrl Pts',(-114.135270955025,83.4816616434102,
12.9725487471968));
#254218=CARTESIAN_POINT('Ctrl Pts',(-114.133641099172,83.4756328049009,
12.9745701495385));
#254219=CARTESIAN_POINT('Ctrl Pts',(-114.007805694041,83.0101675093264,
13.1306354740579));
#254220=CARTESIAN_POINT('Ctrl Pts',(-113.867666657712,82.5450867340379,
13.2789353415663));
#254221=CARTESIAN_POINT('Ctrl Pts',(-113.712210319662,82.0796977881564,
13.4168816899579));
#254222=CARTESIAN_POINT('Ctrl Pts',(-113.690214571606,82.0138492153038,
13.436399923582));
#254223=CARTESIAN_POINT('Ctrl Pts',(-113.667912115099,81.9479944649698,
13.4557108194421));
#254224=CARTESIAN_POINT('Ctrl Pts',(-113.645300019736,81.8821315660405,
13.4748069823197));
#254225=CARTESIAN_POINT('Ctrl Pts',(-113.643270339836,81.8762196591617,
13.4765210692868));
#254226=CARTESIAN_POINT('Ctrl Pts',(-113.641238170047,81.8703077008491,
13.4782334211549));
#254227=CARTESIAN_POINT('Ctrl Pts',(-113.639203508438,81.8643956901358,
13.4799440324456));
#254228=CARTESIAN_POINT('Ctrl Pts',(-113.456290898634,81.332916006182,13.6337250711184));
#254229=CARTESIAN_POINT('Ctrl Pts',(-113.254273359621,80.8043691708234,
13.7724010417179));
#254230=CARTESIAN_POINT('Ctrl Pts',(-113.034078437782,80.2824267541528,
13.8900543869064));
#254231=CARTESIAN_POINT('Ctrl Pts',(-113.032069517046,80.2776648780162,
13.8911277824362));
#254232=CARTESIAN_POINT('Ctrl Pts',(-113.030059078579,80.2729035395786,
13.8921994304486));
#254233=CARTESIAN_POINT('Ctrl Pts',(-113.028047123005,80.2681427414561,
13.8932693264694));
#254234=CARTESIAN_POINT('Ctrl Pts',(-112.841564750851,79.8268780640705,
13.9924349096997));
#254235=CARTESIAN_POINT('Ctrl Pts',(-112.641760412556,79.389376763279,14.0768952568082));
#254236=CARTESIAN_POINT('Ctrl Pts',(-112.427972083071,78.9552639490499,
14.1422627631443));
#254237=CARTESIAN_POINT('Ctrl Pts',(-112.388436056326,78.8749831597535,
14.1543512222522));
#254238=CARTESIAN_POINT('Ctrl Pts',(-112.348421741625,78.7948182514345,
14.1657865821597));
#254239=CARTESIAN_POINT('Ctrl Pts',(-112.307924890089,78.7147668473371,
14.1765409023449));
#254240=CARTESIAN_POINT('Ctrl Pts',(-112.306476768944,78.7119043005831,
14.1769254645483));
#254241=CARTESIAN_POINT('Ctrl Pts',(-112.305028031036,78.7090418994725,
14.1773091556142));
#254242=CARTESIAN_POINT('Ctrl Pts',(-112.303578676147,78.7061796438514,
14.1776919742689));
#254243=CARTESIAN_POINT('Ctrl Pts',(-112.146482129816,78.3959378416688,
14.2191859444306));
#254244=CARTESIAN_POINT('Ctrl Pts',(-111.982145145801,78.0874036287513,
14.2505477198143));
#254245=CARTESIAN_POINT('Ctrl Pts',(-111.810091167185,77.7803237269415,
14.2689228991092));
#254246=CARTESIAN_POINT('Ctrl Pts',(-111.696714227447,77.577969908667,14.281031433956));
#254247=CARTESIAN_POINT('Ctrl Pts',(-111.579986000179,77.3762476415099,
14.2874999986824));
#254248=CARTESIAN_POINT('Ctrl Pts',(-111.45976584278,77.1750847966528,14.2875));
#254249=CARTESIAN_POINT('',(-110.478801107225,75.6605890912239,14.2875));
#254250=CARTESIAN_POINT('Origin',(-90.,90.,14.2875));
#254251=CARTESIAN_POINT('',(-110.478801107225,75.6605890912239,12.3825));
#254252=CARTESIAN_POINT('Origin',(-90.,-90.,17.4625));
#254253=CARTESIAN_POINT('',(-75.6605890912239,-110.478801107225,16.1925));
#254254=CARTESIAN_POINT('',(-110.478801107225,-75.6605890912239,16.1925));
#254255=CARTESIAN_POINT('Origin',(-90.,-90.,16.1925));
#254256=CARTESIAN_POINT('',(-110.478801107225,-75.6605890912239,14.2875));
#254257=CARTESIAN_POINT('',(-110.478801107225,-75.6605890912239,12.3825));
#254258=CARTESIAN_POINT('',(-111.45976584278,-77.1750847966528,14.2875));
#254259=CARTESIAN_POINT('Origin',(-90.,-90.,14.2875));
#254260=CARTESIAN_POINT('',(-115.,-90.,10.4775));
#254261=CARTESIAN_POINT('Ctrl Pts',(-111.45976584278,-77.1750847966528,
14.2875));
#254262=CARTESIAN_POINT('Ctrl Pts',(-111.642205354545,-77.4803584878129,
14.2874999980005));
#254263=CARTESIAN_POINT('Ctrl Pts',(-111.816604025059,-77.7869204404192,
14.2726057755963));
#254264=CARTESIAN_POINT('Ctrl Pts',(-111.983450207187,-78.0950229353511,
14.2457040093625));
#254265=CARTESIAN_POINT('Ctrl Pts',(-112.093394377508,-78.2980486968468,
14.2279769488387));
#254266=CARTESIAN_POINT('Ctrl Pts',(-112.200058693817,-78.5017434125774,
14.2050347428326));
#254267=CARTESIAN_POINT('Ctrl Pts',(-112.303578675868,-78.7061796433008,
14.1776919687023));
#254268=CARTESIAN_POINT('Ctrl Pts',(-112.305032747302,-78.7090512133806,
14.1773079042348));
#254269=CARTESIAN_POINT('Ctrl Pts',(-112.306486197733,-78.7119229298981,
14.1769229616686));
#254270=CARTESIAN_POINT('Ctrl Pts',(-112.30793902738,-78.7147947930089,
14.1765371422901));
#254271=CARTESIAN_POINT('Ctrl Pts',(-112.526985593222,-79.1477923942053,
14.1183662410473));
#254272=CARTESIAN_POINT('Ctrl Pts',(-112.731915857196,-79.5841110072465,
14.0402742394713));
#254273=CARTESIAN_POINT('Ctrl Pts',(-112.923395334248,-80.0241259119978,
13.9466617191921));
#254274=CARTESIAN_POINT('Ctrl Pts',(-112.958736133735,-80.1053381586554,
13.9293839338147));
#254275=CARTESIAN_POINT('Ctrl Pts',(-112.993618688072,-80.1866763161992,
13.9115773060313));
#254276=CARTESIAN_POINT('Ctrl Pts',(-113.028047122842,-80.2681427410701,
13.8932693242905));
#254277=CARTESIAN_POINT('Ctrl Pts',(-113.030067104617,-80.2729225312233,
13.8921951601673));
#254278=CARTESIAN_POINT('Ctrl Pts',(-113.03208555715,-80.2777028659974,
13.8911192300483));
#254279=CARTESIAN_POINT('Ctrl Pts',(-113.034102479811,-80.2824837427445,
13.8900415384618));
#254280=CARTESIAN_POINT('Ctrl Pts',(-113.254288025274,-80.8044075501685,
13.7723909639359));
#254281=CARTESIAN_POINT('Ctrl Pts',(-113.45629755985,-81.3329353614433,
13.6337194701883));
#254282=CARTESIAN_POINT('Ctrl Pts',(-113.639203507904,-81.8643956885853,
13.4799440259955));
#254283=CARTESIAN_POINT('Ctrl Pts',(-113.641248155289,-81.8703367144489,
13.4782250192428));
#254284=CARTESIAN_POINT('Ctrl Pts',(-113.64329028633,-81.876277687381,13.4765042547891));
#254285=CARTESIAN_POINT('Ctrl Pts',(-113.645329902986,-81.8822186083625,
13.4747817381938));
#254286=CARTESIAN_POINT('Ctrl Pts',(-113.805159040923,-82.3477630899785,
13.3398013036916));
#254287=CARTESIAN_POINT('Ctrl Pts',(-113.949521015142,-82.8129009512596,
13.1940957680642));
#254288=CARTESIAN_POINT('Ctrl Pts',(-114.079434896297,-83.2783257874079,
13.0402593946707));
#254289=CARTESIAN_POINT('Ctrl Pts',(-114.09779119816,-83.3440884196296,
13.0185229421652));
#254290=CARTESIAN_POINT('Ctrl Pts',(-114.115858992445,-83.409856773525,
12.9966241002323));
#254291=CARTESIAN_POINT('Ctrl Pts',(-114.133641097615,-83.4756327991407,
12.974570129698));
#254292=CARTESIAN_POINT('Ctrl Pts',(-114.135281411444,-83.4817003217099,
12.9725357567984));
#254293=CARTESIAN_POINT('Ctrl Pts',(-114.136919307652,-83.4877679108745,
12.9705000777652));
#254294=CARTESIAN_POINT('Ctrl Pts',(-114.138554787209,-83.493835567825,
12.9684630962949));
#254295=CARTESIAN_POINT('Ctrl Pts',(-114.291921052846,-84.0628270195057,
12.7774461925192));
#254296=CARTESIAN_POINT('Ctrl Pts',(-114.424042625778,-84.6324262924149,
12.5749877226474));
#254297=CARTESIAN_POINT('Ctrl Pts',(-114.535677960622,-85.2035403844976,
12.3641357736727));
#254298=CARTESIAN_POINT('Ctrl Pts',(-114.634136703081,-85.7072444794929,
12.178171197402));
#254299=CARTESIAN_POINT('Ctrl Pts',(-114.716659190074,-86.2121266771173,
11.9856765646618));
#254300=CARTESIAN_POINT('Ctrl Pts',(-114.783740215493,-86.7188080015107,
11.7887214170753));
#254301=CARTESIAN_POINT('Ctrl Pts',(-114.784265106949,-86.722772650178,
11.7871802946265));
#254302=CARTESIAN_POINT('Ctrl Pts',(-114.784789042279,-86.7267374248492,
11.7856388846567));
#254303=CARTESIAN_POINT('Ctrl Pts',(-114.785312021496,-86.7307023248219,
11.7840971883205));
#254304=CARTESIAN_POINT('Ctrl Pts',(-114.829106259593,-87.0627227336102,
11.6549956595777));
#254305=CARTESIAN_POINT('Ctrl Pts',(-114.866221289693,-87.3958478252276,
11.5237902415043));
#254306=CARTESIAN_POINT('Ctrl Pts',(-114.896617394504,-87.7293197437528,
11.3913030896523));
#254307=CARTESIAN_POINT('Ctrl Pts',(-114.915895932174,-87.9408222038048,
11.3072739496097));
#254308=CARTESIAN_POINT('Ctrl Pts',(-114.932472713487,-88.1524639646833,
11.222729399464));
#254309=CARTESIAN_POINT('Ctrl Pts',(-114.946348419948,-88.3640506336912,
11.137879105755));
#254310=CARTESIAN_POINT('Ctrl Pts',(-114.964225054821,-88.6366463127898,
11.0285630342664));
#254311=CARTESIAN_POINT('Ctrl Pts',(-114.977628511886,-88.9092317828258,
10.9187075038446));
#254312=CARTESIAN_POINT('Ctrl Pts',(-114.986572967953,-89.1819023106261,
10.8085488142425));
#254313=CARTESIAN_POINT('Ctrl Pts',(-114.991045195986,-89.3182375745263,
10.7534694694415));
#254314=CARTESIAN_POINT('Ctrl Pts',(-114.994415138866,-89.4551356267363,
10.6980951474548));
#254315=CARTESIAN_POINT('Ctrl Pts',(-114.996653833646,-89.5917627923241,
10.6427966362161));
#254316=CARTESIAN_POINT('Ctrl Pts',(-114.998892528426,-89.7283899579119,
10.5874981249774));
#254317=CARTESIAN_POINT('Ctrl Pts',(-115.,-89.8647460047638,10.5322757880193));
#254318=CARTESIAN_POINT('Ctrl Pts',(-115.,-90.,10.4775));
#254319=CARTESIAN_POINT('',(-115.,-90.,0.0381));
#254320=CARTESIAN_POINT('',(-115.,-90.,17.4625));
#254321=CARTESIAN_POINT('',(-90.,-115.,0.0381));
#254322=CARTESIAN_POINT('Origin',(-90.,-90.,0.0381));
#254323=CARTESIAN_POINT('',(-90.,-115.,10.4775));
#254324=CARTESIAN_POINT('',(-90.,-115.,17.4625));
#254325=CARTESIAN_POINT('',(-77.1750847966528,-111.45976584278,14.2875));
#254326=CARTESIAN_POINT('Ctrl Pts',(-90.,-115.,10.4775));
#254327=CARTESIAN_POINT('Ctrl Pts',(-89.5656046344881,-115.,10.653423442612));
#254328=CARTESIAN_POINT('Ctrl Pts',(-89.1307534363923,-114.988625659943,
10.8295463814862));
#254329=CARTESIAN_POINT('Ctrl Pts',(-88.6961589262272,-114.965914946797,
11.0044622041873));
#254330=CARTESIAN_POINT('Ctrl Pts',(-88.265494227172,-114.943409594766,
11.177796354485));
#254331=CARTESIAN_POINT('Ctrl Pts',(-87.8350808906164,-114.909771871233,
11.3499462228129));
#254332=CARTESIAN_POINT('Ctrl Pts',(-87.405611112475,-114.864988740008,
11.5195411389418));
#254333=CARTESIAN_POINT('Ctrl Pts',(-87.1802895410429,-114.841493243899,
11.6085192113325));
#254334=CARTESIAN_POINT('Ctrl Pts',(-86.9552277365531,-114.814929056704,
11.696793880338));
#254335=CARTESIAN_POINT('Ctrl Pts',(-86.7305265176413,-114.785288831497,
11.7841654473675));
#254336=CARTESIAN_POINT('Ctrl Pts',(-86.7266202133125,-114.78477355285,
11.7856843529263));
#254337=CARTESIAN_POINT('Ctrl Pts',(-86.7227140306227,-114.784257346139,
11.7872029805025));
#254338=CARTESIAN_POINT('Ctrl Pts',(-86.7188079702436,-114.783740211354,
11.7887213289917));
#254339=CARTESIAN_POINT('Ctrl Pts',(-86.1443627509354,-114.70768772456,
12.0120174243529));
#254340=CARTESIAN_POINT('Ctrl Pts',(-85.5722301488083,-114.611788003633,
12.2295806322944));
#254341=CARTESIAN_POINT('Ctrl Pts',(-85.0015050781307,-114.495317720793,
12.4383933639359));
#254342=CARTESIAN_POINT('Ctrl Pts',(-84.4980219030455,-114.392569776432,
12.6226041206147));
#254343=CARTESIAN_POINT('Ctrl Pts',(-83.9956343000833,-114.273812458544,
12.8000049441012));
#254344=CARTESIAN_POINT('Ctrl Pts',(-83.4937195188483,-114.138523507008,
12.9685020775523));
#254345=CARTESIAN_POINT('Ctrl Pts',(-83.4876905476699,-114.136898423986,
12.9705260553254));
#254346=CARTESIAN_POINT('Ctrl Pts',(-83.48166164341,-114.135270955025,12.9725487471959));
#254347=CARTESIAN_POINT('Ctrl Pts',(-83.4756328049006,-114.133641099172,
12.9745701495376));
#254348=CARTESIAN_POINT('Ctrl Pts',(-83.0101675029287,-114.007805692311,
13.1306354762013));
#254349=CARTESIAN_POINT('Ctrl Pts',(-82.5450867212538,-113.86766665386,
13.2789353456426));
#254350=CARTESIAN_POINT('Ctrl Pts',(-82.0796977689676,-113.712210313252,
13.4168816956454));
#254351=CARTESIAN_POINT('Ctrl Pts',(-82.0138492025101,-113.690214567274,
13.4363999273334));
#254352=CARTESIAN_POINT('Ctrl Pts',(-81.9479944585721,-113.667912112902,
13.4557108212968));
#254353=CARTESIAN_POINT('Ctrl Pts',(-81.8821315660405,-113.645300019736,
13.4748069823194));
#254354=CARTESIAN_POINT('Ctrl Pts',(-81.8762196591616,-113.643270339836,
13.4765210692866));
#254355=CARTESIAN_POINT('Ctrl Pts',(-81.870307700849,-113.641238170047,
13.4782334211547));
#254356=CARTESIAN_POINT('Ctrl Pts',(-81.8643956901357,-113.639203508438,
13.4799440324454));
#254357=CARTESIAN_POINT('Ctrl Pts',(-81.3329160061816,-113.456290898634,
13.633725071118));
#254358=CARTESIAN_POINT('Ctrl Pts',(-80.8043691708234,-113.254273359621,
13.7724010417179));
#254359=CARTESIAN_POINT('Ctrl Pts',(-80.2824267541528,-113.034078437782,
13.8900543869066));
#254360=CARTESIAN_POINT('Ctrl Pts',(-80.2776648780163,-113.032069517046,
13.8911277824363));
#254361=CARTESIAN_POINT('Ctrl Pts',(-80.2729035395786,-113.030059078579,
13.8921994304488));
#254362=CARTESIAN_POINT('Ctrl Pts',(-80.2681427414562,-113.028047123005,
13.8932693264696));
#254363=CARTESIAN_POINT('Ctrl Pts',(-79.826878070857,-112.84156475372,13.9924349081749));
#254364=CARTESIAN_POINT('Ctrl Pts',(-79.3893767767358,-112.641760418702,
14.0768952542102));
#254365=CARTESIAN_POINT('Ctrl Pts',(-78.9552639690786,-112.427972092934,
14.1422627601284));
#254366=CARTESIAN_POINT('Ctrl Pts',(-78.8749831730867,-112.388436062981,
14.1543512203501));
#254367=CARTESIAN_POINT('Ctrl Pts',(-78.7948182580917,-112.348421744993,
14.1657865812652));
#254368=CARTESIAN_POINT('Ctrl Pts',(-78.7147668473371,-112.307924890089,
14.1765409023448));
#254369=CARTESIAN_POINT('Ctrl Pts',(-78.711904300583,-112.306476768944,
14.1769254645481));
#254370=CARTESIAN_POINT('Ctrl Pts',(-78.7090418994725,-112.305028031036,
14.1773091556141));
#254371=CARTESIAN_POINT('Ctrl Pts',(-78.7061796438514,-112.303578676147,
14.1776919742687));
#254372=CARTESIAN_POINT('Ctrl Pts',(-78.3959378426708,-112.146482130324,
14.2191859442963));
#254373=CARTESIAN_POINT('Ctrl Pts',(-78.0874036307441,-111.982145146862,
14.2505477196114));
#254374=CARTESIAN_POINT('Ctrl Pts',(-77.7803237299166,-111.810091168852,
14.2689228989311));
#254375=CARTESIAN_POINT('Ctrl Pts',(-77.5779699106442,-111.696714228591,
14.2810314338925));
#254376=CARTESIAN_POINT('Ctrl Pts',(-77.3762476424957,-111.579986000768,
14.2874999986824));
#254377=CARTESIAN_POINT('Ctrl Pts',(-77.1750847966528,-111.45976584278,
14.2875));
#254378=CARTESIAN_POINT('',(-75.6605890912239,-110.478801107225,14.2875));
#254379=CARTESIAN_POINT('Origin',(-90.,-90.,14.2875));
#254380=CARTESIAN_POINT('',(-75.6605890912239,-110.478801107225,12.3825));
#254381=CARTESIAN_POINT('Origin',(-90.,-115.,17.4625));
#254382=CARTESIAN_POINT('',(90.,-115.,10.4775));
#254383=CARTESIAN_POINT('',(90.,-115.,0.0381));
#254384=CARTESIAN_POINT('',(90.,-115.,17.4625));
#254385=CARTESIAN_POINT('',(-90.,-115.,10.4775));
#254386=CARTESIAN_POINT('',(90.,-115.,0.0381));
#254387=CARTESIAN_POINT('Origin',(-115.,90.,17.4625));
#254388=CARTESIAN_POINT('',(-115.,90.,10.4775));
#254389=CARTESIAN_POINT('',(-115.,-90.,0.0381));
#254390=CARTESIAN_POINT('Origin',(115.,90.,17.4625));
#254391=CARTESIAN_POINT('',(115.,90.,10.4775));
#254392=CARTESIAN_POINT('',(115.,90.,0.0381));
#254393=CARTESIAN_POINT('',(115.,90.,17.4625));
#254394=CARTESIAN_POINT('',(115.,-90.,10.4775));
#254395=CARTESIAN_POINT('',(115.,-90.,10.4775));
#254396=CARTESIAN_POINT('',(115.,-90.,0.0381));
#254397=CARTESIAN_POINT('',(115.,-90.,17.4625));
#254398=CARTESIAN_POINT('',(115.,90.,0.0381));
#254399=CARTESIAN_POINT('Origin',(90.,-90.,17.4625));
#254400=CARTESIAN_POINT('',(110.478801107225,-75.6605890912239,14.2875));
#254401=CARTESIAN_POINT('',(110.478801107225,-75.6605890912239,12.3825));
#254402=CARTESIAN_POINT('',(75.6605890912239,-110.478801107225,14.2875));
#254403=CARTESIAN_POINT('',(75.6605890912239,-110.478801107225,12.3825));
#254404=CARTESIAN_POINT('',(77.1750847966528,-111.45976584278,14.2875));
#254405=CARTESIAN_POINT('Origin',(90.,-90.,14.2875));
#254406=CARTESIAN_POINT('Ctrl Pts',(77.1750847966528,-111.45976584278,14.2875));
#254407=CARTESIAN_POINT('Ctrl Pts',(77.4803584868234,-111.642205353954,
14.2874999980005));
#254408=CARTESIAN_POINT('Ctrl Pts',(77.786920438432,-111.816604023928,14.2726057756926));
#254409=CARTESIAN_POINT('Ctrl Pts',(78.0950229323553,-111.983450205564,
14.2457040096238));
#254410=CARTESIAN_POINT('Ctrl Pts',(78.298048694843,-112.093394376459,14.2279769490641));
#254411=CARTESIAN_POINT('Ctrl Pts',(78.5017434115719,-112.200058693308,
14.2050347429669));
#254412=CARTESIAN_POINT('Ctrl Pts',(78.7061796433008,-112.303578675868,
14.1776919687022));
#254413=CARTESIAN_POINT('Ctrl Pts',(78.7090512133806,-112.305032747302,
14.1773079042347));
#254414=CARTESIAN_POINT('Ctrl Pts',(78.7119229298981,-112.306486197733,
14.1769229616685));
#254415=CARTESIAN_POINT('Ctrl Pts',(78.7147947930089,-112.30793902738,14.1765371422899));
#254416=CARTESIAN_POINT('Ctrl Pts',(79.1477923875285,-112.526985589844,
14.1183662419443));
#254417=CARTESIAN_POINT('Ctrl Pts',(79.5841109937906,-112.731915850876,
14.0402742418796));
#254418=CARTESIAN_POINT('Ctrl Pts',(80.0241258916428,-112.92339532539,13.9466617235228));
#254419=CARTESIAN_POINT('Ctrl Pts',(80.1053381450643,-112.958736127907,
13.9293839367902));
#254420=CARTESIAN_POINT('Ctrl Pts',(80.186676309393,-112.993618685196,13.911577307561));
#254421=CARTESIAN_POINT('Ctrl Pts',(80.2681427410701,-113.028047122842,
13.8932693242907));
#254422=CARTESIAN_POINT('Ctrl Pts',(80.2729225312233,-113.030067104617,
13.8921951601674));
#254423=CARTESIAN_POINT('Ctrl Pts',(80.2777028659974,-113.03208555715,13.8911192300484));
#254424=CARTESIAN_POINT('Ctrl Pts',(80.2824837427445,-113.034102479811,
13.890041538462));
#254425=CARTESIAN_POINT('Ctrl Pts',(80.8044075501684,-113.254288025274,
13.7723909639359));
#254426=CARTESIAN_POINT('Ctrl Pts',(81.3329353614429,-113.45629755985,13.6337194701879));
#254427=CARTESIAN_POINT('Ctrl Pts',(81.8643956885852,-113.639203507904,
13.4799440259953));
#254428=CARTESIAN_POINT('Ctrl Pts',(81.8703367144488,-113.641248155289,
13.4782250192426));
#254429=CARTESIAN_POINT('Ctrl Pts',(81.876277687381,-113.64329028633,13.4765042547889));
#254430=CARTESIAN_POINT('Ctrl Pts',(81.8822186083625,-113.645329902986,
13.4747817381936));
#254431=CARTESIAN_POINT('Ctrl Pts',(82.3477630963775,-113.80515904312,13.3398013018362));
#254432=CARTESIAN_POINT('Ctrl Pts',(82.8129009640461,-113.94952101911,13.1940957640577));
#254433=CARTESIAN_POINT('Ctrl Pts',(83.2783258065996,-114.079434901654,
13.040259388326));
#254434=CARTESIAN_POINT('Ctrl Pts',(83.3440884324251,-114.097791201675,
13.0185229379035));
#254435=CARTESIAN_POINT('Ctrl Pts',(83.4098567799233,-114.115858994174,
12.9966240980859));
#254436=CARTESIAN_POINT('Ctrl Pts',(83.4756327991404,-114.133641097615,
12.974570129697));
#254437=CARTESIAN_POINT('Ctrl Pts',(83.4817003217096,-114.135281411444,
12.9725357567974));
#254438=CARTESIAN_POINT('Ctrl Pts',(83.4877679108742,-114.136919307652,
12.9705000777643));
#254439=CARTESIAN_POINT('Ctrl Pts',(83.4938355678247,-114.138554787209,
12.968463096294));
#254440=CARTESIAN_POINT('Ctrl Pts',(84.0628270192128,-114.291921052767,
12.7774461926172));
#254441=CARTESIAN_POINT('Ctrl Pts',(84.632426291829,-114.424042625642,12.5749877228569));
#254442=CARTESIAN_POINT('Ctrl Pts',(85.2035403836165,-114.53567796045,12.3641357739999));
#254443=CARTESIAN_POINT('Ctrl Pts',(85.7072444789046,-114.634136702985,
12.1781711976289));
#254444=CARTESIAN_POINT('Ctrl Pts',(86.2121266768225,-114.716659190035,
11.9856765647789));
#254445=CARTESIAN_POINT('Ctrl Pts',(86.718808001511,-114.783740215493,11.7887214170762));
#254446=CARTESIAN_POINT('Ctrl Pts',(86.7227726501783,-114.784265106949,
11.7871802946274));
#254447=CARTESIAN_POINT('Ctrl Pts',(86.7267374248495,-114.784789042279,
11.7856388846576));
#254448=CARTESIAN_POINT('Ctrl Pts',(86.7307023248221,-114.785312021496,
11.7840971883214));
#254449=CARTESIAN_POINT('Ctrl Pts',(87.0627227347716,-114.829106259746,
11.6549956591265));
#254450=CARTESIAN_POINT('Ctrl Pts',(87.395847827558,-114.866221289952,11.5237902405866));
#254451=CARTESIAN_POINT('Ctrl Pts',(87.729319747252,-114.896617394822,11.3913030882621));
#254452=CARTESIAN_POINT('Ctrl Pts',(87.9408222061392,-114.915895932356,
11.3072739486773));
#254453=CARTESIAN_POINT('Ctrl Pts',(88.1524639658503,-114.932472713562,
11.2227293989961));
#254454=CARTESIAN_POINT('Ctrl Pts',(88.3640506336914,-114.946348419947,
11.1378791057551));
#254455=CARTESIAN_POINT('Ctrl Pts',(88.6366463127899,-114.964225054819,
11.0285630342665));
#254456=CARTESIAN_POINT('Ctrl Pts',(88.9092317828258,-114.977628511885,
10.9187075038447));
#254457=CARTESIAN_POINT('Ctrl Pts',(89.1819023106262,-114.986572967952,
10.8085488142427));
#254458=CARTESIAN_POINT('Ctrl Pts',(89.3182375745263,-114.991045195985,
10.7534694694417));
#254459=CARTESIAN_POINT('Ctrl Pts',(89.4551356267436,-114.994415138866,
10.6980951474732));
#254460=CARTESIAN_POINT('Ctrl Pts',(89.5917627923341,-114.996653833646,
10.6427966362411));
#254461=CARTESIAN_POINT('Ctrl Pts',(89.7283899579245,-114.998892528426,
10.5874981250089));
#254462=CARTESIAN_POINT('Ctrl Pts',(89.8647460047744,-115.,10.5322757880455));
#254463=CARTESIAN_POINT('Ctrl Pts',(90.,-115.,10.4775));
#254464=CARTESIAN_POINT('Origin',(90.,-90.,0.0381));
#254465=CARTESIAN_POINT('',(111.45976584278,-77.1750847966528,14.2875));
#254466=CARTESIAN_POINT('Ctrl Pts',(115.,-90.,10.4775));
#254467=CARTESIAN_POINT('Ctrl Pts',(115.,-89.5656046355683,10.6534234421179));
#254468=CARTESIAN_POINT('Ctrl Pts',(114.98862566,-89.1307534385709,10.8295463805372));
#254469=CARTESIAN_POINT('Ctrl Pts',(114.96591494697,-88.6961589295072,11.0044622028075));
#254470=CARTESIAN_POINT('Ctrl Pts',(114.943409594942,-88.265494229423,11.1777963535319));
#254471=CARTESIAN_POINT('Ctrl Pts',(114.909771871358,-87.8350808918436,
11.3499462222986));
#254472=CARTESIAN_POINT('Ctrl Pts',(114.86498874003,-87.4056111126796,11.5195411388467));
#254473=CARTESIAN_POINT('Ctrl Pts',(114.841493243915,-87.1802895411801,
11.608519211272));
#254474=CARTESIAN_POINT('Ctrl Pts',(114.814929056713,-86.9552277366222,
11.6967938803096));
#254475=CARTESIAN_POINT('Ctrl Pts',(114.785288831497,-86.7305265176406,
11.7841654473657));
#254476=CARTESIAN_POINT('Ctrl Pts',(114.78477355285,-86.7266202133119,11.7856843529246));
#254477=CARTESIAN_POINT('Ctrl Pts',(114.784257346139,-86.7227140306221,
11.7872029805007));
#254478=CARTESIAN_POINT('Ctrl Pts',(114.783740211354,-86.718807970243,11.7887213289899));
#254479=CARTESIAN_POINT('Ctrl Pts',(114.707687724832,-86.1443627529916,
12.0120174235497));
#254480=CARTESIAN_POINT('Ctrl Pts',(114.611788004319,-85.5722301529056,
12.2295806307328));
#254481=CARTESIAN_POINT('Ctrl Pts',(114.495317722044,-85.0015050842623,
12.4383933616903));
#254482=CARTESIAN_POINT('Ctrl Pts',(114.392569777396,-84.4980219071244,
12.6226041191732));
#254483=CARTESIAN_POINT('Ctrl Pts',(114.273812459093,-83.995634302121,12.8000049434176));
#254484=CARTESIAN_POINT('Ctrl Pts',(114.138523507008,-83.4937195188485,
12.9685020775533));
#254485=CARTESIAN_POINT('Ctrl Pts',(114.136898423986,-83.4876905476702,
12.9705260553264));
#254486=CARTESIAN_POINT('Ctrl Pts',(114.135270955025,-83.4816616434103,
12.9725487471968));
#254487=CARTESIAN_POINT('Ctrl Pts',(114.133641099172,-83.4756328049009,
12.9745701495385));
#254488=CARTESIAN_POINT('Ctrl Pts',(114.007805692247,-83.0101675026927,
13.1306354762821));
#254489=CARTESIAN_POINT('Ctrl Pts',(113.867666653718,-82.5450867207814,
13.2789353457935));
#254490=CARTESIAN_POINT('Ctrl Pts',(113.712210313015,-82.0796977682585,
13.4168816958559));
#254491=CARTESIAN_POINT('Ctrl Pts',(113.690214567113,-82.0138492020373,
13.4363999274722));
#254492=CARTESIAN_POINT('Ctrl Pts',(113.667912112821,-81.9479944583357,
13.4557108213656));
#254493=CARTESIAN_POINT('Ctrl Pts',(113.645300019736,-81.8821315660405,
13.4748069823197));
#254494=CARTESIAN_POINT('Ctrl Pts',(113.643270339836,-81.8762196591617,
13.4765210692869));
#254495=CARTESIAN_POINT('Ctrl Pts',(113.641238170047,-81.8703077008491,
13.478233421155));
#254496=CARTESIAN_POINT('Ctrl Pts',(113.639203508438,-81.8643956901358,
13.4799440324457));
#254497=CARTESIAN_POINT('Ctrl Pts',(113.456290898634,-81.3329160061815,
13.6337250711187));
#254498=CARTESIAN_POINT('Ctrl Pts',(113.254273359621,-80.8043691708234,
13.7724010417179));
#254499=CARTESIAN_POINT('Ctrl Pts',(113.034078437782,-80.2824267541528,
13.8900543869065));
#254500=CARTESIAN_POINT('Ctrl Pts',(113.032069517046,-80.2776648780163,
13.8911277824363));
#254501=CARTESIAN_POINT('Ctrl Pts',(113.030059078579,-80.2729035395786,
13.8921994304487));
#254502=CARTESIAN_POINT('Ctrl Pts',(113.028047123005,-80.2681427414561,
13.8932693264695));
#254503=CARTESIAN_POINT('Ctrl Pts',(112.841564748611,-79.8268780587689,
13.9924349108913));
#254504=CARTESIAN_POINT('Ctrl Pts',(112.641760407755,-79.3893767527665,
14.0768952588379));
#254505=CARTESIAN_POINT('Ctrl Pts',(112.427972075365,-78.9552639334033,
14.1422627655002));
#254506=CARTESIAN_POINT('Ctrl Pts',(112.388436051127,-78.8749831493374,
14.1543512237378));
#254507=CARTESIAN_POINT('Ctrl Pts',(112.348421738994,-78.7948182462339,
14.165786582858));
#254508=CARTESIAN_POINT('Ctrl Pts',(112.307924890089,-78.7147668473371,
14.1765409023446));
#254509=CARTESIAN_POINT('Ctrl Pts',(112.306476768944,-78.711904300583,14.1769254645479));
#254510=CARTESIAN_POINT('Ctrl Pts',(112.305028031036,-78.7090418994725,
14.1773091556138));
#254511=CARTESIAN_POINT('Ctrl Pts',(112.303578676147,-78.7061796438514,
14.1776919742685));
#254512=CARTESIAN_POINT('Ctrl Pts',(112.146482129285,-78.3959378406196,
14.2191859445703));
#254513=CARTESIAN_POINT('Ctrl Pts',(111.98214514469,-78.0874036266646,14.2505477200261));
#254514=CARTESIAN_POINT('Ctrl Pts',(111.81009116544,-77.7803237238264,14.2689228992955));
#254515=CARTESIAN_POINT('Ctrl Pts',(111.696714226249,-77.5779699065967,
14.2810314340224));
#254516=CARTESIAN_POINT('Ctrl Pts',(111.579985999562,-77.3762476404776,
14.2874999986824));
#254517=CARTESIAN_POINT('Ctrl Pts',(111.45976584278,-77.1750847966528,14.2875));
#254518=CARTESIAN_POINT('Origin',(90.,-90.,14.2875));
#254519=CARTESIAN_POINT('Origin',(90.,90.,17.4625));
#254520=CARTESIAN_POINT('',(75.6605890912238,110.478801107225,12.3825));
#254521=CARTESIAN_POINT('',(75.6605890912238,110.478801107225,12.3825));
#254522=CARTESIAN_POINT('',(110.478801107225,75.6605890912239,14.2875));
#254523=CARTESIAN_POINT('',(110.478801107225,75.6605890912239,12.3825));
#254524=CARTESIAN_POINT('',(111.45976584278,77.1750847966528,14.2875));
#254525=CARTESIAN_POINT('Origin',(90.,90.,14.2875));
#254526=CARTESIAN_POINT('Ctrl Pts',(111.45976584278,77.1750847966528,14.2875));
#254527=CARTESIAN_POINT('Ctrl Pts',(111.642205355166,77.4803584888519,14.2874999980005));
#254528=CARTESIAN_POINT('Ctrl Pts',(111.816604026246,77.7869204425061,14.2726057754947));
#254529=CARTESIAN_POINT('Ctrl Pts',(111.98345020889,78.0950229384971,14.2457040090874));
#254530=CARTESIAN_POINT('Ctrl Pts',(112.09339437861,78.298048698951,14.2279769486012));
#254531=CARTESIAN_POINT('Ctrl Pts',(112.200058694352,78.5017434136333,14.2050347426909));
#254532=CARTESIAN_POINT('Ctrl Pts',(112.303578675868,78.7061796433008,14.1776919687019));
#254533=CARTESIAN_POINT('Ctrl Pts',(112.305032747302,78.7090512133806,14.1773079042344));
#254534=CARTESIAN_POINT('Ctrl Pts',(112.306486197733,78.7119229298981,14.1769229616682));
#254535=CARTESIAN_POINT('Ctrl Pts',(112.307939027379,78.7147947930089,14.1765371422897));
#254536=CARTESIAN_POINT('Ctrl Pts',(112.526985595836,79.1477923993722,14.1183662403531));
#254537=CARTESIAN_POINT('Ctrl Pts',(112.731915862087,79.5841110176595,14.0402742376079));
#254538=CARTESIAN_POINT('Ctrl Pts',(112.923395341103,80.0241259277498,13.946661715841));
#254539=CARTESIAN_POINT('Ctrl Pts',(112.958736138246,80.105338169173,13.9293839315123));
#254540=CARTESIAN_POINT('Ctrl Pts',(112.993618690298,80.1866763214663,13.9115773048477));
#254541=CARTESIAN_POINT('Ctrl Pts',(113.028047122842,80.2681427410701,13.8932693242906));
#254542=CARTESIAN_POINT('Ctrl Pts',(113.030067104617,80.2729225312233,13.8921951601673));
#254543=CARTESIAN_POINT('Ctrl Pts',(113.03208555715,80.2777028659974,13.8911192300484));
#254544=CARTESIAN_POINT('Ctrl Pts',(113.034102479811,80.2824837427445,13.8900415384619));
#254545=CARTESIAN_POINT('Ctrl Pts',(113.254288025274,80.8044075501685,13.7723909639359));
#254546=CARTESIAN_POINT('Ctrl Pts',(113.45629755985,81.3329353614428,13.6337194701886));
#254547=CARTESIAN_POINT('Ctrl Pts',(113.639203507904,81.8643956885853,13.4799440259956));
#254548=CARTESIAN_POINT('Ctrl Pts',(113.641248155289,81.8703367144489,13.4782250192429));
#254549=CARTESIAN_POINT('Ctrl Pts',(113.64329028633,81.876277687381,13.4765042547891));
#254550=CARTESIAN_POINT('Ctrl Pts',(113.645329902986,81.8822186083625,13.4747817381939));
#254551=CARTESIAN_POINT('Ctrl Pts',(113.805159043221,82.3477630966713,13.3398013017511));
#254552=CARTESIAN_POINT('Ctrl Pts',(113.949521019293,82.8129009646335,13.1940957638749));
#254553=CARTESIAN_POINT('Ctrl Pts',(114.0794349019,83.2783258074811,13.0402593880359));
#254554=CARTESIAN_POINT('Ctrl Pts',(114.097791201837,83.344088433013,13.0185229377089));
#254555=CARTESIAN_POINT('Ctrl Pts',(114.115858994254,83.4098567802174,12.9966240979884));
#254556=CARTESIAN_POINT('Ctrl Pts',(114.133641097615,83.4756327991407,12.974570129698));
#254557=CARTESIAN_POINT('Ctrl Pts',(114.135281411444,83.4817003217099,12.9725357567984));
#254558=CARTESIAN_POINT('Ctrl Pts',(114.136919307652,83.4877679108745,12.9705000777652));
#254559=CARTESIAN_POINT('Ctrl Pts',(114.138554787209,83.493835567825,12.9684630962949));
#254560=CARTESIAN_POINT('Ctrl Pts',(114.291921052112,84.0628270167828,12.7774461934334));
#254561=CARTESIAN_POINT('Ctrl Pts',(114.424042624513,84.6324262869634,12.5749877245847));
#254562=CARTESIAN_POINT('Ctrl Pts',(114.535677959019,85.2035403762984,12.3641357766992));
#254563=CARTESIAN_POINT('Ctrl Pts',(114.634136702185,85.707244474014,12.1781711994903));
#254564=CARTESIAN_POINT('Ctrl Pts',(114.71665918971,86.212126674368,11.9856765657298));
#254565=CARTESIAN_POINT('Ctrl Pts',(114.783740215493,86.7188080015106,11.7887214170749));
#254566=CARTESIAN_POINT('Ctrl Pts',(114.784265106949,86.7227726501778,11.7871802946262));
#254567=CARTESIAN_POINT('Ctrl Pts',(114.784789042279,86.7267374248491,11.7856388846564));
#254568=CARTESIAN_POINT('Ctrl Pts',(114.785312021496,86.7307023248217,11.7840971883202));
#254569=CARTESIAN_POINT('Ctrl Pts',(114.829106259638,87.0627227339489,11.6549956594459));
#254570=CARTESIAN_POINT('Ctrl Pts',(114.866221289769,87.3958478259074,11.5237902412365));
#254571=CARTESIAN_POINT('Ctrl Pts',(114.896617394597,87.7293197447736,11.3913030892467));
#254572=CARTESIAN_POINT('Ctrl Pts',(114.915895932227,87.9408222044859,11.3072739493377));
#254573=CARTESIAN_POINT('Ctrl Pts',(114.932472713509,88.1524639650238,11.2227293993275));
#254574=CARTESIAN_POINT('Ctrl Pts',(114.946348419948,88.3640506336913,11.137879105755));
#254575=CARTESIAN_POINT('Ctrl Pts',(114.96422505482,88.6366463127898,11.0285630342664));
#254576=CARTESIAN_POINT('Ctrl Pts',(114.977628511886,88.9092317828257,10.9187075038446));
#254577=CARTESIAN_POINT('Ctrl Pts',(114.986572967952,89.1819023106261,10.8085488142425));
#254578=CARTESIAN_POINT('Ctrl Pts',(114.991045195986,89.3182375745263,10.7534694694415));
#254579=CARTESIAN_POINT('Ctrl Pts',(114.994415138866,89.4551356267369,10.6980951474562));
#254580=CARTESIAN_POINT('Ctrl Pts',(114.996653833646,89.5917627923248,10.6427966362178));
#254581=CARTESIAN_POINT('Ctrl Pts',(114.998892528426,89.7283899579127,10.5874981249794));
#254582=CARTESIAN_POINT('Ctrl Pts',(115.,89.8647460047642,10.5322757880204));
#254583=CARTESIAN_POINT('Ctrl Pts',(115.,90.,10.4775));
#254584=CARTESIAN_POINT('',(90.,115.,0.0381));
#254585=CARTESIAN_POINT('Origin',(90.,90.,0.0381));
#254586=CARTESIAN_POINT('',(90.,115.,10.4775));
#254587=CARTESIAN_POINT('',(90.,115.,17.4625));
#254588=CARTESIAN_POINT('',(80.428115389329,113.095,12.3825));
#254589=CARTESIAN_POINT('Ctrl Pts',(90.,115.,10.4775));
#254590=CARTESIAN_POINT('Ctrl Pts',(88.4720214203075,115.,10.8992885166146));
#254591=CARTESIAN_POINT('Ctrl Pts',(86.8039448109204,114.851492965438,11.3641723788953));
#254592=CARTESIAN_POINT('Ctrl Pts',(83.5138272817594,114.202094699092,12.1039861530196));
#254593=CARTESIAN_POINT('Ctrl Pts',(81.8924546881425,113.701905685175,12.3825));
#254594=CARTESIAN_POINT('Ctrl Pts',(80.428115389329,113.095,12.3825));
#254595=CARTESIAN_POINT('Origin',(90.,90.0000000000001,12.3825));
#254596=CARTESIAN_POINT('Origin',(-90.,115.,17.4625));
#254597=CARTESIAN_POINT('',(-20.3338370957105,115.,10.4775));
#254598=CARTESIAN_POINT('',(20.3338370957106,115.,10.4775));
#254599=CARTESIAN_POINT('Ctrl Pts',(-20.3338370957105,115.,10.4775));
#254600=CARTESIAN_POINT('Ctrl Pts',(-19.9267590414958,115.,10.3125994708202));
#254601=CARTESIAN_POINT('Ctrl Pts',(-19.5174840291917,115.,10.1525816988894));
#254602=CARTESIAN_POINT('Ctrl Pts',(-19.106739643588,115.,9.99771295049682));
#254603=CARTESIAN_POINT('Ctrl Pts',(-18.6959952579844,115.,9.84284420210422));
#254604=CARTESIAN_POINT('Ctrl Pts',(-18.2837818084517,115.,9.69312450300941));
#254605=CARTESIAN_POINT('Ctrl Pts',(-17.8708421763035,115.,9.54876232402957));
#254606=CARTESIAN_POINT('Ctrl Pts',(-17.3189441652074,115.,9.35582080605997));
#254607=CARTESIAN_POINT('Ctrl Pts',(-16.7653329534949,115.,9.17228988049683));
#254608=CARTESIAN_POINT('Ctrl Pts',(-16.210031043884,115.,8.99805419968946));
#254609=CARTESIAN_POINT('Ctrl Pts',(-15.936948059999,115.,8.91236964001012));
#254610=CARTESIAN_POINT('Ctrl Pts',(-15.6634560177655,115.,8.82893383759967));
#254611=CARTESIAN_POINT('Ctrl Pts',(-15.3895567777554,115.,8.74773761914341));
#254612=CARTESIAN_POINT('Ctrl Pts',(-15.3869609596534,115.,8.74696810034636));
#254613=CARTESIAN_POINT('Ctrl Pts',(-15.3843650995479,115.,8.74619878028833));
#254614=CARTESIAN_POINT('Ctrl Pts',(-15.3817691974006,115.,8.74542965895521));
#254615=CARTESIAN_POINT('Ctrl Pts',(-13.7198971151702,115.,8.25304543225375));
#254616=CARTESIAN_POINT('Ctrl Pts',(-12.0430776052023,115.000000000003,
7.84278200114024));
#254617=CARTESIAN_POINT('Ctrl Pts',(-10.3515597238144,114.999999999997,
7.51327366480546));
#254618=CARTESIAN_POINT('Ctrl Pts',(-10.3463733638648,114.999999999997,
7.51226335988499));
#254619=CARTESIAN_POINT('Ctrl Pts',(-10.3411868667297,114.999999999997,
7.51125380869066));
#254620=CARTESIAN_POINT('Ctrl Pts',(-10.3360002323986,114.999999999997,
7.51024501128054));
#254621=CARTESIAN_POINT('Ctrl Pts',(-8.23229812819579,114.999999999991,
7.10107615554567));
#254622=CARTESIAN_POINT('Ctrl Pts',(-6.10608444318685,114.999999999993,
6.81590866941424));
#254623=CARTESIAN_POINT('Ctrl Pts',(-3.95654770808245,114.999999999993,
6.65860083511691));
#254624=CARTESIAN_POINT('Ctrl Pts',(-2.64905735818768,114.999999999993,
6.56291581054969));
#254625=CARTESIAN_POINT('Ctrl Pts',(-1.3329376678419,114.999999999994,6.51453825908851));
#254626=CARTESIAN_POINT('Ctrl Pts',(-0.00800503439004147,114.999999999976,
6.51434590949666));
#254627=CARTESIAN_POINT('Ctrl Pts',(0.00263410608483974,114.999999999976,
6.51434436493939));
#254628=CARTESIAN_POINT('Ctrl Pts',(0.0132727023277519,114.999999999976,
6.51434592797752));
#254629=CARTESIAN_POINT('Ctrl Pts',(0.0239107544103369,114.999999999976,
6.51435059818956));
#254630=CARTESIAN_POINT('Ctrl Pts',(1.77562218690493,114.999999999951,6.51511961715718));
#254631=CARTESIAN_POINT('Ctrl Pts',(3.51091746734952,114.999999999965,6.60012007887875));
#254632=CARTESIAN_POINT('Ctrl Pts',(5.23024969626955,114.99999999998,6.76702375956156));
#254633=CARTESIAN_POINT('Ctrl Pts',(6.94958192518957,114.999999999995,6.93392744024437));
#254634=CARTESIAN_POINT('Ctrl Pts',(8.65295106909785,115.,7.18273455731824));
#254635=CARTESIAN_POINT('Ctrl Pts',(10.3407978197663,114.999999999999,7.51117731045924));
#254636=CARTESIAN_POINT('Ctrl Pts',(10.3504347739428,114.999999999999,7.51305259194459));
#254637=CARTESIAN_POINT('Ctrl Pts',(10.3600712202459,114.999999999999,7.51493048841781));
#254638=CARTESIAN_POINT('Ctrl Pts',(10.3697071586587,114.999999999999,7.51681100008705));
#254639=CARTESIAN_POINT('Ctrl Pts',(11.0233231057247,114.999999999998,7.64436810589384));
#254640=CARTESIAN_POINT('Ctrl Pts',(11.6740697898699,114.999999999998,7.78384849352191));
#254641=CARTESIAN_POINT('Ctrl Pts',(12.3222929011397,114.999999999998,7.93535062636677));
#254642=CARTESIAN_POINT('Ctrl Pts',(12.9676692556127,114.999999999998,8.08618741772824));
#254643=CARTESIAN_POINT('Ctrl Pts',(13.6105441559796,114.999999999998,8.24894058328078));
#254644=CARTESIAN_POINT('Ctrl Pts',(14.2512497473851,114.999999999999,8.42375809780361));
#254645=CARTESIAN_POINT('Ctrl Pts',(14.6298031864933,114.999999999999,8.52704699090316));
#254646=CARTESIAN_POINT('Ctrl Pts',(15.0075991707994,114.999999999999,8.63454839025221));
#254647=CARTESIAN_POINT('Ctrl Pts',(15.3847047117197,114.999999999999,8.74630124832653));
#254648=CARTESIAN_POINT('Ctrl Pts',(16.0185779527073,114.999999999999,8.93414560130087));
#254649=CARTESIAN_POINT('Ctrl Pts',(16.6510152471715,115.,9.13423879107251));
#254650=CARTESIAN_POINT('Ctrl Pts',(17.2813626508644,115.,9.34652047011719));
#254651=CARTESIAN_POINT('Ctrl Pts',(17.9026823885883,115.,9.55576190805272));
#254652=CARTESIAN_POINT('Ctrl Pts',(18.5219722813344,115.,9.77684545107347));
#254653=CARTESIAN_POINT('Ctrl Pts',(19.13858688252,115.,10.0097596336116));
#254654=CARTESIAN_POINT('Ctrl Pts',(19.5381882300233,115.,10.1607012769264));
#254655=CARTESIAN_POINT('Ctrl Pts',(19.936665603688,115.,10.3166124539101));
#254656=CARTESIAN_POINT('Ctrl Pts',(20.3338370957106,115.,10.4775));
#254657=CARTESIAN_POINT('',(90.,115.,10.4775));
#254658=CARTESIAN_POINT('',(-90.,115.,0.0381));
#254659=CARTESIAN_POINT('',(-20.509804815317,115.,10.4775));
#254660=CARTESIAN_POINT('Origin',(-90.,-90.,0.));
#254661=CARTESIAN_POINT('',(-90.,-114.492,0.0381));
#254662=CARTESIAN_POINT('',(-90.,-114.492,8.255));
#254663=CARTESIAN_POINT('',(-90.,-114.492,0.));
#254664=CARTESIAN_POINT('',(-114.492,-90.,0.0381));
#254665=CARTESIAN_POINT('Origin',(-90.,-90.,0.0381));
#254666=CARTESIAN_POINT('',(-114.492,-90.,8.255));
#254667=CARTESIAN_POINT('',(-114.492,-90.,0.));
#254668=CARTESIAN_POINT('Origin',(-90.,-90.,8.255));
#254669=CARTESIAN_POINT('Origin',(-114.492,-90.,0.));
#254670=CARTESIAN_POINT('',(-114.492,90.,0.0381));
#254671=CARTESIAN_POINT('',(-114.492,-90.,0.0381));
#254672=CARTESIAN_POINT('',(-114.492,90.,8.255));
#254673=CARTESIAN_POINT('',(-114.492,90.,0.));
#254674=CARTESIAN_POINT('',(-114.492,-90.,8.255));
#254675=CARTESIAN_POINT('Origin',(-90.,90.,0.));
#254676=CARTESIAN_POINT('',(-90.,114.492,0.0381));
#254677=CARTESIAN_POINT('Origin',(-90.,90.,0.0381));
#254678=CARTESIAN_POINT('',(-90.,114.492,8.255));
#254679=CARTESIAN_POINT('',(-90.,114.492,0.));
#254680=CARTESIAN_POINT('Origin',(-90.,90.,8.255));
#254681=CARTESIAN_POINT('Origin',(-9.33180860950279E-17,114.492,0.));
#254682=CARTESIAN_POINT('',(90.,114.492,0.0381));
#254683=CARTESIAN_POINT('',(-9.33180860950279E-17,114.492,0.0381));
#254684=CARTESIAN_POINT('',(90.,114.492,8.255));
#254685=CARTESIAN_POINT('',(90.,114.492,0.));
#254686=CARTESIAN_POINT('',(-9.33180860950279E-17,114.492,8.255));
#254687=CARTESIAN_POINT('Origin',(90.,90.,0.));
#254688=CARTESIAN_POINT('',(114.492,90.,0.0381));
#254689=CARTESIAN_POINT('Origin',(90.,90.,0.0381));
#254690=CARTESIAN_POINT('',(114.492,90.,8.255));
#254691=CARTESIAN_POINT('',(114.492,90.,0.));
#254692=CARTESIAN_POINT('Origin',(90.,90.,8.255));
#254693=CARTESIAN_POINT('Origin',(114.492,90.,0.));
#254694=CARTESIAN_POINT('',(114.492,-90.,0.0381));
#254695=CARTESIAN_POINT('',(114.492,90.,0.0381));
#254696=CARTESIAN_POINT('',(114.492,-90.,8.255));
#254697=CARTESIAN_POINT('',(114.492,-90.,0.));
#254698=CARTESIAN_POINT('',(114.492,90.,8.255));
#254699=CARTESIAN_POINT('Origin',(90.,-90.,0.));
#254700=CARTESIAN_POINT('',(90.,-114.492,0.0381));
#254701=CARTESIAN_POINT('Origin',(90.,-90.,0.0381));
#254702=CARTESIAN_POINT('',(90.,-114.492,8.255));
#254703=CARTESIAN_POINT('',(90.,-114.492,0.));
#254704=CARTESIAN_POINT('Origin',(90.,-90.,8.255));
#254705=CARTESIAN_POINT('Origin',(90.,-114.492,0.));
#254706=CARTESIAN_POINT('',(90.,-114.492,0.0381));
#254707=CARTESIAN_POINT('',(90.,-114.492,8.255));
#254708=CARTESIAN_POINT('Origin',(0.,0.,42.8625));
#254709=CARTESIAN_POINT('',(7.22543403703139,77.6928637726221,42.8625));
#254710=CARTESIAN_POINT('Ctrl Pts',(10.5032495111116,73.8913131000538,42.8625));
#254711=CARTESIAN_POINT('Ctrl Pts',(10.426573623364,73.9022121619655,42.8625));
#254712=CARTESIAN_POINT('Ctrl Pts',(10.350249684026,73.9154545309663,42.8625000002269));
#254713=CARTESIAN_POINT('Ctrl Pts',(10.2745222083119,73.931001476869,42.8624999983791));
#254714=CARTESIAN_POINT('Ctrl Pts',(10.1981874108863,73.946673106682,42.8624999965164));
#254715=CARTESIAN_POINT('Ctrl Pts',(10.1224588082033,73.9646863653303,42.8624999919999));
#254716=CARTESIAN_POINT('Ctrl Pts',(10.047564266732,73.9849532592727,42.8624999868104));
#254717=CARTESIAN_POINT('Ctrl Pts',(9.97591704949705,74.0043414085884,42.862499981846));
#254718=CARTESIAN_POINT('Ctrl Pts',(9.90503303994923,74.0257915565748,42.862499976793));
#254719=CARTESIAN_POINT('Ctrl Pts',(9.83509125233263,74.0491869849564,42.8624999769173));
#254720=CARTESIAN_POINT('Ctrl Pts',(9.72723746351632,74.0852639237641,42.8624999771091));
#254721=CARTESIAN_POINT('Ctrl Pts',(9.62130801394438,74.1260630720874,42.8624999885811));
#254722=CARTESIAN_POINT('Ctrl Pts',(9.51729215731884,74.1715977877844,42.8624999942969));
#254723=CARTESIAN_POINT('Ctrl Pts',(9.41339573292933,74.2170802199826,42.8625000000061));
#254724=CARTESIAN_POINT('Ctrl Pts',(9.31140854462795,74.2672878903899,42.8625));
#254725=CARTESIAN_POINT('Ctrl Pts',(9.21136369896946,74.3222619325388,42.8625));
#254726=CARTESIAN_POINT('Ctrl Pts',(9.01115900292839,74.4322732112421,42.8625));
#254727=CARTESIAN_POINT('Ctrl Pts',(8.81948930735858,74.5614957426143,42.8625));
#254728=CARTESIAN_POINT('Ctrl Pts',(8.64328937573657,74.7047213557556,42.8625));
#254729=CARTESIAN_POINT('Ctrl Pts',(8.46708944411456,74.8479469688968,42.8625));
#254730=CARTESIAN_POINT('Ctrl Pts',(8.30424197097439,75.0062320561475,42.8625));
#254731=CARTESIAN_POINT('Ctrl Pts',(8.15502818007546,75.1798937933935,42.8625));
#254732=CARTESIAN_POINT('Ctrl Pts',(8.00581438917653,75.3535555306395,42.8625));
#254733=CARTESIAN_POINT('Ctrl Pts',(7.87211185550338,75.5409911145111,42.8625));
#254734=CARTESIAN_POINT('Ctrl Pts',(7.75712923570172,75.7366472018307,42.8625));
#254735=CARTESIAN_POINT('Ctrl Pts',(7.64214661590005,75.9323032891504,42.8625));
#254736=CARTESIAN_POINT('Ctrl Pts',(7.54459734451585,76.1376228594692,42.8625));
#254737=CARTESIAN_POINT('Ctrl Pts',(7.46502587018254,76.3529077059775,42.8625));
#254738=CARTESIAN_POINT('Ctrl Pts',(7.43032647871625,76.4467887510171,42.8625));
#254739=CARTESIAN_POINT('Ctrl Pts',(7.39936062409065,76.5417780825022,42.8625000000769));
#254740=CARTESIAN_POINT('Ctrl Pts',(7.37217896131494,76.6375793109204,42.8624999987634));
#254741=CARTESIAN_POINT('Ctrl Pts',(7.34479976166629,76.7340767541082,42.8624999974405));
#254742=CARTESIAN_POINT('Ctrl Pts',(7.32125992945122,76.8313976035036,42.8624999944439));
#254743=CARTESIAN_POINT('Ctrl Pts',(7.30155838910551,76.9292381964642,42.8624999930524));
#254744=CARTESIAN_POINT('Ctrl Pts',(7.29596637731268,76.9570089057617,42.8624999926574));
#254745=CARTESIAN_POINT('Ctrl Pts',(7.29068326752703,76.9848214996602,42.8624999924193));
#254746=CARTESIAN_POINT('Ctrl Pts',(7.28570827437986,77.0126690806324,42.8624999924233));
#254747=CARTESIAN_POINT('Ctrl Pts',(7.26767335427593,77.1136197519324,42.8624999924377));
#254748=CARTESIAN_POINT('Ctrl Pts',(7.25364515271356,77.2152466870781,42.8624999955794));
#254749=CARTESIAN_POINT('Ctrl Pts',(7.2436697699919,77.3175670299304,42.8624999975182));
#254750=CARTESIAN_POINT('Ctrl Pts',(7.23366552760738,77.4201833945677,42.8624999994626));
#254751=CARTESIAN_POINT('Ctrl Pts',(7.22773765182402,77.5234975299984,42.8624999999651));
#254752=CARTESIAN_POINT('Ctrl Pts',(7.2259844893479,77.6275198622504,42.8624999999951));
#254753=CARTESIAN_POINT('Ctrl Pts',(7.22561791497349,77.6492702258872,42.8625000000014));
#254754=CARTESIAN_POINT('Ctrl Pts',(7.22543403727889,77.6710515175201,42.8625));
#254755=CARTESIAN_POINT('Ctrl Pts',(7.2254340370314,77.6928637726221,42.8625));
#254756=CARTESIAN_POINT('',(7.22543403703139,78.3977423334149,42.8625));
#254757=CARTESIAN_POINT('',(7.22543403703139,0.,42.8625));
#254758=CARTESIAN_POINT('',(-7.22543403703142,78.3977423334149,42.8625));
#254759=CARTESIAN_POINT('Origin',(-2.7565840235444E-14,7.21644966006352E-13,
42.8625));
#254760=CARTESIAN_POINT('',(-7.22543403703142,77.692863772622,42.8625));
#254761=CARTESIAN_POINT('',(-7.22543403703142,77.3778479789282,42.8625));
#254762=CARTESIAN_POINT('Ctrl Pts',(-7.22543403703142,77.692863772622,42.8625));
#254763=CARTESIAN_POINT('Ctrl Pts',(-7.22543403725474,77.6143782234018,
42.8625));
#254764=CARTESIAN_POINT('Ctrl Pts',(-7.22781601838741,77.535875429433,42.8625000001524));
#254765=CARTESIAN_POINT('Ctrl Pts',(-7.23257896759688,77.4576191255712,
42.8624999988625));
#254766=CARTESIAN_POINT('Ctrl Pts',(-7.2373752547902,77.3788150712969,42.8624999975636));
#254767=CARTESIAN_POINT('Ctrl Pts',(-7.24458590971855,77.3002611368071,
42.8624999944325));
#254768=CARTESIAN_POINT('Ctrl Pts',(-7.25415854935673,77.2222128388911,
42.8624999909559));
#254769=CARTESIAN_POINT('Ctrl Pts',(-7.26294887859024,77.1505429274844,
42.8624999877634));
#254770=CARTESIAN_POINT('Ctrl Pts',(-7.27373024842269,77.0792993096169,
42.8624999846283));
#254771=CARTESIAN_POINT('Ctrl Pts',(-7.28642524295417,77.0086679922574,
42.8624999847095));
#254772=CARTESIAN_POINT('Ctrl Pts',(-7.30654950086703,76.896702379059,42.8624999848383));
#254773=CARTESIAN_POINT('Ctrl Pts',(-7.33152154531227,76.7859978222717,
42.8624999924738));
#254774=CARTESIAN_POINT('Ctrl Pts',(-7.36134046899601,76.6765419257663,
42.862499996246));
#254775=CARTESIAN_POINT('Ctrl Pts',(-7.39115939267974,76.5670860292609,
42.8625000000181));
#254776=CARTESIAN_POINT('Ctrl Pts',(-7.42582567269418,76.4588786827971,
42.8625));
#254777=CARTESIAN_POINT('Ctrl Pts',(-7.46538237873601,76.3519435477325,
42.8625));
#254778=CARTESIAN_POINT('Ctrl Pts',(-7.54449579081965,76.1380732776034,
42.8625));
#254779=CARTESIAN_POINT('Ctrl Pts',(-7.64384406930363,75.928944977058,42.8625));
#254780=CARTESIAN_POINT('Ctrl Pts',(-7.7591908761306,75.733143325879,42.8625));
#254781=CARTESIAN_POINT('Ctrl Pts',(-7.87453768295757,75.5373416747,42.8625));
#254782=CARTESIAN_POINT('Ctrl Pts',(-8.00653344510973,75.3526470960584,
42.8625));
#254783=CARTESIAN_POINT('Ctrl Pts',(-8.15553849975887,75.1792999831171,
42.8625));
#254784=CARTESIAN_POINT('Ctrl Pts',(-8.30454355440801,75.0059528701759,
42.8625));
#254785=CARTESIAN_POINT('Ctrl Pts',(-8.4701285640905,74.8451674277897,42.8625));
#254786=CARTESIAN_POINT('Ctrl Pts',(-8.64644770717183,74.7021568742844,
42.8625));
#254787=CARTESIAN_POINT('Ctrl Pts',(-8.82276685025317,74.5591463207792,
42.8625));
#254788=CARTESIAN_POINT('Ctrl Pts',(-9.01121135579652,74.4321791961687,
42.8625));
#254789=CARTESIAN_POINT('Ctrl Pts',(-9.21219622436481,74.3218046004446,
42.8625));
#254790=CARTESIAN_POINT('Ctrl Pts',(-9.29461898157906,74.2765406033547,
42.8625));
#254791=CARTESIAN_POINT('Ctrl Pts',(-9.3786096001277,74.234394079442,42.8625000000289));
#254792=CARTESIAN_POINT('Ctrl Pts',(-9.46387041307998,74.1954908710541,
42.862499999644));
#254793=CARTESIAN_POINT('Ctrl Pts',(-9.54941687963667,74.156457323284,42.8624999992578));
#254794=CARTESIAN_POINT('Ctrl Pts',(-9.63624170706638,74.120688949303,42.8624999983669));
#254795=CARTESIAN_POINT('Ctrl Pts',(-9.72402969290818,74.0882624434769,
42.8624999977847));
#254796=CARTESIAN_POINT('Ctrl Pts',(-9.76209983406389,74.0742003637726,
42.8624999975322));
#254797=CARTESIAN_POINT('Ctrl Pts',(-9.80035095542473,74.0607661112639,
42.8624999973601));
#254798=CARTESIAN_POINT('Ctrl Pts',(-9.83875676785274,74.0479629529335,
42.8624999973602));
#254799=CARTESIAN_POINT('Ctrl Pts',(-9.93044982501336,74.0173956857827,
42.8624999973604));
#254800=CARTESIAN_POINT('Ctrl Pts',(-10.0232647089801,73.9903401118788,
42.8624999983476));
#254801=CARTESIAN_POINT('Ctrl Pts',(-10.117219177538,73.9668292728909,42.8624999990185));
#254802=CARTESIAN_POINT('Ctrl Pts',(-10.2108353927062,73.9434030772532,
42.8624999996869));
#254803=CARTESIAN_POINT('Ctrl Pts',(-10.3055833706996,73.9234960907884,
42.8624999999561));
#254804=CARTESIAN_POINT('Ctrl Pts',(-10.4014866529399,73.9071922766141,
42.8624999999904));
#254805=CARTESIAN_POINT('Ctrl Pts',(-10.4352639087986,73.9014500528864,
42.8625000000025));
#254806=CARTESIAN_POINT('Ctrl Pts',(-10.4691845033362,73.8961552566244,
42.8625));
#254807=CARTESIAN_POINT('Ctrl Pts',(-10.5032495111116,73.8913131000538,
42.8625));
#254808=CARTESIAN_POINT('Origin',(-9.76543403703142,0.,-7.78106734735282));
#254809=CARTESIAN_POINT('',(-9.76543403703142,80.4599485582789,18.0027617587917));
#254810=CARTESIAN_POINT('',(-9.76543403703142,77.6928637726221,40.3225000000001));
#254811=CARTESIAN_POINT('Ctrl Pts',(-9.76543403703142,80.4599485582789,
18.0027617587917));
#254812=CARTESIAN_POINT('Ctrl Pts',(-9.76543403703142,79.5378854526247,
25.4427115049615));
#254813=CARTESIAN_POINT('Ctrl Pts',(-9.76543403703142,78.6155344836223,
32.882625582014));
#254814=CARTESIAN_POINT('Ctrl Pts',(-9.76543403703142,77.6928637726221,
40.3225000000001));
#254815=CARTESIAN_POINT('',(-9.76543403703142,80.6811576396149,40.3225));
#254816=CARTESIAN_POINT('',(-9.76543403703142,80.6811576396149,40.3225));
#254817=CARTESIAN_POINT('',(-9.76543404548309,80.681157776892,12.5890686048436));
#254818=CARTESIAN_POINT('',(-9.76543403703142,80.6811576396149,-7.78106734735282));
#254819=CARTESIAN_POINT('',(-9.76543403703142,80.9266905754733,12.3233805729971));
#254820=CARTESIAN_POINT('Ctrl Pts',(-9.76543403703143,80.6811579176687,
12.5890686048431));
#254821=CARTESIAN_POINT('Ctrl Pts',(-9.76543403703143,80.6811578105629,
12.5570686364181));
#254822=CARTESIAN_POINT('Ctrl Pts',(-9.76543403703142,80.6869824098219,
12.5253022376631));
#254823=CARTESIAN_POINT('Ctrl Pts',(-9.76543403703142,80.7103539169444,
12.463082263983));
#254824=CARTESIAN_POINT('Ctrl Pts',(-9.76543403703142,80.7285809497644,
12.4334024804021));
#254825=CARTESIAN_POINT('Ctrl Pts',(-9.76543403703142,80.7750888892602,
12.3827419313172));
#254826=CARTESIAN_POINT('Ctrl Pts',(-9.76543403703142,80.8029593811073,
12.3621289066386));
#254827=CARTESIAN_POINT('Ctrl Pts',(-9.76543403703142,80.8631242630206,
12.3337462130289));
#254828=CARTESIAN_POINT('Ctrl Pts',(-9.76543403703142,80.8945537377669,
12.3255084948528));
#254829=CARTESIAN_POINT('Ctrl Pts',(-9.76543403703142,80.9266905754733,
12.3233805729971));
#254830=CARTESIAN_POINT('',(-9.76543403703143,80.665181319947,12.34051373381));
#254831=CARTESIAN_POINT('Ctrl Pts',(-9.76543403703143,80.926690388265,12.3233777475718));
#254832=CARTESIAN_POINT('Ctrl Pts',(-9.76543403703143,80.8448494085605,
12.3287937059475));
#254833=CARTESIAN_POINT('Ctrl Pts',(-9.7654340370323,80.7630051677245,12.3341606246062));
#254834=CARTESIAN_POINT('Ctrl Pts',(-9.76543403703142,80.6811576390292,
12.3394767046348));
#254835=CARTESIAN_POINT('Ctrl Pts',(-9.76543403703137,80.6758322137124,
12.3398225964122));
#254836=CARTESIAN_POINT('Ctrl Pts',(-9.76543403703143,80.6705067738252,
12.340168272985));
#254837=CARTESIAN_POINT('Ctrl Pts',(-9.76543403703143,80.665181319947,12.34051373381));
#254838=CARTESIAN_POINT('',(-9.76543403703142,80.5172782442711,12.3495568918955));
#254839=CARTESIAN_POINT('Ctrl Pts',(-9.76543403703142,80.6651826441481,
12.3405342165937));
#254840=CARTESIAN_POINT('Ctrl Pts',(-9.76543403703142,80.6405620413662,
12.3421295047908));
#254841=CARTESIAN_POINT('Ctrl Pts',(-9.76543403703209,80.6159377423552,
12.3436782076836));
#254842=CARTESIAN_POINT('Ctrl Pts',(-9.76543403703209,80.5666366040391,
12.3466857490819));
#254843=CARTESIAN_POINT('Ctrl Pts',(-9.76543403703142,80.5419584195077,
12.3481444872065));
#254844=CARTESIAN_POINT('Ctrl Pts',(-9.76543403703143,80.5172782442762,
12.3495568919838));
#254845=CARTESIAN_POINT('',(-9.76543403703142,80.5172782427122,17.0741173620445));
#254846=CARTESIAN_POINT('',(-9.76543403703142,80.5172782427122,-7.78106734735282));
#254847=CARTESIAN_POINT('Origin',(-9.76543403703113,72.9739056302811,17.0745205117662));
#254848=CARTESIAN_POINT('Origin',(9.7654340370314,0.,-7.78106734735282));
#254849=CARTESIAN_POINT('',(9.76543403927482,80.6811576732767,12.5890686048444));
#254850=CARTESIAN_POINT('',(9.7654340370314,80.6811576396149,40.3225));
#254851=CARTESIAN_POINT('',(9.7654340370314,80.6811576396149,-7.78106734735282));
#254852=CARTESIAN_POINT('',(9.7654340370314,77.6928637726221,40.3225));
#254853=CARTESIAN_POINT('',(9.7654340370314,0.,40.3225));
#254854=CARTESIAN_POINT('',(9.7654340370314,80.4599485582789,18.0027617587916));
#254855=CARTESIAN_POINT('Ctrl Pts',(9.7654340370314,77.6928637726221,40.3225));
#254856=CARTESIAN_POINT('Ctrl Pts',(9.7654340370314,78.6155344836223,32.8826255820139));
#254857=CARTESIAN_POINT('Ctrl Pts',(9.7654340370314,79.5378854526247,25.4427115049614));
#254858=CARTESIAN_POINT('Ctrl Pts',(9.7654340370314,80.4599485582789,18.0027617587916));
#254859=CARTESIAN_POINT('',(9.7654340370314,80.5172782427122,17.0741173620444));
#254860=CARTESIAN_POINT('Origin',(9.76543403703169,72.973905630281,17.0745205117664));
#254861=CARTESIAN_POINT('',(9.7654340370314,80.5172782442711,12.3495568918922));
#254862=CARTESIAN_POINT('',(9.7654340370314,80.5172782427122,12.3825));
#254863=CARTESIAN_POINT('',(9.76543420245325,80.6651818783829,12.3405137312319));
#254864=CARTESIAN_POINT('Ctrl Pts',(9.76543403703139,80.5172782442762,12.3495568919806));
#254865=CARTESIAN_POINT('Ctrl Pts',(9.76543403703139,80.5419584195096,12.3481444872035));
#254866=CARTESIAN_POINT('Ctrl Pts',(9.76543403703206,80.5666366040432,12.3466857490791));
#254867=CARTESIAN_POINT('Ctrl Pts',(9.76543403703206,80.6159377423668,12.3436782076814));
#254868=CARTESIAN_POINT('Ctrl Pts',(9.7654340370314,80.6405620413825,12.3421295047889));
#254869=CARTESIAN_POINT('Ctrl Pts',(9.7654340370314,80.6651826441691,12.3405342165921));
#254870=CARTESIAN_POINT('',(9.76543402142917,80.9266904157755,12.3233781631543));
#254871=CARTESIAN_POINT('Ctrl Pts',(9.76543403703141,80.6651813199679,12.3405137338087));
#254872=CARTESIAN_POINT('Ctrl Pts',(9.76543403703141,80.6705067738392,12.340168272984));
#254873=CARTESIAN_POINT('Ctrl Pts',(9.76543403703134,80.6758322137194,12.3398225964117));
#254874=CARTESIAN_POINT('Ctrl Pts',(9.7654340370314,80.6811576390292,12.3394767046348));
#254875=CARTESIAN_POINT('Ctrl Pts',(9.76543403703227,80.7630051677206,12.3341606246064));
#254876=CARTESIAN_POINT('Ctrl Pts',(9.7654340370314,80.8448494085526,12.328793705948));
#254877=CARTESIAN_POINT('Ctrl Pts',(9.76543403703287,80.9266903882648,12.3233777475721));
#254878=CARTESIAN_POINT('Ctrl Pts',(9.76543403703139,80.9266904439379,12.3233785886619));
#254879=CARTESIAN_POINT('Ctrl Pts',(9.76543403703139,80.8945868905325,12.3255033793116));
#254880=CARTESIAN_POINT('Ctrl Pts',(9.7654340370314,80.8631886795284,12.3337259175107));
#254881=CARTESIAN_POINT('Ctrl Pts',(9.7654340370314,80.8030451610623,12.3620704955522));
#254882=CARTESIAN_POINT('Ctrl Pts',(9.7654340370314,80.775168642564,12.3826717602365));
#254883=CARTESIAN_POINT('Ctrl Pts',(9.7654340370314,80.7286417308444,12.4333137812977));
#254884=CARTESIAN_POINT('Ctrl Pts',(9.76543403703139,80.7104027846362,12.4629878785952));
#254885=CARTESIAN_POINT('Ctrl Pts',(9.76543403703139,80.6869950181105,12.5252327683005));
#254886=CARTESIAN_POINT('Ctrl Pts',(9.7654340370314,80.6811576872882,12.5570338786658));
#254887=CARTESIAN_POINT('Ctrl Pts',(9.7654340370314,80.6811577086292,12.5890686048444));
#254888=CARTESIAN_POINT('Origin',(-2.7565840235444E-14,7.21644966006352E-13,
-7.78106734735282));
#254889=CARTESIAN_POINT('Origin',(-2.7565840235444E-14,7.21644966006352E-13,
40.3225));
#254890=CARTESIAN_POINT('Ctrl Pts',(9.76543403530562,80.6811576398238,12.5890686044732));
#254891=CARTESIAN_POINT('Ctrl Pts',(8.642707260293,80.8170495206766,12.3475861026818));
#254892=CARTESIAN_POINT('Ctrl Pts',(7.51318753972854,80.929982574631,12.1455679037829));
#254893=CARTESIAN_POINT('Ctrl Pts',(6.37776783703217,81.0193617440728,11.9852102203789));
#254894=CARTESIAN_POINT('Ctrl Pts',(5.89168688638967,81.0576255786238,11.9165599979046));
#254895=CARTESIAN_POINT('Ctrl Pts',(5.40452517458145,81.0915728838979,11.8555451261434));
#254896=CARTESIAN_POINT('Ctrl Pts',(4.91635528551654,81.1211584650181,11.8023379231986));
#254897=CARTESIAN_POINT('Ctrl Pts',(4.10212074979073,81.1705052241018,11.7135918879401));
#254898=CARTESIAN_POINT('Ctrl Pts',(3.28481153395651,81.2077378726861,11.6464808182021));
#254899=CARTESIAN_POINT('Ctrl Pts',(2.46434966086494,81.2326281782696,11.6015974754808));
#254900=CARTESIAN_POINT('Ctrl Pts',(1.98330333770676,81.2472216534522,11.5752818504709));
#254901=CARTESIAN_POINT('Ctrl Pts',(1.50074701423457,81.2575796604344,11.5566086492317));
#254902=CARTESIAN_POINT('Ctrl Pts',(1.01746939332227,81.2636305860971,11.5456857536254));
#254903=CARTESIAN_POINT('Ctrl Pts',(0.676479489490327,81.267899984204,11.5379788022559));
#254904=CARTESIAN_POINT('Ctrl Pts',(0.335130586181492,81.2700262217726,
11.534130262006));
#254905=CARTESIAN_POINT('Ctrl Pts',(-0.00629963612498389,81.2699997558422,
11.5341780279657));
#254906=CARTESIAN_POINT('Ctrl Pts',(-0.861676302009446,81.2699334514031,
11.5342976948395));
#254907=CARTESIAN_POINT('Ctrl Pts',(-1.71371687815596,81.2563671514032,
11.5588752590179));
#254908=CARTESIAN_POINT('Ctrl Pts',(-2.56248731492883,81.2295916446761,
11.6072244931474));
#254909=CARTESIAN_POINT('Ctrl Pts',(-3.41597307225165,81.2026673873663,
11.6558423301021));
#254910=CARTESIAN_POINT('Ctrl Pts',(-4.26615255418888,81.1623867763625,
11.7284966963816));
#254911=CARTESIAN_POINT('Ctrl Pts',(-5.11310836102155,81.1089947101334,
11.8244898640261));
#254912=CARTESIAN_POINT('Ctrl Pts',(-5.9665546510357,81.055193484058,11.9212186568769));
#254913=CARTESIAN_POINT('Ctrl Pts',(-6.81672796889863,80.9880791154851,
12.0416453265388));
#254914=CARTESIAN_POINT('Ctrl Pts',(-7.6637240426148,80.9078502606431,12.1850559811004));
#254915=CARTESIAN_POINT('Ctrl Pts',(-8.36646147164548,80.8412858208124,
12.3040412253177));
#254916=CARTESIAN_POINT('Ctrl Pts',(-9.06701205871129,80.7656927894985,
12.4388480077385));
#254917=CARTESIAN_POINT('Ctrl Pts',(-9.76543402933603,80.6811576405463,
12.5890686031893));
#254918=CARTESIAN_POINT('Ctrl Pts',(-20.509804815317,115.,12.3825));
#254919=CARTESIAN_POINT('Ctrl Pts',(-9.76543403703142,80.,12.3825));
#254920=CARTESIAN_POINT('Ctrl Pts',(-7.2108267586496,115.,6.80385564663691));
#254921=CARTESIAN_POINT('Ctrl Pts',(-3.29772532864429,80.,11.0907130840649));
#254922=CARTESIAN_POINT('Ctrl Pts',(7.21082675864964,115.,6.80385564663692));
#254923=CARTESIAN_POINT('Ctrl Pts',(3.29772532864426,80.,11.0907130840649));
#254924=CARTESIAN_POINT('Ctrl Pts',(20.509804815317,115.,12.3825));
#254925=CARTESIAN_POINT('Ctrl Pts',(9.76543403703139,80.,12.3825));
#254926=CARTESIAN_POINT('Ctrl Pts',(-9.76543348183844,80.9266905678574,
12.3233804598558));
#254927=CARTESIAN_POINT('Ctrl Pts',(-9.21901381841984,80.9911564147534,
12.2072621082779));
#254928=CARTESIAN_POINT('Ctrl Pts',(-8.67068521395711,81.0503803664516,
12.1003581949099));
#254929=CARTESIAN_POINT('Ctrl Pts',(-8.12078457076909,81.1042435940398,
12.0029639875845));
#254930=CARTESIAN_POINT('Ctrl Pts',(-7.57790689040143,81.1574189165503,
11.9068136338632));
#254931=CARTESIAN_POINT('Ctrl Pts',(-7.03349709193297,81.2053695632012,
11.8199316855308));
#254932=CARTESIAN_POINT('Ctrl Pts',(-6.48788508382262,81.2480057885138,
11.7425585631889));
#254933=CARTESIAN_POINT('Ctrl Pts',(-5.96432468672382,81.2889188159466,
11.6683125750949));
#254934=CARTESIAN_POINT('Ctrl Pts',(-5.43965733257562,81.3249384348352,
11.6028221508719));
#254935=CARTESIAN_POINT('Ctrl Pts',(-4.91417937346711,81.3560071311834,
11.5462604754853));
#254936=CARTESIAN_POINT('Ctrl Pts',(-3.90861272828337,81.4154608993492,
11.438022759367));
#254937=CARTESIAN_POINT('Ctrl Pts',(-2.89900702900751,81.4568548427787,
11.3623506147986));
#254938=CARTESIAN_POINT('Ctrl Pts',(-1.88524103826131,81.4798101320474,
11.3203203829979));
#254939=CARTESIAN_POINT('Ctrl Pts',(-1.25840892529359,81.49400385388,11.2943322365729));
#254940=CARTESIAN_POINT('Ctrl Pts',(-0.629986214081505,81.5011476552561,
11.2812069510319));
#254941=CARTESIAN_POINT('Ctrl Pts',(5.60440135014445E-5,81.5011472661906,
11.2812077224205));
#254942=CARTESIAN_POINT('Ctrl Pts',(0.000515968424032919,81.5011472659066,
11.2812077229836));
#254943=CARTESIAN_POINT('Ctrl Pts',(0.000975892644772834,81.5011472617952,
11.2812077305293));
#254944=CARTESIAN_POINT('Ctrl Pts',(0.0014358166751247,81.5011472538564,
11.2812077450575));
#254945=CARTESIAN_POINT('Ctrl Pts',(0.826165080880329,81.5011330182027,
11.2812337967929));
#254946=CARTESIAN_POINT('Ctrl Pts',(1.65023405465531,81.4888253830682,11.3037129450655));
#254947=CARTESIAN_POINT('Ctrl Pts',(2.47001199742806,81.4644891219574,11.3481105561519));
#254948=CARTESIAN_POINT('Ctrl Pts',(2.48653380514781,81.4639986488601,11.3490053457715));
#254949=CARTESIAN_POINT('Ctrl Pts',(2.50305394112712,81.4635032893928,11.3499090412207));
#254950=CARTESIAN_POINT('Ctrl Pts',(2.51957237562734,81.4630030456335,11.3508216382509));
#254951=CARTESIAN_POINT('Ctrl Pts',(3.32266451172049,81.4386822282343,11.3951902192021));
#254952=CARTESIAN_POINT('Ctrl Pts',(4.12282671528089,81.4028175892564,11.4605982502462));
#254953=CARTESIAN_POINT('Ctrl Pts',(4.92000987776074,81.3556286372825,11.5464932122947));
#254954=CARTESIAN_POINT('Ctrl Pts',(4.95329825353372,81.3536581446283,11.550079971158));
#254955=CARTESIAN_POINT('Ctrl Pts',(4.98658143225163,81.351667909035,11.5537024490998));
#254956=CARTESIAN_POINT('Ctrl Pts',(5.01985942551591,81.3496579463146,11.5573606066733));
#254957=CARTESIAN_POINT('Ctrl Pts',(6.01122202727515,81.289780481464,11.6663383500398));
#254958=CARTESIAN_POINT('Ctrl Pts',(6.99804347270548,81.2124024895723,11.8070343424507));
#254959=CARTESIAN_POINT('Ctrl Pts',(7.98047918803816,81.1178563623326,11.9781794191987));
#254960=CARTESIAN_POINT('Ctrl Pts',(8.57707028891758,81.0604425516847,12.082108488708));
#254961=CARTESIAN_POINT('Ctrl Pts',(9.17204397683082,80.9966972889915,12.1972669259026));
#254962=CARTESIAN_POINT('Ctrl Pts',(9.76543387174275,80.9266904417031,12.3233785549721));
#254963=CARTESIAN_POINT('',(19.6234043038483,113.315263490685,12.231294241899));
#254964=CARTESIAN_POINT('Ctrl Pts',(9.76543420245325,80.6651818783829,12.3405137312319));
#254965=CARTESIAN_POINT('Ctrl Pts',(11.3799678060561,86.1153669381273,12.3153647150579));
#254966=CARTESIAN_POINT('Ctrl Pts',(13.0205007967692,91.5578166430438,12.2930000217267));
#254967=CARTESIAN_POINT('Ctrl Pts',(16.313066495143,102.439221084592,12.2572978841659));
#254968=CARTESIAN_POINT('Ctrl Pts',(17.9668525537566,107.877661915077,12.243175008079));
#254969=CARTESIAN_POINT('Ctrl Pts',(19.6234043038483,113.315263490685,12.231294241899));
#254970=CARTESIAN_POINT('',(-19.6234043038483,113.315263490685,12.231294241899));
#254971=CARTESIAN_POINT('Ctrl Pts',(19.6234043038483,113.315263490685,12.231294241899));
#254972=CARTESIAN_POINT('Ctrl Pts',(18.8409284740723,113.311274371647,11.9148273395859));
#254973=CARTESIAN_POINT('Ctrl Pts',(18.0498151499385,113.307504020477,11.6169295778476));
#254974=CARTESIAN_POINT('Ctrl Pts',(16.459706385983,113.300453260057,11.0615401298248));
#254975=CARTESIAN_POINT('Ctrl Pts',(15.6610703781754,113.297173414208,10.804088311671));
#254976=CARTESIAN_POINT('Ctrl Pts',(13.2546236809651,113.288070000624,10.0912959618231));
#254977=CARTESIAN_POINT('Ctrl Pts',(11.6362978866301,113.282981629452,9.69538531766471));
#254978=CARTESIAN_POINT('Ctrl Pts',(6.73998365714194,113.270687155678,8.74128236982949));
#254979=CARTESIAN_POINT('Ctrl Pts',(3.42104711494492,113.266433067362,8.41452184068842));
#254980=CARTESIAN_POINT('Ctrl Pts',(-3.33143264129344,113.266357991278,
8.40873611349764));
#254981=CARTESIAN_POINT('Ctrl Pts',(-6.66356650895994,113.270541327779,
8.73001511549867));
#254982=CARTESIAN_POINT('Ctrl Pts',(-11.5933138606595,113.282851235877,
9.68524203411009));
#254983=CARTESIAN_POINT('Ctrl Pts',(-13.2269544959225,113.287971157042,
10.0835711394783));
#254984=CARTESIAN_POINT('Ctrl Pts',(-16.4641399389958,113.300205589209,
11.041491514323));
#254985=CARTESIAN_POINT('Ctrl Pts',(-18.0583770680721,113.307284867316,
11.5983298709949));
#254986=CARTESIAN_POINT('Ctrl Pts',(-19.6234043038483,113.315263490685,
12.231294241899));
#254987=CARTESIAN_POINT('Ctrl Pts',(-19.6234043038483,113.315263490685,
12.231294241899));
#254988=CARTESIAN_POINT('Ctrl Pts',(-17.9668525537554,107.877661915073,
12.243175008079));
#254989=CARTESIAN_POINT('Ctrl Pts',(-16.3130664951407,102.439221084584,
12.2572978841659));
#254990=CARTESIAN_POINT('Ctrl Pts',(-13.0205007967646,91.5578166430286,
12.2930000217267));
#254991=CARTESIAN_POINT('Ctrl Pts',(-11.379967806051,86.11536693811,12.3153647150579));
#254992=CARTESIAN_POINT('Ctrl Pts',(-9.76543420245328,80.6651818783619,
12.3405137312333));
#254993=CARTESIAN_POINT('Origin',(0.,0.,12.3825));
#254994=CARTESIAN_POINT('',(24.758292886385,76.0725110230494,12.3825));
#254995=CARTESIAN_POINT('',(10.8629841634368,79.2590409673554,12.3825));
#254996=CARTESIAN_POINT('Origin',(0.,0.,12.3825));
#254997=CARTESIAN_POINT('',(10.8629841634368,79.2590409673554,17.0741173620444));
#254998=CARTESIAN_POINT('',(10.8629841634368,79.2590409673554,12.3825));
#254999=CARTESIAN_POINT('',(24.758292886385,76.0725110230494,17.0741173620444));
#255000=CARTESIAN_POINT('Origin',(0.,0.,17.0741173620444));
#255001=CARTESIAN_POINT('',(24.758292886385,76.0725110230494,12.3825));
#255002=CARTESIAN_POINT('Origin',(0.,0.,12.3825));
#255003=CARTESIAN_POINT('',(20.3338370957106,113.095,12.3825));
#255004=CARTESIAN_POINT('',(20.509804815317,113.095,12.3825));
#255005=CARTESIAN_POINT('',(9.93397247946587,79.8850738159598,12.3825));
#255006=CARTESIAN_POINT('Ctrl Pts',(20.3338370957106,113.095,12.3825));
#255007=CARTESIAN_POINT('Ctrl Pts',(18.6162390952454,107.555098952883,12.3825));
#255008=CARTESIAN_POINT('Ctrl Pts',(16.8951673474018,102.01627317443,12.3824999999886));
#255009=CARTESIAN_POINT('Ctrl Pts',(15.1653526441753,96.4801751438902,12.3824999999964));
#255010=CARTESIAN_POINT('Ctrl Pts',(15.1549732951004,96.446957080785,12.3824999999964));
#255011=CARTESIAN_POINT('Ctrl Pts',(15.1445936258827,96.4137391176421,12.3824999999965));
#255012=CARTESIAN_POINT('Ctrl Pts',(15.1342136354895,96.3805212547838,12.3824999999965));
#255013=CARTESIAN_POINT('Ctrl Pts',(14.2708587200199,93.6176280252437,12.3824999999987));
#255014=CARTESIAN_POINT('Ctrl Pts',(13.4057207197965,90.8552856382803,12.3824999997191));
#255015=CARTESIAN_POINT('Ctrl Pts',(12.5362227209559,88.0943201478487,12.3824999994597));
#255016=CARTESIAN_POINT('Ctrl Pts',(11.7595790473135,85.6282001750045,12.382499999228));
#255017=CARTESIAN_POINT('Ctrl Pts',(10.9794584946655,83.1631782350712,12.3824999997221));
#255018=CARTESIAN_POINT('Ctrl Pts',(10.1939933986301,80.6998523967545,12.3824999999539));
#255019=CARTESIAN_POINT('Ctrl Pts',(10.1073856377522,80.4282386277326,12.3824999999794));
#255020=CARTESIAN_POINT('Ctrl Pts',(10.020712846965,80.1566454956651,12.3824999999961));
#255021=CARTESIAN_POINT('Ctrl Pts',(9.93397247946587,79.8850738159598,12.3824999999994));
#255022=CARTESIAN_POINT('Origin',(11.0354340370314,80.5172782427122,12.3825));
#255023=CARTESIAN_POINT('',(27.0012528338594,76.4071670555372,12.3825));
#255024=CARTESIAN_POINT('Origin',(25.5443686855278,78.4878132480313,12.3825));
#255025=CARTESIAN_POINT('',(75.6605890912238,110.478801107225,12.3825));
#255026=CARTESIAN_POINT('Origin',(0.,0.,12.3825));
#255027=CARTESIAN_POINT('',(-10.8629841634369,79.2590409673554,12.3825));
#255028=CARTESIAN_POINT('',(-9.93397247946588,79.8850738159598,12.3825));
#255029=CARTESIAN_POINT('Origin',(-11.0354340370314,80.5172782427122,12.3825));
#255030=CARTESIAN_POINT('',(-20.3338370957106,113.095,12.3825));
#255031=CARTESIAN_POINT('Ctrl Pts',(-9.93397247946588,79.8850738159598,
12.3824999999994));
#255032=CARTESIAN_POINT('Ctrl Pts',(-10.7214025854466,82.3504048111719,
12.3824999999692));
#255033=CARTESIAN_POINT('Ctrl Pts',(-11.5032683361806,84.8175022341616,
12.3824999992383));
#255034=CARTESIAN_POINT('Ctrl Pts',(-12.281448300187,87.2857645884932,12.3824999993952));
#255035=CARTESIAN_POINT('Ctrl Pts',(-13.2367907647368,90.3159580524864,
12.3824999995878));
#255036=CARTESIAN_POINT('Ctrl Pts',(-14.1865759945479,93.3479079281245,
12.3824999999989));
#255037=CARTESIAN_POINT('Ctrl Pts',(-15.1342136355012,96.3805212547678,
12.3824999999965));
#255038=CARTESIAN_POINT('Ctrl Pts',(-15.1445936258955,96.4137391176299,
12.3824999999965));
#255039=CARTESIAN_POINT('Ctrl Pts',(-15.1549732951142,96.4469570807766,
12.3824999999964));
#255040=CARTESIAN_POINT('Ctrl Pts',(-15.1653526441902,96.4801751438856,
12.3824999999964));
#255041=CARTESIAN_POINT('Ctrl Pts',(-16.8951673474031,102.016273174429,
12.3824999999886));
#255042=CARTESIAN_POINT('Ctrl Pts',(-18.6162390953258,107.555098952858,
12.3825));
#255043=CARTESIAN_POINT('Ctrl Pts',(-20.3338370957106,113.095,12.3825));
#255044=CARTESIAN_POINT('',(-90.,113.095,12.3825));
#255045=CARTESIAN_POINT('',(-27.0012528338594,76.4071670555372,12.3825));
#255046=CARTESIAN_POINT('',(-75.6605890912239,110.478801107225,12.3825));
#255047=CARTESIAN_POINT('',(-24.758292886385,76.0725110230494,12.3825));
#255048=CARTESIAN_POINT('Origin',(-25.5443686855278,78.4878132480313,12.3825));
#255049=CARTESIAN_POINT('Origin',(0.,0.,12.3825));
#255050=CARTESIAN_POINT('Origin',(0.,0.,12.3825));
#255051=CARTESIAN_POINT('',(-24.758292886385,76.0725110230494,17.0741173620445));
#255052=CARTESIAN_POINT('',(-10.8629841634369,79.2590409673554,17.0741173620445));
#255053=CARTESIAN_POINT('Origin',(0.,0.,17.0741173620445));
#255054=CARTESIAN_POINT('',(-10.8629841634369,79.2590409673554,12.3825));
#255055=CARTESIAN_POINT('',(-24.758292886385,76.0725110230494,12.3825));
#255056=CARTESIAN_POINT('Origin',(-90.,-90.,17.4625));
#255057=CARTESIAN_POINT('',(-109.438478010978,76.3890311653897,17.4625));
#255058=CARTESIAN_POINT('',(-76.7149512087496,29.6549915892152,17.4625));
#255059=CARTESIAN_POINT('',(-24.8661421402461,-44.3927817339206,17.4625));
#255060=CARTESIAN_POINT('',(-29.6549915892152,76.7149512087496,17.4625));
#255061=CARTESIAN_POINT('Origin',(0.,0.,17.4625));
#255062=CARTESIAN_POINT('',(-76.3890311653897,109.438478010978,17.4625));
#255063=CARTESIAN_POINT('',(8.18330470534212,50.220290910288,17.4625));
#255064=CARTESIAN_POINT('Origin',(-90.,90.,17.4625));
#255065=CARTESIAN_POINT('Origin',(0.,0.,12.3825));
#255066=CARTESIAN_POINT('Origin',(0.,0.,14.2875));
#255067=CARTESIAN_POINT('Origin',(-90.,-90.,17.4625));
#255068=CARTESIAN_POINT('',(-76.3890311653897,-109.438478010978,17.4625));
#255069=CARTESIAN_POINT('',(-29.6549915892153,-76.7149512087495,17.4625));
#255070=CARTESIAN_POINT('',(-76.3890311653897,-109.438478010978,17.4625));
#255071=CARTESIAN_POINT('',(-76.7149512087496,-29.6549915892152,17.4625));
#255072=CARTESIAN_POINT('Origin',(0.,0.,17.4625));
#255073=CARTESIAN_POINT('',(-109.438478010978,-76.3890311653897,17.4625));
#255074=CARTESIAN_POINT('',(-109.438478010978,-76.3890311653897,17.4625));
#255075=CARTESIAN_POINT('Origin',(-90.,-90.,17.4625));
#255076=CARTESIAN_POINT('Origin',(0.,0.,12.3825));
#255077=CARTESIAN_POINT('',(-24.7582928863851,-76.0725110230494,17.0741173620444));
#255078=CARTESIAN_POINT('',(-24.7582928863851,-76.0725110230494,14.2875));
#255079=CARTESIAN_POINT('',(-24.7582928863851,-76.0725110230494,12.3825));
#255080=CARTESIAN_POINT('',(24.758292886385,-76.0725110230494,14.2875));
#255081=CARTESIAN_POINT('Origin',(0.,0.,14.2875));
#255082=CARTESIAN_POINT('',(24.758292886385,-76.0725110230494,17.0741173620444));
#255083=CARTESIAN_POINT('',(24.758292886385,-76.0725110230494,12.3825));
#255084=CARTESIAN_POINT('Origin',(0.,0.,17.0741173620444));
#255085=CARTESIAN_POINT('Origin',(-90.,-90.,17.4625));
#255086=CARTESIAN_POINT('',(76.7149512087496,-29.6549915892152,17.4625));
#255087=CARTESIAN_POINT('',(50.220290910288,8.18330470534212,17.4625));
#255088=CARTESIAN_POINT('',(29.6549915892152,-76.7149512087496,17.4625));
#255089=CARTESIAN_POINT('Origin',(0.,0.,17.4625));
#255090=CARTESIAN_POINT('',(-44.3927817339206,-24.8661421402461,17.4625));
#255091=CARTESIAN_POINT('Origin',(-90.,-90.,17.4625));
#255092=CARTESIAN_POINT('',(29.6549915892153,76.7149512087496,17.4625));
#255093=CARTESIAN_POINT('',(-128.965117604652,-34.3520449604438,17.4625));
#255094=CARTESIAN_POINT('',(76.7149512087496,29.6549915892152,17.4625));
#255095=CARTESIAN_POINT('Origin',(0.,0.,17.4625));
#255096=CARTESIAN_POINT('',(-34.3520449604435,-128.965117604652,17.4625));
#255097=CARTESIAN_POINT('Origin',(75.6605890912238,110.478801107225,12.3825));
#255098=CARTESIAN_POINT('',(27.0012528338594,76.4071670555372,16.0836603564334));
#255099=CARTESIAN_POINT('',(27.0012528338594,76.4071670555372,17.0741173620444));
#255100=CARTESIAN_POINT('',(27.1270025958466,76.4952184082712,16.1248510148135));
#255101=CARTESIAN_POINT('Ctrl Pts',(27.0012661163029,76.4071769818623,16.0836344441067));
#255102=CARTESIAN_POINT('Ctrl Pts',(27.004737787447,76.4096082525859,16.0839286114052));
#255103=CARTESIAN_POINT('Ctrl Pts',(27.0082239404906,76.4120499969458,16.0841797723559));
#255104=CARTESIAN_POINT('Ctrl Pts',(27.011708212666,76.4144904864622,16.0844643090931));
#255105=CARTESIAN_POINT('Ctrl Pts',(27.0164654915444,76.4178226283401,16.0848528036027));
#255106=CARTESIAN_POINT('Ctrl Pts',(27.0212167836978,76.4211512987678,16.0853190683137));
#255107=CARTESIAN_POINT('Ctrl Pts',(27.0259665551538,76.4244788255243,16.0858213410311));
#255108=CARTESIAN_POINT('Ctrl Pts',(27.0307534510001,76.4278323603537,16.0863275395306));
#255109=CARTESIAN_POINT('Ctrl Pts',(27.0355388328709,76.4311845627265,16.0868702293972));
#255110=CARTESIAN_POINT('Ctrl Pts',(27.0403202016754,76.4345322490831,16.0874595949022));
#255111=CARTESIAN_POINT('Ctrl Pts',(27.0456455283622,76.4382607888011,16.0881160102469));
#255112=CARTESIAN_POINT('Ctrl Pts',(27.0509659278642,76.4419833123646,16.088830242588));
#255113=CARTESIAN_POINT('Ctrl Pts',(27.056268164441,76.4456927956767,16.0896862961657));
#255114=CARTESIAN_POINT('Ctrl Pts',(27.058858523868,76.447505029991,16.0901045133507));
#255115=CARTESIAN_POINT('Ctrl Pts',(27.0614444000977,76.4493141547801,16.0905576105986));
#255116=CARTESIAN_POINT('Ctrl Pts',(27.0640236135651,76.4511197912151,16.0910594910215));
#255117=CARTESIAN_POINT('Ctrl Pts',(27.0646233142434,76.4515396251716,16.0911761847477));
#255118=CARTESIAN_POINT('Ctrl Pts',(27.0652224173107,76.4519590933765,16.0912956547431));
#255119=CARTESIAN_POINT('Ctrl Pts',(27.0658207705618,76.4523781037608,16.0914185979664));
#255120=CARTESIAN_POINT('Ctrl Pts',(27.0694252453324,76.4549022186638,16.092159206872));
#255121=CARTESIAN_POINT('Ctrl Pts',(27.0730526643751,76.4574399975648,16.0929214221552));
#255122=CARTESIAN_POINT('Ctrl Pts',(27.0766494404437,76.4599565375944,16.0938416360863));
#255123=CARTESIAN_POINT('Ctrl Pts',(27.0794164248046,76.4618925010164,16.094549552706));
#255124=CARTESIAN_POINT('Ctrl Pts',(27.0821652338675,76.4638159874324,16.0953521030018));
#255125=CARTESIAN_POINT('Ctrl Pts',(27.0848806691381,76.4657181558853,16.096278407548));
#255126=CARTESIAN_POINT('Ctrl Pts',(27.0856950017747,76.4662885977103,16.0965561972754));
#255127=CARTESIAN_POINT('Ctrl Pts',(27.0865064098576,76.4668571749595,16.0968447965766));
#255128=CARTESIAN_POINT('Ctrl Pts',(27.0873147048412,76.4674237928792,16.0971440360155));
#255129=CARTESIAN_POINT('Ctrl Pts',(27.0892964622733,76.4688130125285,16.0978777037902));
#255130=CARTESIAN_POINT('Ctrl Pts',(27.0912759868229,76.4702047210398,16.0986102840898));
#255131=CARTESIAN_POINT('Ctrl Pts',(27.0932317934192,76.4715818077005,16.0994143656071));
#255132=CARTESIAN_POINT('Ctrl Pts',(27.0950567908676,76.4728667914237,16.100164668178));
#255133=CARTESIAN_POINT('Ctrl Pts',(27.0968611735725,76.4741390840017,16.1009779446282));
#255134=CARTESIAN_POINT('Ctrl Pts',(27.0986398464197,76.4753926606387,16.1018707649377));
#255135=CARTESIAN_POINT('Ctrl Pts',(27.1003347056929,76.4765871669759,16.1027215142946));
#255136=CARTESIAN_POINT('Ctrl Pts',(27.102006284354,76.477764742482,16.103644760763));
#255137=CARTESIAN_POINT('Ctrl Pts',(27.1036611183332,76.4789268718445,16.1046080215383));
#255138=CARTESIAN_POINT('Ctrl Pts',(27.1040884349236,76.4792269606528,16.1048567578559));
#255139=CARTESIAN_POINT('Ctrl Pts',(27.1045146909912,76.4795260526583,16.1051079007521));
#255140=CARTESIAN_POINT('Ctrl Pts',(27.1049401152197,76.4798242409135,16.1053603339431));
#255141=CARTESIAN_POINT('Ctrl Pts',(27.107191856298,76.4814025307667,16.1066964454));
#255142=CARTESIAN_POINT('Ctrl Pts',(27.1094086966922,76.4829517841693,16.108156698499));
#255143=CARTESIAN_POINT('Ctrl Pts',(27.1115676990795,76.4844580502449,16.1097553365817));
#255144=CARTESIAN_POINT('Ctrl Pts',(27.1144415930954,76.4864630730678,16.1118833177486));
#255145=CARTESIAN_POINT('Ctrl Pts',(27.1172143946526,76.4883927334345,16.114251591047));
#255146=CARTESIAN_POINT('Ctrl Pts',(27.1198385003592,76.4902196926299,16.1168182560618));
#255147=CARTESIAN_POINT('Ctrl Pts',(27.1220343788846,76.4917485107921,16.1189660676282));
#255148=CARTESIAN_POINT('Ctrl Pts',(27.1241266280253,76.4932057033932,16.1212487745088));
#255149=CARTESIAN_POINT('Ctrl Pts',(27.1260772883368,76.4945703804111,16.1236712941908));
#255150=CARTESIAN_POINT('Ctrl Pts',(27.1263896838621,76.49478893153,16.1240592573354));
#255151=CARTESIAN_POINT('Ctrl Pts',(27.1266982100994,76.4950049324791,16.1244524123603));
#255152=CARTESIAN_POINT('Ctrl Pts',(27.127002665508,76.4952182372903,16.1248510388561));
#255153=CARTESIAN_POINT('',(27.1805645602856,76.5327357173562,16.1924969468891));
#255154=CARTESIAN_POINT('Ctrl Pts',(27.1270024565239,76.4952187502329,16.1248509667283));
#255155=CARTESIAN_POINT('Ctrl Pts',(27.1424765597207,76.506055562166,16.1451084955576));
#255156=CARTESIAN_POINT('Ctrl Pts',(27.1582694740498,76.5171175291545,16.1650670183879));
#255157=CARTESIAN_POINT('Ctrl Pts',(27.1742368508763,76.5283030898323,16.1847307983824));
#255158=CARTESIAN_POINT('Ctrl Pts',(27.1763430720179,76.5297785522477,16.1873246038395));
#255159=CARTESIAN_POINT('Ctrl Pts',(27.1784523977366,76.531256170399,16.1899133083194));
#255160=CARTESIAN_POINT('Ctrl Pts',(27.1805645602855,76.5327357173562,16.1924969468891));
#255161=CARTESIAN_POINT('',(75.6605890912238,110.478801107225,16.1925));
#255162=CARTESIAN_POINT('Origin',(-75.6605890912239,110.478801107225,12.3825));
#255163=CARTESIAN_POINT('',(-27.1805647392023,76.5327354732306,16.1924983103147));
#255164=CARTESIAN_POINT('',(-75.6605890912239,110.478801107225,16.1925));
#255165=CARTESIAN_POINT('',(-27.1270026766374,76.4952184105125,16.124850980315));
#255166=CARTESIAN_POINT('Ctrl Pts',(-27.180565219782,76.5327358093755,16.1924970380416));
#255167=CARTESIAN_POINT('Ctrl Pts',(-27.1645460760463,76.5215147101881,
16.172902641616));
#255168=CARTESIAN_POINT('Ctrl Pts',(-27.1486864769872,76.5104044317336,
16.1530153195235));
#255169=CARTESIAN_POINT('Ctrl Pts',(-27.1331242506465,76.4995059128408,
16.1328282540153));
#255170=CARTESIAN_POINT('Ctrl Pts',(-27.1310783227674,76.4980731111866,
16.1301743098291));
#255171=CARTESIAN_POINT('Ctrl Pts',(-27.1290376031219,76.496643974394,16.1275152114758));
#255172=CARTESIAN_POINT('Ctrl Pts',(-27.1270024664547,76.4952187349082,
16.1248509673414));
#255173=CARTESIAN_POINT('',(-27.0012528338594,76.4071670555372,16.0836576911637));
#255174=CARTESIAN_POINT('Ctrl Pts',(-27.1270027817058,76.4952182482985,
16.1248509867716));
#255175=CARTESIAN_POINT('Ctrl Pts',(-27.1240985616495,76.4931858448222,
16.1210498254195));
#255176=CARTESIAN_POINT('Ctrl Pts',(-27.1208691627931,76.4909301698259,
16.1175138337718));
#255177=CARTESIAN_POINT('Ctrl Pts',(-27.1174141814671,76.488512642972,16.1144000397266));
#255178=CARTESIAN_POINT('Ctrl Pts',(-27.1156443145459,76.4872742279399,
16.1128049511979));
#255179=CARTESIAN_POINT('Ctrl Pts',(-27.1138145057317,76.4859930227779,
16.1113222644235));
#255180=CARTESIAN_POINT('Ctrl Pts',(-27.1119395463074,76.4846791613504,
16.1099492036558));
#255181=CARTESIAN_POINT('Ctrl Pts',(-27.1101543718988,76.4834282159878,
16.1086418937951));
#255182=CARTESIAN_POINT('Ctrl Pts',(-27.1083279413725,76.4821474488426,
16.1074352882173));
#255183=CARTESIAN_POINT('Ctrl Pts',(-27.1064797666433,76.4808505836342,
16.1062837053202));
#255184=CARTESIAN_POINT('Ctrl Pts',(-27.1054282961436,76.4801127662151,
16.1056285424586));
#255185=CARTESIAN_POINT('Ctrl Pts',(-27.104370813704,76.4793697022192,16.1049758084275));
#255186=CARTESIAN_POINT('Ctrl Pts',(-27.1033071953436,76.4786223827172,
16.1043249532128));
#255187=CARTESIAN_POINT('Ctrl Pts',(-27.1014285386934,76.4773024010352,
16.1031753552716));
#255188=CARTESIAN_POINT('Ctrl Pts',(-27.0995243697347,76.4759644037322,
16.1020872230215));
#255189=CARTESIAN_POINT('Ctrl Pts',(-27.0975893413305,76.4746063119939,
16.1011009878118));
#255190=CARTESIAN_POINT('Ctrl Pts',(-27.0955329405811,76.4731630355737,
16.1000528921767));
#255191=CARTESIAN_POINT('Ctrl Pts',(-27.0934416537043,76.4716969840383,
16.0991197195565));
#255192=CARTESIAN_POINT('Ctrl Pts',(-27.0913213037529,76.4702124719296,
16.0982908776209));
#255193=CARTESIAN_POINT('Ctrl Pts',(-27.0902216751327,76.4694425933533,
16.0978610342767));
#255194=CARTESIAN_POINT('Ctrl Pts',(-27.0891144287658,76.4686678667903,
16.0974583211211));
#255195=CARTESIAN_POINT('Ctrl Pts',(-27.0880015580308,76.4678896257693,
16.097076081408));
#255196=CARTESIAN_POINT('Ctrl Pts',(-27.0853331024396,76.4660235495589,
16.0961595421663));
#255197=CARTESIAN_POINT('Ctrl Pts',(-27.0826307460464,76.4641359871599,
16.0953640053502));
#255198=CARTESIAN_POINT('Ctrl Pts',(-27.0799117554863,76.462236335893,16.0946554141566));
#255199=CARTESIAN_POINT('Ctrl Pts',(-27.0767300191218,76.4600133824172,
16.0938262276189));
#255200=CARTESIAN_POINT('Ctrl Pts',(-27.0735255691118,76.4577737617538,
16.0931150483633));
#255201=CARTESIAN_POINT('Ctrl Pts',(-27.0703421185465,76.4555446329423,
16.0923997928668));
#255202=CARTESIAN_POINT('Ctrl Pts',(-27.0701694407379,76.455423719779,16.0923609957349));
#255203=CARTESIAN_POINT('Ctrl Pts',(-27.0699968278378,76.4553028401788,
16.0923221754269));
#255204=CARTESIAN_POINT('Ctrl Pts',(-27.0698242878259,76.4551819993629,
16.0922833090418));
#255205=CARTESIAN_POINT('Ctrl Pts',(-27.0679952382887,76.4539009988822,
16.0918712971096));
#255206=CARTESIAN_POINT('Ctrl Pts',(-27.0661576675468,76.4526148397304,
16.0915037642175));
#255207=CARTESIAN_POINT('Ctrl Pts',(-27.0643159032437,76.4513260707313,
16.0911596237272));
#255208=CARTESIAN_POINT('Ctrl Pts',(-27.0591307079062,76.4476977459811,
16.0901907507488));
#255209=CARTESIAN_POINT('Ctrl Pts',(-27.0539254560322,76.4440580085204,
16.0893896618873));
#255210=CARTESIAN_POINT('Ctrl Pts',(-27.0487135067179,76.4404106076753,
16.0886634815155));
#255211=CARTESIAN_POINT('Ctrl Pts',(-27.0439334748512,76.4370654691831,
16.087997480158));
#255212=CARTESIAN_POINT('Ctrl Pts',(-27.0391479476081,76.4337143857031,
16.0873933983776));
#255213=CARTESIAN_POINT('Ctrl Pts',(-27.0343616852157,76.4303615098117,
16.0868217458837));
#255214=CARTESIAN_POINT('Ctrl Pts',(-27.0296521096837,76.4270623546536,
16.0862592525689));
#255215=CARTESIAN_POINT('Ctrl Pts',(-27.0249418477206,76.4237617060353,
16.0857279855821));
#255216=CARTESIAN_POINT('Ctrl Pts',(-27.0202287452912,76.4204596636729,
16.0852507551713));
#255217=CARTESIAN_POINT('Ctrl Pts',(-27.0173943327058,76.418473848476,16.0849637535831));
#255218=CARTESIAN_POINT('Ctrl Pts',(-27.0145587580626,76.4164874330431,
16.0846973118287));
#255219=CARTESIAN_POINT('Ctrl Pts',(-27.0117203818392,76.4144993121772,
16.0844653135676));
#255220=CARTESIAN_POINT('Ctrl Pts',(-27.008223903867,76.4120502285228,16.0841795245298));
#255221=CARTESIAN_POINT('Ctrl Pts',(-27.004737697993,76.4096083908123,16.0839285965694));
#255222=CARTESIAN_POINT('Ctrl Pts',(-27.0012653012945,76.4071765600896,
16.0836332011111));
#255223=CARTESIAN_POINT('',(-27.0012528338594,76.4071670555372,12.3825));
#255224=CARTESIAN_POINT('Origin',(-110.478801107225,75.6605890912239,12.3825));
#255225=CARTESIAN_POINT('',(-76.4952184082714,27.1270025958469,16.1248510148134));
#255226=CARTESIAN_POINT('Ctrl Pts',(-76.407176981863,27.0012661163039,16.0836344441047));
#255227=CARTESIAN_POINT('Ctrl Pts',(-76.4096082525859,27.0047377874469,
16.0839286114047));
#255228=CARTESIAN_POINT('Ctrl Pts',(-76.4120499969459,27.0082239404907,
16.0841797723545));
#255229=CARTESIAN_POINT('Ctrl Pts',(-76.4144904864623,27.0117082126661,
16.084464309092));
#255230=CARTESIAN_POINT('Ctrl Pts',(-76.4178226283415,27.0164654915462,
16.0848528036021));
#255231=CARTESIAN_POINT('Ctrl Pts',(-76.4211512987705,27.0212167837015,
16.0853190683136));
#255232=CARTESIAN_POINT('Ctrl Pts',(-76.4244788255282,27.0259665551592,
16.0858213410313));
#255233=CARTESIAN_POINT('Ctrl Pts',(-76.4278323603589,27.0307534510073,
16.0863275395312));
#255234=CARTESIAN_POINT('Ctrl Pts',(-76.4311845627328,27.0355388328798,
16.0868702293981));
#255235=CARTESIAN_POINT('Ctrl Pts',(-76.4345322490906,27.0403202016861,
16.0874595949035));
#255236=CARTESIAN_POINT('Ctrl Pts',(-76.4382607888103,27.0456455283754,
16.0881160102486));
#255237=CARTESIAN_POINT('Ctrl Pts',(-76.4419833123755,27.0509659278798,
16.0888302425902));
#255238=CARTESIAN_POINT('Ctrl Pts',(-76.4456927956894,27.0562681644591,
16.0896862961685));
#255239=CARTESIAN_POINT('Ctrl Pts',(-76.4475050299992,27.0588585238798,
16.0901045133526));
#255240=CARTESIAN_POINT('Ctrl Pts',(-76.4493141547839,27.0614444001031,
16.0905576105995));
#255241=CARTESIAN_POINT('Ctrl Pts',(-76.4511197912145,27.0640236135643,
16.0910594910211));
#255242=CARTESIAN_POINT('Ctrl Pts',(-76.4515396251712,27.0646233142428,
16.0911761847473));
#255243=CARTESIAN_POINT('Ctrl Pts',(-76.4519590933763,27.0652224173104,
16.0912956547428));
#255244=CARTESIAN_POINT('Ctrl Pts',(-76.4523781037608,27.0658207705619,
16.0914185979661));
#255245=CARTESIAN_POINT('Ctrl Pts',(-76.4549022186636,27.0694252453321,
16.0921592068717));
#255246=CARTESIAN_POINT('Ctrl Pts',(-76.4574399975644,27.0730526643745,
16.0929214221549));
#255247=CARTESIAN_POINT('Ctrl Pts',(-76.4599565375938,27.0766494404427,
16.0938416360861));
#255248=CARTESIAN_POINT('Ctrl Pts',(-76.4618925010159,27.0794164248039,
16.094549552706));
#255249=CARTESIAN_POINT('Ctrl Pts',(-76.463815987432,27.082165233867,16.0953521030019));
#255250=CARTESIAN_POINT('Ctrl Pts',(-76.4657181558851,27.0848806691378,
16.0962784075483));
#255251=CARTESIAN_POINT('Ctrl Pts',(-76.4662885977097,27.0856950017738,
16.0965561972754));
#255252=CARTESIAN_POINT('Ctrl Pts',(-76.4668571749586,27.0865064098562,
16.0968447965765));
#255253=CARTESIAN_POINT('Ctrl Pts',(-76.467423792878,27.0873147048393,16.0971440360151));
#255254=CARTESIAN_POINT('Ctrl Pts',(-76.4688130125272,27.0892964622714,
16.0978777037898));
#255255=CARTESIAN_POINT('Ctrl Pts',(-76.4702047210385,27.091275986821,16.0986102840892));
#255256=CARTESIAN_POINT('Ctrl Pts',(-76.4715818076992,27.0932317934172,
16.0994143656064));
#255257=CARTESIAN_POINT('Ctrl Pts',(-76.4728667914224,27.0950567908655,
16.1001646681772));
#255258=CARTESIAN_POINT('Ctrl Pts',(-76.4741390840003,27.0968611735704,
16.1009779446272));
#255259=CARTESIAN_POINT('Ctrl Pts',(-76.4753926606373,27.0986398464175,
16.1018707649366));
#255260=CARTESIAN_POINT('Ctrl Pts',(-76.4765871669744,27.1003347056906,
16.1027215142933));
#255261=CARTESIAN_POINT('Ctrl Pts',(-76.4777647424805,27.1020062843517,
16.1036447607616));
#255262=CARTESIAN_POINT('Ctrl Pts',(-76.4789268718429,27.1036611183308,
16.1046080215368));
#255263=CARTESIAN_POINT('Ctrl Pts',(-76.4792269606518,27.1040884349221,
16.1048567578548));
#255264=CARTESIAN_POINT('Ctrl Pts',(-76.4795260526579,27.1045146909905,
16.1051079007516));
#255265=CARTESIAN_POINT('Ctrl Pts',(-76.4798242409137,27.1049401152199,
16.1053603339431));
#255266=CARTESIAN_POINT('Ctrl Pts',(-76.4814025307668,27.107191856298,16.1066964453999));
#255267=CARTESIAN_POINT('Ctrl Pts',(-76.4829517841693,27.1094086966921,
16.1081566984987));
#255268=CARTESIAN_POINT('Ctrl Pts',(-76.4844580502449,27.1115676990793,
16.1097553365814));
#255269=CARTESIAN_POINT('Ctrl Pts',(-76.4864630730681,27.1144415930957,
16.1118833177486));
#255270=CARTESIAN_POINT('Ctrl Pts',(-76.4883927334351,27.1172143946534,
16.1142515910474));
#255271=CARTESIAN_POINT('Ctrl Pts',(-76.4902196926308,27.1198385003604,
16.1168182560628));
#255272=CARTESIAN_POINT('Ctrl Pts',(-76.4917485107915,27.1220343788836,
16.118966067627));
#255273=CARTESIAN_POINT('Ctrl Pts',(-76.4932057033912,27.1241266280223,
16.1212487745052));
#255274=CARTESIAN_POINT('Ctrl Pts',(-76.4945703804079,27.1260772883321,
16.1236712941847));
#255275=CARTESIAN_POINT('Ctrl Pts',(-76.494788931528,27.126389683859,16.1240592573312));
#255276=CARTESIAN_POINT('Ctrl Pts',(-76.4950049324782,27.126698210098,16.1244524123581));
#255277=CARTESIAN_POINT('Ctrl Pts',(-76.4952182372905,27.1270026655082,
16.124851038856));
#255278=CARTESIAN_POINT('',(-76.5327357173542,27.1805645602828,16.1924969468886));
#255279=CARTESIAN_POINT('Ctrl Pts',(-76.4952187502333,27.1270024565244,
16.124850966728));
#255280=CARTESIAN_POINT('Ctrl Pts',(-76.506055561861,27.1424765592851,16.1451084949868));
#255281=CARTESIAN_POINT('Ctrl Pts',(-76.5171175285349,27.1582694731656,
16.1650670172575));
#255282=CARTESIAN_POINT('Ctrl Pts',(-76.528303088887,27.1742368495269,16.1847307967182));
#255283=CARTESIAN_POINT('Ctrl Pts',(-76.529778551616,27.1763430711163,16.1873246027319));
#255284=CARTESIAN_POINT('Ctrl Pts',(-76.5312561700818,27.1784523972839,
16.1899133077663));
#255285=CARTESIAN_POINT('Ctrl Pts',(-76.5327357173542,27.1805645602828,
16.1924969468886));
#255286=CARTESIAN_POINT('',(-110.478801107225,75.6605890912239,16.1925));
#255287=CARTESIAN_POINT('',(-76.4071670555372,27.0012528338594,14.2875));
#255288=CARTESIAN_POINT('Origin',(0.,0.,12.3825));
#255289=CARTESIAN_POINT('',(-112.039285751595,74.5679259799751,12.3825));
#255290=CARTESIAN_POINT('',(-113.095,76.1978262581577,12.3825));
#255291=CARTESIAN_POINT('Origin',(-90.,90.,12.3825));
#255292=CARTESIAN_POINT('',(-113.095,-76.1978262581577,12.3825));
#255293=CARTESIAN_POINT('',(-113.095,-90.,12.3825));
#255294=CARTESIAN_POINT('',(-112.039285751595,-74.5679259799751,12.3825));
#255295=CARTESIAN_POINT('Origin',(-90.,-90.,12.3825));
#255296=CARTESIAN_POINT('',(-77.9676516999077,-25.9085897226107,12.3825));
#255297=CARTESIAN_POINT('Origin',(0.,0.,12.3825));
#255298=CARTESIAN_POINT('',(-112.039285751595,74.5679259799751,12.3825));
#255299=CARTESIAN_POINT('Origin',(-110.478801107225,-75.6605890912239,12.3825));
#255300=CARTESIAN_POINT('',(-76.5327354732302,-27.1805647392017,16.1924983103146));
#255301=CARTESIAN_POINT('',(-110.478801107225,-75.6605890912239,16.1925));
#255302=CARTESIAN_POINT('',(-76.4952184105099,-27.1270026766394,16.1248509803166));
#255303=CARTESIAN_POINT('Ctrl Pts',(-76.532735809375,-27.1805652197814,
16.1924970380414));
#255304=CARTESIAN_POINT('Ctrl Pts',(-76.5215147093823,-27.1645460748958,
16.1729026402457));
#255305=CARTESIAN_POINT('Ctrl Pts',(-76.5104044301563,-27.1486864747344,
16.1530153167097));
#255306=CARTESIAN_POINT('Ctrl Pts',(-76.4995059105232,-27.1331242473368,
16.132828249725));
#255307=CARTESIAN_POINT('Ctrl Pts',(-76.4980731096455,-27.1310783205666,
16.1301743069634));
#255308=CARTESIAN_POINT('Ctrl Pts',(-76.4966439736256,-27.1290376020245,
16.1275152100406));
#255309=CARTESIAN_POINT('Ctrl Pts',(-76.4952187349081,-27.1270024664543,
16.1248509673423));
#255310=CARTESIAN_POINT('Ctrl Pts',(-76.4952182482945,-27.1270027817086,
16.1248509867732));
#255311=CARTESIAN_POINT('Ctrl Pts',(-76.4931858448006,-27.1240985616638,
16.121049825422));
#255312=CARTESIAN_POINT('Ctrl Pts',(-76.4909301697861,-27.1208691627763,
16.1175138339431));
#255313=CARTESIAN_POINT('Ctrl Pts',(-76.4885126429384,-27.1174141814444,
16.1144000399021));
#255314=CARTESIAN_POINT('Ctrl Pts',(-76.4872742275686,-27.1156443140332,
16.1128049509365));
#255315=CARTESIAN_POINT('Ctrl Pts',(-76.4859930220507,-27.1138145047011,
16.1113222637541));
#255316=CARTESIAN_POINT('Ctrl Pts',(-76.4846791602534,-27.1119395447418,
16.1099492026215));
#255317=CARTESIAN_POINT('Ctrl Pts',(-76.4834282152446,-27.1101543708312,
16.1086418931511));
#255318=CARTESIAN_POINT('Ctrl Pts',(-76.4821474484747,-27.1083279408346,
16.1074352878857));
#255319=CARTESIAN_POINT('Ctrl Pts',(-76.4808505836411,-27.1064797666398,
16.1062837053213));
#255320=CARTESIAN_POINT('Ctrl Pts',(-76.4801127643227,-27.1054282934335,
16.1056285407733));
#255321=CARTESIAN_POINT('Ctrl Pts',(-76.4793696983962,-27.1043708082513,
16.1049758051017));
#255322=CARTESIAN_POINT('Ctrl Pts',(-76.4786223769383,-27.1033071871103,
16.1043249482959));
#255323=CARTESIAN_POINT('Ctrl Pts',(-76.4773023951153,-27.1014285302648,
16.1031753504303));
#255324=CARTESIAN_POINT('Ctrl Pts',(-76.475964397667,-27.0995243610965,
16.1020872183569));
#255325=CARTESIAN_POINT('Ctrl Pts',(-76.4746063057845,-27.0975893324811,
16.1011009833628));
#255326=CARTESIAN_POINT('Ctrl Pts',(-76.4731630291583,-27.0955329314322,
16.1000528879186));
#255327=CARTESIAN_POINT('Ctrl Pts',(-76.4716969774167,-27.0934416442518,
16.0991197155412));
#255328=CARTESIAN_POINT('Ctrl Pts',(-76.4702124651068,-27.0913212940051,
16.0982908738278));
#255329=CARTESIAN_POINT('Ctrl Pts',(-76.4694425873394,-27.0902216665361,
16.0978610311087));
#255330=CARTESIAN_POINT('Ctrl Pts',(-76.4686678615982,-27.0891144213408,
16.0974583185077));
#255331=CARTESIAN_POINT('Ctrl Pts',(-76.4678896214075,-27.0880015517915,
16.0970760792947));
#255332=CARTESIAN_POINT('Ctrl Pts',(-76.4660235449902,-27.0853330959005,
16.0961595401724));
#255333=CARTESIAN_POINT('Ctrl Pts',(-76.4641359823881,-27.0826307392147,
16.0953640034684));
#255334=CARTESIAN_POINT('Ctrl Pts',(-76.4622363309284,-27.0799117483802,
16.0946554123439));
#255335=CARTESIAN_POINT('Ctrl Pts',(-76.4600133772259,-27.0767300116927,
16.0938262258867));
#255336=CARTESIAN_POINT('Ctrl Pts',(-76.4577737563502,-27.0735255613849,
16.0931150466518));
#255337=CARTESIAN_POINT('Ctrl Pts',(-76.4555446273526,-27.070342110563,
16.092399791074));
#255338=CARTESIAN_POINT('Ctrl Pts',(-76.4554237160546,-27.0701694354188,
16.0923609945394));
#255339=CARTESIAN_POINT('Ctrl Pts',(-76.4553028383187,-27.0699968251812,
16.0923221748292));
#255340=CARTESIAN_POINT('Ctrl Pts',(-76.455181999366,-27.0698242878295,
16.0922833090433));
#255341=CARTESIAN_POINT('Ctrl Pts',(-76.4539009977357,-27.0679952366507,
16.0918712967414));
#255342=CARTESIAN_POINT('Ctrl Pts',(-76.4526148374245,-27.0661576642512,
16.0915037635639));
#255343=CARTESIAN_POINT('Ctrl Pts',(-76.4513260672622,-27.0643158982848,
16.0911596228214));
#255344=CARTESIAN_POINT('Ctrl Pts',(-76.4476977425727,-27.0591307030318,
16.0901907500241));
#255345=CARTESIAN_POINT('Ctrl Pts',(-76.4440580051801,-27.053925451258,
16.0893896612632));
#255346=CARTESIAN_POINT('Ctrl Pts',(-76.4404106044097,-27.048713502053,
16.0886634809515));
#255347=CARTESIAN_POINT('Ctrl Pts',(-76.4370654658784,-27.0439334701325,
16.0879974796278));
#255348=CARTESIAN_POINT('Ctrl Pts',(-76.4337143823643,-27.0391479428428,
16.0873933978516));
#255349=CARTESIAN_POINT('Ctrl Pts',(-76.4303615064407,-27.0343616804054,
16.0868217453606));
#255350=CARTESIAN_POINT('Ctrl Pts',(-76.4270623512098,-27.0296521047703,
16.0862592520419));
#255351=CARTESIAN_POINT('Ctrl Pts',(-76.4237617025205,-27.0249418427056,
16.0857279850509));
#255352=CARTESIAN_POINT('Ctrl Pts',(-76.4204596600846,-27.0202287401702,
16.0852507546629));
#255353=CARTESIAN_POINT('Ctrl Pts',(-76.4184738460836,-27.0173943292914,
16.0849637532678));
#255354=CARTESIAN_POINT('Ctrl Pts',(-76.4164874318464,-27.0145587563545,
16.0846973116911));
#255355=CARTESIAN_POINT('Ctrl Pts',(-76.414499312177,-27.0117203818391,
16.0844653135703));
#255356=CARTESIAN_POINT('Ctrl Pts',(-76.4120502285228,-27.0082239038667,
16.0841795245333));
#255357=CARTESIAN_POINT('Ctrl Pts',(-76.4096083908209,-27.0047376980153,
16.083928596514));
#255358=CARTESIAN_POINT('Ctrl Pts',(-76.4071765580783,-27.0012652984223,
16.0836331977649));
#255359=CARTESIAN_POINT('',(-110.478801107225,-75.6605890912239,14.2875));
#255360=CARTESIAN_POINT('Origin',(-75.6605890912239,-110.478801107225,12.3825));
#255361=CARTESIAN_POINT('',(-27.0012528338594,-76.4071670555372,14.2875));
#255362=CARTESIAN_POINT('',(-27.0012528338594,-76.4071670555372,16.0836603564332));
#255363=CARTESIAN_POINT('',(-27.0012528338594,-76.4071670555372,17.0741173620444));
#255364=CARTESIAN_POINT('',(-27.127002595847,-76.4952184082715,16.1248510148133));
#255365=CARTESIAN_POINT('Ctrl Pts',(-27.0012661163037,-76.4071769818629,
16.0836344441051));
#255366=CARTESIAN_POINT('Ctrl Pts',(-27.0047377874469,-76.4096082525859,
16.0839286114036));
#255367=CARTESIAN_POINT('Ctrl Pts',(-27.0082239404904,-76.4120499969456,
16.0841797723569));
#255368=CARTESIAN_POINT('Ctrl Pts',(-27.0117082126658,-76.4144904864621,
16.0844643090938));
#255369=CARTESIAN_POINT('Ctrl Pts',(-27.0164654915443,-76.4178226283401,
16.0848528036029));
#255370=CARTESIAN_POINT('Ctrl Pts',(-27.0212167836978,-76.4211512987679,
16.0853190683137));
#255371=CARTESIAN_POINT('Ctrl Pts',(-27.0259665551539,-76.4244788255244,
16.0858213410309));
#255372=CARTESIAN_POINT('Ctrl Pts',(-27.0307534510004,-76.427832360354,
16.0863275395304));
#255373=CARTESIAN_POINT('Ctrl Pts',(-27.0355388328714,-76.4311845627269,
16.086870229397));
#255374=CARTESIAN_POINT('Ctrl Pts',(-27.0403202016761,-76.4345322490837,
16.0874595949021));
#255375=CARTESIAN_POINT('Ctrl Pts',(-27.0456455283646,-76.4382607888028,
16.0881160102471));
#255376=CARTESIAN_POINT('Ctrl Pts',(-27.0509659278681,-76.4419833123674,
16.0888302425885));
#255377=CARTESIAN_POINT('Ctrl Pts',(-27.0562681644465,-76.4456927956806,
16.0896862961667));
#255378=CARTESIAN_POINT('Ctrl Pts',(-27.0588585238712,-76.4475050299932,
16.0901045133513));
#255379=CARTESIAN_POINT('Ctrl Pts',(-27.0614444000984,-76.4493141547807,
16.0905576105989));
#255380=CARTESIAN_POINT('Ctrl Pts',(-27.0640236135634,-76.4511197912139,
16.0910594910214));
#255381=CARTESIAN_POINT('Ctrl Pts',(-27.064623314242,-76.4515396251707,
16.0911761847476));
#255382=CARTESIAN_POINT('Ctrl Pts',(-27.0652224173098,-76.4519590933759,
16.0912956547432));
#255383=CARTESIAN_POINT('Ctrl Pts',(-27.0658207705614,-76.4523781037604,
16.0914185979665));
#255384=CARTESIAN_POINT('Ctrl Pts',(-27.0694252453316,-76.4549022186632,
16.092159206872));
#255385=CARTESIAN_POINT('Ctrl Pts',(-27.0730526643741,-76.4574399975641,
16.0929214221551));
#255386=CARTESIAN_POINT('Ctrl Pts',(-27.0766494404423,-76.4599565375935,
16.0938416360861));
#255387=CARTESIAN_POINT('Ctrl Pts',(-27.0794164248033,-76.4618925010154,
16.0945495527057));
#255388=CARTESIAN_POINT('Ctrl Pts',(-27.0821652338662,-76.4638159874314,
16.0953521030014));
#255389=CARTESIAN_POINT('Ctrl Pts',(-27.0848806691367,-76.4657181558843,
16.0962784075474));
#255390=CARTESIAN_POINT('Ctrl Pts',(-27.085695001773,-76.4662885977091,
16.0965561972746));
#255391=CARTESIAN_POINT('Ctrl Pts',(-27.0865064098557,-76.4668571749581,
16.0968447965757));
#255392=CARTESIAN_POINT('Ctrl Pts',(-27.087314704839,-76.4674237928777,
16.0971440360144));
#255393=CARTESIAN_POINT('Ctrl Pts',(-27.0892964622713,-76.4688130125271,
16.097877703789));
#255394=CARTESIAN_POINT('Ctrl Pts',(-27.091275986821,-76.4702047210384,
16.0986102840886));
#255395=CARTESIAN_POINT('Ctrl Pts',(-27.0932317934173,-76.4715818076992,
16.0994143656059));
#255396=CARTESIAN_POINT('Ctrl Pts',(-27.0950567908658,-76.4728667914225,
16.1001646681769));
#255397=CARTESIAN_POINT('Ctrl Pts',(-27.0968611735707,-76.4741390840004,
16.1009779446271));
#255398=CARTESIAN_POINT('Ctrl Pts',(-27.0986398464179,-76.4753926606374,
16.1018707649367));
#255399=CARTESIAN_POINT('Ctrl Pts',(-27.1003347056911,-76.4765871669746,
16.1027215142937));
#255400=CARTESIAN_POINT('Ctrl Pts',(-27.1020062843522,-76.4777647424807,
16.1036447607621));
#255401=CARTESIAN_POINT('Ctrl Pts',(-27.1036611183315,-76.4789268718433,
16.1046080215375));
#255402=CARTESIAN_POINT('Ctrl Pts',(-27.1040884349225,-76.479226960652,
16.1048567578554));
#255403=CARTESIAN_POINT('Ctrl Pts',(-27.1045146909907,-76.4795260526579,
16.105107900752));
#255404=CARTESIAN_POINT('Ctrl Pts',(-27.1049401152198,-76.4798242409135,
16.1053603339433));
#255405=CARTESIAN_POINT('Ctrl Pts',(-27.1071918562982,-76.4814025307668,
16.1066964454002));
#255406=CARTESIAN_POINT('Ctrl Pts',(-27.1094086966924,-76.4829517841694,
16.1081566984993));
#255407=CARTESIAN_POINT('Ctrl Pts',(-27.1115676990799,-76.4844580502452,
16.1097553365821));
#255408=CARTESIAN_POINT('Ctrl Pts',(-27.1144415930974,-76.4864630730692,
16.1118833177503));
#255409=CARTESIAN_POINT('Ctrl Pts',(-27.1172143946562,-76.488392733437,
16.1142515910502));
#255410=CARTESIAN_POINT('Ctrl Pts',(-27.1198385003641,-76.4902196926333,
16.1168182560667));
#255411=CARTESIAN_POINT('Ctrl Pts',(-27.1220343788854,-76.4917485107927,
16.1189660676294));
#255412=CARTESIAN_POINT('Ctrl Pts',(-27.1241266280224,-76.4932057033912,
16.1212487745057));
#255413=CARTESIAN_POINT('Ctrl Pts',(-27.1260772883308,-76.4945703804069,
16.1236712941829));
#255414=CARTESIAN_POINT('Ctrl Pts',(-27.1263896838582,-76.4947889315274,
16.12405925733));
#255415=CARTESIAN_POINT('Ctrl Pts',(-27.1266982100976,-76.4950049324779,
16.1244524123575));
#255416=CARTESIAN_POINT('Ctrl Pts',(-27.1270026655083,-76.4952182372905,
16.124851038856));
#255417=CARTESIAN_POINT('',(-27.1805645602868,-76.5327357173571,16.1924969468894));
#255418=CARTESIAN_POINT('Ctrl Pts',(-27.1270024565245,-76.4952187502334,
16.124850966728));
#255419=CARTESIAN_POINT('Ctrl Pts',(-27.1424765592086,-76.5060555618075,
16.1451084948867));
#255420=CARTESIAN_POINT('Ctrl Pts',(-27.1582694730108,-76.5171175284266,
16.1650670170587));
#255421=CARTESIAN_POINT('Ctrl Pts',(-27.1742368492934,-76.5283030887235,
16.1847307964267));
#255422=CARTESIAN_POINT('Ctrl Pts',(-27.1763430709617,-76.5297785515079,
16.1873246025381));
#255423=CARTESIAN_POINT('Ctrl Pts',(-27.1784523972085,-76.5312561700291,
16.1899133076699));
#255424=CARTESIAN_POINT('Ctrl Pts',(-27.1805645602868,-76.5327357173571,
16.1924969468894));
#255425=CARTESIAN_POINT('',(-75.6605890912239,-110.478801107225,16.1925));
#255426=CARTESIAN_POINT('',(-27.0012528338595,-76.4071670555372,14.2875));
#255427=CARTESIAN_POINT('Origin',(0.,0.,12.3825));
#255428=CARTESIAN_POINT('',(-74.5679259799751,-112.039285751595,12.3825));
#255429=CARTESIAN_POINT('',(-76.1978262581577,-113.095,12.3825));
#255430=CARTESIAN_POINT('Origin',(-90.,-90.,12.3825));
#255431=CARTESIAN_POINT('',(76.1978262581577,-113.095,12.3825));
#255432=CARTESIAN_POINT('',(90.,-113.095,12.3825));
#255433=CARTESIAN_POINT('',(74.5679259799751,-112.039285751595,12.3825));
#255434=CARTESIAN_POINT('Origin',(90.,-90.,12.3825));
#255435=CARTESIAN_POINT('',(25.9085897226107,-77.9676516999077,12.3825));
#255436=CARTESIAN_POINT('',(25.9085897226107,-77.9676516999077,12.3825));
#255437=CARTESIAN_POINT('',(25.3478497357421,-77.8839876917858,12.3825));
#255438=CARTESIAN_POINT('Origin',(25.5443686855278,-78.4878132480313,12.3825));
#255439=CARTESIAN_POINT('',(-25.3478497357421,-77.8839876917858,12.3825));
#255440=CARTESIAN_POINT('Origin',(0.,0.,12.3825));
#255441=CARTESIAN_POINT('',(-25.9085897226107,-77.9676516999077,12.3825));
#255442=CARTESIAN_POINT('Origin',(-25.5443686855278,-78.4878132480312,12.3825));
#255443=CARTESIAN_POINT('',(-74.5679259799751,-112.039285751595,12.3825));
#255444=CARTESIAN_POINT('Origin',(75.6605890912239,-110.478801107225,12.3825));
#255445=CARTESIAN_POINT('',(27.1805647391996,-76.5327354732286,16.1924983103144));
#255446=CARTESIAN_POINT('',(75.6605890912239,-110.478801107225,16.1925));
#255447=CARTESIAN_POINT('',(27.1270026766432,-76.4952184105121,16.1248509803218));
#255448=CARTESIAN_POINT('Ctrl Pts',(27.1805652197793,-76.5327358093735,
16.192497038041));
#255449=CARTESIAN_POINT('Ctrl Pts',(27.1645460748553,-76.5215147093538,
16.1729026401982));
#255450=CARTESIAN_POINT('Ctrl Pts',(27.1486864746558,-76.5104044301012,
16.153015316612));
#255451=CARTESIAN_POINT('Ctrl Pts',(27.1331242472215,-76.4995059104423,
16.1328282495759));
#255452=CARTESIAN_POINT('Ctrl Pts',(27.1310783204899,-76.4980731095918,
16.1301743068639));
#255453=CARTESIAN_POINT('Ctrl Pts',(27.1290376019863,-76.4966439735989,
16.127515209991));
#255454=CARTESIAN_POINT('Ctrl Pts',(27.1270024664544,-76.4952187349081,
16.1248509673428));
#255455=CARTESIAN_POINT('',(27.0012528338594,-76.4071670555372,16.0836576814802));
#255456=CARTESIAN_POINT('Ctrl Pts',(27.1270027817125,-76.4952182482966,
16.1248509867785));
#255457=CARTESIAN_POINT('Ctrl Pts',(27.1240985616685,-76.4931858448008,
16.1210498254261));
#255458=CARTESIAN_POINT('Ctrl Pts',(27.1208691627774,-76.4909301697841,
16.1175138339627));
#255459=CARTESIAN_POINT('Ctrl Pts',(27.1174141814443,-76.4885126429366,
16.1144000399211));
#255460=CARTESIAN_POINT('Ctrl Pts',(27.1156443139851,-76.4872742275337,
16.1128049509126));
#255461=CARTESIAN_POINT('Ctrl Pts',(27.1138145046022,-76.485993021981,16.1113222636901));
#255462=CARTESIAN_POINT('Ctrl Pts',(27.1119395445906,-76.4846791601475,
16.1099492025217));
#255463=CARTESIAN_POINT('Ctrl Pts',(27.110154370728,-76.4834282151728,16.1086418930888));
#255464=CARTESIAN_POINT('Ctrl Pts',(27.1083279407825,-76.4821474484391,
16.1074352878535));
#255465=CARTESIAN_POINT('Ctrl Pts',(27.1064797666391,-76.4808505836416,
16.1062837053212));
#255466=CARTESIAN_POINT('Ctrl Pts',(27.1054282931702,-76.4801127641388,
16.1056285406094));
#255467=CARTESIAN_POINT('Ctrl Pts',(27.1043708077217,-76.4793696980249,
16.1049758047786));
#255468=CARTESIAN_POINT('Ctrl Pts',(27.1033071863107,-76.4786223763771,
16.1043249478184));
#255469=CARTESIAN_POINT('Ctrl Pts',(27.1014285294456,-76.47730239454,16.1031753499598));
#255470=CARTESIAN_POINT('Ctrl Pts',(27.0995243602564,-76.4759643970771,
16.1020872179032));
#255471=CARTESIAN_POINT('Ctrl Pts',(27.0975893316198,-76.4746063051802,
16.1011009829297));
#255472=CARTESIAN_POINT('Ctrl Pts',(27.0955329305412,-76.4731630285335,
16.1000528875037));
#255473=CARTESIAN_POINT('Ctrl Pts',(27.0934416433306,-76.4716969767713,
16.0991197151495));
#255474=CARTESIAN_POINT('Ctrl Pts',(27.0913212930545,-76.4702124644414,
16.0982908734576));
#255475=CARTESIAN_POINT('Ctrl Pts',(27.0902216656986,-76.4694425867535,
16.0978610307999));
#255476=CARTESIAN_POINT('Ctrl Pts',(27.0891144206185,-76.4686678610931,
16.0974583182533));
#255477=CARTESIAN_POINT('Ctrl Pts',(27.0880015511858,-76.467889620984,16.0970760790894));
#255478=CARTESIAN_POINT('Ctrl Pts',(27.0853330952647,-76.466023544546,16.0961595399788));
#255479=CARTESIAN_POINT('Ctrl Pts',(27.0826307385496,-76.4641359819234,
16.0953640032855));
#255480=CARTESIAN_POINT('Ctrl Pts',(27.0799117476875,-76.4622363304444,
16.0946554121674));
#255481=CARTESIAN_POINT('Ctrl Pts',(27.0767300109675,-76.460013376719,16.0938262257177));
#255482=CARTESIAN_POINT('Ctrl Pts',(27.0735255606295,-76.4577737558219,
16.0931150464844));
#255483=CARTESIAN_POINT('Ctrl Pts',(27.0703421097814,-76.4555446268054,
16.0923997908983));
#255484=CARTESIAN_POINT('Ctrl Pts',(27.0701694348977,-76.4554237156897,
16.0923609944221));
#255485=CARTESIAN_POINT('Ctrl Pts',(27.0699968249205,-76.4553028381361,
16.0923221747704));
#255486=CARTESIAN_POINT('Ctrl Pts',(27.0698242878289,-76.4551819993657,
16.0922833090431));
#255487=CARTESIAN_POINT('Ctrl Pts',(27.0679952364911,-76.453900997624,16.0918712967054));
#255488=CARTESIAN_POINT('Ctrl Pts',(27.066157663931,-76.4526148372005,16.0915037635003));
#255489=CARTESIAN_POINT('Ctrl Pts',(27.0643158978034,-76.4513260669254,
16.0911596227336));
#255490=CARTESIAN_POINT('Ctrl Pts',(27.0591307025578,-76.4476977422412,
16.0901907499542));
#255491=CARTESIAN_POINT('Ctrl Pts',(27.053925450793,-76.4440580048548,16.0893896612033));
#255492=CARTESIAN_POINT('Ctrl Pts',(27.0487135015978,-76.4404106040911,
16.0886634808975));
#255493=CARTESIAN_POINT('Ctrl Pts',(27.0439334696713,-76.4370654655554,
16.087997479577));
#255494=CARTESIAN_POINT('Ctrl Pts',(27.0391479423763,-76.4337143820375,
16.087393397801));
#255495=CARTESIAN_POINT('Ctrl Pts',(27.0343616799338,-76.4303615061103,
16.0868217453101));
#255496=CARTESIAN_POINT('Ctrl Pts',(27.0296521042877,-76.4270623508715,
16.0862592519905));
#255497=CARTESIAN_POINT('Ctrl Pts',(27.0249418422122,-76.4237617021747,
16.0857279849987));
#255498=CARTESIAN_POINT('Ctrl Pts',(27.0202287396655,-76.4204596597309,
16.0852507546123));
#255499=CARTESIAN_POINT('Ctrl Pts',(27.017394328955,-76.4184738458479,16.0849637532358));
#255500=CARTESIAN_POINT('Ctrl Pts',(27.0145587561863,-76.4164874317286,
16.0846973116763));
#255501=CARTESIAN_POINT('Ctrl Pts',(27.0117203818393,-76.4144993121772,
16.0844653135687));
#255502=CARTESIAN_POINT('Ctrl Pts',(27.0082239038669,-76.4120502285229,
16.0841795245312));
#255503=CARTESIAN_POINT('Ctrl Pts',(27.0047376980176,-76.4096083908218,
16.0839285965081));
#255504=CARTESIAN_POINT('Ctrl Pts',(27.0012652981443,-76.4071765578836,
16.0836331974402));
#255505=CARTESIAN_POINT('',(27.0012528338594,-76.4071670555372,14.2875));
#255506=CARTESIAN_POINT('',(27.0012528338594,-76.4071670555372,12.3825));
#255507=CARTESIAN_POINT('',(75.6605890912239,-110.478801107225,14.2875));
#255508=CARTESIAN_POINT('Origin',(110.478801107225,-75.6605890912239,12.3825));
#255509=CARTESIAN_POINT('',(76.4071670555372,-27.0012528338594,16.0836603564331));
#255510=CARTESIAN_POINT('',(76.4071670555372,-27.0012528338594,17.0741173620445));
#255511=CARTESIAN_POINT('',(76.4952184082716,-27.1270025958472,16.1248510148123));
#255512=CARTESIAN_POINT('Ctrl Pts',(76.4071769818628,-27.0012661163035,
16.0836344441052));
#255513=CARTESIAN_POINT('Ctrl Pts',(76.4096082525859,-27.0047377874469,
16.0839286114014));
#255514=CARTESIAN_POINT('Ctrl Pts',(76.4120499969459,-27.0082239404908,
16.0841797723485));
#255515=CARTESIAN_POINT('Ctrl Pts',(76.4144904864623,-27.0117082126661,
16.0844643090874));
#255516=CARTESIAN_POINT('Ctrl Pts',(76.4178226283408,-27.0164654915454,
16.0848528035995));
#255517=CARTESIAN_POINT('Ctrl Pts',(76.4211512987692,-27.0212167836998,
16.0853190683122));
#255518=CARTESIAN_POINT('Ctrl Pts',(76.4244788255264,-27.0259665551567,
16.0858213410305));
#255519=CARTESIAN_POINT('Ctrl Pts',(76.4278323603563,-27.0307534510038,
16.0863275395311));
#255520=CARTESIAN_POINT('Ctrl Pts',(76.4311845627297,-27.0355388328754,
16.0868702293981));
#255521=CARTESIAN_POINT('Ctrl Pts',(76.4345322490869,-27.0403202016807,
16.0874595949032));
#255522=CARTESIAN_POINT('Ctrl Pts',(76.4382607888044,-27.0456455283668,
16.0881160102479));
#255523=CARTESIAN_POINT('Ctrl Pts',(76.4419833123674,-27.050965927868,16.0888302425885));
#255524=CARTESIAN_POINT('Ctrl Pts',(76.445692795679,-27.0562681644442,16.0896862961658));
#255525=CARTESIAN_POINT('Ctrl Pts',(76.4475050299921,-27.0588585238695,
16.0901045133504));
#255526=CARTESIAN_POINT('Ctrl Pts',(76.4493141547799,-27.0614444000973,
16.0905576105978));
#255527=CARTESIAN_POINT('Ctrl Pts',(76.4511197912136,-27.064023613563,16.0910594910203));
#255528=CARTESIAN_POINT('Ctrl Pts',(76.4515396251699,-27.0646233142409,
16.0911761847463));
#255529=CARTESIAN_POINT('Ctrl Pts',(76.4519590933746,-27.0652224173079,
16.0912956547417));
#255530=CARTESIAN_POINT('Ctrl Pts',(76.4523781037586,-27.0658207705587,
16.0914185979649));
#255531=CARTESIAN_POINT('Ctrl Pts',(76.4549022186616,-27.0694252453293,
16.0921592068704));
#255532=CARTESIAN_POINT('Ctrl Pts',(76.4574399975625,-27.0730526643718,
16.0929214221539));
#255533=CARTESIAN_POINT('Ctrl Pts',(76.459956537592,-27.0766494404402,16.0938416360852));
#255534=CARTESIAN_POINT('Ctrl Pts',(76.4618925010147,-27.0794164248023,
16.0945495527052));
#255535=CARTESIAN_POINT('Ctrl Pts',(76.4638159874315,-27.0821652338663,
16.0953521030014));
#255536=CARTESIAN_POINT('Ctrl Pts',(76.4657181558853,-27.0848806691381,
16.0962784075478));
#255537=CARTESIAN_POINT('Ctrl Pts',(76.4662885977095,-27.0856950017735,
16.0965561972746));
#255538=CARTESIAN_POINT('Ctrl Pts',(76.4668571749578,-27.0865064098552,
16.0968447965753));
#255539=CARTESIAN_POINT('Ctrl Pts',(76.4674237928768,-27.0873147048377,
16.0971440360135));
#255540=CARTESIAN_POINT('Ctrl Pts',(76.4688130125264,-27.0892964622702,
16.097877703788));
#255541=CARTESIAN_POINT('Ctrl Pts',(76.4702047210379,-27.0912759868201,
16.0986102840874));
#255542=CARTESIAN_POINT('Ctrl Pts',(76.4715818076988,-27.0932317934166,
16.0994143656047));
#255543=CARTESIAN_POINT('Ctrl Pts',(76.4728667914221,-27.0950567908652,
16.1001646681756));
#255544=CARTESIAN_POINT('Ctrl Pts',(76.4741390840002,-27.0968611735703,
16.1009779446259));
#255545=CARTESIAN_POINT('Ctrl Pts',(76.4753926606373,-27.0986398464177,
16.1018707649355));
#255546=CARTESIAN_POINT('Ctrl Pts',(76.4765871669746,-27.100334705691,16.1027215142925));
#255547=CARTESIAN_POINT('Ctrl Pts',(76.4777647424808,-27.1020062843523,
16.103644760761));
#255548=CARTESIAN_POINT('Ctrl Pts',(76.4789268718434,-27.1036611183317,
16.1046080215364));
#255549=CARTESIAN_POINT('Ctrl Pts',(76.479226960652,-27.1040884349225,16.1048567578542));
#255550=CARTESIAN_POINT('Ctrl Pts',(76.4795260526579,-27.1045146909906,
16.1051079007507));
#255551=CARTESIAN_POINT('Ctrl Pts',(76.4798242409133,-27.1049401152196,
16.105360333942));
#255552=CARTESIAN_POINT('Ctrl Pts',(76.4814025307667,-27.1071918562981,
16.106696445399));
#255553=CARTESIAN_POINT('Ctrl Pts',(76.4829517841694,-27.1094086966924,
16.1081566984981));
#255554=CARTESIAN_POINT('Ctrl Pts',(76.4844580502452,-27.11156769908,16.109755336581));
#255555=CARTESIAN_POINT('Ctrl Pts',(76.4864630730699,-27.1144415930985,
16.1118833177498));
#255556=CARTESIAN_POINT('Ctrl Pts',(76.4883927334383,-27.1172143946581,
16.1142515910506));
#255557=CARTESIAN_POINT('Ctrl Pts',(76.4902196926352,-27.1198385003668,
16.116818256068));
#255558=CARTESIAN_POINT('Ctrl Pts',(76.4917485107928,-27.1220343788856,
16.1189660676284));
#255559=CARTESIAN_POINT('Ctrl Pts',(76.4932057033898,-27.1241266280203,
16.1212487745022));
#255560=CARTESIAN_POINT('Ctrl Pts',(76.4945703804041,-27.1260772883268,
16.1236712941765));
#255561=CARTESIAN_POINT('Ctrl Pts',(76.4947889315256,-27.1263896838556,
16.1240592573253));
#255562=CARTESIAN_POINT('Ctrl Pts',(76.4950049324771,-27.1266982100965,
16.1244524123546));
#255563=CARTESIAN_POINT('Ctrl Pts',(76.4952182372907,-27.1270026655085,
16.1248510388549));
#255564=CARTESIAN_POINT('',(76.5327357173579,-27.1805645602878,16.1924969468896));
#255565=CARTESIAN_POINT('Ctrl Pts',(76.4952187502335,-27.1270024565246,
16.124850966727));
#255566=CARTESIAN_POINT('Ctrl Pts',(76.5060555611233,-27.1424765582316,
16.145108493606));
#255567=CARTESIAN_POINT('Ctrl Pts',(76.5171175270378,-27.1582694710288,
16.1650670145225));
#255568=CARTESIAN_POINT('Ctrl Pts',(76.5283030866075,-27.1742368462728,
16.1847307926956));
#255569=CARTESIAN_POINT('Ctrl Pts',(76.5297785500957,-27.1763430689457,
16.1873246000552));
#255570=CARTESIAN_POINT('Ctrl Pts',(76.5312561693226,-27.1784523961998,
16.1899133064308));
#255571=CARTESIAN_POINT('Ctrl Pts',(76.5327357173579,-27.1805645602878,
16.1924969468896));
#255572=CARTESIAN_POINT('',(110.478801107225,-75.6605890912239,16.1925));
#255573=CARTESIAN_POINT('',(76.4071670555372,-27.0012528338594,14.2875));
#255574=CARTESIAN_POINT('Origin',(0.,0.,12.3825));
#255575=CARTESIAN_POINT('',(112.039285751595,-74.5679259799751,12.3825));
#255576=CARTESIAN_POINT('',(113.095,-76.1978262581577,12.3825));
#255577=CARTESIAN_POINT('Origin',(90.,-90.,12.3825));
#255578=CARTESIAN_POINT('',(113.095,76.1978262581577,12.3825));
#255579=CARTESIAN_POINT('',(113.095,90.,12.3825));
#255580=CARTESIAN_POINT('',(112.039285751595,74.5679259799752,12.3825));
#255581=CARTESIAN_POINT('Origin',(90.,90.,12.3825));
#255582=CARTESIAN_POINT('',(77.9676516999077,25.9085897226107,12.3825));
#255583=CARTESIAN_POINT('',(112.039285751595,-74.5679259799751,12.3825));
#255584=CARTESIAN_POINT('Origin',(110.478801107225,75.6605890912239,12.3825));
#255585=CARTESIAN_POINT('',(76.532736336798,27.1805822708749,16.1924981569221));
#255586=CARTESIAN_POINT('',(110.478801107225,75.6605890912239,16.1925));
#255587=CARTESIAN_POINT('',(76.4071670555372,27.0012528338594,15.6374346123617));
#255588=CARTESIAN_POINT('Origin',(83.0120747021563,36.4340385244726,14.6668526149847));
#255589=CARTESIAN_POINT('',(76.4071670555372,27.0012528338594,12.3825));
#255590=CARTESIAN_POINT('',(110.478801107225,75.6605890912239,14.2875));
#255591=CARTESIAN_POINT('Origin',(-90.,-90.,8.255));
#255592=CARTESIAN_POINT('Origin',(0.,0.,42.4815));
#255593=CARTESIAN_POINT('Origin',(-90.,-90.,0.0381));
#255594=CARTESIAN_POINT('Origin',(0.,0.,17.0741173620444));
#255595=CARTESIAN_POINT('Origin',(11.0165705888139,72.9917616471425,17.0741029655967));
#255596=CARTESIAN_POINT('Ctrl Pts',(24.6976449914385,76.0424582865173,17.8479876926671));
#255597=CARTESIAN_POINT('Ctrl Pts',(24.7379368836041,76.0624207920021,17.5919904624028));
#255598=CARTESIAN_POINT('Ctrl Pts',(24.758292886385,76.0725110230494,17.3340474816321));
#255599=CARTESIAN_POINT('Ctrl Pts',(24.758292886385,76.0725110230494,17.0741173620444));
#255600=CARTESIAN_POINT('Origin',(0.,0.,17.0741173620445));
#255601=CARTESIAN_POINT('Origin',(-11.016570588808,72.9917616471582,17.0741029655978));
#255602=CARTESIAN_POINT('Ctrl Pts',(-24.758292886385,76.0725110230494,17.0741173620445));
#255603=CARTESIAN_POINT('Ctrl Pts',(-24.758292886385,76.0725110230494,17.3340474816322));
#255604=CARTESIAN_POINT('Ctrl Pts',(-24.7379368836041,76.0624207920021,
17.5919904624029));
#255605=CARTESIAN_POINT('Ctrl Pts',(-24.6976449914385,76.0424582865173,
17.8479876926672));
#255606=CARTESIAN_POINT('Origin',(0.,0.,17.0741173620444));
#255607=CARTESIAN_POINT('Ctrl Pts',(-24.6976449914385,-76.0424582865173,
17.8479876926671));
#255608=CARTESIAN_POINT('Ctrl Pts',(-24.7379368836041,-76.0624207920021,
17.5919904624028));
#255609=CARTESIAN_POINT('Ctrl Pts',(-24.7582928863851,-76.0725110230494,
17.3340474816322));
#255610=CARTESIAN_POINT('Ctrl Pts',(-24.7582928863851,-76.0725110230494,
17.0741173620444));
#255611=CARTESIAN_POINT('Ctrl Pts',(24.758292886385,-76.0725110230494,17.0741173620444));
#255612=CARTESIAN_POINT('Ctrl Pts',(24.758292886385,-76.0725110230494,17.3340474816322));
#255613=CARTESIAN_POINT('Ctrl Pts',(24.7379368836041,-76.0624207920021,
17.5919904624028));
#255614=CARTESIAN_POINT('Ctrl Pts',(24.6976449914385,-76.0424582865173,
17.8479876926671));
#255615=CARTESIAN_POINT('Origin',(0.,0.,17.0741173620445));
#255616=CARTESIAN_POINT('Ctrl Pts',(76.0424582865173,-24.6976449914385,
17.8479876926672));
#255617=CARTESIAN_POINT('Ctrl Pts',(76.0624207920021,-24.7379368836041,
17.5919904624029));
#255618=CARTESIAN_POINT('Ctrl Pts',(76.0725110230494,-24.758292886385,17.3340474816323));
#255619=CARTESIAN_POINT('Ctrl Pts',(76.0725110230494,-24.758292886385,17.0741173620445));
#255620=CARTESIAN_POINT('Ctrl Pts',(76.0725110230494,24.758292886385,17.0741173620445));
#255621=CARTESIAN_POINT('Ctrl Pts',(76.0725110230494,24.758292886385,17.3340474816323));
#255622=CARTESIAN_POINT('Ctrl Pts',(76.0624207920021,24.737936883604,17.5919904624035));
#255623=CARTESIAN_POINT('Ctrl Pts',(76.0424582865173,24.6976449914384,17.8479876926672));
#255624=CARTESIAN_POINT('Origin',(-25.5443686855278,-78.4878132480312,12.3825));
#255625=CARTESIAN_POINT('',(-25.1428889948603,-75.9797434607283,17.0741173620444));
#255626=CARTESIAN_POINT('Origin',(-25.5443686855278,-78.4878132480312,17.0741173620444));
#255627=CARTESIAN_POINT('Ctrl Pts',(-25.1428889948603,-75.9797434607284,
17.0741173620444));
#255628=CARTESIAN_POINT('Ctrl Pts',(-25.1890962633323,-75.9723468244997,
17.0307425600543));
#255629=CARTESIAN_POINT('Ctrl Pts',(-25.2371152677862,-75.965973253375,
16.9901866401575));
#255630=CARTESIAN_POINT('Ctrl Pts',(-25.2866741011431,-75.9609192056981,
16.9519675478226));
#255631=CARTESIAN_POINT('Ctrl Pts',(-25.3351466800543,-75.9559759350792,
16.9145861600128));
#255632=CARTESIAN_POINT('Ctrl Pts',(-25.385092021647,-75.9522954968805,
16.8794402829931));
#255633=CARTESIAN_POINT('Ctrl Pts',(-25.4362249260052,-75.9501164719612,
16.8460788702544));
#255634=CARTESIAN_POINT('Ctrl Pts',(-25.4862159183351,-75.9479861095381,
16.8134624924197));
#255635=CARTESIAN_POINT('Ctrl Pts',(-25.5373416156511,-75.947291198436,
16.7825517666789));
#255636=CARTESIAN_POINT('Ctrl Pts',(-25.5893110141088,-75.9482108801197,
16.7529251953267));
#255637=CARTESIAN_POINT('Ctrl Pts',(-25.5996216874803,-75.9483933439875,
16.7470473150857));
#255638=CARTESIAN_POINT('Ctrl Pts',(-25.6099655036174,-75.9486392118567,
16.7412199819069));
#255639=CARTESIAN_POINT('Ctrl Pts',(-25.620340095261,-75.948949654826,16.7354399041433));
#255640=CARTESIAN_POINT('Ctrl Pts',(-25.6678229409188,-75.9503705026149,
16.7089854132328));
#255641=CARTESIAN_POINT('Ctrl Pts',(-25.7161033957531,-75.9531525557282,
16.6835468572545));
#255642=CARTESIAN_POINT('Ctrl Pts',(-25.7648841738475,-75.9574036133256,
16.6590804688497));
#255643=CARTESIAN_POINT('Ctrl Pts',(-25.8132372046341,-75.9616173943867,
16.6348286205195));
#255644=CARTESIAN_POINT('Ctrl Pts',(-25.8620813654555,-75.9672746984588,
16.6115319650909));
#255645=CARTESIAN_POINT('Ctrl Pts',(-25.9111193560843,-75.9744302796704,
16.5891478764961));
#255646=CARTESIAN_POINT('Ctrl Pts',(-25.9597789956168,-75.981530652217,
16.5669364916428));
#255647=CARTESIAN_POINT('Ctrl Pts',(-26.0086290088543,-75.9901063190922,
16.5456236461848));
#255648=CARTESIAN_POINT('Ctrl Pts',(-26.0573782086223,-76.0001594881172,
16.5251676931017));
#255649=CARTESIAN_POINT('Ctrl Pts',(-26.0882583186412,-76.0065276534822,
16.5122098992352));
#255650=CARTESIAN_POINT('Ctrl Pts',(-26.1190979844471,-76.0134876389456,
16.499595939491));
#255651=CARTESIAN_POINT('Ctrl Pts',(-26.1498243779419,-76.0210292273835,
16.4873152282082));
#255652=CARTESIAN_POINT('Ctrl Pts',(-26.2179462859377,-76.0377492955487,
16.4600882943257));
#255653=CARTESIAN_POINT('Ctrl Pts',(-26.2860317992692,-76.0574561602205,
16.4342868904806));
#255654=CARTESIAN_POINT('Ctrl Pts',(-26.3537219308309,-76.0802112617558,
16.4098106473489));
#255655=CARTESIAN_POINT('Ctrl Pts',(-26.4210710446893,-76.1028517248309,
16.3854577136573));
#255656=CARTESIAN_POINT('Ctrl Pts',(-26.4880282443266,-76.1285099018948,
16.3624166221961));
#255657=CARTESIAN_POINT('Ctrl Pts',(-26.5542307553397,-76.1571956045824,
16.3405885129707));
#255658=CARTESIAN_POINT('Ctrl Pts',(-26.594797053722,-76.1747730764444,
16.327213105023));
#255659=CARTESIAN_POINT('Ctrl Pts',(-26.6350798348181,-76.1934863070453,
16.314293142431));
#255660=CARTESIAN_POINT('Ctrl Pts',(-26.6749951887979,-76.2133278754462,
16.3018058798072));
#255661=CARTESIAN_POINT('Ctrl Pts',(-26.7414052730145,-76.2463397392307,
16.2810299106675));
#255662=CARTESIAN_POINT('Ctrl Pts',(-26.8065749011848,-76.282357702662,
16.2615818620403));
#255663=CARTESIAN_POINT('Ctrl Pts',(-26.870393440276,-76.3214203128057,
16.2431559979634));
#255664=CARTESIAN_POINT('Ctrl Pts',(-26.8885104503037,-76.3325095309195,
16.2379252050151));
#255665=CARTESIAN_POINT('Ctrl Pts',(-26.9065183420908,-76.3438443339879,
16.2327767895739));
#255666=CARTESIAN_POINT('Ctrl Pts',(-26.9244139858109,-76.3554260952922,
16.2277037569974));
#255667=CARTESIAN_POINT('Ctrl Pts',(-26.9473795640672,-76.3702890334318,
16.2211935063209));
#255668=CARTESIAN_POINT('Ctrl Pts',(-26.9702988091961,-76.3856535929665,
16.2155241412993));
#255669=CARTESIAN_POINT('Ctrl Pts',(-26.9928245401834,-76.4012908692599,
16.2092079610165));
#255670=CARTESIAN_POINT('Ctrl Pts',(-27.0099909644426,-76.4132077353212,
16.2043945220878));
#255671=CARTESIAN_POINT('Ctrl Pts',(-27.0269293937101,-76.4252820333718,
16.1992054342301));
#255672=CARTESIAN_POINT('Ctrl Pts',(-27.0434980077865,-76.4373959063312,
16.1929822540025));
#255673=CARTESIAN_POINT('Ctrl Pts',(-27.0482867453259,-76.4408971139712,
16.1911836016449));
#255674=CARTESIAN_POINT('Ctrl Pts',(-27.0532391486278,-76.4445482450871,
16.1893664854189));
#255675=CARTESIAN_POINT('Ctrl Pts',(-27.0570025619875,-76.44733811812,16.1852582407542));
#255676=CARTESIAN_POINT('Ctrl Pts',(-27.0603326521686,-76.4498067623811,
16.1816230234896));
#255677=CARTESIAN_POINT('Ctrl Pts',(-27.0611677349716,-76.450432092947,
16.1755676007548));
#255678=CARTESIAN_POINT('Ctrl Pts',(-27.0602432495845,-76.4497444793078,
16.1701033997377));
#255679=CARTESIAN_POINT('Ctrl Pts',(-27.0601229522577,-76.4496550045753,
16.1693923784665));
#255680=CARTESIAN_POINT('Ctrl Pts',(-27.0599728200255,-76.449543354985,
16.1686913678441));
#255681=CARTESIAN_POINT('Ctrl Pts',(-27.059794441605,-76.4494107416999,
16.1680070028586));
#255682=CARTESIAN_POINT('Ctrl Pts',(-27.057267811496,-76.4475323490217,
16.1583133573314));
#255683=CARTESIAN_POINT('Ctrl Pts',(-27.0523400392582,-76.4438795871955,
16.1500702655799));
#255684=CARTESIAN_POINT('Ctrl Pts',(-27.0470895061924,-76.4400266050576,
16.1422372666814));
#255685=CARTESIAN_POINT('Ctrl Pts',(-27.0459012525003,-76.4391546325944,
16.140464572415));
#255686=CARTESIAN_POINT('Ctrl Pts',(-27.0446965952314,-76.4382722357617,
16.1387128817492));
#255687=CARTESIAN_POINT('Ctrl Pts',(-27.0434998998452,-76.4373972896805,
16.1369701348008));
#255688=CARTESIAN_POINT('Ctrl Pts',(-27.0334981288328,-76.4300846431602,
16.1224045602098));
#255689=CARTESIAN_POINT('Ctrl Pts',(-27.0225381835934,-76.4221888169319,
16.1088060042605));
#255690=CARTESIAN_POINT('Ctrl Pts',(-27.0113044494425,-76.414241579497,
16.0954740612667));
#255691=CARTESIAN_POINT('Ctrl Pts',(-27.007971666701,-76.4118838224582,
16.091518789678));
#255692=CARTESIAN_POINT('Ctrl Pts',(-27.0046149921548,-76.4095212641203,
16.0875869845165));
#255693=CARTESIAN_POINT('Ctrl Pts',(-27.0012528338594,-76.4071670555372,
16.0836603564332));
#255694=CARTESIAN_POINT('Origin',(-25.5443686855278,-78.4878132480312,14.2875));
#255695=CARTESIAN_POINT('Ctrl Pts',(-25.1452786192767,-75.9793621085789,
17.0741173620444));
#255696=CARTESIAN_POINT('Ctrl Pts',(-24.9481252017973,-76.0107288628306,
17.0741173620444));
#255697=CARTESIAN_POINT('Ctrl Pts',(-24.7582928863851,-76.0725110230494,
17.0741173620444));
#255698=CARTESIAN_POINT('Ctrl Pts',(-25.1452785074244,-75.9793621491339,
17.3508457847221));
#255699=CARTESIAN_POINT('Ctrl Pts',(-24.9481251187334,-76.0107288897049,
17.343404115285));
#255700=CARTESIAN_POINT('Ctrl Pts',(-24.7582928856604,-76.0725110232853,
17.337178022204));
#255701=CARTESIAN_POINT('Ctrl Pts',(-25.1240988983272,-75.9676381104172,
17.623822449221));
#255702=CARTESIAN_POINT('Ctrl Pts',(-24.927113661929,-75.9996785825189,
17.6090181824143));
#255703=CARTESIAN_POINT('Ctrl Pts',(-24.7374486679108,-76.0621788292388,
17.5966189870095));
#255704=CARTESIAN_POINT('Ctrl Pts',(-25.0829574281539,-75.9448790163861,
17.8928559119209));
#255705=CARTESIAN_POINT('Ctrl Pts',(-24.8862836604199,-75.9782191703494,
17.8708938349951));
#255706=CARTESIAN_POINT('Ctrl Pts',(-24.6969219387962,-76.0421000528014,
17.8525678740453));
#255707=CARTESIAN_POINT('',(-24.994844812995,-76.0045572676648,17.2916572676617));
#255708=CARTESIAN_POINT('Ctrl Pts',(-24.6976449917882,-76.0424582864821,
17.8479876920601));
#255709=CARTESIAN_POINT('Ctrl Pts',(-24.7503755173217,-76.0371538019006,
17.756416129007));
#255710=CARTESIAN_POINT('Ctrl Pts',(-24.8016570938352,-76.0312759441799,
17.6640492729856));
#255711=CARTESIAN_POINT('Ctrl Pts',(-24.8514227931199,-76.0249016926983,
17.5708849989251));
#255712=CARTESIAN_POINT('Ctrl Pts',(-24.9007299287131,-76.0185861764566,
17.4785791826788));
#255713=CARTESIAN_POINT('Ctrl Pts',(-24.9485484285534,-76.0117822407742,
17.3854910071203));
#255714=CARTESIAN_POINT('Ctrl Pts',(-24.9948448130088,-76.0045572676613,
17.2916572676744));
#255715=CARTESIAN_POINT('Ctrl Pts',(-24.9948448130088,-76.0045572676613,
17.2916572676744));
#255716=CARTESIAN_POINT('Ctrl Pts',(-25.0341234730694,-75.9984274744393,
17.2120470870499));
#255717=CARTESIAN_POINT('Ctrl Pts',(-25.0842002511862,-75.9891380711875,
17.1401458391912));
#255718=CARTESIAN_POINT('Ctrl Pts',(-25.1428889948603,-75.9797434607283,
17.0741173620444));
#255719=CARTESIAN_POINT('Origin',(25.5443686855278,-78.4878132480313,12.3825));
#255720=CARTESIAN_POINT('',(25.1428889948603,-75.9797434607284,17.0741173620444));
#255721=CARTESIAN_POINT('Ctrl Pts',(27.0012528338594,-76.4071670555372,
16.0836576814802));
#255722=CARTESIAN_POINT('Ctrl Pts',(27.0125669096155,-76.4150892566695,
16.0968733108111));
#255723=CARTESIAN_POINT('Ctrl Pts',(27.0238163261266,-76.4231092878419,
16.1101516546325));
#255724=CARTESIAN_POINT('Ctrl Pts',(27.0343062667017,-76.4307070270972,
16.124170648169));
#255725=CARTESIAN_POINT('Ctrl Pts',(27.0373959399464,-76.4329448406986,
16.1282997572844));
#255726=CARTESIAN_POINT('Ctrl Pts',(27.0404199372171,-76.4351457336101,
16.1324931191775));
#255727=CARTESIAN_POINT('Ctrl Pts',(27.0433610058765,-76.4372957466342,
16.1367680561971));
#255728=CARTESIAN_POINT('Ctrl Pts',(27.0486625218437,-76.4411713203446,
16.1444739785989));
#255729=CARTESIAN_POINT('Ctrl Pts',(27.0541110981828,-76.4451930160954,
16.1523581093346));
#255730=CARTESIAN_POINT('Ctrl Pts',(27.0576635438242,-76.4478282794951,
16.1614817309479));
#255731=CARTESIAN_POINT('Ctrl Pts',(27.0584419906684,-76.4484057443416,
16.1634809886902));
#255732=CARTESIAN_POINT('Ctrl Pts',(27.0591295221735,-76.448916457713,16.1655397641649));
#255733=CARTESIAN_POINT('Ctrl Pts',(27.0597047898622,-76.4493440942542,
16.1676692243483));
#255734=CARTESIAN_POINT('Ctrl Pts',(27.061128686084,-76.4504025754923,16.1729400406464));
#255735=CARTESIAN_POINT('Ctrl Pts',(27.0609586584413,-76.4502741704977,
16.1792319783503));
#255736=CARTESIAN_POINT('Ctrl Pts',(27.05833972207,-76.4483300535648,16.1834945076105));
#255737=CARTESIAN_POINT('Ctrl Pts',(27.0580153550188,-76.4480892659368,
16.1840224410349));
#255738=CARTESIAN_POINT('Ctrl Pts',(27.0576533814908,-76.4478206797893,
16.184519243462));
#255739=CARTESIAN_POINT('Ctrl Pts',(27.0572521366115,-76.4475231550697,
16.1849791191285));
#255740=CARTESIAN_POINT('Ctrl Pts',(27.0536112445358,-76.4448234187001,
16.1891520263895));
#255741=CARTESIAN_POINT('Ctrl Pts',(27.0486162668499,-76.441139274083,16.1910424108882));
#255742=CARTESIAN_POINT('Ctrl Pts',(27.0438314274414,-76.4376397222992,
16.1928564397759));
#255743=CARTESIAN_POINT('Ctrl Pts',(27.0219957335603,-76.4216694597787,
16.2011347906466));
#255744=CARTESIAN_POINT('Ctrl Pts',(26.9995297758924,-76.4057789951842,
16.2075349627597));
#255745=CARTESIAN_POINT('Ctrl Pts',(26.9767570400582,-76.3902280645868,
16.2136304689842));
#255746=CARTESIAN_POINT('Ctrl Pts',(26.9596083941578,-76.3785176840609,
16.2182205928317));
#255747=CARTESIAN_POINT('Ctrl Pts',(26.9422864764177,-76.3669990447857,
16.2226379527468));
#255748=CARTESIAN_POINT('Ctrl Pts',(26.9249406691735,-76.3557670482568,
16.2275544634756));
#255749=CARTESIAN_POINT('Ctrl Pts',(26.8616514023731,-76.3147851086444,
16.2454932284381));
#255750=CARTESIAN_POINT('Ctrl Pts',(26.7969330658208,-76.2768724921605,
16.2643805415009));
#255751=CARTESIAN_POINT('Ctrl Pts',(26.7309055253999,-76.2419881596448,
16.2845312318663));
#255752=CARTESIAN_POINT('Ctrl Pts',(26.7126781403842,-76.2323580847438,
16.2900939771887));
#255753=CARTESIAN_POINT('Ctrl Pts',(26.6943507540625,-76.222958992946,16.2957530015098));
#255754=CARTESIAN_POINT('Ctrl Pts',(26.675925399516,-76.2137905122108,16.3015149281042));
#255755=CARTESIAN_POINT('Ctrl Pts',(26.6064313477857,-76.1792101803703,
16.3232469183247));
#255756=CARTESIAN_POINT('Ctrl Pts',(26.5358861365389,-76.1480850328896,
16.3462666758162));
#255757=CARTESIAN_POINT('Ctrl Pts',(26.4646896591077,-76.1204076415521,
16.3707095301105));
#255758=CARTESIAN_POINT('Ctrl Pts',(26.3929595634036,-76.0925228079044,
16.3953355838293));
#255759=CARTESIAN_POINT('Ctrl Pts',(26.3205688608561,-76.0681374467385,
16.4214061465416));
#255760=CARTESIAN_POINT('Ctrl Pts',(26.2479119389207,-76.0471930623806,
16.4490596135311));
#255761=CARTESIAN_POINT('Ctrl Pts',(26.2159174362015,-76.0379701949037,
16.4612368280514));
#255762=CARTESIAN_POINT('Ctrl Pts',(26.1838710809961,-76.0294139168384,
16.4737209810889));
#255763=CARTESIAN_POINT('Ctrl Pts',(26.1518053240938,-76.0215162808905,
16.4865238898931));
#255764=CARTESIAN_POINT('Ctrl Pts',(26.1024355298056,-76.009356746865,16.5062357892841));
#255765=CARTESIAN_POINT('Ctrl Pts',(26.052778843371,-75.9987033871209,16.5268004120897));
#255766=CARTESIAN_POINT('Ctrl Pts',(26.0031235829827,-75.9895850871018,
16.5482718578781));
#255767=CARTESIAN_POINT('Ctrl Pts',(25.9532562285115,-75.9804278397996,
16.5698350153315));
#255768=CARTESIAN_POINT('Ctrl Pts',(25.9033908081985,-75.9728187929612,
16.5923127589954));
#255769=CARTESIAN_POINT('Ctrl Pts',(25.8538229261267,-75.966734496192,16.615759884635));
#255770=CARTESIAN_POINT('Ctrl Pts',(25.8036709954625,-75.9605785093523,
16.6394832831383));
#255771=CARTESIAN_POINT('Ctrl Pts',(25.7538241560404,-75.9559833526325,
16.6641990422746));
#255772=CARTESIAN_POINT('Ctrl Pts',(25.7045846567395,-75.9528712679124,
16.6899639176645));
#255773=CARTESIAN_POINT('Ctrl Pts',(25.6770558349516,-75.951131363428,16.7043685455154));
#255774=CARTESIAN_POINT('Ctrl Pts',(25.6497167346353,-75.9498540709319,
16.719101096162));
#255775=CARTESIAN_POINT('Ctrl Pts',(25.6226187918313,-75.9490188646943,
16.7341714877587));
#255776=CARTESIAN_POINT('Ctrl Pts',(25.5764663692891,-75.9475963658918,
16.7598389373462));
#255777=CARTESIAN_POINT('Ctrl Pts',(25.5307625072541,-75.9474517866683,
16.7865659943229));
#255778=CARTESIAN_POINT('Ctrl Pts',(25.4858135567854,-75.948488279285,16.8145610357063));
#255779=CARTESIAN_POINT('Ctrl Pts',(25.440208013082,-75.9495399125009,16.842965015554));
#255780=CARTESIAN_POINT('Ctrl Pts',(25.3953800373707,-75.951807126726,16.8726742946166));
#255781=CARTESIAN_POINT('Ctrl Pts',(25.3516355174112,-75.9551360230561,
16.9039065155736));
#255782=CARTESIAN_POINT('Ctrl Pts',(25.3063675036794,-75.9585808551156,
16.9362264634999));
#255783=CARTESIAN_POINT('Ctrl Pts',(25.2622601849893,-75.9631623243896,
16.9701772797651));
#255784=CARTESIAN_POINT('Ctrl Pts',(25.2196304529756,-75.9686576195877,
17.0060001477704));
#255785=CARTESIAN_POINT('Ctrl Pts',(25.1934712691005,-75.9720297364354,
17.0279823875551));
#255786=CARTESIAN_POINT('Ctrl Pts',(25.1678679994915,-75.9757449423844,
17.0506695492733));
#255787=CARTESIAN_POINT('Ctrl Pts',(25.1428889948603,-75.9797434607284,
17.0741173620444));
#255788=CARTESIAN_POINT('Origin',(25.5443686855278,-78.4878132480313,17.0741173620444));
#255789=CARTESIAN_POINT('Origin',(25.5443686855278,-78.4878132480313,14.2875));
#255790=CARTESIAN_POINT('Ctrl Pts',(24.758292886385,-76.0725110230494,17.0741173620444));
#255791=CARTESIAN_POINT('Ctrl Pts',(24.9481252017973,-76.0107288628306,
17.0741173620444));
#255792=CARTESIAN_POINT('Ctrl Pts',(25.1452786192766,-75.9793621085789,
17.0741173620444));
#255793=CARTESIAN_POINT('Ctrl Pts',(24.7582928856599,-76.0725110232854,
17.3371780222037));
#255794=CARTESIAN_POINT('Ctrl Pts',(24.9481251187328,-76.0107288897046,
17.3434041152845));
#255795=CARTESIAN_POINT('Ctrl Pts',(25.1452785074237,-75.9793621491333,
17.3508457847214));
#255796=CARTESIAN_POINT('Ctrl Pts',(24.7374486679123,-76.0621788292383,
17.5966189870099));
#255797=CARTESIAN_POINT('Ctrl Pts',(24.9271136619309,-75.9996785825196,
17.6090181824149));
#255798=CARTESIAN_POINT('Ctrl Pts',(25.1240988983294,-75.9676381104188,
17.6238224492219));
#255799=CARTESIAN_POINT('Ctrl Pts',(24.6969219387962,-76.0421000528014,
17.8525678740453));
#255800=CARTESIAN_POINT('Ctrl Pts',(24.8862836604198,-75.9782191703494,
17.8708938349951));
#255801=CARTESIAN_POINT('Ctrl Pts',(25.0829574281538,-75.9448790163861,
17.8928559119209));
#255802=CARTESIAN_POINT('',(24.9948448129998,-76.004557267664,17.2916572676518));
#255803=CARTESIAN_POINT('Ctrl Pts',(25.1428889948603,-75.9797434607284,
17.0741173620444));
#255804=CARTESIAN_POINT('Ctrl Pts',(25.0842002511886,-75.9891380711871,
17.1401458391885));
#255805=CARTESIAN_POINT('Ctrl Pts',(25.0341234730735,-75.9984274744386,
17.2120470870438));
#255806=CARTESIAN_POINT('Ctrl Pts',(24.9948448130136,-76.0045572676606,
17.2916572676645));
#255807=CARTESIAN_POINT('Ctrl Pts',(24.9948448130136,-76.0045572676606,
17.2916572676645));
#255808=CARTESIAN_POINT('Ctrl Pts',(24.9481178557882,-76.0118494355815,
17.386363694133));
#255809=CARTESIAN_POINT('Ctrl Pts',(24.8998402835406,-76.0187126993903,
17.4803105665639));
#255810=CARTESIAN_POINT('Ctrl Pts',(24.8500466861399,-76.0250777755062,
17.5734602270335));
#255811=CARTESIAN_POINT('Ctrl Pts',(24.8007119296855,-76.0313841983473,
17.6657515265775));
#255812=CARTESIAN_POINT('Ctrl Pts',(24.7498896236257,-76.0372026809097,
17.7572599295026));
#255813=CARTESIAN_POINT('Ctrl Pts',(24.697644991789,-76.0424582864817,17.8479876920608));
#255814=CARTESIAN_POINT('Origin',(78.4878132480313,-25.5443686855277,12.3825));
#255815=CARTESIAN_POINT('',(75.9797434607283,-25.1428889948603,17.0741173620445));
#255816=CARTESIAN_POINT('Origin',(78.4878132480312,-25.5443686855278,17.0741173620445));
#255817=CARTESIAN_POINT('Ctrl Pts',(75.9797434607284,-25.1428889948603,
17.0741173620445));
#255818=CARTESIAN_POINT('Ctrl Pts',(75.9723468244997,-25.1890962633322,
17.0307425600544));
#255819=CARTESIAN_POINT('Ctrl Pts',(75.965973253375,-25.2371152677861,16.9901866401576));
#255820=CARTESIAN_POINT('Ctrl Pts',(75.9609192056981,-25.286674101143,16.9519675478227));
#255821=CARTESIAN_POINT('Ctrl Pts',(75.9559759350792,-25.3351466800541,
16.914586160013));
#255822=CARTESIAN_POINT('Ctrl Pts',(75.9522954968805,-25.3850920216466,
16.8794402829934));
#255823=CARTESIAN_POINT('Ctrl Pts',(75.9501164719612,-25.4362249260047,
16.8460788702548));
#255824=CARTESIAN_POINT('Ctrl Pts',(75.9479861095382,-25.4862159183344,
16.8134624924202));
#255825=CARTESIAN_POINT('Ctrl Pts',(75.9472911984361,-25.5373416156502,
16.7825517666794));
#255826=CARTESIAN_POINT('Ctrl Pts',(75.9482108801197,-25.5893110141078,
16.7529251953273));
#255827=CARTESIAN_POINT('Ctrl Pts',(75.9483933439875,-25.5996216874797,
16.7470473150861));
#255828=CARTESIAN_POINT('Ctrl Pts',(75.9486392118567,-25.6099655036172,
16.741219981907));
#255829=CARTESIAN_POINT('Ctrl Pts',(75.948949654826,-25.6203400952611,16.7354399041433));
#255830=CARTESIAN_POINT('Ctrl Pts',(75.9503705026149,-25.667822940919,16.7089854132327));
#255831=CARTESIAN_POINT('Ctrl Pts',(75.9531525557283,-25.7161033957533,
16.6835468572544));
#255832=CARTESIAN_POINT('Ctrl Pts',(75.9574036133257,-25.7648841738477,
16.6590804688496));
#255833=CARTESIAN_POINT('Ctrl Pts',(75.9616173943868,-25.8132372046344,
16.6348286205194));
#255834=CARTESIAN_POINT('Ctrl Pts',(75.9672746984589,-25.8620813654559,
16.6115319650908));
#255835=CARTESIAN_POINT('Ctrl Pts',(75.9744302796705,-25.9111193560848,
16.5891478764959));
#255836=CARTESIAN_POINT('Ctrl Pts',(75.9815306522171,-25.9597789956173,
16.5669364916427));
#255837=CARTESIAN_POINT('Ctrl Pts',(75.9901063190923,-26.0086290088549,
16.5456236461847));
#255838=CARTESIAN_POINT('Ctrl Pts',(76.0001594881174,-26.0573782086229,
16.5251676931015));
#255839=CARTESIAN_POINT('Ctrl Pts',(76.0065276534823,-26.0882583186417,
16.5122098992351));
#255840=CARTESIAN_POINT('Ctrl Pts',(76.0134876389457,-26.1190979844475,
16.4995959394909));
#255841=CARTESIAN_POINT('Ctrl Pts',(76.0210292273836,-26.1498243779423,
16.4873152282081));
#255842=CARTESIAN_POINT('Ctrl Pts',(76.0377492955488,-26.2179462859379,
16.4600882943257));
#255843=CARTESIAN_POINT('Ctrl Pts',(76.0574561602205,-26.2860317992692,
16.4342868904806));
#255844=CARTESIAN_POINT('Ctrl Pts',(76.0802112617558,-26.3537219308308,
16.409810647349));
#255845=CARTESIAN_POINT('Ctrl Pts',(76.1028517248309,-26.4210710446892,
16.3854577136574));
#255846=CARTESIAN_POINT('Ctrl Pts',(76.1285099018948,-26.4880282443265,
16.3624166221961));
#255847=CARTESIAN_POINT('Ctrl Pts',(76.1571956045824,-26.5542307553397,
16.3405885129707));
#255848=CARTESIAN_POINT('Ctrl Pts',(76.1747730764445,-26.5947970537221,
16.327213105023));
#255849=CARTESIAN_POINT('Ctrl Pts',(76.1934863070455,-26.6350798348184,
16.3142931424309));
#255850=CARTESIAN_POINT('Ctrl Pts',(76.2133278754465,-26.6749951887984,
16.3018058798071));
#255851=CARTESIAN_POINT('Ctrl Pts',(76.2463397392302,-26.7414052730132,
16.281029910668));
#255852=CARTESIAN_POINT('Ctrl Pts',(76.2823577026604,-26.8065749011818,
16.2615818620412));
#255853=CARTESIAN_POINT('Ctrl Pts',(76.321420312803,-26.8703934402714,16.2431559979648));
#255854=CARTESIAN_POINT('Ctrl Pts',(76.3325095309177,-26.8885104503009,
16.2379252050159));
#255855=CARTESIAN_POINT('Ctrl Pts',(76.3438443339872,-26.9065183420897,
16.2327767895743));
#255856=CARTESIAN_POINT('Ctrl Pts',(76.3554260952926,-26.9244139858114,
16.2277037569972));
#255857=CARTESIAN_POINT('Ctrl Pts',(76.3702890334322,-26.9473795640677,
16.2211935063208));
#255858=CARTESIAN_POINT('Ctrl Pts',(76.3856535929669,-26.9702988091965,
16.2155241412992));
#255859=CARTESIAN_POINT('Ctrl Pts',(76.4012908692602,-26.9928245401838,
16.2092079610165));
#255860=CARTESIAN_POINT('Ctrl Pts',(76.4132077353215,-27.0099909644431,
16.2043945220878));
#255861=CARTESIAN_POINT('Ctrl Pts',(76.4252820333722,-27.0269293937106,
16.19920543423));
#255862=CARTESIAN_POINT('Ctrl Pts',(76.4373959063317,-27.043498007787,16.1929822540023));
#255863=CARTESIAN_POINT('Ctrl Pts',(76.4408971139716,-27.0482867453264,
16.1911836016447));
#255864=CARTESIAN_POINT('Ctrl Pts',(76.4445482450876,-27.0532391486283,
16.1893664854187));
#255865=CARTESIAN_POINT('Ctrl Pts',(76.4473381181204,-27.057002561988,16.1852582407538));
#255866=CARTESIAN_POINT('Ctrl Pts',(76.4498067623814,-27.0603326521689,
16.1816230234891));
#255867=CARTESIAN_POINT('Ctrl Pts',(76.4504320929472,-27.0611677349717,
16.1755676007542));
#255868=CARTESIAN_POINT('Ctrl Pts',(76.4497444793079,-27.0602432495845,
16.1701033997371));
#255869=CARTESIAN_POINT('Ctrl Pts',(76.4496550045754,-27.0601229522577,
16.1693923784658));
#255870=CARTESIAN_POINT('Ctrl Pts',(76.4495433549851,-27.0599728200255,
16.1686913678435));
#255871=CARTESIAN_POINT('Ctrl Pts',(76.4494107417,-27.059794441605,16.1680070028581));
#255872=CARTESIAN_POINT('Ctrl Pts',(76.4475323490217,-27.0572678114959,
16.158313357331));
#255873=CARTESIAN_POINT('Ctrl Pts',(76.4438795871955,-27.0523400392581,
16.1500702655797));
#255874=CARTESIAN_POINT('Ctrl Pts',(76.4400266050576,-27.0470895061923,
16.1422372666812));
#255875=CARTESIAN_POINT('Ctrl Pts',(76.4391546325943,-27.0459012525002,
16.1404645724148));
#255876=CARTESIAN_POINT('Ctrl Pts',(76.4382722357616,-27.0446965952312,
16.138712881749));
#255877=CARTESIAN_POINT('Ctrl Pts',(76.4373972896805,-27.043499899845,16.1369701348005));
#255878=CARTESIAN_POINT('Ctrl Pts',(76.4300846431601,-27.0334981288326,
16.1224045602096));
#255879=CARTESIAN_POINT('Ctrl Pts',(76.4221888169319,-27.0225381835933,
16.1088060042603));
#255880=CARTESIAN_POINT('Ctrl Pts',(76.414241579497,-27.0113044494424,16.0954740612665));
#255881=CARTESIAN_POINT('Ctrl Pts',(76.4118838224582,-27.0079716667009,
16.0915187896778));
#255882=CARTESIAN_POINT('Ctrl Pts',(76.4095212641203,-27.0046149921547,
16.0875869845164));
#255883=CARTESIAN_POINT('Ctrl Pts',(76.4071670555372,-27.0012528338594,
16.0836603564331));
#255884=CARTESIAN_POINT('Ctrl Pts',(75.9793621085789,-25.1452786192766,
17.0741173620445));
#255885=CARTESIAN_POINT('Ctrl Pts',(76.0107288628305,-24.9481252017973,
17.0741173620445));
#255886=CARTESIAN_POINT('Ctrl Pts',(76.0725110230494,-24.758292886385,17.0741173620445));
#255887=CARTESIAN_POINT('Ctrl Pts',(75.9793621491347,-25.1452785074261,
17.3508457847218));
#255888=CARTESIAN_POINT('Ctrl Pts',(76.010728889705,-24.9481251187354,17.343404115285));
#255889=CARTESIAN_POINT('Ctrl Pts',(76.0725110232845,-24.7582928856628,
17.3371780222044));
#255890=CARTESIAN_POINT('Ctrl Pts',(75.9676381104205,-25.124098898325,17.6238224492217));
#255891=CARTESIAN_POINT('Ctrl Pts',(75.9996785825213,-24.9271136619264,
17.6090181824145));
#255892=CARTESIAN_POINT('Ctrl Pts',(76.0621788292398,-24.7374486679078,
17.5966189870093));
#255893=CARTESIAN_POINT('Ctrl Pts',(75.9448790163861,-25.0829574281538,
17.892855911921));
#255894=CARTESIAN_POINT('Ctrl Pts',(75.9782191703494,-24.8862836604198,
17.8708938349952));
#255895=CARTESIAN_POINT('Ctrl Pts',(76.0421000528014,-24.6969219387962,
17.8525678740454));
#255896=CARTESIAN_POINT('',(76.0045572676648,-24.994844812995,17.2916572676618));
#255897=CARTESIAN_POINT('Ctrl Pts',(76.0424582864821,-24.6976449917882,
17.8479876920602));
#255898=CARTESIAN_POINT('Ctrl Pts',(76.0371538031763,-24.7503755046464,
17.7564161510145));
#255899=CARTESIAN_POINT('Ctrl Pts',(76.0312759470027,-24.8016570691911,
17.6640493173926));
#255900=CARTESIAN_POINT('Ctrl Pts',(76.0249016972925,-24.8514227572423,
17.5708850661044));
#255901=CARTESIAN_POINT('Ctrl Pts',(76.018586179756,-24.9007299055169,17.4785792278443));
#255902=CARTESIAN_POINT('Ctrl Pts',(76.0117822425276,-24.9485484173197,
17.3854910298794));
#255903=CARTESIAN_POINT('Ctrl Pts',(76.0045572676613,-24.9948448130087,
17.2916572676745));
#255904=CARTESIAN_POINT('Ctrl Pts',(76.0045572676613,-24.9948448130087,
17.2916572676745));
#255905=CARTESIAN_POINT('Ctrl Pts',(75.9984274744393,-25.0341234730694,
17.21204708705));
#255906=CARTESIAN_POINT('Ctrl Pts',(75.9891380711875,-25.0842002511861,
17.1401458391913));
#255907=CARTESIAN_POINT('Ctrl Pts',(75.9797434607283,-25.1428889948603,
17.0741173620445));
#255908=CARTESIAN_POINT('Origin',(78.4878132480313,25.5443686855277,12.3825));
#255909=CARTESIAN_POINT('',(76.4499922109615,27.0605762639536,16.1719291773585));
#255910=CARTESIAN_POINT('Ctrl Pts',(76.4071670555372,27.0012528338594,15.6374346123617));
#255911=CARTESIAN_POINT('Ctrl Pts',(76.4079750319809,27.0024067438069,15.6501237643143));
#255912=CARTESIAN_POINT('Ctrl Pts',(76.4087695213968,27.0035394221128,15.6628157309684));
#255913=CARTESIAN_POINT('Ctrl Pts',(76.4095938645954,27.0047125471957,15.675502067928));
#255914=CARTESIAN_POINT('Ctrl Pts',(76.4127017511593,27.0091353891497,15.7233312927615));
#255915=CARTESIAN_POINT('Ctrl Pts',(76.4160289816171,27.0138404705195,15.7711214832916));
#255916=CARTESIAN_POINT('Ctrl Pts',(76.4195777514373,27.0188183898679,15.8188607686969));
#255917=CARTESIAN_POINT('Ctrl Pts',(76.4283481319464,27.0311207506973,15.936842976462));
#255918=CARTESIAN_POINT('Ctrl Pts',(76.4384768596614,27.04509934281,16.0545629245959));
#255919=CARTESIAN_POINT('Ctrl Pts',(76.4499922109615,27.0605762639536,16.1719291773585));
#255920=CARTESIAN_POINT('',(75.9797434607283,25.1428889948603,17.0741173620445));
#255921=CARTESIAN_POINT('Ctrl Pts',(76.4499922109615,27.0605762639536,16.1719291773585));
#255922=CARTESIAN_POINT('Ctrl Pts',(76.4505698705024,27.0613526528738,16.1778167732404));
#255923=CARTESIAN_POINT('Ctrl Pts',(76.4488056783259,27.0589883665235,16.1839366447756));
#255924=CARTESIAN_POINT('Ctrl Pts',(76.4429004146046,27.0510060510084,16.1903007364945));
#255925=CARTESIAN_POINT('Ctrl Pts',(76.4394649837984,27.0463345060122,16.1919741158575));
#255926=CARTESIAN_POINT('Ctrl Pts',(76.4294701394813,27.032639963703,16.1969037700759));
#255927=CARTESIAN_POINT('Ctrl Pts',(76.4227640571818,27.0233220902657,16.1995753950398));
#255928=CARTESIAN_POINT('Ctrl Pts',(76.4028721167673,26.9952807487557,16.2077603480722));
#255929=CARTESIAN_POINT('Ctrl Pts',(76.3898418244125,26.9763750260929,16.2130348003402));
#255930=CARTESIAN_POINT('Ctrl Pts',(76.3515584858927,26.919185257365,16.2291569518415));
#255931=CARTESIAN_POINT('Ctrl Pts',(76.3271240812196,26.8804489710049,16.2401625701034));
#255932=CARTESIAN_POINT('Ctrl Pts',(76.2571329511827,26.7625715555466,16.2745485616773));
#255933=CARTESIAN_POINT('Ctrl Pts',(76.2151700755523,26.6822350597522,16.2990788049764));
#255934=CARTESIAN_POINT('Ctrl Pts',(76.1032564488141,26.4374959840272,16.3781741196505));
#255935=CARTESIAN_POINT('Ctrl Pts',(76.046615195867,26.2669884699004,16.4389027562941));
#255936=CARTESIAN_POINT('Ctrl Pts',(75.9710934258864,25.9287495116366,16.5778273625233));
#255937=CARTESIAN_POINT('Ctrl Pts',(75.9519151365713,25.7614405136926,16.6554073942778));
#255938=CARTESIAN_POINT('Ctrl Pts',(75.9448997961066,25.4371745331233,16.8391041287272));
#255939=CARTESIAN_POINT('Ctrl Pts',(75.9578405366692,25.2797179886133,16.945675869898));
#255940=CARTESIAN_POINT('Ctrl Pts',(75.9797434607283,25.1428889948603,17.0741173620445));
#255941=CARTESIAN_POINT('Origin',(78.4878132480312,25.5443686855277,17.0741173620445));
#255942=CARTESIAN_POINT('Ctrl Pts',(76.0725110230494,24.758292886385,17.0741173620445));
#255943=CARTESIAN_POINT('Ctrl Pts',(76.0107288628306,24.9481252017973,17.0741173620445));
#255944=CARTESIAN_POINT('Ctrl Pts',(75.9793621085789,25.1452786192766,17.0741173620445));
#255945=CARTESIAN_POINT('Ctrl Pts',(76.072511023285,24.7582928856611,17.3371780222032));
#255946=CARTESIAN_POINT('Ctrl Pts',(76.0107288897042,24.948125118734,17.3434041152839));
#255947=CARTESIAN_POINT('Ctrl Pts',(75.9793621491331,25.1452785074248,17.3508457847207));
#255948=CARTESIAN_POINT('Ctrl Pts',(76.0621788292375,24.7374486679144,17.5966189870109));
#255949=CARTESIAN_POINT('Ctrl Pts',(75.9996785825189,24.9271136619333,17.609018182416));
#255950=CARTESIAN_POINT('Ctrl Pts',(75.9676381104182,25.124098898332,17.6238224492231));
#255951=CARTESIAN_POINT('Ctrl Pts',(76.0421000528014,24.6969219387962,17.8525678740454));
#255952=CARTESIAN_POINT('Ctrl Pts',(75.9782191703494,24.8862836604198,17.8708938349953));
#255953=CARTESIAN_POINT('Ctrl Pts',(75.9448790163862,25.0829574281538,17.892855911921));
#255954=CARTESIAN_POINT('',(76.004557267664,24.9948448129998,17.2916572676519));
#255955=CARTESIAN_POINT('Ctrl Pts',(75.9797434607283,25.1428889948603,17.0741173620445));
#255956=CARTESIAN_POINT('Ctrl Pts',(75.9891380711871,25.0842002511886,17.1401458391886));
#255957=CARTESIAN_POINT('Ctrl Pts',(75.9984274744386,25.0341234730735,17.2120470870439));
#255958=CARTESIAN_POINT('Ctrl Pts',(76.0045572676606,24.9948448130136,17.2916572676646));
#255959=CARTESIAN_POINT('Ctrl Pts',(76.0045572676606,24.9948448130136,17.2916572676646));
#255960=CARTESIAN_POINT('Ctrl Pts',(76.0118494335674,24.9481178686905,17.3863636679988));
#255961=CARTESIAN_POINT('Ctrl Pts',(76.0187126955952,24.8998403102119,17.480310514724));
#255962=CARTESIAN_POINT('Ctrl Pts',(76.0250777702285,24.8500467273903,17.5734601499223));
#255963=CARTESIAN_POINT('Ctrl Pts',(76.0313841950981,24.8007119580207,17.6657514756104));
#255964=CARTESIAN_POINT('Ctrl Pts',(76.0372026794419,24.7498896381886,17.757259904234));
#255965=CARTESIAN_POINT('Ctrl Pts',(76.0424582864818,24.697644991789,17.8479876920609));
#255966=CARTESIAN_POINT('Origin',(25.5443686855278,78.4878132480313,12.3825));
#255967=CARTESIAN_POINT('',(25.1428889948602,75.9797434607284,17.0741173620444));
#255968=CARTESIAN_POINT('Origin',(25.5443686855278,78.4878132480313,17.0741173620444));
#255969=CARTESIAN_POINT('Ctrl Pts',(25.1428889948602,75.9797434607284,17.0741173620444));
#255970=CARTESIAN_POINT('Ctrl Pts',(25.1890962633322,75.9723468244998,17.0307425600543));
#255971=CARTESIAN_POINT('Ctrl Pts',(25.237115267786,75.9659732533751,16.9901866401575));
#255972=CARTESIAN_POINT('Ctrl Pts',(25.2866741011429,75.9609192056981,16.9519675478227));
#255973=CARTESIAN_POINT('Ctrl Pts',(25.3351466800541,75.9559759350792,16.9145861600129));
#255974=CARTESIAN_POINT('Ctrl Pts',(25.3850920216467,75.9522954968805,16.8794402829932));
#255975=CARTESIAN_POINT('Ctrl Pts',(25.4362249260049,75.9501164719612,16.8460788702546));
#255976=CARTESIAN_POINT('Ctrl Pts',(25.4862159183347,75.9479861095382,16.8134624924199));
#255977=CARTESIAN_POINT('Ctrl Pts',(25.5373416156507,75.9472911984361,16.782551766679));
#255978=CARTESIAN_POINT('Ctrl Pts',(25.5893110141084,75.9482108801197,16.7529251953268));
#255979=CARTESIAN_POINT('Ctrl Pts',(25.5996216874799,75.9483933439875,16.7470473150859));
#255980=CARTESIAN_POINT('Ctrl Pts',(25.6099655036169,75.9486392118567,16.741219981907));
#255981=CARTESIAN_POINT('Ctrl Pts',(25.6203400952605,75.948949654826,16.7354399041435));
#255982=CARTESIAN_POINT('Ctrl Pts',(25.6678229409182,75.9503705026149,16.7089854132329));
#255983=CARTESIAN_POINT('Ctrl Pts',(25.7161033957525,75.9531525557282,16.6835468572547));
#255984=CARTESIAN_POINT('Ctrl Pts',(25.7648841738468,75.9574036133256,16.6590804688499));
#255985=CARTESIAN_POINT('Ctrl Pts',(25.8132372046333,75.9616173943867,16.6348286205197));
#255986=CARTESIAN_POINT('Ctrl Pts',(25.8620813654547,75.9672746984588,16.6115319650911));
#255987=CARTESIAN_POINT('Ctrl Pts',(25.9111193560836,75.9744302796703,16.5891478764963));
#255988=CARTESIAN_POINT('Ctrl Pts',(25.959778995616,75.9815306522169,16.5669364916431));
#255989=CARTESIAN_POINT('Ctrl Pts',(26.0086290088535,75.990106319092,16.5456236461851));
#255990=CARTESIAN_POINT('Ctrl Pts',(26.0573782086215,76.0001594881171,16.5251676931019));
#255991=CARTESIAN_POINT('Ctrl Pts',(26.0882583186404,76.006527653482,16.5122098992355));
#255992=CARTESIAN_POINT('Ctrl Pts',(26.1190979844463,76.0134876389454,16.4995959394913));
#255993=CARTESIAN_POINT('Ctrl Pts',(26.1498243779411,76.0210292273833,16.4873152282084));
#255994=CARTESIAN_POINT('Ctrl Pts',(26.2179462859366,76.0377492955484,16.460088294326));
#255995=CARTESIAN_POINT('Ctrl Pts',(26.2860317992677,76.05745616022,16.434286890481));
#255996=CARTESIAN_POINT('Ctrl Pts',(26.3537219308291,76.0802112617552,16.4098106473495));
#255997=CARTESIAN_POINT('Ctrl Pts',(26.4210710446877,76.1028517248303,16.3854577136577));
#255998=CARTESIAN_POINT('Ctrl Pts',(26.4880282443252,76.1285099018942,16.3624166221964));
#255999=CARTESIAN_POINT('Ctrl Pts',(26.5542307553386,76.1571956045819,16.3405885129709));
#256000=CARTESIAN_POINT('Ctrl Pts',(26.5947970537208,76.1747730764439,16.3272131050233));
#256001=CARTESIAN_POINT('Ctrl Pts',(26.635079834817,76.1934863070448,16.3142931424312));
#256002=CARTESIAN_POINT('Ctrl Pts',(26.6749951887968,76.2133278754457,16.3018058798074));
#256003=CARTESIAN_POINT('Ctrl Pts',(26.7414052730119,76.2463397392294,16.2810299106682));
#256004=CARTESIAN_POINT('Ctrl Pts',(26.8065749011807,76.2823577026598,16.2615818620414));
#256005=CARTESIAN_POINT('Ctrl Pts',(26.8703934402706,76.3214203128024,16.2431559979649));
#256006=CARTESIAN_POINT('Ctrl Pts',(26.8885104502997,76.332509530917,16.2379252050161));
#256007=CARTESIAN_POINT('Ctrl Pts',(26.9065183420882,76.3438443339862,16.2327767895745));
#256008=CARTESIAN_POINT('Ctrl Pts',(26.9244139858097,76.3554260952914,16.2277037569976));
#256009=CARTESIAN_POINT('Ctrl Pts',(26.9473795640663,76.3702890334313,16.221193506321));
#256010=CARTESIAN_POINT('Ctrl Pts',(26.9702988091955,76.3856535929662,16.2155241412993));
#256011=CARTESIAN_POINT('Ctrl Pts',(26.9928245401832,76.4012908692597,16.2092079610164));
#256012=CARTESIAN_POINT('Ctrl Pts',(27.0099909644421,76.4132077353208,16.2043945220878));
#256013=CARTESIAN_POINT('Ctrl Pts',(27.0269293937092,76.4252820333712,16.1992054342301));
#256014=CARTESIAN_POINT('Ctrl Pts',(27.0434980077852,76.4373959063303,16.1929822540028));
#256015=CARTESIAN_POINT('Ctrl Pts',(27.0482867453246,76.4408971139703,16.1911836016452));
#256016=CARTESIAN_POINT('Ctrl Pts',(27.0532391486265,76.4445482450862,16.1893664854193));
#256017=CARTESIAN_POINT('Ctrl Pts',(27.0570025619865,76.4473381181192,16.1852582407548));
#256018=CARTESIAN_POINT('Ctrl Pts',(27.0603326521677,76.4498067623805,16.1816230234904));
#256019=CARTESIAN_POINT('Ctrl Pts',(27.0611677349713,76.4504320929469,16.1755676007557));
#256020=CARTESIAN_POINT('Ctrl Pts',(27.0602432495844,76.4497444793078,16.1701033997385));
#256021=CARTESIAN_POINT('Ctrl Pts',(27.0601229522577,76.4496550045754,16.1693923784672));
#256022=CARTESIAN_POINT('Ctrl Pts',(27.0599728200255,76.4495433549851,16.1686913678449));
#256023=CARTESIAN_POINT('Ctrl Pts',(27.0597944416051,76.4494107417,16.1680070028595));
#256024=CARTESIAN_POINT('Ctrl Pts',(27.0572678114964,76.447532349022,16.1583133573325));
#256025=CARTESIAN_POINT('Ctrl Pts',(27.0523400392588,76.443879587196,16.1500702655813));
#256026=CARTESIAN_POINT('Ctrl Pts',(27.0470895061932,76.4400266050583,16.142237266683));
#256027=CARTESIAN_POINT('Ctrl Pts',(27.0459012525009,76.4391546325948,16.1404645724163));
#256028=CARTESIAN_POINT('Ctrl Pts',(27.0446965952318,76.438272235762,16.1387128817501));
#256029=CARTESIAN_POINT('Ctrl Pts',(27.0434998998453,76.4373972896807,16.1369701348014));
#256030=CARTESIAN_POINT('Ctrl Pts',(27.0334981288334,76.4300846431606,16.1224045602109));
#256031=CARTESIAN_POINT('Ctrl Pts',(27.0225381835945,76.4221888169328,16.1088060042622));
#256032=CARTESIAN_POINT('Ctrl Pts',(27.0113044494441,76.4142415794981,16.0954740612688));
#256033=CARTESIAN_POINT('Ctrl Pts',(27.007971666702,76.4118838224589,16.0915187896795));
#256034=CARTESIAN_POINT('Ctrl Pts',(27.0046149921553,76.4095212641207,16.0875869845174));
#256035=CARTESIAN_POINT('Ctrl Pts',(27.0012528338594,76.4071670555372,16.0836603564334));
#256036=CARTESIAN_POINT('Ctrl Pts',(25.1452786192766,75.979362108579,17.0741173620444));
#256037=CARTESIAN_POINT('Ctrl Pts',(24.9481252017973,76.0107288628306,17.0741173620444));
#256038=CARTESIAN_POINT('Ctrl Pts',(24.758292886385,76.0725110230494,17.0741173620444));
#256039=CARTESIAN_POINT('Ctrl Pts',(25.1452785074235,75.9793621491333,17.3508457847216));
#256040=CARTESIAN_POINT('Ctrl Pts',(24.9481251187328,76.0107288897045,17.3434041152847));
#256041=CARTESIAN_POINT('Ctrl Pts',(24.7582928856604,76.0725110232853,17.3371780222039));
#256042=CARTESIAN_POINT('Ctrl Pts',(25.1240988983279,75.9676381104205,17.6238224492216));
#256043=CARTESIAN_POINT('Ctrl Pts',(24.9271136619295,75.9996785825208,17.6090181824146));
#256044=CARTESIAN_POINT('Ctrl Pts',(24.737448667911,76.0621788292387,17.5966189870096));
#256045=CARTESIAN_POINT('Ctrl Pts',(25.0829574281538,75.9448790163861,17.8928559119209));
#256046=CARTESIAN_POINT('Ctrl Pts',(24.8862836604198,75.9782191703494,17.8708938349951));
#256047=CARTESIAN_POINT('Ctrl Pts',(24.6969219387962,76.0421000528014,17.8525678740453));
#256048=CARTESIAN_POINT('',(24.994844812995,76.0045572676648,17.2916572676617));
#256049=CARTESIAN_POINT('Ctrl Pts',(24.6976449917882,76.0424582864821,17.8479876920601));
#256050=CARTESIAN_POINT('Ctrl Pts',(24.7503755555246,76.0371537980617,17.7564160626317));
#256051=CARTESIAN_POINT('Ctrl Pts',(24.8016571681256,76.0312759356771,17.6640491390589));
#256052=CARTESIAN_POINT('Ctrl Pts',(24.8514229012875,76.0249016788522,17.5708847963288));
#256053=CARTESIAN_POINT('Ctrl Pts',(24.9007299986423,76.0185861665134,17.478579046466));
#256054=CARTESIAN_POINT('Ctrl Pts',(24.9485484624186,76.0117822354893,17.3854909384809));
#256055=CARTESIAN_POINT('Ctrl Pts',(24.9948448130087,76.0045572676614,17.2916572676743));
#256056=CARTESIAN_POINT('Ctrl Pts',(24.9948448130087,76.0045572676614,17.2916572676743));
#256057=CARTESIAN_POINT('Ctrl Pts',(25.0341234730694,75.9984274744394,17.2120470870498));
#256058=CARTESIAN_POINT('Ctrl Pts',(25.0842002511861,75.9891380711875,17.1401458391912));
#256059=CARTESIAN_POINT('Ctrl Pts',(25.1428889948602,75.9797434607284,17.0741173620444));
#256060=CARTESIAN_POINT('Origin',(-25.5443686855278,78.4878132480313,12.3825));
#256061=CARTESIAN_POINT('',(-25.1428889948604,75.9797434607283,17.0741173620445));
#256062=CARTESIAN_POINT('Ctrl Pts',(-27.0012528338594,76.4071670555372,
16.0836576911637));
#256063=CARTESIAN_POINT('Ctrl Pts',(-27.0125669200987,76.4150892640099,
16.0968733253419));
#256064=CARTESIAN_POINT('Ctrl Pts',(-27.0238163445857,76.4231093010226,
16.1101516770522));
#256065=CARTESIAN_POINT('Ctrl Pts',(-27.0343062910082,76.4307070447021,
16.1241706807122));
#256066=CARTESIAN_POINT('Ctrl Pts',(-27.037395957053,76.4329448531444,16.1282997808854));
#256067=CARTESIAN_POINT('Ctrl Pts',(-27.0404199473186,76.4351457409871,
16.1324931336593));
#256068=CARTESIAN_POINT('Ctrl Pts',(-27.0433610093266,76.4372957491563,
16.1367680612116));
#256069=CARTESIAN_POINT('Ctrl Pts',(-27.0486625246032,76.4411713223755,
16.1444739829716));
#256070=CARTESIAN_POINT('Ctrl Pts',(-27.0541111004947,76.4451930178066,
16.1523581129506));
#256071=CARTESIAN_POINT('Ctrl Pts',(-27.0576635452245,76.4478282805339,
16.1614817339872));
#256072=CARTESIAN_POINT('Ctrl Pts',(-27.0584419922995,76.4484057455524,
16.1634809927086));
#256073=CARTESIAN_POINT('Ctrl Pts',(-27.0591295239125,76.448916459005,16.1655397692371));
#256074=CARTESIAN_POINT('Ctrl Pts',(-27.0597047915435,76.449344095504,16.1676692305701));
#256075=CARTESIAN_POINT('Ctrl Pts',(-27.0611286869983,76.4504025761738,
16.172940047404));
#256076=CARTESIAN_POINT('Ctrl Pts',(-27.0609586565846,76.4502741691125,
16.1792319847823));
#256077=CARTESIAN_POINT('Ctrl Pts',(-27.0583397186354,76.4483300510152,
16.1834945126965));
#256078=CARTESIAN_POINT('Ctrl Pts',(-27.0580153514339,76.4480892632764,
16.1840224458809));
#256079=CARTESIAN_POINT('Ctrl Pts',(-27.0576533777842,76.4478206770397,
16.184519248061));
#256080=CARTESIAN_POINT('Ctrl Pts',(-27.0572521328189,76.4475231522575,
16.1849791234756));
#256081=CARTESIAN_POINT('Ctrl Pts',(-27.0536112395122,76.4448234149856,
16.1891520289663));
#256082=CARTESIAN_POINT('Ctrl Pts',(-27.0486162619737,76.4411392704989,
16.1910424129933));
#256083=CARTESIAN_POINT('Ctrl Pts',(-27.0438314224983,76.4376397186838,
16.1928564416501));
#256084=CARTESIAN_POINT('Ctrl Pts',(-27.0219957234643,76.4216694524754,
16.2011347933047));
#256085=CARTESIAN_POINT('Ctrl Pts',(-26.9995297607086,76.4057789844929,
16.207534966411));
#256086=CARTESIAN_POINT('Ctrl Pts',(-26.9767570197927,76.3902280507481,
16.2136304740377));
#256087=CARTESIAN_POINT('Ctrl Pts',(-26.9596083789282,76.3785176739039,
16.2182205965689));
#256088=CARTESIAN_POINT('Ctrl Pts',(-26.9422864664073,76.3669990382474,
16.2226379555783));
#256089=CARTESIAN_POINT('Ctrl Pts',(-26.924940664306,76.355767045105,16.2275544648554));
#256090=CARTESIAN_POINT('Ctrl Pts',(-26.8616513977226,76.3147851058381,
16.2454932297784));
#256091=CARTESIAN_POINT('Ctrl Pts',(-26.7969330614058,76.2768724896713,
16.264380542811));
#256092=CARTESIAN_POINT('Ctrl Pts',(-26.7309055212341,76.2419881574438,
16.2845312331379));
#256093=CARTESIAN_POINT('Ctrl Pts',(-26.7126781361404,76.2323580825449,
16.2900939784944));
#256094=CARTESIAN_POINT('Ctrl Pts',(-26.6943507497403,76.2229589907508,
16.2957530028506));
#256095=CARTESIAN_POINT('Ctrl Pts',(-26.6759253951148,76.2137905100208,
16.3015149294807));
#256096=CARTESIAN_POINT('Ctrl Pts',(-26.6064313423364,76.1792101778265,
16.3232469200705));
#256097=CARTESIAN_POINT('Ctrl Pts',(-26.5358861300337,76.1480850300989,
16.3462666779649));
#256098=CARTESIAN_POINT('Ctrl Pts',(-26.4646896515466,76.1204076386128,
16.3707095327059));
#256099=CARTESIAN_POINT('Ctrl Pts',(-26.3929595547121,76.0925228047893,
16.3953355868976));
#256100=CARTESIAN_POINT('Ctrl Pts',(-26.320568851033,76.0681374435539,16.42140615013));
#256101=CARTESIAN_POINT('Ctrl Pts',(-26.2479119279717,76.0471930592244,
16.4490596176973));
#256102=CARTESIAN_POINT('Ctrl Pts',(-26.2159174278757,76.0379701926591,
16.4612368312849));
#256103=CARTESIAN_POINT('Ctrl Pts',(-26.1838710753048,76.0294139153945,
16.4737209833412));
#256104=CARTESIAN_POINT('Ctrl Pts',(-26.151805321039,76.0215162801381,16.4865238911129));
#256105=CARTESIAN_POINT('Ctrl Pts',(-26.1024355268121,76.0093567461925,
16.5062357905105));
#256106=CARTESIAN_POINT('Ctrl Pts',(-26.0527788404423,75.9987033865243,
16.5268004133223));
#256107=CARTESIAN_POINT('Ctrl Pts',(-26.0031235801223,75.9895850865765,
16.548271859116));
#256108=CARTESIAN_POINT('Ctrl Pts',(-25.9532562257184,75.9804278393458,
16.5698350165754));
#256109=CARTESIAN_POINT('Ctrl Pts',(-25.9033908054762,75.9728187925742,
16.5923127602445));
#256110=CARTESIAN_POINT('Ctrl Pts',(-25.8538229234789,75.966734495867,16.6157598858881));
#256111=CARTESIAN_POINT('Ctrl Pts',(-25.8036709928875,75.9605785090897,
16.6394832843966));
#256112=CARTESIAN_POINT('Ctrl Pts',(-25.753824153542,75.9559833524274,16.664199043537));
#256113=CARTESIAN_POINT('Ctrl Pts',(-25.7045846543213,75.9528712677596,
16.6899639189295));
#256114=CARTESIAN_POINT('Ctrl Pts',(-25.6770558328495,75.9511313633215,
16.70436854664));
#256115=CARTESIAN_POINT('Ctrl Pts',(-25.6497167328468,75.949854070861,16.7191010971392));
#256116=CARTESIAN_POINT('Ctrl Pts',(-25.6226187903523,75.9490188646487,
16.7341714885812));
#256117=CARTESIAN_POINT('Ctrl Pts',(-25.5764663678453,75.9475963658742,
16.7598389381788));
#256118=CARTESIAN_POINT('Ctrl Pts',(-25.5307625058469,75.9474517866765,
16.7865659951667));
#256119=CARTESIAN_POINT('Ctrl Pts',(-25.4858135554159,75.9484882793166,
16.8145610365622));
#256120=CARTESIAN_POINT('Ctrl Pts',(-25.4402080117497,75.9495399125562,
16.842965016423));
#256121=CARTESIAN_POINT('Ctrl Pts',(-25.3953800360767,75.9518071268027,
16.8726742954997));
#256122=CARTESIAN_POINT('Ctrl Pts',(-25.351635516157,75.9551360231516,16.9039065164716));
#256123=CARTESIAN_POINT('Ctrl Pts',(-25.3063675024672,75.9585808552304,
16.936226464413));
#256124=CARTESIAN_POINT('Ctrl Pts',(-25.2622601838204,75.9631623245209,
16.970177280694));
#256125=CARTESIAN_POINT('Ctrl Pts',(-25.2196304518514,75.9686576197326,
17.0060001487159));
#256126=CARTESIAN_POINT('Ctrl Pts',(-25.193471268367,75.9720297365418,17.0279823882055));
#256127=CARTESIAN_POINT('Ctrl Pts',(-25.1678679991337,75.9757449424417,
17.0506695496094));
#256128=CARTESIAN_POINT('Ctrl Pts',(-25.1428889948604,75.9797434607283,
17.0741173620445));
#256129=CARTESIAN_POINT('Origin',(-25.5443686855278,78.4878132480312,17.0741173620445));
#256130=CARTESIAN_POINT('Ctrl Pts',(-24.758292886385,76.0725110230494,17.0741173620445));
#256131=CARTESIAN_POINT('Ctrl Pts',(-24.9481252017973,76.0107288628305,
17.0741173620445));
#256132=CARTESIAN_POINT('Ctrl Pts',(-25.1452786192768,75.9793621085789,
17.0741173620445));
#256133=CARTESIAN_POINT('Ctrl Pts',(-24.7582928856577,76.0725110232862,
17.3371780222047));
#256134=CARTESIAN_POINT('Ctrl Pts',(-24.9481251187305,76.0107288897052,
17.3434041152857));
#256135=CARTESIAN_POINT('Ctrl Pts',(-25.1452785074214,75.9793621491338,
17.3508457847227));
#256136=CARTESIAN_POINT('Ctrl Pts',(-24.7374486679099,76.0621788292392,
17.5966189870087));
#256137=CARTESIAN_POINT('Ctrl Pts',(-24.9271136619281,75.9996785825204,
17.6090181824136));
#256138=CARTESIAN_POINT('Ctrl Pts',(-25.1240988983264,75.9676381104195,
17.6238224492204));
#256139=CARTESIAN_POINT('Ctrl Pts',(-24.6969219387962,76.0421000528014,
17.8525678740454));
#256140=CARTESIAN_POINT('Ctrl Pts',(-24.8862836604199,75.9782191703494,
17.8708938349952));
#256141=CARTESIAN_POINT('Ctrl Pts',(-25.0829574281539,75.9448790163861,
17.892855911921));
#256142=CARTESIAN_POINT('',(-24.9948448129999,76.004557267664,17.2916572676519));
#256143=CARTESIAN_POINT('Ctrl Pts',(-25.1428889948604,75.9797434607283,
17.0741173620445));
#256144=CARTESIAN_POINT('Ctrl Pts',(-25.0842002511887,75.9891380711871,
17.1401458391885));
#256145=CARTESIAN_POINT('Ctrl Pts',(-25.0341234730736,75.9984274744386,
17.2120470870439));
#256146=CARTESIAN_POINT('Ctrl Pts',(-24.9948448130136,76.0045572676606,
17.2916572676646));
#256147=CARTESIAN_POINT('Ctrl Pts',(-24.9948448130136,76.0045572676606,
17.2916572676646));
#256148=CARTESIAN_POINT('Ctrl Pts',(-24.94811785539,76.0118494356433,17.3863636949506));
#256149=CARTESIAN_POINT('Ctrl Pts',(-24.8998402827123,76.018712699508,17.4803105681817));
#256150=CARTESIAN_POINT('Ctrl Pts',(-24.850046684856,76.0250777756705,17.5734602294373));
#256151=CARTESIAN_POINT('Ctrl Pts',(-24.8007119288024,76.0313841984489,
17.6657515281657));
#256152=CARTESIAN_POINT('Ctrl Pts',(-24.7498896231699,76.0372026809562,
17.7572599302886));
#256153=CARTESIAN_POINT('Ctrl Pts',(-24.697644991789,76.0424582864817,17.8479876920609));
#256154=CARTESIAN_POINT('Ctrl Pts',(-76.0725110230494,-24.758292886385,
17.0741173620445));
#256155=CARTESIAN_POINT('Ctrl Pts',(-76.0107288628305,-24.9481252017973,
17.0741173620445));
#256156=CARTESIAN_POINT('Ctrl Pts',(-75.9793621085789,-25.1452786192767,
17.0741173620445));
#256157=CARTESIAN_POINT('Ctrl Pts',(-76.0725110232863,-24.7582928856572,
17.3371780222034));
#256158=CARTESIAN_POINT('Ctrl Pts',(-76.0107288897045,-24.9481251187298,
17.3434041152839));
#256159=CARTESIAN_POINT('Ctrl Pts',(-75.9793621491325,-25.1452785074205,
17.3508457847206));
#256160=CARTESIAN_POINT('Ctrl Pts',(-76.0621788292369,-24.7374486679163,
17.5966189870106));
#256161=CARTESIAN_POINT('Ctrl Pts',(-75.99967858252,-24.9271136619357,17.609018182416));
#256162=CARTESIAN_POINT('Ctrl Pts',(-75.9676381104206,-25.124098898335,
17.6238224492233));
#256163=CARTESIAN_POINT('Ctrl Pts',(-76.0421000528014,-24.6969219387961,
17.8525678740454));
#256164=CARTESIAN_POINT('Ctrl Pts',(-75.9782191703494,-24.8862836604199,
17.8708938349953));
#256165=CARTESIAN_POINT('Ctrl Pts',(-75.9448790163861,-25.0829574281539,
17.892855911921));
#256166=CARTESIAN_POINT('',(-76.004557267664,-24.9948448129999,17.2916572676518));
#256167=CARTESIAN_POINT('Ctrl Pts',(-75.9797434607283,-25.1428889948604,
17.0741173620445));
#256168=CARTESIAN_POINT('Ctrl Pts',(-75.989138071187,-25.0842002511887,
17.1401458391886));
#256169=CARTESIAN_POINT('Ctrl Pts',(-75.9984274744386,-25.0341234730736,
17.2120470870439));
#256170=CARTESIAN_POINT('Ctrl Pts',(-76.0045572676606,-24.9948448130136,
17.2916572676645));
#256171=CARTESIAN_POINT('Ctrl Pts',(-76.0045572676606,-24.9948448130136,
17.2916572676645));
#256172=CARTESIAN_POINT('Ctrl Pts',(-76.0118494398941,-24.9481178281451,
17.3863637502011));
#256173=CARTESIAN_POINT('Ctrl Pts',(-76.0187127075221,-24.8998402263703,
17.4803106777579));
#256174=CARTESIAN_POINT('Ctrl Pts',(-76.0250777868188,-24.8500465976989,
17.5734603924151));
#256175=CARTESIAN_POINT('Ctrl Pts',(-76.0313842053114,-24.8007118689344,
17.6657516358879));
#256176=CARTESIAN_POINT('Ctrl Pts',(-76.0372026840567,-24.7498895923968,
17.7572599836914));
#256177=CARTESIAN_POINT('Ctrl Pts',(-76.0424582864817,-24.697644991789,
17.8479876920609));
#256178=CARTESIAN_POINT('Ctrl Pts',(-75.9793621085789,25.1452786192766,
17.0741173620445));
#256179=CARTESIAN_POINT('Ctrl Pts',(-76.0107288628305,24.9481252017972,
17.0741173620445));
#256180=CARTESIAN_POINT('Ctrl Pts',(-76.0725110230494,24.758292886385,17.0741173620445));
#256181=CARTESIAN_POINT('Ctrl Pts',(-75.9793621491325,25.1452785074204,
17.3508457847207));
#256182=CARTESIAN_POINT('Ctrl Pts',(-76.0107288897045,24.9481251187298,
17.3434041152841));
#256183=CARTESIAN_POINT('Ctrl Pts',(-76.0725110232863,24.7582928856572,
17.3371780222036));
#256184=CARTESIAN_POINT('Ctrl Pts',(-75.9676381104235,25.1240988983324,
17.6238224492231));
#256185=CARTESIAN_POINT('Ctrl Pts',(-75.9996785825219,24.9271136619338,
17.6090181824158));
#256186=CARTESIAN_POINT('Ctrl Pts',(-76.0621788292373,24.7374486679152,
17.5966189870103));
#256187=CARTESIAN_POINT('Ctrl Pts',(-75.9448790163861,25.0829574281538,
17.892855911921));
#256188=CARTESIAN_POINT('Ctrl Pts',(-75.9782191703494,24.8862836604198,
17.8708938349952));
#256189=CARTESIAN_POINT('Ctrl Pts',(-76.0421000528014,24.6969219387961,
17.8525678740454));
#256190=CARTESIAN_POINT('',(-76.0045572676648,24.9948448129949,17.2916572676618));
#256191=CARTESIAN_POINT('Ctrl Pts',(-76.0424582864821,24.6976449917881,
17.8479876920602));
#256192=CARTESIAN_POINT('Ctrl Pts',(-76.0371538035502,24.7503755009267,
17.7564161574767));
#256193=CARTESIAN_POINT('Ctrl Pts',(-76.031275947831,24.8016570619565,17.6640493304302));
#256194=CARTESIAN_POINT('Ctrl Pts',(-76.0249016986412,24.8514227467087,
17.5708850858271));
#256195=CARTESIAN_POINT('Ctrl Pts',(-76.0185861807249,24.9007298987056,
17.4785792411033));
#256196=CARTESIAN_POINT('Ctrl Pts',(-76.0117822430429,24.9485484140197,
17.3854910365594));
#256197=CARTESIAN_POINT('Ctrl Pts',(-76.0045572676614,24.9948448130087,
17.2916572676745));
#256198=CARTESIAN_POINT('Ctrl Pts',(-76.0045572676613,24.9948448130087,
17.2916572676745));
#256199=CARTESIAN_POINT('Ctrl Pts',(-75.9984274744394,25.0341234730694,
17.21204708705));
#256200=CARTESIAN_POINT('Ctrl Pts',(-75.9891380711875,25.084200251186,17.1401458391913));
#256201=CARTESIAN_POINT('Ctrl Pts',(-75.9797434607283,25.1428889948603,
17.0741173620445));
#256202=CARTESIAN_POINT('Ctrl Pts',(25.9085897226107,-77.9676516999078,
12.3825));
#256203=CARTESIAN_POINT('Ctrl Pts',(25.6490890766241,-77.7859473914177,
12.3825));
#256204=CARTESIAN_POINT('Ctrl Pts',(25.3478497357421,-77.8839876917858,
12.3825));
#256205=CARTESIAN_POINT('Ctrl Pts',(27.0012528338594,-76.4071670555372,
12.3825));
#256206=CARTESIAN_POINT('Ctrl Pts',(25.9632502499131,-75.6803498215769,
12.3825));
#256207=CARTESIAN_POINT('Ctrl Pts',(24.758292886385,-76.0725110230494,12.3825));
#256208=CARTESIAN_POINT('Ctrl Pts',(27.0012528338594,-76.4071670555372,
14.2875));
#256209=CARTESIAN_POINT('Ctrl Pts',(25.9632502499131,-75.6803498215769,
14.2875));
#256210=CARTESIAN_POINT('Ctrl Pts',(24.758292886385,-76.0725110230494,14.2875));
#256211=CARTESIAN_POINT('Origin',(25.3478497357421,-77.8839876917858,14.2875));
#256212=CARTESIAN_POINT('Origin',(25.9085897226107,-77.9676516999077,14.2875));
#256213=CARTESIAN_POINT('Origin',(74.5679259799751,-112.039285751595,14.2875));
#256214=CARTESIAN_POINT('Origin',(74.5679259799751,-112.039285751595,14.2875));
#256215=CARTESIAN_POINT('Origin',(0.,0.,14.2875));
#256216=CARTESIAN_POINT('Origin',(-25.3478497357421,-77.8839876917858,14.2875));
#256217=CARTESIAN_POINT('Origin',(90.,-90.,14.2875));
#256218=CARTESIAN_POINT('Origin',(76.1978262581577,-113.095,14.2875));
#256219=CARTESIAN_POINT('Ctrl Pts',(-25.3478497357421,-77.8839876917858,
12.3825));
#256220=CARTESIAN_POINT('Ctrl Pts',(-25.6490890766241,-77.7859473914177,
12.3825));
#256221=CARTESIAN_POINT('Ctrl Pts',(-25.9085897226107,-77.9676516999077,
12.3825));
#256222=CARTESIAN_POINT('Ctrl Pts',(-24.7582928863851,-76.0725110230494,
12.3825));
#256223=CARTESIAN_POINT('Ctrl Pts',(-25.9632502499132,-75.6803498215769,
12.3825));
#256224=CARTESIAN_POINT('Ctrl Pts',(-27.0012528338595,-76.4071670555372,
12.3825));
#256225=CARTESIAN_POINT('Ctrl Pts',(-24.7582928863851,-76.0725110230494,
14.2875));
#256226=CARTESIAN_POINT('Ctrl Pts',(-25.9632502499132,-75.6803498215769,
14.2875));
#256227=CARTESIAN_POINT('Ctrl Pts',(-27.0012528338595,-76.4071670555372,
14.2875));
#256228=CARTESIAN_POINT('Origin',(-25.9085897226107,-77.9676516999077,14.2875));
#256229=CARTESIAN_POINT('Ctrl Pts',(77.1750847966528,-111.45976584278,14.2875));
#256230=CARTESIAN_POINT('Ctrl Pts',(77.1750847966528,-111.45976584278,12.3825));
#256231=CARTESIAN_POINT('Ctrl Pts',(76.1978262581577,-113.095,12.3825));
#256232=CARTESIAN_POINT('Ctrl Pts',(77.6808356682961,-111.762015741049,
14.2874999966875));
#256233=CARTESIAN_POINT('Ctrl Pts',(77.5941846099562,-111.71023081209,12.5172751948194));
#256234=CARTESIAN_POINT('Ctrl Pts',(76.7421246518763,-113.257643450726,
12.3825));
#256235=CARTESIAN_POINT('Ctrl Pts',(78.1909142917095,-112.04266475307,14.2466073426296));
#256236=CARTESIAN_POINT('Ctrl Pts',(78.0590963418289,-111.971409284925,
12.6053517687442));
#256237=CARTESIAN_POINT('Ctrl Pts',(77.2910619607791,-113.408657903693,
12.3620536717506));
#256238=CARTESIAN_POINT('Ctrl Pts',(79.2214453413673,-112.564492774109,
14.108780097621));
#256239=CARTESIAN_POINT('Ctrl Pts',(79.0242905953313,-112.468920289919,
12.6961322557778));
#256240=CARTESIAN_POINT('Ctrl Pts',(78.4001194763382,-113.689453561681,
12.2931400483747));
#256241=CARTESIAN_POINT('Ctrl Pts',(79.7419020126347,-112.805653119423,
14.0115316944756));
#256242=CARTESIAN_POINT('Ctrl Pts',(79.526944890976,-112.708892347893,12.703865475829));
#256243=CARTESIAN_POINT('Ctrl Pts',(78.9602349460145,-113.819221943657,
12.244515847471));
#256244=CARTESIAN_POINT('Ctrl Pts',(80.7943836707349,-113.250441211302,
13.7750080898747));
#256245=CARTESIAN_POINT('Ctrl Pts',(80.5569292865739,-113.155754679235,
12.6577917414232));
#256246=CARTESIAN_POINT('Ctrl Pts',(80.0929157064278,-114.058562415705,
12.1262540447041));
#256247=CARTESIAN_POINT('Ctrl Pts',(81.3276580610674,-113.45448134688,13.6352465336299));
#256248=CARTESIAN_POINT('Ctrl Pts',(81.0885336408363,-113.366292203084,
12.6062543646742));
#256249=CARTESIAN_POINT('Ctrl Pts',(80.666825605363,-114.168356412835,12.0563732669971));
#256250=CARTESIAN_POINT('Ctrl Pts',(82.4011339813139,-113.823925897865,
13.3246442856472));
#256251=CARTESIAN_POINT('Ctrl Pts',(82.1657264091691,-113.748604057329,
12.4584071352196));
#256252=CARTESIAN_POINT('Ctrl Pts',(81.8221003906478,-114.367154525562,
11.9010721426414));
#256253=CARTESIAN_POINT('Ctrl Pts',(82.9379109315738,-113.98827163761,13.1548625963702));
#256254=CARTESIAN_POINT('Ctrl Pts',(82.7112571397903,-113.921920427821,
12.3636877604077));
#256255=CARTESIAN_POINT('Ctrl Pts',(82.3997797445818,-114.455588968268,
11.8161812982783));
#256256=CARTESIAN_POINT('Ctrl Pts',(84.5510793506422,-114.424380779002,
12.6139948970955));
#256257=CARTESIAN_POINT('Ctrl Pts',(84.3341564328195,-114.375512716331,
12.0384183635703));
#256258=CARTESIAN_POINT('Ctrl Pts',(84.1358715971169,-114.690259297042,
11.5457474483613));
#256259=CARTESIAN_POINT('Ctrl Pts',(85.6303497382816,-114.639636039159,
12.2118226911433));
#256260=CARTESIAN_POINT('Ctrl Pts',(85.4594058856995,-114.611553326324,
11.7583160303656));
#256261=CARTESIAN_POINT('Ctrl Pts',(85.2973823883387,-114.806088152743,
11.3446613455991));
#256262=CARTESIAN_POINT('Ctrl Pts',(87.8072663979372,-114.927844409462,
11.3656205182415));
#256263=CARTESIAN_POINT('Ctrl Pts',(87.7104675830927,-114.920352198467,
11.1472581448906));
#256264=CARTESIAN_POINT('Ctrl Pts',(87.6401800974599,-114.96117307666,10.9215602590933));
#256265=CARTESIAN_POINT('Ctrl Pts',(88.9061071730694,-115.,10.9205098031028));
#256266=CARTESIAN_POINT('Ctrl Pts',(88.8644746746685,-115.,10.8097442389035));
#256267=CARTESIAN_POINT('Ctrl Pts',(88.8227423399098,-115.,10.6990068206853));
#256268=CARTESIAN_POINT('Ctrl Pts',(90.,-115.,10.4775));
#256269=CARTESIAN_POINT('Ctrl Pts',(90.,-115.,10.4775));
#256270=CARTESIAN_POINT('Ctrl Pts',(90.,-115.,10.4775));
#256271=CARTESIAN_POINT('Ctrl Pts',(90.,-115.,10.4775));
#256272=CARTESIAN_POINT('Ctrl Pts',(89.583543836463,-115.,10.5558582760742));
#256273=CARTESIAN_POINT('Ctrl Pts',(89.16698283296,-114.995145444742,10.6342451251674));
#256274=CARTESIAN_POINT('Ctrl Pts',(88.7504746564855,-114.985453756063,
10.7122315109298));
#256275=CARTESIAN_POINT('Ctrl Pts',(88.3493129355897,-114.976119162583,
10.7873444486486));
#256276=CARTESIAN_POINT('Ctrl Pts',(87.9481990723853,-114.962297205616,
10.8620867505664));
#256277=CARTESIAN_POINT('Ctrl Pts',(87.5472762325185,-114.943957243982,
10.9360757308279));
#256278=CARTESIAN_POINT('Ctrl Pts',(87.2069586549715,-114.928389631727,
10.9988802109521));
#256279=CARTESIAN_POINT('Ctrl Pts',(86.8667783863514,-114.909565993822,
11.0611422131555));
#256280=CARTESIAN_POINT('Ctrl Pts',(86.5268333104866,-114.887440575962,
11.1226211406014));
#256281=CARTESIAN_POINT('Ctrl Pts',(86.5074818406287,-114.886181080275,
11.1261208459827));
#256282=CARTESIAN_POINT('Ctrl Pts',(86.4881313431668,-114.884910894891,
11.1296179650593));
#256283=CARTESIAN_POINT('Ctrl Pts',(86.4687819131639,-114.883630015072,
11.1331124382524));
#256284=CARTESIAN_POINT('Ctrl Pts',(85.900400763887,-114.846004723596,11.2357610790286));
#256285=CARTESIAN_POINT('Ctrl Pts',(85.3326432827616,-114.799248326424,
11.3362547894292));
#256286=CARTESIAN_POINT('Ctrl Pts',(84.7653562148502,-114.742990120853,
11.4332724000528));
#256287=CARTESIAN_POINT('Ctrl Pts',(84.1980691469388,-114.686731915282,
11.5302900106764));
#256288=CARTESIAN_POINT('Ctrl Pts',(83.6312517469126,-114.62097164889,11.6238302836077));
#256289=CARTESIAN_POINT('Ctrl Pts',(83.0647232345981,-114.545392304676,
11.7125671552065));
#256290=CARTESIAN_POINT('Ctrl Pts',(83.0359704727094,-114.541556460864,
11.7170707769738));
#256291=CARTESIAN_POINT('Ctrl Pts',(83.0072223038157,-114.537695858892,
11.7215614148314));
#256292=CARTESIAN_POINT('Ctrl Pts',(82.978478279317,-114.533810424182,11.7260389714724));
#256293=CARTESIAN_POINT('Ctrl Pts',(82.6542583520787,-114.489984433187,
11.7765438368714));
#256294=CARTESIAN_POINT('Ctrl Pts',(82.330561948864,-114.442984724948,11.8253691505401));
#256295=CARTESIAN_POINT('Ctrl Pts',(82.0067026925525,-114.392600666908,
11.8722415248233));
#256296=CARTESIAN_POINT('Ctrl Pts',(81.7528333341015,-114.353105212505,
11.9089842127547));
#256297=CARTESIAN_POINT('Ctrl Pts',(81.4988640709653,-114.311529402532,
11.9445266216304));
#256298=CARTESIAN_POINT('Ctrl Pts',(81.2444644384059,-114.267752870079,
11.9787247352563));
#256299=CARTESIAN_POINT('Ctrl Pts',(80.9597456260951,-114.218759079476,
12.016998557419));
#256300=CARTESIAN_POINT('Ctrl Pts',(80.6753810400077,-114.167147236487,
12.0534610877611));
#256301=CARTESIAN_POINT('Ctrl Pts',(80.3915054834947,-114.112878627138,
12.0877657414697));
#256302=CARTESIAN_POINT('Ctrl Pts',(80.1315884873099,-114.063190185828,
12.1191751472552));
#256303=CARTESIAN_POINT('Ctrl Pts',(79.8720812258998,-114.011274194815,
12.1487756059618));
#256304=CARTESIAN_POINT('Ctrl Pts',(79.6131099264372,-113.957084553584,
12.1762747511384));
#256305=CARTESIAN_POINT('Ctrl Pts',(79.5842583911621,-113.951047381324,
12.1793383823544));
#256306=CARTESIAN_POINT('Ctrl Pts',(79.5554139374348,-113.944982071645,
12.1823758526507));
#256307=CARTESIAN_POINT('Ctrl Pts',(79.5265771857676,-113.938888643004,
12.1853866936196));
#256308=CARTESIAN_POINT('Ctrl Pts',(79.1552547066283,-113.860425331486,
12.2241564186487));
#256309=CARTESIAN_POINT('Ctrl Pts',(78.7846328269209,-113.777204059966,
12.2586195275686));
#256310=CARTESIAN_POINT('Ctrl Pts',(78.4147483858496,-113.688967055657,
12.2875599189643));
#256311=CARTESIAN_POINT('Ctrl Pts',(78.2248346050177,-113.6436625734,12.3024190980441));
#256312=CARTESIAN_POINT('Ctrl Pts',(78.03511493423,-113.5970358706,12.3158215393074));
#256313=CARTESIAN_POINT('Ctrl Pts',(77.8455925411284,-113.549052337868,
12.3275976932325));
#256314=CARTESIAN_POINT('Ctrl Pts',(77.5177312889421,-113.466043987941,
12.3479696635768));
#256315=CARTESIAN_POINT('Ctrl Pts',(77.1904629065562,-113.378979813794,
12.3635332048009));
#256316=CARTESIAN_POINT('Ctrl Pts',(76.8637289612717,-113.287580782422,
12.3728032157562));
#256317=CARTESIAN_POINT('Ctrl Pts',(76.6415217694246,-113.225421577993,
12.3791076207086));
#256318=CARTESIAN_POINT('Ctrl Pts',(76.4195614759289,-113.161257371659,
12.3825));
#256319=CARTESIAN_POINT('Ctrl Pts',(76.1978262581578,-113.095,12.3825));
#256320=CARTESIAN_POINT('Origin',(-74.5679259799751,-112.039285751595,14.2875));
#256321=CARTESIAN_POINT('Origin',(-74.5679259799751,-112.039285751595,14.2875));
#256322=CARTESIAN_POINT('Origin',(0.,-113.095,10.4775));
#256323=CARTESIAN_POINT('Ctrl Pts',(-90.,-115.,10.4775));
#256324=CARTESIAN_POINT('Ctrl Pts',(-89.5835438364623,-115.,10.5558582760744));
#256325=CARTESIAN_POINT('Ctrl Pts',(-89.1669828329586,-114.995145444742,
10.6342451251677));
#256326=CARTESIAN_POINT('Ctrl Pts',(-88.7504746564834,-114.985453756063,
10.7122315109302));
#256327=CARTESIAN_POINT('Ctrl Pts',(-88.3493129355877,-114.976119162583,
10.787344448649));
#256328=CARTESIAN_POINT('Ctrl Pts',(-87.9481990723833,-114.962297205616,
10.8620867505668));
#256329=CARTESIAN_POINT('Ctrl Pts',(-87.5472762325166,-114.943957243982,
10.9360757308282));
#256330=CARTESIAN_POINT('Ctrl Pts',(-87.2069586549702,-114.928389631727,
10.9988802109523));
#256331=CARTESIAN_POINT('Ctrl Pts',(-86.8667783863508,-114.909565993822,
11.0611422131556));
#256332=CARTESIAN_POINT('Ctrl Pts',(-86.5268333104866,-114.887440575962,
11.1226211406014));
#256333=CARTESIAN_POINT('Ctrl Pts',(-86.5074818406287,-114.886181080275,
11.1261208459827));
#256334=CARTESIAN_POINT('Ctrl Pts',(-86.4881313431668,-114.884910894891,
11.1296179650593));
#256335=CARTESIAN_POINT('Ctrl Pts',(-86.4687819131639,-114.883630015072,
11.1331124382524));
#256336=CARTESIAN_POINT('Ctrl Pts',(-85.900400763887,-114.846004723596,
11.2357610790286));
#256337=CARTESIAN_POINT('Ctrl Pts',(-85.3326432827616,-114.799248326424,
11.3362547894291));
#256338=CARTESIAN_POINT('Ctrl Pts',(-84.7653562148502,-114.742990120853,
11.4332724000528));
#256339=CARTESIAN_POINT('Ctrl Pts',(-84.1980691469388,-114.686731915282,
11.5302900106764));
#256340=CARTESIAN_POINT('Ctrl Pts',(-83.6312517469126,-114.62097164889,
11.6238302836077));
#256341=CARTESIAN_POINT('Ctrl Pts',(-83.0647232345982,-114.545392304676,
11.7125671552065));
#256342=CARTESIAN_POINT('Ctrl Pts',(-83.0359704727094,-114.541556460864,
11.7170707769738));
#256343=CARTESIAN_POINT('Ctrl Pts',(-83.0072223038157,-114.537695858892,
11.7215614148314));
#256344=CARTESIAN_POINT('Ctrl Pts',(-82.978478279317,-114.533810424182,
11.7260389714724));
#256345=CARTESIAN_POINT('Ctrl Pts',(-82.6542583520783,-114.489984433187,
11.7765438368714));
#256346=CARTESIAN_POINT('Ctrl Pts',(-82.3305619488634,-114.442984724948,
11.8253691505402));
#256347=CARTESIAN_POINT('Ctrl Pts',(-82.0067026925516,-114.392600666908,
11.8722415248234));
#256348=CARTESIAN_POINT('Ctrl Pts',(-81.7528333341009,-114.353105212505,
11.9089842127548));
#256349=CARTESIAN_POINT('Ctrl Pts',(-81.498864070965,-114.311529402532,
11.9445266216304));
#256350=CARTESIAN_POINT('Ctrl Pts',(-81.2444644384059,-114.267752870079,
11.9787247352563));
#256351=CARTESIAN_POINT('Ctrl Pts',(-80.9597456260961,-114.218759079476,
12.0169985574188));
#256352=CARTESIAN_POINT('Ctrl Pts',(-80.6753810400096,-114.167147236488,
12.0534610877609));
#256353=CARTESIAN_POINT('Ctrl Pts',(-80.3915054834976,-114.112878627139,
12.0877657414694));
#256354=CARTESIAN_POINT('Ctrl Pts',(-80.1315884873118,-114.063190185829,
12.119175147255));
#256355=CARTESIAN_POINT('Ctrl Pts',(-79.8720812259008,-114.011274194815,
12.1487756059617));
#256356=CARTESIAN_POINT('Ctrl Pts',(-79.6131099264372,-113.957084553584,
12.1762747511384));
#256357=CARTESIAN_POINT('Ctrl Pts',(-79.5842583911621,-113.951047381324,
12.1793383823544));
#256358=CARTESIAN_POINT('Ctrl Pts',(-79.5554139374348,-113.944982071645,
12.1823758526507));
#256359=CARTESIAN_POINT('Ctrl Pts',(-79.5265771857676,-113.938888643004,
12.1853866936196));
#256360=CARTESIAN_POINT('Ctrl Pts',(-79.1552547066275,-113.860425331486,
12.2241564186488));
#256361=CARTESIAN_POINT('Ctrl Pts',(-78.7846328269193,-113.777204059965,
12.2586195275687));
#256362=CARTESIAN_POINT('Ctrl Pts',(-78.4147483858471,-113.688967055656,
12.2875599189645));
#256363=CARTESIAN_POINT('Ctrl Pts',(-78.2248346050161,-113.643662573399,
12.3024190980442));
#256364=CARTESIAN_POINT('Ctrl Pts',(-78.0351149342292,-113.597035870599,
12.3158215393074));
#256365=CARTESIAN_POINT('Ctrl Pts',(-77.8455925411284,-113.549052337868,
12.3275976932325));
#256366=CARTESIAN_POINT('Ctrl Pts',(-77.5177312889423,-113.466043987941,
12.3479696635768));
#256367=CARTESIAN_POINT('Ctrl Pts',(-77.1904629065567,-113.378979813794,
12.3635332048009));
#256368=CARTESIAN_POINT('Ctrl Pts',(-76.8637289612724,-113.287580782422,
12.3728032157562));
#256369=CARTESIAN_POINT('Ctrl Pts',(-76.6415217694251,-113.225421577994,
12.3791076207086));
#256370=CARTESIAN_POINT('Ctrl Pts',(-76.4195614759291,-113.161257371659,
12.3825));
#256371=CARTESIAN_POINT('Ctrl Pts',(-76.1978262581577,-113.095,12.3825));
#256372=CARTESIAN_POINT('Origin',(-90.,-90.,14.2875));
#256373=CARTESIAN_POINT('Origin',(-76.1978262581577,-113.095,14.2875));
#256374=CARTESIAN_POINT('Ctrl Pts',(-76.1978262581577,-113.095,12.3825));
#256375=CARTESIAN_POINT('Ctrl Pts',(-77.1750847966528,-111.45976584278,
12.3825));
#256376=CARTESIAN_POINT('Ctrl Pts',(-77.1750847966528,-111.45976584278,
14.2875));
#256377=CARTESIAN_POINT('Ctrl Pts',(-76.7421246518763,-113.257643450726,
12.3825));
#256378=CARTESIAN_POINT('Ctrl Pts',(-77.5941846099562,-111.71023081209,
12.5172751948194));
#256379=CARTESIAN_POINT('Ctrl Pts',(-77.6808356682961,-111.762015741049,
14.2874999966875));
#256380=CARTESIAN_POINT('Ctrl Pts',(-77.2910619607791,-113.408657903693,
12.3620536717506));
#256381=CARTESIAN_POINT('Ctrl Pts',(-78.0590963418289,-111.971409284925,
12.6053517687442));
#256382=CARTESIAN_POINT('Ctrl Pts',(-78.1909142917095,-112.04266475307,
14.2466073426296));
#256383=CARTESIAN_POINT('Ctrl Pts',(-78.4001194763382,-113.689453561681,
12.2931400483747));
#256384=CARTESIAN_POINT('Ctrl Pts',(-79.0242905953313,-112.468920289919,
12.6961322557778));
#256385=CARTESIAN_POINT('Ctrl Pts',(-79.2214453413673,-112.564492774109,
14.108780097621));
#256386=CARTESIAN_POINT('Ctrl Pts',(-78.9602349460145,-113.819221943657,
12.244515847471));
#256387=CARTESIAN_POINT('Ctrl Pts',(-79.526944890976,-112.708892347893,
12.703865475829));
#256388=CARTESIAN_POINT('Ctrl Pts',(-79.7419020126347,-112.805653119423,
14.0115316944756));
#256389=CARTESIAN_POINT('Ctrl Pts',(-80.0929157064278,-114.058562415705,
12.1262540447041));
#256390=CARTESIAN_POINT('Ctrl Pts',(-80.5569292865739,-113.155754679235,
12.6577917414232));
#256391=CARTESIAN_POINT('Ctrl Pts',(-80.7943836707349,-113.250441211302,
13.7750080898747));
#256392=CARTESIAN_POINT('Ctrl Pts',(-80.666825605363,-114.168356412835,
12.0563732669971));
#256393=CARTESIAN_POINT('Ctrl Pts',(-81.0885336408363,-113.366292203084,
12.6062543646742));
#256394=CARTESIAN_POINT('Ctrl Pts',(-81.3276580610674,-113.45448134688,
13.6352465336299));
#256395=CARTESIAN_POINT('Ctrl Pts',(-81.8221003906478,-114.367154525562,
11.9010721426414));
#256396=CARTESIAN_POINT('Ctrl Pts',(-82.1657264091691,-113.748604057329,
12.4584071352196));
#256397=CARTESIAN_POINT('Ctrl Pts',(-82.4011339813139,-113.823925897865,
13.3246442856472));
#256398=CARTESIAN_POINT('Ctrl Pts',(-82.3997797445818,-114.455588968268,
11.8161812982783));
#256399=CARTESIAN_POINT('Ctrl Pts',(-82.7112571397903,-113.921920427821,
12.3636877604077));
#256400=CARTESIAN_POINT('Ctrl Pts',(-82.9379109315738,-113.98827163761,
13.1548625963702));
#256401=CARTESIAN_POINT('Ctrl Pts',(-84.1358715971169,-114.690259297042,
11.5457474483613));
#256402=CARTESIAN_POINT('Ctrl Pts',(-84.3341564328195,-114.375512716331,
12.0384183635703));
#256403=CARTESIAN_POINT('Ctrl Pts',(-84.5510793506422,-114.424380779002,
12.6139948970955));
#256404=CARTESIAN_POINT('Ctrl Pts',(-85.2973823883387,-114.806088152743,
11.3446613455991));
#256405=CARTESIAN_POINT('Ctrl Pts',(-85.4594058856995,-114.611553326324,
11.7583160303656));
#256406=CARTESIAN_POINT('Ctrl Pts',(-85.6303497382816,-114.639636039159,
12.2118226911433));
#256407=CARTESIAN_POINT('Ctrl Pts',(-87.6401800974599,-114.96117307666,
10.9215602590933));
#256408=CARTESIAN_POINT('Ctrl Pts',(-87.7104675830927,-114.920352198467,
11.1472581448906));
#256409=CARTESIAN_POINT('Ctrl Pts',(-87.8072663979372,-114.927844409462,
11.3656205182415));
#256410=CARTESIAN_POINT('Ctrl Pts',(-88.8227423399098,-115.,10.6990068206853));
#256411=CARTESIAN_POINT('Ctrl Pts',(-88.8644746746686,-115.,10.8097442389035));
#256412=CARTESIAN_POINT('Ctrl Pts',(-88.9061071730694,-115.,10.9205098031028));
#256413=CARTESIAN_POINT('Ctrl Pts',(-90.,-115.,10.4775));
#256414=CARTESIAN_POINT('Ctrl Pts',(-90.,-115.,10.4775));
#256415=CARTESIAN_POINT('Ctrl Pts',(-90.,-115.,10.4775));
#256416=CARTESIAN_POINT('Origin',(112.039285751595,74.5679259799752,14.2875));
#256417=CARTESIAN_POINT('Origin',(112.039285751595,74.5679259799752,14.2875));
#256418=CARTESIAN_POINT('Origin',(90.,90.,14.2875));
#256419=CARTESIAN_POINT('Origin',(113.095,76.1978262581577,14.2875));
#256420=CARTESIAN_POINT('Ctrl Pts',(111.45976584278,77.1750847966528,14.2875));
#256421=CARTESIAN_POINT('Ctrl Pts',(111.45976584278,77.1750847966528,12.3825));
#256422=CARTESIAN_POINT('Ctrl Pts',(113.095,76.1978262581577,12.3825));
#256423=CARTESIAN_POINT('Ctrl Pts',(111.76201574105,77.6808356682986,14.2874999966875));
#256424=CARTESIAN_POINT('Ctrl Pts',(111.710230812097,77.5941846099538,12.5172751948261));
#256425=CARTESIAN_POINT('Ctrl Pts',(113.257643450739,76.7421246518766,12.3825));
#256426=CARTESIAN_POINT('Ctrl Pts',(112.042664753068,78.1909142917061,14.2466073426296));
#256427=CARTESIAN_POINT('Ctrl Pts',(111.97140928493,78.0590963418208,12.6053517687504));
#256428=CARTESIAN_POINT('Ctrl Pts',(113.408657903689,77.2910619607747,12.3620536717516));
#256429=CARTESIAN_POINT('Ctrl Pts',(112.564492774111,79.2214453413707,14.108780097621));
#256430=CARTESIAN_POINT('Ctrl Pts',(112.468920289915,79.0242905953405,12.696132255772));
#256431=CARTESIAN_POINT('Ctrl Pts',(113.689453561686,78.4001194763425,12.2931400483737));
#256432=CARTESIAN_POINT('Ctrl Pts',(112.805653119421,79.7419020126294,14.0115316944767));
#256433=CARTESIAN_POINT('Ctrl Pts',(112.708892347889,79.5269448909711,12.7038654758262));
#256434=CARTESIAN_POINT('Ctrl Pts',(113.819221943654,78.9602349460102,12.2445158474727));
#256435=CARTESIAN_POINT('Ctrl Pts',(113.250441211304,80.7943836707402,13.7750080898736));
#256436=CARTESIAN_POINT('Ctrl Pts',(113.15575467924,80.5569292865777,12.6577917414259));
#256437=CARTESIAN_POINT('Ctrl Pts',(114.058562415709,80.0929157064321,12.1262540447024));
#256438=CARTESIAN_POINT('Ctrl Pts',(113.454481346879,81.327658061066,13.635246533631));
#256439=CARTESIAN_POINT('Ctrl Pts',(113.366292203071,81.0885336408355,12.6062543646726));
#256440=CARTESIAN_POINT('Ctrl Pts',(114.168356412835,80.666825605363,12.0563732669973));
#256441=CARTESIAN_POINT('Ctrl Pts',(113.823925897865,82.4011339813153,13.3246442856461));
#256442=CARTESIAN_POINT('Ctrl Pts',(113.748604057341,82.1657264091684,12.4584071352213));
#256443=CARTESIAN_POINT('Ctrl Pts',(114.367154525562,81.8221003906478,11.9010721426412));
#256444=CARTESIAN_POINT('Ctrl Pts',(113.98827163761,82.9379109315738,13.1548625963718));
#256445=CARTESIAN_POINT('Ctrl Pts',(113.921920427826,82.7112571397905,12.3636877604088));
#256446=CARTESIAN_POINT('Ctrl Pts',(114.455588968267,82.3997797445818,11.816181298279));
#256447=CARTESIAN_POINT('Ctrl Pts',(114.424380779002,84.5510793506422,12.6139948970922));
#256448=CARTESIAN_POINT('Ctrl Pts',(114.375512716323,84.3341564328201,12.038418363568));
#256449=CARTESIAN_POINT('Ctrl Pts',(114.690259297043,84.1358715971169,11.54574744836));
#256450=CARTESIAN_POINT('Ctrl Pts',(114.639636039159,85.6303497382827,12.2118226911378));
#256451=CARTESIAN_POINT('Ctrl Pts',(114.611553326333,85.4594058856995,11.7583160303623));
#256452=CARTESIAN_POINT('Ctrl Pts',(114.806088152744,85.2973823883387,11.3446613455943));
#256453=CARTESIAN_POINT('Ctrl Pts',(114.927844409462,87.807266397936,11.3656205182469));
#256454=CARTESIAN_POINT('Ctrl Pts',(114.920352198458,87.7104675830927,11.1472581448938));
#256455=CARTESIAN_POINT('Ctrl Pts',(114.961173076658,87.6401800974599,10.921560259098));
#256456=CARTESIAN_POINT('Ctrl Pts',(115.,88.9061071730244,10.9205098029853));
#256457=CARTESIAN_POINT('Ctrl Pts',(115.,88.8644746746419,10.8097442388102));
#256458=CARTESIAN_POINT('Ctrl Pts',(115.,88.8227423398972,10.6990068206156));
#256459=CARTESIAN_POINT('Ctrl Pts',(115.,90.,10.4775));
#256460=CARTESIAN_POINT('Ctrl Pts',(115.,90.,10.4775));
#256461=CARTESIAN_POINT('Ctrl Pts',(115.,90.,10.4775));
#256462=CARTESIAN_POINT('Ctrl Pts',(115.,90.,10.4775));
#256463=CARTESIAN_POINT('Ctrl Pts',(115.,89.5835438336671,10.5558582765748));
#256464=CARTESIAN_POINT('Ctrl Pts',(114.995145444676,89.1669828273719,10.6342451261915));
#256465=CARTESIAN_POINT('Ctrl Pts',(114.985453755867,88.7504746481075,10.7122315124746));
#256466=CARTESIAN_POINT('Ctrl Pts',(114.976119162444,88.3493129324001,10.7873444492202));
#256467=CARTESIAN_POINT('Ctrl Pts',(114.962297205651,87.9481990743845,10.862086750177));
#256468=CARTESIAN_POINT('Ctrl Pts',(114.943957244309,87.5472762396997,10.9360757294963));
#256469=CARTESIAN_POINT('Ctrl Pts',(114.92838963199,87.2069586597576,10.9988802100746));
#256470=CARTESIAN_POINT('Ctrl Pts',(114.909565993977,86.866778388743,11.0611422127244));
#256471=CARTESIAN_POINT('Ctrl Pts',(114.887440575962,86.526833310487,11.1226211406026));
#256472=CARTESIAN_POINT('Ctrl Pts',(114.886181080275,86.5074818406292,11.1261208459839));
#256473=CARTESIAN_POINT('Ctrl Pts',(114.88491089489,86.4881313431673,11.1296179650604));
#256474=CARTESIAN_POINT('Ctrl Pts',(114.883630015071,86.4687819131644,11.1331124382534));
#256475=CARTESIAN_POINT('Ctrl Pts',(114.846004723596,85.9004007638871,11.2357610790281));
#256476=CARTESIAN_POINT('Ctrl Pts',(114.799248326424,85.3326432827615,11.3362547894283));
#256477=CARTESIAN_POINT('Ctrl Pts',(114.742990120853,84.76535621485,11.4332724000518));
#256478=CARTESIAN_POINT('Ctrl Pts',(114.686731915282,84.1980691469384,11.5302900106753));
#256479=CARTESIAN_POINT('Ctrl Pts',(114.620971648891,83.6312517469121,11.6238302836067));
#256480=CARTESIAN_POINT('Ctrl Pts',(114.545392304676,83.0647232345978,11.7125671552059));
#256481=CARTESIAN_POINT('Ctrl Pts',(114.541556460865,83.0359704727091,11.7170707769731));
#256482=CARTESIAN_POINT('Ctrl Pts',(114.537695858892,83.0072223038154,11.7215614148308));
#256483=CARTESIAN_POINT('Ctrl Pts',(114.533810424182,82.9784782793166,11.7260389714718));
#256484=CARTESIAN_POINT('Ctrl Pts',(114.489984433162,82.6542583518944,11.7765438368996));
#256485=CARTESIAN_POINT('Ctrl Pts',(114.442984724895,82.3305619484957,11.8253691505951));
#256486=CARTESIAN_POINT('Ctrl Pts',(114.392600666823,82.0067026919993,11.8722415249027));
#256487=CARTESIAN_POINT('Ctrl Pts',(114.353105212445,81.7528333337324,11.9089842128056));
#256488=CARTESIAN_POINT('Ctrl Pts',(114.311529402501,81.4988640707801,11.9445266216545));
#256489=CARTESIAN_POINT('Ctrl Pts',(114.26775287008,81.2444644384055,11.9787247352557));
#256490=CARTESIAN_POINT('Ctrl Pts',(114.21875907944,80.9597456258849,12.0169985574467));
#256491=CARTESIAN_POINT('Ctrl Pts',(114.167147236413,80.6753810395896,12.053461087814));
#256492=CARTESIAN_POINT('Ctrl Pts',(114.112878627021,80.3915054828696,12.0877657415443));
#256493=CARTESIAN_POINT('Ctrl Pts',(114.063190185747,80.1315884868937,12.1191751473015));
#256494=CARTESIAN_POINT('Ctrl Pts',(114.011274194774,79.872081225692,12.1487756059824));
#256495=CARTESIAN_POINT('Ctrl Pts',(113.957084553587,79.6131099264361,12.1762747511373));
#256496=CARTESIAN_POINT('Ctrl Pts',(113.951047381326,79.5842583911611,12.1793383823534));
#256497=CARTESIAN_POINT('Ctrl Pts',(113.944982071647,79.5554139374339,12.1823758526497));
#256498=CARTESIAN_POINT('Ctrl Pts',(113.938888643006,79.5265771857666,12.1853866936187));
#256499=CARTESIAN_POINT('Ctrl Pts',(113.86042533142,79.155254706309,12.2241564186816));
#256500=CARTESIAN_POINT('Ctrl Pts',(113.777204059827,78.7846328262872,12.2586195276268));
#256501=CARTESIAN_POINT('Ctrl Pts',(113.688967055434,78.4147483849003,12.2875599190377));
#256502=CARTESIAN_POINT('Ctrl Pts',(113.643662573248,78.2248346043861,12.3024190980878));
#256503=CARTESIAN_POINT('Ctrl Pts',(113.597035870523,78.0351149339147,12.3158215393261));
#256504=CARTESIAN_POINT('Ctrl Pts',(113.54905233787,77.8455925411273,12.3275976932321));
#256505=CARTESIAN_POINT('Ctrl Pts',(113.466043987764,77.5177312882442,12.3479696636203));
#256506=CARTESIAN_POINT('Ctrl Pts',(113.378979813428,77.1904629051675,12.3635332048672));
#256507=CARTESIAN_POINT('Ctrl Pts',(113.287580781847,76.8637289591964,12.3728032158153));
#256508=CARTESIAN_POINT('Ctrl Pts',(113.2254215776,76.6415217680418,12.3791076207299));
#256509=CARTESIAN_POINT('Ctrl Pts',(113.161257371457,76.4195614752379,12.3825));
#256510=CARTESIAN_POINT('Ctrl Pts',(113.095,76.1978262581577,12.3825));
#256511=CARTESIAN_POINT('Origin',(112.039285751595,-74.5679259799751,14.2875));
#256512=CARTESIAN_POINT('Origin',(112.039285751595,-74.5679259799751,14.2875));
#256513=CARTESIAN_POINT('Origin',(113.095,0.,10.4775));
#256514=CARTESIAN_POINT('Ctrl Pts',(115.,-90.,10.4775));
#256515=CARTESIAN_POINT('Ctrl Pts',(115.,-89.5835438336648,10.5558582765753));
#256516=CARTESIAN_POINT('Ctrl Pts',(114.995145444676,-89.1669828273673,
10.6342451261923));
#256517=CARTESIAN_POINT('Ctrl Pts',(114.985453755867,-88.7504746481007,
10.7122315124758));
#256518=CARTESIAN_POINT('Ctrl Pts',(114.976119162444,-88.3493129323938,
10.7873444492214));
#256519=CARTESIAN_POINT('Ctrl Pts',(114.962297205651,-87.9481990743787,
10.862086750178));
#256520=CARTESIAN_POINT('Ctrl Pts',(114.943957244309,-87.5472762396945,
10.9360757294973));
#256521=CARTESIAN_POINT('Ctrl Pts',(114.92838963199,-87.2069586597541,10.9988802100753));
#256522=CARTESIAN_POINT('Ctrl Pts',(114.909565993977,-86.8667783887413,
11.0611422127247));
#256523=CARTESIAN_POINT('Ctrl Pts',(114.887440575962,-86.5268333104871,
11.1226211406026));
#256524=CARTESIAN_POINT('Ctrl Pts',(114.886181080275,-86.5074818406292,
11.1261208459839));
#256525=CARTESIAN_POINT('Ctrl Pts',(114.88491089489,-86.4881313431673,11.1296179650604));
#256526=CARTESIAN_POINT('Ctrl Pts',(114.883630015071,-86.4687819131644,
11.1331124382534));
#256527=CARTESIAN_POINT('Ctrl Pts',(114.846004723596,-85.9004007638872,
11.2357610790281));
#256528=CARTESIAN_POINT('Ctrl Pts',(114.799248326424,-85.3326432827615,
11.3362547894283));
#256529=CARTESIAN_POINT('Ctrl Pts',(114.742990120853,-84.76535621485,11.4332724000518));
#256530=CARTESIAN_POINT('Ctrl Pts',(114.686731915282,-84.1980691469384,
11.5302900106753));
#256531=CARTESIAN_POINT('Ctrl Pts',(114.620971648891,-83.631251746912,11.6238302836067));
#256532=CARTESIAN_POINT('Ctrl Pts',(114.545392304676,-83.0647232345978,
11.7125671552059));
#256533=CARTESIAN_POINT('Ctrl Pts',(114.541556460865,-83.035970472709,11.7170707769731));
#256534=CARTESIAN_POINT('Ctrl Pts',(114.537695858892,-83.0072223038154,
11.7215614148308));
#256535=CARTESIAN_POINT('Ctrl Pts',(114.533810424182,-82.9784782793166,
11.7260389714718));
#256536=CARTESIAN_POINT('Ctrl Pts',(114.489984433162,-82.6542583518949,
11.7765438368996));
#256537=CARTESIAN_POINT('Ctrl Pts',(114.442984724895,-82.3305619484966,
11.825369150595));
#256538=CARTESIAN_POINT('Ctrl Pts',(114.392600666823,-82.0067026920007,
11.8722415249025));
#256539=CARTESIAN_POINT('Ctrl Pts',(114.353105212445,-81.7528333337334,
11.9089842128055));
#256540=CARTESIAN_POINT('Ctrl Pts',(114.311529402501,-81.4988640707806,
11.9445266216544));
#256541=CARTESIAN_POINT('Ctrl Pts',(114.26775287008,-81.2444644384055,11.9787247352557));
#256542=CARTESIAN_POINT('Ctrl Pts',(114.21875907944,-80.959745625885,12.0169985574467));
#256543=CARTESIAN_POINT('Ctrl Pts',(114.167147236413,-80.6753810395898,
12.053461087814));
#256544=CARTESIAN_POINT('Ctrl Pts',(114.112878627021,-80.39150548287,12.0877657415442));
#256545=CARTESIAN_POINT('Ctrl Pts',(114.063190185747,-80.1315884868939,
12.1191751473015));
#256546=CARTESIAN_POINT('Ctrl Pts',(114.011274194774,-79.8720812256921,
12.1487756059824));
#256547=CARTESIAN_POINT('Ctrl Pts',(113.957084553586,-79.6131099264361,
12.1762747511373));
#256548=CARTESIAN_POINT('Ctrl Pts',(113.951047381325,-79.584258391161,12.1793383823534));
#256549=CARTESIAN_POINT('Ctrl Pts',(113.944982071647,-79.5554139374338,
12.1823758526497));
#256550=CARTESIAN_POINT('Ctrl Pts',(113.938888643006,-79.5265771857666,
12.1853866936187));
#256551=CARTESIAN_POINT('Ctrl Pts',(113.86042533142,-79.1552547063091,12.2241564186816));
#256552=CARTESIAN_POINT('Ctrl Pts',(113.777204059827,-78.7846328262874,
12.2586195276268));
#256553=CARTESIAN_POINT('Ctrl Pts',(113.688967055434,-78.4147483849006,
12.2875599190377));
#256554=CARTESIAN_POINT('Ctrl Pts',(113.643662573248,-78.2248346043863,
12.3024190980878));
#256555=CARTESIAN_POINT('Ctrl Pts',(113.597035870523,-78.0351149339149,
12.3158215393261));
#256556=CARTESIAN_POINT('Ctrl Pts',(113.54905233787,-77.8455925411274,12.3275976932321));
#256557=CARTESIAN_POINT('Ctrl Pts',(113.466043987764,-77.5177312882447,
12.3479696636203));
#256558=CARTESIAN_POINT('Ctrl Pts',(113.378979813428,-77.1904629051685,
12.3635332048671));
#256559=CARTESIAN_POINT('Ctrl Pts',(113.287580781847,-76.8637289591979,
12.3728032158152));
#256560=CARTESIAN_POINT('Ctrl Pts',(113.2254215776,-76.6415217680428,12.3791076207298));
#256561=CARTESIAN_POINT('Ctrl Pts',(113.161257371458,-76.4195614752384,
12.3825));
#256562=CARTESIAN_POINT('Ctrl Pts',(113.095,-76.1978262581577,12.3825));
#256563=CARTESIAN_POINT('Origin',(90.,-90.,14.2875));
#256564=CARTESIAN_POINT('Origin',(113.095,-76.1978262581577,14.2875));
#256565=CARTESIAN_POINT('Ctrl Pts',(113.095,-76.1978262581577,12.3825));
#256566=CARTESIAN_POINT('Ctrl Pts',(111.45976584278,-77.1750847966528,12.3825));
#256567=CARTESIAN_POINT('Ctrl Pts',(111.45976584278,-77.1750847966528,14.2875));
#256568=CARTESIAN_POINT('Ctrl Pts',(113.257643450739,-76.7421246518766,
12.3825));
#256569=CARTESIAN_POINT('Ctrl Pts',(111.710230812097,-77.5941846099538,
12.5172751948261));
#256570=CARTESIAN_POINT('Ctrl Pts',(111.76201574105,-77.6808356682986,14.2874999966875));
#256571=CARTESIAN_POINT('Ctrl Pts',(113.408657903689,-77.2910619607747,
12.3620536717516));
#256572=CARTESIAN_POINT('Ctrl Pts',(111.97140928493,-78.0590963418208,12.6053517687504));
#256573=CARTESIAN_POINT('Ctrl Pts',(112.042664753068,-78.1909142917061,
14.2466073426296));
#256574=CARTESIAN_POINT('Ctrl Pts',(113.689453561686,-78.4001194763425,
12.2931400483737));
#256575=CARTESIAN_POINT('Ctrl Pts',(112.468920289915,-79.0242905953405,
12.696132255772));
#256576=CARTESIAN_POINT('Ctrl Pts',(112.564492774111,-79.2214453413707,
14.108780097621));
#256577=CARTESIAN_POINT('Ctrl Pts',(113.819221943654,-78.9602349460102,
12.2445158474727));
#256578=CARTESIAN_POINT('Ctrl Pts',(112.708892347889,-79.5269448909711,
12.7038654758262));
#256579=CARTESIAN_POINT('Ctrl Pts',(112.805653119421,-79.7419020126294,
14.0115316944767));
#256580=CARTESIAN_POINT('Ctrl Pts',(114.058562415709,-80.0929157064321,
12.1262540447024));
#256581=CARTESIAN_POINT('Ctrl Pts',(113.15575467924,-80.5569292865777,12.6577917414259));
#256582=CARTESIAN_POINT('Ctrl Pts',(113.250441211304,-80.7943836707402,
13.7750080898736));
#256583=CARTESIAN_POINT('Ctrl Pts',(114.168356412835,-80.666825605363,12.0563732669973));
#256584=CARTESIAN_POINT('Ctrl Pts',(113.366292203071,-81.0885336408355,
12.6062543646726));
#256585=CARTESIAN_POINT('Ctrl Pts',(113.454481346879,-81.327658061066,13.635246533631));
#256586=CARTESIAN_POINT('Ctrl Pts',(114.367154525562,-81.8221003906478,
11.9010721426412));
#256587=CARTESIAN_POINT('Ctrl Pts',(113.748604057341,-82.1657264091684,
12.4584071352213));
#256588=CARTESIAN_POINT('Ctrl Pts',(113.823925897865,-82.4011339813153,
13.3246442856461));
#256589=CARTESIAN_POINT('Ctrl Pts',(114.455588968267,-82.3997797445818,
11.816181298279));
#256590=CARTESIAN_POINT('Ctrl Pts',(113.921920427826,-82.7112571397905,
12.3636877604088));
#256591=CARTESIAN_POINT('Ctrl Pts',(113.98827163761,-82.9379109315738,13.1548625963718));
#256592=CARTESIAN_POINT('Ctrl Pts',(114.690259297043,-84.1358715971169,
11.54574744836));
#256593=CARTESIAN_POINT('Ctrl Pts',(114.375512716323,-84.3341564328201,
12.038418363568));
#256594=CARTESIAN_POINT('Ctrl Pts',(114.424380779002,-84.5510793506422,
12.6139948970922));
#256595=CARTESIAN_POINT('Ctrl Pts',(114.806088152744,-85.2973823883387,
11.3446613455943));
#256596=CARTESIAN_POINT('Ctrl Pts',(114.611553326333,-85.4594058856995,
11.7583160303623));
#256597=CARTESIAN_POINT('Ctrl Pts',(114.639636039159,-85.6303497382827,
12.2118226911378));
#256598=CARTESIAN_POINT('Ctrl Pts',(114.961173076658,-87.6401800974599,
10.921560259098));
#256599=CARTESIAN_POINT('Ctrl Pts',(114.920352198458,-87.7104675830927,
11.1472581448938));
#256600=CARTESIAN_POINT('Ctrl Pts',(114.927844409462,-87.807266397936,11.3656205182469));
#256601=CARTESIAN_POINT('Ctrl Pts',(115.,-88.8227423398972,10.6990068206156));
#256602=CARTESIAN_POINT('Ctrl Pts',(115.,-88.8644746746419,10.8097442388102));
#256603=CARTESIAN_POINT('Ctrl Pts',(115.,-88.9061071730244,10.9205098029853));
#256604=CARTESIAN_POINT('Ctrl Pts',(115.,-90.,10.4775));
#256605=CARTESIAN_POINT('Ctrl Pts',(115.,-90.,10.4775));
#256606=CARTESIAN_POINT('Ctrl Pts',(115.,-90.,10.4775));
#256607=CARTESIAN_POINT('Origin',(-112.039285751595,-74.5679259799751,14.2875));
#256608=CARTESIAN_POINT('Origin',(-112.039285751595,-74.5679259799751,14.2875));
#256609=CARTESIAN_POINT('Origin',(0.,0.,14.2875));
#256610=CARTESIAN_POINT('Origin',(-90.,-90.,14.2875));
#256611=CARTESIAN_POINT('Origin',(-113.095,-76.1978262581577,14.2875));
#256612=CARTESIAN_POINT('Ctrl Pts',(-111.45976584278,-77.1750847966528,
14.2875));
#256613=CARTESIAN_POINT('Ctrl Pts',(-111.45976584278,-77.1750847966528,
12.3825));
#256614=CARTESIAN_POINT('Ctrl Pts',(-113.095,-76.1978262581577,12.3825));
#256615=CARTESIAN_POINT('Ctrl Pts',(-111.762015741049,-77.6808356682973,
14.2874999966875));
#256616=CARTESIAN_POINT('Ctrl Pts',(-111.710230812091,-77.5941846099565,
12.5172751948228));
#256617=CARTESIAN_POINT('Ctrl Pts',(-113.257643450735,-76.7421246518768,
12.3825));
#256618=CARTESIAN_POINT('Ctrl Pts',(-112.042664753069,-78.1909142917078,
14.2466073426301));
#256619=CARTESIAN_POINT('Ctrl Pts',(-111.971409284934,-78.0590963418208,
12.605351768751));
#256620=CARTESIAN_POINT('Ctrl Pts',(-113.408657903693,-77.2910619607747,
12.3620536717506));
#256621=CARTESIAN_POINT('Ctrl Pts',(-112.56449277411,-79.221445341369,14.1087800976205));
#256622=CARTESIAN_POINT('Ctrl Pts',(-112.468920289911,-79.0242905953405,
12.6961322557715));
#256623=CARTESIAN_POINT('Ctrl Pts',(-113.689453561682,-78.4001194763425,
12.2931400483747));
#256624=CARTESIAN_POINT('Ctrl Pts',(-112.805653119421,-79.741902012631,
14.0115316944761));
#256625=CARTESIAN_POINT('Ctrl Pts',(-112.708892347893,-79.5269448909712,
12.7038654758279));
#256626=CARTESIAN_POINT('Ctrl Pts',(-113.819221943657,-78.9602349460102,
12.2445158474711));
#256627=CARTESIAN_POINT('Ctrl Pts',(-113.250441211303,-80.7943836707386,
13.7750080898741));
#256628=CARTESIAN_POINT('Ctrl Pts',(-113.155754679235,-80.5569292865778,
12.6577917414243));
#256629=CARTESIAN_POINT('Ctrl Pts',(-114.058562415706,-80.0929157064321,
12.126254044704));
#256630=CARTESIAN_POINT('Ctrl Pts',(-113.454481346881,-81.3276580610713,
13.6352465336294));
#256631=CARTESIAN_POINT('Ctrl Pts',(-113.36629220308,-81.0885336408403,
12.6062543646709));
#256632=CARTESIAN_POINT('Ctrl Pts',(-114.168356412835,-80.6668256053674,
12.0563732669971));
#256633=CARTESIAN_POINT('Ctrl Pts',(-113.823925897864,-82.40113398131,13.3246442856477));
#256634=CARTESIAN_POINT('Ctrl Pts',(-113.748604057333,-82.1657264091644,
12.4584071352229));
#256635=CARTESIAN_POINT('Ctrl Pts',(-114.367154525562,-81.8221003906434,
11.9010721426414));
#256636=CARTESIAN_POINT('Ctrl Pts',(-113.98827163761,-82.9379109315738,
13.1548625963718));
#256637=CARTESIAN_POINT('Ctrl Pts',(-113.921920427826,-82.7112571397905,
12.3636877604088));
#256638=CARTESIAN_POINT('Ctrl Pts',(-114.455588968267,-82.3997797445818,
11.816181298279));
#256639=CARTESIAN_POINT('Ctrl Pts',(-114.424380779002,-84.5510793506422,
12.6139948970922));
#256640=CARTESIAN_POINT('Ctrl Pts',(-114.375512716323,-84.3341564328201,
12.038418363568));
#256641=CARTESIAN_POINT('Ctrl Pts',(-114.690259297043,-84.1358715971169,
11.54574744836));
#256642=CARTESIAN_POINT('Ctrl Pts',(-114.639636039158,-85.6303497382741,
12.2118226911422));
#256643=CARTESIAN_POINT('Ctrl Pts',(-114.611553326324,-85.4594058856993,
11.7583160303668));
#256644=CARTESIAN_POINT('Ctrl Pts',(-114.806088152744,-85.29738238833,11.3446613455963));
#256645=CARTESIAN_POINT('Ctrl Pts',(-114.927844409463,-87.8072663979446,
11.3656205182426));
#256646=CARTESIAN_POINT('Ctrl Pts',(-114.920352198467,-87.7104675830925,
11.1472581448895));
#256647=CARTESIAN_POINT('Ctrl Pts',(-114.961173076659,-87.6401800974686,
10.9215602590961));
#256648=CARTESIAN_POINT('Ctrl Pts',(-115.,-88.9061071730177,10.920509802988));
#256649=CARTESIAN_POINT('Ctrl Pts',(-115.,-88.8644746746409,10.8097442388105));
#256650=CARTESIAN_POINT('Ctrl Pts',(-115.,-88.8227423398907,10.6990068206168));
#256651=CARTESIAN_POINT('Ctrl Pts',(-115.,-90.,10.4775));
#256652=CARTESIAN_POINT('Ctrl Pts',(-115.,-90.,10.4775));
#256653=CARTESIAN_POINT('Ctrl Pts',(-115.,-90.,10.4775));
#256654=CARTESIAN_POINT('Ctrl Pts',(-115.,-90.,10.4775));
#256655=CARTESIAN_POINT('Ctrl Pts',(-115.,-89.5835438332465,10.555858276654));
#256656=CARTESIAN_POINT('Ctrl Pts',(-114.995145444666,-89.1669828265304,
10.6342451263498));
#256657=CARTESIAN_POINT('Ctrl Pts',(-114.985453755838,-88.7504746468455,
10.7122315127108));
#256658=CARTESIAN_POINT('Ctrl Pts',(-114.976119162398,-88.3493129308016,
10.7873444495187));
#256659=CARTESIAN_POINT('Ctrl Pts',(-114.96229720558,-87.9481990724496,
10.8620867505366));
#256660=CARTESIAN_POINT('Ctrl Pts',(-114.943957244205,-87.5472762374291,
10.9360757299152));
#256661=CARTESIAN_POINT('Ctrl Pts',(-114.928389631906,-87.2069586582444,
10.9988802103514));
#256662=CARTESIAN_POINT('Ctrl Pts',(-114.909565993928,-86.866778387987,
11.0611422128609));
#256663=CARTESIAN_POINT('Ctrl Pts',(-114.887440575962,-86.526833310487,
11.1226211406024));
#256664=CARTESIAN_POINT('Ctrl Pts',(-114.886181080275,-86.5074818406292,
11.1261208459838));
#256665=CARTESIAN_POINT('Ctrl Pts',(-114.884910894891,-86.4881313431672,
11.1296179650603));
#256666=CARTESIAN_POINT('Ctrl Pts',(-114.883630015071,-86.4687819131643,
11.1331124382533));
#256667=CARTESIAN_POINT('Ctrl Pts',(-114.846004723596,-85.9004007638864,
11.2357610790281));
#256668=CARTESIAN_POINT('Ctrl Pts',(-114.799248326424,-85.3326432827608,
11.3362547894284));
#256669=CARTESIAN_POINT('Ctrl Pts',(-114.742990120853,-84.7653562148494,
11.4332724000518));
#256670=CARTESIAN_POINT('Ctrl Pts',(-114.686731915283,-84.198069146938,
11.5302900106753));
#256671=CARTESIAN_POINT('Ctrl Pts',(-114.620971648891,-83.631251746912,
11.6238302836068));
#256672=CARTESIAN_POINT('Ctrl Pts',(-114.545392304676,-83.0647232345978,
11.7125671552059));
#256673=CARTESIAN_POINT('Ctrl Pts',(-114.541556460865,-83.035970472709,
11.7170707769731));
#256674=CARTESIAN_POINT('Ctrl Pts',(-114.537695858892,-83.0072223038153,
11.7215614148308));
#256675=CARTESIAN_POINT('Ctrl Pts',(-114.533810424182,-82.9784782793166,
11.7260389714718));
#256676=CARTESIAN_POINT('Ctrl Pts',(-114.489984433171,-82.6542583519608,
11.7765438368893));
#256677=CARTESIAN_POINT('Ctrl Pts',(-114.442984724914,-82.3305619486271,
11.8253691505752));
#256678=CARTESIAN_POINT('Ctrl Pts',(-114.392600666854,-82.006702692197,
11.872241524874));
#256679=CARTESIAN_POINT('Ctrl Pts',(-114.353105212467,-81.7528333338633,
11.9089842127871));
#256680=CARTESIAN_POINT('Ctrl Pts',(-114.311529402513,-81.4988640708449,
11.9445266216457));
#256681=CARTESIAN_POINT('Ctrl Pts',(-114.26775287008,-81.2444644384056,
11.9787247352559));
#256682=CARTESIAN_POINT('Ctrl Pts',(-114.218759079456,-80.9597456259818,
12.0169985574342));
#256683=CARTESIAN_POINT('Ctrl Pts',(-114.167147236446,-80.6753810397809,
12.0534610877905));
#256684=CARTESIAN_POINT('Ctrl Pts',(-114.112878627073,-80.3915054831543,
12.0877657415112));
#256685=CARTESIAN_POINT('Ctrl Pts',(-114.063190185782,-80.1315884870837,
12.1191751472815));
#256686=CARTESIAN_POINT('Ctrl Pts',(-114.01127419479,-79.8720812257873,
12.1487756059742));
#256687=CARTESIAN_POINT('Ctrl Pts',(-113.957084553584,-79.6131099264375,
12.1762747511387));
#256688=CARTESIAN_POINT('Ctrl Pts',(-113.951047381323,-79.5842583911624,
12.1793383823547));
#256689=CARTESIAN_POINT('Ctrl Pts',(-113.944982071644,-79.5554139374352,
12.182375852651));
#256690=CARTESIAN_POINT('Ctrl Pts',(-113.938888643004,-79.5265771857679,
12.1853866936199));
#256691=CARTESIAN_POINT('Ctrl Pts',(-113.860425331499,-79.1552547066897,
12.2241564186424));
#256692=CARTESIAN_POINT('Ctrl Pts',(-113.777204059993,-78.7846328270462,
12.2586195275573));
#256693=CARTESIAN_POINT('Ctrl Pts',(-113.6889670557,-78.414748386036,12.28755991895));
#256694=CARTESIAN_POINT('Ctrl Pts',(-113.643662573429,-78.224834605143,
12.3024190980355));
#256695=CARTESIAN_POINT('Ctrl Pts',(-113.597035870615,-78.0351149342934,
12.3158215393037));
#256696=CARTESIAN_POINT('Ctrl Pts',(-113.549052337867,-77.8455925411286,
12.3275976932327));
#256697=CARTESIAN_POINT('Ctrl Pts',(-113.46604398788,-77.5177312887046,
12.3479696635915));
#256698=CARTESIAN_POINT('Ctrl Pts',(-113.378979813672,-77.1904629060852,
12.3635332048232));
#256699=CARTESIAN_POINT('Ctrl Pts',(-113.28758078223,-76.8637289605696,
12.3728032157761));
#256700=CARTESIAN_POINT('Ctrl Pts',(-113.225421577863,-76.6415217689565,
12.3791076207157));
#256701=CARTESIAN_POINT('Ctrl Pts',(-113.161257371592,-76.4195614756949,
12.3825));
#256702=CARTESIAN_POINT('Ctrl Pts',(-113.095,-76.1978262581577,12.3825));
#256703=CARTESIAN_POINT('Origin',(-112.039285751595,74.5679259799751,14.2875));
#256704=CARTESIAN_POINT('Origin',(-112.039285751595,74.5679259799751,14.2875));
#256705=CARTESIAN_POINT('Origin',(-113.095,0.,10.4775));
#256706=CARTESIAN_POINT('Ctrl Pts',(-115.,90.,10.4775));
#256707=CARTESIAN_POINT('Ctrl Pts',(-115.,89.5835438332466,10.555858276654));
#256708=CARTESIAN_POINT('Ctrl Pts',(-114.995145444666,89.1669828265306,
10.6342451263498));
#256709=CARTESIAN_POINT('Ctrl Pts',(-114.985453755838,88.7504746468457,
10.7122315127108));
#256710=CARTESIAN_POINT('Ctrl Pts',(-114.976119162398,88.3493129308021,
10.7873444495186));
#256711=CARTESIAN_POINT('Ctrl Pts',(-114.96229720558,87.9481990724504,10.8620867505365));
#256712=CARTESIAN_POINT('Ctrl Pts',(-114.943957244205,87.5472762374302,
10.936075729915));
#256713=CARTESIAN_POINT('Ctrl Pts',(-114.928389631906,87.2069586582452,
10.9988802103513));
#256714=CARTESIAN_POINT('Ctrl Pts',(-114.909565993928,86.8667783879873,
11.0611422128609));
#256715=CARTESIAN_POINT('Ctrl Pts',(-114.887440575962,86.526833310487,11.1226211406024));
#256716=CARTESIAN_POINT('Ctrl Pts',(-114.886181080275,86.5074818406292,
11.1261208459838));
#256717=CARTESIAN_POINT('Ctrl Pts',(-114.884910894891,86.4881313431672,
11.1296179650603));
#256718=CARTESIAN_POINT('Ctrl Pts',(-114.883630015071,86.4687819131643,
11.1331124382533));
#256719=CARTESIAN_POINT('Ctrl Pts',(-114.846004723596,85.9004007638865,
11.2357610790281));
#256720=CARTESIAN_POINT('Ctrl Pts',(-114.799248326424,85.3326432827608,
11.3362547894284));
#256721=CARTESIAN_POINT('Ctrl Pts',(-114.742990120853,84.7653562148494,
11.4332724000518));
#256722=CARTESIAN_POINT('Ctrl Pts',(-114.686731915283,84.198069146938,11.5302900106753));
#256723=CARTESIAN_POINT('Ctrl Pts',(-114.620971648891,83.631251746912,11.6238302836068));
#256724=CARTESIAN_POINT('Ctrl Pts',(-114.545392304676,83.0647232345978,
11.7125671552059));
#256725=CARTESIAN_POINT('Ctrl Pts',(-114.541556460865,83.0359704727091,
11.7170707769731));
#256726=CARTESIAN_POINT('Ctrl Pts',(-114.537695858892,83.0072223038154,
11.7215614148308));
#256727=CARTESIAN_POINT('Ctrl Pts',(-114.533810424182,82.9784782793166,
11.7260389714718));
#256728=CARTESIAN_POINT('Ctrl Pts',(-114.489984433171,82.6542583519613,
11.7765438368892));
#256729=CARTESIAN_POINT('Ctrl Pts',(-114.442984724914,82.3305619486281,
11.825369150575));
#256730=CARTESIAN_POINT('Ctrl Pts',(-114.392600666854,82.0067026921985,
11.8722415248737));
#256731=CARTESIAN_POINT('Ctrl Pts',(-114.353105212467,81.7528333338643,
11.908984212787));
#256732=CARTESIAN_POINT('Ctrl Pts',(-114.311529402513,81.4988640708454,
11.9445266216456));
#256733=CARTESIAN_POINT('Ctrl Pts',(-114.26775287008,81.2444644384056,11.9787247352559));
#256734=CARTESIAN_POINT('Ctrl Pts',(-114.218759079456,80.9597456259804,
12.0169985574344));
#256735=CARTESIAN_POINT('Ctrl Pts',(-114.167147236445,80.6753810397781,
12.0534610877908));
#256736=CARTESIAN_POINT('Ctrl Pts',(-114.112878627072,80.3915054831501,
12.0877657415118));
#256737=CARTESIAN_POINT('Ctrl Pts',(-114.063190185782,80.131588487081,12.1191751472818));
#256738=CARTESIAN_POINT('Ctrl Pts',(-114.01127419479,79.8720812257858,12.1487756059743));
#256739=CARTESIAN_POINT('Ctrl Pts',(-113.957084553584,79.6131099264375,
12.1762747511387));
#256740=CARTESIAN_POINT('Ctrl Pts',(-113.951047381323,79.5842583911624,
12.1793383823547));
#256741=CARTESIAN_POINT('Ctrl Pts',(-113.944982071644,79.5554139374352,
12.182375852651));
#256742=CARTESIAN_POINT('Ctrl Pts',(-113.938888643004,79.5265771857679,
12.1853866936199));
#256743=CARTESIAN_POINT('Ctrl Pts',(-113.860425331499,79.1552547066895,
12.2241564186425));
#256744=CARTESIAN_POINT('Ctrl Pts',(-113.777204059993,78.7846328270459,
12.2586195275573));
#256745=CARTESIAN_POINT('Ctrl Pts',(-113.6889670557,78.4147483860356,12.2875599189501));
#256746=CARTESIAN_POINT('Ctrl Pts',(-113.643662573429,78.2248346051427,
12.3024190980356));
#256747=CARTESIAN_POINT('Ctrl Pts',(-113.597035870615,78.0351149342933,
12.3158215393037));
#256748=CARTESIAN_POINT('Ctrl Pts',(-113.549052337867,77.8455925411286,
12.3275976932327));
#256749=CARTESIAN_POINT('Ctrl Pts',(-113.466043987881,77.5177312887054,
12.3479696635914));
#256750=CARTESIAN_POINT('Ctrl Pts',(-113.378979813672,77.1904629060869,
12.3635332048232));
#256751=CARTESIAN_POINT('Ctrl Pts',(-113.28758078223,76.8637289605722,12.372803215776));
#256752=CARTESIAN_POINT('Ctrl Pts',(-113.225421577863,76.6415217689582,
12.3791076207157));
#256753=CARTESIAN_POINT('Ctrl Pts',(-113.161257371593,76.4195614756958,
12.3825));
#256754=CARTESIAN_POINT('Ctrl Pts',(-113.095,76.1978262581577,12.3825));
#256755=CARTESIAN_POINT('Origin',(-90.,90.,14.2875));
#256756=CARTESIAN_POINT('Origin',(-113.095,76.1978262581577,14.2875));
#256757=CARTESIAN_POINT('Ctrl Pts',(-113.095,76.1978262581577,12.3825));
#256758=CARTESIAN_POINT('Ctrl Pts',(-111.45976584278,77.1750847966528,12.3825));
#256759=CARTESIAN_POINT('Ctrl Pts',(-111.45976584278,77.1750847966528,14.2875));
#256760=CARTESIAN_POINT('Ctrl Pts',(-113.257643450735,76.7421246518768,
12.3825));
#256761=CARTESIAN_POINT('Ctrl Pts',(-111.710230812091,77.5941846099565,
12.5172751948228));
#256762=CARTESIAN_POINT('Ctrl Pts',(-111.762015741049,77.6808356682973,
14.2874999966875));
#256763=CARTESIAN_POINT('Ctrl Pts',(-113.408657903693,77.2910619607747,
12.3620536717506));
#256764=CARTESIAN_POINT('Ctrl Pts',(-111.971409284934,78.0590963418208,
12.605351768751));
#256765=CARTESIAN_POINT('Ctrl Pts',(-112.042664753069,78.1909142917078,
14.2466073426301));
#256766=CARTESIAN_POINT('Ctrl Pts',(-113.689453561682,78.4001194763425,
12.2931400483747));
#256767=CARTESIAN_POINT('Ctrl Pts',(-112.468920289911,79.0242905953405,
12.6961322557715));
#256768=CARTESIAN_POINT('Ctrl Pts',(-112.56449277411,79.221445341369,14.1087800976205));
#256769=CARTESIAN_POINT('Ctrl Pts',(-113.819221943657,78.9602349460102,
12.2445158474711));
#256770=CARTESIAN_POINT('Ctrl Pts',(-112.708892347893,79.5269448909712,
12.7038654758279));
#256771=CARTESIAN_POINT('Ctrl Pts',(-112.805653119421,79.741902012631,14.0115316944761));
#256772=CARTESIAN_POINT('Ctrl Pts',(-114.058562415706,80.0929157064321,
12.126254044704));
#256773=CARTESIAN_POINT('Ctrl Pts',(-113.155754679235,80.5569292865778,
12.6577917414243));
#256774=CARTESIAN_POINT('Ctrl Pts',(-113.250441211303,80.7943836707386,
13.7750080898741));
#256775=CARTESIAN_POINT('Ctrl Pts',(-114.168356412835,80.6668256053674,
12.0563732669971));
#256776=CARTESIAN_POINT('Ctrl Pts',(-113.36629220308,81.0885336408403,12.6062543646709));
#256777=CARTESIAN_POINT('Ctrl Pts',(-113.454481346881,81.3276580610713,
13.6352465336294));
#256778=CARTESIAN_POINT('Ctrl Pts',(-114.367154525562,81.8221003906434,
11.9010721426414));
#256779=CARTESIAN_POINT('Ctrl Pts',(-113.748604057333,82.1657264091644,
12.4584071352229));
#256780=CARTESIAN_POINT('Ctrl Pts',(-113.823925897864,82.40113398131,13.3246442856477));
#256781=CARTESIAN_POINT('Ctrl Pts',(-114.455588968267,82.3997797445818,
11.816181298279));
#256782=CARTESIAN_POINT('Ctrl Pts',(-113.921920427826,82.7112571397905,
12.3636877604088));
#256783=CARTESIAN_POINT('Ctrl Pts',(-113.98827163761,82.9379109315738,13.1548625963718));
#256784=CARTESIAN_POINT('Ctrl Pts',(-114.690259297043,84.1358715971169,
11.54574744836));
#256785=CARTESIAN_POINT('Ctrl Pts',(-114.375512716323,84.3341564328201,
12.038418363568));
#256786=CARTESIAN_POINT('Ctrl Pts',(-114.424380779002,84.5510793506422,
12.6139948970922));
#256787=CARTESIAN_POINT('Ctrl Pts',(-114.806088152744,85.29738238833,11.3446613455963));
#256788=CARTESIAN_POINT('Ctrl Pts',(-114.611553326324,85.4594058856993,
11.7583160303668));
#256789=CARTESIAN_POINT('Ctrl Pts',(-114.639636039158,85.6303497382741,
12.2118226911422));
#256790=CARTESIAN_POINT('Ctrl Pts',(-114.961173076659,87.6401800974686,
10.9215602590961));
#256791=CARTESIAN_POINT('Ctrl Pts',(-114.920352198467,87.7104675830925,
11.1472581448895));
#256792=CARTESIAN_POINT('Ctrl Pts',(-114.927844409463,87.8072663979446,
11.3656205182426));
#256793=CARTESIAN_POINT('Ctrl Pts',(-115.,88.8227423398907,10.6990068206168));
#256794=CARTESIAN_POINT('Ctrl Pts',(-115.,88.8644746746409,10.8097442388105));
#256795=CARTESIAN_POINT('Ctrl Pts',(-115.,88.9061071730177,10.920509802988));
#256796=CARTESIAN_POINT('Ctrl Pts',(-115.,90.,10.4775));
#256797=CARTESIAN_POINT('Ctrl Pts',(-115.,90.,10.4775));
#256798=CARTESIAN_POINT('Ctrl Pts',(-115.,90.,10.4775));
#256799=CARTESIAN_POINT('Origin',(0.,113.095,10.4775));
#256800=CARTESIAN_POINT('Origin',(-20.3338370957106,113.095,10.4775));
#256801=CARTESIAN_POINT('Ctrl Pts',(20.3391723768471,115.,10.4796615646013));
#256802=CARTESIAN_POINT('Ctrl Pts',(19.7022063230879,115.000000000001,12.0516141103967));
#256803=CARTESIAN_POINT('Ctrl Pts',(19.6285538888407,113.315275283147,12.2333790914428));
#256804=CARTESIAN_POINT('Ctrl Pts',(18.7107034466881,115.,9.81979377118478));
#256805=CARTESIAN_POINT('Ctrl Pts',(18.1189784011792,114.999999999841,11.4178986609794));
#256806=CARTESIAN_POINT('Ctrl Pts',(18.0565711864358,113.307258836677,11.5974068452245));
#256807=CARTESIAN_POINT('Ctrl Pts',(17.0532658471793,115.,9.2407677403993));
#256808=CARTESIAN_POINT('Ctrl Pts',(16.5123043069177,115.,10.8637355452915));
#256809=CARTESIAN_POINT('Ctrl Pts',(16.4567953379409,113.300163656376,11.0393495768014));
#256810=CARTESIAN_POINT('Ctrl Pts',(13.7179668220018,115.,8.25237113478313));
#256811=CARTESIAN_POINT('Ctrl Pts',(13.2794521568153,115.,9.91725072790728));
#256812=CARTESIAN_POINT('Ctrl Pts',(13.2377636482649,113.287997034874,10.0867415205811));
#256813=CARTESIAN_POINT('Ctrl Pts',(12.0365764000009,115.,7.84116032508707));
#256814=CARTESIAN_POINT('Ctrl Pts',(11.6512268683337,114.999999999988,9.52405173421115));
#256815=CARTESIAN_POINT('Ctrl Pts',(11.615100586185,113.282903110437,9.69041736234001));
#256816=CARTESIAN_POINT('Ctrl Pts',(6.94924188488841,115.,6.85120498294647));
#256817=CARTESIAN_POINT('Ctrl Pts',(6.71934777368302,115.000000000024,8.57583528434052));
#256818=CARTESIAN_POINT('Ctrl Pts',(6.70566817137969,113.270607871211,8.73629459979534));
#256819=CARTESIAN_POINT('Ctrl Pts',(3.50035936666375,115.,6.51381753263502));
#256820=CARTESIAN_POINT('Ctrl Pts',(3.38780290821946,115.000000000024,8.25451794933572));
#256821=CARTESIAN_POINT('Ctrl Pts',(3.37767114516811,113.266374083612,8.411111618798));
#256822=CARTESIAN_POINT('Ctrl Pts',(-3.51636943826656,115.,6.51485519904957));
#256823=CARTESIAN_POINT('Ctrl Pts',(-3.4032875294127,114.999999999976,8.25551029227645));
#256824=CARTESIAN_POINT('Ctrl Pts',(-3.39312006098893,113.266387061329,
8.41211174275344));
#256825=CARTESIAN_POINT('Ctrl Pts',(-6.96324106057752,115.,6.85321820905684));
#256826=CARTESIAN_POINT('Ctrl Pts',(-6.73290677808119,115.000000000168,
8.57776066608256));
#256827=CARTESIAN_POINT('Ctrl Pts',(-6.71917720241139,113.270632997186,
8.73823497354488));
#256828=CARTESIAN_POINT('Ctrl Pts',(-12.0457199621,115.,7.84329673838536));
#256829=CARTESIAN_POINT('Ctrl Pts',(-11.6600859933304,114.999999999916,
9.52609638746069));
#256830=CARTESIAN_POINT('Ctrl Pts',(-11.6239247024908,113.282929583528,
9.69247643632406));
#256831=CARTESIAN_POINT('Ctrl Pts',(-13.7251356712098,115.,8.25432671895952));
#256832=CARTESIAN_POINT('Ctrl Pts',(-13.2864050182398,114.999999999988,
9.91912443645021));
#256833=CARTESIAN_POINT('Ctrl Pts',(-13.2446823703184,113.288021171429,
10.0886263004162));
#256834=CARTESIAN_POINT('Ctrl Pts',(-17.0557976392124,115.,9.24168756304256));
#256835=CARTESIAN_POINT('Ctrl Pts',(-16.5147655959056,115.000000000012,
10.864618206466));
#256836=CARTESIAN_POINT('Ctrl Pts',(-16.4592390970313,113.300174914246,
11.0402360890187));
#256837=CARTESIAN_POINT('Ctrl Pts',(-18.7092469771287,115.,9.81920401156003));
#256838=CARTESIAN_POINT('Ctrl Pts',(-18.1175604673055,114.999999999804,
11.4173315039314));
#256839=CARTESIAN_POINT('Ctrl Pts',(-18.0551653037824,113.307251671963,
11.596838469021));
#256840=CARTESIAN_POINT('Ctrl Pts',(-20.3391771446538,115.,10.4796634955796));
#256841=CARTESIAN_POINT('Ctrl Pts',(-19.7022109484218,115.000000000001,
12.051615960838));
#256842=CARTESIAN_POINT('Ctrl Pts',(-19.6285584910498,113.315275306605,
12.2333809524079));
#256843=CARTESIAN_POINT('Origin',(20.3338370957106,113.095,10.4775));
#256844=CARTESIAN_POINT('Origin',(-20.3338370957106,113.095,10.4775));
#256845=CARTESIAN_POINT('Origin',(0.,113.095,10.4775));
#256846=CARTESIAN_POINT('Origin',(20.3338370957106,113.095,10.4775));
#256847=CARTESIAN_POINT('Origin',(-24.8661421402461,-44.3927817339206,16.1925));
#256848=CARTESIAN_POINT('Ctrl Pts',(-76.5327353708727,27.1805640649084,
16.1924982582712));
#256849=CARTESIAN_POINT('Ctrl Pts',(-76.5254460991276,27.1701424112581,
16.2200871281663));
#256850=CARTESIAN_POINT('Ctrl Pts',(-76.5184672980905,27.1617293806218,
16.248101336645));
#256851=CARTESIAN_POINT('Ctrl Pts',(-76.5118328073709,27.1555532163276,
16.2765966498027));
#256852=CARTESIAN_POINT('Ctrl Pts',(-76.505358241223,27.1495259286347,16.3044050826943));
#256853=CARTESIAN_POINT('Ctrl Pts',(-76.4992115671826,27.1456288662165,
16.3326717167532));
#256854=CARTESIAN_POINT('Ctrl Pts',(-76.4934339939447,27.144123077721,16.3614476210689));
#256855=CARTESIAN_POINT('Ctrl Pts',(-76.4921585023819,27.1437906508625,
16.3678003615113));
#256856=CARTESIAN_POINT('Ctrl Pts',(-76.4909010391257,27.1435749657779,
16.3741779191892));
#256857=CARTESIAN_POINT('Ctrl Pts',(-76.4896621154026,27.1434791718108,
16.3805808375412));
#256858=CARTESIAN_POINT('Ctrl Pts',(-76.4880193305114,27.1433521511727,
16.3890709627458));
#256859=CARTESIAN_POINT('Ctrl Pts',(-76.486416003788,27.1434370002347,16.3975719419884));
#256860=CARTESIAN_POINT('Ctrl Pts',(-76.4848537692335,27.1437355673519,
16.406076948393));
#256861=CARTESIAN_POINT('Ctrl Pts',(-76.48098548299,27.1444748565121,16.4271363976165));
#256862=CARTESIAN_POINT('Ctrl Pts',(-76.4773696370517,27.1465703673368,
16.4482618838781));
#256863=CARTESIAN_POINT('Ctrl Pts',(-76.4740424808271,27.1499697741393,
16.4691998962322));
#256864=CARTESIAN_POINT('Ctrl Pts',(-76.4707094654665,27.1533751673113,
16.4901747805127));
#256865=CARTESIAN_POINT('Ctrl Pts',(-76.4676662855572,27.15808878871,16.5109605599982));
#256866=CARTESIAN_POINT('Ctrl Pts',(-76.4649378361877,27.1640086579224,
16.5313130815541));
#256867=CARTESIAN_POINT('Ctrl Pts',(-76.4643858787519,27.1652062303853,
16.5354303379478));
#256868=CARTESIAN_POINT('Ctrl Pts',(-76.4638467601764,27.166453014181,16.5395299258882));
#256869=CARTESIAN_POINT('Ctrl Pts',(-76.4633206224266,27.1677479362274,
16.5436099312145));
#256870=CARTESIAN_POINT('Ctrl Pts',(-76.4620493955122,27.1708766601363,
16.5534678298028));
#256871=CARTESIAN_POINT('Ctrl Pts',(-76.4608504005183,27.1742844116283,
16.563227977684));
#256872=CARTESIAN_POINT('Ctrl Pts',(-76.4597221364489,27.1779555862456,
16.5728808843466));
#256873=CARTESIAN_POINT('Ctrl Pts',(-76.4555634683354,27.1914871674015,
16.608460529423));
#256874=CARTESIAN_POINT('Ctrl Pts',(-76.452368326429,27.2085635842065,16.6425190954535));
#256875=CARTESIAN_POINT('Ctrl Pts',(-76.4499894515855,27.2285145118714,
16.6751163767836));
#256876=CARTESIAN_POINT('Ctrl Pts',(-76.4481516192738,27.243927874037,16.7002998525192));
#256877=CARTESIAN_POINT('Ctrl Pts',(-76.4468125093688,27.2611648250175,
16.7246580015644));
#256878=CARTESIAN_POINT('Ctrl Pts',(-76.4459011083305,27.2797726036834,
16.7480930589391));
#256879=CARTESIAN_POINT('Ctrl Pts',(-76.4449881378312,27.2984124255237,
16.7715684722125));
#256880=CARTESIAN_POINT('Ctrl Pts',(-76.4445043286356,27.3184277738337,
16.7941176720264));
#256881=CARTESIAN_POINT('Ctrl Pts',(-76.4443826625376,27.3394063743963,
16.8156722156884));
#256882=CARTESIAN_POINT('Ctrl Pts',(-76.444260240081,27.3605153920852,16.8373607569274));
#256883=CARTESIAN_POINT('Ctrl Pts',(-76.4445044610444,27.3825996603613,
16.8580423102826));
#256884=CARTESIAN_POINT('Ctrl Pts',(-76.4450517552706,27.4052828608609,
16.8776763500028));
#256885=CARTESIAN_POINT('Ctrl Pts',(-76.4451275701148,27.4084250889914,
16.8803961880577));
#256886=CARTESIAN_POINT('Ctrl Pts',(-76.4452092083633,27.4115788786109,
16.8830959690985));
#256887=CARTESIAN_POINT('Ctrl Pts',(-76.4452965083212,27.4147432949496,
16.8857756277876));
#256888=CARTESIAN_POINT('Ctrl Pts',(-76.4456285567621,27.4267792630846,
16.895967803261));
#256889=CARTESIAN_POINT('Ctrl Pts',(-76.4460413746577,27.4390220462592,
16.9059171754194));
#256890=CARTESIAN_POINT('Ctrl Pts',(-76.4465283265827,27.4514363729673,
16.9156217934255));
#256891=CARTESIAN_POINT('Ctrl Pts',(-76.4477740792785,27.4831955265336,
16.9404487905557));
#256892=CARTESIAN_POINT('Ctrl Pts',(-76.4494849825234,27.516130412427,16.9638340074607));
#256893=CARTESIAN_POINT('Ctrl Pts',(-76.4515669382231,27.5499276827806,
16.985939396366));
#256894=CARTESIAN_POINT('Ctrl Pts',(-76.4537247726033,27.5849567239553,
17.0088504353357));
#256895=CARTESIAN_POINT('Ctrl Pts',(-76.4562812377419,27.6209122535191,
17.0303866179463));
#256896=CARTESIAN_POINT('Ctrl Pts',(-76.4591476533543,27.6574962538653,
17.0507077973838));
#256897=CARTESIAN_POINT('Ctrl Pts',(-76.4614800345039,27.6872643839364,
17.0672429905549));
#256898=CARTESIAN_POINT('Ctrl Pts',(-76.464017965945,27.7174496690713,17.0829733141292));
#256899=CARTESIAN_POINT('Ctrl Pts',(-76.466720752886,27.7479141287996,17.0979758062082));
#256900=CARTESIAN_POINT('Ctrl Pts',(-76.4677059340771,27.7590185974006,
17.1034442997812));
#256901=CARTESIAN_POINT('Ctrl Pts',(-76.4687146852109,27.7701762979155,
17.1088237343903));
#256902=CARTESIAN_POINT('Ctrl Pts',(-76.4697457322936,27.7813854912832,
17.1141186859287));
#256903=CARTESIAN_POINT('Ctrl Pts',(-76.4724297283712,27.8105649841858,
17.1279023718521));
#256904=CARTESIAN_POINT('Ctrl Pts',(-76.475268656545,27.8401032155328,17.1410999474322));
#256905=CARTESIAN_POINT('Ctrl Pts',(-76.4782264005115,27.8698177823024,
17.1537242053269));
#256906=CARTESIAN_POINT('Ctrl Pts',(-76.4814236442207,27.9019384502015,
17.1673706972462));
#256907=CARTESIAN_POINT('Ctrl Pts',(-76.4847597640874,27.9342655910912,
17.1803475370963));
#256908=CARTESIAN_POINT('Ctrl Pts',(-76.4881996908383,27.9666279531715,
17.1926699656454));
#256909=CARTESIAN_POINT('Ctrl Pts',(-76.4886519862316,27.9708830865932,
17.1942901680715));
#256910=CARTESIAN_POINT('Ctrl Pts',(-76.489106089515,27.9751389006332,17.1958990522149));
#256911=CARTESIAN_POINT('Ctrl Pts',(-76.4895619325382,27.979395067814,17.1974966476084));
#256912=CARTESIAN_POINT('Ctrl Pts',(-76.493897565698,28.019876502485,17.2126917634966));
#256913=CARTESIAN_POINT('Ctrl Pts',(-76.4984031419556,28.0605401920071,
17.2269450615766));
#256914=CARTESIAN_POINT('Ctrl Pts',(-76.5030665766358,28.1015001037827,
17.240414641407));
#256915=CARTESIAN_POINT('Ctrl Pts',(-76.5035084491037,28.1053811611021,
17.2416909188482));
#256916=CARTESIAN_POINT('Ctrl Pts',(-76.5039517474129,28.1092649053718,
17.2429601347068));
#256917=CARTESIAN_POINT('Ctrl Pts',(-76.5043964665195,28.1131514503917,
17.2442224078976));
#256918=CARTESIAN_POINT('Ctrl Pts',(-76.5073626095466,28.1390735397254,
17.2526413914031));
#256919=CARTESIAN_POINT('Ctrl Pts',(-76.5103875491063,28.1650771837688,
17.2607374323177));
#256920=CARTESIAN_POINT('Ctrl Pts',(-76.5134649041893,28.1911518975641,
17.2685330721676));
#256921=CARTESIAN_POINT('Ctrl Pts',(-76.5205941289253,28.2515584770983,
17.2865930187622));
#256922=CARTESIAN_POINT('Ctrl Pts',(-76.5280003771988,28.3123340561993,
17.3030517999703));
#256923=CARTESIAN_POINT('Ctrl Pts',(-76.5356394395758,28.3734477221374,
17.3181020342891));
#256924=CARTESIAN_POINT('Ctrl Pts',(-76.5435634587841,28.4368410862557,
17.3337136813665));
#256925=CARTESIAN_POINT('Ctrl Pts',(-76.5517380600726,28.5005983551872,
17.3478096641772));
#256926=CARTESIAN_POINT('Ctrl Pts',(-76.5601276442959,28.5647256403924,
17.3605684034646));
#256927=CARTESIAN_POINT('Ctrl Pts',(-76.5638310436267,28.5930332345229,
17.3662004711906));
#256928=CARTESIAN_POINT('Ctrl Pts',(-76.5675765027121,28.6214134362392,
17.3715715053251));
#256929=CARTESIAN_POINT('Ctrl Pts',(-76.5713617072229,28.6498690551227,
17.3766947662572));
#256930=CARTESIAN_POINT('Ctrl Pts',(-76.57901301,28.7073884190481,17.3870507775338));
#256931=CARTESIAN_POINT('Ctrl Pts',(-76.586835094676,28.7652559669882,17.396373658365));
#256932=CARTESIAN_POINT('Ctrl Pts',(-76.5947786108432,28.8232282288209,
17.4047210505559));
#256933=CARTESIAN_POINT('Ctrl Pts',(-76.5971621660813,28.8406235592321,
17.4072257940426));
#256934=CARTESIAN_POINT('Ctrl Pts',(-76.5995567234879,28.8580286627605,
17.4096426038263));
#256935=CARTESIAN_POINT('Ctrl Pts',(-76.6019611150693,28.8754377812504,
17.4119727726841));
#256936=CARTESIAN_POINT('Ctrl Pts',(-76.6127354792386,28.9534501083324,
17.4224145360162));
#256937=CARTESIAN_POINT('Ctrl Pts',(-76.6237599571578,29.0319245446931,
17.4311687491798));
#256938=CARTESIAN_POINT('Ctrl Pts',(-76.6349137015724,29.1101764698682,
17.4382612976214));
#256939=CARTESIAN_POINT('Ctrl Pts',(-76.6366048959584,29.122041473371,17.4393367102955));
#256940=CARTESIAN_POINT('Ctrl Pts',(-76.6382990798901,29.1339014546392,
17.4403739004344));
#256941=CARTESIAN_POINT('Ctrl Pts',(-76.639995850247,29.1457541224831,17.441372936404));
#256942=CARTESIAN_POINT('Ctrl Pts',(-76.6556847858336,29.2553480587374,
17.4506103744062));
#256943=CARTESIAN_POINT('Ctrl Pts',(-76.6716864104207,29.3650148910396,
17.4567325787359));
#256944=CARTESIAN_POINT('Ctrl Pts',(-76.6879909658038,29.4748980638179,
17.4599100505192));
#256945=CARTESIAN_POINT('Ctrl Pts',(-76.6968876072708,29.5348562269499,
17.4616438498508));
#256946=CARTESIAN_POINT('Ctrl Pts',(-76.7058745787282,29.5948790592221,
17.4625));
#256947=CARTESIAN_POINT('Ctrl Pts',(-76.7149512087496,29.6549915892152,
17.4625));
#256948=CARTESIAN_POINT('Origin',(-109.438478010978,76.3890311653897,16.1925));
#256949=CARTESIAN_POINT('Origin',(-90.,90.,16.1925));
#256950=CARTESIAN_POINT('Origin',(-76.3890311653897,109.438478010978,16.1925));
#256951=CARTESIAN_POINT('Origin',(8.18330470534211,50.220290910288,16.1925));
#256952=CARTESIAN_POINT('Ctrl Pts',(-29.6549915892152,76.7149512087496,
17.4625));
#256953=CARTESIAN_POINT('Ctrl Pts',(-29.5784809832296,76.7033985679885,
17.4625));
#256954=CARTESIAN_POINT('Ctrl Pts',(-29.5017645218694,76.691941913157,17.4610789773399));
#256955=CARTESIAN_POINT('Ctrl Pts',(-29.4251260133419,76.6806292437895,
17.4582328812589));
#256956=CARTESIAN_POINT('Ctrl Pts',(-29.3550776153572,76.6702893457232,
17.4556315196873));
#256957=CARTESIAN_POINT('Ctrl Pts',(-29.285091738834,76.6600693732902,17.451839079296));
#256958=CARTESIAN_POINT('Ctrl Pts',(-29.2153959726543,76.6500111634965,
17.4468147853482));
#256959=CARTESIAN_POINT('Ctrl Pts',(-29.1910127660868,76.6464922781962,
17.4450570258185));
#256960=CARTESIAN_POINT('Ctrl Pts',(-29.166665340607,76.6429932651686,17.4431481665627));
#256961=CARTESIAN_POINT('Ctrl Pts',(-29.1423646235815,76.6395162005647,
17.4410854028152));
#256962=CARTESIAN_POINT('Ctrl Pts',(-29.0717236083887,76.6294085410561,
17.4350890478487));
#256963=CARTESIAN_POINT('Ctrl Pts',(-29.0013000923889,76.619457001758,17.427816532758));
#256964=CARTESIAN_POINT('Ctrl Pts',(-28.9308900430927,76.6096539020088,
17.4191389458403));
#256965=CARTESIAN_POINT('Ctrl Pts',(-28.9125941999739,76.6071065955251,
17.4168841005379));
#256966=CARTESIAN_POINT('Ctrl Pts',(-28.894299397661,76.6045693606064,17.4145341520301));
#256967=CARTESIAN_POINT('Ctrl Pts',(-28.8760023419532,76.6020421698847,
17.4120863380179));
#256968=CARTESIAN_POINT('Ctrl Pts',(-28.8096307852525,76.5928749254407,
17.4032070281935));
#256969=CARTESIAN_POINT('Ctrl Pts',(-28.7435548276785,76.5838841660449,
17.3930871840631));
#256970=CARTESIAN_POINT('Ctrl Pts',(-28.6775616925957,76.5750605976978,
17.3815966638215));
#256971=CARTESIAN_POINT('Ctrl Pts',(-28.6679863743367,76.5737803361221,
17.3799294390694));
#256972=CARTESIAN_POINT('Ctrl Pts',(-28.6584128434657,76.5725036108741,
17.378233281295));
#256973=CARTESIAN_POINT('Ctrl Pts',(-28.6488404954756,76.5712304108411,
17.3765077138037));
#256974=CARTESIAN_POINT('Ctrl Pts',(-28.593919594324,76.5639254848986,17.3666073506202));
#256975=CARTESIAN_POINT('Ctrl Pts',(-28.5390197213121,76.5567364098792,
17.3557157603928));
#256976=CARTESIAN_POINT('Ctrl Pts',(-28.4842809217466,76.5497009035207,
17.3437734778876));
#256977=CARTESIAN_POINT('Ctrl Pts',(-28.4340312118297,76.5432423739871,
17.3328105733957));
#256978=CARTESIAN_POINT('Ctrl Pts',(-28.3839169544335,76.5369132259073,
17.3209620182621));
#256979=CARTESIAN_POINT('Ctrl Pts',(-28.3340851368407,76.5307511868738,
17.3081680846677));
#256980=CARTESIAN_POINT('Ctrl Pts',(-28.2843811713795,76.5246049576154,
17.2954069761187));
#256981=CARTESIAN_POINT('Ctrl Pts',(-28.2349573707625,76.5186248279345,
17.2817053136026));
#256982=CARTESIAN_POINT('Ctrl Pts',(-28.1860085131815,76.5128586176739,
17.2669910566473));
#256983=CARTESIAN_POINT('Ctrl Pts',(-28.1614764636036,76.5099687247739,
17.2596166070898));
#256984=CARTESIAN_POINT('Ctrl Pts',(-28.1370017452464,76.5071248960929,
17.2519719554797));
#256985=CARTESIAN_POINT('Ctrl Pts',(-28.1126036317571,76.5043336151744,
17.2440428740804));
#256986=CARTESIAN_POINT('Ctrl Pts',(-28.0701844846433,76.4994806270133,
17.2302571823916));
#256987=CARTESIAN_POINT('Ctrl Pts',(-28.0279824912822,76.4947829028992,
17.2156101298164));
#256988=CARTESIAN_POINT('Ctrl Pts',(-27.9860694428053,76.4902767919903,
17.1999930540297));
#256989=CARTESIAN_POINT('Ctrl Pts',(-27.9466341480602,76.4860370666946,
17.1852992054769));
#256990=CARTESIAN_POINT('Ctrl Pts',(-27.9074544475538,76.4819669295096,
17.1697465428278));
#256991=CARTESIAN_POINT('Ctrl Pts',(-27.8686308801042,76.4781067108578,
17.1532283189415));
#256992=CARTESIAN_POINT('Ctrl Pts',(-27.8377621230887,76.4750374372332,
17.1400946201867));
#256993=CARTESIAN_POINT('Ctrl Pts',(-27.8071191438753,76.4721010301325,
17.1263502154765));
#256994=CARTESIAN_POINT('Ctrl Pts',(-27.7767742650347,76.4693230827018,
17.1119338317452));
#256995=CARTESIAN_POINT('Ctrl Pts',(-27.7671845095149,76.468445180475,17.1073778868627));
#256996=CARTESIAN_POINT('Ctrl Pts',(-27.7576382281078,76.4675842490496,
17.1027621986441));
#256997=CARTESIAN_POINT('Ctrl Pts',(-27.7481373827153,76.4667411216781,
17.09808459864));
#256998=CARTESIAN_POINT('Ctrl Pts',(-27.7165349284568,76.4639366455401,
17.0825256000386));
#256999=CARTESIAN_POINT('Ctrl Pts',(-27.6854146210792,76.4613252274428,
17.0662758428328));
#257000=CARTESIAN_POINT('Ctrl Pts',(-27.6548074136641,76.4589379212242,
17.0492104485405));
#257001=CARTESIAN_POINT('Ctrl Pts',(-27.625042367409,76.4566163020363,17.0326146107177));
#257002=CARTESIAN_POINT('Ctrl Pts',(-27.5957623497434,76.454506551362,17.0152474880124));
#257003=CARTESIAN_POINT('Ctrl Pts',(-27.5670390174753,76.452649048605,16.9969759720338));
#257004=CARTESIAN_POINT('Ctrl Pts',(-27.5394891827037,76.4508674344954,
16.9794509425025));
#257005=CARTESIAN_POINT('Ctrl Pts',(-27.5124513532677,76.4493178278093,
16.9610939515221));
#257006=CARTESIAN_POINT('Ctrl Pts',(-27.4860313730106,76.448047775168,16.9417696634665));
#257007=CARTESIAN_POINT('Ctrl Pts',(-27.4732138949936,76.4474316175612,
16.9323946134121));
#257008=CARTESIAN_POINT('Ctrl Pts',(-27.4605425003863,76.4468814440248,
16.9227916184912));
#257009=CARTESIAN_POINT('Ctrl Pts',(-27.4480332789737,76.4464038210197,
16.9129435541772));
#257010=CARTESIAN_POINT('Ctrl Pts',(-27.4380190788527,76.4460214621024,
16.9050597312283));
#257011=CARTESIAN_POINT('Ctrl Pts',(-27.4281096389904,76.4456876024437,
16.8970089022855));
#257012=CARTESIAN_POINT('Ctrl Pts',(-27.4183213434193,76.4454060812474,
16.8887879984481));
#257013=CARTESIAN_POINT('Ctrl Pts',(-27.3952254081718,76.4447418189892,
16.8693903963502));
#257014=CARTESIAN_POINT('Ctrl Pts',(-27.3726021898248,76.4443701445099,
16.8488671319362));
#257015=CARTESIAN_POINT('Ctrl Pts',(-27.3508659753904,76.4443625463772,
16.8272552303239));
#257016=CARTESIAN_POINT('Ctrl Pts',(-27.3290708073427,76.4443549276367,
16.8055847122633));
#257017=CARTESIAN_POINT('Ctrl Pts',(-27.3081675781444,76.444713403402,16.7828195227726));
#257018=CARTESIAN_POINT('Ctrl Pts',(-27.2886142275261,76.4455134941472,
16.7590305375609));
#257019=CARTESIAN_POINT('Ctrl Pts',(-27.2688420650392,76.4463225383119,
16.7349753415904));
#257020=CARTESIAN_POINT('Ctrl Pts',(-27.2504503195707,76.4475831876966,
16.7098732026395));
#257021=CARTESIAN_POINT('Ctrl Pts',(-27.2339516170994,76.4493763637578,
16.6838334537733));
#257022=CARTESIAN_POINT('Ctrl Pts',(-27.2316065629565,76.4496312380401,
16.680132276601));
#257023=CARTESIAN_POINT('Ctrl Pts',(-27.2292998143515,76.4498968745499,
16.676412217469));
#257024=CARTESIAN_POINT('Ctrl Pts',(-27.2270329030597,76.4501735092113,
16.6726736500796));
#257025=CARTESIAN_POINT('Ctrl Pts',(-27.2082942415873,76.4524602168075,
16.6417700373291));
#257026=CARTESIAN_POINT('Ctrl Pts',(-27.1920956821034,76.4554866376469,
16.6094802657883));
#257027=CARTESIAN_POINT('Ctrl Pts',(-27.1790613975837,76.4593868180785,
16.5757650534976));
#257028=CARTESIAN_POINT('Ctrl Pts',(-27.1746643707654,76.4607025172968,
16.5643914570105));
#257029=CARTESIAN_POINT('Ctrl Pts',(-27.1706359107513,76.4621156292997,
16.5528759158128));
#257030=CARTESIAN_POINT('Ctrl Pts',(-27.1669986019352,76.4636289044872,
16.541229334737));
#257031=CARTESIAN_POINT('Ctrl Pts',(-27.1600415068138,76.4665233519912,
16.5189528725284));
#257032=CARTESIAN_POINT('Ctrl Pts',(-27.1545628735558,76.4697851638502,
16.4962407115116));
#257033=CARTESIAN_POINT('Ctrl Pts',(-27.1506549153929,76.4733862268998,
16.4733464731264));
#257034=CARTESIAN_POINT('Ctrl Pts',(-27.14674695723,76.4769872899494,16.4504522347412));
#257035=CARTESIAN_POINT('Ctrl Pts',(-27.1444098150616,76.4809274578027,
16.4273768616861));
#257036=CARTESIAN_POINT('Ctrl Pts',(-27.1436800109183,76.4851658906467,
16.4043845876077));
#257037=CARTESIAN_POINT('Ctrl Pts',(-27.1434551581826,76.4864717522655,
16.3973006654712));
#257038=CARTESIAN_POINT('Ctrl Pts',(-27.1433783458384,76.4878067469539,
16.3902160073495));
#257039=CARTESIAN_POINT('Ctrl Pts',(-27.1434490350608,76.4891701961808,
16.383133694799));
#257040=CARTESIAN_POINT('Ctrl Pts',(-27.1436556805572,76.4931559613735,
16.3624300013355));
#257041=CARTESIAN_POINT('Ctrl Pts',(-27.1451242300419,76.4973805033892,
16.3417644841304));
#257042=CARTESIAN_POINT('Ctrl Pts',(-27.1478012243608,76.501812217759,16.3212481482302));
#257043=CARTESIAN_POINT('Ctrl Pts',(-27.1505058861726,76.5062897351494,
16.3005197702));
#257044=CARTESIAN_POINT('Ctrl Pts',(-27.1544440119295,76.5109787082553,
16.2799436844039));
#257045=CARTESIAN_POINT('Ctrl Pts',(-27.1595080210178,76.5158361677242,
16.2596351519614));
#257046=CARTESIAN_POINT('Ctrl Pts',(-27.1646853029013,76.520802279844,16.2388723540944));
#257047=CARTESIAN_POINT('Ctrl Pts',(-27.1710392955917,76.525944475937,16.2183892248481));
#257048=CARTESIAN_POINT('Ctrl Pts',(-27.1784017958212,76.531206361274,16.1983095665849));
#257049=CARTESIAN_POINT('Ctrl Pts',(-27.179113452549,76.5317149732923,16.1963686737562));
#257050=CARTESIAN_POINT('Ctrl Pts',(-27.1798344925881,76.5322246958768,
16.194431550985));
#257051=CARTESIAN_POINT('Ctrl Pts',(-27.1805647392023,76.5327354732306,
16.1924983103147));
#257052=CARTESIAN_POINT('Origin',(-128.965117604652,-34.3520449604438,16.1925));
#257053=CARTESIAN_POINT('Ctrl Pts',(27.1805640649112,76.5327353708748,16.1924982582715));
#257054=CARTESIAN_POINT('Ctrl Pts',(27.1701424112491,76.5254460991215,16.2200871281998));
#257055=CARTESIAN_POINT('Ctrl Pts',(27.1617293806052,76.5184672980764,16.2481013367124));
#257056=CARTESIAN_POINT('Ctrl Pts',(27.1555532163089,76.5118328073496,16.2765966499054));
#257057=CARTESIAN_POINT('Ctrl Pts',(27.1495259286137,76.5053582411945,16.3044050828319));
#257058=CARTESIAN_POINT('Ctrl Pts',(27.1456288661985,76.4992115671475,16.3326717169268));
#257059=CARTESIAN_POINT('Ctrl Pts',(27.1441230777122,76.4934339939039,16.36144762128));
#257060=CARTESIAN_POINT('Ctrl Pts',(27.1437906508598,76.4921585023555,16.3678003616526));
#257061=CARTESIAN_POINT('Ctrl Pts',(27.1435749657788,76.4909010391133,16.3741779192602));
#257062=CARTESIAN_POINT('Ctrl Pts',(27.1434791718126,76.4896621154038,16.3805808375413));
#257063=CARTESIAN_POINT('Ctrl Pts',(27.1433521511743,76.4880193305124,16.3890709627459));
#257064=CARTESIAN_POINT('Ctrl Pts',(27.143437000236,76.4864160037888,16.3975719419885));
#257065=CARTESIAN_POINT('Ctrl Pts',(27.1437355673528,76.4848537692341,16.4060769483931));
#257066=CARTESIAN_POINT('Ctrl Pts',(27.1444748565122,76.4809854829899,16.4271363976175));
#257067=CARTESIAN_POINT('Ctrl Pts',(27.1465703673372,76.4773696370516,16.4482618838798));
#257068=CARTESIAN_POINT('Ctrl Pts',(27.1499697741402,76.474042480827,16.4691998962345));
#257069=CARTESIAN_POINT('Ctrl Pts',(27.1533751673143,76.470709465465,16.4901747805256));
#257070=CARTESIAN_POINT('Ctrl Pts',(27.1580887887164,76.4676662855546,16.5109605600215));
#257071=CARTESIAN_POINT('Ctrl Pts',(27.1640086579329,76.4649378361838,16.5313130815873));
#257072=CARTESIAN_POINT('Ctrl Pts',(27.1652062303928,76.4643858787494,16.5354303379699));
#257073=CARTESIAN_POINT('Ctrl Pts',(27.1664530141852,76.4638467601754,16.5395299258992));
#257074=CARTESIAN_POINT('Ctrl Pts',(27.167747936228,76.4633206224269,16.5436099312145));
#257075=CARTESIAN_POINT('Ctrl Pts',(27.1708766601367,76.4620493955123,16.5534678298028));
#257076=CARTESIAN_POINT('Ctrl Pts',(27.1742844116285,76.4608504005184,16.563227977684));
#257077=CARTESIAN_POINT('Ctrl Pts',(27.1779555862458,76.4597221364491,16.5728808843466));
#257078=CARTESIAN_POINT('Ctrl Pts',(27.1914871674018,76.4555634683356,16.6084605294229));
#257079=CARTESIAN_POINT('Ctrl Pts',(27.2085635842082,76.4523683264303,16.6425190954533));
#257080=CARTESIAN_POINT('Ctrl Pts',(27.2285145118719,76.4499894515858,16.6751163767836));
#257081=CARTESIAN_POINT('Ctrl Pts',(27.2439278740326,76.4481516192739,16.7002998525128));
#257082=CARTESIAN_POINT('Ctrl Pts',(27.2611648250078,76.4468125093689,16.724658001552));
#257083=CARTESIAN_POINT('Ctrl Pts',(27.2797726036682,76.4459011083305,16.7480930589212));
#257084=CARTESIAN_POINT('Ctrl Pts',(27.2984124255032,76.4449881378312,16.7715684721892));
#257085=CARTESIAN_POINT('Ctrl Pts',(27.3184277738075,76.4445043286356,16.7941176719983));
#257086=CARTESIAN_POINT('Ctrl Pts',(27.3394063743642,76.4443826625374,16.8156722156559));
#257087=CARTESIAN_POINT('Ctrl Pts',(27.3605153920477,76.4442602400808,16.8373607568908));
#257088=CARTESIAN_POINT('Ctrl Pts',(27.382599660318,76.444504461044,16.8580423102425));
#257089=CARTESIAN_POINT('Ctrl Pts',(27.4052828608116,76.4450517552697,16.8776763499597));
#257090=CARTESIAN_POINT('Ctrl Pts',(27.4084250889586,76.4451275701143,16.8803961880292));
#257091=CARTESIAN_POINT('Ctrl Pts',(27.4115788785947,76.4452092083632,16.8830959690843));
#257092=CARTESIAN_POINT('Ctrl Pts',(27.41474329495,76.4452965083216,16.8857756277874));
#257093=CARTESIAN_POINT('Ctrl Pts',(27.4267792630851,76.4456285567625,16.8959678032609));
#257094=CARTESIAN_POINT('Ctrl Pts',(27.4390220462597,76.4460413746582,16.9059171754193));
#257095=CARTESIAN_POINT('Ctrl Pts',(27.451436372968,76.4465283265831,16.9156217934254));
#257096=CARTESIAN_POINT('Ctrl Pts',(27.4831955265518,76.4477740792797,16.9404487905693));
#257097=CARTESIAN_POINT('Ctrl Pts',(27.5161304124639,76.4494849825256,16.9638340074865));
#257098=CARTESIAN_POINT('Ctrl Pts',(27.549927682837,76.4515669382265,16.9859393964028));
#257099=CARTESIAN_POINT('Ctrl Pts',(27.5849567240302,76.453724772608,17.0088504353828));
#257100=CARTESIAN_POINT('Ctrl Pts',(27.6209122536133,76.4562812377481,17.0303866180024));
#257101=CARTESIAN_POINT('Ctrl Pts',(27.6574962539793,76.4591476533624,17.0507077974477));
#257102=CARTESIAN_POINT('Ctrl Pts',(27.6872643840131,76.4614800345095,17.0672429905956));
#257103=CARTESIAN_POINT('Ctrl Pts',(27.7174496691097,76.4640179659475,17.0829733141488));
#257104=CARTESIAN_POINT('Ctrl Pts',(27.747914128799,76.4667207528852,17.0979758062085));
#257105=CARTESIAN_POINT('Ctrl Pts',(27.7590185974001,76.4677059340764,17.1034442997815));
#257106=CARTESIAN_POINT('Ctrl Pts',(27.7701762979151,76.4687146852103,17.1088237343905));
#257107=CARTESIAN_POINT('Ctrl Pts',(27.7813854912829,76.4697457322932,17.1141186859289));
#257108=CARTESIAN_POINT('Ctrl Pts',(27.8105649841802,76.4724297283706,17.1279023718495));
#257109=CARTESIAN_POINT('Ctrl Pts',(27.8401032155219,76.4752686565441,17.1410999474272));
#257110=CARTESIAN_POINT('Ctrl Pts',(27.8698177822859,76.47822640051,17.1537242053197));
#257111=CARTESIAN_POINT('Ctrl Pts',(27.9019384501796,76.4814236442187,17.167370697237));
#257112=CARTESIAN_POINT('Ctrl Pts',(27.9342655910636,76.4847597640845,17.1803475370853));
#257113=CARTESIAN_POINT('Ctrl Pts',(27.9666279531374,76.4881996908344,17.1926699656325));
#257114=CARTESIAN_POINT('Ctrl Pts',(27.9708830865704,76.4886519862289,17.194290168063));
#257115=CARTESIAN_POINT('Ctrl Pts',(27.9751389006218,76.4891060895135,17.1958990522108));
#257116=CARTESIAN_POINT('Ctrl Pts',(27.9793950678139,76.4895619325379,17.1974966476085));
#257117=CARTESIAN_POINT('Ctrl Pts',(28.019876502463,76.4938975656951,17.2126917634887));
#257118=CARTESIAN_POINT('Ctrl Pts',(28.0605401919643,76.4984031419506,17.2269450615618));
#257119=CARTESIAN_POINT('Ctrl Pts',(28.1015001037186,76.5030665766283,17.2404146413861));
#257120=CARTESIAN_POINT('Ctrl Pts',(28.1053811610594,76.5035084490985,17.2416909188343));
#257121=CARTESIAN_POINT('Ctrl Pts',(28.1092649053504,76.5039517474101,17.2429601346999));
#257122=CARTESIAN_POINT('Ctrl Pts',(28.1131514503916,76.5043964665192,17.2442224078977));
#257123=CARTESIAN_POINT('Ctrl Pts',(28.1390735397253,76.5073626095463,17.2526413914032));
#257124=CARTESIAN_POINT('Ctrl Pts',(28.1650771837687,76.510387549106,17.2607374323178));
#257125=CARTESIAN_POINT('Ctrl Pts',(28.191151897564,76.5134649041889,17.2685330721678));
#257126=CARTESIAN_POINT('Ctrl Pts',(28.2515584771483,76.5205941289305,17.2865930187776));
#257127=CARTESIAN_POINT('Ctrl Pts',(28.3123340562986,76.5280003772098,17.3030517999978));
#257128=CARTESIAN_POINT('Ctrl Pts',(28.3734477222867,76.5356394395931,17.3181020343265));
#257129=CARTESIAN_POINT('Ctrl Pts',(28.4368410864441,76.5435634588064,17.3337136814111));
#257130=CARTESIAN_POINT('Ctrl Pts',(28.5005983554152,76.5517380601004,17.3478096642272));
#257131=CARTESIAN_POINT('Ctrl Pts',(28.5647256406625,76.5601276443299,17.3605684035188));
#257132=CARTESIAN_POINT('Ctrl Pts',(28.5930332347029,76.5638310436492,17.3662004712251));
#257133=CARTESIAN_POINT('Ctrl Pts',(28.6214134363291,76.567576502723,17.3715715053416));
#257134=CARTESIAN_POINT('Ctrl Pts',(28.6498690551224,76.5713617072221,17.3766947662574));
#257135=CARTESIAN_POINT('Ctrl Pts',(28.7073884190851,76.5790130100047,17.3870507775405));
#257136=CARTESIAN_POINT('Ctrl Pts',(28.7652559670614,76.5868350946858,17.3963736583769));
#257137=CARTESIAN_POINT('Ctrl Pts',(28.8232282289298,76.5947786108581,17.4047210505717));
#257138=CARTESIAN_POINT('Ctrl Pts',(28.8406235593049,76.5971621660914,17.4072257940528));
#257139=CARTESIAN_POINT('Ctrl Pts',(28.8580286627969,76.599556723493,17.4096426038313));
#257140=CARTESIAN_POINT('Ctrl Pts',(28.8754377812505,76.6019611150693,17.4119727726842));
#257141=CARTESIAN_POINT('Ctrl Pts',(28.953450108308,76.6127354792352,17.422414536013));
#257142=CARTESIAN_POINT('Ctrl Pts',(29.0319245446426,76.6237599571516,17.431168749174));
#257143=CARTESIAN_POINT('Ctrl Pts',(29.110176469793,76.6349137015637,17.4382612976143));
#257144=CARTESIAN_POINT('Ctrl Pts',(29.1220414733213,76.6366048959535,17.4393367102908));
#257145=CARTESIAN_POINT('Ctrl Pts',(29.133901454615,76.638299079889,17.440373900432));
#257146=CARTESIAN_POINT('Ctrl Pts',(29.1457541224843,76.6399958502497,17.4413729364037));
#257147=CARTESIAN_POINT('Ctrl Pts',(29.2553480580749,76.655684785743,17.4506103743498));
#257148=CARTESIAN_POINT('Ctrl Pts',(29.3650148897119,76.6716864102272,17.4567325786613));
#257149=CARTESIAN_POINT('Ctrl Pts',(29.4748980618221,76.6879909655065,17.4599100504612));
#257150=CARTESIAN_POINT('Ctrl Pts',(29.5348562256177,76.6968876070693,17.4616438498317));
#257151=CARTESIAN_POINT('Ctrl Pts',(29.5948790585548,76.7058745786255,17.4625));
#257152=CARTESIAN_POINT('Ctrl Pts',(29.6549915892153,76.7149512087495,17.4625));
#257153=CARTESIAN_POINT('Origin',(-34.3520449604435,-128.965117604652,16.1925));
#257154=CARTESIAN_POINT('Ctrl Pts',(76.7149512087496,29.6549915892152,17.4625));
#257155=CARTESIAN_POINT('Ctrl Pts',(76.7007359098135,29.5608467821401,17.4625));
#257156=CARTESIAN_POINT('Ctrl Pts',(76.6867030088941,29.4667125209745,17.4604072289322));
#257157=CARTESIAN_POINT('Ctrl Pts',(76.6728916244736,29.3726870671455,17.4561240814492));
#257158=CARTESIAN_POINT('Ctrl Pts',(76.6599282024501,29.2844343908147,17.452103901667));
#257159=CARTESIAN_POINT('Ctrl Pts',(76.6471598475859,29.196277078863,17.4461538204625));
#257160=CARTESIAN_POINT('Ctrl Pts',(76.6346271711136,29.1083236389632,17.4381590482525));
#257161=CARTESIAN_POINT('Ctrl Pts',(76.623564612772,29.0306873844582,17.4311020852649));
#257162=CARTESIAN_POINT('Ctrl Pts',(76.612685722018,28.9532100090808,17.4224515902637));
#257163=CARTESIAN_POINT('Ctrl Pts',(76.6020251850533,28.8759903503099,17.4121058896821));
#257164=CARTESIAN_POINT('Ctrl Pts',(76.5929919275611,28.8105578994449,17.4033394103198));
#257165=CARTESIAN_POINT('Ctrl Pts',(76.5841246883598,28.7453752922117,17.3933663288476));
#257166=CARTESIAN_POINT('Ctrl Pts',(76.5754248746701,28.6803389123986,17.3820812128369));
#257167=CARTESIAN_POINT('Ctrl Pts',(76.5745077284505,28.6734826885746,17.380891520522));
#257168=CARTESIAN_POINT('Ctrl Pts',(76.5735924520281,28.6666281209666,17.3796872111787));
#257169=CARTESIAN_POINT('Ctrl Pts',(76.5726790536845,28.6597751110934,17.3784681359426));
#257170=CARTESIAN_POINT('Ctrl Pts',(76.5653610465084,28.6048698490276,17.3687010924751));
#257171=CARTESIAN_POINT('Ctrl Pts',(76.5581535830946,28.5499526452457,17.3579431897578));
#257172=CARTESIAN_POINT('Ctrl Pts',(76.551095713263,28.4951749625612,17.3461368886708));
#257173=CARTESIAN_POINT('Ctrl Pts',(76.5446169987028,28.4448922315325,17.3352993900234));
#257174=CARTESIAN_POINT('Ctrl Pts',(76.5382643026121,28.3947267788196,17.3235782727003));
#257175=CARTESIAN_POINT('Ctrl Pts',(76.5320763362567,28.3448347290616,17.3109158794063));
#257176=CARTESIAN_POINT('Ctrl Pts',(76.5260889614222,28.2965599993677,17.2986639551717));
#257177=CARTESIAN_POINT('Ctrl Pts',(76.5202557206435,28.2485407157557,17.2855307133555));
#257178=CARTESIAN_POINT('Ctrl Pts',(76.5146209503256,28.2009625196928,17.2714529746984));
#257179=CARTESIAN_POINT('Ctrl Pts',(76.5111206177552,28.1714068324292,17.262707850344));
#257180=CARTESIAN_POINT('Ctrl Pts',(76.5076867892711,28.1419437054236,17.2535816880451));
#257181=CARTESIAN_POINT('Ctrl Pts',(76.5043299432579,28.1125994901801,17.2440469306636));
#257182=CARTESIAN_POINT('Ctrl Pts',(76.4994099378461,28.0695907560184,17.2300721883809));
#257183=CARTESIAN_POINT('Ctrl Pts',(76.4946524666836,28.0268356967203,17.215222656587));
#257184=CARTESIAN_POINT('Ctrl Pts',(76.4900921572824,27.9843757811643,17.1993722202065));
#257185=CARTESIAN_POINT('Ctrl Pts',(76.4857772770164,27.9442009957251,17.1843748309661));
#257186=CARTESIAN_POINT('Ctrl Pts',(76.4816388565531,27.9042902389518,17.1684813247625));
#257187=CARTESIAN_POINT('Ctrl Pts',(76.4777167689223,27.8647187422006,17.1515646848084));
#257188=CARTESIAN_POINT('Ctrl Pts',(76.4753652742226,27.8409935800865,17.1414222828705));
#257189=CARTESIAN_POINT('Ctrl Pts',(76.4730917485966,27.817391151853,17.1309117177248));
#257190=CARTESIAN_POINT('Ctrl Pts',(76.4709068974261,27.7939357204578,17.1200019028265));
#257191=CARTESIAN_POINT('Ctrl Pts',(76.4694744690635,27.7785579109112,17.112849228767));
#257192=CARTESIAN_POINT('Ctrl Pts',(76.4680842075485,27.763288324096,17.1055472028756));
#257193=CARTESIAN_POINT('Ctrl Pts',(76.4667393807873,27.7481342818727,17.0980870415728));
#257194=CARTESIAN_POINT('Ctrl Pts',(76.4639004848743,27.7161444748761,17.0823388262306));
#257195=CARTESIAN_POINT('Ctrl Pts',(76.4612595947587,27.6846459211437,17.0658786658155));
#257196=CARTESIAN_POINT('Ctrl Pts',(76.4588488257704,27.6536746993957,17.0485804548605));
#257197=CARTESIAN_POINT('Ctrl Pts',(76.4565032661768,27.6235412247035,17.031750146832));
#257198=CARTESIAN_POINT('Ctrl Pts',(76.4543754667986,27.5939067174985,17.0141265974772));
#257199=CARTESIAN_POINT('Ctrl Pts',(76.4525070385105,27.5648480032216,16.9955752187322));
#257200=CARTESIAN_POINT('Ctrl Pts',(76.4507095662163,27.5368928314082,16.9777283527198));
#257201=CARTESIAN_POINT('Ctrl Pts',(76.4491520836248,27.5094704097394,16.9590228414135));
#257202=CARTESIAN_POINT('Ctrl Pts',(76.4478838668815,27.4826925239471,16.9393206257464));
#257203=CARTESIAN_POINT('Ctrl Pts',(76.4475882262302,27.4764501906585,16.9347277390013));
#257204=CARTESIAN_POINT('Ctrl Pts',(76.4473083613942,27.4702430809547,16.9300806058261));
#257205=CARTESIAN_POINT('Ctrl Pts',(76.4470450027163,27.4640729822085,16.9253773219914));
#257206=CARTESIAN_POINT('Ctrl Pts',(76.4463836380683,27.4485782006516,16.9135661081653));
#257207=CARTESIAN_POINT('Ctrl Pts',(76.445830245995,27.4333087681932,16.9013716940896));
#257208=CARTESIAN_POINT('Ctrl Pts',(76.4453983713746,27.4183233468248,16.8887840336497));
#257209=CARTESIAN_POINT('Ctrl Pts',(76.4447393676207,27.3954568747781,16.8695763398181));
#257210=CARTESIAN_POINT('Ctrl Pts',(76.4443666032736,27.3730391298257,16.8492614774149));
#257211=CARTESIAN_POINT('Ctrl Pts',(76.4443504330611,27.3514856269793,16.8278798165427));
#257212=CARTESIAN_POINT('Ctrl Pts',(76.4443340891035,27.3297005370019,16.8062684149396));
#257213=CARTESIAN_POINT('Ctrl Pts',(76.4446820842408,27.3087984600255,16.7835670140578));
#257214=CARTESIAN_POINT('Ctrl Pts',(76.4454707611388,27.2892498936118,16.7598514785006));
#257215=CARTESIAN_POINT('Ctrl Pts',(76.4462155696294,27.2707886729506,16.7374550671345));
#257216=CARTESIAN_POINT('Ctrl Pts',(76.4473534742746,27.2535351094313,16.7141544688201));
#257217=CARTESIAN_POINT('Ctrl Pts',(76.4489511499897,27.237916905714,16.6900423941731));
#257218=CARTESIAN_POINT('Ctrl Pts',(76.4513448875845,27.2145167369268,16.653916177179));
#257219=CARTESIAN_POINT('Ctrl Pts',(76.4547511876201,27.1945566457996,16.6158401525527));
#257220=CARTESIAN_POINT('Ctrl Pts',(76.4593869302476,27.1790626912129,16.5757647539218));
#257221=CARTESIAN_POINT('Ctrl Pts',(76.4599500333952,27.1771806422517,16.5708967996533));
#257222=CARTESIAN_POINT('Ctrl Pts',(76.4605309464294,27.1753659415636,16.5660028743095));
#257223=CARTESIAN_POINT('Ctrl Pts',(76.4611298941881,27.1736203958826,16.5610838271793));
#257224=CARTESIAN_POINT('Ctrl Pts',(76.4637830304577,27.1658882180939,16.5392941098575));
#257225=CARTESIAN_POINT('Ctrl Pts',(76.4668030340722,27.1595395614895,16.5169703441688));
#257226=CARTESIAN_POINT('Ctrl Pts',(76.4701643665394,27.1547079235266,16.4943951487428));
#257227=CARTESIAN_POINT('Ctrl Pts',(76.4735256990065,27.1498762855636,16.4718199533169));
#257228=CARTESIAN_POINT('Ctrl Pts',(76.4772282140789,27.1465619921089,16.4489944614982));
#257229=CARTESIAN_POINT('Ctrl Pts',(76.4812333698756,27.1448472169224,16.4262179830525));
#257230=CARTESIAN_POINT('Ctrl Pts',(76.4837575042377,27.1437665291311,16.4118637619405));
#257231=CARTESIAN_POINT('Ctrl Pts',(76.4864043794184,27.1432984744763,16.3974938691297));
#257232=CARTESIAN_POINT('Ctrl Pts',(76.4891686128859,27.1434396622859,16.383133975236));
#257233=CARTESIAN_POINT('Ctrl Pts',(76.4931572620936,27.1436433891605,16.3624133740009));
#257234=CARTESIAN_POINT('Ctrl Pts',(76.4973856936385,27.1451158165625,16.3417311587632));
#257235=CARTESIAN_POINT('Ctrl Pts',(76.5018218230375,27.1478003503532,16.3211985325368));
#257236=CARTESIAN_POINT('Ctrl Pts',(76.5063090129379,27.1505157835224,16.3004295727647));
#257237=CARTESIAN_POINT('Ctrl Pts',(76.5110086870996,27.1544712854893,16.2798136765402));
#257238=CARTESIAN_POINT('Ctrl Pts',(76.5158772286368,27.1595556991521,16.2594666987899));
#257239=CARTESIAN_POINT('Ctrl Pts',(76.5208630385112,27.1647625808542,16.2386296243171));
#257240=CARTESIAN_POINT('Ctrl Pts',(76.5260259237948,27.1711532997666,16.2180745910999));
#257241=CARTESIAN_POINT('Ctrl Pts',(76.531308508193,27.1785550950825,16.1979266545698));
#257242=CARTESIAN_POINT('Ctrl Pts',(76.5317837688064,27.1792210156845,16.1961139962283));
#257243=CARTESIAN_POINT('Ctrl Pts',(76.5322599915831,27.1798950860555,16.1943046333203));
#257244=CARTESIAN_POINT('Ctrl Pts',(76.5327371308321,27.1805771605214,16.1924986571));
#257245=CARTESIAN_POINT('Origin',(50.220290910288,8.18330470534212,16.1925));
#257246=CARTESIAN_POINT('Ctrl Pts',(76.5327353708766,-27.1805640649136,
16.1924982582718));
#257247=CARTESIAN_POINT('Ctrl Pts',(76.5254460991286,-27.170142411259,16.2200871281807));
#257248=CARTESIAN_POINT('Ctrl Pts',(76.5184672980879,-27.1617293806191,
16.2481013366734));
#257249=CARTESIAN_POINT('Ctrl Pts',(76.5118328073647,-27.1555532163233,
16.2765966498456));
#257250=CARTESIAN_POINT('Ctrl Pts',(76.5053582412141,-27.1495259286294,
16.304405082748));
#257251=CARTESIAN_POINT('Ctrl Pts',(76.4992115671709,-27.1456288662117,
16.3326717168179));
#257252=CARTESIAN_POINT('Ctrl Pts',(76.4934339939309,-27.144123077719,16.3614476211452));
#257253=CARTESIAN_POINT('Ctrl Pts',(76.4921585023732,-27.1437906508625,
16.3678003615623));
#257254=CARTESIAN_POINT('Ctrl Pts',(76.4909010391219,-27.1435749657791,
16.3741779192149));
#257255=CARTESIAN_POINT('Ctrl Pts',(76.4896621154036,-27.1434791718122,
16.3805808375412));
#257256=CARTESIAN_POINT('Ctrl Pts',(76.4880193305124,-27.143352151174,16.3890709627455));
#257257=CARTESIAN_POINT('Ctrl Pts',(76.4864160037888,-27.1434370002358,
16.3975719419878));
#257258=CARTESIAN_POINT('Ctrl Pts',(76.4848537692343,-27.1437355673527,
16.4060769483921));
#257259=CARTESIAN_POINT('Ctrl Pts',(76.4809854829898,-27.1444748565126,
16.4271363976198));
#257260=CARTESIAN_POINT('Ctrl Pts',(76.4773696370509,-27.1465703673381,
16.4482618838856));
#257261=CARTESIAN_POINT('Ctrl Pts',(76.4740424808257,-27.1499697741418,
16.4691998962437));
#257262=CARTESIAN_POINT('Ctrl Pts',(76.4707094654638,-27.1533751673159,
16.4901747805338));
#257263=CARTESIAN_POINT('Ctrl Pts',(76.4676662855534,-27.1580887887179,
16.5109605600287));
#257264=CARTESIAN_POINT('Ctrl Pts',(76.4649378361828,-27.1640086579344,
16.5313130815935));
#257265=CARTESIAN_POINT('Ctrl Pts',(76.4643858787488,-27.1652062303936,
16.5354303379737));
#257266=CARTESIAN_POINT('Ctrl Pts',(76.4638467601751,-27.1664530141853,
16.5395299259007));
#257267=CARTESIAN_POINT('Ctrl Pts',(76.4633206224269,-27.1677479362274,
16.5436099312137));
#257268=CARTESIAN_POINT('Ctrl Pts',(76.4620493955123,-27.1708766601362,
16.5534678298022));
#257269=CARTESIAN_POINT('Ctrl Pts',(76.4608504005183,-27.1742844116281,
16.5632279776837));
#257270=CARTESIAN_POINT('Ctrl Pts',(76.4597221364489,-27.1779555862455,
16.5728808843466));
#257271=CARTESIAN_POINT('Ctrl Pts',(76.4555634683355,-27.1914871674013,
16.6084605294227));
#257272=CARTESIAN_POINT('Ctrl Pts',(76.4523683264295,-27.2085635842067,
16.6425190954528));
#257273=CARTESIAN_POINT('Ctrl Pts',(76.4499894515854,-27.2285145118707,
16.6751163767829));
#257274=CARTESIAN_POINT('Ctrl Pts',(76.4481516192734,-27.2439278740341,
16.7002998525161));
#257275=CARTESIAN_POINT('Ctrl Pts',(76.4468125093684,-27.2611648250125,
16.7246580015589));
#257276=CARTESIAN_POINT('Ctrl Pts',(76.4459011083301,-27.2797726036762,
16.7480930589315));
#257277=CARTESIAN_POINT('Ctrl Pts',(76.4449881378309,-27.298412425514,16.7715684722023));
#257278=CARTESIAN_POINT('Ctrl Pts',(76.4445043286353,-27.3184277738214,
16.7941176720138));
#257279=CARTESIAN_POINT('Ctrl Pts',(76.4443826625373,-27.3394063743812,
16.8156722156737));
#257280=CARTESIAN_POINT('Ctrl Pts',(76.4442602400807,-27.360515392067,16.8373607569101));
#257281=CARTESIAN_POINT('Ctrl Pts',(76.444504461044,-27.3825996603397,16.858042310263));
#257282=CARTESIAN_POINT('Ctrl Pts',(76.4450517552698,-27.4052828608358,
16.8776763499813));
#257283=CARTESIAN_POINT('Ctrl Pts',(76.4451275701142,-27.4084250889746,
16.8803961880435));
#257284=CARTESIAN_POINT('Ctrl Pts',(76.445209208363,-27.4115788786024,16.8830959690915));
#257285=CARTESIAN_POINT('Ctrl Pts',(76.4452965083211,-27.4147432949493,
16.8857756277876));
#257286=CARTESIAN_POINT('Ctrl Pts',(76.4456285567619,-27.4267792630841,
16.8959678032609));
#257287=CARTESIAN_POINT('Ctrl Pts',(76.4460413746574,-27.4390220462584,
16.9059171754191));
#257288=CARTESIAN_POINT('Ctrl Pts',(76.4465283265822,-27.4514363729662,
16.9156217934251));
#257289=CARTESIAN_POINT('Ctrl Pts',(76.4477740792775,-27.4831955265325,
16.940448790556));
#257290=CARTESIAN_POINT('Ctrl Pts',(76.4494849825224,-27.5161304124262,
16.9638340074613));
#257291=CARTESIAN_POINT('Ctrl Pts',(76.4515669382221,-27.5499276827804,
16.9859393963669));
#257292=CARTESIAN_POINT('Ctrl Pts',(76.4537247726024,-27.5849567239552,
17.0088504353368));
#257293=CARTESIAN_POINT('Ctrl Pts',(76.4562812377412,-27.6209122535195,
17.0303866179473));
#257294=CARTESIAN_POINT('Ctrl Pts',(76.4591476533537,-27.657496253866,17.0507077973849));
#257295=CARTESIAN_POINT('Ctrl Pts',(76.4614800345035,-27.6872643839368,
17.0672429905556));
#257296=CARTESIAN_POINT('Ctrl Pts',(76.4640179659447,-27.7174496690714,
17.0829733141296));
#257297=CARTESIAN_POINT('Ctrl Pts',(76.4667207528857,-27.7479141287993,
17.0979758062083));
#257298=CARTESIAN_POINT('Ctrl Pts',(76.4677059340768,-27.7590185974001,
17.1034442997812));
#257299=CARTESIAN_POINT('Ctrl Pts',(76.4687146852106,-27.7701762979147,
17.1088237343901));
#257300=CARTESIAN_POINT('Ctrl Pts',(76.4697457322933,-27.7813854912822,
17.1141186859284));
#257301=CARTESIAN_POINT('Ctrl Pts',(76.472429728371,-27.8105649841859,17.1279023718524));
#257302=CARTESIAN_POINT('Ctrl Pts',(76.4752686565451,-27.840103215534,17.1410999474328));
#257303=CARTESIAN_POINT('Ctrl Pts',(76.4782264005117,-27.8698177823045,
17.1537242053278));
#257304=CARTESIAN_POINT('Ctrl Pts',(76.4814236442212,-27.9019384502044,
17.1673706972473));
#257305=CARTESIAN_POINT('Ctrl Pts',(76.4847597640879,-27.9342655910949,
17.1803475370977));
#257306=CARTESIAN_POINT('Ctrl Pts',(76.4881996908386,-27.9666279531757,
17.1926699656471));
#257307=CARTESIAN_POINT('Ctrl Pts',(76.4886519862318,-27.9708830865957,
17.1942901680725));
#257308=CARTESIAN_POINT('Ctrl Pts',(76.489106089515,-27.9751389006341,17.1958990522154));
#257309=CARTESIAN_POINT('Ctrl Pts',(76.4895619325379,-27.9793950678132,
17.1974966476082));
#257310=CARTESIAN_POINT('Ctrl Pts',(76.4938975656961,-28.0198765024714,
17.2126917634919));
#257311=CARTESIAN_POINT('Ctrl Pts',(76.4984031419524,-28.060540191981,17.2269450615677));
#257312=CARTESIAN_POINT('Ctrl Pts',(76.5030665766311,-28.1015001037439,
17.2404146413945));
#257313=CARTESIAN_POINT('Ctrl Pts',(76.5035084491004,-28.1053811610762,
17.2416909188399));
#257314=CARTESIAN_POINT('Ctrl Pts',(76.5039517474111,-28.1092649053587,
17.2429601347027));
#257315=CARTESIAN_POINT('Ctrl Pts',(76.5043964665192,-28.1131514503915,
17.2442224078977));
#257316=CARTESIAN_POINT('Ctrl Pts',(76.5073626095462,-28.139073539725,17.2526413914031));
#257317=CARTESIAN_POINT('Ctrl Pts',(76.5103875491059,-28.1650771837681,
17.2607374323177));
#257318=CARTESIAN_POINT('Ctrl Pts',(76.5134649041888,-28.1911518975632,
17.2685330721676));
#257319=CARTESIAN_POINT('Ctrl Pts',(76.5205941289288,-28.2515584771341,
17.2865930187733));
#257320=CARTESIAN_POINT('Ctrl Pts',(76.5280003772061,-28.3123340562714,
17.3030517999906));
#257321=CARTESIAN_POINT('Ctrl Pts',(76.5356394395873,-28.3734477222465,
17.3181020343168));
#257322=CARTESIAN_POINT('Ctrl Pts',(76.543563458799,-28.4368410863943,17.3337136813998));
#257323=CARTESIAN_POINT('Ctrl Pts',(76.5517380600912,-28.5005983553558,
17.3478096642148));
#257324=CARTESIAN_POINT('Ctrl Pts',(76.5601276443193,-28.5647256405924,
17.3605684035053));
#257325=CARTESIAN_POINT('Ctrl Pts',(76.5638310436417,-28.5930332346559,
17.3662004712166));
#257326=CARTESIAN_POINT('Ctrl Pts',(76.5675765027187,-28.6214134363051,
17.3715715053376));
#257327=CARTESIAN_POINT('Ctrl Pts',(76.5713617072211,-28.6498690551213,
17.3766947662575));
#257328=CARTESIAN_POINT('Ctrl Pts',(76.5790130100033,-28.7073884190766,
17.3870507775391));
#257329=CARTESIAN_POINT('Ctrl Pts',(76.5868350946836,-28.7652559670459,
17.3963736583744));
#257330=CARTESIAN_POINT('Ctrl Pts',(76.5947786108551,-28.8232282289076,
17.4047210505685));
#257331=CARTESIAN_POINT('Ctrl Pts',(76.5971621660893,-28.84062355929,17.4072257940507));
#257332=CARTESIAN_POINT('Ctrl Pts',(76.5995567234919,-28.8580286627894,
17.4096426038302));
#257333=CARTESIAN_POINT('Ctrl Pts',(76.6019611150693,-28.8754377812504,
17.4119727726841));
#257334=CARTESIAN_POINT('Ctrl Pts',(76.6127354792351,-28.9534501083073,
17.4224145360128));
#257335=CARTESIAN_POINT('Ctrl Pts',(76.6237599571512,-29.0319245446418,
17.431168749174));
#257336=CARTESIAN_POINT('Ctrl Pts',(76.6349137015633,-29.1101764697921,
17.4382612976142));
#257337=CARTESIAN_POINT('Ctrl Pts',(76.6366048959531,-29.1220414733205,
17.4393367102908));
#257338=CARTESIAN_POINT('Ctrl Pts',(76.6382990798886,-29.1339014546143,
17.440373900432));
#257339=CARTESIAN_POINT('Ctrl Pts',(76.6399958502493,-29.1457541224838,
17.4413729364037));
#257340=CARTESIAN_POINT('Ctrl Pts',(76.6556847857491,-29.2553480581192,
17.4506103743536));
#257341=CARTESIAN_POINT('Ctrl Pts',(76.6716864102403,-29.3650148897999,
17.4567325786662));
#257342=CARTESIAN_POINT('Ctrl Pts',(76.6879909655265,-29.4748980619541,
17.459910050465));
#257343=CARTESIAN_POINT('Ctrl Pts',(76.696887607083,-29.5348562257057,17.461643849833));
#257344=CARTESIAN_POINT('Ctrl Pts',(76.7058745786326,-29.5948790585987,
17.4625));
#257345=CARTESIAN_POINT('Ctrl Pts',(76.7149512087496,-29.6549915892152,
17.4625));
#257346=CARTESIAN_POINT('Origin',(-44.3927817339206,-24.8661421402461,16.1925));
#257347=CARTESIAN_POINT('Ctrl Pts',(29.6549915892152,-76.7149512087496,
17.4625));
#257348=CARTESIAN_POINT('Ctrl Pts',(29.5784809832681,-76.7033985679909,
17.4625));
#257349=CARTESIAN_POINT('Ctrl Pts',(29.5017645219472,-76.6919419131645,
17.4610789773413));
#257350=CARTESIAN_POINT('Ctrl Pts',(29.4251260134592,-76.6806292438031,
17.4582328812633));
#257351=CARTESIAN_POINT('Ctrl Pts',(29.3550776154898,-76.6702893457392,
17.4556315196937));
#257352=CARTESIAN_POINT('Ctrl Pts',(29.285091738982,-76.6600693733096,17.4518390793048));
#257353=CARTESIAN_POINT('Ctrl Pts',(29.215395972818,-76.6500111635191,17.4468147853601));
#257354=CARTESIAN_POINT('Ctrl Pts',(29.1910127661958,-76.6464922782112,
17.4450570258271));
#257355=CARTESIAN_POINT('Ctrl Pts',(29.1666653406614,-76.6429932651761,
17.4431481665674));
#257356=CARTESIAN_POINT('Ctrl Pts',(29.1423646235818,-76.6395162005647,
17.4410854028152));
#257357=CARTESIAN_POINT('Ctrl Pts',(29.0717236084288,-76.6294085410626,
17.4350890478519));
#257358=CARTESIAN_POINT('Ctrl Pts',(29.0013000924683,-76.6194570017698,
17.4278165327662));
#257359=CARTESIAN_POINT('Ctrl Pts',(28.930890043211,-76.6096539020255,17.4191389458549));
#257360=CARTESIAN_POINT('Ctrl Pts',(28.9125942000528,-76.6071065955362,
17.4168841005481));
#257361=CARTESIAN_POINT('Ctrl Pts',(28.8942993977004,-76.6045693606119,
17.4145341520355));
#257362=CARTESIAN_POINT('Ctrl Pts',(28.8760023419532,-76.6020421698846,
17.412086338018));
#257363=CARTESIAN_POINT('Ctrl Pts',(28.8096307852661,-76.5928749254421,
17.4032070281956));
#257364=CARTESIAN_POINT('Ctrl Pts',(28.7435548277056,-76.5838841660478,
17.3930871840675));
#257365=CARTESIAN_POINT('Ctrl Pts',(28.6775616926366,-76.5750605977029,
17.3815966638287));
#257366=CARTESIAN_POINT('Ctrl Pts',(28.6679863743641,-76.5737803361255,
17.3799294390744));
#257367=CARTESIAN_POINT('Ctrl Pts',(28.6584128434796,-76.5725036108758,
17.3782332812975));
#257368=CARTESIAN_POINT('Ctrl Pts',(28.648840495476,-76.571230410841,17.3765077138038));
#257369=CARTESIAN_POINT('Ctrl Pts',(28.5939195943272,-76.5639254848995,
17.3666073506207));
#257370=CARTESIAN_POINT('Ctrl Pts',(28.539019721318,-76.5567364098806,17.3557157603938));
#257371=CARTESIAN_POINT('Ctrl Pts',(28.4842809217551,-76.5497009035225,
17.3437734778892));
#257372=CARTESIAN_POINT('Ctrl Pts',(28.4340312118414,-76.5432423739892,
17.3328105733981));
#257373=CARTESIAN_POINT('Ctrl Pts',(28.3839169544482,-76.5369132259095,
17.3209620182655));
#257374=CARTESIAN_POINT('Ctrl Pts',(28.3340851368585,-76.5307511868761,
17.3081680846722));
#257375=CARTESIAN_POINT('Ctrl Pts',(28.2843811713914,-76.5246049576167,
17.2954069761221));
#257376=CARTESIAN_POINT('Ctrl Pts',(28.2349573707686,-76.518624827935,17.2817053136045));
#257377=CARTESIAN_POINT('Ctrl Pts',(28.186008513182,-76.5128586176738,17.2669910566475));
#257378=CARTESIAN_POINT('Ctrl Pts',(28.1614764636039,-76.5099687247737,
17.25961660709));
#257379=CARTESIAN_POINT('Ctrl Pts',(28.1370017452465,-76.5071248960927,
17.2519719554798));
#257380=CARTESIAN_POINT('Ctrl Pts',(28.112603631757,-76.5043336151742,17.2440428740805));
#257381=CARTESIAN_POINT('Ctrl Pts',(28.0701844846509,-76.4994806270139,
17.2302571823942));
#257382=CARTESIAN_POINT('Ctrl Pts',(28.0279824912973,-76.4947829029006,
17.2156101298218));
#257383=CARTESIAN_POINT('Ctrl Pts',(27.9860694428279,-76.4902767919924,
17.1999930540383));
#257384=CARTESIAN_POINT('Ctrl Pts',(27.9466341480905,-76.4860370666975,
17.1852992054887));
#257385=CARTESIAN_POINT('Ctrl Pts',(27.9074544475917,-76.4819669295132,
17.1697465428432));
#257386=CARTESIAN_POINT('Ctrl Pts',(27.8686308801497,-76.4781067108621,
17.153228318961));
#257387=CARTESIAN_POINT('Ctrl Pts',(27.837762123119,-76.4750374372359,17.1400946202003));
#257388=CARTESIAN_POINT('Ctrl Pts',(27.8071191438906,-76.4721010301339,
17.1263502154837));
#257389=CARTESIAN_POINT('Ctrl Pts',(27.7767742650356,-76.4693230827021,
17.1119338317454));
#257390=CARTESIAN_POINT('Ctrl Pts',(27.7671845095157,-76.4684451804754,
17.1073778868628));
#257391=CARTESIAN_POINT('Ctrl Pts',(27.7576382281084,-76.46758424905,17.1027621986441));
#257392=CARTESIAN_POINT('Ctrl Pts',(27.7481373827157,-76.4667411216785,
17.0980845986398));
#257393=CARTESIAN_POINT('Ctrl Pts',(27.7165349284677,-76.4639366455415,
17.0825256000436));
#257394=CARTESIAN_POINT('Ctrl Pts',(27.6854146211002,-76.461325227445,17.0662758428433));
#257395=CARTESIAN_POINT('Ctrl Pts',(27.6548074136947,-76.4589379212268,
17.0492104485573));
#257396=CARTESIAN_POINT('Ctrl Pts',(27.6250423674505,-76.4566163020395,
17.0326146107414));
#257397=CARTESIAN_POINT('Ctrl Pts',(27.5957623497953,-76.4545065513655,
17.0152474880437));
#257398=CARTESIAN_POINT('Ctrl Pts',(27.5670390175372,-76.4526490486086,
16.9969759720735));
#257399=CARTESIAN_POINT('Ctrl Pts',(27.5394891827774,-76.4508674344993,
16.9794509425515));
#257400=CARTESIAN_POINT('Ctrl Pts',(27.5124513533527,-76.4493178278133,
16.9610939515815));
#257401=CARTESIAN_POINT('Ctrl Pts',(27.4860313731063,-76.448047775172,16.9417696635372));
#257402=CARTESIAN_POINT('Ctrl Pts',(27.4732138950567,-76.4474316175633,
16.9323946134606));
#257403=CARTESIAN_POINT('Ctrl Pts',(27.4605425004175,-76.4468814440254,
16.9227916185164));
#257404=CARTESIAN_POINT('Ctrl Pts',(27.4480332789739,-76.4464038210192,
16.9129435541778));
#257405=CARTESIAN_POINT('Ctrl Pts',(27.4380190788529,-76.446021462102,16.9050597312288));
#257406=CARTESIAN_POINT('Ctrl Pts',(27.4281096389904,-76.4456876024434,
16.8970089022858));
#257407=CARTESIAN_POINT('Ctrl Pts',(27.4183213434191,-76.4454060812472,
16.8887879984482));
#257408=CARTESIAN_POINT('Ctrl Pts',(27.3952254081782,-76.4447418189891,
16.8693903963557));
#257409=CARTESIAN_POINT('Ctrl Pts',(27.3726021898373,-76.4443701445099,
16.8488671319478));
#257410=CARTESIAN_POINT('Ctrl Pts',(27.3508659754084,-76.4443625463769,
16.8272552303422));
#257411=CARTESIAN_POINT('Ctrl Pts',(27.3290708073661,-76.4443549276361,
16.8055847122883));
#257412=CARTESIAN_POINT('Ctrl Pts',(27.3081675781727,-76.4447134034009,
16.7828195228048));
#257413=CARTESIAN_POINT('Ctrl Pts',(27.2886142275583,-76.4455134941453,
16.7590305376009));
#257414=CARTESIAN_POINT('Ctrl Pts',(27.2688420650758,-76.4463225383092,
16.7349753416389));
#257415=CARTESIAN_POINT('Ctrl Pts',(27.2504503196107,-76.4475831876929,
16.7098732026971));
#257416=CARTESIAN_POINT('Ctrl Pts',(27.2339516171415,-76.4493763637529,
16.6838334538405));
#257417=CARTESIAN_POINT('Ctrl Pts',(27.2316065629842,-76.4496312380366,
16.6801322766463));
#257418=CARTESIAN_POINT('Ctrl Pts',(27.2292998143652,-76.449896874548,16.6764122174921));
#257419=CARTESIAN_POINT('Ctrl Pts',(27.22703290306,-76.4501735092111,16.6726736500803));
#257420=CARTESIAN_POINT('Ctrl Pts',(27.208294241588,-76.4524602168078,16.6417700373296));
#257421=CARTESIAN_POINT('Ctrl Pts',(27.1920956821037,-76.4554866376469,
16.6094802657885));
#257422=CARTESIAN_POINT('Ctrl Pts',(27.1790613975838,-76.4593868180786,
16.5757650534976));
#257423=CARTESIAN_POINT('Ctrl Pts',(27.1746643707656,-76.4607025172968,
16.5643914570107));
#257424=CARTESIAN_POINT('Ctrl Pts',(27.1706359107516,-76.4621156292997,
16.5528759158133));
#257425=CARTESIAN_POINT('Ctrl Pts',(27.1669986019356,-76.4636289044872,
16.5412293347377));
#257426=CARTESIAN_POINT('Ctrl Pts',(27.1600415068142,-76.4665233519912,
16.5189528725292));
#257427=CARTESIAN_POINT('Ctrl Pts',(27.1545628735561,-76.4697851638502,
16.4962407115125));
#257428=CARTESIAN_POINT('Ctrl Pts',(27.1506549153931,-76.4733862268997,
16.4733464731272));
#257429=CARTESIAN_POINT('Ctrl Pts',(27.14674695723,-76.4769872899492,16.450452234742));
#257430=CARTESIAN_POINT('Ctrl Pts',(27.1444098150615,-76.4809274578023,
16.4273768616869));
#257431=CARTESIAN_POINT('Ctrl Pts',(27.1436800109181,-76.4851658906463,
16.4043845876085));
#257432=CARTESIAN_POINT('Ctrl Pts',(27.1434551581823,-76.4864717522652,
16.3973006654718));
#257433=CARTESIAN_POINT('Ctrl Pts',(27.143378345838,-76.4878067469535,16.3902160073498));
#257434=CARTESIAN_POINT('Ctrl Pts',(27.1434490350604,-76.4891701961805,
16.383133694799));
#257435=CARTESIAN_POINT('Ctrl Pts',(27.1436556805567,-76.4931559613736,
16.3624300013325));
#257436=CARTESIAN_POINT('Ctrl Pts',(27.1451242300415,-76.4973805033897,
16.3417644841244));
#257437=CARTESIAN_POINT('Ctrl Pts',(27.1478012243607,-76.5018122177599,
16.3212481482212));
#257438=CARTESIAN_POINT('Ctrl Pts',(27.1505058861726,-76.5062897351503,
16.3005197701895));
#257439=CARTESIAN_POINT('Ctrl Pts',(27.1544440119297,-76.5109787082563,
16.279943684392));
#257440=CARTESIAN_POINT('Ctrl Pts',(27.1595080210185,-76.5158361677253,
16.2596351519481));
#257441=CARTESIAN_POINT('Ctrl Pts',(27.164685302902,-76.5208022798447,16.2388723540821));
#257442=CARTESIAN_POINT('Ctrl Pts',(27.1710392955923,-76.5259444759375,
16.2183892248369));
#257443=CARTESIAN_POINT('Ctrl Pts',(27.178401795822,-76.5312063612745,16.1983095665747));
#257444=CARTESIAN_POINT('Ctrl Pts',(27.1791134525487,-76.5317149732919,
16.1963686737493));
#257445=CARTESIAN_POINT('Ctrl Pts',(27.1798344925866,-76.5322246958756,
16.1944315509814));
#257446=CARTESIAN_POINT('Ctrl Pts',(27.1805647391996,-76.5327354732286,
16.1924983103144));
#257447=CARTESIAN_POINT('Origin',(-76.3890311653897,-109.438478010978,16.1925));
#257448=CARTESIAN_POINT('Ctrl Pts',(-27.1805640649125,-76.5327353708757,
16.1924982582717));
#257449=CARTESIAN_POINT('Ctrl Pts',(-27.1701424112585,-76.525446099128,
16.2200871281786));
#257450=CARTESIAN_POINT('Ctrl Pts',(-27.1617293806189,-76.5184672980878,
16.2481013366692));
#257451=CARTESIAN_POINT('Ctrl Pts',(-27.1555532163233,-76.5118328073651,
16.2765966498393));
#257452=CARTESIAN_POINT('Ctrl Pts',(-27.1495259286296,-76.5053582412149,
16.3044050827398));
#257453=CARTESIAN_POINT('Ctrl Pts',(-27.1456288662118,-76.4992115671722,
16.3326717168078));
#257454=CARTESIAN_POINT('Ctrl Pts',(-27.1441230777188,-76.4934339939327,
16.3614476211331));
#257455=CARTESIAN_POINT('Ctrl Pts',(-27.1437906508621,-76.4921585023742,
16.3678003615543));
#257456=CARTESIAN_POINT('Ctrl Pts',(-27.1435749657785,-76.4909010391221,
16.3741779192108));
#257457=CARTESIAN_POINT('Ctrl Pts',(-27.1434791718117,-76.4896621154032,
16.3805808375412));
#257458=CARTESIAN_POINT('Ctrl Pts',(-27.1433521511735,-76.4880193305119,
16.3890709627458));
#257459=CARTESIAN_POINT('Ctrl Pts',(-27.1434370002354,-76.4864160037884,
16.3975719419884));
#257460=CARTESIAN_POINT('Ctrl Pts',(-27.1437355673525,-76.4848537692339,
16.406076948393));
#257461=CARTESIAN_POINT('Ctrl Pts',(-27.1444748565128,-76.4809854829898,
16.4271363976198));
#257462=CARTESIAN_POINT('Ctrl Pts',(-27.1465703673381,-76.4773696370511,
16.4482618838846));
#257463=CARTESIAN_POINT('Ctrl Pts',(-27.1499697741416,-76.474042480826,
16.4691998962417));
#257464=CARTESIAN_POINT('Ctrl Pts',(-27.1533751673149,-76.4707094654647,
16.4901747805278));
#257465=CARTESIAN_POINT('Ctrl Pts',(-27.1580887887156,-76.4676662855547,
16.5109605600187));
#257466=CARTESIAN_POINT('Ctrl Pts',(-27.1640086579305,-76.4649378361846,
16.5313130815798));
#257467=CARTESIAN_POINT('Ctrl Pts',(-27.165206230391,-76.4643858787499,
16.5354303379649));
#257468=CARTESIAN_POINT('Ctrl Pts',(-27.1664530141842,-76.4638467601756,
16.5395299258967));
#257469=CARTESIAN_POINT('Ctrl Pts',(-27.1677479362278,-76.4633206224268,
16.5436099312145));
#257470=CARTESIAN_POINT('Ctrl Pts',(-27.1708766601366,-76.4620493955123,
16.5534678298028));
#257471=CARTESIAN_POINT('Ctrl Pts',(-27.1742844116285,-76.4608504005184,
16.563227977684));
#257472=CARTESIAN_POINT('Ctrl Pts',(-27.1779555862458,-76.4597221364491,
16.5728808843466));
#257473=CARTESIAN_POINT('Ctrl Pts',(-27.1914871674019,-76.4555634683357,
16.6084605294229));
#257474=CARTESIAN_POINT('Ctrl Pts',(-27.2085635842075,-76.4523683264298,
16.6425190954533));
#257475=CARTESIAN_POINT('Ctrl Pts',(-27.2285145118716,-76.4499894515856,
16.6751163767836));
#257476=CARTESIAN_POINT('Ctrl Pts',(-27.243927874034,-76.4481516192736,
16.7002998525154));
#257477=CARTESIAN_POINT('Ctrl Pts',(-27.2611648250113,-76.4468125093686,
16.7246580015568));
#257478=CARTESIAN_POINT('Ctrl Pts',(-27.2797726036738,-76.4459011083303,
16.7480930589281));
#257479=CARTESIAN_POINT('Ctrl Pts',(-27.2984124255103,-76.4449881378311,
16.7715684721976));
#257480=CARTESIAN_POINT('Ctrl Pts',(-27.3184277738163,-76.4445043286355,
16.794117672008));
#257481=CARTESIAN_POINT('Ctrl Pts',(-27.3394063743747,-76.4443826625374,
16.8156722156667));
#257482=CARTESIAN_POINT('Ctrl Pts',(-27.3605153920599,-76.4442602400808,
16.8373607569029));
#257483=CARTESIAN_POINT('Ctrl Pts',(-27.382599660332,-76.444504461044,16.8580423102556));
#257484=CARTESIAN_POINT('Ctrl Pts',(-27.4052828608275,-76.4450517552699,
16.8776763499738));
#257485=CARTESIAN_POINT('Ctrl Pts',(-27.4084250889692,-76.4451275701144,
16.8803961880385));
#257486=CARTESIAN_POINT('Ctrl Pts',(-27.4115788785998,-76.4452092083632,
16.8830959690889));
#257487=CARTESIAN_POINT('Ctrl Pts',(-27.4147432949497,-76.4452965083214,
16.8857756277875));
#257488=CARTESIAN_POINT('Ctrl Pts',(-27.4267792630848,-76.4456285567623,
16.895967803261));
#257489=CARTESIAN_POINT('Ctrl Pts',(-27.4390220462594,-76.4460413746579,
16.9059171754193));
#257490=CARTESIAN_POINT('Ctrl Pts',(-27.4514363729675,-76.4465283265827,
16.9156217934255));
#257491=CARTESIAN_POINT('Ctrl Pts',(-27.4831955265322,-76.4477740792784,
16.9404487905547));
#257492=CARTESIAN_POINT('Ctrl Pts',(-27.5161304124239,-76.4494849825232,
16.9638340074586));
#257493=CARTESIAN_POINT('Ctrl Pts',(-27.549927682776,-76.4515669382227,
16.985939396363));
#257494=CARTESIAN_POINT('Ctrl Pts',(-27.5849567239488,-76.4537247726028,
17.0088504353318));
#257495=CARTESIAN_POINT('Ctrl Pts',(-27.6209122535109,-76.4562812377412,
17.0303866179415));
#257496=CARTESIAN_POINT('Ctrl Pts',(-27.6574962538552,-76.4591476533534,
17.0507077973783));
#257497=CARTESIAN_POINT('Ctrl Pts',(-27.6872643839296,-76.4614800345033,
17.0672429905514));
#257498=CARTESIAN_POINT('Ctrl Pts',(-27.7174496690679,-76.4640179659447,
17.0829733141275));
#257499=CARTESIAN_POINT('Ctrl Pts',(-27.7479141287996,-76.466720752886,
17.0979758062082));
#257500=CARTESIAN_POINT('Ctrl Pts',(-27.7590185974006,-76.4677059340771,
17.1034442997812));
#257501=CARTESIAN_POINT('Ctrl Pts',(-27.7701762979155,-76.4687146852109,
17.1088237343903));
#257502=CARTESIAN_POINT('Ctrl Pts',(-27.7813854912832,-76.4697457322936,
17.1141186859287));
#257503=CARTESIAN_POINT('Ctrl Pts',(-27.8105649841822,-76.4724297283708,
17.1279023718504));
#257504=CARTESIAN_POINT('Ctrl Pts',(-27.8401032155254,-76.4752686565444,
17.1410999474288));
#257505=CARTESIAN_POINT('Ctrl Pts',(-27.8698177822912,-76.4782264005106,
17.153724205322));
#257506=CARTESIAN_POINT('Ctrl Pts',(-27.9019384501864,-76.4814236442195,
17.1673706972397));
#257507=CARTESIAN_POINT('Ctrl Pts',(-27.9342655910722,-76.4847597640857,
17.1803475370885));
#257508=CARTESIAN_POINT('Ctrl Pts',(-27.9666279531484,-76.4881996908359,
17.1926699656366));
#257509=CARTESIAN_POINT('Ctrl Pts',(-27.9708830865778,-76.48865198623,17.1942901680656));
#257510=CARTESIAN_POINT('Ctrl Pts',(-27.9751389006255,-76.4891060895142,
17.1958990522121));
#257511=CARTESIAN_POINT('Ctrl Pts',(-27.979395067814,-76.4895619325381,
17.1974966476085));
#257512=CARTESIAN_POINT('Ctrl Pts',(-28.0198765024774,-76.4938975656967,
17.2126917634941));
#257513=CARTESIAN_POINT('Ctrl Pts',(-28.0605401919919,-76.4984031419535,
17.2269450615715));
#257514=CARTESIAN_POINT('Ctrl Pts',(-28.10150010376,-76.5030665766328,17.2404146413998));
#257515=CARTESIAN_POINT('Ctrl Pts',(-28.1053811610869,-76.5035084491015,
17.2416909188434));
#257516=CARTESIAN_POINT('Ctrl Pts',(-28.1092649053641,-76.5039517474116,
17.2429601347045));
#257517=CARTESIAN_POINT('Ctrl Pts',(-28.1131514503915,-76.5043964665191,
17.2442224078978));
#257518=CARTESIAN_POINT('Ctrl Pts',(-28.1390735397251,-76.5073626095461,
17.2526413914032));
#257519=CARTESIAN_POINT('Ctrl Pts',(-28.1650771837685,-76.5103875491059,
17.2607374323178));
#257520=CARTESIAN_POINT('Ctrl Pts',(-28.191151897564,-76.5134649041889,
17.2685330721677));
#257521=CARTESIAN_POINT('Ctrl Pts',(-28.2515584771378,-76.5205941289295,
17.2865930187743));
#257522=CARTESIAN_POINT('Ctrl Pts',(-28.3123340562775,-76.5280003772075,
17.303051799992));
#257523=CARTESIAN_POINT('Ctrl Pts',(-28.3734477222549,-76.5356394395893,
17.3181020343185));
#257524=CARTESIAN_POINT('Ctrl Pts',(-28.4368410864034,-76.5435634588014,
17.3337136814015));
#257525=CARTESIAN_POINT('Ctrl Pts',(-28.5005983553654,-76.5517380600939,
17.3478096642164));
#257526=CARTESIAN_POINT('Ctrl Pts',(-28.5647256406029,-76.560127644322,
17.3605684035069));
#257527=CARTESIAN_POINT('Ctrl Pts',(-28.5930332346632,-76.5638310436439,
17.3662004712176));
#257528=CARTESIAN_POINT('Ctrl Pts',(-28.6214134363092,-76.5675765027203,
17.371571505338));
#257529=CARTESIAN_POINT('Ctrl Pts',(-28.6498690551224,-76.5713617072221,
17.3766947662573));
#257530=CARTESIAN_POINT('Ctrl Pts',(-28.7073884190778,-76.5790130100039,
17.3870507775391));
#257531=CARTESIAN_POINT('Ctrl Pts',(-28.7652559670471,-76.5868350946839,
17.3963736583745));
#257532=CARTESIAN_POINT('Ctrl Pts',(-28.8232282289088,-76.5947786108553,
17.4047210505686));
#257533=CARTESIAN_POINT('Ctrl Pts',(-28.8406235592908,-76.5971621660894,
17.4072257940508));
#257534=CARTESIAN_POINT('Ctrl Pts',(-28.8580286627899,-76.599556723492,
17.4096426038302));
#257535=CARTESIAN_POINT('Ctrl Pts',(-28.8754377812505,-76.6019611150693,
17.4119727726841));
#257536=CARTESIAN_POINT('Ctrl Pts',(-28.9534501083453,-76.6127354792404,
17.4224145360179));
#257537=CARTESIAN_POINT('Ctrl Pts',(-29.0319245447185,-76.6237599571619,
17.4311687491825));
#257538=CARTESIAN_POINT('Ctrl Pts',(-29.1101764699068,-76.6349137015798,
17.4382612976246));
#257539=CARTESIAN_POINT('Ctrl Pts',(-29.1220414733971,-76.6366048959643,
17.4393367102974));
#257540=CARTESIAN_POINT('Ctrl Pts',(-29.1339014546529,-76.6382990798944,
17.4403739004352));
#257541=CARTESIAN_POINT('Ctrl Pts',(-29.1457541224843,-76.6399958502497,
17.4413729364037));
#257542=CARTESIAN_POINT('Ctrl Pts',(-29.2553480584429,-76.6556847857963,
17.4506103743807));
#257543=CARTESIAN_POINT('Ctrl Pts',(-29.3650148904473,-76.6716864103373,
17.4567325787024));
#257544=CARTESIAN_POINT('Ctrl Pts',(-29.4748980629263,-76.687990965673,
17.4599100504931));
#257545=CARTESIAN_POINT('Ctrl Pts',(-29.5348562263547,-76.6968876071823,
17.4616438498422));
#257546=CARTESIAN_POINT('Ctrl Pts',(-29.5948790589239,-76.7058745786832,
17.4625));
#257547=CARTESIAN_POINT('Ctrl Pts',(-29.6549915892153,-76.7149512087495,
17.4625));
#257548=CARTESIAN_POINT('Origin',(-76.3890311653897,-109.438478010978,16.1925));
#257549=CARTESIAN_POINT('Origin',(-90.,-90.,16.1925));
#257550=CARTESIAN_POINT('Origin',(-109.438478010978,-76.3890311653897,16.1925));
#257551=CARTESIAN_POINT('Origin',(-109.438478010978,-76.3890311653897,16.1925));
#257552=CARTESIAN_POINT('Ctrl Pts',(-76.7149512087495,-29.6549915892152,
17.4625));
#257553=CARTESIAN_POINT('Ctrl Pts',(-76.7033985679887,-29.5784809832302,
17.4625));
#257554=CARTESIAN_POINT('Ctrl Pts',(-76.6919419131574,-29.5017645218705,
17.4610789773399));
#257555=CARTESIAN_POINT('Ctrl Pts',(-76.6806292437899,-29.4251260133434,
17.4582328812589));
#257556=CARTESIAN_POINT('Ctrl Pts',(-76.6702893457237,-29.3550776153601,
17.4556315196874));
#257557=CARTESIAN_POINT('Ctrl Pts',(-76.6600693732909,-29.2850917388382,
17.4518390792962));
#257558=CARTESIAN_POINT('Ctrl Pts',(-76.6500111634973,-29.21539597266,17.4468147853486));
#257559=CARTESIAN_POINT('Ctrl Pts',(-76.6464922781968,-29.1910127660907,
17.4450570258188));
#257560=CARTESIAN_POINT('Ctrl Pts',(-76.6429932651689,-29.166665340609,
17.4431481665629));
#257561=CARTESIAN_POINT('Ctrl Pts',(-76.6395162005647,-29.1423646235818,
17.4410854028152));
#257562=CARTESIAN_POINT('Ctrl Pts',(-76.6294085410564,-29.0717236083913,
17.4350890478489));
#257563=CARTESIAN_POINT('Ctrl Pts',(-76.6194570017585,-29.0013000923935,
17.4278165327585));
#257564=CARTESIAN_POINT('Ctrl Pts',(-76.6096539020096,-28.9308900430995,
17.4191389458411));
#257565=CARTESIAN_POINT('Ctrl Pts',(-76.6071065955256,-28.9125941999784,
17.4168841005385));
#257566=CARTESIAN_POINT('Ctrl Pts',(-76.6045693606066,-28.8942993976632,
17.4145341520304));
#257567=CARTESIAN_POINT('Ctrl Pts',(-76.6020421698846,-28.8760023419532,
17.4120863380179));
#257568=CARTESIAN_POINT('Ctrl Pts',(-76.5928749254408,-28.8096307852544,
17.4032070281938));
#257569=CARTESIAN_POINT('Ctrl Pts',(-76.5838841660453,-28.7435548276822,
17.3930871840637));
#257570=CARTESIAN_POINT('Ctrl Pts',(-76.5750605976985,-28.6775616926014,
17.3815966638225));
#257571=CARTESIAN_POINT('Ctrl Pts',(-76.5737803361226,-28.6679863743407,
17.3799294390701));
#257572=CARTESIAN_POINT('Ctrl Pts',(-76.5725036108744,-28.6584128434679,
17.3782332812954));
#257573=CARTESIAN_POINT('Ctrl Pts',(-76.5712304108411,-28.6488404954761,
17.3765077138038));
#257574=CARTESIAN_POINT('Ctrl Pts',(-76.563925484898,-28.5939195943194,
17.3666073506194));
#257575=CARTESIAN_POINT('Ctrl Pts',(-76.5567364098782,-28.5390197213025,
17.3557157603908));
#257576=CARTESIAN_POINT('Ctrl Pts',(-76.5497009035193,-28.484280921732,
17.3437734778842));
#257577=CARTESIAN_POINT('Ctrl Pts',(-76.5432423739851,-28.4340312118097,
17.3328105733909));
#257578=CARTESIAN_POINT('Ctrl Pts',(-76.5369132259047,-28.3839169544081,
17.3209620182557));
#257579=CARTESIAN_POINT('Ctrl Pts',(-76.5307511868706,-28.3340851368099,
17.3081680846594));
#257580=CARTESIAN_POINT('Ctrl Pts',(-76.5246049576135,-28.2843811713595,
17.2954069761129));
#257581=CARTESIAN_POINT('Ctrl Pts',(-76.5186248279338,-28.234957370753,
17.2817053135994));
#257582=CARTESIAN_POINT('Ctrl Pts',(-76.512858617674,-28.1860085131821,
17.2669910566475));
#257583=CARTESIAN_POINT('Ctrl Pts',(-76.5099687247737,-28.1614764636039,
17.25961660709));
#257584=CARTESIAN_POINT('Ctrl Pts',(-76.5071248960926,-28.1370017452464,
17.2519719554799));
#257585=CARTESIAN_POINT('Ctrl Pts',(-76.504333615174,-28.1126036317569,
17.2440428740805));
#257586=CARTESIAN_POINT('Ctrl Pts',(-76.499480627012,-28.0701844846356,
17.2302571823893));
#257587=CARTESIAN_POINT('Ctrl Pts',(-76.4947829028971,-28.0279824912673,
17.2156101298114));
#257588=CARTESIAN_POINT('Ctrl Pts',(-76.4902767919876,-27.9860694427833,
17.1999930540216));
#257589=CARTESIAN_POINT('Ctrl Pts',(-76.4860370666911,-27.9466341480291,
17.185299205465));
#257590=CARTESIAN_POINT('Ctrl Pts',(-76.4819669295053,-27.9074544475136,
17.1697465428116));
#257591=CARTESIAN_POINT('Ctrl Pts',(-76.4781067108528,-27.8686308800552,
17.1532283189207));
#257592=CARTESIAN_POINT('Ctrl Pts',(-76.4750374372299,-27.8377621230565,
17.1400946201722));
#257593=CARTESIAN_POINT('Ctrl Pts',(-76.4721010301308,-27.8071191438596,
17.1263502154691));
#257594=CARTESIAN_POINT('Ctrl Pts',(-76.4693230827014,-27.7767742650351,
17.1119338317457));
#257595=CARTESIAN_POINT('Ctrl Pts',(-76.4684451804744,-27.7671845095149,
17.1073778868631));
#257596=CARTESIAN_POINT('Ctrl Pts',(-76.467584249049,-27.7576382281075,
17.1027621986445));
#257597=CARTESIAN_POINT('Ctrl Pts',(-76.4667411216774,-27.7481373827148,
17.0980845986402));
#257598=CARTESIAN_POINT('Ctrl Pts',(-76.4639366455395,-27.7165349284599,
17.0825256000408));
#257599=CARTESIAN_POINT('Ctrl Pts',(-76.4613252274425,-27.685414621086,
17.066275842837));
#257600=CARTESIAN_POINT('Ctrl Pts',(-76.458937921224,-27.6548074136743,
17.049210448547));
#257601=CARTESIAN_POINT('Ctrl Pts',(-76.4566163020363,-27.6250423674227,
17.0326146107265));
#257602=CARTESIAN_POINT('Ctrl Pts',(-76.4545065513622,-27.5957623497606,
17.0152474880236));
#257603=CARTESIAN_POINT('Ctrl Pts',(-76.4526490486054,-27.5670390174958,
16.9969759720477));
#257604=CARTESIAN_POINT('Ctrl Pts',(-76.4508674344959,-27.5394891827278,
16.9794509425192));
#257605=CARTESIAN_POINT('Ctrl Pts',(-76.44931782781,-27.5124513532953,16.9610939515419));
#257606=CARTESIAN_POINT('Ctrl Pts',(-76.4480477751689,-27.4860313730415,
16.9417696634897));
#257607=CARTESIAN_POINT('Ctrl Pts',(-76.4474316175615,-27.4732138950141,
16.9323946134282));
#257608=CARTESIAN_POINT('Ctrl Pts',(-76.4468814440248,-27.4605425003966,
16.9227916184998));
#257609=CARTESIAN_POINT('Ctrl Pts',(-76.4464038210194,-27.4480332789741,
16.9129435541778));
#257610=CARTESIAN_POINT('Ctrl Pts',(-76.4460214621022,-27.438019078853,
16.9050597312288));
#257611=CARTESIAN_POINT('Ctrl Pts',(-76.4456876024435,-27.4281096389905,
16.8970089022858));
#257612=CARTESIAN_POINT('Ctrl Pts',(-76.4454060812472,-27.4183213434192,
16.8887879984481));
#257613=CARTESIAN_POINT('Ctrl Pts',(-76.4447418189892,-27.3952254081783,
16.8693903963557));
#257614=CARTESIAN_POINT('Ctrl Pts',(-76.4443701445099,-27.3726021898374,
16.8488671319479));
#257615=CARTESIAN_POINT('Ctrl Pts',(-76.444362546377,-27.3508659754085,
16.8272552303423));
#257616=CARTESIAN_POINT('Ctrl Pts',(-76.4443549276361,-27.3290708073665,
16.8055847122886));
#257617=CARTESIAN_POINT('Ctrl Pts',(-76.4447134034008,-27.3081675781732,
16.7828195228054));
#257618=CARTESIAN_POINT('Ctrl Pts',(-76.4455134941452,-27.288614227559,
16.7590305376019));
#257619=CARTESIAN_POINT('Ctrl Pts',(-76.4463225383091,-27.2688420650766,
16.73497534164));
#257620=CARTESIAN_POINT('Ctrl Pts',(-76.4475831876929,-27.2504503196115,
16.7098732026983));
#257621=CARTESIAN_POINT('Ctrl Pts',(-76.4493763637529,-27.2339516171425,
16.6838334538418));
#257622=CARTESIAN_POINT('Ctrl Pts',(-76.4496312380366,-27.2316065629849,
16.6801322766471));
#257623=CARTESIAN_POINT('Ctrl Pts',(-76.4498968745481,-27.2292998143657,
16.6764122174925));
#257624=CARTESIAN_POINT('Ctrl Pts',(-76.4501735092112,-27.2270329030601,
16.6726736500804));
#257625=CARTESIAN_POINT('Ctrl Pts',(-76.4524602168079,-27.2082942415882,
16.6417700373295));
#257626=CARTESIAN_POINT('Ctrl Pts',(-76.4554866376467,-27.1920956821034,
16.6094802657886));
#257627=CARTESIAN_POINT('Ctrl Pts',(-76.4593868180784,-27.1790613975836,
16.5757650534976));
#257628=CARTESIAN_POINT('Ctrl Pts',(-76.4607025172967,-27.1746643707655,
16.5643914570108));
#257629=CARTESIAN_POINT('Ctrl Pts',(-76.4621156292997,-27.1706359107516,
16.5528759158133));
#257630=CARTESIAN_POINT('Ctrl Pts',(-76.4636289044873,-27.1669986019358,
16.5412293347378));
#257631=CARTESIAN_POINT('Ctrl Pts',(-76.4665233519918,-27.160041506815,
16.5189528725291));
#257632=CARTESIAN_POINT('Ctrl Pts',(-76.4697851638507,-27.1545628735568,
16.4962407115123));
#257633=CARTESIAN_POINT('Ctrl Pts',(-76.4733862269001,-27.1506549153936,
16.4733464731271));
#257634=CARTESIAN_POINT('Ctrl Pts',(-76.4769872899495,-27.1467469572304,
16.4504522347419));
#257635=CARTESIAN_POINT('Ctrl Pts',(-76.4809274578024,-27.1444098150617,
16.427376861687));
#257636=CARTESIAN_POINT('Ctrl Pts',(-76.4851658906466,-27.1436800109185,
16.4043845876086));
#257637=CARTESIAN_POINT('Ctrl Pts',(-76.4864717522655,-27.1434551581829,
16.3973006654719));
#257638=CARTESIAN_POINT('Ctrl Pts',(-76.4878067469539,-27.1433783458386,
16.3902160073499));
#257639=CARTESIAN_POINT('Ctrl Pts',(-76.489170196181,-27.1434490350611,
16.3831336947991));
#257640=CARTESIAN_POINT('Ctrl Pts',(-76.4931559613738,-27.1436556805576,
16.3624300013349));
#257641=CARTESIAN_POINT('Ctrl Pts',(-76.4973805033897,-27.1451242300423,
16.3417644841291));
#257642=CARTESIAN_POINT('Ctrl Pts',(-76.5018122177595,-27.1478012243613,
16.3212481482282));
#257643=CARTESIAN_POINT('Ctrl Pts',(-76.5062897351498,-27.150505886173,
16.3005197701981));
#257644=CARTESIAN_POINT('Ctrl Pts',(-76.5109787082556,-27.1544440119297,
16.279943684402));
#257645=CARTESIAN_POINT('Ctrl Pts',(-76.5158361677243,-27.1595080210179,
16.2596351519595));
#257646=CARTESIAN_POINT('Ctrl Pts',(-76.5208022798437,-27.1646853029011,
16.2388723540938));
#257647=CARTESIAN_POINT('Ctrl Pts',(-76.5259444759364,-27.1710392955909,
16.2183892248486));
#257648=CARTESIAN_POINT('Ctrl Pts',(-76.5312063612731,-27.1784017958199,
16.1983095665865));
#257649=CARTESIAN_POINT('Ctrl Pts',(-76.5317149732915,-27.179113452548,
16.1963686737572));
#257650=CARTESIAN_POINT('Ctrl Pts',(-76.5322246958761,-27.1798344925873,
16.1944315509855));
#257651=CARTESIAN_POINT('Ctrl Pts',(-76.5327354732302,-27.1805647392017,
16.1924983103146));
#257652=CARTESIAN_POINT('Ctrl Pts',(-28.7459974181807,-74.3634602878982,
19.6929518677509));
#257653=CARTESIAN_POINT('Ctrl Pts',(-28.8447420032202,-74.6189041648808,
17.4625));
#257654=CARTESIAN_POINT('Ctrl Pts',(-29.6549915892153,-76.7149512087496,
17.4625));
#257655=CARTESIAN_POINT('Ctrl Pts',(-28.493917791474,-74.4609043857738,
19.6929518673246));
#257656=CARTESIAN_POINT('Ctrl Pts',(-28.6971725259749,-74.6660793405533,
17.5374731486204));
#257657=CARTESIAN_POINT('Ctrl Pts',(-29.4834701335364,-76.6890525018752,
17.4625));
#257658=CARTESIAN_POINT('Ctrl Pts',(-28.243859153104,-74.5588475342798,
19.6720320649342));
#257659=CARTESIAN_POINT('Ctrl Pts',(-28.5391636116372,-74.7189440966798,
17.5981072780266));
#257660=CARTESIAN_POINT('Ctrl Pts',(-29.3136797628437,-76.6640386379049,
17.4555267321202));
#257661=CARTESIAN_POINT('Ctrl Pts',(-27.7480012895967,-74.7559270342226,
19.587105566441));
#257662=CARTESIAN_POINT('Ctrl Pts',(-28.2117119618043,-74.8327386313741,
17.6836912763777));
#257663=CARTESIAN_POINT('Ctrl Pts',(-28.9778332725227,-76.6159646173257,
17.4272178998376));
#257664=CARTESIAN_POINT('Ctrl Pts',(-27.4997703917942,-74.8560677628261,
19.5220948206211));
#257665=CARTESIAN_POINT('Ctrl Pts',(-28.0404430900693,-74.8942448729349,
17.7096321218675));
#257666=CARTESIAN_POINT('Ctrl Pts',(-28.8101355628285,-76.5926880471497,
17.4055476509051));
#257667=CARTESIAN_POINT('Ctrl Pts',(-27.0236898937073,-75.0518439197728,
19.3489695261652));
#257668=CARTESIAN_POINT('Ctrl Pts',(-27.7022510777803,-75.019660969593,
17.7211023712237));
#257669=CARTESIAN_POINT('Ctrl Pts',(-28.4896086814942,-76.5500480485612,
17.3478392195234));
#257670=CARTESIAN_POINT('Ctrl Pts',(-26.7953551633964,-75.1476280619459,
19.2413577159483));
#257671=CARTESIAN_POINT('Ctrl Pts',(-27.5347169152644,-75.0836522525197,
17.7080778869111));
#257672=CARTESIAN_POINT('Ctrl Pts',(-28.3364379275085,-76.5306138623674,
17.311968615636));
#257673=CARTESIAN_POINT('Ctrl Pts',(-26.4687756770164,-75.2884389844459,
19.0458961827328));
#257674=CARTESIAN_POINT('Ctrl Pts',(-27.2898012152199,-75.1803896028198,
17.6578979817808));
#257675=CARTESIAN_POINT('Ctrl Pts',(-28.11850995103,-76.5048922024804,17.2468147718755));
#257676=CARTESIAN_POINT('Ctrl Pts',(-26.3625884843543,-75.3348967090535,
18.9750294801157));
#257677=CARTESIAN_POINT('Ctrl Pts',(-27.2097290601215,-75.2125498005336,
17.6363116935578));
#257678=CARTESIAN_POINT('Ctrl Pts',(-28.0478532106475,-76.4968949507143,
17.2231925371373));
#257679=CARTESIAN_POINT('Ctrl Pts',(-26.1560856941728,-75.4268801209917,
18.8208466626393));
#257680=CARTESIAN_POINT('Ctrl Pts',(-27.0529295129821,-75.2767579129773,
17.5825320214165));
#257681=CARTESIAN_POINT('Ctrl Pts',(-27.9109420608558,-76.482236449377,
17.1717982652804));
#257682=CARTESIAN_POINT('Ctrl Pts',(-26.055101076053,-75.4727198166016,
18.7368743964311));
#257683=CARTESIAN_POINT('Ctrl Pts',(-26.9755857935384,-75.3090585336027,
17.5501254447864));
#257684=CARTESIAN_POINT('Ctrl Pts',(-27.8442489434606,-76.4755364557142,
17.1438075095173));
#257685=CARTESIAN_POINT('Ctrl Pts',(-25.7681502580856,-75.606056054722,
18.4696518487116));
#257686=CARTESIAN_POINT('Ctrl Pts',(-26.7557364160525,-75.403048816879,
17.4386060175096));
#257687=CARTESIAN_POINT('Ctrl Pts',(-27.6556756091751,-76.4581861338663,
17.0547333270725));
#257688=CARTESIAN_POINT('Ctrl Pts',(-25.5978466210038,-75.6894118596661,
18.2718409363078));
#257689=CARTESIAN_POINT('Ctrl Pts',(-26.6226482272591,-75.4628679834562,
17.3449978161574));
#257690=CARTESIAN_POINT('Ctrl Pts',(-27.5450423948282,-76.4502012574512,
16.9887963557574));
#257691=CARTESIAN_POINT('Ctrl Pts',(-25.3042070746277,-75.8449254994659,
17.8327278472479));
#257692=CARTESIAN_POINT('Ctrl Pts',(-26.394507090712,-75.573296435284,17.1202191600563));
#257693=CARTESIAN_POINT('Ctrl Pts',(-27.3578956810273,-76.4429196593766,
16.8424253269272));
#257694=CARTESIAN_POINT('Ctrl Pts',(-25.1799509742016,-75.9179115378172,
17.5873106315629));
#257695=CARTESIAN_POINT('Ctrl Pts',(-26.2977761963299,-75.6248510373193,
16.9864091667276));
#257696=CARTESIAN_POINT('Ctrl Pts',(-27.2809002299559,-76.4437878571368,
16.7606195878723));
#257697=CARTESIAN_POINT('Ctrl Pts',(-25.0456540278885,-76.0120135407793,
17.2025309630922));
#257698=CARTESIAN_POINT('Ctrl Pts',(-26.1964580005434,-75.6888631781807,
16.7690050915921));
#257699=CARTESIAN_POINT('Ctrl Pts',(-27.2023521345511,-76.4531141362207,
16.6323596984796));
#257700=CARTESIAN_POINT('Ctrl Pts',(-25.0090870943377,-76.0410349984124,
17.0710669460344));
#257701=CARTESIAN_POINT('Ctrl Pts',(-26.1695156242371,-75.7081633852743,
16.6936245453249));
#257702=CARTESIAN_POINT('Ctrl Pts',(-27.1820075724725,-76.4575269782808,
16.5885383593541));
#257703=CARTESIAN_POINT('Ctrl Pts',(-24.9530103267672,-76.0942893550639,
16.8014952531461));
#257704=CARTESIAN_POINT('Ctrl Pts',(-26.1301341325902,-75.7423750031977,
16.5376305767303));
#257705=CARTESIAN_POINT('Ctrl Pts',(-27.1534935975724,-76.4691181075122,
16.4986811285387));
#257706=CARTESIAN_POINT('Ctrl Pts',(-24.9335061597325,-76.1186539510276,
16.662354041917));
#257707=CARTESIAN_POINT('Ctrl Pts',(-26.1176802211135,-75.7573877351405,
16.4562866616969));
#257708=CARTESIAN_POINT('Ctrl Pts',(-27.1453691430058,-76.4763708127826,
16.4523007247637));
#257709=CARTESIAN_POINT('Ctrl Pts',(-24.9029553648527,-76.1824010629028,
16.246342504105));
#257710=CARTESIAN_POINT('Ctrl Pts',(-26.1038934519079,-75.7942282194349,
16.2122544249952));
#257711=CARTESIAN_POINT('Ctrl Pts',(-27.1404954668515,-76.501838453202,
16.3136302120348));
#257712=CARTESIAN_POINT('Ctrl Pts',(-24.9185412707841,-76.21319040096,15.9685880799942));
#257713=CARTESIAN_POINT('Ctrl Pts',(-26.1252772492182,-75.8084359405768,
16.0475610164003));
#257714=CARTESIAN_POINT('Ctrl Pts',(-27.1624313528542,-76.5237673449983,
16.2210111173695));
#257715=CARTESIAN_POINT('Ctrl Pts',(-24.9689556265491,-76.2326069140441,
15.6905058513849));
#257716=CARTESIAN_POINT('Ctrl Pts',(-26.1756393943756,-75.8121214408373,
15.8859547915794));
#257717=CARTESIAN_POINT('Ctrl Pts',(-27.2087011009323,-76.55044485681,16.128351327878));
#257718=CARTESIAN_POINT('',(-25.2552738567447,-75.9418613629793,17.263393070432));
#257719=CARTESIAN_POINT('Ctrl Pts',(-27.1270026655083,-76.4952182372905,
16.124851038856));
#257720=CARTESIAN_POINT('Ctrl Pts',(-27.1261035938166,-76.4949835330535,
16.1335301302474));
#257721=CARTESIAN_POINT('Ctrl Pts',(-27.1250175086501,-76.4945938617305,
16.1433840167284));
#257722=CARTESIAN_POINT('Ctrl Pts',(-27.1236651982618,-76.4938946426406,
16.155016623084));
#257723=CARTESIAN_POINT('Ctrl Pts',(-27.1234107356413,-76.4937630714248,
16.1572055166414));
#257724=CARTESIAN_POINT('Ctrl Pts',(-27.1231468673316,-76.4936205663266,
16.1594572469012));
#257725=CARTESIAN_POINT('Ctrl Pts',(-27.1228730977808,-76.4934661405628,
16.1617756124861));
#257726=CARTESIAN_POINT('Ctrl Pts',(-27.1215904130528,-76.4927426139022,
16.1726377851477));
#257727=CARTESIAN_POINT('Ctrl Pts',(-27.1200357216283,-76.4916920130626,
16.1853170892738));
#257728=CARTESIAN_POINT('Ctrl Pts',(-27.1184437830652,-76.4903847974138,
16.1985845365603));
#257729=CARTESIAN_POINT('Ctrl Pts',(-27.1177371697055,-76.4898045639408,
16.2044735549672));
#257730=CARTESIAN_POINT('Ctrl Pts',(-27.1170231040098,-76.4891738033059,
16.2104789373705));
#257731=CARTESIAN_POINT('Ctrl Pts',(-27.1163213320445,-76.4884987572074,
16.216496794303));
#257732=CARTESIAN_POINT('Ctrl Pts',(-27.1144314500968,-76.4866808484018,
16.2327029691598));
#257733=CARTESIAN_POINT('Ctrl Pts',(-27.1126943705564,-76.4846005967063,
16.2486914456382));
#257734=CARTESIAN_POINT('Ctrl Pts',(-27.1111721910325,-76.4824017849017,
16.2640972093694));
#257735=CARTESIAN_POINT('Ctrl Pts',(-27.1106324721765,-76.481622152688,
16.2695596275976));
#257736=CARTESIAN_POINT('Ctrl Pts',(-27.1101196624094,-76.4808275267717,
16.2749492144025));
#257737=CARTESIAN_POINT('Ctrl Pts',(-27.1096361423663,-76.4800239584191,
16.2802512670944));
#257738=CARTESIAN_POINT('Ctrl Pts',(-27.1088775098617,-76.4787631770293,
16.2885700732554));
#257739=CARTESIAN_POINT('Ctrl Pts',(-27.1081924682407,-76.4774861247357,
16.2966391164394));
#257740=CARTESIAN_POINT('Ctrl Pts',(-27.1075731179889,-76.4761760059692,
16.304634384641));
#257741=CARTESIAN_POINT('Ctrl Pts',(-27.1070239809322,-76.4750144099882,
16.3117232621132));
#257742=CARTESIAN_POINT('Ctrl Pts',(-27.1065264227133,-76.4738263115719,
16.3187548885459));
#257743=CARTESIAN_POINT('Ctrl Pts',(-27.1060881023893,-76.4726008566098,
16.3258128070649));
#257744=CARTESIAN_POINT('Ctrl Pts',(-27.1060320583288,-76.4724441687532,
16.3267152393526));
#257745=CARTESIAN_POINT('Ctrl Pts',(-27.1059770032837,-76.472286877024,
16.3276180342305));
#257746=CARTESIAN_POINT('Ctrl Pts',(-27.1059229723693,-76.4721289660915,
16.3285213027645));
#257747=CARTESIAN_POINT('Ctrl Pts',(-27.1055132758134,-76.4709315855559,
16.335370455917));
#257748=CARTESIAN_POINT('Ctrl Pts',(-27.1051480063898,-76.4696860988077,
16.3423105850798));
#257749=CARTESIAN_POINT('Ctrl Pts',(-27.1048249982606,-76.4683756379704,
16.3494047007319));
#257750=CARTESIAN_POINT('Ctrl Pts',(-27.1045238256026,-76.4671537647793,
16.3560192514934));
#257751=CARTESIAN_POINT('Ctrl Pts',(-27.104259651115,-76.4658752319067,
16.3627681883308));
#257752=CARTESIAN_POINT('Ctrl Pts',(-27.1040326825549,-76.4645307210503,
16.369662327317));
#257753=CARTESIAN_POINT('Ctrl Pts',(-27.1038205223624,-76.4632739316433,
16.3761066641606));
#257754=CARTESIAN_POINT('Ctrl Pts',(-27.1036411260686,-76.4619593190139,
16.3826784026693));
#257755=CARTESIAN_POINT('Ctrl Pts',(-27.103492920931,-76.4605856089551,
16.3893426844127));
#257756=CARTESIAN_POINT('Ctrl Pts',(-27.1033578602488,-76.4593337345553,
16.3954159046341));
#257757=CARTESIAN_POINT('Ctrl Pts',(-27.1032489151466,-76.4580326598464,
16.4015662355561));
#257758=CARTESIAN_POINT('Ctrl Pts',(-27.103160260747,-76.4566888072085,
16.4077247899917));
#257759=CARTESIAN_POINT('Ctrl Pts',(-27.103122501072,-76.4561164335965,
16.4103478410223));
#257760=CARTESIAN_POINT('Ctrl Pts',(-27.1030883438962,-76.4555364067352,
16.4129718046004));
#257761=CARTESIAN_POINT('Ctrl Pts',(-27.1030568879021,-76.4549497809972,
16.4155884735489));
#257762=CARTESIAN_POINT('Ctrl Pts',(-27.102943208167,-76.4528297571273,
16.4250449298059));
#257763=CARTESIAN_POINT('Ctrl Pts',(-27.1028516325168,-76.4506276154508,
16.4344055618678));
#257764=CARTESIAN_POINT('Ctrl Pts',(-27.1027493830597,-76.448361853147,
16.4434727015495));
#257765=CARTESIAN_POINT('Ctrl Pts',(-27.1027301154649,-76.4479348993889,
16.4451812873779));
#257766=CARTESIAN_POINT('Ctrl Pts',(-27.10271035294,-76.4475057389403,16.4468793703382));
#257767=CARTESIAN_POINT('Ctrl Pts',(-27.1026896905074,-76.4470745680892,
16.448565588462));
#257768=CARTESIAN_POINT('Ctrl Pts',(-27.1026199427361,-76.445619114783,
16.454257558912));
#257769=CARTESIAN_POINT('Ctrl Pts',(-27.1025406532752,-76.4441322040595,
16.45984731347));
#257770=CARTESIAN_POINT('Ctrl Pts',(-27.1024250918521,-76.4426004684731,
16.4653566991217));
#257771=CARTESIAN_POINT('Ctrl Pts',(-27.1023811860637,-76.4420185090536,
16.4674499056151));
#257772=CARTESIAN_POINT('Ctrl Pts',(-27.1023318496948,-76.441430218622,
16.4695309610855));
#257773=CARTESIAN_POINT('Ctrl Pts',(-27.1022746925434,-76.4408353908715,
16.4715995364392));
#257774=CARTESIAN_POINT('Ctrl Pts',(-27.1020976108827,-76.43899252286,16.4780083015744));
#257775=CARTESIAN_POINT('Ctrl Pts',(-27.1018561048159,-76.4370710585175,
16.484391780117));
#257776=CARTESIAN_POINT('Ctrl Pts',(-27.1015158539173,-76.4350620986711,
16.4906542061241));
#257777=CARTESIAN_POINT('Ctrl Pts',(-27.1012261996223,-76.4333518788001,
16.4959853855483));
#257778=CARTESIAN_POINT('Ctrl Pts',(-27.1008647151594,-76.431579044118,
16.5012232667718));
#257779=CARTESIAN_POINT('Ctrl Pts',(-27.1004038747174,-76.4297403585954,
16.5063087804242));
#257780=CARTESIAN_POINT('Ctrl Pts',(-27.1000801964386,-76.4284489299119,
16.5098806681233));
#257781=CARTESIAN_POINT('Ctrl Pts',(-27.0997073598881,-76.427125151566,
16.5133767163714));
#257782=CARTESIAN_POINT('Ctrl Pts',(-27.0992746306615,-76.4257650872446,
16.5168023194477));
#257783=CARTESIAN_POINT('Ctrl Pts',(-27.0988720744437,-76.4244998564365,
16.5199890647216));
#257784=CARTESIAN_POINT('Ctrl Pts',(-27.0984176364798,-76.423203394355,
16.5231136244692));
#257785=CARTESIAN_POINT('Ctrl Pts',(-27.0979025055483,-76.4218676567963,
16.5262197343028));
#257786=CARTESIAN_POINT('Ctrl Pts',(-27.0978682970963,-76.4217789540774,
16.5264260026568));
#257787=CARTESIAN_POINT('Ctrl Pts',(-27.0978338210952,-76.4216900756695,
16.5266322092065));
#257788=CARTESIAN_POINT('Ctrl Pts',(-27.0977990750253,-76.4216010180799,
16.5268383756647));
#257789=CARTESIAN_POINT('Ctrl Pts',(-27.0976706878971,-76.4212719492622,
16.5276001630984));
#257790=CARTESIAN_POINT('Ctrl Pts',(-27.0975386143434,-76.4209404362575,
16.5283613866211));
#257791=CARTESIAN_POINT('Ctrl Pts',(-27.0974027448553,-76.4206063221419,
16.5291232095991));
#257792=CARTESIAN_POINT('Ctrl Pts',(-27.0966347185483,-76.4187176830226,
16.5334295486934));
#257793=CARTESIAN_POINT('Ctrl Pts',(-27.0957491893763,-76.4167566024487,
16.5376614540029));
#257794=CARTESIAN_POINT('Ctrl Pts',(-27.0947257635357,-76.4147290835802,
16.5417599888112));
#257795=CARTESIAN_POINT('Ctrl Pts',(-27.0938722704104,-76.413038220064,
16.5451779905302));
#257796=CARTESIAN_POINT('Ctrl Pts',(-27.0929228022848,-76.4113012291759,
16.5485028098222));
#257797=CARTESIAN_POINT('Ctrl Pts',(-27.0918686181416,-76.4095163162293,
16.5517348366204));
#257798=CARTESIAN_POINT('Ctrl Pts',(-27.0910057467585,-76.4080553283051,
16.5543803169683));
#257799=CARTESIAN_POINT('Ctrl Pts',(-27.0900727245973,-76.4065622115663,
16.5569638004546));
#257800=CARTESIAN_POINT('Ctrl Pts',(-27.0890672853603,-76.4050319318842,
16.559511402245));
#257801=CARTESIAN_POINT('Ctrl Pts',(-27.0873467993633,-76.4024133502058,
16.5638708036344));
#257802=CARTESIAN_POINT('Ctrl Pts',(-27.0854160305322,-76.3996858222803,
16.5681213015841));
#257803=CARTESIAN_POINT('Ctrl Pts',(-27.0832453437817,-76.3968549739068,
16.572200145343));
#257804=CARTESIAN_POINT('Ctrl Pts',(-27.0814237924472,-76.3944794420013,
16.5756229438146));
#257805=CARTESIAN_POINT('Ctrl Pts',(-27.0794332007604,-76.3920312477964,
16.5789244111528));
#257806=CARTESIAN_POINT('Ctrl Pts',(-27.0772609129534,-76.3895078513793,
16.5821034643336));
#257807=CARTESIAN_POINT('Ctrl Pts',(-27.0758841940305,-76.3879086122794,
16.5841182354228));
#257808=CARTESIAN_POINT('Ctrl Pts',(-27.0744345916957,-76.3862790519604,
16.5860845447352));
#257809=CARTESIAN_POINT('Ctrl Pts',(-27.0729104400651,-76.3846166914257,
16.5880130337724));
#257810=CARTESIAN_POINT('Ctrl Pts',(-27.0711860864447,-76.3827359747379,
16.5901948357575));
#257811=CARTESIAN_POINT('Ctrl Pts',(-27.0694154757843,-76.3808666413311,
16.5922669270643));
#257812=CARTESIAN_POINT('Ctrl Pts',(-27.0676055223506,-76.3790011612995,
16.5942742310318));
#257813=CARTESIAN_POINT('Ctrl Pts',(-27.0627975216184,-76.3740456584721,
16.5996064781305));
#257814=CARTESIAN_POINT('Ctrl Pts',(-27.0577058759434,-76.369127427657,
16.6044118919298));
#257815=CARTESIAN_POINT('Ctrl Pts',(-27.0523503507039,-76.3642377230746,
16.6087783050424));
#257816=CARTESIAN_POINT('Ctrl Pts',(-27.0469199087843,-76.3592796180242,
16.6132057984709));
#257817=CARTESIAN_POINT('Ctrl Pts',(-27.0412180804736,-76.354350908571,
16.6171815871679));
#257818=CARTESIAN_POINT('Ctrl Pts',(-27.0352768340224,-76.3494322419925,
16.6208506593388));
#257819=CARTESIAN_POINT('Ctrl Pts',(-27.0293355875713,-76.3445135754139,
16.6245197315096));
#257820=CARTESIAN_POINT('Ctrl Pts',(-27.0231548844627,-76.3396049868145,
16.6278819111733));
#257821=CARTESIAN_POINT('Ctrl Pts',(-27.0167787754265,-76.3346762337747,
16.6311389170592));
#257822=CARTESIAN_POINT('Ctrl Pts',(-27.0069163699867,-76.3270525622668,
16.6361767720244));
#257823=CARTESIAN_POINT('Ctrl Pts',(-26.9965742763337,-76.3193994276104,
16.6408622418843));
#257824=CARTESIAN_POINT('Ctrl Pts',(-26.9857761531998,-76.3117344496374,
16.6452464533241));
#257825=CARTESIAN_POINT('Ctrl Pts',(-26.979721736166,-76.3074367608049,
16.6477046438904));
#257826=CARTESIAN_POINT('Ctrl Pts',(-26.9735241809127,-76.3031351576549,
16.6500689942483));
#257827=CARTESIAN_POINT('Ctrl Pts',(-26.9671894394037,-76.2988312337081,
16.6523553297695));
#257828=CARTESIAN_POINT('Ctrl Pts',(-26.9465400268533,-76.2848016950067,
16.6598081177547));
#257829=CARTESIAN_POINT('Ctrl Pts',(-26.9253146403781,-76.271342038953,
16.6661261478315));
#257830=CARTESIAN_POINT('Ctrl Pts',(-26.9037854166562,-76.2582666976204,
16.6722817468521));
#257831=CARTESIAN_POINT('Ctrl Pts',(-26.8683021506932,-76.2367166491816,
16.6824270618915));
#257832=CARTESIAN_POINT('Ctrl Pts',(-26.8318654947868,-76.2163231724478,
16.6915805494727));
#257833=CARTESIAN_POINT('Ctrl Pts',(-26.7948177267223,-76.1969868424102,
16.7005093018093));
#257834=CARTESIAN_POINT('Ctrl Pts',(-26.7912042243465,-76.1951008482416,
16.7013801793133));
#257835=CARTESIAN_POINT('Ctrl Pts',(-26.7875849267696,-76.1932248857237,
16.7022489427311));
#257836=CARTESIAN_POINT('Ctrl Pts',(-26.7839601625935,-76.1913588468482,
16.7031163158079));
#257837=CARTESIAN_POINT('Ctrl Pts',(-26.7552291255581,-76.1765680275182,
16.709991391477));
#257838=CARTESIAN_POINT('Ctrl Pts',(-26.7262008738672,-76.1624139946391,
16.7168106960666));
#257839=CARTESIAN_POINT('Ctrl Pts',(-26.6969732854461,-76.1489165164748,
16.7235973395646));
#257840=CARTESIAN_POINT('Ctrl Pts',(-26.6422867919235,-76.1236619610331,
16.7362955386204));
#257841=CARTESIAN_POINT('Ctrl Pts',(-26.5866819738149,-76.1005180681777,
16.7491519989614));
#257842=CARTESIAN_POINT('Ctrl Pts',(-26.5302810836782,-76.0794074083704,
16.7625435720886));
#257843=CARTESIAN_POINT('Ctrl Pts',(-26.4900870715832,-76.0643629274487,
16.772087057146));
#257844=CARTESIAN_POINT('Ctrl Pts',(-26.4494883805146,-76.0503521064273,
16.7819023270102));
#257845=CARTESIAN_POINT('Ctrl Pts',(-26.4085292238121,-76.0373611942068,
16.7921336012861));
#257846=CARTESIAN_POINT('Ctrl Pts',(-26.3637920322324,-76.0231720122119,
16.8033085988748));
#257847=CARTESIAN_POINT('Ctrl Pts',(-26.319031000209,-76.0103384192578,
16.8148454077151));
#257848=CARTESIAN_POINT('Ctrl Pts',(-26.2743222514898,-75.9987850456328,
16.826926246749));
#257849=CARTESIAN_POINT('Ctrl Pts',(-26.2161351891259,-75.9837486849451,
16.8426490874549));
#257850=CARTESIAN_POINT('Ctrl Pts',(-26.1575989600142,-75.9708594776026,
16.8592311068001));
#257851=CARTESIAN_POINT('Ctrl Pts',(-26.0990044705762,-75.9600230530921,
16.876896595295));
#257852=CARTESIAN_POINT('Ctrl Pts',(-26.0404710851734,-75.9491979291198,
16.8945436617054));
#257853=CARTESIAN_POINT('Ctrl Pts',(-25.9818779784963,-75.9404214117235,
16.9132712882849));
#257854=CARTESIAN_POINT('Ctrl Pts',(-25.9235033740091,-75.9336439589002,
16.9333228296532));
#257855=CARTESIAN_POINT('Ctrl Pts',(-25.8876307737036,-75.9294790509174,
16.9456449847295));
#257856=CARTESIAN_POINT('Ctrl Pts',(-25.8518405543476,-75.9260699331757,
16.9584675280532));
#257857=CARTESIAN_POINT('Ctrl Pts',(-25.8161989867007,-75.9234132458685,
16.9718522765889));
#257858=CARTESIAN_POINT('Ctrl Pts',(-25.7935358469314,-75.9217239577776,
16.9803631375546));
#257859=CARTESIAN_POINT('Ctrl Pts',(-25.770890405978,-75.9203357066719,
16.9891192993506));
#257860=CARTESIAN_POINT('Ctrl Pts',(-25.7483106633375,-75.9192531417283,
16.9981274246417));
#257861=CARTESIAN_POINT('Ctrl Pts',(-25.701936632811,-75.9170297815891,
17.016628214659));
#257862=CARTESIAN_POINT('Ctrl Pts',(-25.6557154305365,-75.9160908879052,
17.0360687208423));
#257863=CARTESIAN_POINT('Ctrl Pts',(-25.6100335199459,-75.9163356254781,
17.0568346693642));
#257864=CARTESIAN_POINT('Ctrl Pts',(-25.5677572969033,-75.9165621173232,
17.0760524704599));
#257865=CARTESIAN_POINT('Ctrl Pts',(-25.5259435982419,-75.9178014945593,
17.0964068028276));
#257866=CARTESIAN_POINT('Ctrl Pts',(-25.4848871407941,-75.9199460216256,
17.1181763511646));
#257867=CARTESIAN_POINT('Ctrl Pts',(-25.4448430530074,-75.9220376689679,
17.1394091062262));
#257868=CARTESIAN_POINT('Ctrl Pts',(-25.4055198689379,-75.9249898990271,
17.1619892996639));
#257869=CARTESIAN_POINT('Ctrl Pts',(-25.367171006334,-75.9286842189027,
17.1861307294231));
#257870=CARTESIAN_POINT('Ctrl Pts',(-25.3326536302604,-75.9320094343022,
17.2078601564093));
#257871=CARTESIAN_POINT('Ctrl Pts',(-25.298925636162,-75.9359354286521,
17.2308544603259));
#257872=CARTESIAN_POINT('Ctrl Pts',(-25.2661521622731,-75.9403670675906,
17.255226251548));
#257873=CARTESIAN_POINT('Ctrl Pts',(-25.2625142518049,-75.9408589869318,
17.2579315611748));
#257874=CARTESIAN_POINT('Ctrl Pts',(-25.2588880803564,-75.9413571303143,
17.2606537951814));
#257875=CARTESIAN_POINT('Ctrl Pts',(-25.2552738568381,-75.9418613633423,
17.2633930704885));
#257876=CARTESIAN_POINT('Ctrl Pts',(-25.2552738568381,-75.9418613633423,
17.2633930704885));
#257877=CARTESIAN_POINT('Ctrl Pts',(-25.2383250955278,-75.944225947726,
17.2762387760169));
#257878=CARTESIAN_POINT('Ctrl Pts',(-25.2219501075692,-75.9466297979537,
17.2896217177115));
#257879=CARTESIAN_POINT('Ctrl Pts',(-25.2063620808095,-75.9489416166775,
17.3037656233412));
#257880=CARTESIAN_POINT('Ctrl Pts',(-25.1906119974262,-75.9512774695875,
17.3180565721873));
#257881=CARTESIAN_POINT('Ctrl Pts',(-25.1756652586958,-75.9535194008974,
17.3331243158819));
#257882=CARTESIAN_POINT('Ctrl Pts',(-25.1617083519771,-75.955550118673,
17.3491621103599));
#257883=CARTESIAN_POINT('Ctrl Pts',(-25.1475411609446,-75.9576114326331,
17.3654415412317));
#257884=CARTESIAN_POINT('Ctrl Pts',(-25.1343938076753,-75.9594551437225,
17.3827204211343));
#257885=CARTESIAN_POINT('Ctrl Pts',(-25.1224278838339,-75.9609767648616,
17.4011633328253));
#257886=CARTESIAN_POINT('Ctrl Pts',(-25.1210536712436,-75.9611515136695,
17.4032813875434));
#257887=CARTESIAN_POINT('Ctrl Pts',(-25.1196950053566,-75.9613220336047,
17.4054147552051));
#257888=CARTESIAN_POINT('Ctrl Pts',(-25.1183521036895,-75.9614881812303,
17.4075636545405));
#257889=CARTESIAN_POINT('Origin',(-29.6549915892153,-76.7149512087495,20.0025));
#257890=CARTESIAN_POINT('Origin',(0.,0.,20.0025));
#257891=CARTESIAN_POINT('Origin',(-76.7149512087496,-29.6549915892152,20.0025));
#257892=CARTESIAN_POINT('Ctrl Pts',(-76.2325975651779,-24.9689313575498,
15.6906397325508));
#257893=CARTESIAN_POINT('Ctrl Pts',(-75.8121196590786,-26.1756150602386,
15.8860328844659));
#257894=CARTESIAN_POINT('Ctrl Pts',(-76.5504320086843,-27.2086788182716,
16.1283959549333));
#257895=CARTESIAN_POINT('Ctrl Pts',(-76.2132400197751,-24.9186909562154,
15.9678244963475));
#257896=CARTESIAN_POINT('Ctrl Pts',(-75.808442527959,-26.1254229642324,
16.0471243598414));
#257897=CARTESIAN_POINT('Ctrl Pts',(-76.5238417787853,-27.1625656651766,
16.2207578908871));
#257898=CARTESIAN_POINT('Ctrl Pts',(-76.1826381079972,-24.9032159272864,
16.2438456162091));
#257899=CARTESIAN_POINT('Ctrl Pts',(-75.7943214248689,-26.1041848761176,
16.2107725763333));
#257900=CARTESIAN_POINT('Ctrl Pts',(-76.5020517602985,-27.1407766635666,
16.3127979160875));
#257901=CARTESIAN_POINT('Ctrl Pts',(-76.1197004175053,-24.9328226963043,
16.6559867599157));
#257902=CARTESIAN_POINT('Ctrl Pts',(-75.7580138780931,-26.1172873190749,
16.4525591935377));
#257903=CARTESIAN_POINT('Ctrl Pts',(-76.4767312134554,-27.1451435881163,
16.4501782974209));
#257904=CARTESIAN_POINT('Ctrl Pts',(-76.0956371509854,-24.9518097701924,
16.7941104173068));
#257905=CARTESIAN_POINT('Ctrl Pts',(-75.7432179427285,-26.1293351405288,
16.5333292440503));
#257906=CARTESIAN_POINT('Ctrl Pts',(-76.4694807636038,-27.1529468723198,
16.4962195166114));
#257907=CARTESIAN_POINT('Ctrl Pts',(-76.0425032131365,-25.007333665712,
17.0641682497331));
#257908=CARTESIAN_POINT('Ctrl Pts',(-75.7091288541233,-26.1682415554308,
16.6896570718777));
#257909=CARTESIAN_POINT('Ctrl Pts',(-76.4577808154574,-27.1810555370838,
16.5862387939012));
#257910=CARTESIAN_POINT('Ctrl Pts',(-76.0135981896351,-25.0435822919597,
17.1955505586787));
#257911=CARTESIAN_POINT('Ctrl Pts',(-75.6899232799147,-26.1949210471997,
16.765020182014));
#257912=CARTESIAN_POINT('Ctrl Pts',(-76.4533313045579,-27.2011812093656,
16.6300328970334));
#257913=CARTESIAN_POINT('Ctrl Pts',(-75.920106096032,-25.1764553135866,
17.5792969885106));
#257914=CARTESIAN_POINT('Ctrl Pts',(-75.6263767700417,-26.2950899509087,
16.9819673365851));
#257915=CARTESIAN_POINT('Ctrl Pts',(-76.4438901441625,-27.2787774842959,
16.7579483734717));
#257916=CARTESIAN_POINT('Ctrl Pts',(-75.847668483287,-25.2993526607363,
17.8240388353672));
#257917=CARTESIAN_POINT('Ctrl Pts',(-75.5752351470897,-26.3907356809332,
17.1155820316983));
#257918=CARTESIAN_POINT('Ctrl Pts',(-76.4428939284363,-27.3548544480353,
16.8395289896477));
#257919=CARTESIAN_POINT('Ctrl Pts',(-75.692343203007,-25.5919984567925,
18.2644739211062));
#257920=CARTESIAN_POINT('Ctrl Pts',(-75.4649619696469,-26.6180940171699,
17.3414092350346));
#257921=CARTESIAN_POINT('Ctrl Pts',(-76.4499649794122,-27.5412643883023,
16.9863406840095));
#257922=CARTESIAN_POINT('Ctrl Pts',(-75.6091210995778,-25.7617839502732,
18.4627331486827));
#257923=CARTESIAN_POINT('Ctrl Pts',(-75.4052371346463,-26.7507911294736,
17.4354381030785));
#257924=CARTESIAN_POINT('Ctrl Pts',(-76.4578597275968,-27.6515244073506,
17.0524270937456));
#257925=CARTESIAN_POINT('Ctrl Pts',(-75.4317357552702,-26.1430805994651,
18.8197595498718));
#257926=CARTESIAN_POINT('Ctrl Pts',(-75.2796463045429,-27.0442130694172,
17.5855829975131));
#257927=CARTESIAN_POINT('Ctrl Pts',(-76.480799671864,-27.9020344677421,
17.1714358939387));
#257928=CARTESIAN_POINT('Ctrl Pts',(-75.3392616135105,-26.3510560884165,
18.9747290102614));
#257929=CARTESIAN_POINT('Ctrl Pts',(-75.2146749685608,-27.203130220885,
17.6396375078348));
#257930=CARTESIAN_POINT('Ctrl Pts',(-76.4956562029921,-28.0399748698363,
17.2230923811499));
#257931=CARTESIAN_POINT('Ctrl Pts',(-75.1503919246079,-26.7887981118754,
19.2381193325709));
#257932=CARTESIAN_POINT('Ctrl Pts',(-75.085497318848,-27.5299162784617,
17.7075896666724));
#257933=CARTESIAN_POINT('Ctrl Pts',(-76.5300629685869,-28.3320433237824,
17.3108891546269));
#257934=CARTESIAN_POINT('Ctrl Pts',(-75.052591949809,-27.021891012889,19.3482083029788));
#257935=CARTESIAN_POINT('Ctrl Pts',(-75.0201494871657,-27.7009559314819,
17.7210643477395));
#257936=CARTESIAN_POINT('Ctrl Pts',(-76.5498913973924,-28.4884000162543,
17.3475854788264));
#257937=CARTESIAN_POINT('Ctrl Pts',(-74.856579759635,-27.4985053196498,
19.521741160188));
#257938=CARTESIAN_POINT('Ctrl Pts',(-74.8945599897644,-28.0395707962217,
17.709745105584));
#257939=CARTESIAN_POINT('Ctrl Pts',(-76.5925703049492,-28.8092814008565,
17.4054297637286));
#257940=CARTESIAN_POINT('Ctrl Pts',(-74.7582415292722,-27.7422284005858,
19.5858151824391));
#257941=CARTESIAN_POINT('Ctrl Pts',(-74.8341192521338,-28.2078168588121,
17.6844550416321));
#257942=CARTESIAN_POINT('Ctrl Pts',(-76.6154156279985,-28.9739291008627,
17.4267877716098));
#257943=CARTESIAN_POINT('Ctrl Pts',(-74.5605143304925,-28.23961600078,19.6716009699542));
#257944=CARTESIAN_POINT('Ctrl Pts',(-74.7198525855419,-28.5364711009162,
17.5990670510742));
#257945=CARTESIAN_POINT('Ctrl Pts',(-76.663616773131,-29.3108001463009,
17.4553830340207));
#257946=CARTESIAN_POINT('Ctrl Pts',(-74.4605859662119,-28.4947415154361,
19.6929518687096));
#257947=CARTESIAN_POINT('Ctrl Pts',(-74.6659231009745,-28.6976612611827,
17.5372248464359));
#257948=CARTESIAN_POINT('Ctrl Pts',(-76.6891359364477,-29.4840227026748,
17.4625));
#257949=CARTESIAN_POINT('Ctrl Pts',(-74.3634602878982,-28.7459974181806,
19.6929518677509));
#257950=CARTESIAN_POINT('Ctrl Pts',(-74.6189041648808,-28.8447420032201,
17.4625));
#257951=CARTESIAN_POINT('Ctrl Pts',(-76.7149512087496,-29.6549915892153,
17.4625));
#257952=CARTESIAN_POINT('',(-75.9418613633423,-25.2552738568382,17.2633930704886));
#257953=CARTESIAN_POINT('Ctrl Pts',(-75.961488153786,-25.11835232551,17.4075632995853));
#257954=CARTESIAN_POINT('Ctrl Pts',(-75.9600460003609,-25.1300086288942,
17.3889110252656));
#257955=CARTESIAN_POINT('Ctrl Pts',(-75.95827300491,-25.1428552490709,17.3714318668807));
#257956=CARTESIAN_POINT('Ctrl Pts',(-75.9562706193827,-25.1567358844424,
17.354967018413));
#257957=CARTESIAN_POINT('Ctrl Pts',(-75.9542900252234,-25.1704654609745,
17.3386813520096));
#257958=CARTESIAN_POINT('Ctrl Pts',(-75.9520849723632,-25.185206735533,
17.3233881142745));
#257959=CARTESIAN_POINT('Ctrl Pts',(-75.949770932865,-25.2007766447904,
17.308897933323));
#257960=CARTESIAN_POINT('Ctrl Pts',(-75.9474896654476,-25.2161260485969,
17.2946129664053));
#257961=CARTESIAN_POINT('Ctrl Pts',(-75.9451024554286,-25.2322808242905,
17.2811085191579));
#257962=CARTESIAN_POINT('Ctrl Pts',(-75.9427372332863,-25.2490337245244,
17.2681673909986));
#257963=CARTESIAN_POINT('Ctrl Pts',(-75.9424448314779,-25.2511048104648,
17.2665675373488));
#257964=CARTESIAN_POINT('Ctrl Pts',(-75.9421527879415,-25.2531849967398,
17.2649762470519));
#257965=CARTESIAN_POINT('Ctrl Pts',(-75.9418613633423,-25.2552738568382,
17.2633930704886));
#257966=CARTESIAN_POINT('Ctrl Pts',(-75.9418613633423,-25.2552738568382,
17.2633930704886));
#257967=CARTESIAN_POINT('Ctrl Pts',(-75.9348768553987,-25.3053371638262,
17.2254493240849));
#257968=CARTESIAN_POINT('Ctrl Pts',(-75.9291204561945,-25.3572644305849,
17.1911044096247));
#257969=CARTESIAN_POINT('Ctrl Pts',(-75.9248495157407,-25.4106833635671,
17.1596330730564));
#257970=CARTESIAN_POINT('Ctrl Pts',(-75.9203244072783,-25.4672813115609,
17.1262888452528));
#257971=CARTESIAN_POINT('Ctrl Pts',(-75.917466983464,-25.5255536813971,
17.096170306839));
#257972=CARTESIAN_POINT('Ctrl Pts',(-75.9165875721914,-25.5850313991953,
17.0683598417424));
#257973=CARTESIAN_POINT('Ctrl Pts',(-75.9157960130219,-25.638567366227,
17.0433276078627));
#257974=CARTESIAN_POINT('Ctrl Pts',(-75.9166071705069,-25.6930793577886,
17.0201642486696));
#257975=CARTESIAN_POINT('Ctrl Pts',(-75.9192482119006,-25.7482100068409,
16.9981680565884));
#257976=CARTESIAN_POINT('Ctrl Pts',(-75.9203084088562,-25.7703411807131,
16.9893380943108));
#257977=CARTESIAN_POINT('Ctrl Pts',(-75.9216656968683,-25.7926041372848,
16.9807230184995));
#257978=CARTESIAN_POINT('Ctrl Pts',(-75.9233227318004,-25.8149722052004,
16.9723142805678));
#257979=CARTESIAN_POINT('Ctrl Pts',(-75.9279208772768,-25.8770418866012,
16.9489806745375));
#257980=CARTESIAN_POINT('Ctrl Pts',(-75.9347968299595,-25.9395105598234,
16.9273736682912));
#257981=CARTESIAN_POINT('Ctrl Pts',(-75.9439477443067,-26.0019469535969,
16.907190121791));
#257982=CARTESIAN_POINT('Ctrl Pts',(-75.9536417898974,-26.0680891143477,
16.8858086278184));
#257983=CARTESIAN_POINT('Ctrl Pts',(-75.9658884088744,-26.134196625868,
16.8660249929661));
#257984=CARTESIAN_POINT('Ctrl Pts',(-75.9807279241721,-26.1997753181405,
16.8475110455355));
#257985=CARTESIAN_POINT('Ctrl Pts',(-75.9863597062774,-26.224663254048,
16.8404847703678));
#257986=CARTESIAN_POINT('Ctrl Pts',(-75.9923654083886,-26.2494750768498,
16.8336416501196));
#257987=CARTESIAN_POINT('Ctrl Pts',(-75.9987489547818,-26.2741836418867,
16.8269646518771));
#257988=CARTESIAN_POINT('Ctrl Pts',(-76.0104251100451,-26.3193781190517,
16.8147517433512));
#257989=CARTESIAN_POINT('Ctrl Pts',(-76.0233691012878,-26.36448065778,16.803132555762));
#257990=CARTESIAN_POINT('Ctrl Pts',(-76.0376323915296,-26.4094030264448,
16.7919150704375));
#257991=CARTESIAN_POINT('Ctrl Pts',(-76.0576095561462,-26.4723212969538,
16.7762038602531));
#257992=CARTESIAN_POINT('Ctrl Pts',(-76.0801913923979,-26.5349890927284,
16.7613285554429));
#257993=CARTESIAN_POINT('Ctrl Pts',(-76.1054321158541,-26.5968842689899,
16.7468658576575));
#257994=CARTESIAN_POINT('Ctrl Pts',(-76.1193622332291,-26.6310436333906,
16.7388840310644));
#257995=CARTESIAN_POINT('Ctrl Pts',(-76.1341013589714,-26.6649677056329,
16.7310274121387));
#257996=CARTESIAN_POINT('Ctrl Pts',(-76.1496523368462,-26.6985700833486,
16.723222678138));
#257997=CARTESIAN_POINT('Ctrl Pts',(-76.1628884630048,-26.7271705555669,
16.7165797232898));
#257998=CARTESIAN_POINT('Ctrl Pts',(-76.1767336953015,-26.7555332799854,
16.7099108265046));
#257999=CARTESIAN_POINT('Ctrl Pts',(-76.1911702998078,-26.7835861605021,
16.7031950108476));
#258000=CARTESIAN_POINT('Ctrl Pts',(-76.2098835997088,-26.8199494179402,
16.694489703972));
#258001=CARTESIAN_POINT('Ctrl Pts',(-76.2295605860698,-26.8556888249402,
16.6856585992521));
#258002=CARTESIAN_POINT('Ctrl Pts',(-76.2502978093625,-26.8905185779364,
16.6759949656899));
#258003=CARTESIAN_POINT('Ctrl Pts',(-76.2528710428106,-26.8948405203745,
16.6747958280445));
#258004=CARTESIAN_POINT('Ctrl Pts',(-76.2554605684613,-26.8991484844249,
16.6735839226241));
#258005=CARTESIAN_POINT('Ctrl Pts',(-76.258066542157,-26.9034419491172,
16.6723579473272));
#258006=CARTESIAN_POINT('Ctrl Pts',(-76.2717835028191,-26.9260412893887,
16.665904829651));
#258007=CARTESIAN_POINT('Ctrl Pts',(-76.2859122483631,-26.9482892129603,
16.6592804200412));
#258008=CARTESIAN_POINT('Ctrl Pts',(-76.300666357626,-26.9698831287184,
16.6513762614161));
#258009=CARTESIAN_POINT('Ctrl Pts',(-76.3062184665341,-26.9780091205966,
16.6484018528137));
#258010=CARTESIAN_POINT('Ctrl Pts',(-76.3119191069635,-26.986126275202,
16.6452107769913));
#258011=CARTESIAN_POINT('Ctrl Pts',(-76.3176690330962,-26.9940602891098,
16.6418055153042));
#258012=CARTESIAN_POINT('Ctrl Pts',(-76.3232350607987,-27.0017405514616,
16.6385091632385));
#258013=CARTESIAN_POINT('Ctrl Pts',(-76.3288474189586,-27.0092489790102,
16.6350110759825));
#258014=CARTESIAN_POINT('Ctrl Pts',(-76.334399446806,-27.0164426883129,
16.6313545907255));
#258015=CARTESIAN_POINT('Ctrl Pts',(-76.3384193031335,-27.0216511776528,
16.628707171476));
#258016=CARTESIAN_POINT('Ctrl Pts',(-76.342403163236,-27.0266992744414,
16.6260035905202));
#258017=CARTESIAN_POINT('Ctrl Pts',(-76.3463237494151,-27.031517147781,
16.6231740162485));
#258018=CARTESIAN_POINT('Ctrl Pts',(-76.3499412952933,-27.0359626253308,
16.620563152904));
#258019=CARTESIAN_POINT('Ctrl Pts',(-76.3535049415088,-27.0402121121311,
16.6178449684742));
#258020=CARTESIAN_POINT('Ctrl Pts',(-76.356983025863,-27.0442217723951,
16.6150107800993));
#258021=CARTESIAN_POINT('Ctrl Pts',(-76.3604504000898,-27.0482190856404,
16.6121853190914));
#258022=CARTESIAN_POINT('Ctrl Pts',(-76.3638327372829,-27.051978040091,
16.609244457524));
#258023=CARTESIAN_POINT('Ctrl Pts',(-76.3670881331192,-27.0554667046297,
16.6062292700873));
#258024=CARTESIAN_POINT('Ctrl Pts',(-76.3704697167254,-27.0590905990513,
16.6030972059948));
#258025=CARTESIAN_POINT('Ctrl Pts',(-76.3737142822046,-27.0624228841696,
16.599885043991));
#258026=CARTESIAN_POINT('Ctrl Pts',(-76.3767636735503,-27.0654401116738,
16.5966933386584));
#258027=CARTESIAN_POINT('Ctrl Pts',(-76.3774080376897,-27.0660776793009,
16.5960189022785));
#258028=CARTESIAN_POINT('Ctrl Pts',(-76.3780436509134,-27.0667012192002,
16.5953455588284));
#258029=CARTESIAN_POINT('Ctrl Pts',(-76.3786699099352,-27.0673105708824,
16.5946745306125));
#258030=CARTESIAN_POINT('Ctrl Pts',(-76.3804986138508,-27.0690899046221,
16.5927150986791));
#258031=CARTESIAN_POINT('Ctrl Pts',(-76.3822466735199,-27.0707485693709,
16.5907819642457));
#258032=CARTESIAN_POINT('Ctrl Pts',(-76.383903674753,-27.0722790207879,
16.5888786971058));
#258033=CARTESIAN_POINT('Ctrl Pts',(-76.386590118736,-27.0747602935343,
16.5857929899537));
#258034=CARTESIAN_POINT('Ctrl Pts',(-76.3892195788868,-27.0770747169505,
16.5825794796198));
#258035=CARTESIAN_POINT('Ctrl Pts',(-76.3918035037155,-27.0792241299055,
16.5791834616252));
#258036=CARTESIAN_POINT('Ctrl Pts',(-76.394700966583,-27.0816343564549,
16.5753753647613));
#258037=CARTESIAN_POINT('Ctrl Pts',(-76.397541081989,-27.083837183862,16.5713382502742));
#258038=CARTESIAN_POINT('Ctrl Pts',(-76.4003286349106,-27.0858449594434,
16.5670618114176));
#258039=CARTESIAN_POINT('Ctrl Pts',(-76.4017815005684,-27.0868914070886,
16.5648329421093));
#258040=CARTESIAN_POINT('Ctrl Pts',(-76.4032199206492,-27.0878850122277,
16.5625400515829));
#258041=CARTESIAN_POINT('Ctrl Pts',(-76.4046437010114,-27.0888282604215,
16.5601869010573));
#258042=CARTESIAN_POINT('Ctrl Pts',(-76.4066000201685,-27.0901243132119,
16.5569535979618));
#258043=CARTESIAN_POINT('Ctrl Pts',(-76.4085291383743,-27.0913240246214,
16.5536060908145));
#258044=CARTESIAN_POINT('Ctrl Pts',(-76.4104440985978,-27.0924256407899,
16.5500691174275));
#258045=CARTESIAN_POINT('Ctrl Pts',(-76.4125548612432,-27.0936398959108,
16.5461704926879));
#258046=CARTESIAN_POINT('Ctrl Pts',(-76.4146483556021,-27.0947350221951,
16.5420420631183));
#258047=CARTESIAN_POINT('Ctrl Pts',(-76.4167317428694,-27.0957153880271,
16.5376476095181));
#258048=CARTESIAN_POINT('Ctrl Pts',(-76.4178724629974,-27.0962521691886,
16.5352415078049));
#258049=CARTESIAN_POINT('Ctrl Pts',(-76.4190099865444,-27.0967546539353,
16.5327567014452));
#258050=CARTESIAN_POINT('Ctrl Pts',(-76.4201444974393,-27.0972241915704,
16.5301935105711));
#258051=CARTESIAN_POINT('Ctrl Pts',(-76.4216120382861,-27.0978315596105,
16.526877907942));
#258052=CARTESIAN_POINT('Ctrl Pts',(-76.4230689252893,-27.0983817195864,
16.5234805955633));
#258053=CARTESIAN_POINT('Ctrl Pts',(-76.4245289971094,-27.0988766739753,
16.5198985636382));
#258054=CARTESIAN_POINT('Ctrl Pts',(-76.4261225061527,-27.0994168626729,
16.5159891667252));
#258055=CARTESIAN_POINT('Ctrl Pts',(-76.4277197747631,-27.0998913111345,
16.5118599671146));
#258056=CARTESIAN_POINT('Ctrl Pts',(-76.4293303340741,-27.1003044176607,
16.5074394223229));
#258057=CARTESIAN_POINT('Ctrl Pts',(-76.4311269682898,-27.1007652521762,
16.5025081528127));
#258058=CARTESIAN_POINT('Ctrl Pts',(-76.4329400958886,-27.1011497779037,
16.4972146199272));
#258059=CARTESIAN_POINT('Ctrl Pts',(-76.4347734732722,-27.1014658926888,
16.4915299793151));
#258060=CARTESIAN_POINT('Ctrl Pts',(-76.436559162974,-27.1017737850635,
16.4859932009684));
#258061=CARTESIAN_POINT('Ctrl Pts',(-76.4383638554399,-27.1020168312817,
16.4800869015256));
#258062=CARTESIAN_POINT('Ctrl Pts',(-76.4401848092304,-27.1022032686856,
16.4738312960571));
#258063=CARTESIAN_POINT('Ctrl Pts',(-76.4402891062215,-27.1022139470786,
16.4734729998546));
#258064=CARTESIAN_POINT('Ctrl Pts',(-76.4403934995095,-27.1022244071686,
16.4731133073643));
#258065=CARTESIAN_POINT('Ctrl Pts',(-76.4404979871102,-27.1022346589781,
16.4727522097065));
#258066=CARTESIAN_POINT('Ctrl Pts',(-76.4422544935175,-27.1024069987472,
16.466681916723));
#258067=CARTESIAN_POINT('Ctrl Pts',(-76.4439950495004,-27.1025185267252,
16.4603561173103));
#258068=CARTESIAN_POINT('Ctrl Pts',(-76.4457036742994,-27.1026104632737,
16.4538373749437));
#258069=CARTESIAN_POINT('Ctrl Pts',(-76.4480632278896,-27.1027374245665,
16.4448352101831));
#258070=CARTESIAN_POINT('Ctrl Pts',(-76.4503610777997,-27.1028277926528,
16.4354693324923));
#258071=CARTESIAN_POINT('Ctrl Pts',(-76.4525659494223,-27.102929293285,
16.425993471235));
#258072=CARTESIAN_POINT('Ctrl Pts',(-76.4530853029501,-27.1029532015756,
16.4237614492331));
#258073=CARTESIAN_POINT('Ctrl Pts',(-76.453599565861,-27.1029775126962,
16.4215234003336));
#258074=CARTESIAN_POINT('Ctrl Pts',(-76.4541084608796,-27.103002507394,
16.4192825790669));
#258075=CARTESIAN_POINT('Ctrl Pts',(-76.4554445776905,-27.1030681316087,
16.4133992458547));
#258076=CARTESIAN_POINT('Ctrl Pts',(-76.4567431175969,-27.1031446841178,
16.4074886487793));
#258077=CARTESIAN_POINT('Ctrl Pts',(-76.4579907926765,-27.1032413604333,
16.4016557351671));
#258078=CARTESIAN_POINT('Ctrl Pts',(-76.4593798496605,-27.1033489917496,
16.395161857456));
#258079=CARTESIAN_POINT('Ctrl Pts',(-76.4607059920239,-27.1034813065929,
16.3887640860712));
#258080=CARTESIAN_POINT('Ctrl Pts',(-76.4619636638711,-27.1036407247952,
16.3825411928141));
#258081=CARTESIAN_POINT('Ctrl Pts',(-76.4633071546945,-27.1038110211188,
16.3758936718375));
#258082=CARTESIAN_POINT('Ctrl Pts',(-76.4645727491349,-27.1040119033633,
16.3694449721487));
#258083=CARTESIAN_POINT('Ctrl Pts',(-76.4657643117174,-27.1042403346288,
16.3632278962589));
#258084=CARTESIAN_POINT('Ctrl Pts',(-76.467089712906,-27.1044944237345,
16.3563125064213));
#258085=CARTESIAN_POINT('Ctrl Pts',(-76.468323724667,-27.1047822481845,
16.3496832154432));
#258086=CARTESIAN_POINT('Ctrl Pts',(-76.4694807350521,-27.1050982652682,
16.3433192109917));
#258087=CARTESIAN_POINT('Ctrl Pts',(-76.4700834269585,-27.1052628799864,
16.3400041724888));
#258088=CARTESIAN_POINT('Ctrl Pts',(-76.4706653444495,-27.1054351607889,
16.3367601398851));
#258089=CARTESIAN_POINT('Ctrl Pts',(-76.4712290846745,-27.1056146245867,
16.3335788333485));
#258090=CARTESIAN_POINT('Ctrl Pts',(-76.4724339017896,-27.1059981719114,
16.3267797929504));
#258091=CARTESIAN_POINT('Ctrl Pts',(-76.4735621797735,-27.1064227170056,
16.3202525650356));
#258092=CARTESIAN_POINT('Ctrl Pts',(-76.4746356788947,-27.1068761140877,
16.313884056441));
#258093=CARTESIAN_POINT('Ctrl Pts',(-76.4758416115454,-27.1073854450543,
16.3067298890093));
#258094=CARTESIAN_POINT('Ctrl Pts',(-76.4769789420409,-27.1079312851641,
16.2997754253287));
#258095=CARTESIAN_POINT('Ctrl Pts',(-76.4780834779718,-27.1085192021475,
16.2927957484855));
#258096=CARTESIAN_POINT('Ctrl Pts',(-76.4787839960327,-27.1088920704749,
16.2883691023696));
#258097=CARTESIAN_POINT('Ctrl Pts',(-76.4794713875341,-27.1092822985717,
16.2839311002524));
#258098=CARTESIAN_POINT('Ctrl Pts',(-76.4801541956933,-27.1096950708922,
16.279414560734));
#258099=CARTESIAN_POINT('Ctrl Pts',(-76.4826886889078,-27.1112272269326,
16.2626497658071));
#258100=CARTESIAN_POINT('Ctrl Pts',(-76.4851267393195,-27.1130539333954,
16.2450093206269));
#258101=CARTESIAN_POINT('Ctrl Pts',(-76.4873049753993,-27.1151298324938,
16.2267576156093));
#258102=CARTESIAN_POINT('Ctrl Pts',(-76.4874570353428,-27.1152747484203,
16.2254834868503));
#258103=CARTESIAN_POINT('Ctrl Pts',(-76.4876078243834,-27.1154208730034,
16.2242063984921));
#258104=CARTESIAN_POINT('Ctrl Pts',(-76.4877572850422,-27.1155681883144,
16.2229264487818));
#258105=CARTESIAN_POINT('Ctrl Pts',(-76.4892866792013,-27.1170756296572,
16.2098290382184));
#258106=CARTESIAN_POINT('Ctrl Pts',(-76.490635746912,-27.1186810477747,
16.1965813411996));
#258107=CARTESIAN_POINT('Ctrl Pts',(-76.4917129528964,-27.1201639637659,
16.1843381520657));
#258108=CARTESIAN_POINT('Ctrl Pts',(-76.4922558078605,-27.120911275161,
16.1781682309056));
#258109=CARTESIAN_POINT('Ctrl Pts',(-76.4927295913191,-27.1216272537546,
16.1722544699356));
#258110=CARTESIAN_POINT('Ctrl Pts',(-76.4931225596015,-27.1222827001223,
16.1667491534086));
#258111=CARTESIAN_POINT('Ctrl Pts',(-76.4940369016729,-27.1238077651632,
16.153939614461));
#258112=CARTESIAN_POINT('Ctrl Pts',(-76.4945873628664,-27.1250450109583,
16.1431163916086));
#258113=CARTESIAN_POINT('Ctrl Pts',(-76.4949373712459,-27.1260738033928,
16.133614386551));
#258114=CARTESIAN_POINT('Ctrl Pts',(-76.4950321308202,-27.1263523336762,
16.1310418597004));
#258115=CARTESIAN_POINT('Ctrl Pts',(-76.4951122559592,-27.126615626805,
16.1285658709055));
#258116=CARTESIAN_POINT('Ctrl Pts',(-76.495181094013,-27.1268653381253,
16.1261726524986));
#258117=CARTESIAN_POINT('Ctrl Pts',(-76.4951938464005,-27.1269115976483,
16.1257293039885));
#258118=CARTESIAN_POINT('Ctrl Pts',(-76.4952062292888,-27.1269574102518,
16.1252887619536));
#258119=CARTESIAN_POINT('Ctrl Pts',(-76.4952182483243,-27.1270027817512,
16.124850986829));
#258120=CARTESIAN_POINT('Ctrl Pts',(74.3634602878983,-28.7459974181805,
19.6929518677509));
#258121=CARTESIAN_POINT('Ctrl Pts',(74.6189041648809,-28.8447420032201,
17.4625));
#258122=CARTESIAN_POINT('Ctrl Pts',(76.7149512087496,-29.6549915892152,
17.4625));
#258123=CARTESIAN_POINT('Ctrl Pts',(74.4609043857744,-28.4939177914721,
19.6929518673255));
#258124=CARTESIAN_POINT('Ctrl Pts',(74.6660793405452,-28.697172525973,17.537473148621));
#258125=CARTESIAN_POINT('Ctrl Pts',(76.6890525018684,-29.4834701335371,
17.4625));
#258126=CARTESIAN_POINT('Ctrl Pts',(74.558847534279,-28.2438591531057,19.6720320649355));
#258127=CARTESIAN_POINT('Ctrl Pts',(74.7189440966799,-28.539163611637,17.5981072780281));
#258128=CARTESIAN_POINT('Ctrl Pts',(76.6640386379029,-29.313679762844,17.4555267321206));
#258129=CARTESIAN_POINT('Ctrl Pts',(74.7559270342238,-27.7480012895941,
19.5871055664396));
#258130=CARTESIAN_POINT('Ctrl Pts',(74.8327386313742,-28.2117119618038,
17.6836912763764));
#258131=CARTESIAN_POINT('Ctrl Pts',(76.6159646173277,-28.9778332725218,
17.4272178998372));
#258132=CARTESIAN_POINT('Ctrl Pts',(74.8560677628267,-27.4997703917927,
19.5220948206209));
#258133=CARTESIAN_POINT('Ctrl Pts',(74.894244872939,-28.0404430900669,17.7096321218676));
#258134=CARTESIAN_POINT('Ctrl Pts',(76.5926880471512,-28.8101355628273,
17.4055476509043));
#258135=CARTESIAN_POINT('Ctrl Pts',(75.0518439197728,-27.0236898937072,
19.3489695261648));
#258136=CARTESIAN_POINT('Ctrl Pts',(75.0196609695894,-27.7022510777816,
17.7211023712238));
#258137=CARTESIAN_POINT('Ctrl Pts',(76.5500480485596,-28.4896086814942,
17.3478392195239));
#258138=CARTESIAN_POINT('Ctrl Pts',(75.1476280619454,-26.7953551633972,
19.2413577159504));
#258139=CARTESIAN_POINT('Ctrl Pts',(75.0836522525161,-27.5347169152613,
17.7080778869124));
#258140=CARTESIAN_POINT('Ctrl Pts',(76.5306138623669,-28.3364379275068,
17.3119686156358));
#258141=CARTESIAN_POINT('Ctrl Pts',(75.2884389844469,-26.4687756770145,
19.0458961827309));
#258142=CARTESIAN_POINT('Ctrl Pts',(75.180389602822,-27.2898012152202,17.6578979817799));
#258143=CARTESIAN_POINT('Ctrl Pts',(76.5048922024806,-28.1185099510298,
17.2468147718753));
#258144=CARTESIAN_POINT('Ctrl Pts',(75.3348967090537,-26.3625884843539,
18.9750294801152));
#258145=CARTESIAN_POINT('Ctrl Pts',(75.212549800534,-27.2097290601206,17.6363116935575));
#258146=CARTESIAN_POINT('Ctrl Pts',(76.4968949507143,-28.0478532106465,
17.2231925371369));
#258147=CARTESIAN_POINT('Ctrl Pts',(75.4268801209925,-26.1560856941709,
18.8208466626381));
#258148=CARTESIAN_POINT('Ctrl Pts',(75.2767579129776,-27.0529295129812,
17.5825320214162));
#258149=CARTESIAN_POINT('Ctrl Pts',(76.4822364493769,-27.9109420608553,
17.1717982652803));
#258150=CARTESIAN_POINT('Ctrl Pts',(75.472719816602,-26.0551010760521,18.7368743964301));
#258151=CARTESIAN_POINT('Ctrl Pts',(75.309058533602,-26.9755857935382,17.5501254447855));
#258152=CARTESIAN_POINT('Ctrl Pts',(76.4755364557143,-27.8442489434604,
17.1438075095172));
#258153=CARTESIAN_POINT('Ctrl Pts',(75.6060560547227,-25.7681502580839,
18.4696518487105));
#258154=CARTESIAN_POINT('Ctrl Pts',(75.4030488168813,-26.7557364160501,
17.4386060175101));
#258155=CARTESIAN_POINT('Ctrl Pts',(76.4581861338659,-27.655675609173,17.0547333270717));
#258156=CARTESIAN_POINT('Ctrl Pts',(75.6894118596666,-25.5978466210022,
18.2718409363073));
#258157=CARTESIAN_POINT('Ctrl Pts',(75.4628679834547,-26.6226482272572,
17.3449978161576));
#258158=CARTESIAN_POINT('Ctrl Pts',(76.4502012574496,-27.5450423948262,
16.9887963557577));
#258159=CARTESIAN_POINT('Ctrl Pts',(75.8449254994665,-25.304207074627,17.8327278472453));
#258160=CARTESIAN_POINT('Ctrl Pts',(75.5732964352864,-26.394507090712,17.1202191600544));
#258161=CARTESIAN_POINT('Ctrl Pts',(76.4429196593781,-27.3578956810278,
16.8424253269258));
#258162=CARTESIAN_POINT('Ctrl Pts',(75.9179115378177,-25.1799509742013,
17.5873106315597));
#258163=CARTESIAN_POINT('Ctrl Pts',(75.6248510373197,-26.2977761963307,
16.9864091667254));
#258164=CARTESIAN_POINT('Ctrl Pts',(76.4437878571375,-27.280900229956,16.7606195878714));
#258165=CARTESIAN_POINT('Ctrl Pts',(76.0120135407799,-25.0456540278874,
17.2025309630903));
#258166=CARTESIAN_POINT('Ctrl Pts',(75.6888631781811,-26.196458000542,16.7690050915913));
#258167=CARTESIAN_POINT('Ctrl Pts',(76.4531141362205,-27.2023521345503,
16.6323596984789));
#258168=CARTESIAN_POINT('Ctrl Pts',(76.0410349984129,-25.0090870943372,
17.0710669460319));
#258169=CARTESIAN_POINT('Ctrl Pts',(75.7081633852747,-26.1695156242359,
16.6936245453235));
#258170=CARTESIAN_POINT('Ctrl Pts',(76.4575269782807,-27.1820075724719,
16.5885383593535));
#258171=CARTESIAN_POINT('Ctrl Pts',(76.0942893550644,-24.9530103267666,
16.8014952531435));
#258172=CARTESIAN_POINT('Ctrl Pts',(75.7423750031981,-26.1301341325905,
16.5376305767288));
#258173=CARTESIAN_POINT('Ctrl Pts',(76.4691181075126,-27.1534935975724,
16.4986811285377));
#258174=CARTESIAN_POINT('Ctrl Pts',(76.1186539510285,-24.9335061597308,
16.6623540419143));
#258175=CARTESIAN_POINT('Ctrl Pts',(75.7573877351407,-26.1176802211109,
16.456286661695));
#258176=CARTESIAN_POINT('Ctrl Pts',(76.4763708127823,-27.1453691430048,
16.4523007247624));
#258177=CARTESIAN_POINT('Ctrl Pts',(76.1824010629023,-24.9029553648553,
16.2463425041019));
#258178=CARTESIAN_POINT('Ctrl Pts',(75.7942282194352,-26.1038934519126,
16.212254424994));
#258179=CARTESIAN_POINT('Ctrl Pts',(76.5018384532032,-27.1404954668531,
16.3136302120345));
#258180=CARTESIAN_POINT('Ctrl Pts',(76.2131904009602,-24.9185412707845,
15.9685880799916));
#258181=CARTESIAN_POINT('Ctrl Pts',(75.8084359405788,-26.1252772492229,
16.0475610164007));
#258182=CARTESIAN_POINT('Ctrl Pts',(76.5237673449999,-27.1624313528561,
16.22101111737));
#258183=CARTESIAN_POINT('Ctrl Pts',(76.2326069140444,-24.9689556265496,
15.6905058513816));
#258184=CARTESIAN_POINT('Ctrl Pts',(75.8121214408374,-26.1756393943761,
15.8859547915775));
#258185=CARTESIAN_POINT('Ctrl Pts',(76.5504448568103,-27.2087011009328,
16.1283513278769));
#258186=CARTESIAN_POINT('',(75.9418613629793,-25.2552738567447,17.263393070432));
#258187=CARTESIAN_POINT('Ctrl Pts',(76.4952182372907,-27.1270026655085,
16.1248510388549));
#258188=CARTESIAN_POINT('Ctrl Pts',(76.4949835330537,-27.1261035938169,
16.1335301302457));
#258189=CARTESIAN_POINT('Ctrl Pts',(76.4945938617307,-27.1250175086505,
16.1433840167261));
#258190=CARTESIAN_POINT('Ctrl Pts',(76.4938946426409,-27.1236651982622,
16.155016623081));
#258191=CARTESIAN_POINT('Ctrl Pts',(76.4937630714253,-27.1234107356421,
16.1572055166349));
#258192=CARTESIAN_POINT('Ctrl Pts',(76.4936205663272,-27.1231468673327,
16.159457246891));
#258193=CARTESIAN_POINT('Ctrl Pts',(76.4934661405637,-27.1228730977824,
16.161775612472));
#258194=CARTESIAN_POINT('Ctrl Pts',(76.4927426139031,-27.121590413054,16.1726377851365));
#258195=CARTESIAN_POINT('Ctrl Pts',(76.4916920130633,-27.1200357216291,
16.1853170892665));
#258196=CARTESIAN_POINT('Ctrl Pts',(76.4903847974142,-27.1184437830655,
16.1985845365573));
#258197=CARTESIAN_POINT('Ctrl Pts',(76.4898045639417,-27.1177371697065,
16.2044735549591));
#258198=CARTESIAN_POINT('Ctrl Pts',(76.4891738033074,-27.1170231040115,
16.210478937357));
#258199=CARTESIAN_POINT('Ctrl Pts',(76.4884987572096,-27.1163213320467,
16.2164967942844));
#258200=CARTESIAN_POINT('Ctrl Pts',(76.4866808484048,-27.1144314500996,
16.2327029691354));
#258201=CARTESIAN_POINT('Ctrl Pts',(76.4846005967103,-27.1126943705596,
16.248691445609));
#258202=CARTESIAN_POINT('Ctrl Pts',(76.4824017849066,-27.1111721910359,
16.2640972093359));
#258203=CARTESIAN_POINT('Ctrl Pts',(76.4816221526914,-27.1106324721787,
16.2695596275751));
#258204=CARTESIAN_POINT('Ctrl Pts',(76.4808275267735,-27.1101196624105,
16.2749492143909));
#258205=CARTESIAN_POINT('Ctrl Pts',(76.4800239584194,-27.1096361423665,
16.2802512670932));
#258206=CARTESIAN_POINT('Ctrl Pts',(76.4787631770299,-27.1088775098621,
16.2885700732516));
#258207=CARTESIAN_POINT('Ctrl Pts',(76.4774861247368,-27.1081924682413,
16.2966391164333));
#258208=CARTESIAN_POINT('Ctrl Pts',(76.4761760059707,-27.1075731179896,
16.3046343846325));
#258209=CARTESIAN_POINT('Ctrl Pts',(76.47501440999,-27.107023980933,16.3117232621031));
#258210=CARTESIAN_POINT('Ctrl Pts',(76.473826311574,-27.1065264227142,16.3187548885341));
#258211=CARTESIAN_POINT('Ctrl Pts',(76.4726008566123,-27.1060881023903,
16.3258128070512));
#258212=CARTESIAN_POINT('Ctrl Pts',(76.4724441687559,-27.1060320583298,
16.326715239338));
#258213=CARTESIAN_POINT('Ctrl Pts',(76.4722868770268,-27.1059770032847,
16.327618034215));
#258214=CARTESIAN_POINT('Ctrl Pts',(76.4721289660945,-27.1059229723704,
16.328521302748));
#258215=CARTESIAN_POINT('Ctrl Pts',(76.4709315855592,-27.1055132758145,
16.3353704558992));
#258216=CARTESIAN_POINT('Ctrl Pts',(76.4696860988113,-27.1051480063909,
16.3423105850608));
#258217=CARTESIAN_POINT('Ctrl Pts',(76.4683756379742,-27.1048249982617,
16.3494047007118));
#258218=CARTESIAN_POINT('Ctrl Pts',(76.4671537647836,-27.1045238256037,
16.3560192514715));
#258219=CARTESIAN_POINT('Ctrl Pts',(76.4658752319113,-27.1042596511161,
16.3627681883072));
#258220=CARTESIAN_POINT('Ctrl Pts',(76.4645307210554,-27.104032682556,16.3696623272918));
#258221=CARTESIAN_POINT('Ctrl Pts',(76.463273931649,-27.1038205223635,16.3761066641332));
#258222=CARTESIAN_POINT('Ctrl Pts',(76.4619593190201,-27.1036411260697,
16.3826784026398));
#258223=CARTESIAN_POINT('Ctrl Pts',(76.4605856089619,-27.103492920932,16.3893426843809));
#258224=CARTESIAN_POINT('Ctrl Pts',(76.4593337345628,-27.1033578602498,
16.3954159045997));
#258225=CARTESIAN_POINT('Ctrl Pts',(76.4580326598547,-27.1032489151476,
16.401566235519));
#258226=CARTESIAN_POINT('Ctrl Pts',(76.4566888072176,-27.103160260748,16.4077247899517));
#258227=CARTESIAN_POINT('Ctrl Pts',(76.4561164336035,-27.1031225010727,
16.410347840992));
#258228=CARTESIAN_POINT('Ctrl Pts',(76.45553640674,-27.1030883438968,16.4129718045799));
#258229=CARTESIAN_POINT('Ctrl Pts',(76.4549497809999,-27.1030568879025,
16.415588473538));
#258230=CARTESIAN_POINT('Ctrl Pts',(76.4528297571347,-27.1029432081676,
16.425044929774));
#258231=CARTESIAN_POINT('Ctrl Pts',(76.4506276154633,-27.1028516325175,
16.434405561816));
#258232=CARTESIAN_POINT('Ctrl Pts',(76.4483618531647,-27.1027493830608,
16.4434727014798));
#258233=CARTESIAN_POINT('Ctrl Pts',(76.4479348994007,-27.1027301154657,
16.4451812873319));
#258234=CARTESIAN_POINT('Ctrl Pts',(76.4475057389463,-27.1027103529406,
16.4468793703157));
#258235=CARTESIAN_POINT('Ctrl Pts',(76.4470745680893,-27.1026896905077,
16.4485655884626));
#258236=CARTESIAN_POINT('Ctrl Pts',(76.4456191147856,-27.1026199427365,
16.454257558903));
#258237=CARTESIAN_POINT('Ctrl Pts',(76.4441322040646,-27.1025406532758,
16.4598473134519));
#258238=CARTESIAN_POINT('Ctrl Pts',(76.442600468481,-27.1024250918531,16.4653566990946));
#258239=CARTESIAN_POINT('Ctrl Pts',(76.4420185090595,-27.1023811860645,
16.4674499055955));
#258240=CARTESIAN_POINT('Ctrl Pts',(76.4414302186258,-27.1023318496955,
16.4695309610732));
#258241=CARTESIAN_POINT('Ctrl Pts',(76.4408353908733,-27.102274692544,16.471599536434));
#258242=CARTESIAN_POINT('Ctrl Pts',(76.4389925228598,-27.1020976108831,
16.4780083015764));
#258243=CARTESIAN_POINT('Ctrl Pts',(76.4370710585152,-27.1018561048159,
16.484391780126));
#258244=CARTESIAN_POINT('Ctrl Pts',(76.4350620986664,-27.1015158539167,
16.4906542061397));
#258245=CARTESIAN_POINT('Ctrl Pts',(76.4333518787977,-27.101226199622,16.4959853855563));
#258246=CARTESIAN_POINT('Ctrl Pts',(76.4315790441179,-27.1008647151594,
16.5012232667724));
#258247=CARTESIAN_POINT('Ctrl Pts',(76.4297403585978,-27.1004038747182,
16.506308780418));
#258248=CARTESIAN_POINT('Ctrl Pts',(76.428448929915,-27.1000801964396,16.5098806681154));
#258249=CARTESIAN_POINT('Ctrl Pts',(76.4271251515698,-27.0997073598893,
16.5133767163619));
#258250=CARTESIAN_POINT('Ctrl Pts',(76.4257650872491,-27.099274630663,16.5168023194369));
#258251=CARTESIAN_POINT('Ctrl Pts',(76.4244998564415,-27.0988720744456,
16.5199890647099));
#258252=CARTESIAN_POINT('Ctrl Pts',(76.4232033943605,-27.098417636482,16.5231136244567));
#258253=CARTESIAN_POINT('Ctrl Pts',(76.4218676568024,-27.0979025055511,
16.5262197342897));
#258254=CARTESIAN_POINT('Ctrl Pts',(76.4217789540814,-27.0978682970983,
16.5264260026484));
#258255=CARTESIAN_POINT('Ctrl Pts',(76.4216900756716,-27.0978338210965,
16.5266322092027));
#258256=CARTESIAN_POINT('Ctrl Pts',(76.42160101808,-27.0977990750257,16.5268383756656));
#258257=CARTESIAN_POINT('Ctrl Pts',(76.4212719492627,-27.0976706878978,
16.5276001630985));
#258258=CARTESIAN_POINT('Ctrl Pts',(76.4209404362583,-27.0975386143442,
16.5283613866205));
#258259=CARTESIAN_POINT('Ctrl Pts',(76.420606322143,-27.0974027448563,16.5291232095979));
#258260=CARTESIAN_POINT('Ctrl Pts',(76.4187176830274,-27.0966347185512,
16.5334295486848));
#258261=CARTESIAN_POINT('Ctrl Pts',(76.4167566024575,-27.0957491893814,
16.5376614539863));
#258262=CARTESIAN_POINT('Ctrl Pts',(76.4147290835934,-27.0947257635434,
16.5417599887868));
#258263=CARTESIAN_POINT('Ctrl Pts',(76.4130382200801,-27.0938722704199,
16.5451779905008));
#258264=CARTESIAN_POINT('Ctrl Pts',(76.4113012291952,-27.0929228022964,
16.5485028097877));
#258265=CARTESIAN_POINT('Ctrl Pts',(76.4095163162519,-27.0918686181557,
16.5517348365811));
#258266=CARTESIAN_POINT('Ctrl Pts',(76.4080553283209,-27.0910057467689,
16.5543803169423));
#258267=CARTESIAN_POINT('Ctrl Pts',(76.4065622115749,-27.0900727246033,
16.5569638004413));
#258268=CARTESIAN_POINT('Ctrl Pts',(76.4050319318852,-27.0890672853614,
16.5595114022443));
#258269=CARTESIAN_POINT('Ctrl Pts',(76.4024133502064,-27.0873467993641,
16.5638708036345));
#258270=CARTESIAN_POINT('Ctrl Pts',(76.3996858222803,-27.0854160305327,
16.5681213015851));
#258271=CARTESIAN_POINT('Ctrl Pts',(76.3968549739062,-27.0832453437817,
16.5722001453448));
#258272=CARTESIAN_POINT('Ctrl Pts',(76.3944794420004,-27.0814237924469,
16.5756229438169));
#258273=CARTESIAN_POINT('Ctrl Pts',(76.3920312477951,-27.0794332007598,
16.5789244111556));
#258274=CARTESIAN_POINT('Ctrl Pts',(76.3895078513776,-27.0772609129525,
16.5821034643369));
#258275=CARTESIAN_POINT('Ctrl Pts',(76.3879086122783,-27.0758841940301,
16.5841182354253));
#258276=CARTESIAN_POINT('Ctrl Pts',(76.3862790519598,-27.0744345916958,
16.5860845447371));
#258277=CARTESIAN_POINT('Ctrl Pts',(76.3846166914258,-27.0729104400659,
16.5880130337735));
#258278=CARTESIAN_POINT('Ctrl Pts',(76.3827359747383,-27.0711860864457,
16.5901948357585));
#258279=CARTESIAN_POINT('Ctrl Pts',(76.3808666413316,-27.0694154757855,
16.5922669270651));
#258280=CARTESIAN_POINT('Ctrl Pts',(76.3790011613002,-27.067605522352,16.5942742310325));
#258281=CARTESIAN_POINT('Ctrl Pts',(76.3740456584696,-27.0627975216168,
16.5996064781347));
#258282=CARTESIAN_POINT('Ctrl Pts',(76.3691274276512,-27.0577058759386,
16.6044118919374));
#258283=CARTESIAN_POINT('Ctrl Pts',(76.3642377230657,-27.0523503506956,
16.608778305053));
#258284=CARTESIAN_POINT('Ctrl Pts',(76.3592796180166,-27.0469199087776,
16.6132057984803));
#258285=CARTESIAN_POINT('Ctrl Pts',(76.3543509085649,-27.0412180804687,
16.6171815871766));
#258286=CARTESIAN_POINT('Ctrl Pts',(76.3494322419877,-27.0352768340194,
16.6208506593465));
#258287=CARTESIAN_POINT('Ctrl Pts',(76.3445135754106,-27.0293355875702,
16.6245197315165));
#258288=CARTESIAN_POINT('Ctrl Pts',(76.3396049868128,-27.0231548844634,
16.627881911179));
#258289=CARTESIAN_POINT('Ctrl Pts',(76.3346762337748,-27.0167787754288,
16.6311389170626));
#258290=CARTESIAN_POINT('Ctrl Pts',(76.3270525622607,-27.0069163699799,
16.6361767720303));
#258291=CARTESIAN_POINT('Ctrl Pts',(76.3193994275977,-26.9965742763171,
16.6408622418929));
#258292=CARTESIAN_POINT('Ctrl Pts',(76.3117344496181,-26.9857761531729,
16.6452464533356));
#258293=CARTESIAN_POINT('Ctrl Pts',(76.3074367607922,-26.9797217361478,
16.6477046438977));
#258294=CARTESIAN_POINT('Ctrl Pts',(76.3031351576487,-26.9735241809036,
16.6500689942518));
#258295=CARTESIAN_POINT('Ctrl Pts',(76.2988312337083,-26.9671894394041,
16.6523553297696));
#258296=CARTESIAN_POINT('Ctrl Pts',(76.284801695007,-26.946540026854,16.6598081177547));
#258297=CARTESIAN_POINT('Ctrl Pts',(76.2713420389531,-26.9253146403795,
16.6661261478332));
#258298=CARTESIAN_POINT('Ctrl Pts',(76.2582666976207,-26.9037854166578,
16.6722817468538));
#258299=CARTESIAN_POINT('Ctrl Pts',(76.2367166491782,-26.8683021506889,
16.6824270618949));
#258300=CARTESIAN_POINT('Ctrl Pts',(76.2163231724411,-26.8318654947762,
16.6915805494775));
#258301=CARTESIAN_POINT('Ctrl Pts',(76.1969868424008,-26.7948177267048,
16.7005093018145));
#258302=CARTESIAN_POINT('Ctrl Pts',(76.1951008482355,-26.7912042243353,
16.7013801793169));
#258303=CARTESIAN_POINT('Ctrl Pts',(76.1932248857209,-26.7875849267645,
16.702248942733));
#258304=CARTESIAN_POINT('Ctrl Pts',(76.1913588468486,-26.7839601625947,
16.7031163158082));
#258305=CARTESIAN_POINT('Ctrl Pts',(76.1765680275187,-26.7552291255587,
16.7099913914764));
#258306=CARTESIAN_POINT('Ctrl Pts',(76.1624139946396,-26.7262008738675,
16.7168106960657));
#258307=CARTESIAN_POINT('Ctrl Pts',(76.148916516475,-26.6969732854462,16.723597339564));
#258308=CARTESIAN_POINT('Ctrl Pts',(76.1236619610203,-26.6422867918957,
16.7362955386267));
#258309=CARTESIAN_POINT('Ctrl Pts',(76.1005180681542,-26.5866819737582,
16.7491519989745));
#258310=CARTESIAN_POINT('Ctrl Pts',(76.079407408338,-26.5302810835918,16.7625435721094));
#258311=CARTESIAN_POINT('Ctrl Pts',(76.0643629274286,-26.4900870715251,
16.7720870571605));
#258312=CARTESIAN_POINT('Ctrl Pts',(76.0503521064178,-26.4494883804854,
16.7819023270183));
#258313=CARTESIAN_POINT('Ctrl Pts',(76.0373611942065,-26.4085292238124,
16.7921336012873));
#258314=CARTESIAN_POINT('Ctrl Pts',(76.0231720122117,-26.363792032233,16.8033085988763));
#258315=CARTESIAN_POINT('Ctrl Pts',(76.0103384192577,-26.3190310002098,
16.8148454077162));
#258316=CARTESIAN_POINT('Ctrl Pts',(75.9987850456331,-26.2743222514904,
16.8269262467483));
#258317=CARTESIAN_POINT('Ctrl Pts',(75.9837486849486,-26.2161351891359,
16.8426490874492));
#258318=CARTESIAN_POINT('Ctrl Pts',(75.9708594776084,-26.1575989600339,
16.8592311067897));
#258319=CARTESIAN_POINT('Ctrl Pts',(75.9600230530993,-26.0990044706059,
16.87689659528));
#258320=CARTESIAN_POINT('Ctrl Pts',(75.9491979291291,-26.0404710852166,
16.8945436616849));
#258321=CARTESIAN_POINT('Ctrl Pts',(75.9404214117338,-25.9818779785533,
16.9132712882588));
#258322=CARTESIAN_POINT('Ctrl Pts',(75.9336439589103,-25.9235033740798,
16.9333228296216));
#258323=CARTESIAN_POINT('Ctrl Pts',(75.9294790509236,-25.8876307737501,
16.9456449847059));
#258324=CARTESIAN_POINT('Ctrl Pts',(75.9260699331789,-25.8518405543699,
16.9584675280385));
#258325=CARTESIAN_POINT('Ctrl Pts',(75.9234132458697,-25.8161989866991,
16.9718522765842));
#258326=CARTESIAN_POINT('Ctrl Pts',(75.9217239577786,-25.79353584693,16.9803631375505));
#258327=CARTESIAN_POINT('Ctrl Pts',(75.9203357066725,-25.7708904059774,
16.9891192993483));
#258328=CARTESIAN_POINT('Ctrl Pts',(75.9192531417283,-25.7483106633381,
16.9981274246421));
#258329=CARTESIAN_POINT('Ctrl Pts',(75.9170297815808,-25.7019366326703,
17.0166282147223));
#258330=CARTESIAN_POINT('Ctrl Pts',(75.9160908878973,-25.655715430254,17.0360687209725));
#258331=CARTESIAN_POINT('Ctrl Pts',(75.9163356254781,-25.6100335195254,
17.0568346695685));
#258332=CARTESIAN_POINT('Ctrl Pts',(75.9165621173305,-25.5677572963717,
17.0760524707252));
#258333=CARTESIAN_POINT('Ctrl Pts',(75.9178014945793,-25.525943597602,17.0964068031593));
#258334=CARTESIAN_POINT('Ctrl Pts',(75.9199460216627,-25.4848871400518,
17.1181763515707));
#258335=CARTESIAN_POINT('Ctrl Pts',(75.9220376690096,-25.4448430523975,
17.1394091065817));
#258336=CARTESIAN_POINT('Ctrl Pts',(75.9249898990674,-25.4055198684575,
17.1619892999607));
#258337=CARTESIAN_POINT('Ctrl Pts',(75.9286842189365,-25.367171005978,17.1861307296523));
#258338=CARTESIAN_POINT('Ctrl Pts',(75.9320094343453,-25.3326536298594,
17.2078601566765));
#258339=CARTESIAN_POINT('Ctrl Pts',(75.9359354287058,-25.2989256357191,
17.2308544606354));
#258340=CARTESIAN_POINT('Ctrl Pts',(75.9403670676557,-25.2661521617921,
17.2552262519058));
#258341=CARTESIAN_POINT('Ctrl Pts',(75.9408589869758,-25.2625142514853,
17.2579315614148));
#258342=CARTESIAN_POINT('Ctrl Pts',(75.9413571303365,-25.2588880801971,
17.2606537953022));
#258343=CARTESIAN_POINT('Ctrl Pts',(75.9418613633423,-25.2552738568382,
17.2633930704885));
#258344=CARTESIAN_POINT('Ctrl Pts',(75.9418613633423,-25.2552738568381,
17.2633930704885));
#258345=CARTESIAN_POINT('Ctrl Pts',(75.9442259477234,-25.2383250955474,
17.2762387760005));
#258346=CARTESIAN_POINT('Ctrl Pts',(75.9466297979483,-25.2219501076077,
17.2896217176776));
#258347=CARTESIAN_POINT('Ctrl Pts',(75.9489416166696,-25.2063620808647,
17.3037656232882));
#258348=CARTESIAN_POINT('Ctrl Pts',(75.9512774695743,-25.1906119975164,
17.3180565720987));
#258349=CARTESIAN_POINT('Ctrl Pts',(75.9535194008795,-25.1756652588171,
17.3331243157543));
#258350=CARTESIAN_POINT('Ctrl Pts',(75.9555501186517,-25.1617083521244,
17.3491621101886));
#258351=CARTESIAN_POINT('Ctrl Pts',(75.9576114326053,-25.1475411611397,
17.3654415409911));
#258352=CARTESIAN_POINT('Ctrl Pts',(75.9594551436902,-25.1343938079096,
17.3827204208166));
#258353=CARTESIAN_POINT('Ctrl Pts',(75.9609767648281,-25.1224278840972,
17.4011633324196));
#258354=CARTESIAN_POINT('Ctrl Pts',(75.9611515136477,-25.1210536714171,
17.403281387271));
#258355=CARTESIAN_POINT('Ctrl Pts',(75.9613220335941,-25.1196950054424,
17.405414755068));
#258356=CARTESIAN_POINT('Ctrl Pts',(75.9614881812303,-25.1183521036895,
17.4075636545405));
#258357=CARTESIAN_POINT('Origin',(76.7149512087496,-29.6549915892152,20.0025));
#258358=CARTESIAN_POINT('Origin',(0.,0.,20.0025));
#258359=CARTESIAN_POINT('Origin',(29.6549915892152,-76.7149512087496,20.0025));
#258360=CARTESIAN_POINT('Ctrl Pts',(24.9689313575499,-76.2325975651779,
15.6906397325506));
#258361=CARTESIAN_POINT('Ctrl Pts',(26.1756150602387,-75.8121196590786,
15.8860328844658));
#258362=CARTESIAN_POINT('Ctrl Pts',(27.2086788182716,-76.5504320086843,
16.1283959549332));
#258363=CARTESIAN_POINT('Ctrl Pts',(24.9186909562146,-76.2132400197753,
15.967824496348));
#258364=CARTESIAN_POINT('Ctrl Pts',(26.1254229642367,-75.8084425279589,
16.0471243598434));
#258365=CARTESIAN_POINT('Ctrl Pts',(27.1625656651728,-76.5238417787825,
16.2207578908838));
#258366=CARTESIAN_POINT('Ctrl Pts',(24.9032159272874,-76.1826381079971,
16.2438456162079));
#258367=CARTESIAN_POINT('Ctrl Pts',(26.1041848761176,-75.7943214248689,
16.2107725763322));
#258368=CARTESIAN_POINT('Ctrl Pts',(27.1407766635653,-76.5020517602977,
16.3127979160872));
#258369=CARTESIAN_POINT('Ctrl Pts',(24.9328226963038,-76.1197004175054,
16.655986759916));
#258370=CARTESIAN_POINT('Ctrl Pts',(26.1172873190749,-75.7580138780931,
16.4525591935381));
#258371=CARTESIAN_POINT('Ctrl Pts',(27.1451435881169,-76.4767312134558,
16.4501782974209));
#258372=CARTESIAN_POINT('Ctrl Pts',(24.9518097701927,-76.0956371509853,
16.7941104173067));
#258373=CARTESIAN_POINT('Ctrl Pts',(26.1293351405296,-75.7432179427276,
16.53332924405));
#258374=CARTESIAN_POINT('Ctrl Pts',(27.1529468723189,-76.469480763603,16.4962195166118));
#258375=CARTESIAN_POINT('Ctrl Pts',(25.0073336657117,-76.0425032131366,
17.0641682497328));
#258376=CARTESIAN_POINT('Ctrl Pts',(26.1682415554301,-75.7091288541243,
16.6896570718779));
#258377=CARTESIAN_POINT('Ctrl Pts',(27.1810555370846,-76.4577808154581,
16.5862387939007));
#258378=CARTESIAN_POINT('Ctrl Pts',(25.0435822919594,-76.0135981896352,
17.1955505586789));
#258379=CARTESIAN_POINT('Ctrl Pts',(26.1949210472009,-75.6899232799157,
16.7650201820139));
#258380=CARTESIAN_POINT('Ctrl Pts',(27.2011812093655,-76.4533313045578,
16.6300328970335));
#258381=CARTESIAN_POINT('Ctrl Pts',(25.1764553135872,-75.9201060960319,
17.5792969885097));
#258382=CARTESIAN_POINT('Ctrl Pts',(26.2950899509062,-75.6263767700398,
16.9819673365851));
#258383=CARTESIAN_POINT('Ctrl Pts',(27.2787774842961,-76.4438901441629,
16.7579483734713));
#258384=CARTESIAN_POINT('Ctrl Pts',(25.2993526607364,-75.8476684832869,
17.8240388353678));
#258385=CARTESIAN_POINT('Ctrl Pts',(26.3907356809326,-75.5752351470898,
17.1155820316982));
#258386=CARTESIAN_POINT('Ctrl Pts',(27.3548544480355,-76.4428939284366,
16.8395289896475));
#258387=CARTESIAN_POINT('Ctrl Pts',(25.5919984567923,-75.6923432030072,
18.2644739211054));
#258388=CARTESIAN_POINT('Ctrl Pts',(26.6180940171703,-75.4649619696469,
17.3414092350345));
#258389=CARTESIAN_POINT('Ctrl Pts',(27.5412643883021,-76.4499649794119,
16.9863406840096));
#258390=CARTESIAN_POINT('Ctrl Pts',(25.7617839502726,-75.6091210995781,
18.4627331486824));
#258391=CARTESIAN_POINT('Ctrl Pts',(26.750791129475,-75.4052371346464,17.4354381030784));
#258392=CARTESIAN_POINT('Ctrl Pts',(27.6515244073534,-76.4578597275994,
17.052427093745));
#258393=CARTESIAN_POINT('Ctrl Pts',(26.1430805994656,-75.43173575527,18.819759549872));
#258394=CARTESIAN_POINT('Ctrl Pts',(27.0442130694157,-75.2796463045429,
17.585582997513));
#258395=CARTESIAN_POINT('Ctrl Pts',(27.9020344677393,-76.4807996718613,
17.1714358939392));
#258396=CARTESIAN_POINT('Ctrl Pts',(26.351056088416,-75.3392616135106,18.9747290102619));
#258397=CARTESIAN_POINT('Ctrl Pts',(27.2031302208849,-75.2146749685589,
17.6396375078353));
#258398=CARTESIAN_POINT('Ctrl Pts',(28.0399748698375,-76.4956562029936,
17.2230923811496));
#258399=CARTESIAN_POINT('Ctrl Pts',(26.7887981118758,-75.1503919246078,
19.2381193325703));
#258400=CARTESIAN_POINT('Ctrl Pts',(27.5299162784616,-75.08549731885,17.7075896666719));
#258401=CARTESIAN_POINT('Ctrl Pts',(28.3320433237811,-76.5300629685854,
17.3108891546272));
#258402=CARTESIAN_POINT('Ctrl Pts',(27.0218910128879,-75.0525919498094,
19.3482083029786));
#258403=CARTESIAN_POINT('Ctrl Pts',(27.7009559314819,-75.0201494871695,
17.7210643477395));
#258404=CARTESIAN_POINT('Ctrl Pts',(28.4884000162545,-76.5498913973941,
17.3475854788259));
#258405=CARTESIAN_POINT('Ctrl Pts',(27.4985053196508,-74.8565797596346,
19.5217411601882));
#258406=CARTESIAN_POINT('Ctrl Pts',(28.0395707962217,-74.8945599897605,
17.709745105584));
#258407=CARTESIAN_POINT('Ctrl Pts',(28.8092814008563,-76.5925703049476,
17.4054297637291));
#258408=CARTESIAN_POINT('Ctrl Pts',(27.7422284005853,-74.7582415292723,
19.5858151824391));
#258409=CARTESIAN_POINT('Ctrl Pts',(28.2078168588111,-74.8341192521319,
17.6844550416302));
#258410=CARTESIAN_POINT('Ctrl Pts',(28.9739291008626,-76.6154156280005,
17.4267877716095));
#258411=CARTESIAN_POINT('Ctrl Pts',(28.2396160007804,-74.5605143304923,
19.6716009699542));
#258412=CARTESIAN_POINT('Ctrl Pts',(28.5364711009172,-74.7198525855438,
17.5990670510762));
#258413=CARTESIAN_POINT('Ctrl Pts',(29.3108001463009,-76.663616773129,17.455383034021));
#258414=CARTESIAN_POINT('Ctrl Pts',(28.4947415154358,-74.460585966212,19.6929518687096));
#258415=CARTESIAN_POINT('Ctrl Pts',(28.6976612611857,-74.6659231009672,
17.5372248464455));
#258416=CARTESIAN_POINT('Ctrl Pts',(29.4840227026762,-76.68913593644,17.4625));
#258417=CARTESIAN_POINT('Ctrl Pts',(28.7459974181806,-74.3634602878982,
19.6929518677509));
#258418=CARTESIAN_POINT('Ctrl Pts',(28.8447420032201,-74.6189041648808,
17.4625));
#258419=CARTESIAN_POINT('Ctrl Pts',(29.6549915892153,-76.7149512087496,
17.4625));
#258420=CARTESIAN_POINT('',(25.255273856838,-75.9418613633423,17.2633930704885));
#258421=CARTESIAN_POINT('Ctrl Pts',(25.1183523255102,-75.961488153786,17.4075632995852));
#258422=CARTESIAN_POINT('Ctrl Pts',(25.1300086289488,-75.9600460003542,
17.3889110251782));
#258423=CARTESIAN_POINT('Ctrl Pts',(25.1428552491918,-75.9582730048931,
17.3714318667196));
#258424=CARTESIAN_POINT('Ctrl Pts',(25.1567358846387,-75.9562706193538,
17.3549670181865));
#258425=CARTESIAN_POINT('Ctrl Pts',(25.1704654612226,-75.9542900251859,
17.3386813517454));
#258426=CARTESIAN_POINT('Ctrl Pts',(25.1852067358384,-75.9520849723162,
17.3233881139774));
#258427=CARTESIAN_POINT('Ctrl Pts',(25.2007766451559,-75.9497709328093,
17.3088979329943));
#258428=CARTESIAN_POINT('Ctrl Pts',(25.2161260489864,-75.9474896653885,
17.2946129660782));
#258429=CARTESIAN_POINT('Ctrl Pts',(25.232280824703,-75.9451024553672,17.2811085188303));
#258430=CARTESIAN_POINT('Ctrl Pts',(25.2490337249568,-75.9427372332249,
17.2681673906668));
#258431=CARTESIAN_POINT('Ctrl Pts',(25.2511048107543,-75.942444831437,17.2665675371288));
#258432=CARTESIAN_POINT('Ctrl Pts',(25.2531849968851,-75.9421527879211,
17.2649762469424));
#258433=CARTESIAN_POINT('Ctrl Pts',(25.2552738568381,-75.9418613633423,
17.2633930704885));
#258434=CARTESIAN_POINT('Ctrl Pts',(25.2552738568381,-75.9418613633423,
17.2633930704885));
#258435=CARTESIAN_POINT('Ctrl Pts',(25.3053371640301,-75.9348768553703,
17.2254493239301));
#258436=CARTESIAN_POINT('Ctrl Pts',(25.3572644310084,-75.9291204561474,
17.1911044093464));
#258437=CARTESIAN_POINT('Ctrl Pts',(25.4106833642209,-75.924849515688,17.1596330726746));
#258438=CARTESIAN_POINT('Ctrl Pts',(25.4672813124795,-75.920324407218,17.126288844749));
#258439=CARTESIAN_POINT('Ctrl Pts',(25.5255536825938,-75.9174669834122,
17.0961703062381));
#258440=CARTESIAN_POINT('Ctrl Pts',(25.5850314006763,-75.9165875721685,
17.0683598410554));
#258441=CARTESIAN_POINT('Ctrl Pts',(25.6385673672631,-75.9157960130354,
17.0433276074261));
#258442=CARTESIAN_POINT('Ctrl Pts',(25.6930793583591,-75.9166071705315,
17.0201642484432));
#258443=CARTESIAN_POINT('Ctrl Pts',(25.7482100069341,-75.9192482119053,
16.9981680565501));
#258444=CARTESIAN_POINT('Ctrl Pts',(25.7703411807749,-75.9203084088606,
16.989338094284));
#258445=CARTESIAN_POINT('Ctrl Pts',(25.7926041373149,-75.9216656968715,
16.9807230184841));
#258446=CARTESIAN_POINT('Ctrl Pts',(25.8149722051989,-75.9233227318013,
16.9723142805638));
#258447=CARTESIAN_POINT('Ctrl Pts',(25.8770418865906,-75.9279208772774,
16.9489806745353));
#258448=CARTESIAN_POINT('Ctrl Pts',(25.9395105598039,-75.9347968299589,
16.9273736682915));
#258449=CARTESIAN_POINT('Ctrl Pts',(26.0019469535689,-75.9439477443041,
16.9071901217942));
#258450=CARTESIAN_POINT('Ctrl Pts',(26.0680891143166,-75.9536417898937,
16.8858086278227));
#258451=CARTESIAN_POINT('Ctrl Pts',(26.1341966258341,-75.965888408869,16.8660249929721));
#258452=CARTESIAN_POINT('Ctrl Pts',(26.1997753181043,-75.9807279241647,
16.8475110455431));
#258453=CARTESIAN_POINT('Ctrl Pts',(26.2246632540871,-75.9863597062865,
16.8404847703544));
#258454=CARTESIAN_POINT('Ctrl Pts',(26.2494750769638,-75.9923654084165,
16.8336416500865));
#258455=CARTESIAN_POINT('Ctrl Pts',(26.274183642075,-75.9987489548308,16.8269646518251));
#258456=CARTESIAN_POINT('Ctrl Pts',(26.3193781191767,-76.0104251100811,
16.8147517433184));
#258457=CARTESIAN_POINT('Ctrl Pts',(26.3644806578422,-76.0233691013076,
16.8031325557463));
#258458=CARTESIAN_POINT('Ctrl Pts',(26.4094030264447,-76.0376323915297,
16.7919150704374));
#258459=CARTESIAN_POINT('Ctrl Pts',(26.4723212970277,-76.0576095561699,
16.7762038602346));
#258460=CARTESIAN_POINT('Ctrl Pts',(26.5349890928756,-76.0801913924513,
16.761328555408));
#258461=CARTESIAN_POINT('Ctrl Pts',(26.5968842692081,-76.1054321159433,
16.7468658576066));
#258462=CARTESIAN_POINT('Ctrl Pts',(26.6310436335351,-76.1193622332921,
16.7388840310311));
#258463=CARTESIAN_POINT('Ctrl Pts',(26.6649677057044,-76.1341013590046,
16.7310274121222));
#258464=CARTESIAN_POINT('Ctrl Pts',(26.6985700833486,-76.1496523368463,
16.7232226781382));
#258465=CARTESIAN_POINT('Ctrl Pts',(26.7271705556572,-76.1628884630466,
16.7165797232691));
#258466=CARTESIAN_POINT('Ctrl Pts',(26.7555332801645,-76.1767336953889,
16.7099108264627));
#258467=CARTESIAN_POINT('Ctrl Pts',(26.7835861607673,-76.1911702999443,
16.703195010784));
#258468=CARTESIAN_POINT('Ctrl Pts',(26.8199494181624,-76.2098835998295,
16.6944897039172));
#258469=CARTESIAN_POINT('Ctrl Pts',(26.8556888251213,-76.2295605861727,
16.6856585992062));
#258470=CARTESIAN_POINT('Ctrl Pts',(26.8905185780769,-76.2502978094459,
16.6759949656516));
#258471=CARTESIAN_POINT('Ctrl Pts',(26.8948405205601,-76.2528710429215,
16.6747958279932));
#258472=CARTESIAN_POINT('Ctrl Pts',(26.8991484846555,-76.2554605686,16.6735839225594));
#258473=CARTESIAN_POINT('Ctrl Pts',(26.9034419493924,-76.258066542324,16.6723579472489));
#258474=CARTESIAN_POINT('Ctrl Pts',(26.9260412895686,-76.2717835029343,
16.6659048295947));
#258475=CARTESIAN_POINT('Ctrl Pts',(26.9482892130479,-76.285912248423,16.6592804200091));
#258476=CARTESIAN_POINT('Ctrl Pts',(26.9698831287183,-76.3006663576261,
16.6513762614162));
#258477=CARTESIAN_POINT('Ctrl Pts',(26.9780091205859,-76.3062184665269,
16.6484018528176));
#258478=CARTESIAN_POINT('Ctrl Pts',(26.986126275181,-76.3119191069485,16.6452107770005));
#258479=CARTESIAN_POINT('Ctrl Pts',(26.9940602890789,-76.3176690330733,
16.641805515319));
#258480=CARTESIAN_POINT('Ctrl Pts',(27.0017405515385,-76.3232350608532,
16.6385091632085));
#258481=CARTESIAN_POINT('Ctrl Pts',(27.0092489791902,-76.3288474190919,
16.6350110759018));
#258482=CARTESIAN_POINT('Ctrl Pts',(27.0164426885853,-76.3343994470152,
16.6313545905897));
#258483=CARTESIAN_POINT('Ctrl Pts',(27.0216511779323,-76.3384193033514,
16.6287071713309));
#258484=CARTESIAN_POINT('Ctrl Pts',(27.0266992747262,-76.3424031634616,
16.6260035903663));
#258485=CARTESIAN_POINT('Ctrl Pts',(27.031517148069,-76.3463237496473,16.623174016085));
#258486=CARTESIAN_POINT('Ctrl Pts',(27.0359626255992,-76.3499412955132,
16.620563152745));
#258487=CARTESIAN_POINT('Ctrl Pts',(27.0402121123801,-76.3535049417161,
16.61784496832));
#258488=CARTESIAN_POINT('Ctrl Pts',(27.0442217726251,-76.3569830260576,
16.6150107799504));
#258489=CARTESIAN_POINT('Ctrl Pts',(27.0482190858534,-76.3604504002732,
16.6121853189465));
#258490=CARTESIAN_POINT('Ctrl Pts',(27.0519780402871,-76.363832737455,16.6092444573834));
#258491=CARTESIAN_POINT('Ctrl Pts',(27.0554667048094,-76.36708813328,16.6062292699511));
#258492=CARTESIAN_POINT('Ctrl Pts',(27.0590905992174,-76.3704697168776,
16.6030972058604));
#258493=CARTESIAN_POINT('Ctrl Pts',(27.062422884322,-76.373714282348,16.5998850438583));
#258494=CARTESIAN_POINT('Ctrl Pts',(27.0654401118128,-76.3767636736847,
16.5966933385278));
#258495=CARTESIAN_POINT('Ctrl Pts',(27.0660776794783,-76.3774080378641,
16.5960189021046));
#258496=CARTESIAN_POINT('Ctrl Pts',(27.0667012194144,-76.3780436511264,
16.5953455586113));
#258497=CARTESIAN_POINT('Ctrl Pts',(27.0673105711314,-76.3786699101857,
16.5946745303528));
#258498=CARTESIAN_POINT('Ctrl Pts',(27.0690899047773,-76.3804986140098,
16.5927150985099));
#258499=CARTESIAN_POINT('Ctrl Pts',(27.0707485694433,-76.3822466735942,
16.5907819641661));
#258500=CARTESIAN_POINT('Ctrl Pts',(27.0722790207895,-76.3839036747509,
16.5888786971137));
#258501=CARTESIAN_POINT('Ctrl Pts',(27.0747602935228,-76.3865901187202,
16.585792989977));
#258502=CARTESIAN_POINT('Ctrl Pts',(27.077074716928,-76.3892195788573,16.5825794796621));
#258503=CARTESIAN_POINT('Ctrl Pts',(27.0792241298737,-76.391803503673,16.579183461688));
#258504=CARTESIAN_POINT('Ctrl Pts',(27.0816343564139,-76.3947009665273,
16.5753753648454));
#258505=CARTESIAN_POINT('Ctrl Pts',(27.0838371838135,-76.3975410819206,
16.5713382503816));
#258506=CARTESIAN_POINT('Ctrl Pts',(27.0858449593888,-76.4003286348304,
16.5670618115476));
#258507=CARTESIAN_POINT('Ctrl Pts',(27.0868914071294,-76.4017815006189,
16.5648329420413));
#258508=CARTESIAN_POINT('Ctrl Pts',(27.0878850123543,-76.4032199208278,
16.5625400513047));
#258509=CARTESIAN_POINT('Ctrl Pts',(27.0888282606249,-76.4046437013157,
16.5601869005576));
#258510=CARTESIAN_POINT('Ctrl Pts',(27.0901243133997,-76.4066000204624,
16.5569535974602));
#258511=CARTESIAN_POINT('Ctrl Pts',(27.0913240247944,-76.4085291386582,
16.5536060903116));
#258512=CARTESIAN_POINT('Ctrl Pts',(27.0924256409491,-76.4104440988722,
16.5500691169233));
#258513=CARTESIAN_POINT('Ctrl Pts',(27.0936398960553,-76.4125548615076,
16.5461704921812));
#258514=CARTESIAN_POINT('Ctrl Pts',(27.0947350223258,-76.4146483558569,
16.5420420626088));
#258515=CARTESIAN_POINT('Ctrl Pts',(27.095715388145,-76.4167317431154,16.5376476090047));
#258516=CARTESIAN_POINT('Ctrl Pts',(27.0962521693207,-76.4178724632835,
16.5352415071946));
#258517=CARTESIAN_POINT('Ctrl Pts',(27.0967546540791,-76.4190099868706,
16.5327567007312));
#258518=CARTESIAN_POINT('Ctrl Pts',(27.0972241917238,-76.4201444978056,
16.530193509747));
#258519=CARTESIAN_POINT('Ctrl Pts',(27.097831559752,-76.4216120386457,16.5268779071077));
#258520=CARTESIAN_POINT('Ctrl Pts',(27.0983817197162,-76.4230689256427,
16.5234805947187));
#258521=CARTESIAN_POINT('Ctrl Pts',(27.0988766740941,-76.4245289974568,
16.5198985627827));
#258522=CARTESIAN_POINT('Ctrl Pts',(27.0994168627798,-76.426122506494,16.5159891658567));
#258523=CARTESIAN_POINT('Ctrl Pts',(27.0998913112301,-76.4277197750987,
16.5118599662324));
#258524=CARTESIAN_POINT('Ctrl Pts',(27.1003044177461,-76.4293303344044,
16.5074394214254));
#258525=CARTESIAN_POINT('Ctrl Pts',(27.1007652522506,-76.4311269686156,
16.5025081518939));
#258526=CARTESIAN_POINT('Ctrl Pts',(27.1011497779682,-76.4329400962105,
16.4972146189847));
#258527=CARTESIAN_POINT('Ctrl Pts',(27.1014658927446,-76.4347734735907,
16.4915299783456));
#258528=CARTESIAN_POINT('Ctrl Pts',(27.1017737851231,-76.4365591633602,
16.4859931997521));
#258529=CARTESIAN_POINT('Ctrl Pts',(27.1020168313413,-76.4383638558958,
16.4800869000299));
#258530=CARTESIAN_POINT('Ctrl Pts',(27.1022032687421,-76.4401848097576,
16.4738312942521));
#258531=CARTESIAN_POINT('Ctrl Pts',(27.1022139471165,-76.4402891065731,
16.4734729986491));
#258532=CARTESIAN_POINT('Ctrl Pts',(27.1022244071887,-76.4403934996852,
16.4731133067631));
#258533=CARTESIAN_POINT('Ctrl Pts',(27.102234658981,-76.4404979871097,16.4727522097143));
#258534=CARTESIAN_POINT('Ctrl Pts',(27.1024069987553,-76.4422544935438,
16.4666819166367));
#258535=CARTESIAN_POINT('Ctrl Pts',(27.1025185267331,-76.4439950495549,
16.4603561171173));
#258536=CARTESIAN_POINT('Ctrl Pts',(27.1026104632814,-76.4457036743809,
16.4538373746393));
#258537=CARTESIAN_POINT('Ctrl Pts',(27.102737424572,-76.4480632279764,16.4448352098468));
#258538=CARTESIAN_POINT('Ctrl Pts',(27.102827792657,-76.4503610778911,16.4354693321256));
#258539=CARTESIAN_POINT('Ctrl Pts',(27.1029292932916,-76.4525659495159,
16.4259934708457));
#258540=CARTESIAN_POINT('Ctrl Pts',(27.1029532015921,-76.4530853032462,
16.4237614479703));
#258541=CARTESIAN_POINT('Ctrl Pts',(27.1029775127231,-76.4535995663555,
16.421523398193));
#258542=CARTESIAN_POINT('Ctrl Pts',(27.1030025074321,-76.4541084615682,
16.4192825760479));
#258543=CARTESIAN_POINT('Ctrl Pts',(27.1030681316507,-76.4554445783686,
16.4133992428192));
#258544=CARTESIAN_POINT('Ctrl Pts',(27.1031446841667,-76.4567431182623,
16.4074886457421));
#258545=CARTESIAN_POINT('Ctrl Pts',(27.1032413604899,-76.4579907933282,
16.4016557321397));
#258546=CARTESIAN_POINT('Ctrl Pts',(27.1033489918153,-76.4593798503026,
16.3951618544127));
#258547=CARTESIAN_POINT('Ctrl Pts',(27.1034813066692,-76.4607059926544,
16.388764083027));
#258548=CARTESIAN_POINT('Ctrl Pts',(27.1036407248819,-76.461963664489,16.3825411897797));
#258549=CARTESIAN_POINT('Ctrl Pts',(27.1038110212171,-76.4633071553021,
16.375893668798));
#258550=CARTESIAN_POINT('Ctrl Pts',(27.1040119034733,-76.4645727497306,
16.3694449691171));
#258551=CARTESIAN_POINT('Ctrl Pts',(27.1042403347499,-76.4657643123006,
16.3632278932428));
#258552=CARTESIAN_POINT('Ctrl Pts',(27.1044944238694,-76.4670897134834,
16.3563125033811));
#258553=CARTESIAN_POINT('Ctrl Pts',(27.1047822483331,-76.4683237252368,
16.3496832123915));
#258554=CARTESIAN_POINT('Ctrl Pts',(27.1050982654298,-76.4694807356141,
16.343319207933));
#258555=CARTESIAN_POINT('Ctrl Pts',(27.105262880177,-76.4700834275971,16.3400041689821));
#258556=CARTESIAN_POINT('Ctrl Pts',(27.1054351610104,-76.4706653451591,
16.3367601359508));
#258557=CARTESIAN_POINT('Ctrl Pts',(27.1056146248408,-76.4712290854507,
16.333578829002));
#258558=CARTESIAN_POINT('Ctrl Pts',(27.1059981721683,-76.4724339024974,
16.326779788912));
#258559=CARTESIAN_POINT('Ctrl Pts',(27.1064227172635,-76.4735621804249,
16.3202525612503));
#258560=CARTESIAN_POINT('Ctrl Pts',(27.1068761143464,-76.4746356794987,
16.3138840528669));
#258561=CARTESIAN_POINT('Ctrl Pts',(27.1073854453231,-76.475841612118,16.3067298855434));
#258562=CARTESIAN_POINT('Ctrl Pts',(27.107931285444,-76.476978942591,16.2997754219255));
#258563=CARTESIAN_POINT('Ctrl Pts',(27.1085192024402,-76.4780834785054,
16.2927957451074));
#258564=CARTESIAN_POINT('Ctrl Pts',(27.1088920706866,-76.4787839963881,
16.2883691000673));
#258565=CARTESIAN_POINT('Ctrl Pts',(27.1092822986947,-76.47947138772,16.283931099016));
#258566=CARTESIAN_POINT('Ctrl Pts',(27.1096950709151,-76.4801541957116,
16.2794145606048));
#258567=CARTESIAN_POINT('Ctrl Pts',(27.1112272268462,-76.4826886887379,
16.2626497669182));
#258568=CARTESIAN_POINT('Ctrl Pts',(27.1130539331532,-76.4851267389767,
16.2450093231248));
#258569=CARTESIAN_POINT('Ctrl Pts',(27.1151298320358,-76.4873049749148,
16.226757619706));
#258570=CARTESIAN_POINT('Ctrl Pts',(27.1152747483161,-76.4874570352355,
16.225483487815));
#258571=CARTESIAN_POINT('Ctrl Pts',(27.1154208732589,-76.4876078246471,
16.2242063963108));
#258572=CARTESIAN_POINT('Ctrl Pts',(27.1155681889353,-76.48775728567,16.2229264434411));
#258573=CARTESIAN_POINT('Ctrl Pts',(27.1170756303587,-76.4892866798432,
16.2098290323389));
#258574=CARTESIAN_POINT('Ctrl Pts',(27.1186810485305,-76.4906357475266,
16.1965813349553));
#258575=CARTESIAN_POINT('Ctrl Pts',(27.1201639645387,-76.4917129534571,
16.1843381456719));
#258576=CARTESIAN_POINT('Ctrl Pts',(27.1209112758457,-76.4922558083237,
16.1781682252344));
#258577=CARTESIAN_POINT('Ctrl Pts',(27.1216272543498,-76.492729591696,16.1722544649754));
#258578=CARTESIAN_POINT('Ctrl Pts',(27.1222827006365,-76.4931225599098,
16.1667491490938));
#258579=CARTESIAN_POINT('Ctrl Pts',(27.1238077656216,-76.4940369019011,
16.153939610534));
#258580=CARTESIAN_POINT('Ctrl Pts',(27.1250450113581,-76.4945873630332,
16.1431163880602));
#258581=CARTESIAN_POINT('Ctrl Pts',(27.1260738037428,-76.4949373713663,
16.1336143833205));
#258582=CARTESIAN_POINT('Ctrl Pts',(27.1263523340118,-76.4950321309278,
16.131041856564));
#258583=CARTESIAN_POINT('Ctrl Pts',(27.1266156271271,-76.4951122560551,
16.1285658678582));
#258584=CARTESIAN_POINT('Ctrl Pts',(27.1268653384347,-76.4951810940983,
16.1261726495344));
#258585=CARTESIAN_POINT('Ctrl Pts',(27.1269115978525,-76.4951938464555,
16.125729302025));
#258586=CARTESIAN_POINT('Ctrl Pts',(27.1269574103529,-76.4952062293152,
16.1252887609781));
#258587=CARTESIAN_POINT('Ctrl Pts',(27.1270027817512,-76.4952182483237,
16.1248509868291));
#258588=CARTESIAN_POINT('Ctrl Pts',(28.7459974181806,74.3634602878982,19.6929518677509));
#258589=CARTESIAN_POINT('Ctrl Pts',(28.8447420032201,74.6189041648808,17.4625));
#258590=CARTESIAN_POINT('Ctrl Pts',(29.6549915892153,76.7149512087496,17.4625));
#258591=CARTESIAN_POINT('Ctrl Pts',(28.493917791474,74.4609043857737,19.6929518673248));
#258592=CARTESIAN_POINT('Ctrl Pts',(28.6971725259776,74.6660793405484,17.5374731486251));
#258593=CARTESIAN_POINT('Ctrl Pts',(29.4834701335382,76.6890525018674,17.4625));
#258594=CARTESIAN_POINT('Ctrl Pts',(28.2438591531039,74.5588475342798,19.6720320649347));
#258595=CARTESIAN_POINT('Ctrl Pts',(28.5391636116362,74.7189440966818,17.5981072780286));
#258596=CARTESIAN_POINT('Ctrl Pts',(29.3136797628433,76.6640386379029,17.4555267321205));
#258597=CARTESIAN_POINT('Ctrl Pts',(27.7480012895968,74.7559270342227,19.5871055664405));
#258598=CARTESIAN_POINT('Ctrl Pts',(28.2117119618052,74.8327386313722,17.6836912763758));
#258599=CARTESIAN_POINT('Ctrl Pts',(28.9778332725232,76.6159646173277,17.4272178998373));
#258600=CARTESIAN_POINT('Ctrl Pts',(27.4997703917934,74.8560677628264,19.5220948206211));
#258601=CARTESIAN_POINT('Ctrl Pts',(28.0404430900709,74.8942448729348,17.709632121867));
#258602=CARTESIAN_POINT('Ctrl Pts',(28.8101355628305,76.5926880471497,17.4055476509055));
#258603=CARTESIAN_POINT('Ctrl Pts',(27.0236898937082,75.0518439197725,19.3489695261652));
#258604=CARTESIAN_POINT('Ctrl Pts',(27.7022510777789,75.019660969593,17.7211023712242));
#258605=CARTESIAN_POINT('Ctrl Pts',(28.4896086814922,76.5500480485612,17.347839219523));
#258606=CARTESIAN_POINT('Ctrl Pts',(26.795355163397,75.1476280619454,19.2413577159505));
#258607=CARTESIAN_POINT('Ctrl Pts',(27.5347169152635,75.0836522525177,17.708077886913));
#258608=CARTESIAN_POINT('Ctrl Pts',(28.3364379275085,76.5306138623668,17.3119686156363));
#258609=CARTESIAN_POINT('Ctrl Pts',(26.4687756770162,75.2884389844461,19.0458961827317));
#258610=CARTESIAN_POINT('Ctrl Pts',(27.2898012152204,75.1803896028207,17.6578979817798));
#258611=CARTESIAN_POINT('Ctrl Pts',(28.1185099510301,76.5048922024807,17.2468147718754));
#258612=CARTESIAN_POINT('Ctrl Pts',(26.3625884843545,75.3348967090535,18.9750294801153));
#258613=CARTESIAN_POINT('Ctrl Pts',(27.209729060121,75.2125498005356,17.6363116935578));
#258614=CARTESIAN_POINT('Ctrl Pts',(28.0478532106456,76.4968949507142,17.2231925371365));
#258615=CARTESIAN_POINT('Ctrl Pts',(26.1560856941727,75.4268801209916,18.8208466626397));
#258616=CARTESIAN_POINT('Ctrl Pts',(27.0529295129826,75.2767579129753,17.5825320214165));
#258617=CARTESIAN_POINT('Ctrl Pts',(27.9109420608577,76.4822364493771,17.1717982652812));
#258618=CARTESIAN_POINT('Ctrl Pts',(26.055101076053,75.4727198166016,18.7368743964309));
#258619=CARTESIAN_POINT('Ctrl Pts',(26.9755857935394,75.3090585336016,17.5501254447857));
#258620=CARTESIAN_POINT('Ctrl Pts',(27.8442489434616,76.4755364557152,17.1438075095171));
#258621=CARTESIAN_POINT('Ctrl Pts',(25.7681502580856,75.6060560547219,18.4696518487122));
#258622=CARTESIAN_POINT('Ctrl Pts',(26.7557364160507,75.4030488168808,17.4386060175111));
#258623=CARTESIAN_POINT('Ctrl Pts',(27.6556756091732,76.4581861338644,17.054733327073));
#258624=CARTESIAN_POINT('Ctrl Pts',(25.5978466210046,75.689411859666,18.2718409363062));
#258625=CARTESIAN_POINT('Ctrl Pts',(26.6226482272615,75.4628679834582,17.3449978161555));
#258626=CARTESIAN_POINT('Ctrl Pts',(27.545042394829,76.4502012574522,16.9887963557568));
#258627=CARTESIAN_POINT('Ctrl Pts',(25.304207074627,75.8449254994659,17.8327278472497));
#258628=CARTESIAN_POINT('Ctrl Pts',(26.3945070907096,75.5732964352821,17.1202191600582));
#258629=CARTESIAN_POINT('Ctrl Pts',(27.3578956810266,76.4429196593756,16.8424253269279));
#258630=CARTESIAN_POINT('Ctrl Pts',(25.1799509742014,75.9179115378174,17.5873106315618));
#258631=CARTESIAN_POINT('Ctrl Pts',(26.2977761963289,75.6248510373174,16.9864091667271));
#258632=CARTESIAN_POINT('Ctrl Pts',(27.2809002299547,76.443787857136,16.7606195878724));
#258633=CARTESIAN_POINT('Ctrl Pts',(25.0456540278887,76.0120135407792,17.2025309630928));
#258634=CARTESIAN_POINT('Ctrl Pts',(26.1964580005439,75.6888631781817,16.7690050915924));
#258635=CARTESIAN_POINT('Ctrl Pts',(27.2023521345518,76.4531141362212,16.6323596984796));
#258636=CARTESIAN_POINT('Ctrl Pts',(25.0090870943394,76.0410349984119,17.0710669460338));
#258637=CARTESIAN_POINT('Ctrl Pts',(26.1695156242376,75.7081633852743,16.6936245453245));
#258638=CARTESIAN_POINT('Ctrl Pts',(27.182007572472,76.4575269782804,16.5885383593542));
#258639=CARTESIAN_POINT('Ctrl Pts',(24.9530103267656,76.0942893550643,16.8014952531469));
#258640=CARTESIAN_POINT('Ctrl Pts',(26.1301341325897,75.7423750031978,16.5376305767308));
#258641=CARTESIAN_POINT('Ctrl Pts',(27.153493597573,76.4691181075126,16.4986811285387));
#258642=CARTESIAN_POINT('Ctrl Pts',(24.9335061597312,76.118653951028,16.6623540419173));
#258643=CARTESIAN_POINT('Ctrl Pts',(26.1176802211114,75.7573877351394,16.4562866616969));
#258644=CARTESIAN_POINT('Ctrl Pts',(27.145369143004,76.4763708127814,16.4523007247639));
#258645=CARTESIAN_POINT('Ctrl Pts',(24.9029553648553,76.1824010629019,16.2463425041047));
#258646=CARTESIAN_POINT('Ctrl Pts',(26.1038934519123,75.7942282194368,16.2122544249953));
#258647=CARTESIAN_POINT('Ctrl Pts',(27.140495466855,76.5018384532045,16.3136302120344));
#258648=CARTESIAN_POINT('Ctrl Pts',(24.9185412707801,76.2131904009613,15.9685880799943));
#258649=CARTESIAN_POINT('Ctrl Pts',(26.1252772492172,75.8084359405689,16.047561016401));
#258650=CARTESIAN_POINT('Ctrl Pts',(27.16243135285,76.5237673449954,16.2210111173688));
#258651=CARTESIAN_POINT('Ctrl Pts',(24.968955626549,76.2326069140441,15.690505851385));
#258652=CARTESIAN_POINT('Ctrl Pts',(26.1756393943756,75.8121214408373,15.8859547915794));
#258653=CARTESIAN_POINT('Ctrl Pts',(27.2087011009323,76.55044485681,16.128351327878));
#258654=CARTESIAN_POINT('',(25.2552738567446,75.9418613629793,17.263393070432));
#258655=CARTESIAN_POINT('Ctrl Pts',(27.127002665508,76.4952182372903,16.1248510388561));
#258656=CARTESIAN_POINT('Ctrl Pts',(27.1261035938164,76.4949835330533,16.1335301302458));
#258657=CARTESIAN_POINT('Ctrl Pts',(27.1250175086501,76.4945938617303,16.1433840167243));
#258658=CARTESIAN_POINT('Ctrl Pts',(27.123665198262,76.4938946426406,16.1550166230771));
#258659=CARTESIAN_POINT('Ctrl Pts',(27.1234107356406,76.4937630714244,16.1572055166426));
#258660=CARTESIAN_POINT('Ctrl Pts',(27.1231468673298,76.4936205663255,16.1594572469111));
#258661=CARTESIAN_POINT('Ctrl Pts',(27.1228730977779,76.4934661405611,16.1617756125053));
#258662=CARTESIAN_POINT('Ctrl Pts',(27.1215904130496,76.4927426139001,16.1726377851693));
#258663=CARTESIAN_POINT('Ctrl Pts',(27.1200357216248,76.4916920130601,16.1853170892971));
#258664=CARTESIAN_POINT('Ctrl Pts',(27.1184437830616,76.490384797411,16.1985845365846));
#258665=CARTESIAN_POINT('Ctrl Pts',(27.117737169702,76.4898045639378,16.2044735549916));
#258666=CARTESIAN_POINT('Ctrl Pts',(27.1170231040063,76.4891738033028,16.2104789373948));
#258667=CARTESIAN_POINT('Ctrl Pts',(27.116321332041,76.4884987572042,16.2164967943271));
#258668=CARTESIAN_POINT('Ctrl Pts',(27.1144314500939,76.4866808483987,16.2327029691798));
#258669=CARTESIAN_POINT('Ctrl Pts',(27.1126943705541,76.4846005967037,16.2486914456544));
#258670=CARTESIAN_POINT('Ctrl Pts',(27.1111721910307,76.4824017848996,16.2640972093815));
#258671=CARTESIAN_POINT('Ctrl Pts',(27.1106324721751,76.4816221526864,16.2695596276057));
#258672=CARTESIAN_POINT('Ctrl Pts',(27.1101196624085,76.4808275267706,16.2749492144068));
#258673=CARTESIAN_POINT('Ctrl Pts',(27.1096361423658,76.4800239584187,16.2802512670947));
#258674=CARTESIAN_POINT('Ctrl Pts',(27.1088775098608,76.4787631770283,16.2885700732594));
#258675=CARTESIAN_POINT('Ctrl Pts',(27.1081924682396,76.4774861247342,16.2966391164468));
#258676=CARTESIAN_POINT('Ctrl Pts',(27.1075731179875,76.4761760059671,16.3046343846518));
#258677=CARTESIAN_POINT('Ctrl Pts',(27.1070239809311,76.4750144099865,16.3117232621208));
#258678=CARTESIAN_POINT('Ctrl Pts',(27.1065264227125,76.4738263115708,16.3187548885504));
#258679=CARTESIAN_POINT('Ctrl Pts',(27.1060881023887,76.4726008566093,16.3258128070659));
#258680=CARTESIAN_POINT('Ctrl Pts',(27.1060320583278,76.4724441687516,16.32671523936));
#258681=CARTESIAN_POINT('Ctrl Pts',(27.1059770032823,76.4722868770211,16.3276180342443));
#258682=CARTESIAN_POINT('Ctrl Pts',(27.1059229723675,76.4721289660875,16.3285213027847));
#258683=CARTESIAN_POINT('Ctrl Pts',(27.1055132758118,76.4709315855521,16.3353704559359));
#258684=CARTESIAN_POINT('Ctrl Pts',(27.1051480063883,76.469686098804,16.3423105850976));
#258685=CARTESIAN_POINT('Ctrl Pts',(27.1048249982592,76.4683756379668,16.3494047007489));
#258686=CARTESIAN_POINT('Ctrl Pts',(27.1045238256014,76.4671537647759,16.356019251509));
#258687=CARTESIAN_POINT('Ctrl Pts',(27.1042596511139,76.4658752319034,16.3627681883452));
#258688=CARTESIAN_POINT('Ctrl Pts',(27.1040326825539,76.4645307210473,16.3696623273304));
#258689=CARTESIAN_POINT('Ctrl Pts',(27.1038205223615,76.4632739316405,16.3761066641726));
#258690=CARTESIAN_POINT('Ctrl Pts',(27.1036411260678,76.4619593190114,16.3826784026799));
#258691=CARTESIAN_POINT('Ctrl Pts',(27.1034929209303,76.4605856089528,16.3893426844219));
#258692=CARTESIAN_POINT('Ctrl Pts',(27.1033578602482,76.4593337345533,16.3954159046419));
#258693=CARTESIAN_POINT('Ctrl Pts',(27.1032489151461,76.4580326598448,16.4015662355624));
#258694=CARTESIAN_POINT('Ctrl Pts',(27.1031602607466,76.4566888072072,16.4077247899965));
#258695=CARTESIAN_POINT('Ctrl Pts',(27.1031225010715,76.4561164335946,16.4103478410299));
#258696=CARTESIAN_POINT('Ctrl Pts',(27.1030883438957,76.4555364067326,16.4129718046109));
#258697=CARTESIAN_POINT('Ctrl Pts',(27.1030568879016,76.4549497809939,16.4155884735622));
#258698=CARTESIAN_POINT('Ctrl Pts',(27.1029432081665,76.4528297571237,16.4250449298201));
#258699=CARTESIAN_POINT('Ctrl Pts',(27.1028516325163,76.450627615447,16.4344055618827));
#258700=CARTESIAN_POINT('Ctrl Pts',(27.1027493830592,76.448361853143,16.4434727015646));
#258701=CARTESIAN_POINT('Ctrl Pts',(27.1027301154644,76.4479348993861,16.4451812873881));
#258702=CARTESIAN_POINT('Ctrl Pts',(27.1027103529397,76.4475057389387,16.4468793703434));
#258703=CARTESIAN_POINT('Ctrl Pts',(27.1026896905071,76.4470745680889,16.4485655884623));
#258704=CARTESIAN_POINT('Ctrl Pts',(27.1026199427357,76.4456191147826,16.4542575589124));
#258705=CARTESIAN_POINT('Ctrl Pts',(27.1025406532748,76.4441322040591,16.4598473134706));
#258706=CARTESIAN_POINT('Ctrl Pts',(27.1024250918518,76.4426004684727,16.4653566991224));
#258707=CARTESIAN_POINT('Ctrl Pts',(27.1023811860632,76.4420185090524,16.4674499056184));
#258708=CARTESIAN_POINT('Ctrl Pts',(27.1023318496943,76.4414302186201,16.4695309610912));
#258709=CARTESIAN_POINT('Ctrl Pts',(27.1022746925428,76.4408353908689,16.4715995364473));
#258710=CARTESIAN_POINT('Ctrl Pts',(27.1020976108819,76.4389925228555,16.4780083015884));
#258711=CARTESIAN_POINT('Ctrl Pts',(27.1018561048147,76.4370710585111,16.4843917801369));
#258712=CARTESIAN_POINT('Ctrl Pts',(27.1015158539155,76.4350620986625,16.4906542061495));
#258713=CARTESIAN_POINT('Ctrl Pts',(27.1012261996205,76.4333518787932,16.4959853855679));
#258714=CARTESIAN_POINT('Ctrl Pts',(27.1008647151577,76.4315790441127,16.5012232667857));
#258715=CARTESIAN_POINT('Ctrl Pts',(27.1004038747161,76.4297403585919,16.5063087804329));
#258716=CARTESIAN_POINT('Ctrl Pts',(27.1000801964374,76.4284489299087,16.509880668131));
#258717=CARTESIAN_POINT('Ctrl Pts',(27.0997073598869,76.4271251515631,16.5133767163781));
#258718=CARTESIAN_POINT('Ctrl Pts',(27.0992746306603,76.425765087242,16.5168023194537));
#258719=CARTESIAN_POINT('Ctrl Pts',(27.0988720744426,76.4244998564341,16.519989064727));
#258720=CARTESIAN_POINT('Ctrl Pts',(27.0984176364788,76.4232033943528,16.5231136244741));
#258721=CARTESIAN_POINT('Ctrl Pts',(27.0979025055475,76.4218676567943,16.5262197343075));
#258722=CARTESIAN_POINT('Ctrl Pts',(27.0978682970957,76.4217789540758,16.5264260026604));
#258723=CARTESIAN_POINT('Ctrl Pts',(27.0978338210948,76.4216900756685,16.526632209209));
#258724=CARTESIAN_POINT('Ctrl Pts',(27.097799075025,76.4216010180793,16.526838375666));
#258725=CARTESIAN_POINT('Ctrl Pts',(27.0976706878967,76.4212719492612,16.5276001631009));
#258726=CARTESIAN_POINT('Ctrl Pts',(27.0975386143428,76.4209404362559,16.5283613866249));
#258727=CARTESIAN_POINT('Ctrl Pts',(27.0974027448545,76.4206063221397,16.5291232096043));
#258728=CARTESIAN_POINT('Ctrl Pts',(27.0966347185492,76.4187176830239,16.5334295486912));
#258729=CARTESIAN_POINT('Ctrl Pts',(27.0957491893792,76.4167566024538,16.5376614539927));
#258730=CARTESIAN_POINT('Ctrl Pts',(27.0947257635409,76.4147290835896,16.5417599887933));
#258731=CARTESIAN_POINT('Ctrl Pts',(27.0938722704172,76.413038220076,16.5451779905074));
#258732=CARTESIAN_POINT('Ctrl Pts',(27.0929228022934,76.4113012291909,16.5485028097945));
#258733=CARTESIAN_POINT('Ctrl Pts',(27.0918686181525,76.4095163162474,16.5517348365881));
#258734=CARTESIAN_POINT('Ctrl Pts',(27.091005746766,76.4080553283169,16.5543803169481));
#258735=CARTESIAN_POINT('Ctrl Pts',(27.0900727246007,76.4065622115715,16.556963800446));
#258736=CARTESIAN_POINT('Ctrl Pts',(27.0890672853592,76.4050319318825,16.559511402248));
#258737=CARTESIAN_POINT('Ctrl Pts',(27.0873467993626,76.4024133502048,16.5638708036362));
#258738=CARTESIAN_POINT('Ctrl Pts',(27.0854160305322,76.3996858222801,16.5681213015847));
#258739=CARTESIAN_POINT('Ctrl Pts',(27.0832453437824,76.3968549739074,16.5722001453423));
#258740=CARTESIAN_POINT('Ctrl Pts',(27.0814237924483,76.3944794420026,16.5756229438131));
#258741=CARTESIAN_POINT('Ctrl Pts',(27.079433200762,76.3920312477983,16.5789244111505));
#258742=CARTESIAN_POINT('Ctrl Pts',(27.0772609129556,76.3895078513819,16.5821034643305));
#258743=CARTESIAN_POINT('Ctrl Pts',(27.0758841940319,76.387908612281,16.5841182354208));
#258744=CARTESIAN_POINT('Ctrl Pts',(27.0744345916962,76.386279051961,16.5860845447345));
#258745=CARTESIAN_POINT('Ctrl Pts',(27.0729104400646,76.3846166914253,16.5880130337727));
#258746=CARTESIAN_POINT('Ctrl Pts',(27.0711860864439,76.3827359747372,16.5901948357581));
#258747=CARTESIAN_POINT('Ctrl Pts',(27.0694154757831,76.3808666413301,16.5922669270651));
#258748=CARTESIAN_POINT('Ctrl Pts',(27.0676055223491,76.3790011612981,16.594274231033));
#258749=CARTESIAN_POINT('Ctrl Pts',(27.0627975216168,76.3740456584708,16.5996064781316));
#258750=CARTESIAN_POINT('Ctrl Pts',(27.0577058759418,76.3691274276556,16.6044118919307));
#258751=CARTESIAN_POINT('Ctrl Pts',(27.0523503507023,76.3642377230734,16.6087783050431));
#258752=CARTESIAN_POINT('Ctrl Pts',(27.0469199087826,76.3592796180229,16.6132057984716));
#258753=CARTESIAN_POINT('Ctrl Pts',(27.0412180804719,76.3543509085699,16.6171815871685));
#258754=CARTESIAN_POINT('Ctrl Pts',(27.0352768340208,76.3494322419913,16.6208506593392));
#258755=CARTESIAN_POINT('Ctrl Pts',(27.0293355875697,76.3445135754128,16.62451973151));
#258756=CARTESIAN_POINT('Ctrl Pts',(27.023154884461,76.3396049868135,16.6278819111735));
#258757=CARTESIAN_POINT('Ctrl Pts',(27.0167787754247,76.3346762337737,16.6311389170594));
#258758=CARTESIAN_POINT('Ctrl Pts',(27.0069163699815,76.3270525622631,16.6361767720262));
#258759=CARTESIAN_POINT('Ctrl Pts',(26.9965742763248,76.3193994276041,16.6408622418876));
#258760=CARTESIAN_POINT('Ctrl Pts',(26.9857761531869,76.3117344496284,16.6452464533288));
#258761=CARTESIAN_POINT('Ctrl Pts',(26.9797217361569,76.3074367607988,16.6477046438934));
#258762=CARTESIAN_POINT('Ctrl Pts',(26.9735241809076,76.3031351576516,16.6500689942496));
#258763=CARTESIAN_POINT('Ctrl Pts',(26.9671894394028,76.2988312337076,16.6523553297694));
#258764=CARTESIAN_POINT('Ctrl Pts',(26.9465400268522,76.284801695006,16.6598081177547));
#258765=CARTESIAN_POINT('Ctrl Pts',(26.9253146403767,76.2713420389522,16.6661261478315));
#258766=CARTESIAN_POINT('Ctrl Pts',(26.903785416654,76.2582666976198,16.6722817468509));
#258767=CARTESIAN_POINT('Ctrl Pts',(26.8683021506494,76.2367166491567,16.6824270618998));
#258768=CARTESIAN_POINT('Ctrl Pts',(26.8318654947013,76.2163231723991,16.6915805494964));
#258769=CARTESIAN_POINT('Ctrl Pts',(26.7948177265923,76.1969868423419,16.7005093018421));
#258770=CARTESIAN_POINT('Ctrl Pts',(26.7912042242594,76.1951008481959,16.7013801793356));
#258771=CARTESIAN_POINT('Ctrl Pts',(26.7875849267253,76.1932248857004,16.7022489427428));
#258772=CARTESIAN_POINT('Ctrl Pts',(26.7839601625922,76.1913588468472,16.7031163158091));
#258773=CARTESIAN_POINT('Ctrl Pts',(26.7552291255565,76.1765680275177,16.7099913914764));
#258774=CARTESIAN_POINT('Ctrl Pts',(26.7262008738658,76.162413994639,16.7168106960652));
#258775=CARTESIAN_POINT('Ctrl Pts',(26.696973285445,76.1489165164747,16.7235973395635));
#258776=CARTESIAN_POINT('Ctrl Pts',(26.6422867919015,76.1236619610232,16.7362955386249));
#258777=CARTESIAN_POINT('Ctrl Pts',(26.5866819737713,76.1005180681597,16.7491519989711));
#258778=CARTESIAN_POINT('Ctrl Pts',(26.5302810836122,76.0794074083457,16.7625435721042));
#258779=CARTESIAN_POINT('Ctrl Pts',(26.4900870715386,76.0643629274333,16.7720870571569));
#258780=CARTESIAN_POINT('Ctrl Pts',(26.449488380492,76.05035210642,16.7819023270163));
#258781=CARTESIAN_POINT('Ctrl Pts',(26.4085292238118,76.0373611942064,16.792133601287));
#258782=CARTESIAN_POINT('Ctrl Pts',(26.363792032232,76.0231720122115,16.8033085988761));
#258783=CARTESIAN_POINT('Ctrl Pts',(26.3190310002086,76.0103384192572,16.814845407717));
#258784=CARTESIAN_POINT('Ctrl Pts',(26.2743222514893,75.998785045632,16.826926246751));
#258785=CARTESIAN_POINT('Ctrl Pts',(26.216135189131,75.9837486849458,16.8426490874556));
#258786=CARTESIAN_POINT('Ctrl Pts',(26.1575989600244,75.9708594776047,16.859231106798));
#258787=CARTESIAN_POINT('Ctrl Pts',(26.0990044705915,75.9600230530952,16.8768965952897));
#258788=CARTESIAN_POINT('Ctrl Pts',(26.0404710852013,75.9491979291252,16.8945436616947));
#258789=CARTESIAN_POINT('Ctrl Pts',(25.9818779785369,75.9404214117304,16.9132712882681));
#258790=CARTESIAN_POINT('Ctrl Pts',(25.9235033740623,75.9336439589075,16.9333228296305));
#258791=CARTESIAN_POINT('Ctrl Pts',(25.8876307737383,75.9294790509219,16.9456449847123));
#258792=CARTESIAN_POINT('Ctrl Pts',(25.851840554364,75.9260699331781,16.9584675280423));
#258793=CARTESIAN_POINT('Ctrl Pts',(25.8161989866991,75.9234132458693,16.9718522765856));
#258794=CARTESIAN_POINT('Ctrl Pts',(25.7935358469298,75.9217239577783,16.9803631375517));
#258795=CARTESIAN_POINT('Ctrl Pts',(25.7708904059767,75.9203357066724,16.9891192993487));
#258796=CARTESIAN_POINT('Ctrl Pts',(25.7483106633367,75.9192531417285,16.9981274246413));
#258797=CARTESIAN_POINT('Ctrl Pts',(25.7019366327795,75.917029781587,17.0166282146742));
#258798=CARTESIAN_POINT('Ctrl Pts',(25.6557154304738,75.916090887903,17.0360687208733));
#258799=CARTESIAN_POINT('Ctrl Pts',(25.6100335198526,75.9163356254776,17.056834669412));
#258800=CARTESIAN_POINT('Ctrl Pts',(25.5677572967879,75.9165621173243,17.0760524705204));
#258801=CARTESIAN_POINT('Ctrl Pts',(25.5259435981048,75.9178014945631,17.0964068029014));
#258802=CARTESIAN_POINT('Ctrl Pts',(25.4848871406365,75.9199460216331,17.1181763512532));
#258803=CARTESIAN_POINT('Ctrl Pts',(25.4448430528779,75.9220376689764,17.1394091063037));
#258804=CARTESIAN_POINT('Ctrl Pts',(25.4055198688358,75.9249898990354,17.1619892997284));
#258805=CARTESIAN_POINT('Ctrl Pts',(25.3671710062583,75.9286842189098,17.1861307294728));
#258806=CARTESIAN_POINT('Ctrl Pts',(25.3326536301789,75.932009434311,17.2078601564642));
#258807=CARTESIAN_POINT('Ctrl Pts',(25.2989256360752,75.9359354286627,17.2308544603867));
#258808=CARTESIAN_POINT('Ctrl Pts',(25.2661521621818,75.9403670676029,17.2552262516159));
#258809=CARTESIAN_POINT('Ctrl Pts',(25.2625142517442,75.9408589869402,17.2579315612203));
#258810=CARTESIAN_POINT('Ctrl Pts',(25.2588880803261,75.9413571303185,17.2606537952043));
#258811=CARTESIAN_POINT('Ctrl Pts',(25.2552738568381,75.9418613633423,17.2633930704885));
#258812=CARTESIAN_POINT('Ctrl Pts',(25.2552738568381,75.9418613633423,17.2633930704885));
#258813=CARTESIAN_POINT('Ctrl Pts',(25.2383250955439,75.9442259477243,17.2762387760009));
#258814=CARTESIAN_POINT('Ctrl Pts',(25.2219501076014,75.9466297979497,17.2896217176795));
#258815=CARTESIAN_POINT('Ctrl Pts',(25.2063620808563,75.9489416166713,17.3037656232924));
#258816=CARTESIAN_POINT('Ctrl Pts',(25.1906119975066,75.9512774695763,17.3180565721045));
#258817=CARTESIAN_POINT('Ctrl Pts',(25.1756652588064,75.9535194008814,17.3331243157626));
#258818=CARTESIAN_POINT('Ctrl Pts',(25.1617083521129,75.9555501186536,17.3491621101996));
#258819=CARTESIAN_POINT('Ctrl Pts',(25.1475411611284,75.9576114326071,17.3654415410039));
#258820=CARTESIAN_POINT('Ctrl Pts',(25.1343938078986,75.9594551436918,17.3827204208315));
#258821=CARTESIAN_POINT('Ctrl Pts',(25.1224278840864,75.9609767648295,17.4011633324362));
#258822=CARTESIAN_POINT('Ctrl Pts',(25.12105367141,75.9611515136486,17.4032813872821));
#258823=CARTESIAN_POINT('Ctrl Pts',(25.1196950054388,75.9613220335946,17.4054147550736));
#258824=CARTESIAN_POINT('Ctrl Pts',(25.1183521036895,75.9614881812303,17.4075636545405));
#258825=CARTESIAN_POINT('Origin',(29.6549915892153,76.7149512087495,20.0025));
#258826=CARTESIAN_POINT('Origin',(0.,0.,20.0025));
#258827=CARTESIAN_POINT('Origin',(76.7149512087496,29.6549915892152,20.0025));
#258828=CARTESIAN_POINT('Ctrl Pts',(76.2270397428134,24.9561066903835,15.7661615844266));
#258829=CARTESIAN_POINT('Ctrl Pts',(75.8108535386762,26.1626160164788,15.9301351099137));
#258830=CARTESIAN_POINT('Ctrl Pts',(76.5433020278671,27.1967142373006,16.1535699055586));
#258831=CARTESIAN_POINT('Ctrl Pts',(76.2058614110631,24.9127382418325,16.0399812791097));
#258832=CARTESIAN_POINT('Ctrl Pts',(75.8053384807186,26.1182670027238,16.0896762568481));
#258833=CARTESIAN_POINT('Ctrl Pts',(76.517885002826,27.1555364032829,16.2448123919216));
#258834=CARTESIAN_POINT('Ctrl Pts',(76.1737533047141,24.9032085414216,16.3126628275193));
#258835=CARTESIAN_POINT('Ctrl Pts',(75.7896805171524,26.1022033001563,16.2513677269997));
#258836=CARTESIAN_POINT('Ctrl Pts',(76.4971501245561,27.1380437449529,16.3357369865075));
#258837=CARTESIAN_POINT('Ctrl Pts',(76.1088055482311,24.9409015162127,16.7198279320328));
#258838=CARTESIAN_POINT('Ctrl Pts',(75.751382754071,26.1222593418385,16.4898842731734));
#258839=CARTESIAN_POINT('Ctrl Pts',(76.4732843611527,27.1482624002493,16.4714586881349));
#258840=CARTESIAN_POINT('Ctrl Pts',(76.0840986821809,24.9625025815324,16.8562699832887));
#258841=CARTESIAN_POINT('Ctrl Pts',(75.7359563155035,26.1365526017809,16.5694930915592));
#258842=CARTESIAN_POINT('Ctrl Pts',(76.4665075541088,27.1579592507432,16.5169393719347));
#258843=CARTESIAN_POINT('Ctrl Pts',(76.0302035557089,25.0223408867823,17.1211357027625));
#258844=CARTESIAN_POINT('Ctrl Pts',(75.7010090395948,26.1792011664334,16.7223674157641));
#258845=CARTESIAN_POINT('Ctrl Pts',(76.4557551903463,27.189285584288,16.6052279449151));
#258846=CARTESIAN_POINT('Ctrl Pts',(76.0009882041842,25.0604718640614,17.2500386492964));
#258847=CARTESIAN_POINT('Ctrl Pts',(75.6814529502716,26.2075059010005,16.7960334331997));
#258848=CARTESIAN_POINT('Ctrl Pts',(76.4517310112362,27.2108217423656,16.6481955938982));
#258849=CARTESIAN_POINT('Ctrl Pts',(75.9067264066431,25.198342960339,17.6266213749776));
#258850=CARTESIAN_POINT('Ctrl Pts',(75.617033261059,26.3119626202797,17.0080082070259));
#258851=CARTESIAN_POINT('Ctrl Pts',(76.4434487742633,27.2921796118939,16.7737231689762));
#258852=CARTESIAN_POINT('Ctrl Pts',(75.8341334517195,25.3235144045994,17.8663209238626));
#258853=CARTESIAN_POINT('Ctrl Pts',(75.5656656095422,26.4095014785168,17.138034603396));
#258854=CARTESIAN_POINT('Ctrl Pts',(76.443086689911,27.3700274901018,16.8536230191253));
#258855=CARTESIAN_POINT('Ctrl Pts',(75.6793115466567,25.6181437847437,18.2967865872453));
#258856=CARTESIAN_POINT('Ctrl Pts',(75.4556558389512,26.6384413152297,17.3570330067414));
#258857=CARTESIAN_POINT('Ctrl Pts',(76.4510616926957,27.5581771453565,16.9971115727434));
#258858=CARTESIAN_POINT('Ctrl Pts',(75.5964910133644,25.7881636116429,18.4907575655788));
#258859=CARTESIAN_POINT('Ctrl Pts',(75.3962436041948,26.7712230598584,17.4481057023255));
#258860=CARTESIAN_POINT('Ctrl Pts',(76.4592507908039,27.6687468882713,17.0617685660245));
#258861=CARTESIAN_POINT('Ctrl Pts',(75.4201247071596,26.1689222277689,18.8401402132359));
#258862=CARTESIAN_POINT('Ctrl Pts',(75.2714903396935,27.063945082347,17.5930975378977));
#258863=CARTESIAN_POINT('Ctrl Pts',(76.482579458453,27.9191372577337,17.1782294484131));
#258864=CARTESIAN_POINT('Ctrl Pts',(75.3287012831505,26.3751256473571,18.9911133259122));
#258865=CARTESIAN_POINT('Ctrl Pts',(75.2073607607574,27.2212827369394,17.6447564223772));
#258866=CARTESIAN_POINT('Ctrl Pts',(76.4974527826309,28.0559817658927,17.2285538196831));
#258867=CARTESIAN_POINT('Ctrl Pts',(75.1416312561383,26.8095530404412,19.2484985828626));
#258868=CARTESIAN_POINT('Ctrl Pts',(75.0796306617783,27.5451541663913,17.709236776907));
#258869=CARTESIAN_POINT('Ctrl Pts',(76.5318000250945,28.3459497946491,17.3143489047412));
#258870=CARTESIAN_POINT('Ctrl Pts',(75.0448154219373,27.0405974954697,19.3560977072767));
#258871=CARTESIAN_POINT('Ctrl Pts',(75.0150709808039,27.7144253322462,17.7214394194467));
#258872=CARTESIAN_POINT('Ctrl Pts',(76.551521599115,28.5009695287673,17.3502152802456));
#258873=CARTESIAN_POINT('Ctrl Pts',(74.7540920556819,27.7481365991003,19.6103581821464));
#258874=CARTESIAN_POINT('Ctrl Pts',(74.8268871764671,28.2225181462175,17.7018269936053));
#258875=CARTESIAN_POINT('Ctrl Pts',(76.6150183791995,28.9773980402713,17.4349687706577));
#258876=CARTESIAN_POINT('Ctrl Pts',(74.5573270579655,28.2444805055458,19.6929518696644));
#258877=CARTESIAN_POINT('Ctrl Pts',(74.7114471924104,28.5552565684103,17.6095740109439));
#258878=CARTESIAN_POINT('Ctrl Pts',(76.6634338736826,29.3138035781366,17.4625));
#258879=CARTESIAN_POINT('Ctrl Pts',(74.3634602878982,28.7459974181806,19.6929518677509));
#258880=CARTESIAN_POINT('Ctrl Pts',(74.6189041648808,28.8447420032201,17.4625));
#258881=CARTESIAN_POINT('Ctrl Pts',(76.7149512087496,29.6549915892152,17.4625));
#258882=CARTESIAN_POINT('',(75.9418613907131,25.2552738638853,17.2633930747485));
#258883=CARTESIAN_POINT('Ctrl Pts',(75.9614888783998,25.1183464686498,17.4075726719158));
#258884=CARTESIAN_POINT('Ctrl Pts',(75.9600468328487,25.1300023941469,17.3889199736803));
#258885=CARTESIAN_POINT('Ctrl Pts',(75.9582739286019,25.1428486640187,17.3714404189718));
#258886=CARTESIAN_POINT('Ctrl Pts',(75.956271615219,25.1567289812122,17.3549752069932));
#258887=CARTESIAN_POINT('Ctrl Pts',(75.9542910924864,25.1704582425619,17.3386891815889));
#258888=CARTESIAN_POINT('Ctrl Pts',(75.952086092421,25.1851992333012,17.3233956168879));
#258889=CARTESIAN_POINT('Ctrl Pts',(75.9497720847174,25.2007688946097,17.3089051461458));
#258890=CARTESIAN_POINT('Ctrl Pts',(75.9474908499987,25.2161180448657,17.2946199020231));
#258891=CARTESIAN_POINT('Ctrl Pts',(75.945103652396,25.2322726009112,17.2811152127705));
#258892=CARTESIAN_POINT('Ctrl Pts',(75.9427384198447,25.2490253201792,17.2681738831956));
#258893=CARTESIAN_POINT('Ctrl Pts',(75.9424456215465,25.251099182933,17.2665718422994));
#258894=CARTESIAN_POINT('Ctrl Pts',(75.9421531821386,25.2531821712323,17.2649783885439));
#258895=CARTESIAN_POINT('Ctrl Pts',(75.9418613633423,25.2552738568381,17.2633930704886));
#258896=CARTESIAN_POINT('',(76.4940243385606,27.123919681122,16.1529193687788));
#258897=CARTESIAN_POINT('Ctrl Pts',(75.9418614454548,25.2552738779798,17.2633930832684));
#258898=CARTESIAN_POINT('Ctrl Pts',(75.9365384120977,25.2934285134618,17.2344751189325));
#258899=CARTESIAN_POINT('Ctrl Pts',(75.9319214636048,25.332694849713,17.2076986349233));
#258900=CARTESIAN_POINT('Ctrl Pts',(75.9281351401283,25.3728650680937,17.1826763946697));
#258901=CARTESIAN_POINT('Ctrl Pts',(75.9242738575013,25.4138305501284,17.1571587805044));
#258902=CARTESIAN_POINT('Ctrl Pts',(75.921276377852,25.4557366826118,17.1334650775218));
#258903=CARTESIAN_POINT('Ctrl Pts',(75.919265820559,25.4983989473329,17.1112236978224));
#258904=CARTESIAN_POINT('Ctrl Pts',(75.9172478169732,25.5412192158649,17.0888999450288));
#258905=CARTESIAN_POINT('Ctrl Pts',(75.9162240339414,25.5848018402272,17.0680389986439));
#258906=CARTESIAN_POINT('Ctrl Pts',(75.9163105407607,25.6289865102456,17.0483098578789));
#258907=CARTESIAN_POINT('Ctrl Pts',(75.9163971000492,25.6731979796606,17.0285687507676));
#258908=CARTESIAN_POINT('Ctrl Pts',(75.9175953146014,25.7180127240943,17.009960645641));
#258909=CARTESIAN_POINT('Ctrl Pts',(75.9200131196572,25.7632880277473,16.9922021492894));
#258910=CARTESIAN_POINT('Ctrl Pts',(75.9208133176951,25.7782723661501,16.9863247879602));
#258911=CARTESIAN_POINT('Ctrl Pts',(75.9217470339365,25.7933072658459,16.9805408907029));
#258912=CARTESIAN_POINT('Ctrl Pts',(75.92281796933,25.8083878526028,16.9748413874889));
#258913=CARTESIAN_POINT('Ctrl Pts',(75.9266539103138,25.8624044078057,16.9544265631223));
#258914=CARTESIAN_POINT('Ctrl Pts',(75.9321927734631,25.9166410369771,16.9353703453911));
#258915=CARTESIAN_POINT('Ctrl Pts',(75.939475260865,25.970905038449,16.9174202920556));
#258916=CARTESIAN_POINT('Ctrl Pts',(75.9468216077909,26.0256448764201,16.8993128362008));
#258917=CARTESIAN_POINT('Ctrl Pts',(75.9559423034969,26.0804129308954,16.8823309775028));
#258918=CARTESIAN_POINT('Ctrl Pts',(75.966865448933,26.1350308076104,16.8662635483136));
#258919=CARTESIAN_POINT('Ctrl Pts',(75.9779822941092,26.1906172211435,16.849911195988));
#258920=CARTESIAN_POINT('Ctrl Pts',(75.990966169439,26.2460483691195,16.8345059849871));
#258921=CARTESIAN_POINT('Ctrl Pts',(76.0058318119529,26.3011513056163,16.8198753596885));
#258922=CARTESIAN_POINT('Ctrl Pts',(76.0144317203761,26.3330288519297,16.8114114108466));
#258923=CARTESIAN_POINT('Ctrl Pts',(76.0236611245447,26.3647968075541,16.8032076252318));
#258924=CARTESIAN_POINT('Ctrl Pts',(76.0335204515053,26.3964234203472,16.7952379320009));
#258925=CARTESIAN_POINT('Ctrl Pts',(76.0465904882018,26.4383493034671,16.7846728920742));
#258926=CARTESIAN_POINT('Ctrl Pts',(76.0607989879201,26.4801552170103,16.7745161348116));
#258927=CARTESIAN_POINT('Ctrl Pts',(76.076181153933,26.5217114878631,16.7646135070096));
#258928=CARTESIAN_POINT('Ctrl Pts',(76.0919178815735,26.564225638056,16.754482621898));
#258929=CARTESIAN_POINT('Ctrl Pts',(76.1088831745402,26.6064784254766,16.744617907061));
#258930=CARTESIAN_POINT('Ctrl Pts',(76.1270927055454,26.6483386168421,16.7349036639692));
#258931=CARTESIAN_POINT('Ctrl Pts',(76.1321077576901,26.6598672521718,16.7322282828385));
#258932=CARTESIAN_POINT('Ctrl Pts',(76.1372170507315,26.6713661579223,16.7295645869382));
#258933=CARTESIAN_POINT('Ctrl Pts',(76.1424206041304,26.6828327105675,16.7269107591349));
#258934=CARTESIAN_POINT('Ctrl Pts',(76.1535835707417,26.7074314288879,16.7212176127617));
#258935=CARTESIAN_POINT('Ctrl Pts',(76.1651211245957,26.7318858270285,16.7157439161817));
#258936=CARTESIAN_POINT('Ctrl Pts',(76.1770916036276,26.7560986664057,16.710212104333));
#258937=CARTESIAN_POINT('Ctrl Pts',(76.1892078939106,26.7806064400448,16.7046129100175));
#258938=CARTESIAN_POINT('Ctrl Pts',(76.2017677451098,26.8048664435746,16.6989544081906));
#258939=CARTESIAN_POINT('Ctrl Pts',(76.2148157305206,26.8287898949487,16.692999142927));
#258940=CARTESIAN_POINT('Ctrl Pts',(76.2278918585853,26.8527649458142,16.687031033001));
#258941=CARTESIAN_POINT('Ctrl Pts',(76.2414581212042,26.8764013225654,16.6807652464606));
#258942=CARTESIAN_POINT('Ctrl Pts',(76.2555440512879,26.8996289161678,16.6740083767523));
#258943=CARTESIAN_POINT('Ctrl Pts',(76.2664668899232,26.9176405955741,16.6687688081142));
#258944=CARTESIAN_POINT('Ctrl Pts',(76.2777018328891,26.9354066661027,16.6632349103941));
#258945=CARTESIAN_POINT('Ctrl Pts',(76.2892574542475,26.9529072015636,16.6573331470885));
#258946=CARTESIAN_POINT('Ctrl Pts',(76.2970453605966,26.9647016803719,16.6533556560915));
#258947=CARTESIAN_POINT('Ctrl Pts',(76.3050296927762,26.9765199249428,16.6492837031864));
#258948=CARTESIAN_POINT('Ctrl Pts',(76.3131571939983,26.9880307645767,16.6447775694554));
#258949=CARTESIAN_POINT('Ctrl Pts',(76.3209361875772,26.9990480188537,16.6404646589554));
#258950=CARTESIAN_POINT('Ctrl Pts',(76.3288457889269,27.0097828635244,16.6357546796883));
#258951=CARTESIAN_POINT('Ctrl Pts',(76.3368225865422,27.019982665784,16.6303684690638));
#258952=CARTESIAN_POINT('Ctrl Pts',(76.3439369962744,27.0290797465877,16.6255645726716));
#258953=CARTESIAN_POINT('Ctrl Pts',(76.3511042487789,27.0377508834012,16.6202234204512));
#258954=CARTESIAN_POINT('Ctrl Pts',(76.3582739443018,27.0458546401499,16.6141527467482));
#258955=CARTESIAN_POINT('Ctrl Pts',(76.3648732839341,27.0533137355762,16.6085650007364));
#258956=CARTESIAN_POINT('Ctrl Pts',(76.3714742611997,27.0602917480244,16.6023596051119));
#258957=CARTESIAN_POINT('Ctrl Pts',(76.3780396076468,27.0667174263885,16.5953847330164));
#258958=CARTESIAN_POINT('Ctrl Pts',(76.3848383240895,27.0733715101451,16.5881619340393));
#258959=CARTESIAN_POINT('Ctrl Pts',(76.3914209742982,27.0790454161737,16.5799443021262));
#258960=CARTESIAN_POINT('Ctrl Pts',(76.3975982251587,27.0837210218629,16.5709392072));
#258961=CARTESIAN_POINT('Ctrl Pts',(76.3980209336111,27.0840409729365,16.5703229897554));
#258962=CARTESIAN_POINT('Ctrl Pts',(76.3984417507368,27.0843562498919,16.5697030660327));
#258963=CARTESIAN_POINT('Ctrl Pts',(76.3988606189191,27.0846668466571,16.5690794942353));
#258964=CARTESIAN_POINT('Ctrl Pts',(76.4054137841379,27.0895261126631,16.5593237543952));
#258965=CARTESIAN_POINT('Ctrl Pts',(76.4114901846566,27.093245410726,16.5486722305523));
#258966=CARTESIAN_POINT('Ctrl Pts',(76.416877640854,27.0957927187002,16.5373328835886));
#258967=CARTESIAN_POINT('Ctrl Pts',(76.4172351860215,27.095961773932,16.5365803338581));
#258968=CARTESIAN_POINT('Ctrl Pts',(76.4175897023702,27.0961256557399,16.5358247401331));
#258969=CARTESIAN_POINT('Ctrl Pts',(76.4179411301446,27.0962843493429,16.5350661571352));
#258970=CARTESIAN_POINT('Ctrl Pts',(76.4231203592808,27.0986231244543,16.5238864057029));
#258971=CARTESIAN_POINT('Ctrl Pts',(76.4276313558999,27.1000270257133,16.5124226895554));
#258972=CARTESIAN_POINT('Ctrl Pts',(76.4316784850439,27.1009185160801,16.5007540438377));
#258973=CARTESIAN_POINT('Ctrl Pts',(76.4357092910718,27.1018064108362,16.4891324607791));
#258974=CARTESIAN_POINT('Ctrl Pts',(76.4392804564639,27.1021859277025,16.4773075420962));
#258975=CARTESIAN_POINT('Ctrl Pts',(76.4425873543179,27.1024353107015,16.4653907080849));
#258976=CARTESIAN_POINT('Ctrl Pts',(76.4429680133926,27.102464017334,16.4640189538887));
#258977=CARTESIAN_POINT('Ctrl Pts',(76.4433451597764,27.1024909575151,16.4626460183039));
#258978=CARTESIAN_POINT('Ctrl Pts',(76.4437190824838,27.1025166752918,16.4612720996402));
#258979=CARTESIAN_POINT('Ctrl Pts',(76.4469339796244,27.1027377905252,16.4494594787538));
#258980=CARTESIAN_POINT('Ctrl Pts',(76.4499306971237,27.1029008537886,16.4375780171924));
#258981=CARTESIAN_POINT('Ctrl Pts',(76.4527422098279,27.1030868022619,16.4256727165939));
#258982=CARTESIAN_POINT('Ctrl Pts',(76.4559507900088,27.1032990120752,16.4120860408196));
#258983=CARTESIAN_POINT('Ctrl Pts',(76.4589211030455,27.1035230776377,16.3984375728355));
#258984=CARTESIAN_POINT('Ctrl Pts',(76.4617002467785,27.1038478560124,16.3847624646941));
#258985=CARTESIAN_POINT('Ctrl Pts',(76.4623520422173,27.1039240266187,16.3815552275135));
#258986=CARTESIAN_POINT('Ctrl Pts',(76.462993426712,27.1040058139871,16.3783464458544));
#258987=CARTESIAN_POINT('Ctrl Pts',(76.4636250782641,27.1040943433334,16.3751364513276));
#258988=CARTESIAN_POINT('Ctrl Pts',(76.4641777733722,27.1041718065114,16.3723277061167));
#258989=CARTESIAN_POINT('Ctrl Pts',(76.4647230169086,27.1042544313724,16.369518032365));
#258990=CARTESIAN_POINT('Ctrl Pts',(76.4652612709139,27.1043429664181,16.3667076535841));
#258991=CARTESIAN_POINT('Ctrl Pts',(76.4686617029972,27.1049022886096,16.3489530208693));
#258992=CARTESIAN_POINT('Ctrl Pts',(76.4717819392994,27.1056974920644,16.3311709383671));
#258993=CARTESIAN_POINT('Ctrl Pts',(76.4747456942296,27.1069148091889,16.3134161472461));
#258994=CARTESIAN_POINT('Ctrl Pts',(76.4750658663008,27.1070463149829,16.311498111382));
#258995=CARTESIAN_POINT('Ctrl Pts',(76.4753841981967,27.1071827142443,16.3095804292481));
#258996=CARTESIAN_POINT('Ctrl Pts',(76.4757008361693,27.1073242180731,16.3076631955713));
#258997=CARTESIAN_POINT('Ctrl Pts',(76.4793038165454,27.1089343708732,16.2858472546199));
#258998=CARTESIAN_POINT('Ctrl Pts',(76.4826051109754,27.1110715810776,16.2640219361389));
#258999=CARTESIAN_POINT('Ctrl Pts',(76.4854470365061,27.1134723701869,16.2421547185838));
#259000=CARTESIAN_POINT('Ctrl Pts',(76.488337228718,27.1159139338068,16.2199161126836));
#259001=CARTESIAN_POINT('Ctrl Pts',(76.4907521576887,27.1186282162397,16.1976339393734));
#259002=CARTESIAN_POINT('Ctrl Pts',(76.4925052054321,27.1212940444935,16.1752508035511));
#259003=CARTESIAN_POINT('Ctrl Pts',(76.4930872524614,27.1221791529691,16.1678191532948));
#259004=CARTESIAN_POINT('Ctrl Pts',(76.4935961816787,27.1230585570135,16.1603762016909));
#259005=CARTESIAN_POINT('Ctrl Pts',(76.4940247511736,27.1239194136308,16.1529193631625));
#259006=CARTESIAN_POINT('Origin',(77.4800206767709,27.1771821124719,15.1653884328171));
#259007=CARTESIAN_POINT('Ctrl Pts',(-24.9689313575503,76.2325975651782,
15.6906397325477));
#259008=CARTESIAN_POINT('Ctrl Pts',(-26.1756150602392,75.8121196590787,
15.8860328844641));
#259009=CARTESIAN_POINT('Ctrl Pts',(-27.2086788182721,76.5504320086846,
16.1283959549323));
#259010=CARTESIAN_POINT('Ctrl Pts',(-24.9186909562191,76.2132400197742,
15.9678244963451));
#259011=CARTESIAN_POINT('Ctrl Pts',(-26.1254229642346,75.8084425279472,
16.0471243598401));
#259012=CARTESIAN_POINT('Ctrl Pts',(-27.1625656651785,76.5238417787868,
16.2207578908869));
#259013=CARTESIAN_POINT('Ctrl Pts',(-24.9032159272866,76.1826381079975,
16.2438456162063));
#259014=CARTESIAN_POINT('Ctrl Pts',(-26.104184876118,75.7943214248672,16.2107725763316));
#259015=CARTESIAN_POINT('Ctrl Pts',(-27.1407766635656,76.5020517602981,
16.3127979160863));
#259016=CARTESIAN_POINT('Ctrl Pts',(-24.9328226963039,76.1197004175058,
16.6559867599131));
#259017=CARTESIAN_POINT('Ctrl Pts',(-26.1172873190745,75.7580138780943,
16.4525591935362));
#259018=CARTESIAN_POINT('Ctrl Pts',(-27.1451435881167,76.4767312134559,
16.4501782974201));
#259019=CARTESIAN_POINT('Ctrl Pts',(-24.9518097701917,76.0956371509859,
16.794110417305));
#259020=CARTESIAN_POINT('Ctrl Pts',(-26.1293351405267,75.7432179427279,
16.5333292440492));
#259021=CARTESIAN_POINT('Ctrl Pts',(-27.1529468723184,76.469480763603,16.4962195166108));
#259022=CARTESIAN_POINT('Ctrl Pts',(-25.0073336657117,76.042503213137,17.0641682497299));
#259023=CARTESIAN_POINT('Ctrl Pts',(-26.1682415554322,75.7091288541245,
16.689657071876));
#259024=CARTESIAN_POINT('Ctrl Pts',(-27.1810555370846,76.4577808154583,
16.5862387939002));
#259025=CARTESIAN_POINT('Ctrl Pts',(-25.043582291958,76.0135981896359,17.195550558677));
#259026=CARTESIAN_POINT('Ctrl Pts',(-26.1949210471983,75.6899232799161,
16.765020182013));
#259027=CARTESIAN_POINT('Ctrl Pts',(-27.2011812093646,76.4533313045575,
16.6300328970328));
#259028=CARTESIAN_POINT('Ctrl Pts',(-25.1764553135876,75.9201060960321,
17.5792969885075));
#259029=CARTESIAN_POINT('Ctrl Pts',(-26.2950899509095,75.6263767700401,
16.9819673365835));
#259030=CARTESIAN_POINT('Ctrl Pts',(-27.2787774842966,76.4438901441637,
16.7579483734706));
#259031=CARTESIAN_POINT('Ctrl Pts',(-25.2993526607335,75.8476684832879,
17.8240388353673));
#259032=CARTESIAN_POINT('Ctrl Pts',(-26.3907356809289,75.5752351470883,
17.1155820316989));
#259033=CARTESIAN_POINT('Ctrl Pts',(-27.3548544480324,76.4428939284352,
16.8395289896467));
#259034=CARTESIAN_POINT('Ctrl Pts',(-25.5919984567931,75.6923432030072,
18.264473921103));
#259035=CARTESIAN_POINT('Ctrl Pts',(-26.6180940171725,75.4649619696492,
17.3414092350324));
#259036=CARTESIAN_POINT('Ctrl Pts',(-27.5412643883038,76.4499649794134,
16.9863406840095));
#259037=CARTESIAN_POINT('Ctrl Pts',(-25.7617839502725,75.6091210995783,
18.4627331486811));
#259038=CARTESIAN_POINT('Ctrl Pts',(-26.7507911294727,75.4052371346467,
17.435438103078));
#259039=CARTESIAN_POINT('Ctrl Pts',(-27.6515244073507,76.4578597275981,
17.0524270937445));
#259040=CARTESIAN_POINT('Ctrl Pts',(-26.1430805994636,75.4317357552708,
18.8197595498714));
#259041=CARTESIAN_POINT('Ctrl Pts',(-27.0442130694164,75.2796463045432,
17.5855829975127));
#259042=CARTESIAN_POINT('Ctrl Pts',(-27.9020344677406,76.4807996718625,
17.171435893939));
#259043=CARTESIAN_POINT('Ctrl Pts',(-26.3510560884158,75.3392616135107,
18.9747290102613));
#259044=CARTESIAN_POINT('Ctrl Pts',(-27.2031302208847,75.2146749685611,
17.6396375078347));
#259045=CARTESIAN_POINT('Ctrl Pts',(-28.0399748698368,76.4956562029936,
17.2230923811494));
#259046=CARTESIAN_POINT('Ctrl Pts',(-26.7887981118742,75.1503919246085,
19.2381193325699));
#259047=CARTESIAN_POINT('Ctrl Pts',(-27.5299162784606,75.0854973188483,
17.7075896666723));
#259048=CARTESIAN_POINT('Ctrl Pts',(-28.3320433237805,76.5300629685854,
17.3108891546271));
#259049=CARTESIAN_POINT('Ctrl Pts',(-27.0218910128871,75.0525919498098,
19.3482083029783));
#259050=CARTESIAN_POINT('Ctrl Pts',(-27.7009559314809,75.0201494871697,
17.7210643477414));
#259051=CARTESIAN_POINT('Ctrl Pts',(-28.4884000162535,76.5498913973921,
17.3475854788263));
#259052=CARTESIAN_POINT('Ctrl Pts',(-27.4985053196503,74.8565797596348,
19.521741160188));
#259053=CARTESIAN_POINT('Ctrl Pts',(-28.0395707962218,74.8945599897606,
17.7097451055821));
#259054=CARTESIAN_POINT('Ctrl Pts',(-28.8092814008564,76.5925703049495,
17.4054297637285));
#259055=CARTESIAN_POINT('Ctrl Pts',(-27.7422284005861,74.758241529272,19.5858151824399));
#259056=CARTESIAN_POINT('Ctrl Pts',(-28.2078168588108,74.8341192521282,
17.6844550416307));
#259057=CARTESIAN_POINT('Ctrl Pts',(-28.9739291008619,76.6154156279985,
17.4267877716097));
#259058=CARTESIAN_POINT('Ctrl Pts',(-28.2396160007789,74.560514330493,19.6716009699532));
#259059=CARTESIAN_POINT('Ctrl Pts',(-28.536471100917,74.7198525855479,17.5990670510758));
#259060=CARTESIAN_POINT('Ctrl Pts',(-29.3108001463012,76.6636167731309,
17.4553830340207));
#259061=CARTESIAN_POINT('Ctrl Pts',(-28.4947415154366,74.4605859662117,
19.6929518687095));
#259062=CARTESIAN_POINT('Ctrl Pts',(-28.697661261183,74.6659231009684,17.5372248464383));
#259063=CARTESIAN_POINT('Ctrl Pts',(-29.4840227026744,76.6891359364473,
17.4625));
#259064=CARTESIAN_POINT('Ctrl Pts',(-28.7459974181806,74.3634602878982,
19.6929518677509));
#259065=CARTESIAN_POINT('Ctrl Pts',(-28.8447420032201,74.6189041648809,
17.4625));
#259066=CARTESIAN_POINT('Ctrl Pts',(-29.6549915892152,76.7149512087496,
17.4625));
#259067=CARTESIAN_POINT('',(-25.2552738568382,75.9418613633423,17.2633930704884));
#259068=CARTESIAN_POINT('Ctrl Pts',(-25.1183523255102,75.961488153786,17.4075632995852));
#259069=CARTESIAN_POINT('Ctrl Pts',(-25.1300086289606,75.9600460003527,
17.3889110251594));
#259070=CARTESIAN_POINT('Ctrl Pts',(-25.1428552492175,75.9582730048897,
17.3714318666836));
#259071=CARTESIAN_POINT('Ctrl Pts',(-25.1567358846801,75.9562706193481,
17.354967018135));
#259072=CARTESIAN_POINT('Ctrl Pts',(-25.1704654612766,75.9542900251785,
17.3386813516821));
#259073=CARTESIAN_POINT('Ctrl Pts',(-25.1852067359063,75.9520849723068,
17.3233881139037));
#259074=CARTESIAN_POINT('Ctrl Pts',(-25.2007766452391,75.9497709327977,
17.3088979329118));
#259075=CARTESIAN_POINT('Ctrl Pts',(-25.2161260490804,75.9474896653754,
17.294612965991));
#259076=CARTESIAN_POINT('Ctrl Pts',(-25.2322808248086,75.9451024553525,
17.2811085187395));
#259077=CARTESIAN_POINT('Ctrl Pts',(-25.2490337250752,75.9427372332084,
17.2681673905741));
#259078=CARTESIAN_POINT('Ctrl Pts',(-25.2511048108336,75.942444831426,17.2665675370673));
#259079=CARTESIAN_POINT('Ctrl Pts',(-25.253184996925,75.9421527879157,17.2649762469118));
#259080=CARTESIAN_POINT('Ctrl Pts',(-25.2552738568382,75.9418613633423,
17.2633930704885));
#259081=CARTESIAN_POINT('Ctrl Pts',(-25.2552738568382,75.9418613633423,
17.2633930704885));
#259082=CARTESIAN_POINT('Ctrl Pts',(-25.3053371640352,75.9348768553696,
17.2254493239264));
#259083=CARTESIAN_POINT('Ctrl Pts',(-25.35726443102,75.9291204561457,17.1911044093421));
#259084=CARTESIAN_POINT('Ctrl Pts',(-25.4106833642394,75.9248495156856,
17.1596330726701));
#259085=CARTESIAN_POINT('Ctrl Pts',(-25.4672813125568,75.9203244072107,
17.126288844714));
#259086=CARTESIAN_POINT('Ctrl Pts',(-25.5255536827334,75.9174669834034,
17.096170306179));
#259087=CARTESIAN_POINT('Ctrl Pts',(-25.5850314008785,75.9165875721633,
17.068359840973));
#259088=CARTESIAN_POINT('Ctrl Pts',(-25.6385673670598,75.9157960130403,
17.0433276075386));
#259089=CARTESIAN_POINT('Ctrl Pts',(-25.6930793577338,75.9166071705228,
17.0201642487191));
#259090=CARTESIAN_POINT('Ctrl Pts',(-25.748210005877,75.9192482118546,16.9981680569719));
#259091=CARTESIAN_POINT('Ctrl Pts',(-25.7703411800655,75.9203084088181,
16.9893380945566));
#259092=CARTESIAN_POINT('Ctrl Pts',(-25.7926041369582,75.9216656968463,
16.9807230186151));
#259093=CARTESIAN_POINT('Ctrl Pts',(-25.8149722051984,75.9233227318027,
16.9723142805604));
#259094=CARTESIAN_POINT('Ctrl Pts',(-25.8770418865484,75.9279208772763,
16.9489806745464));
#259095=CARTESIAN_POINT('Ctrl Pts',(-25.9395105597218,75.9347968299509,
16.9273736683177));
#259096=CARTESIAN_POINT('Ctrl Pts',(-26.0019469534467,75.943947744286,16.9071901218341));
#259097=CARTESIAN_POINT('Ctrl Pts',(-26.0680891141755,75.9536417898683,
16.8858086278695));
#259098=CARTESIAN_POINT('Ctrl Pts',(-26.134196625674,75.9658884088346,16.8660249930255));
#259099=CARTESIAN_POINT('Ctrl Pts',(-26.1997753179222,75.980727924121,16.8475110455998));
#259100=CARTESIAN_POINT('Ctrl Pts',(-26.2246632532517,75.9863597060933,
16.8404847705945));
#259101=CARTESIAN_POINT('Ctrl Pts',(-26.2494750754786,75.9923654080542,
16.8336416505));
#259102=CARTESIAN_POINT('Ctrl Pts',(-26.2741836399454,75.9987489542799,
16.8269646524032));
#259103=CARTESIAN_POINT('Ctrl Pts',(-26.3193781177628,76.0104251096745,
16.8147517436859));
#259104=CARTESIAN_POINT('Ctrl Pts',(-26.3644806571394,76.0233691010834,
16.8031325559241));
#259105=CARTESIAN_POINT('Ctrl Pts',(-26.4094030264466,76.037632391529,16.7919150704385));
#259106=CARTESIAN_POINT('Ctrl Pts',(-26.4723212964722,76.0576095559919,
16.7762038603737));
#259107=CARTESIAN_POINT('Ctrl Pts',(-26.5349890917676,76.0801913920499,
16.7613285556708));
#259108=CARTESIAN_POINT('Ctrl Pts',(-26.5968842675656,76.1054321152718,
16.7468658579898));
#259109=CARTESIAN_POINT('Ctrl Pts',(-26.6310436324481,76.1193622328184,
16.738884031282));
#259110=CARTESIAN_POINT('Ctrl Pts',(-26.6649677051668,76.1341013587548,
16.731027412246));
#259111=CARTESIAN_POINT('Ctrl Pts',(-26.6985700833499,76.1496523368464,
16.7232226781364));
#259112=CARTESIAN_POINT('Ctrl Pts',(-26.7271705546382,76.1628884625751,
16.7165797235039));
#259113=CARTESIAN_POINT('Ctrl Pts',(-26.7555332781428,76.1767336944032,
16.7099108269339));
#259114=CARTESIAN_POINT('Ctrl Pts',(-26.7835861577699,76.1911702984035,
16.7031950114971));
#259115=CARTESIAN_POINT('Ctrl Pts',(-26.8199494155057,76.2098835983951,
16.6944897045596));
#259116=CARTESIAN_POINT('Ctrl Pts',(-26.8556888227993,76.2295605848596,
16.6856585997866));
#259117=CARTESIAN_POINT('Ctrl Pts',(-26.8905185760864,76.250297808266,16.6759949661901));
#259118=CARTESIAN_POINT('Ctrl Pts',(-26.8948405181937,76.2528710415097,
16.6747958286422));
#259119=CARTESIAN_POINT('Ctrl Pts',(-26.8991484819158,76.2554605669536,
16.6735839233218));
#259120=CARTESIAN_POINT('Ctrl Pts',(-26.9034419462822,76.2580665404398,
16.6723579481277));
#259121=CARTESIAN_POINT('Ctrl Pts',(-26.9260412875341,76.2717835016351,
16.6659048302225));
#259122=CARTESIAN_POINT('Ctrl Pts',(-26.9482892120592,76.2859122477468,
16.6592804203713));
#259123=CARTESIAN_POINT('Ctrl Pts',(-26.9698831287204,76.3006663576261,
16.6513762614156));
#259124=CARTESIAN_POINT('Ctrl Pts',(-26.9780091206901,76.3062184665964,
16.6484018527796));
#259125=CARTESIAN_POINT('Ctrl Pts',(-26.9861262753852,76.3119191070937,
16.6452107769111));
#259126=CARTESIAN_POINT('Ctrl Pts',(-26.9940602893765,76.3176690332947,
16.6418055151727));
#259127=CARTESIAN_POINT('Ctrl Pts',(-27.0017405506363,76.3232350602132,
16.6385091635609));
#259128=CARTESIAN_POINT('Ctrl Pts',(-27.0092489771401,76.3288474175746,
16.6350110768171));
#259129=CARTESIAN_POINT('Ctrl Pts',(-27.0164426855061,76.3343994446543,
16.6313545921147));
#259130=CARTESIAN_POINT('Ctrl Pts',(-27.021651174773,76.338419300893,16.6287071729592));
#259131=CARTESIAN_POINT('Ctrl Pts',(-27.0266992715061,76.3424031609164,
16.6260035920946));
#259132=CARTESIAN_POINT('Ctrl Pts',(-27.0315171448137,76.3463237470274,
16.6231740179233));
#259133=CARTESIAN_POINT('Ctrl Pts',(-27.0359626225497,76.3499412930184,
16.6205631545447));
#259134=CARTESIAN_POINT('Ctrl Pts',(-27.0402121095371,76.3535049393509,
16.6178449700777));
#259135=CARTESIAN_POINT('Ctrl Pts',(-27.0442217699856,76.3569830238244,
16.6150107816619));
#259136=CARTESIAN_POINT('Ctrl Pts',(-27.0482190833947,76.3604503981526,
16.6121853206275));
#259137=CARTESIAN_POINT('Ctrl Pts',(-27.0519780380087,76.3638327354503,
16.6092444590309));
#259138=CARTESIAN_POINT('Ctrl Pts',(-27.0554667027077,76.3670881313929,
16.6062292715612));
#259139=CARTESIAN_POINT('Ctrl Pts',(-27.0590905972579,76.370469715074,16.6030972074673));
#259140=CARTESIAN_POINT('Ctrl Pts',(-27.0624228825075,76.3737142806329,
16.5998850454597));
#259141=CARTESIAN_POINT('Ctrl Pts',(-27.0654401101436,76.3767636720628,
16.5966933401164));
#259142=CARTESIAN_POINT('Ctrl Pts',(-27.0660776774096,76.377408035827,16.5960189041457));
#259143=CARTESIAN_POINT('Ctrl Pts',(-27.0667012169651,76.3780436486863,
16.595345561103));
#259144=CARTESIAN_POINT('Ctrl Pts',(-27.0673105683208,76.3786699073557,
16.5946745332907));
#259145=CARTESIAN_POINT('Ctrl Pts',(-27.0690899030251,76.3804986122136,
16.5927151004236));
#259146=CARTESIAN_POINT('Ctrl Pts',(-27.0707485686258,76.382246672755,16.5907819650672));
#259147=CARTESIAN_POINT('Ctrl Pts',(-27.0722790207717,76.383903674775,16.5888786970253));
#259148=CARTESIAN_POINT('Ctrl Pts',(-27.0747602936418,76.3865901188883,
16.5857929897265));
#259149=CARTESIAN_POINT('Ctrl Pts',(-27.0770747171622,76.3892195791676,
16.5825794792118));
#259150=CARTESIAN_POINT('Ctrl Pts',(-27.0792241302057,76.3918035041202,
16.579183461021));
#259151=CARTESIAN_POINT('Ctrl Pts',(-27.0816343568413,76.3947009671108,
16.5753753639578));
#259152=CARTESIAN_POINT('Ctrl Pts',(-27.083837184317,76.3975410826346,16.5713382492547));
#259153=CARTESIAN_POINT('Ctrl Pts',(-27.0858449599544,76.4003286356654,
16.5670618101874));
#259154=CARTESIAN_POINT('Ctrl Pts',(-27.0868914066365,76.4017815000024,
16.5648329428828));
#259155=CARTESIAN_POINT('Ctrl Pts',(-27.0878850109093,76.4032199187874,
16.5625400544833));
#259156=CARTESIAN_POINT('Ctrl Pts',(-27.088828258327,76.4046436978792,16.5601869061983));
#259157=CARTESIAN_POINT('Ctrl Pts',(-27.0901243112776,76.4066000171422,
16.5569536031214));
#259158=CARTESIAN_POINT('Ctrl Pts',(-27.0913240228374,76.4085291354499,
16.5536060959882));
#259159=CARTESIAN_POINT('Ctrl Pts',(-27.0924256391468,76.4104440957709,
16.5500691226174));
#259160=CARTESIAN_POINT('Ctrl Pts',(-27.0936398944198,76.4125548585178,
16.5461704979064));
#259161=CARTESIAN_POINT('Ctrl Pts',(-27.0947350208453,76.4146483529728,
16.5420420683693));
#259162=CARTESIAN_POINT('Ctrl Pts',(-27.0957153868087,76.41673174033,16.5376476148134));
#259163=CARTESIAN_POINT('Ctrl Pts',(-27.0962521678256,76.4178724600469,
16.5352415140951));
#259164=CARTESIAN_POINT('Ctrl Pts',(-27.0967546524525,76.4190099831835,
16.5327567087975));
#259165=CARTESIAN_POINT('Ctrl Pts',(-27.097224189991,76.4201444936685,16.5301935190525));
#259166=CARTESIAN_POINT('Ctrl Pts',(-27.0978315581571,76.4216120345913,
16.5268779165143));
#259167=CARTESIAN_POINT('Ctrl Pts',(-27.0983817182553,76.4230689216671,
16.5234806042216));
#259168=CARTESIAN_POINT('Ctrl Pts',(-27.0988766727596,76.4245289935568,
16.519898572385));
#259169=CARTESIAN_POINT('Ctrl Pts',(-27.0994168615817,76.4261225026722,
16.5159891755784));
#259170=CARTESIAN_POINT('Ctrl Pts',(-27.0998913101598,76.427719771351,16.5118599760785));
#259171=CARTESIAN_POINT('Ctrl Pts',(-27.1003044167921,76.4293303307267,
16.5074394314103));
#259172=CARTESIAN_POINT('Ctrl Pts',(-27.100765251422,76.4311269649994,16.5025081620798));
#259173=CARTESIAN_POINT('Ctrl Pts',(-27.1011497772522,76.4329400926505,
16.4972146293963));
#259174=CARTESIAN_POINT('Ctrl Pts',(-27.1014658921266,76.4347734700811,
16.4915299890183));
#259175=CARTESIAN_POINT('Ctrl Pts',(-27.1017737844554,76.4365591590576,
16.4859932132902));
#259176=CARTESIAN_POINT('Ctrl Pts',(-27.1020168306712,76.4383638507765,
16.4800869168181));
#259177=CARTESIAN_POINT('Ctrl Pts',(-27.1022032681051,76.4401848038024,
16.4738313146433));
#259178=CARTESIAN_POINT('Ctrl Pts',(-27.1022139466895,76.4402891026013,
16.4734730122689));
#259179=CARTESIAN_POINT('Ctrl Pts',(-27.1022244069632,76.4403934977004,
16.4731133135585));
#259180=CARTESIAN_POINT('Ctrl Pts',(-27.1022346589492,76.4404979871153,
16.4727522096321));
#259181=CARTESIAN_POINT('Ctrl Pts',(-27.1024069986673,76.4422544932462,
16.4666819176221));
#259182=CARTESIAN_POINT('Ctrl Pts',(-27.1025185266476,76.4439950489396,
16.4603561193072));
#259183=CARTESIAN_POINT('Ctrl Pts',(-27.1026104631992,76.4457036734619,
16.4538373780825));
#259184=CARTESIAN_POINT('Ctrl Pts',(-27.1027374245136,76.4480632269946,
16.4448352136609));
#259185=CARTESIAN_POINT('Ctrl Pts',(-27.1028277926133,76.4503610768553,
16.435469336288));
#259186=CARTESIAN_POINT('Ctrl Pts',(-27.1029292932191,76.4525659484553,
16.4259934752636));
#259187=CARTESIAN_POINT('Ctrl Pts',(-27.1029532014078,76.4530852998992,
16.4237614622497));
#259188=CARTESIAN_POINT('Ctrl Pts',(-27.1029775124212,76.4535995607684,
16.4215234223818));
#259189=CARTESIAN_POINT('Ctrl Pts',(-27.1030025070032,76.4541084537907,
16.4192826101514));
#259190=CARTESIAN_POINT('Ctrl Pts',(-27.103068131177,76.4554445707162,16.4133992770811));
#259191=CARTESIAN_POINT('Ctrl Pts',(-27.1031446836156,76.4567431107572,
16.407488679998));
#259192=CARTESIAN_POINT('Ctrl Pts',(-27.1032413598512,76.457990785983,16.4016557662627));
#259193=CARTESIAN_POINT('Ctrl Pts',(-27.1033489910739,76.4593798430705,
16.3951618886918));
#259194=CARTESIAN_POINT('Ctrl Pts',(-27.1034813058099,76.4607059855568,
16.3887641172962));
#259195=CARTESIAN_POINT('Ctrl Pts',(-27.1036407239054,76.4619636575372,
16.38254122392));
#259196=CARTESIAN_POINT('Ctrl Pts',(-27.1038110201107,76.4633071484696,
16.3758937029806));
#259197=CARTESIAN_POINT('Ctrl Pts',(-27.1040119022358,76.4645727430344,
16.3694450031958));
#259198=CARTESIAN_POINT('Ctrl Pts',(-27.1042403333882,76.4657643057464,
16.3632279271333));
#259199=CARTESIAN_POINT('Ctrl Pts',(-27.1044944223521,76.4670897069963,
16.3563125375353));
#259200=CARTESIAN_POINT('Ctrl Pts',(-27.1047822466638,76.4683237188364,
16.3496832466663));
#259201=CARTESIAN_POINT('Ctrl Pts',(-27.1050982636136,76.4694807293036,
16.3433192422796));
#259202=CARTESIAN_POINT('Ctrl Pts',(-27.1052628780315,76.4700834204082,
16.3400042084553));
#259203=CARTESIAN_POINT('Ctrl Pts',(-27.1054351585133,76.4706653371565,
16.3367601803189));
#259204=CARTESIAN_POINT('Ctrl Pts',(-27.1056146219711,76.4712290766849,
16.3335788780875));
#259205=CARTESIAN_POINT('Ctrl Pts',(-27.1059981692671,76.4724338945032,
16.3267798345215));
#259206=CARTESIAN_POINT('Ctrl Pts',(-27.10642271435,76.4735621730668,16.3202526040048));
#259207=CARTESIAN_POINT('Ctrl Pts',(-27.1068761114234,76.4746356726752,
16.3138840932371));
#259208=CARTESIAN_POINT('Ctrl Pts',(-27.1073854422856,76.4758416056492,
16.306729924693));
#259209=CARTESIAN_POINT('Ctrl Pts',(-27.1079312822812,76.476978936377,16.2997754603678));
#259210=CARTESIAN_POINT('Ctrl Pts',(-27.1085191991319,76.478083472477,16.292795783268));
#259211=CARTESIAN_POINT('Ctrl Pts',(-27.1088920682948,76.4787839923727,
16.2883691260731));
#259212=CARTESIAN_POINT('Ctrl Pts',(-27.1092822973043,76.4794713856191,
16.28393111298));
#259213=CARTESIAN_POINT('Ctrl Pts',(-27.1096950706557,76.4801541955039,
16.27941456206));
#259214=CARTESIAN_POINT('Ctrl Pts',(-27.1112272278191,76.4826886906515,
16.2626497543951));
#259215=CARTESIAN_POINT('Ctrl Pts',(-27.1130539358815,76.4851267428394,
16.245009294971));
#259216=CARTESIAN_POINT('Ctrl Pts',(-27.1151298371978,76.4873049803749,
16.2267575735314));
#259217=CARTESIAN_POINT('Ctrl Pts',(-27.1152747494852,76.487457036439,16.2254834769829));
#259218=CARTESIAN_POINT('Ctrl Pts',(-27.1154208703689,76.4876078216653,
16.2242064209797));
#259219=CARTESIAN_POINT('Ctrl Pts',(-27.1155681819217,76.4877572785791,
16.2229265037606));
#259220=CARTESIAN_POINT('Ctrl Pts',(-27.1170756224333,76.489286672591,16.2098290987628));
#259221=CARTESIAN_POINT('Ctrl Pts',(-27.118681039989,76.490635740581,16.1965814055142));
#259222=CARTESIAN_POINT('Ctrl Pts',(-27.120163955804,76.4917129471206,16.1843382179293));
#259223=CARTESIAN_POINT('Ctrl Pts',(-27.1209112681079,76.4922558030891,
16.1781682893142));
#259224=CARTESIAN_POINT('Ctrl Pts',(-27.1216272476248,76.4927295874375,
16.1722545210085));
#259225=CARTESIAN_POINT('Ctrl Pts',(-27.1222826948279,76.4931225564269,
16.1667491978235));
#259226=CARTESIAN_POINT('Ctrl Pts',(-27.123807760442,76.4940368993218,16.1539396548969));
#259227=CARTESIAN_POINT('Ctrl Pts',(-27.1250450068388,76.4945873611468,
16.1431164281593));
#259228=CARTESIAN_POINT('Ctrl Pts',(-27.1260737997838,76.4949373700034,
16.1336144198422));
#259229=CARTESIAN_POINT('Ctrl Pts',(-27.126352330216,76.4950321297104,16.1310418920111));
#259230=CARTESIAN_POINT('Ctrl Pts',(-27.1266156234859,76.4951122549698,
16.1285659022891));
#259231=CARTESIAN_POINT('Ctrl Pts',(-27.1268653349371,76.4951810931326,
16.1261726830171));
#259232=CARTESIAN_POINT('Ctrl Pts',(-27.1269115955426,76.4951938458321,
16.1257293242043));
#259233=CARTESIAN_POINT('Ctrl Pts',(-27.1269574092079,76.4952062290152,
16.1252887719971));
#259234=CARTESIAN_POINT('Ctrl Pts',(-27.1270027817488,76.4952182483286,
16.1248509868279));
#259235=CARTESIAN_POINT('Origin',(-29.6549915892152,76.7149512087496,20.0025));
#259236=CARTESIAN_POINT('Origin',(0.,0.,20.0025));
#259237=CARTESIAN_POINT('Origin',(-76.7149512087496,29.6549915892152,20.0025));
#259238=CARTESIAN_POINT('Ctrl Pts',(-74.3634602878982,28.7459974181806,
19.6929518677509));
#259239=CARTESIAN_POINT('Ctrl Pts',(-74.6189041648808,28.8447420032201,
17.4625));
#259240=CARTESIAN_POINT('Ctrl Pts',(-76.7149512087496,29.6549915892152,
17.4625));
#259241=CARTESIAN_POINT('Ctrl Pts',(-74.460904385774,28.4939177914733,19.6929518673245));
#259242=CARTESIAN_POINT('Ctrl Pts',(-74.6660793405586,28.6971725259743,
17.5374731486144));
#259243=CARTESIAN_POINT('Ctrl Pts',(-76.6890525018813,29.4834701335368,
17.4625));
#259244=CARTESIAN_POINT('Ctrl Pts',(-74.5588475342795,28.2438591531047,
19.6720320649351));
#259245=CARTESIAN_POINT('Ctrl Pts',(-74.7189440966779,28.5391636116357,
17.5981072780271));
#259246=CARTESIAN_POINT('Ctrl Pts',(-76.664038637903,29.3136797628422,17.4555267321203));
#259247=CARTESIAN_POINT('Ctrl Pts',(-74.7559270342231,27.7480012895958,
19.5871055664401));
#259248=CARTESIAN_POINT('Ctrl Pts',(-74.832738631376,28.2117119618056,17.6836912763772));
#259249=CARTESIAN_POINT('Ctrl Pts',(-76.6159646173276,28.9778332725242,
17.4272178998374));
#259250=CARTESIAN_POINT('Ctrl Pts',(-74.8560677628266,27.4997703917926,
19.5220948206219));
#259251=CARTESIAN_POINT('Ctrl Pts',(-74.8942448729349,28.0404430900653,
17.709632121869));
#259252=CARTESIAN_POINT('Ctrl Pts',(-76.5926880471475,28.8101355628242,
17.4055476509048));
#259253=CARTESIAN_POINT('Ctrl Pts',(-75.0518439197724,27.0236898937087,
19.3489695261644));
#259254=CARTESIAN_POINT('Ctrl Pts',(-75.019660969593,27.7022510777841,17.7211023712223));
#259255=CARTESIAN_POINT('Ctrl Pts',(-76.5500480485634,28.4896086814983,
17.3478392195236));
#259256=CARTESIAN_POINT('Ctrl Pts',(-75.1476280619453,26.7953551633978,
19.2413577159494));
#259257=CARTESIAN_POINT('Ctrl Pts',(-75.0836522525197,27.5347169152634,
17.7080778869115));
#259258=CARTESIAN_POINT('Ctrl Pts',(-76.5306138623673,28.3364379275071,
17.3119686156356));
#259259=CARTESIAN_POINT('Ctrl Pts',(-75.2884389844463,26.4687756770156,
19.0458961827322));
#259260=CARTESIAN_POINT('Ctrl Pts',(-75.1803896028198,27.2898012152202,
17.6578979817805));
#259261=CARTESIAN_POINT('Ctrl Pts',(-76.5048922024805,28.1185099510306,
17.2468147718757));
#259262=CARTESIAN_POINT('Ctrl Pts',(-75.3348967090533,26.3625884843546,
18.9750294801163));
#259263=CARTESIAN_POINT('Ctrl Pts',(-75.2125498005327,27.2097290601216,
17.636311693557));
#259264=CARTESIAN_POINT('Ctrl Pts',(-76.496894950715,28.0478532106478,17.223192537137));
#259265=CARTESIAN_POINT('Ctrl Pts',(-75.4268801209919,26.1560856941723,
18.8208466626385));
#259266=CARTESIAN_POINT('Ctrl Pts',(-75.2767579129783,27.0529295129818,
17.5825320214172));
#259267=CARTESIAN_POINT('Ctrl Pts',(-76.4822364493763,27.9109420608553,
17.1717982652807));
#259268=CARTESIAN_POINT('Ctrl Pts',(-75.4727198166015,26.0551010760532,
18.7368743964314));
#259269=CARTESIAN_POINT('Ctrl Pts',(-75.3090585336007,26.9755857935383,
17.5501254447862));
#259270=CARTESIAN_POINT('Ctrl Pts',(-76.4755364557142,27.8442489434605,
17.1438075095173));
#259271=CARTESIAN_POINT('Ctrl Pts',(-75.6060560547223,25.768150258085,18.4696518487109));
#259272=CARTESIAN_POINT('Ctrl Pts',(-75.4030488168829,26.7557364160525,
17.43860601751));
#259273=CARTESIAN_POINT('Ctrl Pts',(-76.4581861338663,27.655675609175,17.0547333270725));
#259274=CARTESIAN_POINT('Ctrl Pts',(-75.6894118596661,25.597846621004,18.271840936307));
#259275=CARTESIAN_POINT('Ctrl Pts',(-75.4628679834562,26.6226482272605,
17.3449978161568));
#259276=CARTESIAN_POINT('Ctrl Pts',(-76.4502012574515,27.5450423948284,
16.9887963557572));
#259277=CARTESIAN_POINT('Ctrl Pts',(-75.8449254994659,25.3042070746273,
17.8327278472486));
#259278=CARTESIAN_POINT('Ctrl Pts',(-75.5732964352841,26.3945070907105,
17.1202191600567));
#259279=CARTESIAN_POINT('Ctrl Pts',(-76.4429196593763,27.357895681027,16.8424253269274));
#259280=CARTESIAN_POINT('Ctrl Pts',(-75.9179115378165,25.1799509742042,
17.5873106315617));
#259281=CARTESIAN_POINT('Ctrl Pts',(-75.6248510373213,26.2977761963332,
16.986409166726));
#259282=CARTESIAN_POINT('Ctrl Pts',(-76.4437878571387,27.280900229958,16.7606195878717));
#259283=CARTESIAN_POINT('Ctrl Pts',(-76.0120135407797,25.0456540278871,
17.2025309630926));
#259284=CARTESIAN_POINT('Ctrl Pts',(-75.6888631781798,26.1964580005417,
16.7690050915928));
#259285=CARTESIAN_POINT('Ctrl Pts',(-76.4531141362198,27.20235213455,16.6323596984798));
#259286=CARTESIAN_POINT('Ctrl Pts',(-76.0410349984125,25.0090870943374,
17.0710669460341));
#259287=CARTESIAN_POINT('Ctrl Pts',(-75.7081633852753,26.1695156242373,
16.6936245453246));
#259288=CARTESIAN_POINT('Ctrl Pts',(-76.4575269782811,27.1820075724729,
16.5885383593541));
#259289=CARTESIAN_POINT('Ctrl Pts',(-76.0942893550638,24.9530103267675,
16.8014952531461));
#259290=CARTESIAN_POINT('Ctrl Pts',(-75.7423750031968,26.1301341325899,
16.5376305767305));
#259291=CARTESIAN_POINT('Ctrl Pts',(-76.4691181075119,27.1534935975719,
16.4986811285387));
#259292=CARTESIAN_POINT('Ctrl Pts',(-76.1186539510279,24.9335061597315,
16.6623540419172));
#259293=CARTESIAN_POINT('Ctrl Pts',(-75.7573877351404,26.1176802211128,
16.4562866616968));
#259294=CARTESIAN_POINT('Ctrl Pts',(-76.4763708127829,27.145369143006,16.4523007247637));
#259295=CARTESIAN_POINT('Ctrl Pts',(-76.1824010629023,24.9029553648545,
16.2463425041043));
#259296=CARTESIAN_POINT('Ctrl Pts',(-75.7942282194349,26.1038934519093,
16.2122544249952));
#259297=CARTESIAN_POINT('Ctrl Pts',(-76.5018384532016,27.1404954668508,
16.3136302120345));
#259298=CARTESIAN_POINT('Ctrl Pts',(-76.2131904009612,24.9185412707804,
15.9685880799941));
#259299=CARTESIAN_POINT('Ctrl Pts',(-75.8084359405768,26.1252772492191,
16.0475610164009));
#259300=CARTESIAN_POINT('Ctrl Pts',(-76.5237673449924,27.1624313528461,
16.2210111173636));
#259301=CARTESIAN_POINT('Ctrl Pts',(-76.2326069140442,24.9689556265491,
15.6905058513847));
#259302=CARTESIAN_POINT('Ctrl Pts',(-75.8121214408373,26.1756393943756,
15.8859547915793));
#259303=CARTESIAN_POINT('Ctrl Pts',(-76.55044485681,27.2087011009323,16.1283513278779));
#259304=CARTESIAN_POINT('',(-75.9418613629793,25.2552738567446,17.2633930704321));
#259305=CARTESIAN_POINT('Ctrl Pts',(-76.4952182372905,27.1270026655082,
16.124851038856));
#259306=CARTESIAN_POINT('Ctrl Pts',(-76.4949835330535,27.1261035938165,
16.1335301302463));
#259307=CARTESIAN_POINT('Ctrl Pts',(-76.4945938617306,27.1250175086504,
16.1433840167245));
#259308=CARTESIAN_POINT('Ctrl Pts',(-76.493894642641,27.1236651982624,16.1550166230773));
#259309=CARTESIAN_POINT('Ctrl Pts',(-76.493763071425,27.1234107356416,16.157205516638));
#259310=CARTESIAN_POINT('Ctrl Pts',(-76.4936205663265,27.1231468673314,
16.1594572469015));
#259311=CARTESIAN_POINT('Ctrl Pts',(-76.4934661405624,27.1228730977802,
16.1617756124903));
#259312=CARTESIAN_POINT('Ctrl Pts',(-76.4927426139016,27.1215904130517,
16.172637785155));
#259313=CARTESIAN_POINT('Ctrl Pts',(-76.4916920130616,27.1200357216268,
16.1853170892844));
#259314=CARTESIAN_POINT('Ctrl Pts',(-76.4903847974124,27.1184437830634,
16.1985845365741));
#259315=CARTESIAN_POINT('Ctrl Pts',(-76.4898045639396,27.1177371697041,
16.2044735549782));
#259316=CARTESIAN_POINT('Ctrl Pts',(-76.489173803305,27.1170231040088,16.2104789373784));
#259317=CARTESIAN_POINT('Ctrl Pts',(-76.4884987572068,27.1163213320438,
16.2164967943079));
#259318=CARTESIAN_POINT('Ctrl Pts',(-76.4866808484003,27.1144314500953,
16.2327029691722));
#259319=CARTESIAN_POINT('Ctrl Pts',(-76.4846005967038,27.1126943705542,
16.2486914456572));
#259320=CARTESIAN_POINT('Ctrl Pts',(-76.4824017848981,27.1111721910298,
16.2640972093943));
#259321=CARTESIAN_POINT('Ctrl Pts',(-76.4816221526855,27.1106324721747,
16.2695596276141));
#259322=CARTESIAN_POINT('Ctrl Pts',(-76.4808275267704,27.1101196624084,
16.2749492144108));
#259323=CARTESIAN_POINT('Ctrl Pts',(-76.480023958419,27.1096361423661,16.2802512670947));
#259324=CARTESIAN_POINT('Ctrl Pts',(-76.4787631770291,27.1088775098614,
16.288570073256));
#259325=CARTESIAN_POINT('Ctrl Pts',(-76.4774861247355,27.1081924682404,
16.2966391164402));
#259326=CARTESIAN_POINT('Ctrl Pts',(-76.4761760059689,27.1075731179885,
16.3046343846423));
#259327=CARTESIAN_POINT('Ctrl Pts',(-76.4750144099875,27.1070239809317,
16.3117232621168));
#259328=CARTESIAN_POINT('Ctrl Pts',(-76.4738263115708,27.1065264227128,
16.3187548885519));
#259329=CARTESIAN_POINT('Ctrl Pts',(-76.4726008566083,27.1060881023887,
16.3258128070736));
#259330=CARTESIAN_POINT('Ctrl Pts',(-76.472444168752,27.1060320583283,16.3267152393595));
#259331=CARTESIAN_POINT('Ctrl Pts',(-76.4722868770231,27.1059770032833,
16.3276180342357));
#259332=CARTESIAN_POINT('Ctrl Pts',(-76.4721289660909,27.1059229723691,
16.3285213027679));
#259333=CARTESIAN_POINT('Ctrl Pts',(-76.4709315855552,27.1055132758132,
16.3353704559211));
#259334=CARTESIAN_POINT('Ctrl Pts',(-76.469686098807,27.1051480063896,16.3423105850843));
#259335=CARTESIAN_POINT('Ctrl Pts',(-76.4683756379696,27.1048249982604,
16.3494047007367));
#259336=CARTESIAN_POINT('Ctrl Pts',(-76.4671537647784,27.1045238256025,
16.3560192514989));
#259337=CARTESIAN_POINT('Ctrl Pts',(-76.4658752319056,27.1042596511149,
16.3627681883368));
#259338=CARTESIAN_POINT('Ctrl Pts',(-76.4645307210492,27.1040326825547,
16.3696623273235));
#259339=CARTESIAN_POINT('Ctrl Pts',(-76.4632739316421,27.1038205223623,
16.3761066641678));
#259340=CARTESIAN_POINT('Ctrl Pts',(-76.4619593190125,27.1036411260684,
16.3826784026771));
#259341=CARTESIAN_POINT('Ctrl Pts',(-76.4605856089535,27.1034929209309,
16.3893426844209));
#259342=CARTESIAN_POINT('Ctrl Pts',(-76.4593337345535,27.1033578602487,
16.3954159046432));
#259343=CARTESIAN_POINT('Ctrl Pts',(-76.4580326598444,27.1032489151465,
16.4015662355659));
#259344=CARTESIAN_POINT('Ctrl Pts',(-76.4566888072063,27.1031602607469,
16.4077247900022));
#259345=CARTESIAN_POINT('Ctrl Pts',(-76.4561164335948,27.1031225010719,
16.4103478410302));
#259346=CARTESIAN_POINT('Ctrl Pts',(-76.455536406734,27.1030883438962,16.4129718046058));
#259347=CARTESIAN_POINT('Ctrl Pts',(-76.4549497809965,27.103056887902,16.4155884735518));
#259348=CARTESIAN_POINT('Ctrl Pts',(-76.4528297571289,27.102943208167,16.4250449297984));
#259349=CARTESIAN_POINT('Ctrl Pts',(-76.4506276154548,27.1028516325169,
16.4344055618506));
#259350=CARTESIAN_POINT('Ctrl Pts',(-76.4483618531535,27.1027493830599,
16.4434727015235));
#259351=CARTESIAN_POINT('Ctrl Pts',(-76.4479348993932,27.102730115465,16.4451812873606));
#259352=CARTESIAN_POINT('Ctrl Pts',(-76.4475057389425,27.1027103529401,
16.4468793703295));
#259353=CARTESIAN_POINT('Ctrl Pts',(-76.4470745680892,27.1026896905073,
16.4485655884618));
#259354=CARTESIAN_POINT('Ctrl Pts',(-76.4456191147842,27.102619942736,16.4542575589071));
#259355=CARTESIAN_POINT('Ctrl Pts',(-76.444132204062,27.1025406532752,16.4598473134608));
#259356=CARTESIAN_POINT('Ctrl Pts',(-76.4426004684769,27.1024250918524,
16.4653566991082));
#259357=CARTESIAN_POINT('Ctrl Pts',(-76.442018509056,27.1023811860638,16.4674499056068));
#259358=CARTESIAN_POINT('Ctrl Pts',(-76.4414302186229,27.1023318496948,
16.4695309610823));
#259359=CARTESIAN_POINT('Ctrl Pts',(-76.440835390871,27.1022746925433,16.4715995364411));
#259360=CARTESIAN_POINT('Ctrl Pts',(-76.4389925228595,27.1020976108826,
16.4780083015759));
#259361=CARTESIAN_POINT('Ctrl Pts',(-76.4370710585172,27.1018561048158,
16.4843917801182));
#259362=CARTESIAN_POINT('Ctrl Pts',(-76.4350620986708,27.1015158539172,
16.490654206125));
#259363=CARTESIAN_POINT('Ctrl Pts',(-76.4333518787998,27.1012261996222,
16.4959853855495));
#259364=CARTESIAN_POINT('Ctrl Pts',(-76.4315790441175,27.1008647151592,
16.5012232667733));
#259365=CARTESIAN_POINT('Ctrl Pts',(-76.4297403585947,27.1004038747172,
16.506308780426));
#259366=CARTESIAN_POINT('Ctrl Pts',(-76.4284489299112,27.1000801964384,
16.5098806681252));
#259367=CARTESIAN_POINT('Ctrl Pts',(-76.4271251515653,27.0997073598879,
16.5133767163734));
#259368=CARTESIAN_POINT('Ctrl Pts',(-76.4257650872438,27.0992746306612,
16.5168023194498));
#259369=CARTESIAN_POINT('Ctrl Pts',(-76.4244998564356,27.0988720744434,
16.5199890647238));
#259370=CARTESIAN_POINT('Ctrl Pts',(-76.4232033943541,27.0984176364795,
16.5231136244715));
#259371=CARTESIAN_POINT('Ctrl Pts',(-76.4218676567953,27.0979025055479,
16.5262197343051));
#259372=CARTESIAN_POINT('Ctrl Pts',(-76.4217789540767,27.097868297096,16.5264260026584));
#259373=CARTESIAN_POINT('Ctrl Pts',(-76.4216900756692,27.0978338210951,
16.5266322092073));
#259374=CARTESIAN_POINT('Ctrl Pts',(-76.4216010180799,27.0977990750252,
16.5268383756647));
#259375=CARTESIAN_POINT('Ctrl Pts',(-76.4212719492621,27.097670687897,16.5276001630987));
#259376=CARTESIAN_POINT('Ctrl Pts',(-76.4209404362573,27.0975386143432,
16.5283613866217));
#259377=CARTESIAN_POINT('Ctrl Pts',(-76.4206063221415,27.097402744855,16.5291232096001));
#259378=CARTESIAN_POINT('Ctrl Pts',(-76.4187176830246,27.096634718549,16.5334295486889));
#259379=CARTESIAN_POINT('Ctrl Pts',(-76.4167566024533,27.0957491893783,
16.5376614539927));
#259380=CARTESIAN_POINT('Ctrl Pts',(-76.4147290835877,27.0947257635391,
16.5417599887957));
#259381=CARTESIAN_POINT('Ctrl Pts',(-76.4130382200732,27.0938722704149,
16.5451779905115));
#259382=CARTESIAN_POINT('Ctrl Pts',(-76.411301229187,27.0929228022905,16.5485028098004));
#259383=CARTESIAN_POINT('Ctrl Pts',(-76.4095163162424,27.0918686181488,
16.551734836596));
#259384=CARTESIAN_POINT('Ctrl Pts',(-76.408055328314,27.0910057467635,16.5543803169521));
#259385=CARTESIAN_POINT('Ctrl Pts',(-76.4065622115707,27.0900727245997,
16.5569638004465));
#259386=CARTESIAN_POINT('Ctrl Pts',(-76.405031931884,27.0890672853599,16.5595114022451));
#259387=CARTESIAN_POINT('Ctrl Pts',(-76.4024133502076,27.0873467993646,
16.5638708036317));
#259388=CARTESIAN_POINT('Ctrl Pts',(-76.3996858222844,27.0854160305355,
16.5681213015784));
#259389=CARTESIAN_POINT('Ctrl Pts',(-76.3968549739135,27.0832453437873,
16.5722001453341));
#259390=CARTESIAN_POINT('Ctrl Pts',(-76.3944794420099,27.0814237924544,
16.5756229438037));
#259391=CARTESIAN_POINT('Ctrl Pts',(-76.3920312478068,27.0794332007694,
16.5789244111398));
#259392=CARTESIAN_POINT('Ctrl Pts',(-76.3895078513918,27.0772609129644,
16.5821034643185));
#259393=CARTESIAN_POINT('Ctrl Pts',(-76.3879086122879,27.0758841940382,
16.584118235413));
#259394=CARTESIAN_POINT('Ctrl Pts',(-76.3862790519647,27.0744345916997,
16.5860845447305));
#259395=CARTESIAN_POINT('Ctrl Pts',(-76.3846166914258,27.072910440065,16.5880130337724));
#259396=CARTESIAN_POINT('Ctrl Pts',(-76.3827359747379,27.0711860864444,
16.5901948357573));
#259397=CARTESIAN_POINT('Ctrl Pts',(-76.3808666413311,27.0694154757839,
16.5922669270639));
#259398=CARTESIAN_POINT('Ctrl Pts',(-76.3790011612993,27.06760552235,16.5942742310314));
#259399=CARTESIAN_POINT('Ctrl Pts',(-76.3740456584702,27.0627975216158,
16.5996064781317));
#259400=CARTESIAN_POINT('Ctrl Pts',(-76.3691274276531,27.0577058759388,
16.6044118919327));
#259401=CARTESIAN_POINT('Ctrl Pts',(-76.3642377230688,27.052350350697,16.6087783050469));
#259402=CARTESIAN_POINT('Ctrl Pts',(-76.3592796180193,27.0469199087783,
16.6132057984744));
#259403=CARTESIAN_POINT('Ctrl Pts',(-76.354350908567,27.0412180804687,16.6171815871709));
#259404=CARTESIAN_POINT('Ctrl Pts',(-76.3494322419893,27.0352768340187,
16.6208506593413));
#259405=CARTESIAN_POINT('Ctrl Pts',(-76.3445135754116,27.0293355875688,
16.6245197315117));
#259406=CARTESIAN_POINT('Ctrl Pts',(-76.3396049868132,27.0231548844613,
16.6278819111749));
#259407=CARTESIAN_POINT('Ctrl Pts',(-76.3346762337744,27.0167787754263,
16.63113891706));
#259408=CARTESIAN_POINT('Ctrl Pts',(-76.3270525622666,27.0069163699866,
16.6361767720248));
#259409=CARTESIAN_POINT('Ctrl Pts',(-76.3193994276104,26.9965742763337,
16.6408622418844));
#259410=CARTESIAN_POINT('Ctrl Pts',(-76.3117344496374,26.9857761531999,
16.6452464533241));
#259411=CARTESIAN_POINT('Ctrl Pts',(-76.307436760805,26.9797217361661,16.6477046438903));
#259412=CARTESIAN_POINT('Ctrl Pts',(-76.303135157655,26.9735241809127,16.6500689942482));
#259413=CARTESIAN_POINT('Ctrl Pts',(-76.2988312337081,26.9671894394036,
16.6523553297695));
#259414=CARTESIAN_POINT('Ctrl Pts',(-76.2848016950066,26.9465400268532,
16.6598081177547));
#259415=CARTESIAN_POINT('Ctrl Pts',(-76.2713420389528,26.925314640378,16.6661261478319));
#259416=CARTESIAN_POINT('Ctrl Pts',(-76.2582666976199,26.9037854166563,
16.6722817468537));
#259417=CARTESIAN_POINT('Ctrl Pts',(-76.236716649198,26.8683021507223,16.6824270618866));
#259418=CARTESIAN_POINT('Ctrl Pts',(-76.2163231724805,26.8318654948446,
16.6915805494573));
#259419=CARTESIAN_POINT('Ctrl Pts',(-76.1969868424568,26.7948177268109,
16.7005093017872));
#259420=CARTESIAN_POINT('Ctrl Pts',(-76.1951008482725,26.7912042244055,
16.7013801792984));
#259421=CARTESIAN_POINT('Ctrl Pts',(-76.1932248857391,26.7875849267988,
16.7022489427234));
#259422=CARTESIAN_POINT('Ctrl Pts',(-76.1913588468482,26.7839601625929,
16.7031163158074));
#259423=CARTESIAN_POINT('Ctrl Pts',(-76.176568027518,26.7552291255579,16.7099913914772));
#259424=CARTESIAN_POINT('Ctrl Pts',(-76.162413994639,26.7262008738672,16.716810696067));
#259425=CARTESIAN_POINT('Ctrl Pts',(-76.1489165164747,26.6969732854461,
16.7235973395649));
#259426=CARTESIAN_POINT('Ctrl Pts',(-76.1236619610359,26.6422867919294,
16.7362955386192));
#259427=CARTESIAN_POINT('Ctrl Pts',(-76.1005180681828,26.5866819738269,
16.7491519989587));
#259428=CARTESIAN_POINT('Ctrl Pts',(-76.0794074083773,26.5302810836964,
16.7625435720843));
#259429=CARTESIAN_POINT('Ctrl Pts',(-76.064362927453,26.4900870715955,16.7720870571431));
#259430=CARTESIAN_POINT('Ctrl Pts',(-76.0503521064293,26.4494883805208,
16.7819023270087));
#259431=CARTESIAN_POINT('Ctrl Pts',(-76.0373611942068,26.4085292238121,
16.7921336012861));
#259432=CARTESIAN_POINT('Ctrl Pts',(-76.023172012212,26.3637920322323,16.8033085988748));
#259433=CARTESIAN_POINT('Ctrl Pts',(-76.010338419258,26.3190310002086,16.8148454077145));
#259434=CARTESIAN_POINT('Ctrl Pts',(-75.9987850456331,26.2743222514891,
16.8269262467475));
#259435=CARTESIAN_POINT('Ctrl Pts',(-75.9837486849446,26.2161351891203,
16.8426490874534));
#259436=CARTESIAN_POINT('Ctrl Pts',(-75.9708594776013,26.157598960004,16.8592311067997));
#259437=CARTESIAN_POINT('Ctrl Pts',(-75.9600230530903,26.0990044705617,
16.8768965952961));
#259438=CARTESIAN_POINT('Ctrl Pts',(-75.9491979291169,26.0404710851514,
16.8945436617091));
#259439=CARTESIAN_POINT('Ctrl Pts',(-75.94042141172,25.9818779784671,16.9132712882918));
#259440=CARTESIAN_POINT('Ctrl Pts',(-75.9336439588965,25.9235033739726,
16.9333228296636));
#259441=CARTESIAN_POINT('Ctrl Pts',(-75.9294790509155,25.8876307736792,
16.9456449847365));
#259442=CARTESIAN_POINT('Ctrl Pts',(-75.9260699331751,25.8518405543353,
16.9584675280565));
#259443=CARTESIAN_POINT('Ctrl Pts',(-75.9234132458688,25.8161989867003,
16.971852276588));
#259444=CARTESIAN_POINT('Ctrl Pts',(-75.9217239577779,25.793535846931,16.9803631375538));
#259445=CARTESIAN_POINT('Ctrl Pts',(-75.9203357066719,25.7708904059779,
16.9891192993509));
#259446=CARTESIAN_POINT('Ctrl Pts',(-75.9192531417279,25.748310663338,16.9981274246436));
#259447=CARTESIAN_POINT('Ctrl Pts',(-75.9170297815819,25.7019366326876,
17.016628214714));
#259448=CARTESIAN_POINT('Ctrl Pts',(-75.9160908878986,25.6557154302892,
17.0360687209549));
#259449=CARTESIAN_POINT('Ctrl Pts',(-75.9163356254785,25.6100335195781,
17.056834669541));
#259450=CARTESIAN_POINT('Ctrl Pts',(-75.91656211733,25.567757296436,17.0760524706907));
#259451=CARTESIAN_POINT('Ctrl Pts',(-75.9178014945773,25.5259435976778,
17.0964068031176));
#259452=CARTESIAN_POINT('Ctrl Pts',(-75.9199460216587,25.4848871401385,
17.1181763515212));
#259453=CARTESIAN_POINT('Ctrl Pts',(-75.922037669005,25.4448430524687,17.1394091065384));
#259454=CARTESIAN_POINT('Ctrl Pts',(-75.9249898990629,25.4055198685136,
17.1619892999248));
#259455=CARTESIAN_POINT('Ctrl Pts',(-75.9286842189327,25.3671710060197,
17.1861307296247));
#259456=CARTESIAN_POINT('Ctrl Pts',(-75.9320094343406,25.3326536299033,
17.2078601566467));
#259457=CARTESIAN_POINT('Ctrl Pts',(-75.9359354287002,25.298925635765,17.2308544606032));
#259458=CARTESIAN_POINT('Ctrl Pts',(-75.9403670676492,25.2661521618397,
17.2552262518704));
#259459=CARTESIAN_POINT('Ctrl Pts',(-75.9408589869714,25.2625142515169,
17.2579315613911));
#259460=CARTESIAN_POINT('Ctrl Pts',(-75.9413571303343,25.2588880802128,
17.2606537952903));
#259461=CARTESIAN_POINT('Ctrl Pts',(-75.9418613633423,25.2552738568381,
17.2633930704886));
#259462=CARTESIAN_POINT('Ctrl Pts',(-75.9418613633423,25.2552738568381,
17.2633930704886));
#259463=CARTESIAN_POINT('Ctrl Pts',(-75.9442259477114,25.2383250956303,
17.2762387759409));
#259464=CARTESIAN_POINT('Ctrl Pts',(-75.9466297979243,25.221950107767,17.2896217175501));
#259465=CARTESIAN_POINT('Ctrl Pts',(-75.9489416166353,25.2063620810916,
17.3037656230845));
#259466=CARTESIAN_POINT('Ctrl Pts',(-75.9512774695206,25.1906119978725,
17.3180565717624));
#259467=CARTESIAN_POINT('Ctrl Pts',(-75.9535194008088,25.1756652592871,
17.3331243152708));
#259468=CARTESIAN_POINT('Ctrl Pts',(-75.9555501185693,25.1617083526887,
17.3491621095395));
#259469=CARTESIAN_POINT('Ctrl Pts',(-75.9576114325003,25.147541161873,17.36544154009));
#259470=CARTESIAN_POINT('Ctrl Pts',(-75.9594551435701,25.1343938087813,
17.3827204196343));
#259471=CARTESIAN_POINT('Ctrl Pts',(-75.9609767647043,25.1224278850708,
17.401163330919));
#259472=CARTESIAN_POINT('Ctrl Pts',(-75.9611515135672,25.1210536720588,
17.4032813862633));
#259473=CARTESIAN_POINT('Ctrl Pts',(-75.9613220335549,25.1196950057595,
17.4054147545603));
#259474=CARTESIAN_POINT('Ctrl Pts',(-75.9614881812303,25.1183521036896,
17.4075636545403));
#259475=CARTESIAN_POINT('Ctrl Pts',(10.8641498708349,79.2111064053766,17.847987692667));
#259476=CARTESIAN_POINT('Ctrl Pts',(9.7654340370314,79.359520501561,17.8663812527205));
#259477=CARTESIAN_POINT('Ctrl Pts',(9.7654340370314,80.4599485582789,18.0027617587916));
#259478=CARTESIAN_POINT('Ctrl Pts',(10.8621713328006,78.2644852096539,25.4882815344998));
#259479=CARTESIAN_POINT('Ctrl Pts',(9.76543403703139,78.415025968742,25.5016215881557));
#259480=CARTESIAN_POINT('Ctrl Pts',(9.7654340370314,79.5130559971843,25.6430556014337));
#259481=CARTESIAN_POINT('Ctrl Pts',(10.8601243292931,77.317574634656,33.1285376594865));
#259482=CARTESIAN_POINT('Ctrl Pts',(9.76543403703139,77.4696829514656,33.1417037687789));
#259483=CARTESIAN_POINT('Ctrl Pts',(9.7654340370314,78.5658598958838,33.2833117264721));
#259484=CARTESIAN_POINT('Ctrl Pts',(10.858001215061,76.370342253395,40.7687517688986));
#259485=CARTESIAN_POINT('Ctrl Pts',(9.7654340370314,76.5233256693937,40.7877246696809));
#259486=CARTESIAN_POINT('Ctrl Pts',(9.7654340370314,77.6183256595919,40.9235258350231));
#259487=CARTESIAN_POINT('Ctrl Pts',(9.7654340370314,77.6928637726221,40.3225));
#259488=CARTESIAN_POINT('Ctrl Pts',(9.7654340370314,77.6406907450683,40.3348699258231));
#259489=CARTESIAN_POINT('Ctrl Pts',(9.7683743292685,77.5889301320358,40.347142091233));
#259490=CARTESIAN_POINT('Ctrl Pts',(9.77421593702744,77.5376245532549,40.3593064230311));
#259491=CARTESIAN_POINT('Ctrl Pts',(9.7800356824703,77.4865109864726,40.3714252296113));
#259492=CARTESIAN_POINT('Ctrl Pts',(9.78873516574705,77.4358485949097,40.3834371171633));
#259493=CARTESIAN_POINT('Ctrl Pts',(9.80032672757758,77.3856866947242,40.3953304235289));
#259494=CARTESIAN_POINT('Ctrl Pts',(9.81145263908703,77.3375398728577,40.4067459580457));
#259495=CARTESIAN_POINT('Ctrl Pts',(9.82524326664853,77.2898538147198,40.4180523240903));
#259496=CARTESIAN_POINT('Ctrl Pts',(9.84175291335836,77.2426843219429,40.4292363172717));
#259497=CARTESIAN_POINT('Ctrl Pts',(9.84292121245742,77.2393463900729,40.4300277484506));
#259498=CARTESIAN_POINT('Ctrl Pts',(9.84410288781287,77.236011786251,40.4308183913332));
#259499=CARTESIAN_POINT('Ctrl Pts',(9.84529794460256,77.2326805409166,40.4316082386352));
#259500=CARTESIAN_POINT('Ctrl Pts',(9.86516996289905,77.1772868819652,40.4447422253815));
#259501=CARTESIAN_POINT('Ctrl Pts',(9.88842098537268,77.1237590602342,40.4574340218528));
#259502=CARTESIAN_POINT('Ctrl Pts',(9.91505186507416,77.0719801851636,40.4697110373831));
#259503=CARTESIAN_POINT('Ctrl Pts',(9.92388396091018,77.0548077901083,40.4737826932563));
#259504=CARTESIAN_POINT('Ctrl Pts',(9.93308817911335,77.0378279739812,40.4778086771577));
#259505=CARTESIAN_POINT('Ctrl Pts',(9.94266563537454,77.0210370924819,40.4817898423615));
#259506=CARTESIAN_POINT('Ctrl Pts',(9.96873208562553,76.9753382487247,40.4926251666788));
#259507=CARTESIAN_POINT('Ctrl Pts',(9.99776047110971,76.9308062595847,40.50318366357));
#259508=CARTESIAN_POINT('Ctrl Pts',(10.0295120097993,76.8880200231596,40.5133278667756));
#259509=CARTESIAN_POINT('Ctrl Pts',(10.0411035752289,76.8724000097847,40.5170312210079));
#259510=CARTESIAN_POINT('Ctrl Pts',(10.0530582321017,76.8570131032765,40.5206792556205));
#259511=CARTESIAN_POINT('Ctrl Pts',(10.0653648162887,76.8418891614267,40.5242648814378));
#259512=CARTESIAN_POINT('Ctrl Pts',(10.068651836502,76.8378496406458,40.525222582158));
#259513=CARTESIAN_POINT('Ctrl Pts',(10.0719632027711,76.8338298192818,40.5261756223058));
#259514=CARTESIAN_POINT('Ctrl Pts',(10.0752986447752,76.8298302814747,40.5271238626224));
#259515=CARTESIAN_POINT('Ctrl Pts',(10.1248353857937,76.7704306371993,40.541206774251));
#259516=CARTESIAN_POINT('Ctrl Pts',(10.1790585260117,76.7160472771173,40.5541023854872));
#259517=CARTESIAN_POINT('Ctrl Pts',(10.2380522716906,76.6666407817785,40.5658176329226));
#259518=CARTESIAN_POINT('Ctrl Pts',(10.2796785900014,76.6317792811579,40.574083977316));
#259519=CARTESIAN_POINT('Ctrl Pts',(10.3240382810484,76.5992118758775,40.5818062215632));
#259520=CARTESIAN_POINT('Ctrl Pts',(10.3703731787742,76.5696242835505,40.5888209763611));
#259521=CARTESIAN_POINT('Ctrl Pts',(10.3857677071117,76.5597939601685,40.5911515920918));
#259522=CARTESIAN_POINT('Ctrl Pts',(10.4013800550833,76.5502929101763,40.5934040296095));
#259523=CARTESIAN_POINT('Ctrl Pts',(10.4171817032987,76.5411473570588,40.5955720423396));
#259524=CARTESIAN_POINT('Ctrl Pts',(10.4205823443447,76.5391791609,40.5960386160146));
#259525=CARTESIAN_POINT('Ctrl Pts',(10.4239920323319,76.5372272679841,40.5965013264119));
#259526=CARTESIAN_POINT('Ctrl Pts',(10.427410423321,76.5352919854596,40.596960100647));
#259527=CARTESIAN_POINT('Ctrl Pts',(10.4699717833534,76.5111963637033,40.6026721609271));
#259528=CARTESIAN_POINT('Ctrl Pts',(10.5138127373806,76.4895921179992,40.6077938499824));
#259529=CARTESIAN_POINT('Ctrl Pts',(10.5587950181376,76.4706502604835,40.6122845088192));
#259530=CARTESIAN_POINT('Ctrl Pts',(10.603385198479,76.4518735148759,40.6167360235937));
#259531=CARTESIAN_POINT('Ctrl Pts',(10.649096703806,76.4357131151363,40.6205674210037));
#259532=CARTESIAN_POINT('Ctrl Pts',(10.6957749766315,76.4222898455887,40.6237499580585));
#259533=CARTESIAN_POINT('Ctrl Pts',(10.741990927449,76.4089995259674,40.6269009738759));
#259534=CARTESIAN_POINT('Ctrl Pts',(10.7891543927876,76.3983925009905,40.6294158916108));
#259535=CARTESIAN_POINT('Ctrl Pts',(10.8370986845467,76.3905388100093,40.6312780057494));
#259536=CARTESIAN_POINT('Ctrl Pts',(10.8440625860396,76.3893980625222,40.6315484775606));
#259537=CARTESIAN_POINT('Ctrl Pts',(10.8510429350674,76.3883153199295,40.6318051966655));
#259538=CARTESIAN_POINT('Ctrl Pts',(10.8580391950581,76.3872907109282,40.6320481322491));
#259539=CARTESIAN_POINT('Origin',(11.0354340370314,80.4599485582789,18.0027617587916));
#259540=CARTESIAN_POINT('Ctrl Pts',(10.8629841634368,79.2590409673554,17.0741173620444));
#259541=CARTESIAN_POINT('Ctrl Pts',(9.76543403703139,79.4094675874129,17.0741173620444));
#259542=CARTESIAN_POINT('Ctrl Pts',(9.7654340370314,80.5172782427122,17.0741173620444));
#259543=CARTESIAN_POINT('Ctrl Pts',(10.8629841634028,79.2590409673601,17.3330517996227));
#259544=CARTESIAN_POINT('Ctrl Pts',(9.7654340370314,79.4094675877083,17.3392431182821));
#259545=CARTESIAN_POINT('Ctrl Pts',(9.7654340370314,80.5172782429666,17.3848387320851));
#259546=CARTESIAN_POINT('Ctrl Pts',(10.8633722599807,79.2430601863238,17.5910193441541));
#259547=CARTESIAN_POINT('Ctrl Pts',(9.7654340370314,79.392803294839,17.6034496884161));
#259548=CARTESIAN_POINT('Ctrl Pts',(9.7654340370314,80.4981651198115,17.6943996807311));
#259549=CARTESIAN_POINT('Ctrl Pts',(10.8641498708349,79.2111064053766,17.847987692667));
#259550=CARTESIAN_POINT('Ctrl Pts',(9.7654340370314,79.359520501561,17.8663812527205));
#259551=CARTESIAN_POINT('Ctrl Pts',(9.7654340370314,80.4599485582789,18.0027617587916));
#259552=CARTESIAN_POINT('Origin',(11.0354340370314,80.5172782427122,17.0741173620444));
#259553=CARTESIAN_POINT('Origin',(11.0354340370314,80.5172782427122,12.3825));
#259554=CARTESIAN_POINT('Ctrl Pts',(9.93397247946587,79.8850738159598,12.3824999999994));
#259555=CARTESIAN_POINT('Ctrl Pts',(9.87891393978383,79.9809998523955,12.3824999342017));
#259556=CARTESIAN_POINT('Ctrl Pts',(9.83665735537327,80.0836518503505,12.3772814134038));
#259557=CARTESIAN_POINT('Ctrl Pts',(9.77984203925996,80.2969364364516,12.3639187544469));
#259558=CARTESIAN_POINT('Ctrl Pts',(9.76543403689542,80.4068623726219,12.3558758059475));
#259559=CARTESIAN_POINT('Ctrl Pts',(9.76543403703139,80.5172782442762,12.3495568919806));
#259560=CARTESIAN_POINT('Ctrl Pts',(-9.76543403703141,80.4599485582789,
18.0027617587917));
#259561=CARTESIAN_POINT('Ctrl Pts',(-9.76543403703142,79.359520501561,17.8663812527206));
#259562=CARTESIAN_POINT('Ctrl Pts',(-10.8641498708349,79.2111064053766,
17.8479876926672));
#259563=CARTESIAN_POINT('Ctrl Pts',(-9.76543403703141,79.5130559971301,
25.6430556014271));
#259564=CARTESIAN_POINT('Ctrl Pts',(-9.76543403713151,78.4150259686878,
25.5016215881491));
#259565=CARTESIAN_POINT('Ctrl Pts',(-10.86217133288,78.2644852096432,25.4882815344986));
#259566=CARTESIAN_POINT('Ctrl Pts',(-9.76543403703142,78.5658598956831,
33.2833117264472));
#259567=CARTESIAN_POINT('Ctrl Pts',(-9.76543403703142,77.4696829512648,
33.1417037687541));
#259568=CARTESIAN_POINT('Ctrl Pts',(-10.8601243293212,77.3175746346521,
33.1285376594861));
#259569=CARTESIAN_POINT('Ctrl Pts',(-9.76543403703142,77.6183256595919,
40.9235258350231));
#259570=CARTESIAN_POINT('Ctrl Pts',(-9.76543403703142,76.5233256693937,
40.7877246696809));
#259571=CARTESIAN_POINT('Ctrl Pts',(-10.8580012150611,76.370342253395,40.7687517688986));
#259572=CARTESIAN_POINT('Ctrl Pts',(-10.8580391950582,76.3872907109282,
40.6320481322491));
#259573=CARTESIAN_POINT('Ctrl Pts',(-10.8038338229833,76.3952291394678,
40.6301659271477));
#259574=CARTESIAN_POINT('Ctrl Pts',(-10.7506894857011,76.4066910151546,
40.6274486565634));
#259575=CARTESIAN_POINT('Ctrl Pts',(-10.6987376202637,76.421510168725,40.6239354244084));
#259576=CARTESIAN_POINT('Ctrl Pts',(-10.6458391128062,76.4365993498172,
40.620358175819));
#259577=CARTESIAN_POINT('Ctrl Pts',(-10.594176367347,76.4551693794646,40.6159556693214));
#259578=CARTESIAN_POINT('Ctrl Pts',(-10.5438898994474,76.4770976611215,
40.6107566553931));
#259579=CARTESIAN_POINT('Ctrl Pts',(-10.5042776831975,76.4943712512395,
40.6066612302695));
#259580=CARTESIAN_POINT('Ctrl Pts',(-10.4655194169616,76.5137297868398,
40.6020712995237));
#259581=CARTESIAN_POINT('Ctrl Pts',(-10.4276880145587,76.5351350735785,
40.5969957588345));
#259582=CARTESIAN_POINT('Ctrl Pts',(-10.4242613480823,76.5370739067654,
40.5965360300371));
#259583=CARTESIAN_POINT('Ctrl Pts',(-10.4208458708561,76.5390275045006,
40.5960727978901));
#259584=CARTESIAN_POINT('Ctrl Pts',(-10.417441529947,76.5409958524294,40.5956060656757));
#259585=CARTESIAN_POINT('Ctrl Pts',(-10.3539733392929,76.5776923775294,
40.5869046312546));
#259586=CARTESIAN_POINT('Ctrl Pts',(-10.2946065930604,76.6193798556825,
40.5770207119274));
#259587=CARTESIAN_POINT('Ctrl Pts',(-10.2391051819928,76.6657602207944,
40.5660242594495));
#259588=CARTESIAN_POINT('Ctrl Pts',(-10.1944993133031,76.7030356059813,
40.5571865325189));
#259589=CARTESIAN_POINT('Ctrl Pts',(-10.1521266719203,76.7436824784756,
40.5475495232825));
#259590=CARTESIAN_POINT('Ctrl Pts',(-10.112768827324,76.7868622699144,40.5373116645919));
#259591=CARTESIAN_POINT('Ctrl Pts',(-10.1000103154398,76.8008597305954,
40.5339928893106));
#259592=CARTESIAN_POINT('Ctrl Pts',(-10.0875683378583,76.8151236613885,
40.5306109028825));
#259593=CARTESIAN_POINT('Ctrl Pts',(-10.0754687483719,76.8296263455661,
40.5271722631609));
#259594=CARTESIAN_POINT('Ctrl Pts',(-10.0721400686965,76.8336161329977,
40.5262262698968));
#259595=CARTESIAN_POINT('Ctrl Pts',(-10.0688379426855,76.8376221197981,
40.5252764323596));
#259596=CARTESIAN_POINT('Ctrl Pts',(-10.0655622810809,76.8416442509437,
40.5243227633055));
#259597=CARTESIAN_POINT('Ctrl Pts',(-10.0197772889645,76.8978628916408,
40.5109930194578));
#259598=CARTESIAN_POINT('Ctrl Pts',(-9.97910469542405,76.9573064495693,
40.4968987634144));
#259599=CARTESIAN_POINT('Ctrl Pts',(-9.94335294128108,77.0198338045965,
40.4820734444561));
#259600=CARTESIAN_POINT('Ctrl Pts',(-9.91378625397024,77.0715439038288,
40.4698129112198));
#259601=CARTESIAN_POINT('Ctrl Pts',(-9.88745885424494,77.1258101444836,
40.4569463905791));
#259602=CARTESIAN_POINT('Ctrl Pts',(-9.8649496492485,77.1812643278188,40.4437982715083));
#259603=CARTESIAN_POINT('Ctrl Pts',(-9.85807764537128,77.1981943510226,
40.4397841837052));
#259604=CARTESIAN_POINT('Ctrl Pts',(-9.85156135507736,77.2152354151264,
40.4357437739529));
#259605=CARTESIAN_POINT('Ctrl Pts',(-9.84541680798104,77.2323494285094,
40.431686073453));
#259606=CARTESIAN_POINT('Ctrl Pts',(-9.81300496672525,77.3226240535266,
40.4102821290442));
#259607=CARTESIAN_POINT('Ctrl Pts',(-9.79038099604269,77.4153316528972,
40.3883014811186));
#259608=CARTESIAN_POINT('Ctrl Pts',(-9.7776621016632,77.5097070805337,40.3659254999368));
#259609=CARTESIAN_POINT('Ctrl Pts',(-9.7695177379922,77.5701390474441,40.3515973576626));
#259610=CARTESIAN_POINT('Ctrl Pts',(-9.76543403703142,77.6312555924454,
40.3371069464355));
#259611=CARTESIAN_POINT('Ctrl Pts',(-9.76543403703142,77.6928637726221,
40.3225000000001));
#259612=CARTESIAN_POINT('Origin',(-11.0354340370314,80.4599485582789,18.0027617587917));
#259613=CARTESIAN_POINT('Ctrl Pts',(-9.76543403703142,80.5172782427122,
17.0741173620445));
#259614=CARTESIAN_POINT('Ctrl Pts',(-9.76543403703142,79.4094675874129,
17.0741173620445));
#259615=CARTESIAN_POINT('Ctrl Pts',(-10.8629841634369,79.2590409673554,
17.0741173620445));
#259616=CARTESIAN_POINT('Ctrl Pts',(-9.76543403703142,80.5172782429666,
17.3848387320852));
#259617=CARTESIAN_POINT('Ctrl Pts',(-9.76543403703142,79.4094675877083,
17.3392431182822));
#259618=CARTESIAN_POINT('Ctrl Pts',(-10.8629841634031,79.25904096736,17.3330517996228));
#259619=CARTESIAN_POINT('Ctrl Pts',(-9.76543403703142,80.4981651198115,
17.6943996807312));
#259620=CARTESIAN_POINT('Ctrl Pts',(-9.76543403703142,79.392803294839,17.6034496884162));
#259621=CARTESIAN_POINT('Ctrl Pts',(-10.8633722599797,79.2430601863239,
17.5910193441543));
#259622=CARTESIAN_POINT('Ctrl Pts',(-9.76543403703142,80.4599485582789,
18.0027617587917));
#259623=CARTESIAN_POINT('Ctrl Pts',(-9.76543403703142,79.359520501561,17.8663812527206));
#259624=CARTESIAN_POINT('Ctrl Pts',(-10.8641498708349,79.2111064053766,
17.8479876926671));
#259625=CARTESIAN_POINT('Origin',(-11.0354340370314,80.5172782427121,17.0741173620445));
#259626=CARTESIAN_POINT('Origin',(-11.0354340370314,80.5172782427122,12.3825));
#259627=CARTESIAN_POINT('Ctrl Pts',(-9.76543403703142,80.5172782442762,
12.3495568919838));
#259628=CARTESIAN_POINT('Ctrl Pts',(-9.76543403689582,80.407164861761,12.3558584950094));
#259629=CARTESIAN_POINT('Ctrl Pts',(-9.77976311228818,80.2975378399709,
12.363874307156));
#259630=CARTESIAN_POINT('Ctrl Pts',(-9.83642681214443,80.0842125738188,
12.3772530427028));
#259631=CARTESIAN_POINT('Ctrl Pts',(-9.87876331331359,79.9812622821722,
12.3824999340235));
#259632=CARTESIAN_POINT('Ctrl Pts',(-9.93397247946588,79.8850738159598,
12.3824999999994));
#259633=CARTESIAN_POINT('Ctrl Pts',(19.6282160049318,113.33109747126,12.2312547539759));
#259634=CARTESIAN_POINT('Ctrl Pts',(19.968791267623,113.225505581264,12.3825000000002));
#259635=CARTESIAN_POINT('Ctrl Pts',(20.3387380182653,113.110807356014,12.3825));
#259636=CARTESIAN_POINT('Ctrl Pts',(17.9262673743939,107.744499663662,12.2434569899102));
#259637=CARTESIAN_POINT('Ctrl Pts',(18.257711262191,107.651751796601,12.3824999999443));
#259638=CARTESIAN_POINT('Ctrl Pts',(18.6092072977809,107.532395334702,12.3825));
#259639=CARTESIAN_POINT('Ctrl Pts',(16.2272244965966,102.15710346924,12.2580230532609));
#259640=CARTESIAN_POINT('Ctrl Pts',(16.5451782447696,102.073466334938,12.3824999999848));
#259641=CARTESIAN_POINT('Ctrl Pts',(16.8761662824142,101.955067506485,12.3825));
#259642=CARTESIAN_POINT('Ctrl Pts',(12.847024800685,90.9828768181336,12.2950955201719));
#259643=CARTESIAN_POINT('Ctrl Pts',(13.1184592484314,90.9129457862284,12.3825000000151));
#259644=CARTESIAN_POINT('Ctrl Pts',(13.3939133181762,90.811238296817,12.3825));
#259645=CARTESIAN_POINT('Ctrl Pts',(11.1637373488142,85.3967648634315,12.3186057573121));
#259646=CARTESIAN_POINT('Ctrl Pts',(11.4074622813581,85.3412573398049,12.382499999807));
#259647=CARTESIAN_POINT('Ctrl Pts',(11.6464930192604,85.2441534264155,12.3825));
#259648=CARTESIAN_POINT('Ctrl Pts',(9.50982386430973,79.8014081751007,12.3445056966244));
#259649=CARTESIAN_POINT('Ctrl Pts',(9.68831043192349,79.7443724057398,12.3825));
#259650=CARTESIAN_POINT('Ctrl Pts',(9.87042927168866,79.6861759359438,12.3825));
#259651=CARTESIAN_POINT('Origin',(20.3338370957105,113.095,10.4775));
#259652=CARTESIAN_POINT('Origin',(20.3338370957106,113.095,10.4775));
#259653=CARTESIAN_POINT('Ctrl Pts',(-20.338738022895,113.110807370947,12.3825));
#259654=CARTESIAN_POINT('Ctrl Pts',(-19.968791272205,113.225505596211,12.3824999999999));
#259655=CARTESIAN_POINT('Ctrl Pts',(-19.6282160094772,113.331097486218,
12.2312547539385));
#259656=CARTESIAN_POINT('Ctrl Pts',(-18.6092073009371,107.532395344573,
12.3825));
#259657=CARTESIAN_POINT('Ctrl Pts',(-18.2577112653127,107.6517518065,12.3825000000253));
#259658=CARTESIAN_POINT('Ctrl Pts',(-17.9262673774906,107.744499673551,
12.2434569899207));
#259659=CARTESIAN_POINT('Ctrl Pts',(-16.8761662839561,101.955067511533,
12.3825));
#259660=CARTESIAN_POINT('Ctrl Pts',(-16.5451782462744,102.073466340022,
12.3824999999898));
#259661=CARTESIAN_POINT('Ctrl Pts',(-16.2272244980822,102.157103474302,
12.2580230532285));
#259662=CARTESIAN_POINT('Ctrl Pts',(-13.3939133181817,90.8112382967211,
12.3825));
#259663=CARTESIAN_POINT('Ctrl Pts',(-13.1184592484483,90.912945786136,12.3825000000101));
#259664=CARTESIAN_POINT('Ctrl Pts',(-12.8470248006833,90.9828768180411,
12.2950955201813));
#259665=CARTESIAN_POINT('Ctrl Pts',(-11.6464930191708,85.2441534264819,
12.3825));
#259666=CARTESIAN_POINT('Ctrl Pts',(-11.4074622811763,85.3412573398973,
12.3824999999188));
#259667=CARTESIAN_POINT('Ctrl Pts',(-11.1637373486809,85.3967648635073,
12.3186057572813));
#259668=CARTESIAN_POINT('Ctrl Pts',(-9.87042927168149,79.6861759359214,
12.3825));
#259669=CARTESIAN_POINT('Ctrl Pts',(-9.68831043191372,79.7443724057182,
12.3825));
#259670=CARTESIAN_POINT('Ctrl Pts',(-9.5098238642975,79.8014081750798,12.3445056966233));
#259671=CARTESIAN_POINT('Origin',(-20.3338370957106,113.095,10.4775));
#259672=CARTESIAN_POINT('Origin',(-20.3338370957106,113.095,10.4775));
#259673=CARTESIAN_POINT('Ctrl Pts',(9.97906670428255,80.6550131021071,12.6355897418272));
#259674=CARTESIAN_POINT('Ctrl Pts',(10.0306565474884,80.6485542978432,12.3963818596608));
#259675=CARTESIAN_POINT('Ctrl Pts',(10.0626130773097,80.8910903102766,12.3874807730462));
#259676=CARTESIAN_POINT('Ctrl Pts',(8.32489473089131,80.8596741618412,12.2721732806416));
#259677=CARTESIAN_POINT('Ctrl Pts',(8.38220322552675,80.853588835157,12.0386865759819));
#259678=CARTESIAN_POINT('Ctrl Pts',(8.39484377214235,81.0939065240695,12.0224470193747));
#259679=CARTESIAN_POINT('Ctrl Pts',(6.65782497351594,81.0143136970555,11.9945489971187));
#259680=CARTESIAN_POINT('Ctrl Pts',(6.69895405423401,81.0111835475032,11.7604293808636));
#259681=CARTESIAN_POINT('Ctrl Pts',(6.71387712855119,81.2473407845731,11.7435792721713));
#259682=CARTESIAN_POINT('Ctrl Pts',(4.1545853934931,81.167929206631,11.7183089462413));
#259683=CARTESIAN_POINT('Ctrl Pts',(4.17758614754292,81.1667081501201,11.4852779313552));
#259684=CARTESIAN_POINT('Ctrl Pts',(4.18963063148697,81.3998032104587,11.4660958435514));
#259685=CARTESIAN_POINT('Ctrl Pts',(3.32813735528307,81.2060674095149,11.649567866613));
#259686=CARTESIAN_POINT('Ctrl Pts',(3.34606415307882,81.2053149583786,11.4167992749039));
#259687=CARTESIAN_POINT('Ctrl Pts',(3.35622483782533,81.4376673268027,11.3970442061328));
#259688=CARTESIAN_POINT('Ctrl Pts',(1.66882448528439,81.2571037391673,11.5575387285848));
#259689=CARTESIAN_POINT('Ctrl Pts',(1.67821450599537,81.256876957723,11.3252958333052));
#259690=CARTESIAN_POINT('Ctrl Pts',(1.68291996832573,81.4883403078153,11.3045989360452));
#259691=CARTESIAN_POINT('Ctrl Pts',(0.834784835272045,81.2699994403931,
11.5342541227382));
#259692=CARTESIAN_POINT('Ctrl Pts',(0.839074610794663,81.2699304222547,
11.3020962817064));
#259693=CARTESIAN_POINT('Ctrl Pts',(0.841835610486893,81.5011467291217,
11.2812087546069));
#259694=CARTESIAN_POINT('Ctrl Pts',(-3.37266473870902,81.2700023175606,
11.5342489298588));
#259695=CARTESIAN_POINT('Ctrl Pts',(-3.38999574980634,81.2699333290047,
11.3020911179797));
#259696=CARTESIAN_POINT('Ctrl Pts',(-3.40115100228494,81.5011495862201,
11.2812035383244));
#259697=CARTESIAN_POINT('Ctrl Pts',(-6.69953756680781,81.0607706805708,
11.9150344302535));
#259698=CARTESIAN_POINT('Ctrl Pts',(-6.78961021185513,81.0517495349953,
11.6929294186456));
#259699=CARTESIAN_POINT('Ctrl Pts',(-6.75613034542886,81.2931923541874,
11.6637198264307));
#259700=CARTESIAN_POINT('Ctrl Pts',(-9.97933244163048,80.6549803814545,
12.6356486412316));
#259701=CARTESIAN_POINT('Ctrl Pts',(-10.0309242199162,80.6485200313328,
12.3964424789898));
#259702=CARTESIAN_POINT('Ctrl Pts',(-10.0628811435792,80.8910578280727,
12.3875399644105));
#259703=CARTESIAN_POINT('Ctrl Pts',(76.532738233499,27.1805870613698,16.1925));
#259704=CARTESIAN_POINT('Ctrl Pts',(76.532738233499,27.1805870613698,16.1925));
#259705=CARTESIAN_POINT('Ctrl Pts',(76.532738233499,27.1805870613698,16.1925));
#259706=CARTESIAN_POINT('Ctrl Pts',(76.4822360033882,27.108462402101,16.0119303091303));
#259707=CARTESIAN_POINT('Ctrl Pts',(76.4461624483558,27.0569440263853,16.0425775126009));
#259708=CARTESIAN_POINT('Ctrl Pts',(76.4100103023385,27.0053134111113,16.0732804919947));
#259709=CARTESIAN_POINT('Ctrl Pts',(76.4397549856158,27.0477932212451,15.8256195009857));
#259710=CARTESIAN_POINT('Ctrl Pts',(76.3671168872244,26.9440552658148,15.8737167831498));
#259711=CARTESIAN_POINT('Ctrl Pts',(76.3145038880894,26.8290932950587,15.9238883805606));
#259712=CARTESIAN_POINT('Ctrl Pts',(76.4065721949852,27.0004032849478,15.6340057707333));
#259713=CARTESIAN_POINT('Ctrl Pts',(76.2985554613104,26.8461394020553,15.6908641824603));
#259714=CARTESIAN_POINT('Ctrl Pts',(76.2443511862693,26.664968902009,15.7450581469137));
#259715=CARTESIAN_POINT('Ctrl Pts',(76.4071670555573,27.0012528338882,15.6374346124286));
#259716=CARTESIAN_POINT('Ctrl Pts',(76.4176851262999,27.016274195654,15.7161206159306));
#259717=CARTESIAN_POINT('Ctrl Pts',(76.4293098622517,27.0328195014371,15.7940085055158));
#259718=CARTESIAN_POINT('Ctrl Pts',(76.44205216039,27.0508562735771,15.8712754089344));
#259719=CARTESIAN_POINT('Ctrl Pts',(76.4549544984364,27.069119582824,15.949512764307));
#259720=CARTESIAN_POINT('Ctrl Pts',(76.469002736108,27.0889124184517,16.0271138595694));
#259721=CARTESIAN_POINT('Ctrl Pts',(76.4842364901892,27.1102366114595,16.1042351543385));
#259722=CARTESIAN_POINT('Ctrl Pts',(76.4874461624915,27.1147295073867,16.120484207751));
#259723=CARTESIAN_POINT('Ctrl Pts',(76.4907085588544,27.1192904969234,16.1367118525517));
#259724=CARTESIAN_POINT('Ctrl Pts',(76.4940242019312,27.1239197716699,16.1529193708669));
#259725=CARTESIAN_POINT('Ctrl Pts',(76.4496012596383,27.0600511154422,16.1720905903401));
#259726=CARTESIAN_POINT('Ctrl Pts',(76.4728494185474,27.091261572645,16.1624955941075));
#259727=CARTESIAN_POINT('Ctrl Pts',(76.4940242023748,27.1239197722893,16.1529193730355));
#259728=CARTESIAN_POINT('Ctrl Pts',(76.4324251716318,27.0369532490963,15.9953515848464));
#259729=CARTESIAN_POINT('Ctrl Pts',(76.4463480572545,27.0564032612897,15.9905628215355));
#259730=CARTESIAN_POINT('Ctrl Pts',(76.4598027159916,27.0761400025693,15.9856379879077));
#259731=CARTESIAN_POINT('Ctrl Pts',(76.4184454096962,27.0173599928704,15.8170364535711));
#259732=CARTESIAN_POINT('Ctrl Pts',(76.4245770423424,27.0261168718125,15.8152865503265));
#259733=CARTESIAN_POINT('Ctrl Pts',(76.4307073155649,27.0348718092963,15.8135400053977));
#259734=CARTESIAN_POINT('Ctrl Pts',(76.4071670555573,27.0012528338882,15.6374346124286));
#259735=CARTESIAN_POINT('Ctrl Pts',(76.4071670555573,27.0012528338882,15.6374346124286));
#259736=CARTESIAN_POINT('Ctrl Pts',(76.4071670555573,27.0012528338882,15.6374346124286));
#259737=CARTESIAN_POINT('Origin',(75.4310816924321,27.8186800531739,16.171929177394));
#259738=CARTESIAN_POINT('Ctrl Pts',(76.0135189288796,24.9743362449089,17.2567539685303));
#259739=CARTESIAN_POINT('Ctrl Pts',(75.9991603762543,25.0368598246417,17.3329617590086));
#259740=CARTESIAN_POINT('Ctrl Pts',(75.9698282088072,25.0952662902613,17.4081821724392));
#259741=CARTESIAN_POINT('Ctrl Pts',(75.9684245146036,25.1582927283603,17.0243415107349));
#259742=CARTESIAN_POINT('Ctrl Pts',(75.9600761821103,25.2156521066941,17.1240992078125));
#259743=CARTESIAN_POINT('Ctrl Pts',(75.9323827028628,25.2682007021653,17.2228395557702));
#259744=CARTESIAN_POINT('Ctrl Pts',(75.9418437641948,25.3910520091979,16.862700351237));
#259745=CARTESIAN_POINT('Ctrl Pts',(75.9388483528643,25.445796768841,16.9834260323936));
#259746=CARTESIAN_POINT('Ctrl Pts',(75.9089806068547,25.4963947971894,17.1020365608016));
#259747=CARTESIAN_POINT('Ctrl Pts',(75.9541657983329,25.7887320240513,16.6415771202465));
#259748=CARTESIAN_POINT('Ctrl Pts',(75.9591105110421,25.8384885908314,16.7940129727795));
#259749=CARTESIAN_POINT('Ctrl Pts',(75.9243559941834,25.8898093808734,16.9419191856935));
#259750=CARTESIAN_POINT('Ctrl Pts',(75.9755313586025,25.9560410312404,16.5655243592805));
#259751=CARTESIAN_POINT('Ctrl Pts',(75.9835274011649,26.0037786517969,16.730097613125));
#259752=CARTESIAN_POINT('Ctrl Pts',(75.9462476067507,26.0563925183529,16.888987323054));
#259753=CARTESIAN_POINT('Ctrl Pts',(76.0537110495859,26.2901439472438,16.430093768641));
#259754=CARTESIAN_POINT('Ctrl Pts',(76.0669818398559,26.3329365721293,16.617385587321));
#259755=CARTESIAN_POINT('Ctrl Pts',(76.0249595721014,26.3897550778952,16.7964776672641));
#259756=CARTESIAN_POINT('Ctrl Pts',(76.1106254906956,26.4559143405794,16.3716494180751));
#259757=CARTESIAN_POINT('Ctrl Pts',(76.1261665775814,26.4957943220995,16.5698206523398));
#259758=CARTESIAN_POINT('Ctrl Pts',(76.0817008086393,26.5557571967131,16.7582736038159));
#259759=CARTESIAN_POINT('Ctrl Pts',(76.2206362259214,26.6928863098607,16.2954976206041));
#259760=CARTESIAN_POINT('Ctrl Pts',(76.2382520010556,26.7274552575817,16.5052911886963));
#259761=CARTESIAN_POINT('Ctrl Pts',(76.1926335678084,26.7915039216042,16.7036134975717));
#259762=CARTESIAN_POINT('Ctrl Pts',(76.2615893549122,26.7704586218702,16.2719030686384));
#259763=CARTESIAN_POINT('Ctrl Pts',(76.2797058737871,26.8031110554089,16.4852296809776));
#259764=CARTESIAN_POINT('Ctrl Pts',(76.2339253041331,26.8686071917093,16.6865119483355));
#259765=CARTESIAN_POINT('Ctrl Pts',(76.3293506348445,26.8839886375728,16.2388534884045));
#259766=CARTESIAN_POINT('Ctrl Pts',(76.3475815823904,26.9132368525625,16.4509817168048));
#259767=CARTESIAN_POINT('Ctrl Pts',(76.3047198064137,26.9781622528333,16.6513143014549));
#259768=CARTESIAN_POINT('Ctrl Pts',(76.352936031986,26.9212671030173,16.2282720121333));
#259769=CARTESIAN_POINT('Ctrl Pts',(76.3710861233276,26.949270802543,16.439505830876));
#259770=CARTESIAN_POINT('Ctrl Pts',(76.3295234781731,27.0137899593914,16.639113518033));
#259771=CARTESIAN_POINT('Ctrl Pts',(76.3897977681848,26.9762969849698,16.2127741097789));
#259772=CARTESIAN_POINT('Ctrl Pts',(76.4073792368665,27.0019658578953,16.4134596674917));
#259773=CARTESIAN_POINT('Ctrl Pts',(76.3718135183751,27.0620819877444,16.6041529821789));
#259774=CARTESIAN_POINT('Ctrl Pts',(76.4023273523985,26.9944844920511,16.2076984546917));
#259775=CARTESIAN_POINT('Ctrl Pts',(76.4196215779418,27.0192636816435,16.4043770534771));
#259776=CARTESIAN_POINT('Ctrl Pts',(76.3864139085197,27.0775694765284,16.591707715843));
#259777=CARTESIAN_POINT('Ctrl Pts',(76.4182736725831,27.0169978024882,16.2011700710385));
#259778=CARTESIAN_POINT('Ctrl Pts',(76.4349444211234,27.0403624632552,16.381098623647));
#259779=CARTESIAN_POINT('Ctrl Pts',(76.4092245675447,27.0924838923546,16.5537833743782));
#259780=CARTESIAN_POINT('Ctrl Pts',(76.4214772237873,27.0214895124959,16.1998527480328));
#259781=CARTESIAN_POINT('Ctrl Pts',(76.4380023011771,27.0445457602702,16.3757607500836));
#259782=CARTESIAN_POINT('Ctrl Pts',(76.4140487138282,27.0952122751629,16.5448980557904));
#259783=CARTESIAN_POINT('Ctrl Pts',(76.4279076878214,27.0304439095153,16.197147126751));
#259784=CARTESIAN_POINT('Ctrl Pts',(76.4441127500533,27.0528532380362,16.3617442626138));
#259785=CARTESIAN_POINT('Ctrl Pts',(76.4248418621342,27.0997179766929,16.5207709779264));
#259786=CARTESIAN_POINT('Ctrl Pts',(76.4311355139959,27.0349078309285,16.1957692072802));
#259787=CARTESIAN_POINT('Ctrl Pts',(76.4471475072276,27.0569532640503,16.353378507755));
#259788=CARTESIAN_POINT('Ctrl Pts',(76.4307401571975,27.1014806667834,16.5061220168225));
#259789=CARTESIAN_POINT('Ctrl Pts',(76.4375990464852,27.0437858881523,16.1927492164626));
#259790=CARTESIAN_POINT('Ctrl Pts',(76.4533656745128,27.0653090310172,16.3262439284466));
#259791=CARTESIAN_POINT('Ctrl Pts',(76.4456774700282,27.1032717188634,16.4567548936541));
#259792=CARTESIAN_POINT('Ctrl Pts',(76.4408619220711,27.0482365818426,16.1912703300228));
#259793=CARTESIAN_POINT('Ctrl Pts',(76.4564740580196,27.0694680856207,16.3056985101718));
#259794=CARTESIAN_POINT('Ctrl Pts',(76.455545261251,27.1023654406524,16.4183837546514));
#259795=CARTESIAN_POINT('Ctrl Pts',(76.4456024830061,27.0546608085524,16.1874122722788));
#259796=CARTESIAN_POINT('Ctrl Pts',(76.4626691372742,27.0777286074699,16.2584144265338));
#259797=CARTESIAN_POINT('Ctrl Pts',(76.4724831553652,27.105919574582,16.3289405788401));
#259798=CARTESIAN_POINT('Ctrl Pts',(76.4471920450455,27.0568070233922,16.1858770660613));
#259799=CARTESIAN_POINT('Ctrl Pts',(76.4650242491595,27.0808620750697,16.2408811596319));
#259800=CARTESIAN_POINT('Ctrl Pts',(76.4782041251027,27.1082005910335,16.2956491527569));
#259801=CARTESIAN_POINT('Ctrl Pts',(76.4824975375383,27.1043580483931,16.1112477802486));
#259802=CARTESIAN_POINT('Ctrl Pts',(76.5324864042392,27.1705424338065,15.6967037653767));
#259803=CARTESIAN_POINT('Ctrl Pts',(76.6206938565971,27.2122852390614,15.2747264778709));
#259804=CARTESIAN_POINT('Ctrl Pts',(76.0596473272883,26.5325612269295,14.9152913818395));
#259805=CARTESIAN_POINT('Ctrl Pts',(76.5169321639722,27.1543749835465,12.0112890458989));
#259806=CARTESIAN_POINT('Ctrl Pts',(76.0362901547838,28.43850005779,10.812760927815));
#259807=CARTESIAN_POINT('Ctrl Pts',(67.4282061989127,15.0466061792269,43.6759546261335));
#259808=CARTESIAN_POINT('Ctrl Pts',(66.2614595719668,13.6559904578472,92.6380204617887));
#259809=CARTESIAN_POINT('Ctrl Pts',(44.6874817572436,-42.6649830590962,
383.024483305851));
#259810=CARTESIAN_POINT('Origin',(74.7257085670769,24.9421491495265,17.0741173620445));
#259811=CARTESIAN_POINT('Ctrl Pts',(75.9397262748,25.2708374178295,17.2518520136118));
#259812=CARTESIAN_POINT('Ctrl Pts',(75.9685632596794,25.216936348383,17.1547259853702));
#259813=CARTESIAN_POINT('Ctrl Pts',(75.9772090303541,25.1589733721721,17.0560474933639));
#259814=CARTESIAN_POINT('Ctrl Pts',(75.9481612403383,25.2082186978402,17.2973276044734));
#259815=CARTESIAN_POINT('Ctrl Pts',(75.9759984326351,25.1530396512954,17.2125718697421));
#259816=CARTESIAN_POINT('Ctrl Pts',(75.987289897294,25.0938856962963,17.126659867066));
#259817=CARTESIAN_POINT('Ctrl Pts',(75.9580441980768,25.1496292036213,17.3506767479875));
#259818=CARTESIAN_POINT('Ctrl Pts',(75.9851307385962,25.0926862211882,17.2798459584166));
#259819=CARTESIAN_POINT('Ctrl Pts',(75.9990697411205,25.0322694075925,17.2080611432674));
#259820=CARTESIAN_POINT('Ctrl Pts',(75.9627753173077,25.1074704497584,17.4259425795047));
#259821=CARTESIAN_POINT('Ctrl Pts',(75.9901905947633,25.0462350072204,17.3727027235267));
#259822=CARTESIAN_POINT('Ctrl Pts',(76.0065414441445,24.9819025616069,17.318579611819));
#259823=CARTESIAN_POINT('Origin',(74.7646897896784,24.7225971487503,17.2528005263547));
#259824=CARTESIAN_POINT('Ctrl Pts',(75.961489026876,25.1183452685166,17.4075745924791));
#259825=CARTESIAN_POINT('Ctrl Pts',(75.9888185880884,25.0581838218694,17.3500764673617));
#259826=CARTESIAN_POINT('Ctrl Pts',(76.0045572676606,24.9948448130137,17.2916572676644));
#259827=CARTESIAN_POINT('Ctrl Pts',(75.9867440840342,24.9827521037965,17.5589921227903));
#259828=CARTESIAN_POINT('Ctrl Pts',(76.0047941374301,24.9436535528168,17.5184791523472));
#259829=CARTESIAN_POINT('Ctrl Pts',(76.0189046879114,24.9029090128953,17.4779931990458));
#259830=CARTESIAN_POINT('Ctrl Pts',(76.0138748889673,24.8422792694551,17.7055224896847));
#259831=CARTESIAN_POINT('Ctrl Pts',(76.0228272111373,24.8230534553229,17.6845460983331));
#259832=CARTESIAN_POINT('Ctrl Pts',(76.0317753893963,24.8038409415364,17.6635683446408));
#259833=CARTESIAN_POINT('Ctrl Pts',(76.042458286517,24.6976449914381,17.8479876926701));
#259834=CARTESIAN_POINT('Ctrl Pts',(76.042458286517,24.6976449914381,17.8479876926701));
#259835=CARTESIAN_POINT('Ctrl Pts',(76.042458286517,24.6976449914381,17.8479876926701));
#259836=CARTESIAN_POINT('Ctrl Pts',(25.0804618860237,75.9725615368778,17.42016687813));
#259837=CARTESIAN_POINT('Ctrl Pts',(25.0218849779072,76.0018311057243,17.3465486623464));
#259838=CARTESIAN_POINT('Ctrl Pts',(24.9591222047285,76.01654431203,17.2720397183974));
#259839=CARTESIAN_POINT('Ctrl Pts',(25.2741629194071,75.9311692985981,17.2143925574792));
#259840=CARTESIAN_POINT('Ctrl Pts',(25.2217620983607,75.958681184656,17.1148633560418));
#259841=CARTESIAN_POINT('Ctrl Pts',(25.1645554520732,75.9667333080871,17.0143457047747));
#259842=CARTESIAN_POINT('Ctrl Pts',(25.5065028345103,75.9076483674903,17.0946463742361));
#259843=CARTESIAN_POINT('Ctrl Pts',(25.4560812233288,75.9374572719628,16.9750964736288));
#259844=CARTESIAN_POINT('Ctrl Pts',(25.4014568018248,75.9400754392651,16.8534468191218));
#259845=CARTESIAN_POINT('Ctrl Pts',(25.9210527955236,75.9275280255501,16.929244875955));
#259846=CARTESIAN_POINT('Ctrl Pts',(25.8696322348271,75.9625142169106,16.7791814037363));
#259847=CARTESIAN_POINT('Ctrl Pts',(25.8202904741259,75.9568105611576,16.6244542312898));
#259848=CARTESIAN_POINT('Ctrl Pts',(26.1003508790249,75.9538339499108,16.8739158934014));
#259849=CARTESIAN_POINT('Ctrl Pts',(26.0473908953034,75.9915498547677,16.7122017332863));
#259850=CARTESIAN_POINT('Ctrl Pts',(26.0002790025707,75.9825893385705,16.5445597191504));
#259851=CARTESIAN_POINT('Ctrl Pts',(26.4483576685963,76.0436899102596,16.7801350408625));
#259852=CARTESIAN_POINT('Ctrl Pts',(26.3907212263412,76.0862364212148,16.5977546210469));
#259853=CARTESIAN_POINT('Ctrl Pts',(26.3489939258796,76.0719119444782,16.4067913625631));
#259854=CARTESIAN_POINT('Ctrl Pts',(26.6209880248573,76.1074179294988,16.7422284473565));
#259855=CARTESIAN_POINT('Ctrl Pts',(26.5597476890913,76.1525248745944,16.5501048951609));
#259856=CARTESIAN_POINT('Ctrl Pts',(26.5212227642717,76.1359425371639,16.3477329791976));
#259857=CARTESIAN_POINT('Ctrl Pts',(26.8247483133823,76.2123121583579,16.6934782675247));
#259858=CARTESIAN_POINT('Ctrl Pts',(26.7604265541748,76.2574262010901,16.4943208592323));
#259859=CARTESIAN_POINT('Ctrl Pts',(26.7269236186754,76.2394155534515,16.2836305889901));
#259860=CARTESIAN_POINT('Ctrl Pts',(26.8648052287377,76.2345275940671,16.6835961109164));
#259861=CARTESIAN_POINT('Ctrl Pts',(26.7999815868847,76.2794711085834,16.4833268552169));
#259862=CARTESIAN_POINT('Ctrl Pts',(26.7675182843409,76.2612367837886,16.2713262631411));
#259863=CARTESIAN_POINT('Ctrl Pts',(26.9428805656769,76.2819273824504,16.6613225028936));
#259864=CARTESIAN_POINT('Ctrl Pts',(26.877812280624,76.325608218886,16.460395029503));
#259865=CARTESIAN_POINT('Ctrl Pts',(26.8475982558576,76.307141242556,16.2476495576019));
#259866=CARTESIAN_POINT('Ctrl Pts',(26.9810543502164,76.3069759166512,16.6496028712586));
#259867=CARTESIAN_POINT('Ctrl Pts',(26.9160778594133,76.3496981928984,16.4488297968031));
#259868=CARTESIAN_POINT('Ctrl Pts',(26.8870847364683,76.3312252545636,16.236284876982));
#259869=CARTESIAN_POINT('Ctrl Pts',(27.0347146146409,76.348479787188,16.6221367327716));
#259870=CARTESIAN_POINT('Ctrl Pts',(26.9722866202233,76.3871914756644,16.4263729310828));
#259871=CARTESIAN_POINT('Ctrl Pts',(26.9454540778621,76.3690625317951,16.2198040383442));
#259872=CARTESIAN_POINT('Ctrl Pts',(27.0520461010348,76.3629033141244,16.6116902389514));
#259873=CARTESIAN_POINT('Ctrl Pts',(26.9907978709005,76.3998985070121,16.4182354344391));
#259874=CARTESIAN_POINT('Ctrl Pts',(26.9647604072736,76.381956422089,16.2144102296118));
#259875=CARTESIAN_POINT('Ctrl Pts',(27.0754324956893,76.3870229007004,16.5857176723783));
#259876=CARTESIAN_POINT('Ctrl Pts',(27.0180627224541,76.4191298939433,16.4005487707549));
#259877=CARTESIAN_POINT('Ctrl Pts',(26.993440890971,76.4016850635576,16.2063864536409));
#259878=CARTESIAN_POINT('Ctrl Pts',(27.0828077996879,76.3954507470087,16.5755244414192));
#259879=CARTESIAN_POINT('Ctrl Pts',(27.0270559839662,76.4255606544124,16.3938428354607));
#259880=CARTESIAN_POINT('Ctrl Pts',(27.0029569073645,76.4083274633204,16.2037237985546));
#259881=CARTESIAN_POINT('Ctrl Pts',(27.0922320376545,76.4098047654343,16.5516204721261));
#259882=CARTESIAN_POINT('Ctrl Pts',(27.0403670147032,76.4351975383171,16.379224441304));
#259883=CARTESIAN_POINT('Ctrl Pts',(27.0171572804521,76.4183850872755,16.1996869095685));
#259884=CARTESIAN_POINT('Ctrl Pts',(27.0950953264234,76.4148733708239,16.5422413732297));
#259885=CARTESIAN_POINT('Ctrl Pts',(27.0447678397126,76.4384035784988,16.3736104964544));
#259886=CARTESIAN_POINT('Ctrl Pts',(27.0218787739723,76.4217535244975,16.1983342860912));
#259887=CARTESIAN_POINT('Ctrl Pts',(27.0997431526784,76.4263249193079,16.5161165141993));
#259888=CARTESIAN_POINT('Ctrl Pts',(27.0535116464061,76.4448069459393,16.3585277802149));
#259889=CARTESIAN_POINT('Ctrl Pts',(27.0312909576619,76.42851717559,16.1955743904641));
#259890=CARTESIAN_POINT('Ctrl Pts',(27.1014904674051,76.4326137594198,16.500204580009));
#259891=CARTESIAN_POINT('Ctrl Pts',(27.0578166604433,76.4479765311902,16.3494953976019));
#259892=CARTESIAN_POINT('Ctrl Pts',(27.035983172867,76.4319135317257,16.1941800679768));
#259893=CARTESIAN_POINT('Ctrl Pts',(27.1026704184044,76.444945265315,16.4573094494972));
#259894=CARTESIAN_POINT('Ctrl Pts',(27.0644828819285,76.4528969605584,16.3261248042041));
#259895=CARTESIAN_POINT('Ctrl Pts',(27.0429752642404,76.4370110131298,16.1919016822556));
#259896=CARTESIAN_POINT('Ctrl Pts',(27.1027728684423,76.4496135704595,16.4393960541736));
#259897=CARTESIAN_POINT('Ctrl Pts',(27.0667393944962,76.4545638835509,16.3164891117538));
#259898=CARTESIAN_POINT('Ctrl Pts',(27.0453014012289,76.4387129855077,16.191114532674));
#259899=CARTESIAN_POINT('Ctrl Pts',(27.103348843805,76.4602856539461,16.3918070921655));
#259900=CARTESIAN_POINT('Ctrl Pts',(27.0716717101299,76.4582133271172,16.2912288897505));
#259901=CARTESIAN_POINT('Ctrl Pts',(27.0498984940075,76.4420884316598,16.1893010704596));
#259902=CARTESIAN_POINT('Ctrl Pts',(27.103921956882,76.4662567117721,16.3621450323075));
#259903=CARTESIAN_POINT('Ctrl Pts',(27.0743744435426,76.4602162047732,16.2756512778861));
#259904=CARTESIAN_POINT('Ctrl Pts',(27.0521738675702,76.4437652233597,16.1883092099684));
#259905=CARTESIAN_POINT('Ctrl Pts',(27.1079500471734,76.4780100141054,16.294962253566));
#259906=CARTESIAN_POINT('Ctrl Pts',(27.0805869451208,76.4648464736715,16.2402396311017));
#259907=CARTESIAN_POINT('Ctrl Pts',(27.0565399426139,76.44699327834,16.1852909757062));
#259908=CARTESIAN_POINT('Ctrl Pts',(27.1117437396561,76.4840868539103,16.2559882667085));
#259909=CARTESIAN_POINT('Ctrl Pts',(27.0843760577268,76.4676882621526,16.2196371037558));
#259910=CARTESIAN_POINT('Ctrl Pts',(27.0588362934594,76.4486982192428,16.1831963663287));
#259911=CARTESIAN_POINT('Ctrl Pts',(27.1186429162632,76.4907257277754,16.1967720341455));
#259912=CARTESIAN_POINT('Ctrl Pts',(27.088970607914,76.4711321232317,16.1872136925927));
#259913=CARTESIAN_POINT('Ctrl Pts',(27.0604496119645,76.449897797078,16.1776432448508));
#259914=CARTESIAN_POINT('Ctrl Pts',(27.1210505518365,76.4924398017442,16.1773616860778));
#259915=CARTESIAN_POINT('Ctrl Pts',(27.0902380459636,76.4720805095757,16.1763774272393));
#259916=CARTESIAN_POINT('Ctrl Pts',(27.0606161752026,76.4500218115713,16.1753910477049));
#259917=CARTESIAN_POINT('Ctrl Pts',(27.124723692261,76.4945108031749,16.1461844913816));
#259918=CARTESIAN_POINT('Ctrl Pts',(27.0917434440934,76.4731956267604,16.1586478057256));
#259919=CARTESIAN_POINT('Ctrl Pts',(27.0602497730199,76.4497492188553,16.171136001378));
#259920=CARTESIAN_POINT('Ctrl Pts',(27.1261031628968,76.4950020357299,16.133681728625));
#259921=CARTESIAN_POINT('Ctrl Pts',(27.0920805335392,76.4734376571502,16.1513715711389));
#259922=CARTESIAN_POINT('Ctrl Pts',(27.0597799419463,76.4493997295785,16.1691026721927));
#259923=CARTESIAN_POINT('Ctrl Pts',(27.13156819983,76.4963255984209,16.0800932837589));
#259924=CARTESIAN_POINT('Ctrl Pts',(27.0928134511323,76.4739251360543,16.1197927836122));
#259925=CARTESIAN_POINT('Ctrl Pts',(27.0569687226394,76.4473109346435,16.1596448232299));
#259926=CARTESIAN_POINT('Ctrl Pts',(27.1323195784948,76.49451130004,16.0589082957883));
#259927=CARTESIAN_POINT('Ctrl Pts',(27.09092096414,76.4724331002845,16.1061418174196));
#259928=CARTESIAN_POINT('Ctrl Pts',(27.0534134152984,76.4446774540829,16.1536294662393));
#259929=CARTESIAN_POINT('Ctrl Pts',(27.1329837771627,76.4909539904125,16.0195114651259));
#259930=CARTESIAN_POINT('Ctrl Pts',(27.0869366765608,76.4693129058743,16.0806139918041));
#259931=CARTESIAN_POINT('Ctrl Pts',(27.0464009528429,76.4395165697625,16.1421882796318));
#259932=CARTESIAN_POINT('Ctrl Pts',(27.1324755596785,76.4887423766883,16.0040405252725));
#259933=CARTESIAN_POINT('Ctrl Pts',(27.0844779770551,76.4674056396185,16.0701604569275));
#259934=CARTESIAN_POINT('Ctrl Pts',(27.0426984150638,76.436805864295,16.1368608677846));
#259935=CARTESIAN_POINT('Ctrl Pts',(27.1176445692947,76.4487554850658,15.7668594205244));
#259936=CARTESIAN_POINT('Ctrl Pts',(27.0392647575274,76.4325632146525,15.9058934996621));
#259937=CARTESIAN_POINT('Ctrl Pts',(26.978304049824,76.3899445519393,16.0485446134497));
#259938=CARTESIAN_POINT('Ctrl Pts',(27.0267181002176,76.3890441685062,15.9290103439652));
#259939=CARTESIAN_POINT('Ctrl Pts',(26.9607754137162,76.3752347443015,15.9631551147917));
#259940=CARTESIAN_POINT('Ctrl Pts',(26.9028259695809,76.3392599186689,16.0018551686532));
#259941=CARTESIAN_POINT('Ctrl Pts',(27.0702645564447,76.3535975697862,14.8756002301201));
#259942=CARTESIAN_POINT('Ctrl Pts',(26.9358287323369,76.3662706710394,15.3627392753264));
#259943=CARTESIAN_POINT('Ctrl Pts',(26.8612497825162,76.3194480577275,15.8395311951992));
#259944=CARTESIAN_POINT('Origin',(24.9421491495265,74.7257085670769,17.0741173620444));
#259945=CARTESIAN_POINT('Ctrl Pts',(25.1074704499368,75.962775317243,17.4259425795535));
#259946=CARTESIAN_POINT('Ctrl Pts',(25.0462350073064,75.9901905947506,17.3727027235419));
#259947=CARTESIAN_POINT('Ctrl Pts',(24.9819025616059,76.0065414441456,17.3185796118044));
#259948=CARTESIAN_POINT('Ctrl Pts',(25.1496292029159,75.958044198321,17.3506767478669));
#259949=CARTESIAN_POINT('Ctrl Pts',(25.0926862207362,75.9851307386925,17.2798459583226));
#259950=CARTESIAN_POINT('Ctrl Pts',(25.0322694073611,75.9990697411724,17.2080611431853));
#259951=CARTESIAN_POINT('Ctrl Pts',(25.2082186982409,75.94816124025,17.2973276043272));
#259952=CARTESIAN_POINT('Ctrl Pts',(25.1530396514998,75.9759984326018,17.2125718696368));
#259953=CARTESIAN_POINT('Ctrl Pts',(25.0938856963519,75.9872898972842,17.1266598669887));
#259954=CARTESIAN_POINT('Ctrl Pts',(25.2708374177375,75.9397262748181,17.2518520136545));
#259955=CARTESIAN_POINT('Ctrl Pts',(25.216936348314,75.968563259699,17.154725985359));
#259956=CARTESIAN_POINT('Ctrl Pts',(25.1589733721109,75.9772090303638,17.0560474933022));
#259957=CARTESIAN_POINT('Origin',(24.7225971487432,74.7646897896797,17.2528005263626));
#259958=CARTESIAN_POINT('Ctrl Pts',(24.9948448130087,76.0045572676614,17.2916572676743));
#259959=CARTESIAN_POINT('Ctrl Pts',(25.0581838218632,75.9888185880893,17.3500764673706));
#259960=CARTESIAN_POINT('Ctrl Pts',(25.1183452685093,75.9614890268773,17.4075745924872));
#259961=CARTESIAN_POINT('Ctrl Pts',(24.9029090128636,76.0189046879184,17.4779931990423));
#259962=CARTESIAN_POINT('Ctrl Pts',(24.9436535528443,76.0047941374266,17.5184791523504));
#259963=CARTESIAN_POINT('Ctrl Pts',(24.9827521037621,75.9867440840482,17.55899212277));
#259964=CARTESIAN_POINT('Ctrl Pts',(24.803840941519,76.0317753894034,17.6635683446283));
#259965=CARTESIAN_POINT('Ctrl Pts',(24.8230534553019,76.0228272111432,17.6845460983396));
#259966=CARTESIAN_POINT('Ctrl Pts',(24.8422792694592,76.0138748889657,17.7055224896865));
#259967=CARTESIAN_POINT('Ctrl Pts',(24.6976449914385,76.0424582865173,17.8479876926674));
#259968=CARTESIAN_POINT('Ctrl Pts',(24.6976449914385,76.0424582865173,17.8479876926674));
#259969=CARTESIAN_POINT('Ctrl Pts',(24.6976449914385,76.0424582865173,17.8479876926674));
#259970=CARTESIAN_POINT('Ctrl Pts',(-24.9589179253363,76.01659273472,17.271923598526));
#259971=CARTESIAN_POINT('Ctrl Pts',(-25.0217593831366,76.0018779351851,
17.3465144252831));
#259972=CARTESIAN_POINT('Ctrl Pts',(-25.0804061471587,75.9725739124909,
17.4202136823926));
#259973=CARTESIAN_POINT('Ctrl Pts',(-25.1644631759507,75.9667363952496,
17.0140601850114));
#259974=CARTESIAN_POINT('Ctrl Pts',(-25.2217418913752,75.9586992553381,
17.1147005696024));
#259975=CARTESIAN_POINT('Ctrl Pts',(-25.27420346249,75.9311549697297,17.2143522966372));
#259976=CARTESIAN_POINT('Ctrl Pts',(-25.4013568067359,75.9400924589015,
16.8531572347146));
#259977=CARTESIAN_POINT('Ctrl Pts',(-25.4560486787868,75.9375037638146,
16.9749518252951));
#259978=CARTESIAN_POINT('Ctrl Pts',(-25.5065310406966,75.9076590514475,
17.0946441542763));
#259979=CARTESIAN_POINT('Ctrl Pts',(-25.8199808098823,75.9567824207016,
16.6241920453249));
#259980=CARTESIAN_POINT('Ctrl Pts',(-25.8693789122518,75.9625371920841,
16.7790876761471));
#259981=CARTESIAN_POINT('Ctrl Pts',(-25.9208598320779,75.9275121101251,
16.9293154168732));
#259982=CARTESIAN_POINT('Ctrl Pts',(-26.0000535557612,75.9825492872224,
16.5442194952226));
#259983=CARTESIAN_POINT('Ctrl Pts',(-26.0472138461683,75.9915734867984,
16.7120520477243));
#259984=CARTESIAN_POINT('Ctrl Pts',(-26.1002356612948,75.9538145397959,
16.8739507932185));
#259985=CARTESIAN_POINT('Ctrl Pts',(-26.348734118025,76.0718263565562,16.4064067143953));
#259986=CARTESIAN_POINT('Ctrl Pts',(-26.3904925511526,76.0862325753191,
16.5975865850527));
#259987=CARTESIAN_POINT('Ctrl Pts',(-26.4481950399281,76.0436375882038,
16.7801750181481));
#259988=CARTESIAN_POINT('Ctrl Pts',(-26.5206773054617,76.1357086392241,
16.3474135480229));
#259989=CARTESIAN_POINT('Ctrl Pts',(-26.5592282331617,76.1523784609536,
16.5499987072448));
#259990=CARTESIAN_POINT('Ctrl Pts',(-26.6205318943627,76.1072227609038,
16.7423277269629));
#259991=CARTESIAN_POINT('Ctrl Pts',(-26.7264920249991,76.2391872025004,
16.2832499587999));
#259992=CARTESIAN_POINT('Ctrl Pts',(-26.7600048034107,76.2572914161368,
16.4941794865568));
#259993=CARTESIAN_POINT('Ctrl Pts',(-26.824398868812,76.2121224123054,16.6935643217025));
#259994=CARTESIAN_POINT('Ctrl Pts',(-26.7670983623262,76.2610052221557,
16.2709381057852));
#259995=CARTESIAN_POINT('Ctrl Pts',(-26.7995686636006,76.2793339264537,
16.4831824942709));
#259996=CARTESIAN_POINT('Ctrl Pts',(-26.8644662376051,76.2343342569761,
16.6836830243191));
#259997=CARTESIAN_POINT('Ctrl Pts',(-26.8471814943334,76.3068912734128,
16.2472568170159));
#259998=CARTESIAN_POINT('Ctrl Pts',(-26.8773983376708,76.3254529676178,
16.4602585575014));
#259999=CARTESIAN_POINT('Ctrl Pts',(-26.9425455013332,76.2817116055851,
16.6614278018637));
#260000=CARTESIAN_POINT('Ctrl Pts',(-26.8866594659865,76.3309600827125,
16.2358941826432));
#260001=CARTESIAN_POINT('Ctrl Pts',(-26.9156538041466,76.3495273607928,
16.4486994615681));
#260002=CARTESIAN_POINT('Ctrl Pts',(-26.9807109662172,76.3067428814873,
16.6497176791804));
#260003=CARTESIAN_POINT('Ctrl Pts',(-26.9450028183287,76.3687633480519,
16.2194335079569));
#260004=CARTESIAN_POINT('Ctrl Pts',(-26.9718386918007,76.3869839753116,
16.4263030318194));
#260005=CARTESIAN_POINT('Ctrl Pts',(-27.0343640337368,76.3481925870805,
16.6223462099112));
#260006=CARTESIAN_POINT('Ctrl Pts',(-26.9643135712108,76.381654087884,16.2140445092996));
#260007=CARTESIAN_POINT('Ctrl Pts',(-26.9903552533354,76.3996866408693,
16.418184305942));
#260008=CARTESIAN_POINT('Ctrl Pts',(-27.0517070202451,76.3626055712697,
16.6119303438144));
#260009=CARTESIAN_POINT('Ctrl Pts',(-26.9930030958707,76.401380124159,16.2060411922581));
#260010=CARTESIAN_POINT('Ctrl Pts',(-27.0176339860631,76.4189117637762,
16.4005910944646));
#260011=CARTESIAN_POINT('Ctrl Pts',(-27.0751338525107,76.3866896894671,
16.5861155304994));
#260012=CARTESIAN_POINT('Ctrl Pts',(-27.0025216597485,76.4080213751607,
16.203387528453));
#260013=CARTESIAN_POINT('Ctrl Pts',(-27.026632165822,76.4253400029413,16.3939233817012));
#260014=CARTESIAN_POINT('Ctrl Pts',(-27.0825251253766,76.3951028705659,
16.5759864041684));
#260015=CARTESIAN_POINT('Ctrl Pts',(-27.0167251805518,76.4180768548563,
16.1993760622623));
#260016=CARTESIAN_POINT('Ctrl Pts',(-27.0399520663499,76.4349711944826,
16.3794519172504));
#260017=CARTESIAN_POINT('Ctrl Pts',(-27.0919957484794,76.4094060117648,
16.5523397019094));
#260018=CARTESIAN_POINT('Ctrl Pts',(-27.0214474035482,76.4214443578374,
16.1980339064543));
#260019=CARTESIAN_POINT('Ctrl Pts',(-27.0443560687477,76.4381750002681,
16.3739005940378));
#260020=CARTESIAN_POINT('Ctrl Pts',(-27.0948782490049,76.4144529107837,
16.5430709433479));
#260021=CARTESIAN_POINT('Ctrl Pts',(-27.0308618441442,76.4282067437578,
16.19530514003));
#260022=CARTESIAN_POINT('Ctrl Pts',(-27.053106800039,76.444572163028,16.3590502469535));
#260023=CARTESIAN_POINT('Ctrl Pts',(-27.0995848854146,76.4258296167095,
16.5173659130853));
#260024=CARTESIAN_POINT('Ctrl Pts',(-27.0355558280438,76.4316029371517,
16.1939295287546));
#260025=CARTESIAN_POINT('Ctrl Pts',(-27.0574185499143,76.4477400974505,
16.3501709551169));
#260026=CARTESIAN_POINT('Ctrl Pts',(-27.1013790741377,76.4320671394762,
16.5017321290356));
#260027=CARTESIAN_POINT('Ctrl Pts',(-27.0425542463667,76.4367029519925,
16.1917093206043));
#260028=CARTESIAN_POINT('Ctrl Pts',(-27.0640786984513,76.4526420016968,
16.3273830388961));
#260029=CARTESIAN_POINT('Ctrl Pts',(-27.102629006752,76.4442399758458,16.4599278648171));
#260030=CARTESIAN_POINT('Ctrl Pts',(-27.0448820844151,76.4384054861842,
16.1909469831181));
#260031=CARTESIAN_POINT('Ctrl Pts',(-27.0663285798975,76.454298592053,16.3180252537668));
#260032=CARTESIAN_POINT('Ctrl Pts',(-27.1027558329562,76.4488339487676,
16.4425406392177));
#260033=CARTESIAN_POINT('Ctrl Pts',(-27.0494862895922,76.4417848360543,
16.1892131480628));
#260034=CARTESIAN_POINT('Ctrl Pts',(-27.0712224151044,76.4579068033435,
16.2933864311227));
#260035=CARTESIAN_POINT('Ctrl Pts',(-27.1032790984671,76.4593812159613,
16.3961238758005));
#260036=CARTESIAN_POINT('Ctrl Pts',(-27.0517726556214,76.4434690777321,
16.1882712263809));
#260037=CARTESIAN_POINT('Ctrl Pts',(-27.0738999783668,76.4598835948997,
16.2780430539621));
#260038=CARTESIAN_POINT('Ctrl Pts',(-27.1037600523946,76.4653396358795,
16.3668982051164));
#260039=CARTESIAN_POINT('Ctrl Pts',(-27.0561659022714,76.4467160440046,
16.1854342155749));
#260040=CARTESIAN_POINT('Ctrl Pts',(-27.0800526954001,76.4644564134043,
16.2430395007726));
#260041=CARTESIAN_POINT('Ctrl Pts',(-27.1075193430059,76.4771343839088,
16.3003874919345));
#260042=CARTESIAN_POINT('Ctrl Pts',(-27.058446159053,76.4484083289748,16.1835540069008));
#260043=CARTESIAN_POINT('Ctrl Pts',(-27.0837265632002,76.4672060746151,
16.2231638663765));
#260044=CARTESIAN_POINT('Ctrl Pts',(-27.1110283194281,76.4831388147606,
16.2626673994512));
#260045=CARTESIAN_POINT('Ctrl Pts',(-27.0602641873015,76.4497597899656,
16.1782706332977));
#260046=CARTESIAN_POINT('Ctrl Pts',(-27.0884790761337,76.4707669780906,
16.1906859326517));
#260047=CARTESIAN_POINT('Ctrl Pts',(-27.1178762326902,76.4900906769913,
16.2030845287967));
#260048=CARTESIAN_POINT('Ctrl Pts',(-27.0605327252718,76.4499596839005,
16.1760791918826));
#260049=CARTESIAN_POINT('Ctrl Pts',(-27.0898596110057,76.4718011937839,
16.1795821117081));
#260050=CARTESIAN_POINT('Ctrl Pts',(-27.120358948079,76.4919704112056,16.1830789607914));
#260051=CARTESIAN_POINT('Ctrl Pts',(-27.0602871265233,76.4497769572404,
16.1718015139879));
#260052=CARTESIAN_POINT('Ctrl Pts',(-27.0915502375945,76.473057377783,16.1610984554029));
#260053=CARTESIAN_POINT('Ctrl Pts',(-27.1242386851068,76.494295831555,16.150415767633));
#260054=CARTESIAN_POINT('Ctrl Pts',(-27.0598504162012,76.4494520710877,
16.1697479358136));
#260055=CARTESIAN_POINT('Ctrl Pts',(-27.0919480009677,76.4733461094145,
16.1535475368814));
#260056=CARTESIAN_POINT('Ctrl Pts',(-27.1257019179669,76.4948627285816,
16.137383211141));
#260057=CARTESIAN_POINT('Ctrl Pts',(-27.0582086402039,76.4482320673373,
16.1639666862077));
#260058=CARTESIAN_POINT('Ctrl Pts',(-27.0925161435607,76.4737375074722,
16.1338103699281));
#260059=CARTESIAN_POINT('Ctrl Pts',(-27.1291949135698,76.4958195376337,
16.1037499831074));
#260060=CARTESIAN_POINT('Ctrl Pts',(-27.0567042052342,76.4471157252128,
16.1606292110335));
#260061=CARTESIAN_POINT('Ctrl Pts',(-27.0921025230806,76.4733973732767,
16.1245076433474));
#260062=CARTESIAN_POINT('Ctrl Pts',(-27.1303768997729,76.495511080392,16.0885277310218));
#260063=CARTESIAN_POINT('Ctrl Pts',(-27.0534903168296,76.4447377920072,
16.1542190781187));
#260064=CARTESIAN_POINT('Ctrl Pts',(-27.0908610714654,76.4724034604763,
16.1076940433688));
#260065=CARTESIAN_POINT('Ctrl Pts',(-27.1320488746758,76.4944955999903,
16.0614128323374));
#260066=CARTESIAN_POINT('Ctrl Pts',(-27.0517739692635,76.4434708941462,
16.151235327988));
#260067=CARTESIAN_POINT('Ctrl Pts',(-27.089983151407,76.4717122955942,16.1006285062877));
#260068=CARTESIAN_POINT('Ctrl Pts',(-27.1324478121814,76.4937176499756,
16.0503186646554));
#260069=CARTESIAN_POINT('Ctrl Pts',(-27.0464903416048,76.4395819036986,
16.1426043113602));
#260070=CARTESIAN_POINT('Ctrl Pts',(-27.0870015822935,76.4693799219042,
16.0812344084128));
#260071=CARTESIAN_POINT('Ctrl Pts',(-27.1330005797391,76.4910613333798,
16.0203313765123));
#260072=CARTESIAN_POINT('Ctrl Pts',(-27.0427755268835,76.4368619767283,
16.1372659298901));
#260073=CARTESIAN_POINT('Ctrl Pts',(-27.0845393340012,76.4674716671333,
16.0707205771816));
#260074=CARTESIAN_POINT('Ctrl Pts',(-27.1325040255392,76.4888476730249,
16.0047512272665));
#260075=CARTESIAN_POINT('Ctrl Pts',(-26.9782305736964,76.38988746594,16.0488344459415));
#260076=CARTESIAN_POINT('Ctrl Pts',(-27.0392919375054,76.4326304782598,
15.9056407248496));
#260077=CARTESIAN_POINT('Ctrl Pts',(-27.1178463029269,76.4488518511461,
15.7660809748921));
#260078=CARTESIAN_POINT('Ctrl Pts',(-26.9009713153748,76.3379547637161,
16.0003561832371));
#260079=CARTESIAN_POINT('Ctrl Pts',(-26.9591175339555,76.3740242720092,
15.9620876053608));
#260080=CARTESIAN_POINT('Ctrl Pts',(-27.0253527090181,76.3877008594034,
15.9284160632215));
#260081=CARTESIAN_POINT('Ctrl Pts',(-26.8672868551547,76.3238925583658,
15.8466387166555));
#260082=CARTESIAN_POINT('Ctrl Pts',(-26.9411427646962,76.3705353343011,
15.3686915139899));
#260083=CARTESIAN_POINT('Ctrl Pts',(-27.0744152689117,76.3583349950857,
14.8796637100114));
#260084=CARTESIAN_POINT('Origin',(-24.9421491495268,74.7257085670769,17.0741173620444));
#260085=CARTESIAN_POINT('Ctrl Pts',(-25.2708374177665,75.9397262748117,
17.251852013646));
#260086=CARTESIAN_POINT('Ctrl Pts',(-25.2169363483573,75.9685632596837,
17.1547259853851));
#260087=CARTESIAN_POINT('Ctrl Pts',(-25.1589733721729,75.977209030354,17.0560474933636));
#260088=CARTESIAN_POINT('Ctrl Pts',(-25.2082186981158,75.9481612402803,
17.2973276043548));
#260089=CARTESIAN_POINT('Ctrl Pts',(-25.1530396514114,75.9759984326147,
17.2125718696916));
#260090=CARTESIAN_POINT('Ctrl Pts',(-25.0938856962957,75.9872898972941,
17.1266598670703));
#260091=CARTESIAN_POINT('Ctrl Pts',(-25.1496292031321,75.9580441982454,
17.3506767479114));
#260092=CARTESIAN_POINT('Ctrl Pts',(-25.0926862209603,75.9851307386431,
17.2798459583833));
#260093=CARTESIAN_POINT('Ctrl Pts',(-25.0322694075985,75.9990697411192,
17.2080611432671));
#260094=CARTESIAN_POINT('Ctrl Pts',(-25.1074704498864,75.9627753172623,
17.4259425795317));
#260095=CARTESIAN_POINT('Ctrl Pts',(-25.0462350072807,75.9901905947506,
17.3727027235389));
#260096=CARTESIAN_POINT('Ctrl Pts',(-24.9819025616059,76.0065414441447,
17.3185796118194));
#260097=CARTESIAN_POINT('Origin',(-24.7225971487503,74.7646897896784,17.2528005263547));
#260098=CARTESIAN_POINT('Ctrl Pts',(-25.1183452685167,75.961489026876,17.4075745924791));
#260099=CARTESIAN_POINT('Ctrl Pts',(-25.0581838218695,75.9888185880884,
17.3500764673617));
#260100=CARTESIAN_POINT('Ctrl Pts',(-24.9948448130137,76.0045572676605,
17.2916572676644));
#260101=CARTESIAN_POINT('Ctrl Pts',(-24.9827521037895,75.9867440840366,
17.55899212279));
#260102=CARTESIAN_POINT('Ctrl Pts',(-24.9436535528084,76.0047941374264,
17.5184791523466));
#260103=CARTESIAN_POINT('Ctrl Pts',(-24.9029090128894,76.0189046879127,
17.4779931990465));
#260104=CARTESIAN_POINT('Ctrl Pts',(-24.8422792694326,76.0138748889786,
17.7055224896539));
#260105=CARTESIAN_POINT('Ctrl Pts',(-24.8230534553004,76.0228272111476,
17.6845460983103));
#260106=CARTESIAN_POINT('Ctrl Pts',(-24.8038409415144,76.0317753894055,
17.6635683446243));
#260107=CARTESIAN_POINT('Ctrl Pts',(-24.6976449914381,76.042458286517,17.8479876926703));
#260108=CARTESIAN_POINT('Ctrl Pts',(-24.6976449914381,76.042458286517,17.8479876926703));
#260109=CARTESIAN_POINT('Ctrl Pts',(-24.6976449914381,76.042458286517,17.8479876926703));
#260110=CARTESIAN_POINT('Ctrl Pts',(-75.9418613633423,25.2552738568381,
17.2633930704886));
#260111=CARTESIAN_POINT('Ctrl Pts',(-75.9705307448155,25.2008887299308,
17.1691547678158));
#260112=CARTESIAN_POINT('Ctrl Pts',(-75.9798097533928,25.1424732627575,
17.073436084435));
#260113=CARTESIAN_POINT('Ctrl Pts',(-75.9205954929399,25.4077025358094,
17.1478651038322));
#260114=CARTESIAN_POINT('Ctrl Pts',(-75.9494543541835,25.3561156594532,
17.0372776844065));
#260115=CARTESIAN_POINT('Ctrl Pts',(-75.954463116562,25.3006469547484,16.9248602113907));
#260116=CARTESIAN_POINT('Ctrl Pts',(-75.9109616438354,25.5755944946747,
17.0670794578486));
#260117=CARTESIAN_POINT('Ctrl Pts',(-75.9415927766753,25.5249041770603,
16.942644169398));
#260118=CARTESIAN_POINT('Ctrl Pts',(-75.9428621479078,25.4713720494591,
16.8155375287585));
#260119=CARTESIAN_POINT('Ctrl Pts',(-75.9275280255483,25.9210527955289,
16.9292448759623));
#260120=CARTESIAN_POINT('Ctrl Pts',(-75.9624784012936,25.8696848744371,
16.7793350248215));
#260121=CARTESIAN_POINT('Ctrl Pts',(-75.9568220105354,25.8203898867078,
16.6247659603065));
#260122=CARTESIAN_POINT('Ctrl Pts',(-75.9538339499128,26.1003508790234,
16.8739158933932));
#260123=CARTESIAN_POINT('Ctrl Pts',(-75.9915111973655,26.0474451773173,
16.71236748428));
#260124=CARTESIAN_POINT('Ctrl Pts',(-75.9826073212052,26.0003738093527,
16.5448970501221));
#260125=CARTESIAN_POINT('Ctrl Pts',(-76.043689910258,26.4483576685996,16.7801350408706));
#260126=CARTESIAN_POINT('Ctrl Pts',(-76.0861927069939,26.3907804446495,
16.5979420070057));
#260127=CARTESIAN_POINT('Ctrl Pts',(-76.0719406400684,26.3490777035775,
16.4071746837876));
#260128=CARTESIAN_POINT('Ctrl Pts',(-76.1074179294937,26.620988024866,16.7422284473806));
#260129=CARTESIAN_POINT('Ctrl Pts',(-76.1524784685812,26.5598106931415,
16.5503025518547));
#260130=CARTESIAN_POINT('Ctrl Pts',(-76.1359757159749,26.5213000181803,
16.3481386613362));
#260131=CARTESIAN_POINT('Ctrl Pts',(-76.2123121583599,26.8247483133817,
16.6934782675186));
#260132=CARTESIAN_POINT('Ctrl Pts',(-76.2573797435207,26.7604927914798,
16.4945259476778));
#260133=CARTESIAN_POINT('Ctrl Pts',(-76.2394515594669,26.7269907489909,
16.2840525403652));
#260134=CARTESIAN_POINT('Ctrl Pts',(-76.2345275940666,26.8648052287403,
16.683596110921));
#260135=CARTESIAN_POINT('Ctrl Pts',(-76.2794248197493,26.8000483509318,
16.4835331192511));
#260136=CARTESIAN_POINT('Ctrl Pts',(-76.2612732322625,26.7675833243841,
16.271750775101));
#260137=CARTESIAN_POINT('Ctrl Pts',(-76.2819273824524,26.9428805656769,
16.6613225028887));
#260138=CARTESIAN_POINT('Ctrl Pts',(-76.3255632280466,26.8778793003309,
16.4606019828592));
#260139=CARTESIAN_POINT('Ctrl Pts',(-76.3071781559159,26.8476587910104,
16.2480755374178));
#260140=CARTESIAN_POINT('Ctrl Pts',(-76.3069759166525,26.9810543502174,
16.6496028712566));
#260141=CARTESIAN_POINT('Ctrl Pts',(-76.3496541916651,26.9161447810771,
16.4490365803292));
#260142=CARTESIAN_POINT('Ctrl Pts',(-76.3312621827901,26.887142831161,16.2367104776612));
#260143=CARTESIAN_POINT('Ctrl Pts',(-76.3484797871886,27.0347146146424,
16.6221367327725));
#260144=CARTESIAN_POINT('Ctrl Pts',(-76.3871516364481,26.9723508665169,
16.4265743967641));
#260145=CARTESIAN_POINT('Ctrl Pts',(-76.3690988044595,26.9455078882792,
16.2202180012282));
#260146=CARTESIAN_POINT('Ctrl Pts',(-76.362903314126,27.0520461010359,16.6116902389491));
#260147=CARTESIAN_POINT('Ctrl Pts',(-76.399860448142,26.9908608801288,16.4184344514163));
#260148=CARTESIAN_POINT('Ctrl Pts',(-76.3819923354247,26.964812643049,16.2148188442204));
#260149=CARTESIAN_POINT('Ctrl Pts',(-76.3870229007013,27.0754324956906,
16.5857176723783));
#260150=CARTESIAN_POINT('Ctrl Pts',(-76.4190969025662,27.0181216724747,
16.4007390401198));
#260151=CARTESIAN_POINT('Ctrl Pts',(-76.4017200269266,26.9934903445586,
16.2067761581036));
#260152=CARTESIAN_POINT('Ctrl Pts',(-76.3954507470092,27.0828077996898,
16.5755244414213));
#260153=CARTESIAN_POINT('Ctrl Pts',(-76.4255297302771,27.0271132434182,
16.3940294300836));
#260154=CARTESIAN_POINT('Ctrl Pts',(-76.4083620212357,27.0030053344321,
16.2041055763287));
#260155=CARTESIAN_POINT('Ctrl Pts',(-76.4098047654361,27.0922320376552,
16.5516204721224));
#260156=CARTESIAN_POINT('Ctrl Pts',(-76.4351714897886,27.0404202191174,
16.3794012893797));
#260157=CARTESIAN_POINT('Ctrl Pts',(-76.4184188459322,27.0172039742048,
16.2000478703811));
#260158=CARTESIAN_POINT('Ctrl Pts',(-76.4148733708259,27.0950953264236,
16.542241373224));
#260159=CARTESIAN_POINT('Ctrl Pts',(-76.4383794519954,27.0448194425868,
16.3737834007286));
#260160=CARTESIAN_POINT('Ctrl Pts',(-76.4217869746101,27.0219248435745,
16.1986868469487));
#260161=CARTESIAN_POINT('Ctrl Pts',(-76.4263249193091,27.0997431526797,
16.5161165141982));
#260162=CARTESIAN_POINT('Ctrl Pts',(-76.4447880196842,27.0535589891232,
16.3586891567135));
#260163=CARTESIAN_POINT('Ctrl Pts',(-76.4285499486556,27.0313357366994,
16.1959025863163));
#260164=CARTESIAN_POINT('Ctrl Pts',(-76.4326137594215,27.1014904674059,
16.5002045800054));
#260165=CARTESIAN_POINT('Ctrl Pts',(-76.4479608116379,27.0578613485225,
16.3496496068196));
#260166=CARTESIAN_POINT('Ctrl Pts',(-76.4319458773626,27.036027204956,16.194493130941));
#260167=CARTESIAN_POINT('Ctrl Pts',(-76.4449452653173,27.1026704184048,
16.4573094494898));
#260168=CARTESIAN_POINT('Ctrl Pts',(-76.4528888389789,27.0645218853297,
16.3262587915595));
#260169=CARTESIAN_POINT('Ctrl Pts',(-76.4370430684111,27.0430187136298,
16.1921727274436));
#260170=CARTESIAN_POINT('Ctrl Pts',(-76.4496135704622,27.1027728684425,
16.4393960541631));
#260171=CARTESIAN_POINT('Ctrl Pts',(-76.4545588311619,27.0667761709923,
16.3166145530677));
#260172=CARTESIAN_POINT('Ctrl Pts',(-76.4387449966536,27.045344739669,16.1913678957922));
#260173=CARTESIAN_POINT('Ctrl Pts',(-76.4602856539487,27.1033488438057,
16.3918070921552));
#260174=CARTESIAN_POINT('Ctrl Pts',(-76.458215438751,27.0717039880843,16.2913313756112));
#260175=CARTESIAN_POINT('Ctrl Pts',(-76.4421210567288,27.0499425769547,
16.1895073884942));
#260176=CARTESIAN_POINT('Ctrl Pts',(-76.4662567117745,27.1039219568828,
16.3621450322986));
#260177=CARTESIAN_POINT('Ctrl Pts',(-76.4602223544582,27.0744045251034,
16.2757393349363));
#260178=CARTESIAN_POINT('Ctrl Pts',(-76.4437985416506,27.0522188526216,
16.188486160607));
#260179=CARTESIAN_POINT('Ctrl Pts',(-76.4780100141095,27.1079500471749,
16.2949622535397));
#260180=CARTESIAN_POINT('Ctrl Pts',(-76.464859856734,27.080614764543,16.2402952662867));
#260181=CARTESIAN_POINT('Ctrl Pts',(-76.4470294934426,27.0565887317523,
16.1854024533813));
#260182=CARTESIAN_POINT('Ctrl Pts',(-76.4840868539133,27.1117437396586,
16.2559882666882));
#260183=CARTESIAN_POINT('Ctrl Pts',(-76.467704925846,27.0844038678372,16.2196740425616));
#260184=CARTESIAN_POINT('Ctrl Pts',(-76.4487367623946,27.0588881357365,
16.1832703333258));
#260185=CARTESIAN_POINT('Ctrl Pts',(-76.4907257277775,27.1186429162657,
16.1967720341265));
#260186=CARTESIAN_POINT('Ctrl Pts',(-76.4711520289686,27.0890007529114,
16.1872234031905));
#260187=CARTESIAN_POINT('Ctrl Pts',(-76.4499409067105,27.0605075183523,
16.1776626753881));
#260188=CARTESIAN_POINT('Ctrl Pts',(-76.4924398017457,27.1210505518387,
16.1773616860606));
#260189=CARTESIAN_POINT('Ctrl Pts',(-76.4721011935177,27.0902693498065,
16.1763784271835));
#260190=CARTESIAN_POINT('Ctrl Pts',(-76.4500665941387,27.0606763157615,
16.1753930502819));
#260191=CARTESIAN_POINT('Ctrl Pts',(-76.4945108031758,27.1247236922628,
16.1461844913689));
#260192=CARTESIAN_POINT('Ctrl Pts',(-76.4732172840265,27.0917769536449,
16.1586351423791));
#260193=CARTESIAN_POINT('Ctrl Pts',(-76.4497968134883,27.060313707542,16.1711106500328));
#260194=CARTESIAN_POINT('Ctrl Pts',(-76.4950020357304,27.126103162898,16.1336817286145));
#260195=CARTESIAN_POINT('Ctrl Pts',(-76.4734595694155,27.0921151050378,
16.1513535959096));
#260196=CARTESIAN_POINT('Ctrl Pts',(-76.4494485206262,27.0598455093621,
16.1690666806019));
#260197=CARTESIAN_POINT('Ctrl Pts',(-76.4963255984212,27.1315681998314,
16.0800932837505));
#260198=CARTESIAN_POINT('Ctrl Pts',(-76.4739479072672,27.0928528473111,
16.1197524270407));
#260199=CARTESIAN_POINT('Ctrl Pts',(-76.4473649309662,27.0570414552056,
16.1595639629175));
#260200=CARTESIAN_POINT('Ctrl Pts',(-76.4945113000399,27.1323195784954,
16.0589082957826));
#260201=CARTESIAN_POINT('Ctrl Pts',(-76.4724555516724,27.0909630625156,
16.1060937855057));
#260202=CARTESIAN_POINT('Ctrl Pts',(-76.4447337452728,27.0534894962345,
16.1535331468431));
#260203=CARTESIAN_POINT('Ctrl Pts',(-76.4909539904122,27.1329837771628,
16.019511465123));
#260204=CARTESIAN_POINT('Ctrl Pts',(-76.4693349255398,27.0869835291923,
16.0805518203704));
#260205=CARTESIAN_POINT('Ctrl Pts',(-76.4395769622165,27.0464831294603,
16.1420634614074));
#260206=CARTESIAN_POINT('Ctrl Pts',(-76.4887423766881,27.1324755596788,
16.0040405252692));
#260207=CARTESIAN_POINT('Ctrl Pts',(-76.4674273552134,27.0845268268888,
16.0700931629596));
#260208=CARTESIAN_POINT('Ctrl Pts',(-76.4368678681646,27.0427830918246,
16.1367256935079));
#260209=CARTESIAN_POINT('Ctrl Pts',(-76.4487554850644,27.1176445692895,
15.7668594205398));
#260210=CARTESIAN_POINT('Ctrl Pts',(-76.432579761112,27.0393448518373,15.9057514243235));
#260211=CARTESIAN_POINT('Ctrl Pts',(-76.3900305449946,26.9784271091622,
16.0482566941911));
#260212=CARTESIAN_POINT('Ctrl Pts',(-76.3890441685912,27.0267181004289,
15.9290103437534));
#260213=CARTESIAN_POINT('Ctrl Pts',(-76.3752488344031,26.960842696207,15.9631202761283));
#260214=CARTESIAN_POINT('Ctrl Pts',(-76.3393326181439,26.9029431213673,
16.0017769419879));
#260215=CARTESIAN_POINT('Ctrl Pts',(-76.353597569064,27.0702645546813,14.8756002316582));
#260216=CARTESIAN_POINT('Ctrl Pts',(-76.3662576106953,26.9359672642415,
15.3622372916713));
#260217=CARTESIAN_POINT('Ctrl Pts',(-76.3195417069851,26.8613991063355,
15.838576931848));
#260218=CARTESIAN_POINT('Origin',(-74.7257085670769,24.9421491495265,17.0741173620445));
#260219=CARTESIAN_POINT('Ctrl Pts',(-75.9627753172452,25.1074704499294,
17.4259425795553));
#260220=CARTESIAN_POINT('Ctrl Pts',(-75.9901905947509,25.0462350073013,
17.3727027235441));
#260221=CARTESIAN_POINT('Ctrl Pts',(-76.0065414441465,24.9819025616011,
17.3185796118072));
#260222=CARTESIAN_POINT('Ctrl Pts',(-75.9580441983129,25.1496292029441,
17.3506767478586));
#260223=CARTESIAN_POINT('Ctrl Pts',(-75.9851307386898,25.0926862207585,
17.2798459583165));
#260224=CARTESIAN_POINT('Ctrl Pts',(-75.9990697411671,25.0322694073851,
17.2080611431797));
#260225=CARTESIAN_POINT('Ctrl Pts',(-75.9481612402487,25.2082186982314,
17.2973276043539));
#260226=CARTESIAN_POINT('Ctrl Pts',(-75.9759984326013,25.1530396514968,
17.212571869659));
#260227=CARTESIAN_POINT('Ctrl Pts',(-75.9872898972843,25.0938856963526,
17.1266598670131));
#260228=CARTESIAN_POINT('Ctrl Pts',(-75.9397262748186,25.2708374177395,
17.2518520136476));
#260229=CARTESIAN_POINT('Ctrl Pts',(-75.9685632596988,25.2169363483151,
17.1547259853546));
#260230=CARTESIAN_POINT('Ctrl Pts',(-75.9772090303636,25.1589733721118,
17.0560474932984));
#260231=CARTESIAN_POINT('Origin',(-74.7646897896797,24.7225971487431,17.2528005263626));
#260232=CARTESIAN_POINT('Ctrl Pts',(-76.0045572676614,24.9948448130087,
17.2916572676744));
#260233=CARTESIAN_POINT('Ctrl Pts',(-75.9888185880893,25.0581838218632,
17.3500764673707));
#260234=CARTESIAN_POINT('Ctrl Pts',(-75.9614890268774,25.1183452685092,
17.4075745924872));
#260235=CARTESIAN_POINT('Ctrl Pts',(-76.0189046879213,24.9029090128515,
17.4779931990339));
#260236=CARTESIAN_POINT('Ctrl Pts',(-76.0047941374461,24.9436535527978,
17.5184791523175));
#260237=CARTESIAN_POINT('Ctrl Pts',(-75.9867440840532,24.9827521037523,
17.5589921227563));
#260238=CARTESIAN_POINT('Ctrl Pts',(-76.0317753893929,24.8038409415446,
17.6635683446451));
#260239=CARTESIAN_POINT('Ctrl Pts',(-76.0228272111303,24.8230534553329,
17.6845460983615));
#260240=CARTESIAN_POINT('Ctrl Pts',(-76.0138748889535,24.8422792694848,
17.7055224897174));
#260241=CARTESIAN_POINT('Ctrl Pts',(-76.0424582865173,24.6976449914384,
17.8479876926675));
#260242=CARTESIAN_POINT('Ctrl Pts',(-76.0424582865173,24.6976449914384,
17.8479876926675));
#260243=CARTESIAN_POINT('Ctrl Pts',(-76.0424582865173,24.6976449914384,
17.8479876926675));
#260244=CARTESIAN_POINT('Ctrl Pts',(-75.9797580906608,-25.1427975233705,
17.073967452658));
#260245=CARTESIAN_POINT('Ctrl Pts',(-75.9704505449959,-25.2010408670593,
17.1694183903461));
#260246=CARTESIAN_POINT('Ctrl Pts',(-75.9418613633423,-25.2552738568381,
17.2633930704886));
#260247=CARTESIAN_POINT('Ctrl Pts',(-75.9544312451061,-25.3009789767176,
16.9254608534837));
#260248=CARTESIAN_POINT('Ctrl Pts',(-75.9493702728614,-25.3562842637719,
17.0375667811434));
#260249=CARTESIAN_POINT('Ctrl Pts',(-75.9205921485561,-25.4077265047638,
17.1478469399056));
#260250=CARTESIAN_POINT('Ctrl Pts',(-75.9428615286961,-25.4716594454445,
16.8162542379909));
#260251=CARTESIAN_POINT('Ctrl Pts',(-75.9415132164522,-25.5250369424895,
16.9430041875803));
#260252=CARTESIAN_POINT('Ctrl Pts',(-75.9109678945307,-25.5755858398725,
17.0670893643824));
#260253=CARTESIAN_POINT('Ctrl Pts',(-75.956838159693,-25.8204679631934,
16.6257193108577));
#260254=CARTESIAN_POINT('Ctrl Pts',(-75.962361720977,-25.869636826486,16.7798402976816));
#260255=CARTESIAN_POINT('Ctrl Pts',(-75.9275121102471,-25.9208598333928,
16.929315416431));
#260256=CARTESIAN_POINT('Ctrl Pts',(-75.9826370080728,-26.0005181671523,
16.5458722711726));
#260257=CARTESIAN_POINT('Ctrl Pts',(-75.991384088087,-26.0474798054162,
16.7128641318258));
#260258=CARTESIAN_POINT('Ctrl Pts',(-75.9538145400774,-26.1002356629363,
16.8739507927146));
#260259=CARTESIAN_POINT('Ctrl Pts',(-76.0719664887017,-26.3491447856912,
16.408284820677));
#260260=CARTESIAN_POINT('Ctrl Pts',(-76.0860184034591,-26.3907826882672,
16.5985046605215));
#260261=CARTESIAN_POINT('Ctrl Pts',(-76.043637588925,-26.4481950421709,
16.7801750176051));
#260262=CARTESIAN_POINT('Ctrl Pts',(-76.1358706771697,-26.5210561310895,
16.349401056146));
#260263=CARTESIAN_POINT('Ctrl Pts',(-76.152151115887,-26.5595368821915,
16.550967028566));
#260264=CARTESIAN_POINT('Ctrl Pts',(-76.1072227619321,-26.6205318969174,
16.7423277264094));
#260265=CARTESIAN_POINT('Ctrl Pts',(-76.2393631100495,-26.7268213040049,
16.2853173372501));
#260266=CARTESIAN_POINT('Ctrl Pts',(-76.257063787892,-26.7603293208145,
16.495184288063));
#260267=CARTESIAN_POINT('Ctrl Pts',(-76.2121224138048,-26.8243988715869,
16.6935643210242));
#260268=CARTESIAN_POINT('Ctrl Pts',(-76.2611833023277,-26.7674174132351,
16.2730180591461));
#260269=CARTESIAN_POINT('Ctrl Pts',(-76.2791071179994,-26.7998957670328,
16.4841930682975));
#260270=CARTESIAN_POINT('Ctrl Pts',(-76.2343342585777,-26.8644662404173,
16.6836830236006));
#260271=CARTESIAN_POINT('Ctrl Pts',(-76.3070716523925,-26.8474785038813,
16.2493440730816));
#260272=CARTESIAN_POINT('Ctrl Pts',(-76.3252324890958,-26.8777267177194,
16.4612725591729));
#260273=CARTESIAN_POINT('Ctrl Pts',(-76.2817116074213,-26.9425455041864,
16.6614278009669));
#260274=CARTESIAN_POINT('Ctrl Pts',(-76.3311405493927,-26.8869445368854,
16.2379796218529));
#260275=CARTESIAN_POINT('Ctrl Pts',(-76.3493117166703,-26.9159817137041,
16.4497126498075));
#260276=CARTESIAN_POINT('Ctrl Pts',(-76.3067428834464,-26.980710969085,
16.6497176781945));
#260277=CARTESIAN_POINT('Ctrl Pts',(-76.3689406638797,-26.945266929949,
16.2214623761187));
#260278=CARTESIAN_POINT('Ctrl Pts',(-76.3867886098726,-26.972153594934,
16.4272903747554));
#260279=CARTESIAN_POINT('Ctrl Pts',(-76.34819258934,-27.0343640364953,16.6223462082648));
#260280=CARTESIAN_POINT('Ctrl Pts',(-76.3818296697896,-26.9645699757353,
16.2160473363937));
#260281=CARTESIAN_POINT('Ctrl Pts',(-76.3994999566085,-26.9906641344935,
16.4191597276068));
#260282=CARTESIAN_POINT('Ctrl Pts',(-76.3626055736382,-27.0517070229519,
16.6119303419184));
#260283=CARTESIAN_POINT('Ctrl Pts',(-76.4015511235838,-26.9932458782157,
16.2079521753699));
#260284=CARTESIAN_POINT('Ctrl Pts',(-76.4187497306501,-27.0179231387113,
16.4015240394823));
#260285=CARTESIAN_POINT('Ctrl Pts',(-76.3866896921813,-27.075133854949,
16.586115527268));
#260286=CARTESIAN_POINT('Ctrl Pts',(-76.4081904188892,-27.0027594180855,
16.2052600005569));
#260287=CARTESIAN_POINT('Ctrl Pts',(-76.4251880251479,-27.0269131016926,
16.394838476637));
#260288=CARTESIAN_POINT('Ctrl Pts',(-76.3951028734164,-27.0825251276998,
16.5759864003958));
#260289=CARTESIAN_POINT('Ctrl Pts',(-76.4182420489946,-27.0169544485405,
16.2011478343014));
#260290=CARTESIAN_POINT('Ctrl Pts',(-76.4348428493639,-27.0402133489551,
16.3803198781631));
#260291=CARTESIAN_POINT('Ctrl Pts',(-76.4094060150498,-27.0919957504364,
16.5523396960077));
#260292=CARTESIAN_POINT('Ctrl Pts',(-76.4216080672702,-27.0216736152669,
16.199765076445));
#260293=CARTESIAN_POINT('Ctrl Pts',(-76.4380559634305,-27.044609595188,
16.3747494976438));
#260294=CARTESIAN_POINT('Ctrl Pts',(-76.4144529142496,-27.0948782508066,
16.5430709365392));
#260295=CARTESIAN_POINT('Ctrl Pts',(-76.4283671919628,-27.0310817132732,
16.1969190323981));
#260296=CARTESIAN_POINT('Ctrl Pts',(-76.4444782315775,-27.0533397410452,
16.3598436849778));
#260297=CARTESIAN_POINT('Ctrl Pts',(-76.4258296207998,-27.0995848867389,
16.5173659028209));
#260298=CARTESIAN_POINT('Ctrl Pts',(-76.4317613407867,-27.0357720446273,
16.1954706757853));
#260299=CARTESIAN_POINT('Ctrl Pts',(-76.447661611145,-27.0576387022135,
16.3509299496292));
#260300=CARTESIAN_POINT('Ctrl Pts',(-76.4320671439904,-27.1013790750866,
16.5017321165198));
#260301=CARTESIAN_POINT('Ctrl Pts',(-76.436859866445,-27.0427673796964,
16.1930500015502));
#260302=CARTESIAN_POINT('Ctrl Pts',(-76.4526000023644,-27.0642714137363,
16.3280456162467));
#260303=CARTESIAN_POINT('Ctrl Pts',(-76.4442399817405,-27.1026290071146,
16.45992784308));
#260304=CARTESIAN_POINT('Ctrl Pts',(-76.4385621324104,-27.045094548124,
16.1922036321779));
#260305=CARTESIAN_POINT('Ctrl Pts',(-76.4542712961586,-27.0665105524591,
16.3186472465446));
#260306=CARTESIAN_POINT('Ctrl Pts',(-76.4488339552935,-27.1027558331057,
16.4425406130888));
#260307=CARTESIAN_POINT('Ctrl Pts',(-76.4419441675585,-27.0497018479052,
16.1902449666111));
#260308=CARTESIAN_POINT('Ctrl Pts',(-76.4579141594516,-27.0713822986317,
16.2938988063911));
#260309=CARTESIAN_POINT('Ctrl Pts',(-76.4593812236218,-27.1032790990182,
16.3961238394874));
#260310=CARTESIAN_POINT('Ctrl Pts',(-76.4436315420317,-27.0519922188866,
16.1891611954603));
#260311=CARTESIAN_POINT('Ctrl Pts',(-76.4599107853122,-27.0740487753853,
16.2784857984419));
#260312=CARTESIAN_POINT('Ctrl Pts',(-76.4653396439829,-27.1037600537445,
16.3668981633898));
#260313=CARTESIAN_POINT('Ctrl Pts',(-76.4468920465821,-27.0564031404483,
16.1860061090073));
#260314=CARTESIAN_POINT('Ctrl Pts',(-76.4645195023081,-27.0801893738403,
16.2433248387421));
#260315=CARTESIAN_POINT('Ctrl Pts',(-76.4771343917457,-27.1075193467349,
16.300387443764));
#260316=CARTESIAN_POINT('Ctrl Pts',(-76.4485949814437,-27.0586973262713,
16.183947451681));
#260317=CARTESIAN_POINT('Ctrl Pts',(-76.4672853182553,-27.0838623506706,
16.2233603028531));
#260318=CARTESIAN_POINT('Ctrl Pts',(-76.4831388228296,-27.1110283253036,
16.2626673435081));
#260319=CARTESIAN_POINT('Ctrl Pts',(-76.4499684765458,-27.0605445606376,
16.1783939855022));
#260320=CARTESIAN_POINT('Ctrl Pts',(-76.4708630581003,-27.0886252421466,
16.1907475480153));
#260321=CARTESIAN_POINT('Ctrl Pts',(-76.4900906826273,-27.1178762392995,
16.2030844742334));
#260322=CARTESIAN_POINT('Ctrl Pts',(-76.4501766603085,-27.060824146804,
16.1761139907089));
#260323=CARTESIAN_POINT('Ctrl Pts',(-76.4719014767742,-27.0900112557936,
16.1795994700338));
#260324=CARTESIAN_POINT('Ctrl Pts',(-76.4919704154291,-27.120358954105,
16.1830789111177));
#260325=CARTESIAN_POINT('Ctrl Pts',(-76.4500082006625,-27.0605977646083,
16.171695172017));
#260326=CARTESIAN_POINT('Ctrl Pts',(-76.4731629849128,-27.0917127790436,
16.1610453142631));
#260327=CARTESIAN_POINT('Ctrl Pts',(-76.4942958336546,-27.1242386896308,
16.1504157284619));
#260328=CARTESIAN_POINT('Ctrl Pts',(-76.4496893833318,-27.0601693247177,
16.1695869905218));
#260329=CARTESIAN_POINT('Ctrl Pts',(-76.4734531078006,-27.0921158531867,
16.1534671350758));
#260330=CARTESIAN_POINT('Ctrl Pts',(-76.4948627299487,-27.1257019217084,
16.1373831769476));
#260331=CARTESIAN_POINT('Ctrl Pts',(-76.4484852990103,-27.0585494357892,
16.1636671740135));
#260332=CARTESIAN_POINT('Ctrl Pts',(-76.4738473436354,-27.0926985841542,
16.1336608349858));
#260333=CARTESIAN_POINT('Ctrl Pts',(-76.495819537497,-27.1291949155818,
16.1037499599793));
#260334=CARTESIAN_POINT('Ctrl Pts',(-76.4473766016455,-27.0570557850954,
16.1602705170287));
#260335=CARTESIAN_POINT('Ctrl Pts',(-76.4735073861303,-27.0922929334494,
16.1243286343765));
#260336=CARTESIAN_POINT('Ctrl Pts',(-76.4955110799672,-27.1303769013237,
16.0885277102575));
#260337=CARTESIAN_POINT('Ctrl Pts',(-76.4450122863737,-27.0538613837634,
16.1537572314779));
#260338=CARTESIAN_POINT('Ctrl Pts',(-76.4725134018884,-27.0910660428777,
16.1074637130129));
#260339=CARTESIAN_POINT('Ctrl Pts',(-76.4944955990249,-27.1320488754092,
16.0614128160212));
#260340=CARTESIAN_POINT('Ctrl Pts',(-76.4437510438076,-27.0521533110402,
16.1507330414467));
#260341=CARTESIAN_POINT('Ctrl Pts',(-76.4718218219973,-27.0901945097804,
16.100378089317));
#260342=CARTESIAN_POINT('Ctrl Pts',(-76.4937176488737,-27.132447812647,
16.0503186498413));
#260343=CARTESIAN_POINT('Ctrl Pts',(-76.4398773268223,-27.0468923857308,
16.1419954697044));
#260344=CARTESIAN_POINT('Ctrl Pts',(-76.4694878830294,-27.0872306322465,
16.0809311346633));
#260345=CARTESIAN_POINT('Ctrl Pts',(-76.4910613319352,-27.1330005795651,
16.0203313649665));
#260346=CARTESIAN_POINT('Ctrl Pts',(-76.4371653460925,-27.043189907853,
16.1366059166316));
#260347=CARTESIAN_POINT('Ctrl Pts',(-76.4675781349584,-27.0847782338116,
16.0703919912701));
#260348=CARTESIAN_POINT('Ctrl Pts',(-76.4888476714809,-27.132504025135,
16.0047512167351));
#260349=CARTESIAN_POINT('Ctrl Pts',(-76.3903090358906,-26.9788341835779,
16.047420025793));
#260350=CARTESIAN_POINT('Ctrl Pts',(-76.4327115984196,-27.0396847828042,
15.9049427900151));
#260351=CARTESIAN_POINT('Ctrl Pts',(-76.4488518482171,-27.1178462992563,
15.7660809785745));
#260352=CARTESIAN_POINT('Ctrl Pts',(-76.3383110453087,-26.9015467539818,
15.9999776993634));
#260353=CARTESIAN_POINT('Ctrl Pts',(-76.3740925666315,-26.9594482821516,
15.9619194428568));
#260354=CARTESIAN_POINT('Ctrl Pts',(-76.3877008591798,-27.0253527112511,
15.9284160251555));
#260355=CARTESIAN_POINT('Ctrl Pts',(-76.324348131815,-26.8680119970124,
15.8419552498495));
#260356=CARTESIAN_POINT('Ctrl Pts',(-76.3704738204621,-26.9418146644021,
15.3662261076973));
#260357=CARTESIAN_POINT('Ctrl Pts',(-76.3583349938827,-27.0744152558263,
14.8796638553843));
#260358=CARTESIAN_POINT('Origin',(-74.7257085670769,-24.9421491495267,17.0741173620445));
#260359=CARTESIAN_POINT('Ctrl Pts',(-75.9397262748104,-25.2708374177706,
17.2518520136472));
#260360=CARTESIAN_POINT('Ctrl Pts',(-75.9685632596807,-25.2169363483673,
17.1547259853961));
#260361=CARTESIAN_POINT('Ctrl Pts',(-75.9772090303525,-25.1589733721825,
17.0560474933749));
#260362=CARTESIAN_POINT('Ctrl Pts',(-75.9481612402858,-25.2082186980985,
17.2973276043494));
#260363=CARTESIAN_POINT('Ctrl Pts',(-75.9759984326193,-25.1530396513852,
17.2125718696724));
#260364=CARTESIAN_POINT('Ctrl Pts',(-75.9872898972957,-25.0938856962862,
17.1266598670748));
#260365=CARTESIAN_POINT('Ctrl Pts',(-75.9580441982361,-25.1496292031562,
17.3506767479224));
#260366=CARTESIAN_POINT('Ctrl Pts',(-75.9851307386312,-25.0926862209931,
17.2798459584101));
#260367=CARTESIAN_POINT('Ctrl Pts',(-75.9990697411128,-25.0322694076272,
17.2080611432832));
#260368=CARTESIAN_POINT('Ctrl Pts',(-75.9627753172647,-25.1074704498802,
17.4259425795287));
#260369=CARTESIAN_POINT('Ctrl Pts',(-75.990190594752,-25.0462350072764,
17.3727027235357));
#260370=CARTESIAN_POINT('Ctrl Pts',(-76.0065414441443,-24.9819025616068,
17.3185796118225));
#260371=CARTESIAN_POINT('Origin',(-74.7646897896784,-24.7225971487503,17.2528005263547));
#260372=CARTESIAN_POINT('Ctrl Pts',(-75.961489026876,-25.1183452685166,
17.4075745924789));
#260373=CARTESIAN_POINT('Ctrl Pts',(-75.9888185880884,-25.0581838218695,
17.3500764673615));
#260374=CARTESIAN_POINT('Ctrl Pts',(-76.0045572676606,-24.9948448130137,
17.2916572676642));
#260375=CARTESIAN_POINT('Ctrl Pts',(-75.9867440840261,-24.9827521038113,
17.5589921228149));
#260376=CARTESIAN_POINT('Ctrl Pts',(-76.0047941374114,-24.9436535528488,
17.5184791523768));
#260377=CARTESIAN_POINT('Ctrl Pts',(-76.0189046879073,-24.9029090129121,
17.4779931990604));
#260378=CARTESIAN_POINT('Ctrl Pts',(-76.0138748889937,-24.8422792694005,
17.7055224896176));
#260379=CARTESIAN_POINT('Ctrl Pts',(-76.022827211163,-24.823053455264,17.6845460982823));
#260380=CARTESIAN_POINT('Ctrl Pts',(-76.0317753894186,-24.803840941482,
17.6635683446042));
#260381=CARTESIAN_POINT('Ctrl Pts',(-76.042458286517,-24.6976449914381,
17.8479876926702));
#260382=CARTESIAN_POINT('Ctrl Pts',(-76.042458286517,-24.6976449914381,
17.8479876926702));
#260383=CARTESIAN_POINT('Ctrl Pts',(-76.042458286517,-24.6976449914381,
17.8479876926702));
#260384=CARTESIAN_POINT('Ctrl Pts',(-25.0804618860071,-75.9725615368863,
17.4201668781018));
#260385=CARTESIAN_POINT('Ctrl Pts',(-25.0218849778562,-76.0018311057342,
17.3465486622735));
#260386=CARTESIAN_POINT('Ctrl Pts',(-24.9591222046954,-76.0165443120349,
17.2720397183493));
#260387=CARTESIAN_POINT('Ctrl Pts',(-25.2741629194232,-75.9311692985899,
17.2143925575073));
#260388=CARTESIAN_POINT('Ctrl Pts',(-25.2217620984046,-75.958681184649,
17.1148633561065));
#260389=CARTESIAN_POINT('Ctrl Pts',(-25.164555452101,-75.9667333080832,
17.0143457048175));
#260390=CARTESIAN_POINT('Ctrl Pts',(-25.5065028345047,-75.9076483674931,
17.0946463742245));
#260391=CARTESIAN_POINT('Ctrl Pts',(-25.4560812233242,-75.9374572719603,
16.975096473616));
#260392=CARTESIAN_POINT('Ctrl Pts',(-25.4014568018213,-75.940075439265,
16.8534468191097));
#260393=CARTESIAN_POINT('Ctrl Pts',(-25.9210527955286,-75.9275280255481,
16.9292448759631));
#260394=CARTESIAN_POINT('Ctrl Pts',(-25.869632234831,-75.9625142169128,
16.779181403744));
#260395=CARTESIAN_POINT('Ctrl Pts',(-25.8202904741286,-75.9568105611577,
16.6244542312956));
#260396=CARTESIAN_POINT('Ctrl Pts',(-26.1003508790253,-75.9538339499116,
16.8739158933986));
#260397=CARTESIAN_POINT('Ctrl Pts',(-26.0473908953036,-75.9915498547682,
16.712201733282));
#260398=CARTESIAN_POINT('Ctrl Pts',(-26.0002790025707,-75.9825893385704,
16.5445597191471));
#260399=CARTESIAN_POINT('Ctrl Pts',(-26.4483576685983,-76.0436899102593,
16.780135040865));
#260400=CARTESIAN_POINT('Ctrl Pts',(-26.3907212263427,-76.0862364212154,
16.5977546210492));
#260401=CARTESIAN_POINT('Ctrl Pts',(-26.348993925881,-76.0719119444786,
16.4067913625623));
#260402=CARTESIAN_POINT('Ctrl Pts',(-26.6209880248636,-76.1074179294954,
16.7422284473727));
#260403=CARTESIAN_POINT('Ctrl Pts',(-26.5597476890932,-76.1525248745973,
16.5501048951729));
#260404=CARTESIAN_POINT('Ctrl Pts',(-26.5212227642732,-76.1359425371645,
16.347732979202));
#260405=CARTESIAN_POINT('Ctrl Pts',(-26.8247483133827,-76.2123121583597,
16.6934782675206));
#260406=CARTESIAN_POINT('Ctrl Pts',(-26.7604265541758,-76.2574262010907,
16.4943208592278));
#260407=CARTESIAN_POINT('Ctrl Pts',(-26.7269236186766,-76.2394155534521,
16.2836305889859));
#260408=CARTESIAN_POINT('Ctrl Pts',(-26.86480522874,-76.2345275940673,16.6835961109188));
#260409=CARTESIAN_POINT('Ctrl Pts',(-26.7999815868866,-76.279471108584,
16.4833268552187));
#260410=CARTESIAN_POINT('Ctrl Pts',(-26.7675182843423,-76.2612367837894,
16.2713262631396));
#260411=CARTESIAN_POINT('Ctrl Pts',(-26.9428805656779,-76.2819273824521,
16.6613225028908));
#260412=CARTESIAN_POINT('Ctrl Pts',(-26.8778122806246,-76.3256082188876,
16.4603950294985));
#260413=CARTESIAN_POINT('Ctrl Pts',(-26.8475982558589,-76.3071412425567,
16.2476495575985));
#260414=CARTESIAN_POINT('Ctrl Pts',(-26.9810543502183,-76.3069759166523,
16.6496028712585));
#260415=CARTESIAN_POINT('Ctrl Pts',(-26.9160778594147,-76.3496981928992,
16.448829796802));
#260416=CARTESIAN_POINT('Ctrl Pts',(-26.8870847364698,-76.3312252545645,
16.2362848769795));
#260417=CARTESIAN_POINT('Ctrl Pts',(-27.0347146146425,-76.3484797871891,
16.6221367327712));
#260418=CARTESIAN_POINT('Ctrl Pts',(-26.9722866202247,-76.387191475666,
16.4263729310814));
#260419=CARTESIAN_POINT('Ctrl Pts',(-26.9454540778636,-76.369062531796,
16.2198040383418));
#260420=CARTESIAN_POINT('Ctrl Pts',(-27.0520461010368,-76.362903314126,
16.6116902389505));
#260421=CARTESIAN_POINT('Ctrl Pts',(-26.990797870902,-76.3998985070137,
16.4182354344378));
#260422=CARTESIAN_POINT('Ctrl Pts',(-26.9647604072753,-76.3819564220901,
16.2144102296094));
#260423=CARTESIAN_POINT('Ctrl Pts',(-27.0754324956906,-76.3870229007017,
16.5857176723771));
#260424=CARTESIAN_POINT('Ctrl Pts',(-27.0180627224554,-76.4191298939445,
16.4005487707529));
#260425=CARTESIAN_POINT('Ctrl Pts',(-26.9934408909725,-76.4016850635586,
16.2063864536385));
#260426=CARTESIAN_POINT('Ctrl Pts',(-27.082807799689,-76.3954507470103,
16.5755244414166));
#260427=CARTESIAN_POINT('Ctrl Pts',(-27.0270559839675,-76.4255606544136,
16.3938428354582));
#260428=CARTESIAN_POINT('Ctrl Pts',(-27.002956907366,-76.4083274633214,
16.2037237985522));
#260429=CARTESIAN_POINT('Ctrl Pts',(-27.0922320376559,-76.4098047654361,
16.5516204721235));
#260430=CARTESIAN_POINT('Ctrl Pts',(-27.0403670147046,-76.4351975383185,
16.3792244413015));
#260431=CARTESIAN_POINT('Ctrl Pts',(-27.0171572804536,-76.4183850872766,
16.1996869095663));
#260432=CARTESIAN_POINT('Ctrl Pts',(-27.0950953264238,-76.4148733708263,
16.542241373223));
#260433=CARTESIAN_POINT('Ctrl Pts',(-27.0447678397139,-76.4384035785,16.3736104964499));
#260434=CARTESIAN_POINT('Ctrl Pts',(-27.0218787739739,-76.4217535244985,
16.1983342860888));
#260435=CARTESIAN_POINT('Ctrl Pts',(-27.09974315268,-76.4263249193095,16.5161165141971));
#260436=CARTESIAN_POINT('Ctrl Pts',(-27.0535116464076,-76.4448069459407,
16.3585277802127));
#260437=CARTESIAN_POINT('Ctrl Pts',(-27.0312909576635,-76.4285171755911,
16.1955743904622));
#260438=CARTESIAN_POINT('Ctrl Pts',(-27.1014904674061,-76.4326137594219,
16.5002045800044));
#260439=CARTESIAN_POINT('Ctrl Pts',(-27.0578166604448,-76.4479765311915,
16.3494953975989));
#260440=CARTESIAN_POINT('Ctrl Pts',(-27.0359831728686,-76.4319135317268,
16.1941800679749));
#260441=CARTESIAN_POINT('Ctrl Pts',(-27.1026704184049,-76.4449452653179,
16.4573094494877));
#260442=CARTESIAN_POINT('Ctrl Pts',(-27.06448288193,-76.4528969605597,16.3261248041982));
#260443=CARTESIAN_POINT('Ctrl Pts',(-27.042975264242,-76.4370110131309,
16.1919016822539));
#260444=CARTESIAN_POINT('Ctrl Pts',(-27.1027728684428,-76.4496135704626,
16.4393960541623));
#260445=CARTESIAN_POINT('Ctrl Pts',(-27.0667393944978,-76.4545638835523,
16.3164891117473));
#260446=CARTESIAN_POINT('Ctrl Pts',(-27.0453014012305,-76.4387129855089,
16.1911145326723));
#260447=CARTESIAN_POINT('Ctrl Pts',(-27.1033488438058,-76.4602856539495,
16.3918070921512));
#260448=CARTESIAN_POINT('Ctrl Pts',(-27.0716717101316,-76.4582133271186,
16.2912288897422));
#260449=CARTESIAN_POINT('Ctrl Pts',(-27.0498984940091,-76.4420884316609,
16.1893010704581));
#260450=CARTESIAN_POINT('Ctrl Pts',(-27.103921956883,-76.4662567117755,
16.3621450322927));
#260451=CARTESIAN_POINT('Ctrl Pts',(-27.0743744435445,-76.4602162047745,
16.2756512778778));
#260452=CARTESIAN_POINT('Ctrl Pts',(-27.0521738675717,-76.4437652233608,
16.1883092099671));
#260453=CARTESIAN_POINT('Ctrl Pts',(-27.1079500471755,-76.4780100141098,
16.2949622535392));
#260454=CARTESIAN_POINT('Ctrl Pts',(-27.0805869451232,-76.4648464736733,
16.2402396310873));
#260455=CARTESIAN_POINT('Ctrl Pts',(-27.0565399426152,-76.446993278341,
16.1852909757043));
#260456=CARTESIAN_POINT('Ctrl Pts',(-27.1117437396593,-76.4840868539141,
16.2559882666832));
#260457=CARTESIAN_POINT('Ctrl Pts',(-27.0843760577293,-76.4676882621546,
16.2196371037421));
#260458=CARTESIAN_POINT('Ctrl Pts',(-27.0588362934608,-76.4486982192438,
16.1831963663266));
#260459=CARTESIAN_POINT('Ctrl Pts',(-27.1186429162664,-76.490725727778,
16.1967720341217));
#260460=CARTESIAN_POINT('Ctrl Pts',(-27.0889706079157,-76.4711321232331,
16.1872136925794));
#260461=CARTESIAN_POINT('Ctrl Pts',(-27.060449611965,-76.4498977970784,
16.1776432448482));
#260462=CARTESIAN_POINT('Ctrl Pts',(-27.1210505518396,-76.4924398017463,
16.1773616860554));
#260463=CARTESIAN_POINT('Ctrl Pts',(-27.0902380459652,-76.472080509577,
16.1763774272268));
#260464=CARTESIAN_POINT('Ctrl Pts',(-27.0606161752027,-76.4500218115713,
16.1753910477022));
#260465=CARTESIAN_POINT('Ctrl Pts',(-27.1247236922632,-76.4945108031759,
16.1461844913658));
#260466=CARTESIAN_POINT('Ctrl Pts',(-27.0917434440942,-76.4731956267612,
16.1586478057165));
#260467=CARTESIAN_POINT('Ctrl Pts',(-27.0602497730195,-76.4497492188549,
16.1711360013758));
#260468=CARTESIAN_POINT('Ctrl Pts',(-27.1261031628986,-76.4950020357306,
16.1336817286105));
#260469=CARTESIAN_POINT('Ctrl Pts',(-27.0920805335398,-76.4734376571505,
16.1513715711306));
#260470=CARTESIAN_POINT('Ctrl Pts',(-27.0597799419457,-76.4493997295781,
16.1691026721905));
#260471=CARTESIAN_POINT('Ctrl Pts',(-27.1315681998307,-76.4963255984206,
16.0800932837524));
#260472=CARTESIAN_POINT('Ctrl Pts',(-27.0928134511318,-76.4739251360541,
16.1197927836083));
#260473=CARTESIAN_POINT('Ctrl Pts',(-27.0569687226382,-76.4473109346426,
16.1596448232286));
#260474=CARTESIAN_POINT('Ctrl Pts',(-27.1323195784959,-76.4945113000399,
16.0589082957796));
#260475=CARTESIAN_POINT('Ctrl Pts',(-27.0909209641397,-76.4724331002842,
16.1061418174148));
#260476=CARTESIAN_POINT('Ctrl Pts',(-27.0534134152975,-76.4446774540823,
16.1536294662377));
#260477=CARTESIAN_POINT('Ctrl Pts',(-27.1329837771626,-76.490953990412,
16.0195114651226));
#260478=CARTESIAN_POINT('Ctrl Pts',(-27.0869366765604,-76.469312905874,
16.0806139918018));
#260479=CARTESIAN_POINT('Ctrl Pts',(-27.0464009528417,-76.4395165697616,
16.1421882796313));
#260480=CARTESIAN_POINT('Ctrl Pts',(-27.132475559678,-76.4887423766877,
16.0040405252701));
#260481=CARTESIAN_POINT('Ctrl Pts',(-27.0844779770543,-76.4674056396179,
16.0701604569259));
#260482=CARTESIAN_POINT('Ctrl Pts',(-27.0426984150624,-76.436805864294,
16.1368608677843));
#260483=CARTESIAN_POINT('Ctrl Pts',(-27.1176445693019,-76.4487554850671,
15.7668594205044));
#260484=CARTESIAN_POINT('Ctrl Pts',(-27.0392647575279,-76.432563214653,
15.9058934996543));
#260485=CARTESIAN_POINT('Ctrl Pts',(-26.9783040498254,-76.3899445519403,
16.0485446134454));
#260486=CARTESIAN_POINT('Ctrl Pts',(-27.0267181003067,-76.3890441685664,
15.9290103440671));
#260487=CARTESIAN_POINT('Ctrl Pts',(-26.9607754137872,-76.3752347443676,
15.9631551147876));
#260488=CARTESIAN_POINT('Ctrl Pts',(-26.9028259696071,-76.3392599186865,
16.0018551686374));
#260489=CARTESIAN_POINT('Ctrl Pts',(-27.0702645554341,-76.3535975691974,
14.8756002297544));
#260490=CARTESIAN_POINT('Ctrl Pts',(-26.9358287316524,-76.3662706704139,
15.3627392755869));
#260491=CARTESIAN_POINT('Ctrl Pts',(-26.8612497822103,-76.3194480575193,
15.8395311954951));
#260492=CARTESIAN_POINT('Origin',(-24.9421491495266,-74.7257085670769,17.0741173620444));
#260493=CARTESIAN_POINT('Ctrl Pts',(-25.1074704499414,-75.9627753172411,
17.4259425795563));
#260494=CARTESIAN_POINT('Ctrl Pts',(-25.046235007313,-75.9901905947504,
17.3727027235404));
#260495=CARTESIAN_POINT('Ctrl Pts',(-24.981902561604,-76.0065414441461,
17.3185796118018));
#260496=CARTESIAN_POINT('Ctrl Pts',(-25.1496292028979,-75.9580441983283,
17.3506767478559));
#260497=CARTESIAN_POINT('Ctrl Pts',(-25.0926862206973,-75.9851307386982,
17.2798459583171));
#260498=CARTESIAN_POINT('Ctrl Pts',(-25.032269407339,-75.9990697411774,
17.2080611431692));
#260499=CARTESIAN_POINT('Ctrl Pts',(-25.2082186982554,-75.9481612402448,
17.2973276043357));
#260500=CARTESIAN_POINT('Ctrl Pts',(-25.1530396515149,-75.9759984326107,
17.2125718696202));
#260501=CARTESIAN_POINT('Ctrl Pts',(-25.0938856963612,-75.9872898972827,
17.1266598669893));
#260502=CARTESIAN_POINT('Ctrl Pts',(-25.2708374177341,-75.9397262748193,
17.2518520136524));
#260503=CARTESIAN_POINT('Ctrl Pts',(-25.2169363483077,-75.9685632596981,
17.1547259853579));
#260504=CARTESIAN_POINT('Ctrl Pts',(-25.1589733721019,-75.9772090303652,
17.0560474932908));
#260505=CARTESIAN_POINT('Origin',(-24.7225971487431,-74.7646897896797,17.2528005263626));
#260506=CARTESIAN_POINT('Ctrl Pts',(-24.9948448130087,-76.0045572676613,
17.2916572676744));
#260507=CARTESIAN_POINT('Ctrl Pts',(-25.0581838218632,-75.9888185880893,
17.3500764673707));
#260508=CARTESIAN_POINT('Ctrl Pts',(-25.1183452685093,-75.9614890268773,
17.4075745924872));
#260509=CARTESIAN_POINT('Ctrl Pts',(-24.9029090128662,-76.0189046879179,
17.4779931990395));
#260510=CARTESIAN_POINT('Ctrl Pts',(-24.9436535528188,-76.0047941374338,
17.5184791523303));
#260511=CARTESIAN_POINT('Ctrl Pts',(-24.9827521037685,-75.9867440840462,
17.5589921227692));
#260512=CARTESIAN_POINT('Ctrl Pts',(-24.8038409415453,-76.0317753893924,
17.6635683446476));
#260513=CARTESIAN_POINT('Ctrl Pts',(-24.8230534553307,-76.0228272111309,
17.6845460983631));
#260514=CARTESIAN_POINT('Ctrl Pts',(-24.842279269484,-76.0138748889534,
17.7055224897201));
#260515=CARTESIAN_POINT('Ctrl Pts',(-24.6976449914385,-76.0424582865173,
17.8479876926674));
#260516=CARTESIAN_POINT('Ctrl Pts',(-24.6976449914385,-76.0424582865173,
17.8479876926674));
#260517=CARTESIAN_POINT('Ctrl Pts',(-24.6976449914385,-76.0424582865173,
17.8479876926674));
#260518=CARTESIAN_POINT('Ctrl Pts',(25.1183452685168,-75.9614890268759,
17.4075745924789));
#260519=CARTESIAN_POINT('Ctrl Pts',(25.0581838218696,-75.9888185880884,
17.3500764673614));
#260520=CARTESIAN_POINT('Ctrl Pts',(24.9948448130138,-76.0045572676605,
17.2916572676642));
#260521=CARTESIAN_POINT('Ctrl Pts',(24.9827521037791,-75.9867440840413,
17.5589921227799));
#260522=CARTESIAN_POINT('Ctrl Pts',(24.9436535528272,-76.0047941374361,
17.5184791523559));
#260523=CARTESIAN_POINT('Ctrl Pts',(24.9029090128812,-76.0189046879146,
17.4779931990425));
#260524=CARTESIAN_POINT('Ctrl Pts',(24.8422792694397,-76.0138748889755,
17.7055224896604));
#260525=CARTESIAN_POINT('Ctrl Pts',(24.8230534553045,-76.0228272111454,
17.6845460983164));
#260526=CARTESIAN_POINT('Ctrl Pts',(24.8038409415197,-76.0317753894035,
17.6635683446265));
#260527=CARTESIAN_POINT('Ctrl Pts',(24.6976449914381,-76.042458286517,17.8479876926702));
#260528=CARTESIAN_POINT('Ctrl Pts',(24.6976449914381,-76.042458286517,17.8479876926702));
#260529=CARTESIAN_POINT('Ctrl Pts',(24.6976449914381,-76.042458286517,17.8479876926702));
#260530=CARTESIAN_POINT('Origin',(24.7225971487503,-74.7646897896784,17.2528005263546));
#260531=CARTESIAN_POINT('Ctrl Pts',(25.2708374177646,-75.9397262748126,
17.2518520136429));
#260532=CARTESIAN_POINT('Ctrl Pts',(25.216936348354,-75.9685632596854,17.1547259853771));
#260533=CARTESIAN_POINT('Ctrl Pts',(25.1589733721664,-75.977209030355,17.0560474933546));
#260534=CARTESIAN_POINT('Ctrl Pts',(25.2082186981224,-75.9481612402767,
17.2973276043667));
#260535=CARTESIAN_POINT('Ctrl Pts',(25.1530396514148,-75.9759984326127,
17.2125718697077));
#260536=CARTESIAN_POINT('Ctrl Pts',(25.0938856963024,-75.9872898972931,
17.1266598670757));
#260537=CARTESIAN_POINT('Ctrl Pts',(25.1496292031279,-75.9580441982479,
17.3506767479025));
#260538=CARTESIAN_POINT('Ctrl Pts',(25.092686220964,-75.9851307386456,17.279845958371));
#260539=CARTESIAN_POINT('Ctrl Pts',(25.0322694075872,-75.9990697411219,
17.2080611432543));
#260540=CARTESIAN_POINT('Ctrl Pts',(25.1074704498875,-75.9627753172617,
17.4259425795336));
#260541=CARTESIAN_POINT('Ctrl Pts',(25.0462350072772,-75.9901905947512,
17.3727027235393));
#260542=CARTESIAN_POINT('Ctrl Pts',(24.9819025616038,-76.0065414441453,
17.3185796118177));
#260543=CARTESIAN_POINT('Origin',(24.9421491495265,-74.7257085670769,17.0741173620444));
#260544=CARTESIAN_POINT('Ctrl Pts',(24.9589179244775,-76.0165927349248,
17.2719235983584));
#260545=CARTESIAN_POINT('Ctrl Pts',(25.0217593825187,-76.0018779353611,
17.3465144253549));
#260546=CARTESIAN_POINT('Ctrl Pts',(25.080406146805,-75.9725739125722,17.4202136827156));
#260547=CARTESIAN_POINT('Ctrl Pts',(25.1644631755165,-75.9667363952717,
17.0140601840459));
#260548=CARTESIAN_POINT('Ctrl Pts',(25.221741891211,-75.958699255426,17.1147005690572));
#260549=CARTESIAN_POINT('Ctrl Pts',(25.2742034625189,-75.9311549696869,
17.2143522965184));
#260550=CARTESIAN_POINT('Ctrl Pts',(25.4013568068367,-75.9400924588407,
16.8531572333247));
#260551=CARTESIAN_POINT('Ctrl Pts',(25.4560486791227,-75.9375037638634,
16.9749518244653));
#260552=CARTESIAN_POINT('Ctrl Pts',(25.5065310412202,-75.9076590513784,
17.0946441539564));
#260553=CARTESIAN_POINT('Ctrl Pts',(25.8199808109355,-75.9567824207869,
16.6241920433869));
#260554=CARTESIAN_POINT('Ctrl Pts',(25.8693789134686,-75.9625371923871,
16.7790876749283));
#260555=CARTESIAN_POINT('Ctrl Pts',(25.9208598335162,-75.9275121102613,
16.9293154163786));
#260556=CARTESIAN_POINT('Ctrl Pts',(26.000053557193,-75.982549287452,16.5442194930891));
#260557=CARTESIAN_POINT('Ctrl Pts',(26.0472138477371,-75.9915734872872,
16.7120520463995));
#260558=CARTESIAN_POINT('Ctrl Pts',(26.1002356630946,-75.9538145401055,
16.8739507926621));
#260559=CARTESIAN_POINT('Ctrl Pts',(26.3487341201567,-76.0718263572337,
16.4064067119874));
#260560=CARTESIAN_POINT('Ctrl Pts',(26.3904925533402,-76.0862325763166,
16.5975865835765));
#260561=CARTESIAN_POINT('Ctrl Pts',(26.4481950423898,-76.0436375889943,
16.7801750175556));
#260562=CARTESIAN_POINT('Ctrl Pts',(26.5206773079536,-76.1357086402236,
16.3474135454721));
#260563=CARTESIAN_POINT('Ctrl Pts',(26.5592282356561,-76.1523784623028,
16.5499987057077));
#260564=CARTESIAN_POINT('Ctrl Pts',(26.6205318971682,-76.1072227620321,
16.7423277263585));
#260565=CARTESIAN_POINT('Ctrl Pts',(26.7264920278152,-76.2391872039751,
16.2832499561865));
#260566=CARTESIAN_POINT('Ctrl Pts',(26.7600048061527,-76.2572914179578,
16.4941794849072));
#260567=CARTESIAN_POINT('Ctrl Pts',(26.8243988718558,-76.2121224139505,
16.6935643209576));
#260568=CARTESIAN_POINT('Ctrl Pts',(26.7670983652051,-76.2610052237305,
16.2709381031613));
#260569=CARTESIAN_POINT('Ctrl Pts',(26.7995686663897,-76.2793339283727,
16.483182492595));
#260570=CARTESIAN_POINT('Ctrl Pts',(26.8644662406905,-76.2343342587333,
16.6836830235308));
#260571=CARTESIAN_POINT('Ctrl Pts',(26.8471814973332,-76.3068912751988,
16.2472568143868));
#260572=CARTESIAN_POINT('Ctrl Pts',(26.877398340547,-76.3254529697315,16.4602585557158));
#260573=CARTESIAN_POINT('Ctrl Pts',(26.9425455044634,-76.2817116075996,
16.6614278008798));
#260574=CARTESIAN_POINT('Ctrl Pts',(26.8866594690452,-76.3309600846097,
16.2358941800171));
#260575=CARTESIAN_POINT('Ctrl Pts',(26.9156538070631,-76.3495273630062,
16.4486994597328));
#260576=CARTESIAN_POINT('Ctrl Pts',(26.9807109693644,-76.306742883636,16.6497176781018));
#260577=CARTESIAN_POINT('Ctrl Pts',(26.9450028214736,-76.3687633501263,
16.2194335053764));
#260578=CARTESIAN_POINT('Ctrl Pts',(26.97183869477,-76.3869839776596,16.42630302961));
#260579=CARTESIAN_POINT('Ctrl Pts',(27.0343640367628,-76.3481925895598,
16.6223462081032));
#260580=CARTESIAN_POINT('Ctrl Pts',(26.9643135743833,-76.3816540900187,
16.2140445067397));
#260581=CARTESIAN_POINT('Ctrl Pts',(26.9903552563186,-76.3996866432579,
16.4181843035957));
#260582=CARTESIAN_POINT('Ctrl Pts',(27.0517070232152,-76.3626055738679,
16.6119303417357));
#260583=CARTESIAN_POINT('Ctrl Pts',(26.9930030990806,-76.4013801263841,
16.2060411897629));
#260584=CARTESIAN_POINT('Ctrl Pts',(27.0176339890546,-76.4189117662005,
16.4005910913664));
#260585=CARTESIAN_POINT('Ctrl Pts',(27.0751338551856,-76.3866896924452,
16.586115526953));
#260586=CARTESIAN_POINT('Ctrl Pts',(27.0025216629709,-76.4080213774166,
16.2033875259851));
#260587=CARTESIAN_POINT('Ctrl Pts',(27.0266321688135,-76.4253400053729,
16.3939233783011));
#260588=CARTESIAN_POINT('Ctrl Pts',(27.0825251279255,-76.3951028736931,
16.5759864000299));
#260589=CARTESIAN_POINT('Ctrl Pts',(27.0167251837918,-76.4180768571583,
16.1993760598583));
#260590=CARTESIAN_POINT('Ctrl Pts',(27.0399520693394,-76.4349711969098,
16.3794519126528));
#260591=CARTESIAN_POINT('Ctrl Pts',(27.0919957506263,-76.4094060153691,
16.5523396954336));
#260592=CARTESIAN_POINT('Ctrl Pts',(27.021447406794,-76.4214443601548,16.1980339040756));
#260593=CARTESIAN_POINT('Ctrl Pts',(27.0443560717347,-76.4381750026904,
16.3739005889315));
#260594=CARTESIAN_POINT('Ctrl Pts',(27.0948782509814,-76.4144529145863,
16.5430709358771));
#260595=CARTESIAN_POINT('Ctrl Pts',(27.0308618473994,-76.4282067461047,
16.1953051377168));
#260596=CARTESIAN_POINT('Ctrl Pts',(27.0531068030348,-76.4445721654389,
16.3590502399129));
#260597=CARTESIAN_POINT('Ctrl Pts',(27.0995848868676,-76.4258296211971,
16.5173659018241));
#260598=CARTESIAN_POINT('Ctrl Pts',(27.0355558313041,-76.431602939514,16.1939295264868));
#260599=CARTESIAN_POINT('Ctrl Pts',(27.0574185528962,-76.4477400998369,
16.3501709468135));
#260600=CARTESIAN_POINT('Ctrl Pts',(27.1013790751781,-76.4320671444298,
16.5017321152991));
#260601=CARTESIAN_POINT('Ctrl Pts',(27.0425542496203,-76.4367029543674,
16.1917093184004));
#260602=CARTESIAN_POINT('Ctrl Pts',(27.0640787016057,-76.4526420041684,
16.3273830254781));
#260603=CARTESIAN_POINT('Ctrl Pts',(27.1026290071501,-76.4442399823126,
16.4599278409708));
#260604=CARTESIAN_POINT('Ctrl Pts',(27.044882087663,-76.4384054885609,16.1909469809412));
#260605=CARTESIAN_POINT('Ctrl Pts',(27.0663285831481,-76.454298594577,16.3180252379247));
#260606=CARTESIAN_POINT('Ctrl Pts',(27.1027558331205,-76.448833955927,16.4425406105531));
#260607=CARTESIAN_POINT('Ctrl Pts',(27.0494862927941,-76.4417848384089,
16.189213145832));
#260608=CARTESIAN_POINT('Ctrl Pts',(27.0712224187978,-76.457906806159,16.2933864096896));
#260609=CARTESIAN_POINT('Ctrl Pts',(27.1032790990715,-76.4593812243663,
16.3961238359575));
#260610=CARTESIAN_POINT('Ctrl Pts',(27.0517726588334,-76.4434690801001,
16.1882712240633));
#260611=CARTESIAN_POINT('Ctrl Pts',(27.0738999824816,-76.4598835980122,
16.2780430295813));
#260612=CARTESIAN_POINT('Ctrl Pts',(27.1037600538756,-76.4653396447702,
16.3668981593358));
#260613=CARTESIAN_POINT('Ctrl Pts',(27.056165905205,-76.4467160461775,16.1854342125082));
#260614=CARTESIAN_POINT('Ctrl Pts',(27.0800527001779,-76.4644564169994,
16.2430394726561));
#260615=CARTESIAN_POINT('Ctrl Pts',(27.1075193470971,-76.477134392507,16.3003874390844));
#260616=CARTESIAN_POINT('Ctrl Pts',(27.058446161956,-76.448408331131,16.183554002614));
#260617=CARTESIAN_POINT('Ctrl Pts',(27.0837265687902,-76.4672060788238,
16.2231638334608));
#260618=CARTESIAN_POINT('Ctrl Pts',(27.1110283258744,-76.4831388236134,
16.2626673380729));
#260619=CARTESIAN_POINT('Ctrl Pts',(27.0602641883352,-76.4497597907345,
16.178270627192));
#260620=CARTESIAN_POINT('Ctrl Pts',(27.0884790804448,-76.4707669813323,
16.1906858996445));
#260621=CARTESIAN_POINT('Ctrl Pts',(27.1178762399416,-76.4900906831748,
16.2030844689337));
#260622=CARTESIAN_POINT('Ctrl Pts',(27.0605327253119,-76.4499596839301,
16.1760791854255));
#260623=CARTESIAN_POINT('Ctrl Pts',(27.0898596142588,-76.4718011962243,
16.1795820812116));
#260624=CARTESIAN_POINT('Ctrl Pts',(27.1203589546904,-76.4919704158393,
16.1830789062925));
#260625=CARTESIAN_POINT('Ctrl Pts',(27.0602871252534,-76.4497769562955,
16.1718015077251));
#260626=CARTESIAN_POINT('Ctrl Pts',(27.091550239126,-76.4730573789198,16.161098430761));
#260627=CARTESIAN_POINT('Ctrl Pts',(27.1242386900703,-76.4942958338587,
16.150415724656));
#260628=CARTESIAN_POINT('Ctrl Pts',(27.0598504145463,-76.4494520698569,
16.1697479299107));
#260629=CARTESIAN_POINT('Ctrl Pts',(27.0919480018444,-76.4733461100563,
16.1535475151469));
#260630=CARTESIAN_POINT('Ctrl Pts',(27.1257019220719,-76.4948627300815,
16.1373831736257));
#260631=CARTESIAN_POINT('Ctrl Pts',(27.0582086378074,-76.4482320655577,
16.1639666812434));
#260632=CARTESIAN_POINT('Ctrl Pts',(27.0925161430721,-76.4737375070857,
16.1338103547262));
#260633=CARTESIAN_POINT('Ctrl Pts',(27.1291949157768,-76.4958195374835,
16.1037499577342));
#260634=CARTESIAN_POINT('Ctrl Pts',(27.0567042026752,-76.4471157233158,
16.1606292063217));
#260635=CARTESIAN_POINT('Ctrl Pts',(27.0921025222746,-76.4733973726533,
16.1245076295647));
#260636=CARTESIAN_POINT('Ctrl Pts',(27.1303769014743,-76.495511079926,16.088527708241));
#260637=CARTESIAN_POINT('Ctrl Pts',(27.0534903139798,-76.4447377899016,
16.154219073874));
#260638=CARTESIAN_POINT('Ctrl Pts',(27.0908610700863,-76.4724034594285,
16.1076940322559));
#260639=CARTESIAN_POINT('Ctrl Pts',(27.1320488754804,-76.4944955989311,
16.0614128144368));
#260640=CARTESIAN_POINT('Ctrl Pts',(27.0517739663595,-76.4434708920043,
16.1512353239512));
#260641=CARTESIAN_POINT('Ctrl Pts',(27.0899831498703,-76.4717122944326,
16.1006284961015));
#260642=CARTESIAN_POINT('Ctrl Pts',(27.1324478126924,-76.4937176487667,
16.050318648402));
#260643=CARTESIAN_POINT('Ctrl Pts',(27.0464903385136,-76.4395819014306,
16.1426043077347));
#260644=CARTESIAN_POINT('Ctrl Pts',(27.087001580347,-76.4693799204485,16.0812344002251));
#260645=CARTESIAN_POINT('Ctrl Pts',(27.1330005795476,-76.4910613317947,
16.0203313638476));
#260646=CARTESIAN_POINT('Ctrl Pts',(27.0427755237225,-76.436861974418,16.1372659264035));
#260647=CARTESIAN_POINT('Ctrl Pts',(27.0845393319118,-76.4674716655807,
16.0707205696176));
#260648=CARTESIAN_POINT('Ctrl Pts',(27.1325040250962,-76.4888476713311,
16.0047512157116));
#260649=CARTESIAN_POINT('Ctrl Pts',(26.9782305695083,-76.3898874630358,
16.0488344443928));
#260650=CARTESIAN_POINT('Ctrl Pts',(27.0392919333536,-76.4326304753448,
15.9056407261267));
#260651=CARTESIAN_POINT('Ctrl Pts',(27.1178462988928,-76.4488518479317,
15.7660809789566));
#260652=CARTESIAN_POINT('Ctrl Pts',(26.9009713129947,-76.3379547623971,
16.0003561766751));
#260653=CARTESIAN_POINT('Ctrl Pts',(26.959117533273,-76.3740242719226,15.9620875813222));
#260654=CARTESIAN_POINT('Ctrl Pts',(27.0253527115695,-76.387700859183,15.9284160212411));
#260655=CARTESIAN_POINT('Ctrl Pts',(26.8672868453189,-76.323892551556,15.8466387280156));
#260656=CARTESIAN_POINT('Ctrl Pts',(26.9411427564858,-76.3705353286247,
15.3686915983964));
#260657=CARTESIAN_POINT('Ctrl Pts',(27.0744152538546,-76.3583349935937,
14.8796638708869));
#260658=CARTESIAN_POINT('Ctrl Pts',(75.9725615368492,-25.0804618860833,
17.4201668782156));
#260659=CARTESIAN_POINT('Ctrl Pts',(76.0018311057085,-25.0218849780074,
17.3465486624662));
#260660=CARTESIAN_POINT('Ctrl Pts',(76.0165443120274,-24.9591222047477,
17.2720397184167));
#260661=CARTESIAN_POINT('Ctrl Pts',(75.931169298622,-25.2741629193577,17.2143925574082));
#260662=CARTESIAN_POINT('Ctrl Pts',(75.958681184672,-25.2217620982712,17.114863355933));
#260663=CARTESIAN_POINT('Ctrl Pts',(75.9667333080915,-25.1645554520448,
17.0143457047411));
#260664=CARTESIAN_POINT('Ctrl Pts',(75.9076483674902,-25.50650283451,17.0946463742361));
#260665=CARTESIAN_POINT('Ctrl Pts',(75.9374572719645,-25.4560812233272,
16.9750964736227));
#260666=CARTESIAN_POINT('Ctrl Pts',(75.9400754392653,-25.4014568018194,
16.8534468191075));
#260667=CARTESIAN_POINT('Ctrl Pts',(75.9275280255502,-25.9210527955254,
16.9292448759546));
#260668=CARTESIAN_POINT('Ctrl Pts',(75.9625142169127,-25.869632234825,16.7791814037269));
#260669=CARTESIAN_POINT('Ctrl Pts',(75.9568105611571,-25.8202904741216,
16.6244542312725));
#260670=CARTESIAN_POINT('Ctrl Pts',(75.9538339499134,-26.1003508790237,
16.8739158933912));
#260671=CARTESIAN_POINT('Ctrl Pts',(75.9915498547703,-26.0473908953001,
16.7122017332653));
#260672=CARTESIAN_POINT('Ctrl Pts',(75.9825893385697,-26.0002790025666,
16.5445597191247));
#260673=CARTESIAN_POINT('Ctrl Pts',(76.043689910258,-26.4483576686014,16.7801350408721));
#260674=CARTESIAN_POINT('Ctrl Pts',(76.0862364212178,-26.3907212263421,
16.5977546210478));
#260675=CARTESIAN_POINT('Ctrl Pts',(76.0719119444774,-26.3489939258776,
16.4067913625481));
#260676=CARTESIAN_POINT('Ctrl Pts',(76.1074179294968,-26.6209880248623,
16.7422284473672));
#260677=CARTESIAN_POINT('Ctrl Pts',(76.1525248745982,-26.559747689091,16.5501048951559));
#260678=CARTESIAN_POINT('Ctrl Pts',(76.1359425371629,-26.5212227642695,
16.3477329791785));
#260679=CARTESIAN_POINT('Ctrl Pts',(76.21231215836,-26.8247483133844,16.6934782675217));
#260680=CARTESIAN_POINT('Ctrl Pts',(76.2574262010941,-26.7604265541735,
16.494320859219));
#260681=CARTESIAN_POINT('Ctrl Pts',(76.239415553451,-26.7269236186745,16.2836305889652));
#260682=CARTESIAN_POINT('Ctrl Pts',(76.2345275940678,-26.8648052287415,
16.6835961109194));
#260683=CARTESIAN_POINT('Ctrl Pts',(76.2794711085875,-26.7999815868845,
16.483326855209));
#260684=CARTESIAN_POINT('Ctrl Pts',(76.2612367837882,-26.7675182843401,
16.2713262631183));
#260685=CARTESIAN_POINT('Ctrl Pts',(76.2819273824529,-26.9428805656787,
16.6613225028898));
#260686=CARTESIAN_POINT('Ctrl Pts',(76.3256082188901,-26.8778122806222,
16.4603950294871));
#260687=CARTESIAN_POINT('Ctrl Pts',(76.3071412425556,-26.847598255857,16.2476495575766));
#260688=CARTESIAN_POINT('Ctrl Pts',(76.3069759166547,-26.981054350217,16.6496028712503));
#260689=CARTESIAN_POINT('Ctrl Pts',(76.3496981929022,-26.916077859412,16.4488297967862));
#260690=CARTESIAN_POINT('Ctrl Pts',(76.3312252545631,-26.8870847364676,
16.2362848769561));
#260691=CARTESIAN_POINT('Ctrl Pts',(76.3484797871891,-27.0347146146448,
16.622136732775));
#260692=CARTESIAN_POINT('Ctrl Pts',(76.3871914756689,-26.9722866202228,
16.4263729310736));
#260693=CARTESIAN_POINT('Ctrl Pts',(76.3690625317952,-26.9454540778622,
16.2198040383217));
#260694=CARTESIAN_POINT('Ctrl Pts',(76.3629033141268,-27.0520461010375,
16.6116902389496));
#260695=CARTESIAN_POINT('Ctrl Pts',(76.3998985070162,-26.9907978709001,
16.418235434428));
#260696=CARTESIAN_POINT('Ctrl Pts',(76.381956422089,-26.9647604072736,16.2144102295885));
#260697=CARTESIAN_POINT('Ctrl Pts',(76.3870229007027,-27.0754324956918,
16.5857176723765));
#260698=CARTESIAN_POINT('Ctrl Pts',(76.4191298939471,-27.0180627224535,
16.4005487707426));
#260699=CARTESIAN_POINT('Ctrl Pts',(76.4016850635578,-26.9934408909713,
16.2063864536189));
#260700=CARTESIAN_POINT('Ctrl Pts',(76.3954507470115,-27.08280779969,16.5755244414153));
#260701=CARTESIAN_POINT('Ctrl Pts',(76.4255606544161,-27.0270559839657,
16.393842835448));
#260702=CARTESIAN_POINT('Ctrl Pts',(76.4083274633205,-27.0029569073648,
16.2037237985328));
#260703=CARTESIAN_POINT('Ctrl Pts',(76.4098047654372,-27.0922320376568,
16.5516204721222));
#260704=CARTESIAN_POINT('Ctrl Pts',(76.4351975383206,-27.0403670147031,
16.3792244412919));
#260705=CARTESIAN_POINT('Ctrl Pts',(76.4183850872758,-27.0171572804525,
16.199686909548));
#260706=CARTESIAN_POINT('Ctrl Pts',(76.4148733708268,-27.0950953264254,
16.5422413732253));
#260707=CARTESIAN_POINT('Ctrl Pts',(76.4384035785022,-27.0447678397125,
16.3736104964424));
#260708=CARTESIAN_POINT('Ctrl Pts',(76.4217535244978,-27.0218787739728,
16.1983342860712));
#260709=CARTESIAN_POINT('Ctrl Pts',(76.4263249193116,-27.0997431526799,
16.5161165141907));
#260710=CARTESIAN_POINT('Ctrl Pts',(76.4448069459424,-27.0535116464063,
16.3585277802011));
#260711=CARTESIAN_POINT('Ctrl Pts',(76.4285171755903,-27.0312909576624,
16.1955743904452));
#260712=CARTESIAN_POINT('Ctrl Pts',(76.4326137594236,-27.1014904674066,
16.5002045800003));
#260713=CARTESIAN_POINT('Ctrl Pts',(76.4479765311931,-27.0578166604438,
16.3494953975893));
#260714=CARTESIAN_POINT('Ctrl Pts',(76.431913531726,-27.0359831728675,16.1941800679589));
#260715=CARTESIAN_POINT('Ctrl Pts',(76.4449452653199,-27.1026704184053,
16.4573094494813));
#260716=CARTESIAN_POINT('Ctrl Pts',(76.452896960561,-27.0644828819291,16.3261248041879));
#260717=CARTESIAN_POINT('Ctrl Pts',(76.4370110131303,-27.042975264241,16.19190168224));
#260718=CARTESIAN_POINT('Ctrl Pts',(76.4496135704653,-27.1027728684427,
16.4393960541509));
#260719=CARTESIAN_POINT('Ctrl Pts',(76.4545638835533,-27.0667393944972,
16.316489111735));
#260720=CARTESIAN_POINT('Ctrl Pts',(76.4387129855081,-27.0453014012295,
16.1911145326591));
#260721=CARTESIAN_POINT('Ctrl Pts',(76.4602856539522,-27.1033488438061,
16.3918070921387));
#260722=CARTESIAN_POINT('Ctrl Pts',(76.4582133271196,-27.0716717101313,
16.2912288897306));
#260723=CARTESIAN_POINT('Ctrl Pts',(76.4420884316602,-27.0498984940081,
16.1893010704474));
#260724=CARTESIAN_POINT('Ctrl Pts',(76.4662567117788,-27.1039219568836,
16.362145032275));
#260725=CARTESIAN_POINT('Ctrl Pts',(76.4602162047754,-27.0743744435445,
16.2756512778644));
#260726=CARTESIAN_POINT('Ctrl Pts',(76.44376522336,-27.0521738675706,16.1883092099575));
#260727=CARTESIAN_POINT('Ctrl Pts',(76.4780100141125,-27.107950047177,16.2949622535236));
#260728=CARTESIAN_POINT('Ctrl Pts',(76.4648464736739,-27.0805869451234,
16.2402396310762));
#260729=CARTESIAN_POINT('Ctrl Pts',(76.4469932783401,-27.0565399426139,
16.1852909756979));
#260730=CARTESIAN_POINT('Ctrl Pts',(76.4840868539169,-27.1117437396614,
16.255988266664));
#260731=CARTESIAN_POINT('Ctrl Pts',(76.4676882621551,-27.0843760577297,
16.2196371037299));
#260732=CARTESIAN_POINT('Ctrl Pts',(76.4486982192426,-27.0588362934592,
16.1831963663216));
#260733=CARTESIAN_POINT('Ctrl Pts',(76.4907257277799,-27.1186429162688,
16.1967720341036));
#260734=CARTESIAN_POINT('Ctrl Pts',(76.4711321232332,-27.0889706079157,
16.1872136925689));
#260735=CARTESIAN_POINT('Ctrl Pts',(76.4498977970766,-27.0604496119625,
16.1776432448454));
#260736=CARTESIAN_POINT('Ctrl Pts',(76.4924398017475,-27.1210505518414,
16.1773616860397));
#260737=CARTESIAN_POINT('Ctrl Pts',(76.4720805095765,-27.0902380459647,
16.1763774272179));
#260738=CARTESIAN_POINT('Ctrl Pts',(76.4500218115691,-27.0606161751996,
16.1753910477002));
#260739=CARTESIAN_POINT('Ctrl Pts',(76.4945108031767,-27.1247236922648,
16.1461844913533));
#260740=CARTESIAN_POINT('Ctrl Pts',(76.4731956267605,-27.091743444093,16.15864780571));
#260741=CARTESIAN_POINT('Ctrl Pts',(76.4497492188525,-27.0602497730161,
16.1711360013752));
#260742=CARTESIAN_POINT('Ctrl Pts',(76.4950020357312,-27.1261031628999,
16.1336817285995));
#260743=CARTESIAN_POINT('Ctrl Pts',(76.4734376571497,-27.0920805335384,
16.1513715711251));
#260744=CARTESIAN_POINT('Ctrl Pts',(76.4493997295754,-27.0597799419421,
16.1691026721906));
#260745=CARTESIAN_POINT('Ctrl Pts',(76.4963255984204,-27.131568199831,16.0800932837475));
#260746=CARTESIAN_POINT('Ctrl Pts',(76.4739251360527,-27.0928134511296,
16.1197927836073));
#260747=CARTESIAN_POINT('Ctrl Pts',(76.4473109346395,-27.056968722634,16.1596448232313));
#260748=CARTESIAN_POINT('Ctrl Pts',(76.4945113000399,-27.1323195784967,
16.0589082957738));
#260749=CARTESIAN_POINT('Ctrl Pts',(76.4724331002834,-27.0909209641377,
16.1061418174134));
#260750=CARTESIAN_POINT('Ctrl Pts',(76.4446774540792,-27.0534134152933,
16.1536294662411));
#260751=CARTESIAN_POINT('Ctrl Pts',(76.4909539904116,-27.1329837771621,
16.0195114651211));
#260752=CARTESIAN_POINT('Ctrl Pts',(76.4693129058723,-27.0869366765573,
16.0806139918042));
#260753=CARTESIAN_POINT('Ctrl Pts',(76.4395165697581,-27.0464009528369,
16.1421882796369));
#260754=CARTESIAN_POINT('Ctrl Pts',(76.4887423766876,-27.1324755596786,
16.0040405252658));
#260755=CARTESIAN_POINT('Ctrl Pts',(76.4674056396168,-27.0844779770519,
16.0701604569266));
#260756=CARTESIAN_POINT('Ctrl Pts',(76.4368058642907,-27.0426984150579,
16.1368608677898));
#260757=CARTESIAN_POINT('Ctrl Pts',(76.448755485065,-27.1176445692923,15.7668594205343));
#260758=CARTESIAN_POINT('Ctrl Pts',(76.4325632146506,-27.0392647575183,
15.905893499679));
#260759=CARTESIAN_POINT('Ctrl Pts',(76.3899445519341,-26.9783040498165,
16.0485446134662));
#260760=CARTESIAN_POINT('Ctrl Pts',(76.3890441685523,-27.0267181003279,
15.9290103438536));
#260761=CARTESIAN_POINT('Ctrl Pts',(76.3752347443254,-26.9607754137721,
15.9631551147061));
#260762=CARTESIAN_POINT('Ctrl Pts',(76.3392599186918,-26.9028259696125,
16.0018551686097));
#260763=CARTESIAN_POINT('Ctrl Pts',(76.353597569397,-27.0702645555105,14.8756002309254));
#260764=CARTESIAN_POINT('Ctrl Pts',(76.3662706708498,-26.9358287319212,
15.3627392759442));
#260765=CARTESIAN_POINT('Ctrl Pts',(76.3194480575026,-26.8612497821939,
15.8395311956764));
#260766=CARTESIAN_POINT('Origin',(74.7257085670769,-24.9421491495266,17.0741173620444));
#260767=CARTESIAN_POINT('Ctrl Pts',(75.9627753172425,-25.1074704499379,
17.425942579555));
#260768=CARTESIAN_POINT('Ctrl Pts',(75.9901905947506,-25.0462350073073,
17.3727027235416));
#260769=CARTESIAN_POINT('Ctrl Pts',(76.006541444146,-24.981902561604,17.3185796118039));
#260770=CARTESIAN_POINT('Ctrl Pts',(75.9580441983231,-25.1496292029117,
17.3506767478614));
#260771=CARTESIAN_POINT('Ctrl Pts',(75.9851307386948,-25.0926862207269,
17.2798459583192));
#260772=CARTESIAN_POINT('Ctrl Pts',(75.9990697411736,-25.0322694073559,
17.2080611431766));
#260773=CARTESIAN_POINT('Ctrl Pts',(75.9481612402476,-25.2082186982459,
17.2973276043341));
#260774=CARTESIAN_POINT('Ctrl Pts',(75.9759984326039,-25.1530396515039,
17.212571869635));
#260775=CARTESIAN_POINT('Ctrl Pts',(75.9872898972835,-25.0938856963563,
17.1266598669944));
#260776=CARTESIAN_POINT('Ctrl Pts',(75.9397262748187,-25.2708374177363,
17.2518520136529));
#260777=CARTESIAN_POINT('Ctrl Pts',(75.9685632596991,-25.2169363483118,
17.1547259853573));
#260778=CARTESIAN_POINT('Ctrl Pts',(75.9772090303644,-25.1589733721069,
17.0560474932961));
#260779=CARTESIAN_POINT('Origin',(74.7646897896797,-24.7225971487432,17.2528005263628));
#260780=CARTESIAN_POINT('Ctrl Pts',(76.0045572676613,-24.9948448130087,
17.2916572676745));
#260781=CARTESIAN_POINT('Ctrl Pts',(75.9888185880893,-25.0581838218632,
17.3500764673708));
#260782=CARTESIAN_POINT('Ctrl Pts',(75.9614890268773,-25.1183452685093,
17.4075745924873));
#260783=CARTESIAN_POINT('Ctrl Pts',(76.0189046879197,-24.9029090128582,
17.4779931990371));
#260784=CARTESIAN_POINT('Ctrl Pts',(76.004794137431,-24.9436535528328,17.5184791523393));
#260785=CARTESIAN_POINT('Ctrl Pts',(75.9867440840503,-24.9827521037588,
17.5589921227622));
#260786=CARTESIAN_POINT('Ctrl Pts',(76.0317753893939,-24.8038409415422,
17.663568344644));
#260787=CARTESIAN_POINT('Ctrl Pts',(76.0228272111318,-24.823053455328,17.6845460983626));
#260788=CARTESIAN_POINT('Ctrl Pts',(76.013874888955,-24.8422792694812,17.7055224897144));
#260789=CARTESIAN_POINT('Ctrl Pts',(76.0424582865173,-24.6976449914384,
17.8479876926675));
#260790=CARTESIAN_POINT('Ctrl Pts',(76.0424582865173,-24.6976449914384,
17.8479876926675));
#260791=CARTESIAN_POINT('Ctrl Pts',(76.0424582865173,-24.6976449914384,
17.8479876926675));
#260792=CARTESIAN_POINT('Ctrl Pts',(-10.5032495111116,73.8913131000538,
42.8625));
#260793=CARTESIAN_POINT('Ctrl Pts',(-10.8194981777074,76.1161511576644,
42.8625));
#260794=CARTESIAN_POINT('Ctrl Pts',(-10.8580391950582,76.3872907109282,
40.6320481322491));
#260795=CARTESIAN_POINT('Ctrl Pts',(-10.0498719735697,73.9557582643349,
42.8625));
#260796=CARTESIAN_POINT('Ctrl Pts',(-10.6359163209588,76.1470117154128,
42.8625));
#260797=CARTESIAN_POINT('Ctrl Pts',(-10.7069125966304,76.4094233456861,
40.6268004742471));
#260798=CARTESIAN_POINT('Ctrl Pts',(-9.61416596216602,74.1010554093231,
42.8625));
#260799=CARTESIAN_POINT('Ctrl Pts',(-10.4617751497477,76.2168938632405,
42.8625));
#260800=CARTESIAN_POINT('Ctrl Pts',(-10.5616780116939,76.4593229171357,
40.6149692390278));
#260801=CARTESIAN_POINT('Ctrl Pts',(-9.01121135502815,74.4321791952113,
42.8625));
#260802=CARTESIAN_POINT('Ctrl Pts',(-10.2324603050541,76.3707063913054,
42.8625));
#260803=CARTESIAN_POINT('Ctrl Pts',(-10.3606931432216,76.5730413834782,
40.5880065872607));
#260804=CARTESIAN_POINT('Ctrl Pts',(-8.82276685013128,74.5591463206078,
42.8625));
#260805=CARTESIAN_POINT('Ctrl Pts',(-10.1626132722428,76.429280000154,42.8624999999992));
#260806=CARTESIAN_POINT('Ctrl Pts',(-10.2978783081087,76.6166459400673,
40.5776679558998));
#260807=CARTESIAN_POINT('Ctrl Pts',(-8.47012856407996,74.8451674277979,
42.8625));
#260808=CARTESIAN_POINT('Ctrl Pts',(-10.0366590959459,76.5589310255573,
42.8625000000008));
#260809=CARTESIAN_POINT('Ctrl Pts',(-10.1803322126703,76.7148746948338,
40.5543779788271));
#260810=CARTESIAN_POINT('Ctrl Pts',(-8.30454355451,75.0059528700596,42.8625));
#260811=CARTESIAN_POINT('Ctrl Pts',(-9.98011487798406,76.6308815760035,
42.8625));
#260812=CARTESIAN_POINT('Ctrl Pts',(-10.1251372092705,76.7700935312232,
40.5412856450937));
#260813=CARTESIAN_POINT('Ctrl Pts',(-8.00653344424111,75.3526470955157,
42.8625));
#260814=CARTESIAN_POINT('Ctrl Pts',(-9.88423732636679,76.7826313398306,
42.8625));
#260815=CARTESIAN_POINT('Ctrl Pts',(-10.0258005063557,76.889159348055,40.5130553109125));
#260816=CARTESIAN_POINT('Ctrl Pts',(-7.87453768264795,75.537341674481,42.8625));
#260817=CARTESIAN_POINT('Ctrl Pts',(-9.84501292103885,76.862025038882,42.8625));
#260818=CARTESIAN_POINT('Ctrl Pts',(-9.98180191901158,76.9525893314949,
40.4980161791992));
#260819=CARTESIAN_POINT('Ctrl Pts',(-7.64384406928706,75.9289449770848,
42.8625));
#260820=CARTESIAN_POINT('Ctrl Pts',(-9.7832976556328,77.026013436169,42.8625));
#260821=CARTESIAN_POINT('Ctrl Pts',(-9.90490404767533,77.087078327256,40.4661291586505));
#260822=CARTESIAN_POINT('Ctrl Pts',(-7.54449579085874,76.138073277502,42.8625));
#260823=CARTESIAN_POINT('Ctrl Pts',(-9.76082396850354,77.1115552436014,
42.8625));
#260824=CARTESIAN_POINT('Ctrl Pts',(-9.87178795472008,77.1588996123912,
40.4491005377577));
#260825=CARTESIAN_POINT('Ctrl Pts',(-7.30715555334537,76.77968408777,42.8625));
#260826=CARTESIAN_POINT('Ctrl Pts',(-9.72005612520358,77.3667579800968,
42.8625));
#260827=CARTESIAN_POINT('Ctrl Pts',(-9.79267454297696,77.3792490712788,
40.3968564392364));
#260828=CARTESIAN_POINT('Ctrl Pts',(-7.22543403834982,77.2295173162425,
42.8625));
#260829=CARTESIAN_POINT('Ctrl Pts',(-9.72799316153702,77.5349482149457,
42.8625000000016));
#260830=CARTESIAN_POINT('Ctrl Pts',(-9.76543403703142,77.53373600667,40.360228281325));
#260831=CARTESIAN_POINT('Ctrl Pts',(-7.22543403703142,77.692863772622,42.8625));
#260832=CARTESIAN_POINT('Ctrl Pts',(-9.76543403703142,77.6928637726221,
42.8625));
#260833=CARTESIAN_POINT('Ctrl Pts',(-9.76543403703142,77.6928637726221,
40.3225));
#260834=CARTESIAN_POINT('Origin',(-7.22543403703142,77.692863772622,40.3225000000001));
#260835=CARTESIAN_POINT('Origin',(-7.22543403703142,0.,40.3225));
#260836=CARTESIAN_POINT('Ctrl Pts',(-9.76543403703143,80.6811576396149,
40.3225));
#260837=CARTESIAN_POINT('Ctrl Pts',(-9.76543403703143,80.6811576396149,
40.5734833092634));
#260838=CARTESIAN_POINT('Ctrl Pts',(-9.72826133827436,80.6482300667132,
40.8191813005851));
#260839=CARTESIAN_POINT('Ctrl Pts',(-9.57979077264777,80.5164913076875,
41.3141267879751));
#260840=CARTESIAN_POINT('Ctrl Pts',(-9.46269022074881,80.4125005677019,
41.5513261178172));
#260841=CARTESIAN_POINT('Ctrl Pts',(-9.13655730339021,80.1220365304268,
42.0266708314762));
#260842=CARTESIAN_POINT('Ctrl Pts',(-8.91315643821528,79.9225400586233,
42.243196993227));
#260843=CARTESIAN_POINT('Ctrl Pts',(-8.4557159958063,79.5121708037282,42.5602310880019));
#260844=CARTESIAN_POINT('Ctrl Pts',(-8.22361432068508,79.3032203173786,
42.6713019811039));
#260845=CARTESIAN_POINT('Ctrl Pts',(-7.73973487957791,78.8657441556769,
42.8233283921749));
#260846=CARTESIAN_POINT('Ctrl Pts',(-7.48535212294286,78.6347875624617,
42.8617809540987));
#260847=CARTESIAN_POINT('Ctrl Pts',(-7.23018356331462,78.4020741645152,
42.8624966696506));
#260848=CARTESIAN_POINT('Ctrl Pts',(-7.22780877734985,78.3999082730286,
42.8625));
#260849=CARTESIAN_POINT('Ctrl Pts',(-7.22543403703142,78.3977423334149,
42.8625));
#260850=CARTESIAN_POINT('Ctrl Pts',(7.2254340370314,77.6928637726221,42.8625));
#260851=CARTESIAN_POINT('Ctrl Pts',(9.7654340370314,77.6928637726221,42.8625));
#260852=CARTESIAN_POINT('Ctrl Pts',(9.7654340370314,77.6928637726221,40.3225));
#260853=CARTESIAN_POINT('Ctrl Pts',(7.22543404223311,77.2344170949798,42.8625));
#260854=CARTESIAN_POINT('Ctrl Pts',(9.72839370096131,77.5366375762832,42.8625));
#260855=CARTESIAN_POINT('Ctrl Pts',(9.76543403703139,77.5354187456466,40.3598293135595));
#260856=CARTESIAN_POINT('Ctrl Pts',(7.30588292190357,76.7834773995825,42.8625));
#260857=CARTESIAN_POINT('Ctrl Pts',(9.71986880761174,77.3682612423042,42.8625));
#260858=CARTESIAN_POINT('Ctrl Pts',(9.79225033127547,77.3805518141073,40.3965475634802));
#260859=CARTESIAN_POINT('Ctrl Pts',(7.54459734351766,76.1376228588779,42.8625));
#260860=CARTESIAN_POINT('Ctrl Pts',(9.76082461763374,77.1113880289587,42.8625));
#260861=CARTESIAN_POINT('Ctrl Pts',(9.87182180621682,77.1587449246315,40.4491372136505));
#260862=CARTESIAN_POINT('Ctrl Pts',(7.6421466156822,75.9323032890386,42.8625));
#260863=CARTESIAN_POINT('Ctrl Pts',(9.78289158219672,77.0273950913578,42.8625));
#260864=CARTESIAN_POINT('Ctrl Pts',(9.9043382299849,77.0882316781324,40.4658557023577));
#260865=CARTESIAN_POINT('Ctrl Pts',(7.87211185551081,75.5409911144992,42.8625));
#260866=CARTESIAN_POINT('Ctrl Pts',(9.84431775555056,76.8635766939471,42.8625));
#260867=CARTESIAN_POINT('Ctrl Pts',(9.98099330978796,76.9538426649305,40.4977190163966));
#260868=CARTESIAN_POINT('Ctrl Pts',(8.00581438906634,75.3535555307654,42.8625));
#260869=CARTESIAN_POINT('Ctrl Pts',(9.88401297106729,76.7830262232379,42.8624999999992));
#260870=CARTESIAN_POINT('Ctrl Pts',(10.0255608207902,76.8894713331461,40.5129813396039));
#260871=CARTESIAN_POINT('Ctrl Pts',(8.30424197032195,75.0062320553663,42.8625));
#260872=CARTESIAN_POINT('Ctrl Pts',(9.9800101345932,76.6310079116545,42.8625000000008));
#260873=CARTESIAN_POINT('Ctrl Pts',(10.1250366817144,76.7701894127781,40.5412629118058));
#260874=CARTESIAN_POINT('Ctrl Pts',(8.46708944384426,74.8479469686107,42.8625));
#260875=CARTESIAN_POINT('Ctrl Pts',(10.0356040736642,76.5601795029381,42.8625));
#260876=CARTESIAN_POINT('Ctrl Pts',(10.1793191727176,76.7158292777585,40.5541516480795));
#260877=CARTESIAN_POINT('Ctrl Pts',(8.81948930738161,74.5614957425962,42.8625));
#260878=CARTESIAN_POINT('Ctrl Pts',(10.1614125709453,76.43035700652,42.8625));
#260879=CARTESIAN_POINT('Ctrl Pts',(10.296785793733,76.6174528062696,40.5774766481521));
#260880=CARTESIAN_POINT('Ctrl Pts',(9.01115900281434,74.4322732113038,42.8625));
#260881=CARTESIAN_POINT('Ctrl Pts',(10.2324466057663,76.3707480311754,42.8625));
#260882=CARTESIAN_POINT('Ctrl Pts',(10.3606756921529,76.573073670993,40.5879989317086));
#260883=CARTESIAN_POINT('Ctrl Pts',(9.61177309064578,74.1022393738552,42.8625));
#260884=CARTESIAN_POINT('Ctrl Pts',(10.4608564764661,76.2174456694345,42.8625));
#260885=CARTESIAN_POINT('Ctrl Pts',(10.5608803885151,76.459729529522,40.6148728315803));
#260886=CARTESIAN_POINT('Ctrl Pts',(10.0442301749684,73.9565602111107,42.8625));
#260887=CARTESIAN_POINT('Ctrl Pts',(10.6336336926735,76.1473954357262,42.8625));
#260888=CARTESIAN_POINT('Ctrl Pts',(10.7050285749523,76.4096992633537,40.6267350470548));
#260889=CARTESIAN_POINT('Ctrl Pts',(10.5032495111116,73.8913131000538,42.8625));
#260890=CARTESIAN_POINT('Ctrl Pts',(10.8194981777074,76.1161511576644,42.8625));
#260891=CARTESIAN_POINT('Ctrl Pts',(10.8580391950581,76.3872907109282,40.6320481322491));
#260892=CARTESIAN_POINT('Origin',(7.22543403703139,77.6928637726221,40.3225));
#260893=CARTESIAN_POINT('Origin',(-2.7565840235444E-14,7.21644966006352E-13,
40.3225));
#260894=CARTESIAN_POINT('Ctrl Pts',(9.76543403703141,80.6811576396149,40.3225));
#260895=CARTESIAN_POINT('Ctrl Pts',(9.76543403703141,80.6811576396149,40.5734833092633));
#260896=CARTESIAN_POINT('Ctrl Pts',(9.72826133827443,80.6482300667132,40.819181300585));
#260897=CARTESIAN_POINT('Ctrl Pts',(9.57979077264777,80.5164913076875,41.3141267879752));
#260898=CARTESIAN_POINT('Ctrl Pts',(9.46269022074867,80.4125005677018,41.5513261178174));
#260899=CARTESIAN_POINT('Ctrl Pts',(9.13655730339017,80.1220365304269,42.0266708314761));
#260900=CARTESIAN_POINT('Ctrl Pts',(8.91315643821524,79.9225400586233,42.243196993227));
#260901=CARTESIAN_POINT('Ctrl Pts',(8.45571599580626,79.5121708037282,42.5602310880019));
#260902=CARTESIAN_POINT('Ctrl Pts',(8.22361432068505,79.3032203173786,42.6713019811039));
#260903=CARTESIAN_POINT('Ctrl Pts',(7.73973487957849,78.8657441556775,42.8233283921747));
#260904=CARTESIAN_POINT('Ctrl Pts',(7.4853521229467,78.6347875624646,42.8617809540987));
#260905=CARTESIAN_POINT('Ctrl Pts',(7.23018356331449,78.4020741645151,42.8624966696506));
#260906=CARTESIAN_POINT('Ctrl Pts',(7.2278087773499,78.3999082730286,42.8625));
#260907=CARTESIAN_POINT('Ctrl Pts',(7.22543403703139,78.3977423334149,42.8625));
#260908=CARTESIAN_POINT('Origin',(7.22543403703139,0.,40.3225));
#260909=CARTESIAN_POINT('Origin',(0.,92.7,30.1625));
#260910=CARTESIAN_POINT('',(-0.952500000000001,92.7,30.1625));
#260911=CARTESIAN_POINT('',(0.952500000000001,92.7,30.1625));
#260912=CARTESIAN_POINT('Origin',(0.,92.7,30.1625));
#260913=CARTESIAN_POINT('Origin',(-5.80244527768194,66.322253007815,4.445));
#260914=CARTESIAN_POINT('',(-7.70019617754672,66.1562213178808,4.445));
#260915=CARTESIAN_POINT('',(-5.80244527768194,66.322253007815,6.35));
#260916=CARTESIAN_POINT('Origin',(-5.80244527768194,66.322253007815,4.445));
#260917=CARTESIAN_POINT('',(-7.67883747572177,66.2094701536372,4.445));
#260918=CARTESIAN_POINT('Origin',(-7.63693781421789,66.1617557075452,4.445));
#260919=CARTESIAN_POINT('Origin',(-5.80690631599121,66.3732429090145,4.445));
#260920=CARTESIAN_POINT('Origin',(-5.80244527768194,66.322253007815,4.445));
#260921=CARTESIAN_POINT('Origin',(-5.79969559744267,66.2908240188643,4.445));
#260922=CARTESIAN_POINT('',(-3.9019446975779,66.4568557087986,4.445));
#260923=CARTESIAN_POINT('',(-5.79969559744267,66.2908240188643,6.35));
#260924=CARTESIAN_POINT('Origin',(-5.79969559744267,66.2908240188643,4.445));
#260925=CARTESIAN_POINT('',(-3.95966867124224,66.3880629558053,4.445));
#260926=CARTESIAN_POINT('Origin',(-3.96520306090672,66.4513213191341,4.445));
#260927=CARTESIAN_POINT('Origin',(-5.79416120777819,66.2275656555355,4.445));
#260928=CARTESIAN_POINT('Origin',(-5.79969559744267,66.2908240188643,4.445));
#260929=CARTESIAN_POINT('Ctrl Pts',(-5.62465651441568,65.8691607435455,
5.70752129153081));
#260930=CARTESIAN_POINT('Ctrl Pts',(-5.63790471104907,65.7947780994363,
5.5263494271517));
#260931=CARTESIAN_POINT('Ctrl Pts',(-5.65892533799205,65.793128368605,5.33119064940291));
#260932=CARTESIAN_POINT('Ctrl Pts',(-5.78778340659959,65.8551936059547,
5.72536825578739));
#260933=CARTESIAN_POINT('Ctrl Pts',(-5.77764549719958,65.7827958377032,
5.5416830532429));
#260934=CARTESIAN_POINT('Ctrl Pts',(-5.77361112064157,65.7832641425467,
5.34381854412852));
#260935=CARTESIAN_POINT('Ctrl Pts',(-5.95339386843844,65.8404505247366,
5.71116838370947));
#260936=CARTESIAN_POINT('Ctrl Pts',(-5.91972549086594,65.7701600468525,
5.52945686894868));
#260937=CARTESIAN_POINT('Ctrl Pts',(-5.89048374747282,65.7728957801126,
5.33371655958433));
#260938=CARTESIAN_POINT('Ctrl Pts',(-6.19051191645161,65.8185545400719,
5.64266439295642));
#260939=CARTESIAN_POINT('Ctrl Pts',(-6.12280879673811,65.7514893855043,
5.47063103361691));
#260940=CARTESIAN_POINT('Ctrl Pts',(-6.05710404049759,65.7576898743807,
5.28531446245343));
#260941=CARTESIAN_POINT('Ctrl Pts',(-6.26635324587272,65.8114233229095,
5.61246633480641));
#260942=CARTESIAN_POINT('Ctrl Pts',(-6.18780235406067,65.745412351332,5.44468251173949));
#260943=CARTESIAN_POINT('Ctrl Pts',(-6.11047600283212,65.7527482825607,
5.2639426202062));
#260944=CARTESIAN_POINT('Ctrl Pts',(-6.41227161791133,65.7974900401404,
5.5372277684103));
#260945=CARTESIAN_POINT('Ctrl Pts',(-6.31273591873296,65.7335644293773,
5.38009364421865));
#260946=CARTESIAN_POINT('Ctrl Pts',(-6.21292662446779,65.7431469168115,
5.2108238923688));
#260947=CARTESIAN_POINT('Ctrl Pts',(-6.48267530224625,65.7906533823261,
5.49171207331871));
#260948=CARTESIAN_POINT('Ctrl Pts',(-6.37301403184221,65.7277587397228,
5.34101748828414));
#260949=CARTESIAN_POINT('Ctrl Pts',(-6.26235611220587,65.7384524764899,
5.17868364459097));
#260950=CARTESIAN_POINT('Ctrl Pts',(-6.67625832145065,65.771609690581,5.3375639439796));
#260951=CARTESIAN_POINT('Ctrl Pts',(-6.53859812806969,65.7116183426713,
5.20882050652558));
#260952=CARTESIAN_POINT('Ctrl Pts',(-6.39793957073026,65.7254424976304,
5.0701310476513));
#260953=CARTESIAN_POINT('Ctrl Pts',(-6.78626175412378,65.7604319347151,
5.20765442851689));
#260954=CARTESIAN_POINT('Ctrl Pts',(-6.63260327913571,65.7021800114779,
5.09750267265541));
#260955=CARTESIAN_POINT('Ctrl Pts',(-6.47480199997683,65.7178765272223,
4.97884055097215));
#260956=CARTESIAN_POINT('Ctrl Pts',(-6.94711837759049,65.7439022860098,
4.91695248025269));
#260957=CARTESIAN_POINT('Ctrl Pts',(-6.76998082727741,65.6882320874307,
4.84858322570707));
#260958=CARTESIAN_POINT('Ctrl Pts',(-6.58701829346881,65.7067237529874,
4.7749299918791));
#260959=CARTESIAN_POINT('Ctrl Pts',(-6.99956413262688,65.7383832850395,
4.75269553806659));
#260960=CARTESIAN_POINT('Ctrl Pts',(-6.81469918225909,65.6835983754984,
4.70817642224148));
#260961=CARTESIAN_POINT('Ctrl Pts',(-6.62345593201658,65.7030378048493,
4.66021655474088));
#260962=CARTESIAN_POINT('Ctrl Pts',(-7.03663553754223,65.7344992036835,
4.42043150549321));
#260963=CARTESIAN_POINT('Ctrl Pts',(-6.84632924814695,65.680326321646,4.42392531515964));
#260964=CARTESIAN_POINT('Ctrl Pts',(-6.64925400403071,65.7004320115443,
4.42768942481514));
#260965=CARTESIAN_POINT('Ctrl Pts',(-7.02175067111833,65.7360778057269,
4.2482238053988));
#260966=CARTESIAN_POINT('Ctrl Pts',(-6.83369078626271,65.6816453095259,
4.27696682318786));
#260967=CARTESIAN_POINT('Ctrl Pts',(-6.63902317906353,65.7014735525984,
4.30793133907197));
#260968=CARTESIAN_POINT('Ctrl Pts',(-6.95157881920653,65.7433920557505,
4.00755588597506));
#260969=CARTESIAN_POINT('Ctrl Pts',(-6.77373147910964,65.687815467461,4.07078461642782));
#260970=CARTESIAN_POINT('Ctrl Pts',(-6.59000859522952,65.7064017694204,
4.13890003156499));
#260971=CARTESIAN_POINT('Ctrl Pts',(-6.91964686688078,65.7467134097066,
3.92826718530274));
#260972=CARTESIAN_POINT('Ctrl Pts',(-6.74651699790575,65.6906072261033,
4.00306354599665));
#260973=CARTESIAN_POINT('Ctrl Pts',(-6.56784982525329,65.7086239030736,
4.08364051696471));
#260974=CARTESIAN_POINT('Ctrl Pts',(-6.84256578106127,65.7546542138477,
3.78073711455572));
#260975=CARTESIAN_POINT('Ctrl Pts',(-6.68069740936757,65.6973018864277,
3.87676636256858));
#260976=CARTESIAN_POINT('Ctrl Pts',(-6.51409836326281,65.7139743814014,
3.98021640596179));
#260977=CARTESIAN_POINT('Ctrl Pts',(-6.79735138508887,65.7592837801704,
3.71148839023358));
#260978=CARTESIAN_POINT('Ctrl Pts',(-6.6419854773461,65.701216650196,3.81734832354759));
#260979=CARTESIAN_POINT('Ctrl Pts',(-6.48235366389942,65.7171182506776,
3.93138820287611));
#260980=CARTESIAN_POINT('Ctrl Pts',(-6.63878879347099,65.775312120901,3.51465375123548));
#260981=CARTESIAN_POINT('Ctrl Pts',(-6.50675035368678,65.7147367021846,
3.64903407158234));
#260982=CARTESIAN_POINT('Ctrl Pts',(-6.37211727164478,65.7279297649216,
3.79379510141207));
#260983=CARTESIAN_POINT('Ctrl Pts',(-6.51075654656604,65.7880289020976,
3.40837559058612));
#260984=CARTESIAN_POINT('Ctrl Pts',(-6.3970094597364,65.7255268760605,3.55761353944892));
#260985=CARTESIAN_POINT('Ctrl Pts',(-6.28197311160879,65.7366443924548,
3.71837851255275));
#260986=CARTESIAN_POINT('Ctrl Pts',(-6.22090193659141,65.8158107296672,
3.25007929659638));
#260987=CARTESIAN_POINT('Ctrl Pts',(-6.1489336050582,65.7491363445969,3.42177380399819));
#260988=CARTESIAN_POINT('Ctrl Pts',(-6.07865960801857,65.7557563971943,
3.60672526232144));
#260989=CARTESIAN_POINT('Ctrl Pts',(-6.063764387523,65.830429565192,3.20051147934914));
#260990=CARTESIAN_POINT('Ctrl Pts',(-6.01420487377899,65.7616099376474,
3.37914354468415));
#260991=CARTESIAN_POINT('Ctrl Pts',(-5.96793753428448,65.7659218676103,
3.57156666118844));
#260992=CARTESIAN_POINT('Ctrl Pts',(-5.89874125546025,65.8451815059264,
3.18246633414093));
#260993=CARTESIAN_POINT('Ctrl Pts',(-5.8728108939582,65.7742266046314,3.36364162741095));
#260994=CARTESIAN_POINT('Ctrl Pts',(-5.85185860383796,65.7762489610748,
3.55880407300439));
#260995=CARTESIAN_POINT('',(-5.89874124598147,65.8451814395652,3.18246636753802));
#260996=CARTESIAN_POINT('',(-5.76176670013149,65.8572952859405,5.715));
#260997=CARTESIAN_POINT('Ctrl Pts',(-5.89874124128049,65.8451813460936,
3.18246633411965));
#260998=CARTESIAN_POINT('Ctrl Pts',(-5.91453706816504,65.8437693867186,
3.18419359570151));
#260999=CARTESIAN_POINT('Ctrl Pts',(-5.93059885152208,65.8423280911914,
3.18625668216982));
#261000=CARTESIAN_POINT('Ctrl Pts',(-5.94657746690739,65.8408892064149,
3.18862589385767));
#261001=CARTESIAN_POINT('Ctrl Pts',(-5.96270790642316,65.839436649776,3.19101761710211));
#261002=CARTESIAN_POINT('Ctrl Pts',(-5.97875324884626,65.8379865797637,
3.1937213007479));
#261003=CARTESIAN_POINT('Ctrl Pts',(-5.99436250455736,65.8365709410658,
3.19665315116031));
#261004=CARTESIAN_POINT('Ctrl Pts',(-6.0021360594916,65.8358659397904,3.19811324001154));
#261005=CARTESIAN_POINT('Ctrl Pts',(-6.00980161978126,65.835169463883,3.19962909119738));
#261006=CARTESIAN_POINT('Ctrl Pts',(-6.01731694016751,65.8344853621198,
3.2011857013321));
#261007=CARTESIAN_POINT('Ctrl Pts',(-6.05487166684455,65.8310668445558,
3.20896422109546));
#261008=CARTESIAN_POINT('Ctrl Pts',(-6.092920386141,65.8275735275046,3.21863403952643));
#261009=CARTESIAN_POINT('Ctrl Pts',(-6.13123923038697,65.8240249968494,
3.23038727980661));
#261010=CARTESIAN_POINT('Ctrl Pts',(-6.15039865250996,65.8222507315218,
3.2362638999467));
#261011=CARTESIAN_POINT('Ctrl Pts',(-6.16962494894135,65.8204627202671,
3.24266113654303));
#261012=CARTESIAN_POINT('Ctrl Pts',(-6.18888612199635,65.8186637625198,
3.24960122559044));
#261013=CARTESIAN_POINT('Ctrl Pts',(-6.19851670852385,65.8177642836462,
3.25307127011415));
#261014=CARTESIAN_POINT('Ctrl Pts',(-6.20815601600891,65.8168620679918,
3.25667702289134));
#261015=CARTESIAN_POINT('Ctrl Pts',(-6.21779972592886,65.8159574933785,
3.26042110097521));
#261016=CARTESIAN_POINT('Ctrl Pts',(-6.22354858670786,65.8154182534429,
3.26265304115472));
#261017=CARTESIAN_POINT('Ctrl Pts',(-6.22977209879967,65.8148336278359,
3.26512271208716));
#261018=CARTESIAN_POINT('Ctrl Pts',(-6.23562008984126,65.8142836562234,
3.26749611071574));
#261019=CARTESIAN_POINT('Ctrl Pts',(-6.2395820996655,65.8139110508422,3.26910408662001));
#261020=CARTESIAN_POINT('Ctrl Pts',(-6.2433722047729,65.8135543114577,3.27066665087196));
#261021=CARTESIAN_POINT('Ctrl Pts',(-6.24673118035708,65.8132378771829,
3.2720673182109));
#261022=CARTESIAN_POINT('Ctrl Pts',(-6.27496153960131,65.8105784195504,
3.28383916387304));
#261023=CARTESIAN_POINT('Ctrl Pts',(-6.30403799522795,65.8078219476894,
3.29716815336018));
#261024=CARTESIAN_POINT('Ctrl Pts',(-6.33374660499682,65.8049871791206,
3.31230056833604));
#261025=CARTESIAN_POINT('Ctrl Pts',(-6.36243141784723,65.8022501003242,
3.32691150082109));
#261026=CARTESIAN_POINT('Ctrl Pts',(-6.39170562294076,65.7994400232553,
3.34320429251119));
#261027=CARTESIAN_POINT('Ctrl Pts',(-6.42132866158343,65.7965779940722,
3.36139467404666));
#261028=CARTESIAN_POINT('Ctrl Pts',(-6.43333454817107,65.7954180456213,
3.36876703244429));
#261029=CARTESIAN_POINT('Ctrl Pts',(-6.44539716698001,65.7942496131585,
3.3764509684881));
#261030=CARTESIAN_POINT('Ctrl Pts',(-6.45749812305003,65.7930743060343,
3.38446019757032));
#261031=CARTESIAN_POINT('Ctrl Pts',(-6.46235449067882,65.7926026306196,
3.38767446928749));
#261032=CARTESIAN_POINT('Ctrl Pts',(-6.46605024896355,65.7922432868207,
3.39016318463709));
#261033=CARTESIAN_POINT('Ctrl Pts',(-6.46935097253908,65.7919220986225,
3.39240185996761));
#261034=CARTESIAN_POINT('Ctrl Pts',(-6.47224219126605,65.7916407586945,
3.39436279365113));
#261035=CARTESIAN_POINT('Ctrl Pts',(-6.47482951628492,65.7913887639756,
3.39613316459923));
#261036=CARTESIAN_POINT('Ctrl Pts',(-6.47761348995547,65.7911174858446,
3.39805375361407));
#261037=CARTESIAN_POINT('Ctrl Pts',(-6.48357575222877,65.7905365064398,
3.40216695897476));
#261038=CARTESIAN_POINT('Ctrl Pts',(-6.48983134525266,65.7899261058292,
3.40655799551078));
#261039=CARTESIAN_POINT('Ctrl Pts',(-6.49636717968699,65.7892874291817,
3.41124422202922));
#261040=CARTESIAN_POINT('Ctrl Pts',(-6.50943884855564,65.7880100758867,
3.42061667506608));
#261041=CARTESIAN_POINT('Ctrl Pts',(-6.52363273791384,65.7866195086591,
3.43116809080685));
#261042=CARTESIAN_POINT('Ctrl Pts',(-6.53881665568116,65.7851272928074,
3.4430505988898));
#261043=CARTESIAN_POINT('Ctrl Pts',(-6.55465485172031,65.7835707770548,
3.45544512679351));
#261044=CARTESIAN_POINT('Ctrl Pts',(-6.57157096016989,65.7819036004173,
3.46928829748607));
#261045=CARTESIAN_POINT('Ctrl Pts',(-6.58937129934023,65.780142707847,3.48477057689116));
#261046=CARTESIAN_POINT('Ctrl Pts',(-6.60570096910835,65.7785273007531,
3.49897370569244));
#261047=CARTESIAN_POINT('Ctrl Pts',(-6.6227745709665,65.776833043257,3.51455688881379));
#261048=CARTESIAN_POINT('Ctrl Pts',(-6.64040473228574,65.7750763283395,
3.53167436232706));
#261049=CARTESIAN_POINT('Ctrl Pts',(-6.6496167612483,65.7741584179241,3.54061850406887));
#261050=CARTESIAN_POINT('Ctrl Pts',(-6.65892885831413,65.7732286293093,
3.54993916518537));
#261051=CARTESIAN_POINT('Ctrl Pts',(-6.66798038885463,65.7723231835145,
3.55928633621133));
#261052=CARTESIAN_POINT('Ctrl Pts',(-6.67703191939512,65.7714177377196,
3.5686335072373));
#261053=CARTESIAN_POINT('Ctrl Pts',(-6.68582285772196,65.7705366369923,
3.5780067897777));
#261054=CARTESIAN_POINT('Ctrl Pts',(-6.69403626419771,65.7697122795355,
3.58701472554693));
#261055=CARTESIAN_POINT('Ctrl Pts',(-6.71046307714923,65.7680635646218,
3.6050305970854));
#261056=CARTESIAN_POINT('Ctrl Pts',(-6.72530111653888,65.7665688417378,
3.62234411642252));
#261057=CARTESIAN_POINT('Ctrl Pts',(-6.73872275617943,65.765213030129,3.63876109479846));
#261058=CARTESIAN_POINT('Ctrl Pts',(-6.7531238721136,65.7637582749212,3.65637614148517));
#261059=CARTESIAN_POINT('Ctrl Pts',(-6.7658950958259,65.7624633772103,3.67295891113754));
#261060=CARTESIAN_POINT('Ctrl Pts',(-6.7772346714358,65.7613109928834,3.68832137747729));
#261061=CARTESIAN_POINT('Ctrl Pts',(-6.78703174915314,65.7603153648987,
3.70159412081779));
#261062=CARTESIAN_POINT('Ctrl Pts',(-6.795760119052,65.7594261207258,3.71395700901375));
#261063=CARTESIAN_POINT('Ctrl Pts',(-6.80353339829515,65.7586333201509,
3.72531661708647));
#261064=CARTESIAN_POINT('Ctrl Pts',(-6.80855589015674,65.7581210737346,
3.73265631727112));
#261065=CARTESIAN_POINT('Ctrl Pts',(-6.8143994459443,65.7575251087004,3.74136671501387));
#261066=CARTESIAN_POINT('Ctrl Pts',(-6.8206226487531,65.7568895371171,3.7509519120683));
#261067=CARTESIAN_POINT('Ctrl Pts',(-6.82637393849287,65.7563021617031,
3.75981025192424));
#261068=CARTESIAN_POINT('Ctrl Pts',(-6.83244860633706,65.755681035264,3.7694160965401));
#261069=CARTESIAN_POINT('Ctrl Pts',(-6.8385324498745,65.7550579827651,3.77935205384102));
#261070=CARTESIAN_POINT('Ctrl Pts',(-6.84448373672446,65.7544485055291,
3.78907152339391));
#261071=CARTESIAN_POINT('Ctrl Pts',(-6.85044347056101,65.7538372144028,
3.79910681273385));
#261072=CARTESIAN_POINT('Ctrl Pts',(-6.8561602580791,65.7532501619865,3.80903947240748));
#261073=CARTESIAN_POINT('Ctrl Pts',(-6.85939077234152,65.7529184230165,
3.81465234478341));
#261074=CARTESIAN_POINT('Ctrl Pts',(-6.86254453502902,65.7525943517106,
3.82023193151967));
#261075=CARTESIAN_POINT('Ctrl Pts',(-6.8655825571821,65.752282091527,3.82569909457176));
#261076=CARTESIAN_POINT('Ctrl Pts',(-6.88237538588129,65.7505560567885,
3.8559191285209));
#261077=CARTESIAN_POINT('Ctrl Pts',(-6.89728625413067,65.7490172503012,
3.88565223467586));
#261078=CARTESIAN_POINT('Ctrl Pts',(-6.91054998657791,65.7476451275704,
3.91466340603655));
#261079=CARTESIAN_POINT('Ctrl Pts',(-6.91297014379172,65.7473947642026,
3.91995690814306));
#261080=CARTESIAN_POINT('Ctrl Pts',(-6.91533547889627,65.7471499488435,
3.92522651374083));
#261081=CARTESIAN_POINT('Ctrl Pts',(-6.91764743439568,65.7469105552903,
3.93047097789414));
#261082=CARTESIAN_POINT('Ctrl Pts',(-6.92242338991714,65.7464160245944,
3.94130480559387));
#261083=CARTESIAN_POINT('Ctrl Pts',(-6.92710067411788,65.745931219565,3.95231420713329));
#261084=CARTESIAN_POINT('Ctrl Pts',(-6.93181538577873,65.7454422461516,
3.96389252435494));
#261085=CARTESIAN_POINT('Ctrl Pts',(-6.93449595269714,65.7451642384918,
3.97047541984203));
#261086=CARTESIAN_POINT('Ctrl Pts',(-6.93718782216788,65.7448849530287,
3.97724254552527));
#261087=CARTESIAN_POINT('Ctrl Pts',(-6.93990887240687,65.7446024604459,
3.98426875594416));
#261088=CARTESIAN_POINT('Ctrl Pts',(-6.94741583834282,65.7438231061489,
4.00365300747972));
#261089=CARTESIAN_POINT('Ctrl Pts',(-6.95437281189231,65.7430997577542,
4.02302622213965));
#261090=CARTESIAN_POINT('Ctrl Pts',(-6.96080003035281,65.7424306447279,
4.04235399436845));
#261091=CARTESIAN_POINT('Ctrl Pts',(-6.97365446727381,65.7410924186753,
4.08100953882604));
#261092=CARTESIAN_POINT('Ctrl Pts',(-6.98438972241911,65.7399711482183,
4.11948337297493));
#261093=CARTESIAN_POINT('Ctrl Pts',(-6.99318642138732,65.7390510306648,
4.1575395955445));
#261094=CARTESIAN_POINT('Ctrl Pts',(-6.99854013800823,65.738491042349,4.1807008099996));
#261095=CARTESIAN_POINT('Ctrl Pts',(-7.00333302368036,65.7379893808958,
4.20440502108826));
#261096=CARTESIAN_POINT('Ctrl Pts',(-7.00746546267396,65.7375564545666,
4.22840798423732));
#261097=CARTESIAN_POINT('Ctrl Pts',(-7.01012303973934,65.7372780390631,
4.24384432206707));
#261098=CARTESIAN_POINT('Ctrl Pts',(-7.01250843221597,65.7370279667777,
4.25940385023512));
#261099=CARTESIAN_POINT('Ctrl Pts',(-7.01460617258545,65.7368080412401,
4.27501873030309));
#261100=CARTESIAN_POINT('Ctrl Pts',(-7.01912623074679,65.7363341617097,
4.30866453657961));
#261101=CARTESIAN_POINT('Ctrl Pts',(-7.02226976618557,65.7360039022401,
4.34220383776488));
#261102=CARTESIAN_POINT('Ctrl Pts',(-7.02409087870873,65.7358125713606,
4.37571237378465));
#261103=CARTESIAN_POINT('Ctrl Pts',(-7.02592092947349,65.735620301406,4.40938537377183));
#261104=CARTESIAN_POINT('Ctrl Pts',(-7.0264156011419,65.7355683221668,4.44302806162844));
#261105=CARTESIAN_POINT('Ctrl Pts',(-7.02557811473608,65.7356563941057,
4.47672408041568));
#261106=CARTESIAN_POINT('Ctrl Pts',(-7.02527260074477,65.7356885226386,
4.48901634584167));
#261107=CARTESIAN_POINT('Ctrl Pts',(-7.02478930660299,65.7357393325811,
4.50131571716726));
#261108=CARTESIAN_POINT('Ctrl Pts',(-7.02412666816216,65.7358089628303,
4.51362617421114));
#261109=CARTESIAN_POINT('Ctrl Pts',(-7.02261121110448,65.7359682075194,
4.54178024415509));
#261110=CARTESIAN_POINT('Ctrl Pts',(-7.02014930390684,65.7362272864016,
4.57006165151967));
#261111=CARTESIAN_POINT('Ctrl Pts',(-7.01674425656352,65.7365846781431,
4.59822734515461));
#261112=CARTESIAN_POINT('Ctrl Pts',(-7.01332971002708,65.7369430669143,
4.62647161372138));
#261113=CARTESIAN_POINT('Ctrl Pts',(-7.00896679749447,65.7374003140195,
4.65459896476515));
#261114=CARTESIAN_POINT('Ctrl Pts',(-7.00371091900996,65.7379503304987,
4.68237068653922));
#261115=CARTESIAN_POINT('Ctrl Pts',(-6.99938248507902,65.7384032918824,
4.70524185131249));
#261116=CARTESIAN_POINT('Ctrl Pts',(-6.99444945044594,65.7389190814976,
4.72787181270826));
#261117=CARTESIAN_POINT('Ctrl Pts',(-6.98896824514582,65.7394920685988,
4.75013438165693));
#261118=CARTESIAN_POINT('Ctrl Pts',(-6.98417733347399,65.7399928946836,
4.76959324071821));
#261119=CARTESIAN_POINT('Ctrl Pts',(-6.97882431758015,65.7405527989667,
4.78934227036311));
#261120=CARTESIAN_POINT('Ctrl Pts',(-6.97294530311642,65.7411665604242,
4.80909223502358));
#261121=CARTESIAN_POINT('Ctrl Pts',(-6.96708556129561,65.7417783098428,
4.82877745515604));
#261122=CARTESIAN_POINT('Ctrl Pts',(-6.96070327729375,65.7424435627342,
4.848463179883));
#261123=CARTESIAN_POINT('Ctrl Pts',(-6.95388408904521,65.7431527847758,
4.86787579382654));
#261124=CARTESIAN_POINT('Ctrl Pts',(-6.94695897889933,65.7438730231058,
4.88758994232613));
#261125=CARTESIAN_POINT('Ctrl Pts',(-6.93958340157387,65.7446385970478,
4.90702200599908));
#261126=CARTESIAN_POINT('Ctrl Pts',(-6.93189785267586,65.7454350762153,
4.92590519949645));
#261127=CARTESIAN_POINT('Ctrl Pts',(-6.92499028020138,65.746150931081,4.94287692518106));
#261128=CARTESIAN_POINT('Ctrl Pts',(-6.91783323848293,65.7468916701725,
4.95940543329911));
#261129=CARTESIAN_POINT('Ctrl Pts',(-6.91056037343467,65.7476440483002,
4.97531387376239));
#261130=CARTESIAN_POINT('Ctrl Pts',(-6.89741820969321,65.7490036055702,
5.00406063697777));
#261131=CARTESIAN_POINT('Ctrl Pts',(-6.88265306472704,65.7505274323005,
5.03352893815075));
#261132=CARTESIAN_POINT('Ctrl Pts',(-6.86603348701363,65.7522357778755,
5.06348872824643));
#261133=CARTESIAN_POINT('Ctrl Pts',(-6.86284470051636,65.75256355692,5.06923709175876));
#261134=CARTESIAN_POINT('Ctrl Pts',(-6.85958766659747,65.7528981269418,
5.07500339655698));
#261135=CARTESIAN_POINT('Ctrl Pts',(-6.856260788359,65.7532396276514,5.08078579696316));
#261136=CARTESIAN_POINT('Ctrl Pts',(-6.8459277014796,65.7543003086407,5.09874559034469));
#261137=CARTESIAN_POINT('Ctrl Pts',(-6.83492067751536,65.7554278628972,
5.11686118101104));
#261138=CARTESIAN_POINT('Ctrl Pts',(-6.82319313264974,65.7566263659764,
5.135072656704));
#261139=CARTESIAN_POINT('Ctrl Pts',(-6.82026124643334,65.7569259917462,
5.13962552562724));
#261140=CARTESIAN_POINT('Ctrl Pts',(-6.81728431941741,65.7572300525387,
5.14418438193023));
#261141=CARTESIAN_POINT('Ctrl Pts',(-6.81426168033028,65.7575386070824,
5.14874816890694));
#261142=CARTESIAN_POINT('Ctrl Pts',(-6.81206183096614,65.757763170286,5.15206965175335));
#261143=CARTESIAN_POINT('Ctrl Pts',(-6.81081436432581,65.7578904337753,
5.15392926336868));
#261144=CARTESIAN_POINT('Ctrl Pts',(-6.80954130507221,65.7580203548224,
5.1558237372768));
#261145=CARTESIAN_POINT('Ctrl Pts',(-6.80906515425585,65.7580689480144,
5.15653231018524));
#261146=CARTESIAN_POINT('Ctrl Pts',(-6.80858497267273,65.7581179523965,
5.15724545910831));
#261147=CARTESIAN_POINT('Ctrl Pts',(-6.80804822984616,65.7581727169983,
5.15804058038008));
#261148=CARTESIAN_POINT('Ctrl Pts',(-6.80410462238006,65.7585750886402,
5.16388257030264));
#261149=CARTESIAN_POINT('Ctrl Pts',(-6.79988716877684,65.7590052079178,
5.17002569950334));
#261150=CARTESIAN_POINT('Ctrl Pts',(-6.79537903268354,65.7594645478209,
5.17645687223928));
#261151=CARTESIAN_POINT('Ctrl Pts',(-6.78580277267813,65.7604402855208,
5.19011807966171));
#261152=CARTESIAN_POINT('Ctrl Pts',(-6.77491644358952,65.761547737429,5.20508192788034));
#261153=CARTESIAN_POINT('Ctrl Pts',(-6.76253880448289,65.7628027600726,
5.22119211573532));
#261154=CARTESIAN_POINT('Ctrl Pts',(-6.75160877166964,65.7639110036203,
5.23541816323643));
#261155=CARTESIAN_POINT('Ctrl Pts',(-6.73951519499464,65.7651343766085,
5.25053774026995));
#261156=CARTESIAN_POINT('Ctrl Pts',(-6.72611969221624,65.7664849859145,
5.26641222989509));
#261157=CARTESIAN_POINT('Ctrl Pts',(-6.71183711917666,65.7679250345921,
5.28333795200408));
#261158=CARTESIAN_POINT('Ctrl Pts',(-6.69607408882078,65.7695097633137,
5.30112266565437));
#261159=CARTESIAN_POINT('Ctrl Pts',(-6.67865372552338,65.7712546466914,
5.31955642099153));
#261160=CARTESIAN_POINT('Ctrl Pts',(-6.67055762604082,65.7720655798028,
5.32812349358921));
#261161=CARTESIAN_POINT('Ctrl Pts',(-6.6620509552059,65.7729164113109,5.33687924790332));
#261162=CARTESIAN_POINT('Ctrl Pts',(-6.65344510022094,65.7737755720605,
5.34548002799559));
#261163=CARTESIAN_POINT('Ctrl Pts',(-6.64477621580735,65.774641025318,5.3541438003479));
#261164=CARTESIAN_POINT('Ctrl Pts',(-6.63600686527661,65.7755149148551,
5.36265013683573));
#261165=CARTESIAN_POINT('Ctrl Pts',(-6.62749295825142,65.7763616805538,
5.37068603553));
#261166=CARTESIAN_POINT('Ctrl Pts',(-6.62627270638101,65.7764830428643,
5.37183777707275));
#261167=CARTESIAN_POINT('Ctrl Pts',(-6.62505776031649,65.7766038428803,
5.37297991970546));
#261168=CARTESIAN_POINT('Ctrl Pts',(-6.62384922451688,65.7767239709552,
5.37411160598602));
#261169=CARTESIAN_POINT('Ctrl Pts',(-6.60481950617975,65.7786155189177,
5.39193124457015));
#261170=CARTESIAN_POINT('Ctrl Pts',(-6.58652892184038,65.7804258306708,
5.40795995874192));
#261171=CARTESIAN_POINT('Ctrl Pts',(-6.56920790676337,65.782134745741,5.42239957587053));
#261172=CARTESIAN_POINT('Ctrl Pts',(-6.5537403803089,65.7836607930853,5.435294037248));
#261173=CARTESIAN_POINT('Ctrl Pts',(-6.53904502063578,65.785106070809,5.44692155865749));
#261174=CARTESIAN_POINT('Ctrl Pts',(-6.5252520515588,65.7864591858047,5.45741722333808));
#261175=CARTESIAN_POINT('Ctrl Pts',(-6.51063267008387,65.7878933733383,
5.46854174083263));
#261176=CARTESIAN_POINT('Ctrl Pts',(-6.49702705057888,65.7892240235553,
5.47839520486671));
#261177=CARTESIAN_POINT('Ctrl Pts',(-6.48455627972228,65.7904405427442,
5.48712222544258));
#261178=CARTESIAN_POINT('Ctrl Pts',(-6.47832089429397,65.7910488023387,
5.49148573573051));
#261179=CARTESIAN_POINT('Ctrl Pts',(-6.47236870678754,65.7916285741663,
5.49556733942024));
#261180=CARTESIAN_POINT('Ctrl Pts',(-6.46671197311601,65.7921787859736,
5.49938314995723));
#261181=CARTESIAN_POINT('Ctrl Pts',(-6.46384655950873,65.7924574952944,
5.5013160455239));
#261182=CARTESIAN_POINT('Ctrl Pts',(-6.45959513205277,65.7928706896663,
5.5041638149449));
#261183=CARTESIAN_POINT('Ctrl Pts',(-6.45490906743274,65.7933256517398,
5.5072488405822));
#261184=CARTESIAN_POINT('Ctrl Pts',(-6.45034417454503,65.7937688494551,
5.51025409397327));
#261185=CARTESIAN_POINT('Ctrl Pts',(-6.44536610427237,65.7942517463725,
5.51348319963084));
#261186=CARTESIAN_POINT('Ctrl Pts',(-6.44088172190684,65.794686236133,5.51635105564596));
#261187=CARTESIAN_POINT('Ctrl Pts',(-6.41092000451291,65.7975892132554,
5.5355121985744));
#261188=CARTESIAN_POINT('Ctrl Pts',(-6.38123637199579,65.8004462364061,
5.552713371747));
#261189=CARTESIAN_POINT('Ctrl Pts',(-6.35208534056764,65.8032350383018,
5.56816839001326));
#261190=CARTESIAN_POINT('Ctrl Pts',(-6.34586874315358,65.8038297636959,
5.57146424686228));
#261191=CARTESIAN_POINT('Ctrl Pts',(-6.33967618401766,65.8044214025736,
5.57468073798643));
#261192=CARTESIAN_POINT('Ctrl Pts',(-6.33350983849427,65.8050097646177,
5.57781999967329));
#261193=CARTESIAN_POINT('Ctrl Pts',(-6.3220951691016,65.8060988956422,5.58363116191788));
#261194=CARTESIAN_POINT('Ctrl Pts',(-6.3110960380657,65.8071462001763,5.58901693396477));
#261195=CARTESIAN_POINT('Ctrl Pts',(-6.3001362097979,65.8081871579159,5.59419568021758));
#261196=CARTESIAN_POINT('Ctrl Pts',(-6.2887742088532,65.8092663137686,5.59956446140456));
#261197=CARTESIAN_POINT('Ctrl Pts',(-6.27745426307281,65.8103386646702,
5.60471100753469));
#261198=CARTESIAN_POINT('Ctrl Pts',(-6.2657318630546,65.81144595617,5.60982619698701));
#261199=CARTESIAN_POINT('Ctrl Pts',(-6.25472797486926,65.8124853774348,
5.61462785643327));
#261200=CARTESIAN_POINT('Ctrl Pts',(-6.24336918957263,65.8135556106234,
5.61940187932597));
#261201=CARTESIAN_POINT('Ctrl Pts',(-6.23126962222113,65.8146927786727,
5.62426010254449));
#261202=CARTESIAN_POINT('Ctrl Pts',(-6.23047956672726,65.8147670313992,
5.62457732594866));
#261203=CARTESIAN_POINT('Ctrl Pts',(-6.22968634671726,65.8148415700443,
5.6248948907272));
#261204=CARTESIAN_POINT('Ctrl Pts',(-6.22888985219174,65.8149164048895,
5.62521282041139));
#261205=CARTESIAN_POINT('Ctrl Pts',(-6.19036579175731,65.8185359427609,
5.64059012932621));
#261206=CARTESIAN_POINT('Ctrl Pts',(-6.15186901093432,65.8221216693507,
5.65375153185709));
#261207=CARTESIAN_POINT('Ctrl Pts',(-6.11365657603432,65.825651094271,5.66486594522758));
#261208=CARTESIAN_POINT('Ctrl Pts',(-6.09861523048941,65.8270403619254,
5.66924084916845));
#261209=CARTESIAN_POINT('Ctrl Pts',(-6.08388431537106,65.8283967393513,
5.67322584538408));
#261210=CARTESIAN_POINT('Ctrl Pts',(-6.06913706391957,65.8297499270775,
5.67693553666014));
#261211=CARTESIAN_POINT('Ctrl Pts',(-6.054426279115,65.8310997686738,5.68063605470129));
#261212=CARTESIAN_POINT('Ctrl Pts',(-6.039698919231,65.8324464642731,5.6840626287897));
#261213=CARTESIAN_POINT('Ctrl Pts',(-6.02461786668289,65.8338206117543,
5.6872795401997));
#261214=CARTESIAN_POINT('Ctrl Pts',(-6.01640907093671,65.8345685765241,
5.6890305432291));
#261215=CARTESIAN_POINT('Ctrl Pts',(-6.00809529157055,65.8353246915127,
5.69071857742997));
#261216=CARTESIAN_POINT('Ctrl Pts',(-5.99962103174957,65.8360939900876,
5.69234758469808));
#261217=CARTESIAN_POINT('Ctrl Pts',(-5.94977634842706,65.8406189214277,
5.70192922995375));
#261218=CARTESIAN_POINT('Ctrl Pts',(-5.89974030855588,65.8451090257662,
5.7084207146655));
#261219=CARTESIAN_POINT('Ctrl Pts',(-5.84988722567234,65.8495315549123,
5.71191535187211));
#261220=CARTESIAN_POINT('Ctrl Pts',(-5.82042620503947,65.8521450787885,
5.71398053165424));
#261221=CARTESIAN_POINT('Ctrl Pts',(-5.79102856600027,65.8547350482164,
5.71500000109184));
#261222=CARTESIAN_POINT('Ctrl Pts',(-5.76176668704775,65.8572951308982,
5.715));
#261223=CARTESIAN_POINT('',(-5.85194569933787,65.7762408833968,3.55799308010885));
#261224=CARTESIAN_POINT('Origin',(-5.94198106391481,66.7882436665578,3.557992738206));
#261225=CARTESIAN_POINT('',(-5.75542126790783,65.7847570433117,5.33729874159373));
#261226=CARTESIAN_POINT('Ctrl Pts',(-5.7554212679173,65.7847570433109,5.33729874159373));
#261227=CARTESIAN_POINT('Ctrl Pts',(-5.84313044680229,65.7770834834129,
5.33729913870664));
#261228=CARTESIAN_POINT('Ctrl Pts',(-5.93046744301797,65.7692612122682,
5.32362871093108));
#261229=CARTESIAN_POINT('Ctrl Pts',(-6.01397172210868,65.7616246556023,
5.29784699382705));
#261230=CARTESIAN_POINT('Ctrl Pts',(-6.10597963581641,65.7532104323506,
5.2694398028618));
#261231=CARTESIAN_POINT('Ctrl Pts',(-6.19333444614957,65.7450218153952,
5.22632902530969));
#261232=CARTESIAN_POINT('Ctrl Pts',(-6.27141366972007,65.7375729990231,
5.17060080687608));
#261233=CARTESIAN_POINT('Ctrl Pts',(-6.30478895463498,65.7343889718603,
5.14677955093925));
#261234=CARTESIAN_POINT('Ctrl Pts',(-6.3364695108738,65.7313408750752,5.12065287386765));
#261235=CARTESIAN_POINT('Ctrl Pts',(-6.36609460015343,65.7284715535097,
5.09238371018883));
#261236=CARTESIAN_POINT('Ctrl Pts',(-6.44701031459408,65.7206345069363,
5.01517146775067));
#261237=CARTESIAN_POINT('Ctrl Pts',(-6.51382295507419,65.7140126737621,
4.92157085026347));
#261238=CARTESIAN_POINT('Ctrl Pts',(-6.56068516324688,65.7093337617069,
4.81963336896564));
#261239=CARTESIAN_POINT('Ctrl Pts',(-6.60024843912357,65.7053836045193,
4.7335729622537));
#261240=CARTESIAN_POINT('Ctrl Pts',(-6.62613370765204,65.7027670840136,
4.64058810563573));
#261241=CARTESIAN_POINT('Ctrl Pts',(-6.63690428983301,65.7016790855929,
4.54620310203547));
#261242=CARTESIAN_POINT('Ctrl Pts',(-6.63889132827675,65.7014783634172,
4.52879024286822));
#261243=CARTESIAN_POINT('Ctrl Pts',(-6.64036391441504,65.7013295239355,
4.51132972877378));
#261244=CARTESIAN_POINT('Ctrl Pts',(-6.64131300674474,65.7012335863269,
4.49385624771197));
#261245=CARTESIAN_POINT('Ctrl Pts',(-6.64633202250417,65.7007262464669,
4.40145251197823));
#261246=CARTESIAN_POINT('Ctrl Pts',(-6.63637949906751,65.7017363710718,
4.30822438948042));
#261247=CARTESIAN_POINT('Ctrl Pts',(-6.61279609273244,65.7041099251378,
4.21848944197469));
#261248=CARTESIAN_POINT('Ctrl Pts',(-6.58652533303231,65.7067539481265,
4.11852910506948));
#261249=CARTESIAN_POINT('Ctrl Pts',(-6.54334010983073,65.711089321915,4.02290340321605));
#261250=CARTESIAN_POINT('Ctrl Pts',(-6.48508720106723,65.7168378515978,
3.93758044687316));
#261251=CARTESIAN_POINT('Ctrl Pts',(-6.46865421195338,65.7184594963826,
3.9135110700385));
#261252=CARTESIAN_POINT('Ctrl Pts',(-6.45102212258308,65.7201932683606,
3.89026157430445));
#261253=CARTESIAN_POINT('Ctrl Pts',(-6.43223233013131,65.7220322302183,
3.86796593773786));
#261254=CARTESIAN_POINT('Ctrl Pts',(-6.35963673813889,65.7291371796241,
3.78182528772519));
#261255=CARTESIAN_POINT('Ctrl Pts',(-6.27057697962562,65.7377278929563,
3.71049475514339));
#261256=CARTESIAN_POINT('Ctrl Pts',(-6.1716590922992,65.747013295412,3.65761804421069));
#261257=CARTESIAN_POINT('Ctrl Pts',(-6.09089475947035,65.7545946273091,
3.61444534414512));
#261258=CARTESIAN_POINT('Ctrl Pts',(-6.00355863234323,65.7626386207393,
3.58357464837312));
#261259=CARTESIAN_POINT('Ctrl Pts',(-5.91325097800447,65.7707579102581,
3.56698920682791));
#261260=CARTESIAN_POINT('Ctrl Pts',(-5.89295235276776,65.7725828985864,
3.5632612652179));
#261261=CARTESIAN_POINT('Ctrl Pts',(-5.87250361938545,65.7744118972737,
3.56025504919194));
#261262=CARTESIAN_POINT('Ctrl Pts',(-5.85194569928665,65.7762408834014,
3.55799308057809));
#261263=CARTESIAN_POINT('',(-5.6588379396032,65.7931355567733,5.33200232567716));
#261264=CARTESIAN_POINT('Origin',(-5.75437963344684,65.7728758969229,4.44759572280564));
#261265=CARTESIAN_POINT('',(-5.62465650879763,65.8691606621927,5.70752127913496));
#261266=CARTESIAN_POINT('Origin',(-5.74590223951866,66.8053982735026,5.33200196893336));
#261267=CARTESIAN_POINT('Ctrl Pts',(-5.76176671321524,65.8572954409828,
5.715));
#261268=CARTESIAN_POINT('Ctrl Pts',(-5.73889644435691,65.8592959118043,
5.71499999912934));
#261269=CARTESIAN_POINT('Ctrl Pts',(-5.71600351087933,65.8612858392142,
5.71437328350013));
#261270=CARTESIAN_POINT('Ctrl Pts',(-5.670326752844,65.8652384015502,5.71188182802081));
#261271=CARTESIAN_POINT('Ctrl Pts',(-5.64757588348546,65.8671983519392,
5.71002878127821));
#261272=CARTESIAN_POINT('Ctrl Pts',(-5.62465651442489,65.8691607435447,
5.70752129153182));
#261273=CARTESIAN_POINT('Origin',(-3.98912952672225E-15,8.70861844988177E-14,
17.4625000000011));
#261274=CARTESIAN_POINT('',(-5.75542048012727,65.7847571122336,3.55270126407068));
#261275=CARTESIAN_POINT('Ctrl Pts',(-5.75542048012727,65.7847571122336,
3.55270126407068));
#261276=CARTESIAN_POINT('Ctrl Pts',(-5.74247305973189,65.7858898647401,
3.55270083404508));
#261277=CARTESIAN_POINT('Ctrl Pts',(-5.72728301852202,65.7872142683301,
3.55303663437051));
#261278=CARTESIAN_POINT('Ctrl Pts',(-5.71323826307051,65.7884339513264,
3.5537085593055));
#261279=CARTESIAN_POINT('Ctrl Pts',(-5.69919350761899,65.7896536343226,
3.55438048424048));
#261280=CARTESIAN_POINT('Ctrl Pts',(-5.68515719669277,65.790868052569,3.55538858394171));
#261281=CARTESIAN_POINT('Ctrl Pts',(-5.67112933463474,65.7920772227818,
3.55673285840919));
#261282=CARTESIAN_POINT('Ctrl Pts',(-5.64307361051867,65.7944955632075,
3.55942140734414));
#261283=CARTESIAN_POINT('Ctrl Pts',(-5.61564345930465,65.7968421930535,
3.56338271048258));
#261284=CARTESIAN_POINT('Ctrl Pts',(-5.58815941470242,65.7991763441953,
3.56868087970656));
#261285=CARTESIAN_POINT('Ctrl Pts',(-5.53319132549797,65.8038446464791,
3.57927721815451));
#261286=CARTESIAN_POINT('Ctrl Pts',(-5.47901133019916,65.8083759215683,
3.59514139742869));
#261287=CARTESIAN_POINT('Ctrl Pts',(-5.42652662461076,65.812703500244,3.61617550274095));
#261288=CARTESIAN_POINT('Ctrl Pts',(-5.32155721343395,65.8213586575955,
3.65824371336546));
#261289=CARTESIAN_POINT('Ctrl Pts',(-5.22615715431841,65.828968679653,3.71966185501488));
#261290=CARTESIAN_POINT('Ctrl Pts',(-5.14453528743527,65.8353468122936,
3.79734567088282));
#261291=CARTESIAN_POINT('Ctrl Pts',(-5.06291342055214,65.8417249449342,
3.87502948675077));
#261292=CARTESIAN_POINT('Ctrl Pts',(-4.99635722470383,65.846774948607,3.96823454036102));
#261293=CARTESIAN_POINT('Ctrl Pts',(-4.94933658123897,65.850309039702,4.07025885888143));
#261294=CARTESIAN_POINT('Ctrl Pts',(-4.90963743741027,65.8532928438429,
4.15639715467043));
#261295=CARTESIAN_POINT('Ctrl Pts',(-4.88363346483278,65.855215237196,4.2509570946994));
#261296=CARTESIAN_POINT('Ctrl Pts',(-4.87286763711114,65.8560118304308,
4.34458329058431));
#261297=CARTESIAN_POINT('Ctrl Pts',(-4.87088215339171,65.8561587418378,
4.36185026646838));
#261298=CARTESIAN_POINT('Ctrl Pts',(-4.86941494537251,65.8562672203297,
4.37908548343429));
#261299=CARTESIAN_POINT('Ctrl Pts',(-4.86847567621377,65.8563366564582,
4.39623025764058));
#261300=CARTESIAN_POINT('Ctrl Pts',(-4.8635283934026,65.8567023877948,4.48653456066477));
#261301=CARTESIAN_POINT('Ctrl Pts',(-4.87299393225409,65.8560065907437,
4.58113033271353));
#261302=CARTESIAN_POINT('Ctrl Pts',(-4.8961834270689,65.8542824808466,4.67087033143761));
#261303=CARTESIAN_POINT('Ctrl Pts',(-4.90126896622311,65.8539043773795,
4.69055063412873));
#261304=CARTESIAN_POINT('Ctrl Pts',(-4.90701453125571,65.8534766187393,
4.70999740297233));
#261305=CARTESIAN_POINT('Ctrl Pts',(-4.91341283206931,65.852999229802,4.72911416018214));
#261306=CARTESIAN_POINT('Ctrl Pts',(-4.94898667534586,65.8503450002287,
4.83540121118988));
#261307=CARTESIAN_POINT('Ctrl Pts',(-5.00523480399401,65.8461241794492,
4.93580822988598));
#261308=CARTESIAN_POINT('Ctrl Pts',(-5.07790028461974,65.840519909233,5.02192061733624));
#261309=CARTESIAN_POINT('Ctrl Pts',(-5.15056576524547,65.8349156390167,
5.1080330047865));
#261310=CARTESIAN_POINT('Ctrl Pts',(-5.23976344718343,65.8279111585203,
5.17939248795535));
#261311=CARTESIAN_POINT('Ctrl Pts',(-5.33881247999378,65.8198770473032,
5.23230434621982));
#261312=CARTESIAN_POINT('Ctrl Pts',(-5.41955366575217,65.8133279306911,
5.27543617755364));
#261313=CARTESIAN_POINT('Ctrl Pts',(-5.5068409177372,65.8060942041597,5.30630970940009));
#261314=CARTESIAN_POINT('Ctrl Pts',(-5.59705836360422,65.7984199726183,
5.32292362304353));
#261315=CARTESIAN_POINT('Ctrl Pts',(-5.61751492718868,65.7966798612243,
5.32669078334792));
#261316=CARTESIAN_POINT('Ctrl Pts',(-5.63812216055857,65.7949173115934,
5.32972479472675));
#261317=CARTESIAN_POINT('Ctrl Pts',(-5.6588379396032,65.7931355567733,5.33200232567716));
#261318=CARTESIAN_POINT('Ctrl Pts',(-5.85194569898496,65.7762408834282,
3.5579930805449));
#261319=CARTESIAN_POINT('Ctrl Pts',(-5.83593933394768,65.7776649292109,
3.5562322864657));
#261320=CARTESIAN_POINT('Ctrl Pts',(-5.81987010370942,65.77908866856,3.5549075948924));
#261321=CARTESIAN_POINT('Ctrl Pts',(-5.78769205961313,65.7819277211714,
3.553143174725));
#261322=CARTESIAN_POINT('Ctrl Pts',(-5.77021143863637,65.7834630710414,
3.5527017560376));
#261323=CARTESIAN_POINT('Ctrl Pts',(-5.75542048012727,65.7847571122336,
3.55270126407068));
#261324=CARTESIAN_POINT('Origin',(10.0340663510524,-114.689903201906,4.445));
#261325=CARTESIAN_POINT('',(-5.7941612077782,66.2275656555355,3.175));
#261326=CARTESIAN_POINT('Origin',(-5.7941612077782,66.2275656555355,4.445));
#261327=CARTESIAN_POINT('',(-5.7617667341226,65.8572951273169,3.175));
#261328=CARTESIAN_POINT('',(10.0340663510524,-114.689903201906,3.175));
#261329=CARTESIAN_POINT('Origin',(-5.76074896190133,65.8337676350829,4.43574689648524));
#261330=CARTESIAN_POINT('Ctrl Pts',(-5.62465649482951,65.8691605147753,
5.70752129157735));
#261331=CARTESIAN_POINT('Ctrl Pts',(-5.58478094862187,65.8725733428444,
5.70315872721441));
#261332=CARTESIAN_POINT('Ctrl Pts',(-5.54304491598344,65.8761096064448,
5.69646988868971));
#261333=CARTESIAN_POINT('Ctrl Pts',(-5.46821395219,65.8823912144796,5.68094793183612));
#261334=CARTESIAN_POINT('Ctrl Pts',(-5.43031265137476,65.8855432879058,
5.67131322823348));
#261335=CARTESIAN_POINT('Ctrl Pts',(-5.37306241680832,65.8902593919637,
5.6537697159104));
#261336=CARTESIAN_POINT('Ctrl Pts',(-5.3443386854768,65.8926143587643,5.64422545064104));
#261337=CARTESIAN_POINT('Ctrl Pts',(-5.31553775508236,65.8949585103482,
5.63347370408195));
#261338=CARTESIAN_POINT('Ctrl Pts',(-5.29632845038175,65.8965181335808,
5.6260324645471));
#261339=CARTESIAN_POINT('Ctrl Pts',(-5.28553065111783,65.8973924062449,
5.62168005422912));
#261340=CARTESIAN_POINT('Ctrl Pts',(-5.24381167530971,65.9007628197157,
5.60433180876094));
#261341=CARTESIAN_POINT('Ctrl Pts',(-5.20925335774763,65.9035306522036,
5.58828560454417));
#261342=CARTESIAN_POINT('Ctrl Pts',(-5.13848808894195,65.9091465352246,
5.55105091210214));
#261343=CARTESIAN_POINT('Ctrl Pts',(-5.10228029053816,65.9119946598744,
5.52986074877017));
#261344=CARTESIAN_POINT('Ctrl Pts',(-5.05657131457127,65.9155541063456,
5.49967414867441));
#261345=CARTESIAN_POINT('Ctrl Pts',(-5.05164098672593,65.9159368425922,
5.49630764637292));
#261346=CARTESIAN_POINT('Ctrl Pts',(-5.03965557645362,65.9168663885211,
5.48805933378198));
#261347=CARTESIAN_POINT('Ctrl Pts',(-5.02080250933399,65.9183260383822,
5.47485591449452));
#261348=CARTESIAN_POINT('Ctrl Pts',(-4.99943768814662,65.9199717860853,
5.45901019489878));
#261349=CARTESIAN_POINT('Ctrl Pts',(-4.95375363345269,65.9234768895244,
5.42334213938015));
#261350=CARTESIAN_POINT('Ctrl Pts',(-4.91931462043666,65.9261022643759,
5.39426828545766));
#261351=CARTESIAN_POINT('Ctrl Pts',(-4.86396112783238,65.9302738558047,
5.3406626551402));
#261352=CARTESIAN_POINT('Ctrl Pts',(-4.84517703641354,65.9316813708319,
5.32127488448207));
#261353=CARTESIAN_POINT('Ctrl Pts',(-4.81231674059695,65.9341341565153,
5.28534110579567));
#261354=CARTESIAN_POINT('Ctrl Pts',(-4.79747782267421,65.9352363376361,
5.26808062242643));
#261355=CARTESIAN_POINT('Ctrl Pts',(-4.75721778545189,65.9382154751491,
5.21900018510425));
#261356=CARTESIAN_POINT('Ctrl Pts',(-4.73603395996656,65.9397667249603,
5.18991521556927));
#261357=CARTESIAN_POINT('Ctrl Pts',(-4.70254379818341,65.9422125678302,
5.14118315439145));
#261358=CARTESIAN_POINT('Ctrl Pts',(-4.67680062679918,65.9440855394807,
5.10072222188373));
#261359=CARTESIAN_POINT('Ctrl Pts',(-4.63677165145856,65.9469771382894,
5.02895983248803));
#261360=CARTESIAN_POINT('Ctrl Pts',(-4.61942342781782,65.9482215759738,
4.99377678011774));
#261361=CARTESIAN_POINT('Ctrl Pts',(-4.59680525672921,65.9498382659438,
4.94262996607723));
#261362=CARTESIAN_POINT('Ctrl Pts',(-4.58952137463054,65.9503579328167,
4.92520576511086));
#261363=CARTESIAN_POINT('Ctrl Pts',(-4.57454093443883,65.9514246648816,
4.88665216134801));
#261364=CARTESIAN_POINT('Ctrl Pts',(-4.55370826475622,65.9529048689791,
4.82885958216214));
#261365=CARTESIAN_POINT('Ctrl Pts',(-4.53760876604915,65.9540412091005,
4.77148576378849));
#261366=CARTESIAN_POINT('Ctrl Pts',(-4.5199909193678,65.9552820905794,4.69582490828914));
#261367=CARTESIAN_POINT('Ctrl Pts',(-4.51262962933517,65.9557993403288,
4.65619031440224));
#261368=CARTESIAN_POINT('Ctrl Pts',(-4.49633146802346,65.9569433440707,
4.53608031601762));
#261369=CARTESIAN_POINT('Ctrl Pts',(-4.4932116366907,65.9571603038214,4.45655263790621));
#261370=CARTESIAN_POINT('Ctrl Pts',(-4.5016784398326,65.9565681203517,4.29783458701837));
#261371=CARTESIAN_POINT('Ctrl Pts',(-4.51367679322992,65.9557276352643,
4.21750115465559));
#261372=CARTESIAN_POINT('Ctrl Pts',(-4.55112069875617,65.9530883852659,
4.06510551948798));
#261373=CARTESIAN_POINT('Ctrl Pts',(-4.57940219984027,65.95108461875,3.98465833433704));
#261374=CARTESIAN_POINT('Ctrl Pts',(-4.62647759117148,65.9477157319952,
3.88166400755938));
#261375=CARTESIAN_POINT('Ctrl Pts',(-4.64448938506461,65.9464216405874,
3.8462930296191));
#261376=CARTESIAN_POINT('Ctrl Pts',(-4.67557881765161,65.9441720386244,
3.7922777912675));
#261377=CARTESIAN_POINT('Ctrl Pts',(-4.68938079462409,65.94317046133,3.76957373396999));
#261378=CARTESIAN_POINT('Ctrl Pts',(-4.70431639697893,65.9420821438308,
3.74671681689983));
#261379=CARTESIAN_POINT('Ctrl Pts',(-4.7103827143969,65.9416397563165,3.73756396983769));
#261380=CARTESIAN_POINT('Ctrl Pts',(-4.71175591745022,65.94153953322,3.73552823755546));
#261381=CARTESIAN_POINT('Ctrl Pts',(-4.71766631767027,65.9411082008532,
3.72678303218439));
#261382=CARTESIAN_POINT('Ctrl Pts',(-4.72187699968702,65.9408007204284,
3.72065685633667));
#261383=CARTESIAN_POINT('Ctrl Pts',(-4.74436504471929,65.9391564677656,
3.68860998466841));
#261384=CARTESIAN_POINT('Ctrl Pts',(-4.76692523567626,65.9375009879014,
3.65839689018539));
#261385=CARTESIAN_POINT('Ctrl Pts',(-4.80949049683516,65.9343440177535,
3.60794709652002));
#261386=CARTESIAN_POINT('Ctrl Pts',(-4.82513750608849,65.9331790153847,
3.59028425850477));
#261387=CARTESIAN_POINT('Ctrl Pts',(-4.85969448029927,65.9305934010222,
3.55367536178758));
#261388=CARTESIAN_POINT('Ctrl Pts',(-4.87913743792476,65.9291324474435,
3.53430983686811));
#261389=CARTESIAN_POINT('Ctrl Pts',(-4.93368078409887,65.9250099373155,
3.48317767954649));
#261390=CARTESIAN_POINT('Ctrl Pts',(-4.96731044415668,65.922440365982,3.45561193051492));
#261391=CARTESIAN_POINT('Ctrl Pts',(-5.01148882032945,65.9190437725999,
3.42200008030123));
#261392=CARTESIAN_POINT('Ctrl Pts',(-5.02518131852106,65.9179869304159,
3.41208793767203));
#261393=CARTESIAN_POINT('Ctrl Pts',(-5.04398394922112,65.9165309450815,
3.3989357969476));
#261394=CARTESIAN_POINT('Ctrl Pts',(-5.04996267078607,65.9160671165245,
3.39483806869276));
#261395=CARTESIAN_POINT('Ctrl Pts',(-5.06131746615798,65.9151846467314,
3.38718237834165));
#261396=CARTESIAN_POINT('Ctrl Pts',(-5.07200690120929,65.9143524134979,
3.38010441024829));
#261397=CARTESIAN_POINT('Ctrl Pts',(-5.11727986407102,65.9108170937777,
3.3511367059735));
#261398=CARTESIAN_POINT('Ctrl Pts',(-5.15308340275494,65.9079936118378,
3.33082419418418));
#261399=CARTESIAN_POINT('Ctrl Pts',(-5.20550653408049,65.9038232860139,
3.30407887907678));
#261400=CARTESIAN_POINT('Ctrl Pts',(-5.22276891828361,65.9024438445753,
3.29578390756948));
#261401=CARTESIAN_POINT('Ctrl Pts',(-5.25677913901012,65.8997142191736,
3.28033613906633));
#261402=CARTESIAN_POINT('Ctrl Pts',(-5.27289349468372,65.8984158432432,
3.27339763828448));
#261403=CARTESIAN_POINT('Ctrl Pts',(-5.33096559013756,65.8937120368811,
3.25012126608546));
#261404=CARTESIAN_POINT('Ctrl Pts',(-5.36965444985258,65.8905467713476,
3.23683858823736));
#261405=CARTESIAN_POINT('Ctrl Pts',(-5.44645936542805,65.884203038107,3.21440327730483));
#261406=CARTESIAN_POINT('Ctrl Pts',(-5.48272834473528,65.8811802522662,
3.20559401919178));
#261407=CARTESIAN_POINT('Ctrl Pts',(-5.60232583337562,65.8711124237307,
3.18249177319905));
#261408=CARTESIAN_POINT('Ctrl Pts',(-5.6825483361046,65.8642257654837,3.17499999999995));
#261409=CARTESIAN_POINT('Ctrl Pts',(-5.7617667341226,65.8572951273169,3.175));
#261410=CARTESIAN_POINT('Origin',(-5.80522998710715,66.3540823821931,4.445));
#261411=CARTESIAN_POINT('',(-5.80522998710715,66.3540823821931,6.35));
#261412=CARTESIAN_POINT('Origin',(-5.5838544005281,63.8237478490401,4.445));
#261413=CARTESIAN_POINT('',(-5.86057388375191,66.9866660154814,4.445));
#261414=CARTESIAN_POINT('Origin',(-5.5838544005281,63.8237478490401,4.445));
#261415=CARTESIAN_POINT('Origin',(-5.7941612077782,66.2275656555355,4.445));
#261416=CARTESIAN_POINT('Ctrl Pts',(-6.15431105802085,65.8219579492574,
3.2376058358314));
#261417=CARTESIAN_POINT('Ctrl Pts',(-6.09196446923405,65.7542552094537,
3.41112704653794));
#261418=CARTESIAN_POINT('Ctrl Pts',(-6.03200067711174,65.7599158653485,
3.59808142686584));
#261419=CARTESIAN_POINT('Ctrl Pts',(-5.74917274455676,65.8600210538758,
3.10349479056237));
#261420=CARTESIAN_POINT('Ctrl Pts',(-5.74441843420203,65.7867232581855,
3.29579590096035));
#261421=CARTESIAN_POINT('Ctrl Pts',(-5.74615976170068,65.7863610329078,
3.50297858761136));
#261422=CARTESIAN_POINT('Ctrl Pts',(-5.30414356229518,65.8968204131924,
3.18782913062388));
#261423=CARTESIAN_POINT('Ctrl Pts',(-5.36319861850554,65.8183839519767,
3.36843862041187));
#261424=CARTESIAN_POINT('Ctrl Pts',(-5.43332317502891,65.8125499436892,
3.56303021908321));
#261425=CARTESIAN_POINT('Ctrl Pts',(-4.84458288585805,65.9320186944127,
3.55329062024494));
#261426=CARTESIAN_POINT('Ctrl Pts',(-4.96994589552014,65.8488657795094,
3.68202484868787));
#261427=CARTESIAN_POINT('Ctrl Pts',(-5.11113200152783,65.8380126734016,
3.82073050102231));
#261428=CARTESIAN_POINT('Ctrl Pts',(-4.73576546676296,65.9400109632291,
3.68162295226985));
#261429=CARTESIAN_POINT('Ctrl Pts',(-4.87703402958295,65.8557944238857,
3.79197796828375));
#261430=CARTESIAN_POINT('Ctrl Pts',(-5.03527059122988,65.8438185211497,
3.91088264279539));
#261431=CARTESIAN_POINT('Ctrl Pts',(-4.61386911108362,65.9488102407144,
3.90174828639309));
#261432=CARTESIAN_POINT('Ctrl Pts',(-4.77298912823442,65.8634389748918,
3.9803875182256));
#261433=CARTESIAN_POINT('Ctrl Pts',(-4.95036141413464,65.8502383625224,
4.06512039686388));
#261434=CARTESIAN_POINT('Ctrl Pts',(-4.58087640128896,65.9511594036629,
3.978277556413));
#261435=CARTESIAN_POINT('Ctrl Pts',(-4.74483475405062,65.8654819452878,
4.04588200245608));
#261436=CARTESIAN_POINT('Ctrl Pts',(-4.92739373892393,65.8519572258984,
4.11872530044206));
#261437=CARTESIAN_POINT('Ctrl Pts',(-4.52999467176735,65.954763888308,4.13775932520177));
#261438=CARTESIAN_POINT('Ctrl Pts',(-4.70143575750546,65.8686166166315,
4.18229018094601));
#261439=CARTESIAN_POINT('Ctrl Pts',(-4.89201655455833,65.8545947797837,
4.23027211590684));
#261440=CARTESIAN_POINT('Ctrl Pts',(-4.51219216318015,65.9560125449433,
4.22135767615932));
#261441=CARTESIAN_POINT('Ctrl Pts',(-4.6862523681243,65.8697037316857,4.25379868918615));
#261442=CARTESIAN_POINT('Ctrl Pts',(-4.87964094281487,65.8555108601014,
4.28875393216471));
#261443=CARTESIAN_POINT('Ctrl Pts',(-4.48446767193232,65.9579557151991,
4.47154323956553));
#261444=CARTESIAN_POINT('Ctrl Pts',(-4.6626169462531,65.8713953445337,4.46767570477302));
#261445=CARTESIAN_POINT('Ctrl Pts',(-4.86038908992741,65.8569354625126,
4.46350834785649));
#261446=CARTESIAN_POINT('Ctrl Pts',(-4.49975936877847,65.9568960291476,
4.64353769016378));
#261447=CARTESIAN_POINT('Ctrl Pts',(-4.67561628585122,65.8704766362668,
4.61463767040416));
#261448=CARTESIAN_POINT('Ctrl Pts',(-4.87092992967729,65.8561635955122,
4.58349799088226));
#261449=CARTESIAN_POINT('Ctrl Pts',(-4.59372963797714,65.9502572949783,
4.96366679064011));
#261450=CARTESIAN_POINT('Ctrl Pts',(-4.75582205540001,65.8646924066107,
4.88862271283806));
#261451=CARTESIAN_POINT('Ctrl Pts',(-4.9363817116022,65.8512898691079,4.80776315422202));
#261452=CARTESIAN_POINT('Ctrl Pts',(-4.67383602477745,65.9445549388601,
5.11609535395164));
#261453=CARTESIAN_POINT('Ctrl Pts',(-4.82406048883673,65.8597427462409,
5.01890497900004));
#261454=CARTESIAN_POINT('Ctrl Pts',(-4.99189710122369,65.8471371293895,
4.91418421673991));
#261455=CARTESIAN_POINT('Ctrl Pts',(-4.8299491643489,65.9330162944123,5.30924877121673));
#261456=CARTESIAN_POINT('Ctrl Pts',(-4.95757441530503,65.8497260824747,
5.18455891300591));
#261457=CARTESIAN_POINT('Ctrl Pts',(-5.10118680227484,65.8387301893256,
5.05021018314642));
#261458=CARTESIAN_POINT('Ctrl Pts',(-4.88942536164016,65.928563662165,5.36959095245021));
#261459=CARTESIAN_POINT('Ctrl Pts',(-5.00835572047755,65.8458708401228,
5.23621810911562));
#261460=CARTESIAN_POINT('Ctrl Pts',(-5.14264821972077,65.8355096208282,
5.09251447827068));
#261461=CARTESIAN_POINT('Ctrl Pts',(-5.01651316953247,65.9188654923848,
5.47539810873861));
#261462=CARTESIAN_POINT('Ctrl Pts',(-5.11706482667001,65.8374748101095,
5.3269745251348));
#261463=CARTESIAN_POINT('Ctrl Pts',(-5.23165922815084,65.8284961046547,
5.16705626289246));
#261464=CARTESIAN_POINT('Ctrl Pts',(-5.08472188597174,65.91357826105,5.5217149024354));
#261465=CARTESIAN_POINT('Ctrl Pts',(-5.1753714150773,65.832906099351,5.3666841446406));
#261466=CARTESIAN_POINT('Ctrl Pts',(-5.27935318699374,65.8246929385831,
5.19964768151785));
#261467=CARTESIAN_POINT('Ctrl Pts',(-5.41751533989557,65.8872370343221,
5.70319668970765));
#261468=CARTESIAN_POINT('Ctrl Pts',(-5.46050286975101,65.8101487534843,
5.52260955944026));
#261469=CARTESIAN_POINT('Ctrl Pts',(-5.51340877289195,65.8057388144173,
5.32804540784423));
#261470=CARTESIAN_POINT('Ctrl Pts',(-5.72854262822302,65.8611654382057,
5.75192877312679));
#261471=CARTESIAN_POINT('Ctrl Pts',(-5.72623641199483,65.7877711381099,
5.56425071252817));
#261472=CARTESIAN_POINT('Ctrl Pts',(-5.73060092143395,65.7873412035761,
5.36203962651343));
#261473=CARTESIAN_POINT('Ctrl Pts',(-6.01225604074569,65.8349011493704,
5.68677934832659));
#261474=CARTESIAN_POINT('Ctrl Pts',(-5.9714165725876,65.7652479247564,5.50875528664603));
#261475=CARTESIAN_POINT('Ctrl Pts',(-5.93450867162861,65.7687601808892,
5.31696209593943));
#261476=CARTESIAN_POINT('Origin',(-1.11575217567831E-14,1.92862511296078E-13,
2.30953198860262));
#261477=CARTESIAN_POINT('',(-1.92523812794069E-14,-66.0995441972306,2.30953198860216));
#261478=CARTESIAN_POINT('',(5.7609548697913,-65.8480154755621,2.30953198860216));
#261479=CARTESIAN_POINT('Origin',(-1.11575217567831E-14,1.92862511296078E-13,
2.30953198860262));
#261480=CARTESIAN_POINT('',(-1.93280139964607E-14,-66.2265441972306,2.18253198860216));
#261481=CARTESIAN_POINT('Origin',(-1.92679342937561E-14,-66.2265441972306,
2.30953198860216));
#261482=CARTESIAN_POINT('Origin',(-1.12176014594878E-14,1.93749043458829E-13,
2.18253198860262));
#261483=CARTESIAN_POINT('Origin',(-1.11575217567831E-14,1.92862511296078E-13,
2.30953198860262));
#261484=CARTESIAN_POINT('Origin',(-1.11575217567831E-14,1.92862511296078E-13,
2.30953198860262));
#261485=CARTESIAN_POINT('',(-1.93435670108099E-14,-66.3535441972306,2.18253198860216));
#261486=CARTESIAN_POINT('Origin',(-1.12176014594878E-14,1.93749043458829E-13,
2.18253198860262));
#261487=CARTESIAN_POINT('',(-1.92990403224544E-14,-66.4805441972306,2.30953198860216));
#261488=CARTESIAN_POINT('Origin',(-1.92834873081052E-14,-66.3535441972306,
2.30953198860216));
#261489=CARTESIAN_POINT('',(5.79416120777816,-66.2275656555351,2.30953198860216));
#261490=CARTESIAN_POINT('Origin',(-1.11575217567831E-14,1.92862511296078E-13,
2.30953198860262));
#261491=CARTESIAN_POINT('Origin',(-1.11575217567831E-14,1.92862511296078E-13,
2.30953198860262));
#261492=CARTESIAN_POINT('Origin',(10.0229975717235,-114.563386475249,4.445));
#261493=CARTESIAN_POINT('',(-5.76095486979065,65.8480154755627,3.17499999999344));
#261494=CARTESIAN_POINT('Ctrl Pts',(-4.49472415811104,65.9465480356947,
4.445));
#261495=CARTESIAN_POINT('Ctrl Pts',(-4.49472415811104,65.9465480356947,
4.28553175692096));
#261496=CARTESIAN_POINT('Ctrl Pts',(-4.52652892656956,65.9444044626199,
4.11543688631087));
#261497=CARTESIAN_POINT('Ctrl Pts',(-4.65584563900152,65.9354005480955,
3.80253630366508));
#261498=CARTESIAN_POINT('Ctrl Pts',(-4.75335449032797,65.9285073424601,
3.65973026004741));
#261499=CARTESIAN_POINT('Ctrl Pts',(-4.97827514565221,65.9119051150063,
3.43421851625708));
#261500=CARTESIAN_POINT('Ctrl Pts',(-5.12067995098529,65.9010838904671,
3.33647993284444));
#261501=CARTESIAN_POINT('Ctrl Pts',(-5.43259037593922,65.8761047945766,
3.20687056606523));
#261502=CARTESIAN_POINT('Ctrl Pts',(-5.60209345225226,65.8619140486688,
3.175));
#261503=CARTESIAN_POINT('Ctrl Pts',(-5.91981628733042,65.8341169024562,
3.175));
#261504=CARTESIAN_POINT('Ctrl Pts',(-6.08920842820953,65.8186581587365,
3.20687056606523));
#261505=CARTESIAN_POINT('Ctrl Pts',(-6.40071780743065,65.7890950891441,
3.33647993284444));
#261506=CARTESIAN_POINT('Ctrl Pts',(-6.54283824971022,65.7750235800303,
3.43421851625708));
#261507=CARTESIAN_POINT('Ctrl Pts',(-6.76722480142868,65.7523165204273,
3.65973026004741));
#261508=CARTESIAN_POINT('Ctrl Pts',(-6.86444926679916,65.742172768441,3.80253630366508));
#261509=CARTESIAN_POINT('Ctrl Pts',(-6.99336488114522,65.7285842818164,
4.11543688631087));
#261510=CARTESIAN_POINT('Ctrl Pts',(-7.02505869126407,65.7251724491156,
4.28553175692096));
#261511=CARTESIAN_POINT('Ctrl Pts',(-7.02505869126407,65.7251724491156,
4.60446824307904));
#261512=CARTESIAN_POINT('Ctrl Pts',(-6.99336488114522,65.7285842818164,
4.77456311368913));
#261513=CARTESIAN_POINT('Ctrl Pts',(-6.86444926679916,65.742172768441,5.08746369633492));
#261514=CARTESIAN_POINT('Ctrl Pts',(-6.76722480142868,65.7523165204273,
5.23026973995259));
#261515=CARTESIAN_POINT('Ctrl Pts',(-6.54283824971022,65.7750235800303,
5.45578148374292));
#261516=CARTESIAN_POINT('Ctrl Pts',(-6.40071780743066,65.7890950891441,
5.55352006715556));
#261517=CARTESIAN_POINT('Ctrl Pts',(-6.08920842820953,65.8186581587365,
5.68312943393477));
#261518=CARTESIAN_POINT('Ctrl Pts',(-5.91981628733042,65.8341169024562,
5.715));
#261519=CARTESIAN_POINT('Ctrl Pts',(-5.60209345225226,65.8619140486688,
5.715));
#261520=CARTESIAN_POINT('Ctrl Pts',(-5.43259037593922,65.8761047945766,
5.68312943393477));
#261521=CARTESIAN_POINT('Ctrl Pts',(-5.12067995098529,65.9010838904671,
5.55352006715557));
#261522=CARTESIAN_POINT('Ctrl Pts',(-4.97827514565221,65.9119051150063,
5.45578148374292));
#261523=CARTESIAN_POINT('Ctrl Pts',(-4.75335449032797,65.9285073424601,
5.23026973995259));
#261524=CARTESIAN_POINT('Ctrl Pts',(-4.65584563900152,65.9354005480955,
5.08746369633493));
#261525=CARTESIAN_POINT('Ctrl Pts',(-4.52652892656956,65.9444044626199,
4.77456311368913));
#261526=CARTESIAN_POINT('Ctrl Pts',(-4.49472415811104,65.9465480356947,
4.60446824307904));
#261527=CARTESIAN_POINT('Ctrl Pts',(-4.49472415811104,65.9465480356947,
4.445));
#261528=CARTESIAN_POINT('',(-5.7941612077782,66.2275656555355,3.175));
#261529=CARTESIAN_POINT('',(10.0229975717235,-114.563386475249,3.175));
#261530=CARTESIAN_POINT('',(-5.79416120777819,66.2275656555354,5.715));
#261531=CARTESIAN_POINT('Ctrl Pts',(-5.7941612077782,66.2275656555355,3.175));
#261532=CARTESIAN_POINT('Ctrl Pts',(-5.9530225774129,66.2136670866202,3.175));
#261533=CARTESIAN_POINT('Ctrl Pts',(-6.12241501552111,66.1982119784345,
3.20687054727211));
#261534=CARTESIAN_POINT('Ctrl Pts',(-6.43392555716451,66.1686620439684,
3.33647990006866));
#261535=CARTESIAN_POINT('Ctrl Pts',(-6.57604684440547,66.1545998466684,
3.43421849077535));
#261536=CARTESIAN_POINT('Ctrl Pts',(-6.80043497757575,66.1319102785373,
3.65973028551737));
#261537=CARTESIAN_POINT('Ctrl Pts',(-6.89766026532391,66.1217758425954,
3.80253635930903));
#261538=CARTESIAN_POINT('Ctrl Pts',(-7.0265770154737,66.1082004985806,4.11543695516789));
#261539=CARTESIAN_POINT('Ctrl Pts',(-7.05827112497043,66.1047923034812,
4.28553180502499));
#261540=CARTESIAN_POINT('Ctrl Pts',(-7.05827112497043,66.1047923034812,
4.60446819497501));
#261541=CARTESIAN_POINT('Ctrl Pts',(-7.0265770154737,66.1082004985806,4.77456304483211));
#261542=CARTESIAN_POINT('Ctrl Pts',(-6.89766026532391,66.1217758425954,
5.08746364069097));
#261543=CARTESIAN_POINT('Ctrl Pts',(-6.80043497757575,66.1319102785373,
5.23026971448264));
#261544=CARTESIAN_POINT('Ctrl Pts',(-6.57604684440547,66.1545998466684,
5.45578150922466));
#261545=CARTESIAN_POINT('Ctrl Pts',(-6.43392555716451,66.1686620439684,
5.55352009993134));
#261546=CARTESIAN_POINT('Ctrl Pts',(-6.12241501552111,66.1982119784344,
5.68312945272789));
#261547=CARTESIAN_POINT('Ctrl Pts',(-5.9530225774129,66.2136670866202,5.715));
#261548=CARTESIAN_POINT('Ctrl Pts',(-5.7941612077782,66.2275656555355,5.715));
#261549=CARTESIAN_POINT('Ctrl Pts',(-5.7941612077782,66.2275656555355,5.715));
#261550=CARTESIAN_POINT('Ctrl Pts',(-5.6352998381435,66.2414642244507,5.715));
#261551=CARTESIAN_POINT('Ctrl Pts',(-5.46579710042078,66.2556586022737,
5.6831294527279));
#261552=CARTESIAN_POINT('Ctrl Pts',(-5.15388781159512,66.280650835591,5.55352009993135));
#261553=CARTESIAN_POINT('Ctrl Pts',(-5.011483791117,66.2914813772026,5.45578150922466));
#261554=CARTESIAN_POINT('Ctrl Pts',(-4.78656461572897,66.3081011050097,
5.23026971448264));
#261555=CARTESIAN_POINT('Ctrl Pts',(-4.68905657223274,66.3150036279624,
5.08746364069097));
#261556=CARTESIAN_POINT('Ctrl Pts',(-4.55974102344273,66.3240206826611,
4.77456304483211));
#261557=CARTESIAN_POINT('Ctrl Pts',(-4.52793659181739,66.3261678900603,
4.60446819497501));
#261558=CARTESIAN_POINT('Ctrl Pts',(-4.52793659181739,66.3261678900603,
4.445));
#261559=CARTESIAN_POINT('Ctrl Pts',(-4.52793659181739,66.3261678900603,
4.28553180502499));
#261560=CARTESIAN_POINT('Ctrl Pts',(-4.55974102344273,66.3240206826611,
4.11543695516789));
#261561=CARTESIAN_POINT('Ctrl Pts',(-4.68905657223274,66.3150036279624,
3.80253635930903));
#261562=CARTESIAN_POINT('Ctrl Pts',(-4.78656461572897,66.3081011050097,
3.65973028551737));
#261563=CARTESIAN_POINT('Ctrl Pts',(-5.011483791117,66.2914813772026,3.43421849077535));
#261564=CARTESIAN_POINT('Ctrl Pts',(-5.15388781159512,66.280650835591,3.33647990006866));
#261565=CARTESIAN_POINT('Ctrl Pts',(-5.46579710042078,66.2556586022738,
3.20687054727211));
#261566=CARTESIAN_POINT('Ctrl Pts',(-5.6352998381435,66.2414642244507,3.175));
#261567=CARTESIAN_POINT('Ctrl Pts',(-5.7941612077782,66.2275656555355,3.175));
#261568=CARTESIAN_POINT('Origin',(-3.98912952672225E-15,8.70861844988177E-14,
17.4625000000011));
#261569=CARTESIAN_POINT('',(5.76095486979131,-65.8480154755622,17.4625000000006));
#261570=CARTESIAN_POINT('Origin',(-3.98912952672225E-15,8.70861844988177E-14,
17.4625000000011));
#261571=CARTESIAN_POINT('',(5.76095486979131,-65.8480154755622,17.4625000000006));
#261572=CARTESIAN_POINT('Origin',(-3.98912952672225E-15,8.70861844988177E-14,
17.4625000000011));
#261573=CARTESIAN_POINT('',(5.79416120777817,-66.2275656555352,17.4625000000006));
#261574=CARTESIAN_POINT('',(5.79416120777817,-66.2275656555352,17.4625000000006));
#261575=CARTESIAN_POINT('Origin',(-3.98912952672225E-15,8.70861844988177E-14,
17.4625000000011));
#261576=CARTESIAN_POINT('Origin',(-3.98912952672225E-15,8.70861844988177E-14,
17.4625000000011));
#261577=CARTESIAN_POINT('Origin',(-1.12176014594878E-14,1.93749043458829E-13,
2.18253198860262));
#261578=CARTESIAN_POINT('Origin',(5.70044441203719E-15,0.,40.48125));
#261579=CARTESIAN_POINT('',(-56.0881943187058,-6.86882276423578E-15,40.10025));
#261580=CARTESIAN_POINT('Origin',(5.64679317051213E-15,0.,40.10025));
#261581=CARTESIAN_POINT('',(-56.4113006433413,-6.9083918768607E-15,40.2793507603272));
#261582=CARTESIAN_POINT('Origin',(-56.0881943187058,-6.86882276423578E-15,
40.48125));
#261583=CARTESIAN_POINT('Origin',(5.67201358560304E-15,0.,40.2793507603272));
#261584=CARTESIAN_POINT('Origin',(0.,0.,42.1005));
#261585=CARTESIAN_POINT('',(-50.889,-6.23210509618097E-15,42.4815));
#261586=CARTESIAN_POINT('Origin',(0.,0.,42.4815));
#261587=CARTESIAN_POINT('',(-51.27,-6.27876413922848E-15,42.1005));
#261588=CARTESIAN_POINT('Origin',(-50.889,-6.23210509618097E-15,42.1005));
#261589=CARTESIAN_POINT('',(51.27,6.27876413922848E-15,42.1005));
#261590=CARTESIAN_POINT('Origin',(0.,0.,42.1005));
#261591=CARTESIAN_POINT('Origin',(0.,0.,42.1005));
#261592=CARTESIAN_POINT('Origin',(-1.38777878078145E-14,-1.38777878078145E-14,
42.1005));
#261593=CARTESIAN_POINT('',(50.,-7.75455381207769E-15,42.1005));
#261594=CARTESIAN_POINT('',(-50.,-2.00010218035512E-14,42.1005));
#261595=CARTESIAN_POINT('Origin',(-1.38777878078145E-14,-1.38777878078145E-14,
42.1005));
#261596=CARTESIAN_POINT('Origin',(-1.38777878078145E-14,-1.38777878078145E-14,
42.1005));
#261597=CARTESIAN_POINT('',(-50.381,-2.00476808465987E-14,42.4815));
#261598=CARTESIAN_POINT('Origin',(-50.381,-2.00476808465987E-14,42.1005));
#261599=CARTESIAN_POINT('Origin',(-1.38777878078145E-14,-1.38777878078145E-14,
42.4815));
#261600=CARTESIAN_POINT('Origin',(5.67808972806842E-15,0.,40.3225));
#261601=CARTESIAN_POINT('',(-56.5223703788014,-6.92199399646203E-15,40.4570994931153));
#261602=CARTESIAN_POINT('Origin',(5.69704361235785E-15,0.,40.4570994931153));
#261603=CARTESIAN_POINT('',(-56.7377745952251,-6.94837340487864E-15,40.5765));
#261604=CARTESIAN_POINT('Origin',(-56.7377745952251,-6.94837340487864E-15,
40.3225));
#261605=CARTESIAN_POINT('Origin',(5.71385722241845E-15,0.,40.5765));
#261606=CARTESIAN_POINT('Origin',(5.67808972806842E-15,0.,40.3225));
#261607=CARTESIAN_POINT('',(-57.4087519663171,-7.03054443385946E-15,40.5765));
#261608=CARTESIAN_POINT('Origin',(5.71385722241845E-15,0.,40.5765));
#261609=CARTESIAN_POINT('',(-57.6241561827409,-7.05692384227608E-15,40.1879005068848));
#261610=CARTESIAN_POINT('Origin',(-57.4087519663171,-7.03054443385946E-15,
40.3225));
#261611=CARTESIAN_POINT('Origin',(5.65913584377898E-15,0.,40.1879005068848));
#261612=CARTESIAN_POINT('Origin',(6.93889390390723E-15,0.,49.276));
#261613=CARTESIAN_POINT('',(-56.875,-6.96517867015057E-15,38.989));
#261614=CARTESIAN_POINT('Origin',(5.49031038273072E-15,0.,38.989));
#261615=CARTESIAN_POINT('',(-56.875,-6.96517867015057E-15,38.6715));
#261616=CARTESIAN_POINT('',(-56.875,-6.96517867015057E-15,49.276));
#261617=CARTESIAN_POINT('Origin',(5.44560101479317E-15,0.,38.6715));
#261618=CARTESIAN_POINT('Origin',(5.64679317051213E-15,0.,40.10025));
#261619=CARTESIAN_POINT('',(-56.2993860673093,-6.89468629412914E-15,40.10025));
#261620=CARTESIAN_POINT('Origin',(5.71385722241845E-15,0.,40.5765));
#261621=CARTESIAN_POINT('',(-57.8669800961561,-7.08666119510811E-15,40.5765));
#261622=CARTESIAN_POINT('Origin',(0.,0.,42.4815));
#261623=CARTESIAN_POINT('',(51.27,-6.27876413922848E-15,40.10025));
#261624=CARTESIAN_POINT('Origin',(5.64679317051213E-15,0.,40.10025));
#261625=CARTESIAN_POINT('',(51.27,-6.27876413922848E-15,42.4815));
#261626=CARTESIAN_POINT('Origin',(-1.38777878078145E-14,-1.38777878078145E-14,
225.059263108502));
#261627=CARTESIAN_POINT('',(50.,-2.00010218035512E-14,17.4625));
#261628=CARTESIAN_POINT('',(50.,-2.00010218035512E-14,225.059263108502));
#261629=CARTESIAN_POINT('Origin',(-1.38777878078145E-14,-1.38777878078145E-14,
17.4625));
#261630=CARTESIAN_POINT('Origin',(-1.38777878078145E-14,-1.38777878078145E-14,
225.059263108502));
#261631=CARTESIAN_POINT('',(65.,-2.18379920022723E-14,17.4625));
#261632=CARTESIAN_POINT('Origin',(-1.38777878078145E-14,-1.38777878078145E-14,
17.4625));
#261633=CARTESIAN_POINT('',(65.,-2.18379920022723E-14,38.6715));
#261634=CARTESIAN_POINT('',(65.,-2.18379920022723E-14,225.059263108502));
#261635=CARTESIAN_POINT('Origin',(-1.38777878078145E-14,-1.38777878078145E-14,
38.6715));
#261636=CARTESIAN_POINT('Origin',(-1.38777878078145E-14,-1.38777878078145E-14,
38.6715));
#261637=CARTESIAN_POINT('Origin',(-1.38777878078145E-14,-1.38777878078145E-14,
17.4625));
#261638=CARTESIAN_POINT('Origin',(0.,0.,42.4815));
#261639=CARTESIAN_POINT('Origin',(57.8669800961561,0.,40.5765));
#261640=CARTESIAN_POINT('Origin',(56.2993860673093,0.,40.10025));
#261641=CARTESIAN_POINT('Origin',(40.4567708333334,-1.14908083048704E-13,
48.26));
#261642=CARTESIAN_POINT('',(48.3916666666642,-4.72273670613199,48.26));
#261643=CARTESIAN_POINT('',(48.3968749999976,-4.72273670613199,48.26));
#261644=CARTESIAN_POINT('',(40.4567708333334,-4.72273670613191,48.26));
#261645=CARTESIAN_POINT('',(49.2650632938682,-2.14259623628835,52.4687436799701));
#261646=CARTESIAN_POINT('Ctrl Pts',(48.3916666666642,-4.72273670613199,
48.26));
#261647=CARTESIAN_POINT('Ctrl Pts',(48.4578124999975,-4.722736706132,46.303778404803));
#261648=CARTESIAN_POINT('Ctrl Pts',(48.5239583333308,-3.3394791506646,44.9205208493356));
#261649=CARTESIAN_POINT('Ctrl Pts',(48.5901041666641,-1.95622159519721,
43.5372632938682));
#261650=CARTESIAN_POINT('Ctrl Pts',(48.6562499999974,-1.70749941551634E-13,
43.5372632938682));
#261651=CARTESIAN_POINT('Ctrl Pts',(48.7223958333307,1.95622159519687,43.5372632938682));
#261652=CARTESIAN_POINT('Ctrl Pts',(48.7885416666641,3.33947915066426,44.9205208493356));
#261653=CARTESIAN_POINT('Ctrl Pts',(48.8546874999974,4.72273670613166,46.303778404803));
#261654=CARTESIAN_POINT('Ctrl Pts',(48.9208333333307,4.72273670613165,48.26));
#261655=CARTESIAN_POINT('Ctrl Pts',(48.986979166664,4.72273670613166,50.216221595197));
#261656=CARTESIAN_POINT('Ctrl Pts',(49.0531249999973,3.33947915066426,51.5994791506644));
#261657=CARTESIAN_POINT('Ctrl Pts',(49.1192708333306,1.95622159519687,52.9827367061318));
#261658=CARTESIAN_POINT('Ctrl Pts',(49.1854166666639,-1.71440780215362E-13,
52.9827367061318));
#261659=CARTESIAN_POINT('Ctrl Pts',(49.2237251595434,-1.13294968517034,
52.9827367061318));
#261660=CARTESIAN_POINT('Ctrl Pts',(49.2650632938682,-2.14259623628835,
52.4687436799701));
#261661=CARTESIAN_POINT('',(49.2650632938682,-2.01456111142428,52.5315085770466));
#261662=CARTESIAN_POINT('Origin',(49.2650632939072,4.32918355108836E-6,
48.2599912028394));
#261663=CARTESIAN_POINT('Ctrl Pts',(48.3968749999976,-4.72273670613199,
48.26));
#261664=CARTESIAN_POINT('Ctrl Pts',(48.4630208333309,-4.722736706132,46.303778404803));
#261665=CARTESIAN_POINT('Ctrl Pts',(48.5291666666642,-3.3394791506646,44.9205208493356));
#261666=CARTESIAN_POINT('Ctrl Pts',(48.5953124999975,-1.95622159519721,
43.5372632938682));
#261667=CARTESIAN_POINT('Ctrl Pts',(48.6614583333308,-1.70768126350274E-13,
43.5372632938682));
#261668=CARTESIAN_POINT('Ctrl Pts',(48.7276041666641,1.95622159519687,43.5372632938682));
#261669=CARTESIAN_POINT('Ctrl Pts',(48.7937499999974,3.33947915066426,44.9205208493356));
#261670=CARTESIAN_POINT('Ctrl Pts',(48.8598958333308,4.72273670613166,46.303778404803));
#261671=CARTESIAN_POINT('Ctrl Pts',(48.9260416666641,4.72273670613165,48.26));
#261672=CARTESIAN_POINT('Ctrl Pts',(48.9921874999974,4.72273670613166,50.216221595197));
#261673=CARTESIAN_POINT('Ctrl Pts',(49.0583333333307,3.33947915066426,51.5994791506644));
#261674=CARTESIAN_POINT('Ctrl Pts',(49.124479166664,1.95622159519687,52.9827367061318));
#261675=CARTESIAN_POINT('Ctrl Pts',(49.1906249999973,-1.71458965014002E-13,
52.9827367061318));
#261676=CARTESIAN_POINT('Ctrl Pts',(49.2263929373901,-1.05781434774344,
52.9827367061318));
#261677=CARTESIAN_POINT('Ctrl Pts',(49.2650632938682,-2.01456111142428,
52.5315085770466));
#261678=CARTESIAN_POINT('Origin',(40.4567708333334,-1.14908083048704E-13,
48.26));
#261679=CARTESIAN_POINT('',(47.3333333333312,-4.72273670613199,48.26));
#261680=CARTESIAN_POINT('',(47.3385416666645,-4.72273670613199,48.26));
#261681=CARTESIAN_POINT('',(40.4567708333334,-4.72273670613191,48.26));
#261682=CARTESIAN_POINT('Ctrl Pts',(47.3333333333312,-4.72273670613199,
48.26));
#261683=CARTESIAN_POINT('Ctrl Pts',(47.3994791666645,-4.72273670613199,
46.303778404803));
#261684=CARTESIAN_POINT('Ctrl Pts',(47.4656249999978,-3.3394791506646,44.9205208493356));
#261685=CARTESIAN_POINT('Ctrl Pts',(47.5317708333311,-1.95622159519721,
43.5372632938682));
#261686=CARTESIAN_POINT('Ctrl Pts',(47.5979166666644,-1.67054790468026E-13,
43.5372632938682));
#261687=CARTESIAN_POINT('Ctrl Pts',(47.6640624999977,1.95622159519688,43.5372632938682));
#261688=CARTESIAN_POINT('Ctrl Pts',(47.7302083333311,3.33947915066426,44.9205208493356));
#261689=CARTESIAN_POINT('Ctrl Pts',(47.7963541666644,4.72273670613166,46.303778404803));
#261690=CARTESIAN_POINT('Ctrl Pts',(47.8624999999977,4.72273670613166,48.26));
#261691=CARTESIAN_POINT('Ctrl Pts',(47.928645833331,4.72273670613166,50.216221595197));
#261692=CARTESIAN_POINT('Ctrl Pts',(47.9947916666643,3.33947915066427,51.5994791506644));
#261693=CARTESIAN_POINT('Ctrl Pts',(48.0609374999976,1.95622159519687,52.9827367061318));
#261694=CARTESIAN_POINT('Ctrl Pts',(48.1270833333309,-1.67745629131754E-13,
52.9827367061318));
#261695=CARTESIAN_POINT('Ctrl Pts',(48.1932291666642,-1.95622159519721,
52.9827367061318));
#261696=CARTESIAN_POINT('Ctrl Pts',(48.2593749999975,-3.3394791506646,51.5994791506644));
#261697=CARTESIAN_POINT('Ctrl Pts',(48.3255208333308,-4.722736706132,50.216221595197));
#261698=CARTESIAN_POINT('Ctrl Pts',(48.3916666666642,-4.72273670613199,
48.26));
#261699=CARTESIAN_POINT('Ctrl Pts',(47.3385416666645,-4.72273670613199,
48.26));
#261700=CARTESIAN_POINT('Ctrl Pts',(47.4046874999979,-4.72273670613199,
46.303778404803));
#261701=CARTESIAN_POINT('Ctrl Pts',(47.4708333333312,-3.3394791506646,44.9205208493356));
#261702=CARTESIAN_POINT('Ctrl Pts',(47.5369791666645,-1.95622159519721,
43.5372632938682));
#261703=CARTESIAN_POINT('Ctrl Pts',(47.6031249999978,-1.67072975266666E-13,
43.5372632938682));
#261704=CARTESIAN_POINT('Ctrl Pts',(47.6692708333311,1.95622159519688,43.5372632938682));
#261705=CARTESIAN_POINT('Ctrl Pts',(47.7354166666644,3.33947915066426,44.9205208493356));
#261706=CARTESIAN_POINT('Ctrl Pts',(47.8015624999978,4.72273670613166,46.303778404803));
#261707=CARTESIAN_POINT('Ctrl Pts',(47.8677083333311,4.72273670613166,48.26));
#261708=CARTESIAN_POINT('Ctrl Pts',(47.9338541666644,4.72273670613166,50.216221595197));
#261709=CARTESIAN_POINT('Ctrl Pts',(47.9999999999977,3.33947915066427,51.5994791506644));
#261710=CARTESIAN_POINT('Ctrl Pts',(48.066145833331,1.95622159519687,52.9827367061318));
#261711=CARTESIAN_POINT('Ctrl Pts',(48.1322916666643,-1.67763813930394E-13,
52.9827367061318));
#261712=CARTESIAN_POINT('Ctrl Pts',(48.1984374999976,-1.95622159519721,
52.9827367061318));
#261713=CARTESIAN_POINT('Ctrl Pts',(48.2645833333309,-3.3394791506646,51.5994791506644));
#261714=CARTESIAN_POINT('Ctrl Pts',(48.3307291666642,-4.722736706132,50.216221595197));
#261715=CARTESIAN_POINT('Ctrl Pts',(48.3968749999976,-4.72273670613199,
48.26));
#261716=CARTESIAN_POINT('Origin',(40.4567708333334,-1.14908083048704E-13,
48.26));
#261717=CARTESIAN_POINT('',(46.2749999999982,-4.72273670613199,48.26));
#261718=CARTESIAN_POINT('',(46.2802083333315,-4.72273670613199,48.26));
#261719=CARTESIAN_POINT('',(40.4567708333334,-4.72273670613191,48.26));
#261720=CARTESIAN_POINT('Ctrl Pts',(46.2749999999982,-4.72273670613199,
48.26));
#261721=CARTESIAN_POINT('Ctrl Pts',(46.3411458333315,-4.72273670613199,
46.303778404803));
#261722=CARTESIAN_POINT('Ctrl Pts',(46.4072916666648,-3.3394791506646,44.9205208493356));
#261723=CARTESIAN_POINT('Ctrl Pts',(46.4734374999981,-1.95622159519721,
43.5372632938682));
#261724=CARTESIAN_POINT('Ctrl Pts',(46.5395833333314,-1.63359639384419E-13,
43.5372632938682));
#261725=CARTESIAN_POINT('Ctrl Pts',(46.6057291666648,1.95622159519688,43.5372632938682));
#261726=CARTESIAN_POINT('Ctrl Pts',(46.6718749999981,3.33947915066427,44.9205208493356));
#261727=CARTESIAN_POINT('Ctrl Pts',(46.7380208333314,4.72273670613166,46.303778404803));
#261728=CARTESIAN_POINT('Ctrl Pts',(46.8041666666647,4.72273670613166,48.26));
#261729=CARTESIAN_POINT('Ctrl Pts',(46.870312499998,4.72273670613166,50.216221595197));
#261730=CARTESIAN_POINT('Ctrl Pts',(46.9364583333313,3.33947915066427,51.5994791506644));
#261731=CARTESIAN_POINT('Ctrl Pts',(47.0026041666646,1.95622159519688,52.9827367061318));
#261732=CARTESIAN_POINT('Ctrl Pts',(47.0687499999979,-1.64050478048146E-13,
52.9827367061318));
#261733=CARTESIAN_POINT('Ctrl Pts',(47.1348958333312,-1.95622159519721,
52.9827367061318));
#261734=CARTESIAN_POINT('Ctrl Pts',(47.2010416666646,-3.3394791506646,51.5994791506644));
#261735=CARTESIAN_POINT('Ctrl Pts',(47.2671874999979,-4.72273670613199,
50.216221595197));
#261736=CARTESIAN_POINT('Ctrl Pts',(47.3333333333312,-4.72273670613199,
48.26));
#261737=CARTESIAN_POINT('Ctrl Pts',(46.2802083333315,-4.72273670613199,
48.26));
#261738=CARTESIAN_POINT('Ctrl Pts',(46.3463541666649,-4.72273670613199,
46.303778404803));
#261739=CARTESIAN_POINT('Ctrl Pts',(46.4124999999982,-3.3394791506646,44.9205208493356));
#261740=CARTESIAN_POINT('Ctrl Pts',(46.4786458333315,-1.95622159519721,
43.5372632938682));
#261741=CARTESIAN_POINT('Ctrl Pts',(46.5447916666648,-1.63377824183059E-13,
43.5372632938682));
#261742=CARTESIAN_POINT('Ctrl Pts',(46.6109374999981,1.95622159519688,43.5372632938682));
#261743=CARTESIAN_POINT('Ctrl Pts',(46.6770833333314,3.33947915066427,44.9205208493356));
#261744=CARTESIAN_POINT('Ctrl Pts',(46.7432291666648,4.72273670613166,46.303778404803));
#261745=CARTESIAN_POINT('Ctrl Pts',(46.8093749999981,4.72273670613166,48.26));
#261746=CARTESIAN_POINT('Ctrl Pts',(46.8755208333314,4.72273670613166,50.216221595197));
#261747=CARTESIAN_POINT('Ctrl Pts',(46.9416666666647,3.33947915066427,51.5994791506644));
#261748=CARTESIAN_POINT('Ctrl Pts',(47.007812499998,1.95622159519688,52.9827367061318));
#261749=CARTESIAN_POINT('Ctrl Pts',(47.0739583333313,-1.64068662846786E-13,
52.9827367061318));
#261750=CARTESIAN_POINT('Ctrl Pts',(47.1401041666646,-1.95622159519721,
52.9827367061318));
#261751=CARTESIAN_POINT('Ctrl Pts',(47.2062499999979,-3.3394791506646,51.5994791506644));
#261752=CARTESIAN_POINT('Ctrl Pts',(47.2723958333312,-4.72273670613199,
50.216221595197));
#261753=CARTESIAN_POINT('Ctrl Pts',(47.3385416666645,-4.72273670613199,
48.26));
#261754=CARTESIAN_POINT('Origin',(40.4567708333334,-1.14908083048704E-13,
48.26));
#261755=CARTESIAN_POINT('',(45.2166666666652,-4.72273670613198,48.26));
#261756=CARTESIAN_POINT('',(45.2218749999985,-4.72273670613198,48.26));
#261757=CARTESIAN_POINT('',(40.4567708333334,-4.72273670613191,48.26));
#261758=CARTESIAN_POINT('Ctrl Pts',(45.2166666666652,-4.72273670613198,
48.26));
#261759=CARTESIAN_POINT('Ctrl Pts',(45.2828124999985,-4.72273670613199,
46.303778404803));
#261760=CARTESIAN_POINT('Ctrl Pts',(45.3489583333318,-3.33947915066459,
44.9205208493356));
#261761=CARTESIAN_POINT('Ctrl Pts',(45.4151041666651,-1.9562215951972,43.5372632938682));
#261762=CARTESIAN_POINT('Ctrl Pts',(45.4812499999984,-1.59664488300811E-13,
43.5372632938682));
#261763=CARTESIAN_POINT('Ctrl Pts',(45.5473958333317,1.95622159519688,43.5372632938682));
#261764=CARTESIAN_POINT('Ctrl Pts',(45.6135416666651,3.33947915066427,44.9205208493356));
#261765=CARTESIAN_POINT('Ctrl Pts',(45.6796874999984,4.72273670613167,46.303778404803));
#261766=CARTESIAN_POINT('Ctrl Pts',(45.7458333333317,4.72273670613167,48.26));
#261767=CARTESIAN_POINT('Ctrl Pts',(45.811979166665,4.72273670613167,50.216221595197));
#261768=CARTESIAN_POINT('Ctrl Pts',(45.8781249999983,3.33947915066427,51.5994791506644));
#261769=CARTESIAN_POINT('Ctrl Pts',(45.9442708333316,1.95622159519688,52.9827367061318));
#261770=CARTESIAN_POINT('Ctrl Pts',(46.0104166666649,-1.60355326964539E-13,
52.9827367061318));
#261771=CARTESIAN_POINT('Ctrl Pts',(46.0765624999982,-1.9562215951972,52.9827367061318));
#261772=CARTESIAN_POINT('Ctrl Pts',(46.1427083333315,-3.33947915066459,
51.5994791506644));
#261773=CARTESIAN_POINT('Ctrl Pts',(46.2088541666648,-4.72273670613199,
50.216221595197));
#261774=CARTESIAN_POINT('Ctrl Pts',(46.2749999999982,-4.72273670613199,
48.26));
#261775=CARTESIAN_POINT('Ctrl Pts',(45.2218749999985,-4.72273670613198,
48.26));
#261776=CARTESIAN_POINT('Ctrl Pts',(45.2880208333319,-4.72273670613199,
46.303778404803));
#261777=CARTESIAN_POINT('Ctrl Pts',(45.3541666666652,-3.33947915066459,
44.9205208493356));
#261778=CARTESIAN_POINT('Ctrl Pts',(45.4203124999985,-1.9562215951972,43.5372632938682));
#261779=CARTESIAN_POINT('Ctrl Pts',(45.4864583333318,-1.59682673099451E-13,
43.5372632938682));
#261780=CARTESIAN_POINT('Ctrl Pts',(45.5526041666651,1.95622159519688,43.5372632938682));
#261781=CARTESIAN_POINT('Ctrl Pts',(45.6187499999984,3.33947915066427,44.9205208493356));
#261782=CARTESIAN_POINT('Ctrl Pts',(45.6848958333318,4.72273670613167,46.303778404803));
#261783=CARTESIAN_POINT('Ctrl Pts',(45.7510416666651,4.72273670613167,48.26));
#261784=CARTESIAN_POINT('Ctrl Pts',(45.8171874999984,4.72273670613167,50.216221595197));
#261785=CARTESIAN_POINT('Ctrl Pts',(45.8833333333317,3.33947915066427,51.5994791506644));
#261786=CARTESIAN_POINT('Ctrl Pts',(45.949479166665,1.95622159519688,52.9827367061318));
#261787=CARTESIAN_POINT('Ctrl Pts',(46.0156249999983,-1.60373511763179E-13,
52.9827367061318));
#261788=CARTESIAN_POINT('Ctrl Pts',(46.0817708333316,-1.9562215951972,52.9827367061318));
#261789=CARTESIAN_POINT('Ctrl Pts',(46.1479166666649,-3.33947915066459,
51.5994791506644));
#261790=CARTESIAN_POINT('Ctrl Pts',(46.2140624999982,-4.72273670613199,
50.216221595197));
#261791=CARTESIAN_POINT('Ctrl Pts',(46.2802083333315,-4.72273670613199,
48.26));
#261792=CARTESIAN_POINT('Origin',(40.4567708333334,-1.14908083048704E-13,
48.26));
#261793=CARTESIAN_POINT('',(44.1583333333322,-4.72273670613198,48.26));
#261794=CARTESIAN_POINT('',(44.1635416666655,-4.72273670613198,48.26));
#261795=CARTESIAN_POINT('',(40.4567708333334,-4.72273670613191,48.26));
#261796=CARTESIAN_POINT('Ctrl Pts',(44.1583333333322,-4.72273670613198,
48.26));
#261797=CARTESIAN_POINT('Ctrl Pts',(44.2244791666655,-4.72273670613198,
46.303778404803));
#261798=CARTESIAN_POINT('Ctrl Pts',(44.2906249999988,-3.33947915066459,
44.9205208493356));
#261799=CARTESIAN_POINT('Ctrl Pts',(44.3567708333321,-1.9562215951972,43.5372632938682));
#261800=CARTESIAN_POINT('Ctrl Pts',(44.4229166666654,-1.55969337217203E-13,
43.5372632938682));
#261801=CARTESIAN_POINT('Ctrl Pts',(44.4890624999988,1.95622159519689,43.5372632938682));
#261802=CARTESIAN_POINT('Ctrl Pts',(44.5552083333321,3.33947915066428,44.9205208493356));
#261803=CARTESIAN_POINT('Ctrl Pts',(44.6213541666654,4.72273670613167,46.303778404803));
#261804=CARTESIAN_POINT('Ctrl Pts',(44.6874999999987,4.72273670613167,48.26));
#261805=CARTESIAN_POINT('Ctrl Pts',(44.753645833332,4.72273670613167,50.216221595197));
#261806=CARTESIAN_POINT('Ctrl Pts',(44.8197916666653,3.33947915066428,51.5994791506644));
#261807=CARTESIAN_POINT('Ctrl Pts',(44.8859374999986,1.95622159519688,52.9827367061318));
#261808=CARTESIAN_POINT('Ctrl Pts',(44.9520833333319,-1.56660175880931E-13,
52.9827367061318));
#261809=CARTESIAN_POINT('Ctrl Pts',(45.0182291666652,-1.9562215951972,52.9827367061318));
#261810=CARTESIAN_POINT('Ctrl Pts',(45.0843749999985,-3.33947915066459,
51.5994791506644));
#261811=CARTESIAN_POINT('Ctrl Pts',(45.1505208333318,-4.72273670613198,
50.216221595197));
#261812=CARTESIAN_POINT('Ctrl Pts',(45.2166666666652,-4.72273670613198,
48.26));
#261813=CARTESIAN_POINT('Ctrl Pts',(44.1635416666655,-4.72273670613198,
48.26));
#261814=CARTESIAN_POINT('Ctrl Pts',(44.2296874999989,-4.72273670613198,
46.303778404803));
#261815=CARTESIAN_POINT('Ctrl Pts',(44.2958333333322,-3.33947915066459,
44.9205208493356));
#261816=CARTESIAN_POINT('Ctrl Pts',(44.3619791666655,-1.9562215951972,43.5372632938682));
#261817=CARTESIAN_POINT('Ctrl Pts',(44.4281249999988,-1.55987522015843E-13,
43.5372632938682));
#261818=CARTESIAN_POINT('Ctrl Pts',(44.4942708333321,1.95622159519689,43.5372632938682));
#261819=CARTESIAN_POINT('Ctrl Pts',(44.5604166666654,3.33947915066428,44.9205208493356));
#261820=CARTESIAN_POINT('Ctrl Pts',(44.6265624999988,4.72273670613167,46.303778404803));
#261821=CARTESIAN_POINT('Ctrl Pts',(44.6927083333321,4.72273670613167,48.26));
#261822=CARTESIAN_POINT('Ctrl Pts',(44.7588541666654,4.72273670613167,50.216221595197));
#261823=CARTESIAN_POINT('Ctrl Pts',(44.8249999999987,3.33947915066428,51.5994791506644));
#261824=CARTESIAN_POINT('Ctrl Pts',(44.891145833332,1.95622159519688,52.9827367061318));
#261825=CARTESIAN_POINT('Ctrl Pts',(44.9572916666653,-1.56678360679571E-13,
52.9827367061318));
#261826=CARTESIAN_POINT('Ctrl Pts',(45.0234374999986,-1.9562215951972,52.9827367061318));
#261827=CARTESIAN_POINT('Ctrl Pts',(45.0895833333319,-3.33947915066459,
51.5994791506644));
#261828=CARTESIAN_POINT('Ctrl Pts',(45.1557291666652,-4.72273670613198,
50.216221595197));
#261829=CARTESIAN_POINT('Ctrl Pts',(45.2218749999985,-4.72273670613198,
48.26));
#261830=CARTESIAN_POINT('Origin',(40.4567708333334,-1.14908083048704E-13,
48.26));
#261831=CARTESIAN_POINT('',(43.0999999999992,-4.72273670613198,48.26));
#261832=CARTESIAN_POINT('',(43.1052083333325,-4.72273670613198,48.26));
#261833=CARTESIAN_POINT('',(40.4567708333334,-4.72273670613191,48.26));
#261834=CARTESIAN_POINT('Ctrl Pts',(43.0999999999992,-4.72273670613198,
48.26));
#261835=CARTESIAN_POINT('Ctrl Pts',(43.1661458333325,-4.72273670613198,
46.303778404803));
#261836=CARTESIAN_POINT('Ctrl Pts',(43.2322916666658,-3.33947915066458,
44.9205208493356));
#261837=CARTESIAN_POINT('Ctrl Pts',(43.2984374999991,-1.95622159519719,
43.5372632938682));
#261838=CARTESIAN_POINT('Ctrl Pts',(43.3645833333324,-1.52274186133595E-13,
43.5372632938682));
#261839=CARTESIAN_POINT('Ctrl Pts',(43.4307291666657,1.95622159519689,43.5372632938682));
#261840=CARTESIAN_POINT('Ctrl Pts',(43.4968749999991,3.33947915066428,44.9205208493356));
#261841=CARTESIAN_POINT('Ctrl Pts',(43.5630208333324,4.72273670613167,46.303778404803));
#261842=CARTESIAN_POINT('Ctrl Pts',(43.6291666666657,4.72273670613167,48.26));
#261843=CARTESIAN_POINT('Ctrl Pts',(43.695312499999,4.72273670613167,50.216221595197));
#261844=CARTESIAN_POINT('Ctrl Pts',(43.7614583333323,3.33947915066428,51.5994791506644));
#261845=CARTESIAN_POINT('Ctrl Pts',(43.8276041666656,1.95622159519689,52.9827367061318));
#261846=CARTESIAN_POINT('Ctrl Pts',(43.8937499999989,-1.52965024797323E-13,
52.9827367061318));
#261847=CARTESIAN_POINT('Ctrl Pts',(43.9598958333322,-1.95622159519719,
52.9827367061318));
#261848=CARTESIAN_POINT('Ctrl Pts',(44.0260416666655,-3.33947915066459,
51.5994791506644));
#261849=CARTESIAN_POINT('Ctrl Pts',(44.0921874999988,-4.72273670613198,
50.216221595197));
#261850=CARTESIAN_POINT('Ctrl Pts',(44.1583333333322,-4.72273670613198,
48.26));
#261851=CARTESIAN_POINT('Ctrl Pts',(43.1052083333325,-4.72273670613198,
48.26));
#261852=CARTESIAN_POINT('Ctrl Pts',(43.1713541666659,-4.72273670613198,
46.303778404803));
#261853=CARTESIAN_POINT('Ctrl Pts',(43.2374999999992,-3.33947915066458,
44.9205208493356));
#261854=CARTESIAN_POINT('Ctrl Pts',(43.3036458333325,-1.95622159519719,
43.5372632938682));
#261855=CARTESIAN_POINT('Ctrl Pts',(43.3697916666658,-1.52292370932235E-13,
43.5372632938682));
#261856=CARTESIAN_POINT('Ctrl Pts',(43.4359374999991,1.95622159519689,43.5372632938682));
#261857=CARTESIAN_POINT('Ctrl Pts',(43.5020833333324,3.33947915066428,44.9205208493356));
#261858=CARTESIAN_POINT('Ctrl Pts',(43.5682291666658,4.72273670613167,46.303778404803));
#261859=CARTESIAN_POINT('Ctrl Pts',(43.6343749999991,4.72273670613167,48.26));
#261860=CARTESIAN_POINT('Ctrl Pts',(43.7005208333324,4.72273670613167,50.216221595197));
#261861=CARTESIAN_POINT('Ctrl Pts',(43.7666666666657,3.33947915066428,51.5994791506644));
#261862=CARTESIAN_POINT('Ctrl Pts',(43.832812499999,1.95622159519689,52.9827367061318));
#261863=CARTESIAN_POINT('Ctrl Pts',(43.8989583333323,-1.52983209595963E-13,
52.9827367061318));
#261864=CARTESIAN_POINT('Ctrl Pts',(43.9651041666656,-1.95622159519719,
52.9827367061318));
#261865=CARTESIAN_POINT('Ctrl Pts',(44.0312499999989,-3.33947915066459,
51.5994791506644));
#261866=CARTESIAN_POINT('Ctrl Pts',(44.0973958333322,-4.72273670613198,
50.216221595197));
#261867=CARTESIAN_POINT('Ctrl Pts',(44.1635416666655,-4.72273670613198,
48.26));
#261868=CARTESIAN_POINT('Origin',(40.475,-1.41317707189676E-13,48.26));
#261869=CARTESIAN_POINT('',(42.2906249999995,-1.4205919993051E-13,43.5102));
#261870=CARTESIAN_POINT('',(42.09425,-1.46389605610939E-13,43.5102));
#261871=CARTESIAN_POINT('',(40.475,-1.40736024453017E-13,43.5102));
#261872=CARTESIAN_POINT('',(42.09425,-4.36624125519658,46.3900969700488));
#261873=CARTESIAN_POINT('Ctrl Pts',(42.2906249999995,-1.39957490041809E-13,
43.5102));
#261874=CARTESIAN_POINT('Ctrl Pts',(42.2803266558546,-0.306312377614008,
43.5102));
#261875=CARTESIAN_POINT('Ctrl Pts',(42.2696165070132,-0.612600594710988,
43.5398292002881));
#261876=CARTESIAN_POINT('Ctrl Pts',(42.2364131029764,-1.52596251485008,
43.7190485024123));
#261877=CARTESIAN_POINT('Ctrl Pts',(42.2135208891992,-2.1078242421188,43.9581541159291));
#261878=CARTESIAN_POINT('Ctrl Pts',(42.1749789086954,-3.00697611076851,
44.5550320160166));
#261879=CARTESIAN_POINT('Ctrl Pts',(42.15983788401,-3.34869201888137,44.8607436451311));
#261880=CARTESIAN_POINT('Ctrl Pts',(42.1278937490674,-3.93944645506941,
45.5661866234652));
#261881=CARTESIAN_POINT('Ctrl Pts',(42.1111319270672,-4.18359566378184,
45.9636177871492));
#261882=CARTESIAN_POINT('Ctrl Pts',(42.09425,-4.36624125519674,46.3900969700492));
#261883=CARTESIAN_POINT('Origin',(42.09425,-1.46971288347598E-13,48.26));
#261884=CARTESIAN_POINT('Origin',(40.475,-1.41317707189676E-13,48.26));
#261885=CARTESIAN_POINT('',(43.3489583333325,-1.209737311199E-13,43.5102));
#261886=CARTESIAN_POINT('',(42.3270833333327,-1.51906687130258E-13,43.5102));
#261887=CARTESIAN_POINT('',(40.475,-1.40736024453017E-13,43.5102));
#261888=CARTESIAN_POINT('Ctrl Pts',(43.3489583333325,-8.75688410673092E-14,
43.5102));
#261889=CARTESIAN_POINT('Ctrl Pts',(43.3350462619249,-0.413798530173326,
43.5102));
#261890=CARTESIAN_POINT('Ctrl Pts',(43.3204123302741,-0.826670368689188,
43.5642725719142));
#261891=CARTESIAN_POINT('Ctrl Pts',(43.2830916071324,-1.82594941130075,
43.8317260420044));
#261892=CARTESIAN_POINT('Ctrl Pts',(43.2603987577855,-2.38686058154388,
44.107094813422));
#261893=CARTESIAN_POINT('Ctrl Pts',(43.2169625534066,-3.3688243669304,44.8554914890222));
#261894=CARTESIAN_POINT('Ctrl Pts',(43.1966949382382,-3.78128185410704,
45.3203462387159));
#261895=CARTESIAN_POINT('Ctrl Pts',(43.1521835512767,-4.40771574233591,
46.3848087314946));
#261896=CARTESIAN_POINT('Ctrl Pts',(43.1294619675453,-4.61444584304949,
46.9750056411961));
#261897=CARTESIAN_POINT('Ctrl Pts',(43.0859479536865,-4.78902391945533,
48.1969672260124));
#261898=CARTESIAN_POINT('Ctrl Pts',(43.0657543266859,-4.75696102960577,
48.8168166627173));
#261899=CARTESIAN_POINT('Ctrl Pts',(43.0213051463692,-4.45711948033103,
50.0147078667041));
#261900=CARTESIAN_POINT('Ctrl Pts',(42.9985556170619,-4.19029907601681,
50.5808457666315));
#261901=CARTESIAN_POINT('Ctrl Pts',(42.9549633791372,-3.45765603924943,
51.57397596087));
#261902=CARTESIAN_POINT('Ctrl Pts',(42.9348366133039,-3.00063580575634,
51.992828129818));
#261903=CARTESIAN_POINT('Ctrl Pts',(42.8904524036951,-1.94712039905108,
52.6365582703688));
#261904=CARTESIAN_POINT('Ctrl Pts',(42.8676758816576,-1.35939952094611,
52.8532110500324));
#261905=CARTESIAN_POINT('Ctrl Pts',(42.824005292089,-0.140814301270381,
53.0471837815254));
#261906=CARTESIAN_POINT('Ctrl Pts',(42.803937588497,0.477998516061842,53.025340855115));
#261907=CARTESIAN_POINT('Ctrl Pts',(42.7596209950149,1.68036223673757,52.7458177117104));
#261908=CARTESIAN_POINT('Ctrl Pts',(42.7368185887115,2.25178562281226,52.4879606083973));
#261909=CARTESIAN_POINT('Ctrl Pts',(42.6930698118832,3.2563675740869,51.7717238131867));
#261910=CARTESIAN_POINT('Ctrl Pts',(42.673052782406,3.68179377358338,51.3227646567323));
#261911=CARTESIAN_POINT('Ctrl Pts',(42.6288062995307,4.34323297804011,50.2806811074282));
#261912=CARTESIAN_POINT('Ctrl Pts',(42.6059792614027,4.57008234897593,49.6956812528288));
#261913=CARTESIAN_POINT('Ctrl Pts',(42.5621527543214,4.7839982734579,48.4807191874492));
#261914=CARTESIAN_POINT('Ctrl Pts',(42.5421775196057,4.77260115723484,47.8629689153095));
#261915=CARTESIAN_POINT('Ctrl Pts',(42.4980034591323,4.51390729703929,46.6562169031062));
#261916=CARTESIAN_POINT('Ctrl Pts',(42.4751531709417,4.26532764079793,46.0795264810782));
#261917=CARTESIAN_POINT('Ctrl Pts',(42.4312496794982,3.56596209792612,45.063354420355));
#261918=CARTESIAN_POINT('Ctrl Pts',(42.4113069799741,3.12519122669073,44.6312525735299));
#261919=CARTESIAN_POINT('Ctrl Pts',(42.3672074406395,2.09489088525768,43.9519179105999));
#261920=CARTESIAN_POINT('Ctrl Pts',(42.3443353961348,1.51283444959629,43.7147306798429));
#261921=CARTESIAN_POINT('Ctrl Pts',(42.3113269822488,0.603833353132325,
43.5389852708176));
#261922=CARTESIAN_POINT('Ctrl Pts',(42.3007756214429,0.301918536111562,
43.5102));
#261923=CARTESIAN_POINT('Ctrl Pts',(42.2906249999995,-1.41414657761629E-13,
43.5102));
#261924=CARTESIAN_POINT('',(42.0942499999981,-4.66218791181221,47.3519229575834));
#261925=CARTESIAN_POINT('Origin',(42.09425,-1.46971288347598E-13,48.26));
#261926=CARTESIAN_POINT('Ctrl Pts',(42.0942499999949,-4.66218791181116,
47.3519229575838));
#261927=CARTESIAN_POINT('Ctrl Pts',(42.1068206953643,-4.59479830822025,
47.0059357994818));
#261928=CARTESIAN_POINT('Ctrl Pts',(42.1196360322443,-4.48910763171995,
46.6685368854524));
#261929=CARTESIAN_POINT('Ctrl Pts',(42.1452521950012,-4.20537339562081,
46.0241402159149));
#261930=CARTESIAN_POINT('Ctrl Pts',(42.157973999885,-4.02838111187797,45.7190573960525));
#261931=CARTESIAN_POINT('Ctrl Pts',(42.1918930242666,-3.45736524908123,
44.9466976226431));
#261932=CARTESIAN_POINT('Ctrl Pts',(42.2118479691889,-3.00461394811903,
44.531241285202));
#261933=CARTESIAN_POINT('Ctrl Pts',(42.2562007886005,-1.95293188098839,
43.885339138662));
#261934=CARTESIAN_POINT('Ctrl Pts',(42.2791600006447,-1.36067932859376,
43.666508184532));
#261935=CARTESIAN_POINT('Ctrl Pts',(42.3101114315129,-0.496745708215736,
43.529668100058));
#261936=CARTESIAN_POINT('Ctrl Pts',(42.3187355945367,-0.248293869611008,
43.5102));
#261937=CARTESIAN_POINT('Ctrl Pts',(42.3270833333327,-1.57374113740616E-13,
43.5102));
#261938=CARTESIAN_POINT('Origin',(40.475,-1.41317707189676E-13,48.26));
#261939=CARTESIAN_POINT('',(44.4072916666655,-1.14616064620334E-13,43.5102));
#261940=CARTESIAN_POINT('',(43.3854166666657,-1.47405174749987E-13,43.5102));
#261941=CARTESIAN_POINT('',(40.475,-1.40736024453017E-13,43.5102));
#261942=CARTESIAN_POINT('Ctrl Pts',(44.4072916666655,-7.68829444552921E-14,
43.5102));
#261943=CARTESIAN_POINT('Ctrl Pts',(44.390373149306,-0.503221800043606,
43.5102));
#261944=CARTESIAN_POINT('Ctrl Pts',(44.3724228202082,-1.00400848126724,
43.5901712341933));
#261945=CARTESIAN_POINT('Ctrl Pts',(44.3317689812627,-2.06827713231815,
43.9400702898141));
#261946=CARTESIAN_POINT('Ctrl Pts',(44.3093144518142,-2.61018179015523,
44.2442115659873));
#261947=CARTESIAN_POINT('Ctrl Pts',(44.2664558238078,-3.55263113629584,
45.0465299325764));
#261948=CARTESIAN_POINT('Ctrl Pts',(44.245434120635,-3.94250983519268,45.5389303845271));
#261949=CARTESIAN_POINT('Ctrl Pts',(44.2005289482455,-4.50748616977311,
46.640562123251));
#261950=CARTESIAN_POINT('Ctrl Pts',(44.1780452588232,-4.67930167148466,
47.2381452413367));
#261951=CARTESIAN_POINT('Ctrl Pts',(44.1351207318422,-4.78561759298201,
48.470848328726));
#261952=CARTESIAN_POINT('Ctrl Pts',(44.1142015396868,-4.71704371069777,
49.0943336232483));
#261953=CARTESIAN_POINT('Ctrl Pts',(44.0693356980773,-4.34523111346089,
50.274806553015));
#261954=CARTESIAN_POINT('Ctrl Pts',(44.0468223876693,-4.04739745399845,
50.8210722831369));
#261955=CARTESIAN_POINT('Ctrl Pts',(44.003829825242,-3.25703080618318,51.7724559182725));
#261956=CARTESIAN_POINT('Ctrl Pts',(43.9830123427014,-2.77083588879391,
52.1674392770573));
#261957=CARTESIAN_POINT('Ctrl Pts',(43.9381885376627,-1.67739508145053,
52.7463474425375));
#261958=CARTESIAN_POINT('Ctrl Pts',(43.9156452722035,-1.08129701659063,
52.9260262159433));
#261959=CARTESIAN_POINT('Ctrl Pts',(43.8725826769129,0.149139245221818,
53.0477291476656));
#261960=CARTESIAN_POINT('Ctrl Pts',(43.8518653644044,0.771810656405597,
52.9874638415031));
#261961=CARTESIAN_POINT('Ctrl Pts',(43.8070863850711,1.95644428853696,52.6319334746694));
#261962=CARTESIAN_POINT('Ctrl Pts',(43.7845129695506,2.5073606068132,52.3410113002896));
#261963=CARTESIAN_POINT('Ctrl Pts',(43.7413785072399,3.46835273705067,51.5636520648355));
#261964=CARTESIAN_POINT('Ctrl Pts',(43.7207590458096,3.86882423654003,51.0841452638541));
#261965=CARTESIAN_POINT('Ctrl Pts',(43.676027748612,4.46269147749009,49.9996522475672));
#261966=CARTESIAN_POINT('Ctrl Pts',(43.6534241378127,4.6508483976716,49.4052710434922));
#261967=CARTESIAN_POINT('Ctrl Pts',(43.6102161612666,4.78912928491696,48.1773773978022));
#261968=CARTESIAN_POINT('Ctrl Pts',(43.5896914222037,4.73776279420102,47.5555879400912));
#261969=CARTESIAN_POINT('Ctrl Pts',(43.5450107117975,4.39973740307766,46.3666264055932));
#261970=CARTESIAN_POINT('Ctrl Pts',(43.5223770192419,4.11631541612944,45.8108105370223));
#261971=CARTESIAN_POINT('Ctrl Pts',(43.4790940907976,3.35297349292576,44.8395962919077));
#261972=CARTESIAN_POINT('Ctrl Pts',(43.4586601181008,2.88059882280426,44.4332850148768));
#261973=CARTESIAN_POINT('Ctrl Pts',(43.4140329253292,1.80578318535348,43.8235300453172));
#261974=CARTESIAN_POINT('Ctrl Pts',(43.3913694300322,1.21336611326357,43.6263311050531));
#261975=CARTESIAN_POINT('Ctrl Pts',(43.3625984281871,0.40046982445354,43.5228482498025));
#261976=CARTESIAN_POINT('Ctrl Pts',(43.355686867337,0.200132489239812,43.5102));
#261977=CARTESIAN_POINT('Ctrl Pts',(43.3489583333325,-8.88872309090516E-14,
43.5102));
#261978=CARTESIAN_POINT('Ctrl Pts',(42.3270833333327,-1.58692503582358E-13,
43.5102));
#261979=CARTESIAN_POINT('Ctrl Pts',(42.3391268191607,0.358219605675742,
43.5102));
#261980=CARTESIAN_POINT('Ctrl Pts',(42.3517222752219,0.716072144886732,
43.5507220553516));
#261981=CARTESIAN_POINT('Ctrl Pts',(42.3870580817766,1.67550713468126,43.771834687857));
#261982=CARTESIAN_POINT('Ctrl Pts',(42.4100044194964,2.25071018064939,44.0309023121474));
#261983=CARTESIAN_POINT('Ctrl Pts',(42.4537685521365,3.25541035829208,44.7479563537824));
#261984=CARTESIAN_POINT('Ctrl Pts',(42.4736799101133,3.67877054229839,45.1942548347034));
#261985=CARTESIAN_POINT('Ctrl Pts',(42.5178973195813,4.34157757559234,46.2349070557574));
#261986=CARTESIAN_POINT('Ctrl Pts',(42.540829050309,4.56986676457151,46.8224244789149));
#261987=CARTESIAN_POINT('Ctrl Pts',(42.5846736373396,4.78365346537182,48.0379778377521));
#261988=CARTESIAN_POINT('Ctrl Pts',(42.6045767469768,4.77261296903086,48.6534449009786));
#261989=CARTESIAN_POINT('Ctrl Pts',(42.6487233031513,4.51547977408557,49.8600252782213));
#261990=CARTESIAN_POINT('Ctrl Pts',(42.671638691677,4.2665792047384,50.4385191081282));
#261991=CARTESIAN_POINT('Ctrl Pts',(42.715562820233,3.5670288607229,51.4552284488377));
#261992=CARTESIAN_POINT('Ctrl Pts',(42.7354671391831,3.12734152872271,51.8866946633223));
#261993=CARTESIAN_POINT('Ctrl Pts',(42.779541005205,2.09805709469439,52.5666383944541));
#261994=CARTESIAN_POINT('Ctrl Pts',(42.8024383362143,1.51551485277587,52.8044685584805));
#261995=CARTESIAN_POINT('Ctrl Pts',(42.8464407839502,0.303969126019783,
53.0392662005292));
#261996=CARTESIAN_POINT('Ctrl Pts',(42.8663559369636,-0.312565072840083,
53.0387117164381));
#261997=CARTESIAN_POINT('Ctrl Pts',(42.9103555026472,-1.52316486228873,
52.8018373341256));
#261998=CARTESIAN_POINT('Ctrl Pts',(42.9332331024559,-2.10481239179906,
52.5632640013233));
#261999=CARTESIAN_POINT('Ctrl Pts',(42.9773123779921,-3.13351782190955,
51.8815339846769));
#262000=CARTESIAN_POINT('Ctrl Pts',(42.9972479789687,-3.5731893320044,51.4485358354931));
#262001=CARTESIAN_POINT('Ctrl Pts',(43.0411719049501,-4.27027386260167,
50.430811146772));
#262002=CARTESIAN_POINT('Ctrl Pts',(43.0640281646247,-4.51759478199554,
49.8534217239611));
#262003=CARTESIAN_POINT('Ctrl Pts',(43.1081824830168,-4.7734775994132,48.6460925451697));
#262004=CARTESIAN_POINT('Ctrl Pts',(43.1281480926504,-4.7834671271449,48.0284855337753));
#262005=CARTESIAN_POINT('Ctrl Pts',(43.1719952818798,-4.5668549003936,46.8140251467023));
#262006=CARTESIAN_POINT('Ctrl Pts',(43.1948286809473,-4.33862772648435,
46.2294067979673));
#262007=CARTESIAN_POINT('Ctrl Pts',(43.2390560053496,-3.67480020980593,
45.1888823666758));
#262008=CARTESIAN_POINT('Ctrl Pts',(43.2590609647297,-3.24848507962646,
44.7410135082265));
#262009=CARTESIAN_POINT('Ctrl Pts',(43.3028305952225,-2.24235732064402,
44.027011163012));
#262010=CARTESIAN_POINT('Ctrl Pts',(43.3256397201589,-1.67022655307121,
43.7703793781029));
#262011=CARTESIAN_POINT('Ctrl Pts',(43.3608198337942,-0.714876476888766,
43.5505848889162));
#262012=CARTESIAN_POINT('Ctrl Pts',(43.3733935813015,-0.357612817396849,
43.5102));
#262013=CARTESIAN_POINT('Ctrl Pts',(43.3854166666658,-1.35585986882347E-13,
43.5102));
#262014=CARTESIAN_POINT('Origin',(40.475,-1.41317707189676E-13,48.26));
#262015=CARTESIAN_POINT('',(45.4656249999985,-1.50815726624334E-13,43.5102));
#262016=CARTESIAN_POINT('',(44.4437499999988,-1.09371457579084E-13,43.5102));
#262017=CARTESIAN_POINT('',(40.475,-1.40736024453017E-13,43.5102));
#262018=CARTESIAN_POINT('Ctrl Pts',(45.4656249999985,-1.42941214420489E-13,
43.5102));
#262019=CARTESIAN_POINT('Ctrl Pts',(45.4465902340685,-0.566167174768725,
43.5102));
#262020=CARTESIAN_POINT('Ctrl Pts',(45.4262808000091,-1.12831666969857,
43.611430906197));
#262021=CARTESIAN_POINT('Ctrl Pts',(45.3833509845901,-2.23435532889645,
44.023921560264));
#262022=CARTESIAN_POINT('Ctrl Pts',(45.3611023288805,-2.76208488292788,
44.3475011828492));
#262023=CARTESIAN_POINT('Ctrl Pts',(45.3186849235856,-3.67593158760918,
45.1871891138994));
#262024=CARTESIAN_POINT('Ctrl Pts',(45.2968843047985,-4.04943203210985,
45.6993730995744));
#262025=CARTESIAN_POINT('Ctrl Pts',(45.2517488041455,-4.5696569085595,46.8263923479332));
#262026=CARTESIAN_POINT('Ctrl Pts',(45.229477640157,-4.71644566319307,47.428020559987));
#262027=CARTESIAN_POINT('Ctrl Pts',(45.1870137044426,-4.7736692402272,48.6673586058746));
#262028=CARTESIAN_POINT('Ctrl Pts',(45.1653022980402,-4.67825065771647,
49.293389621709));
#262029=CARTESIAN_POINT('Ctrl Pts',(45.1201885041776,-4.25428195262979,
50.4596338382426));
#262030=CARTESIAN_POINT('Ctrl Pts',(45.097893833954,-3.93474684068756,50.9904073321236));
#262031=CARTESIAN_POINT('Ctrl Pts',(45.055380912789,-3.10290584598713,51.9103453537364));
#262032=CARTESIAN_POINT('Ctrl Pts',(45.0337617192976,-2.59492452463785,
52.2873404412951));
#262033=CARTESIAN_POINT('Ctrl Pts',(44.9886714132759,-1.47320517645412,
52.8171150725375));
#262034=CARTESIAN_POINT('Ctrl Pts',(44.9663522622886,-0.87234891209692,
52.9692133241849));
#262035=CARTESIAN_POINT('Ctrl Pts',(44.9237878756165,0.365654927904257,
53.0368711415337));
#262036=CARTESIAN_POINT('Ctrl Pts',(44.9022636356118,0.991153230745726,
52.9472027181652));
#262037=CARTESIAN_POINT('Ctrl Pts',(44.8571987189914,2.16054571570894,52.5343443824201));
#262038=CARTESIAN_POINT('Ctrl Pts',(44.8348541472401,2.69469457492858,52.2193747943591));
#262039=CARTESIAN_POINT('Ctrl Pts',(44.7922358051748,3.6214179089656,51.3963449289351));
#262040=CARTESIAN_POINT('Ctrl Pts',(44.7708089405814,4.00230089366428,50.8930517722625));
#262041=CARTESIAN_POINT('Ctrl Pts',(44.7257714374295,4.54270093040375,49.7773041716469));
#262042=CARTESIAN_POINT('Ctrl Pts',(44.7034005514389,4.7007270027171,49.1773644929559));
#262043=CARTESIAN_POINT('Ctrl Pts',(44.6607257712771,4.78002074245624,47.940896882699));
#262044=CARTESIAN_POINT('Ctrl Pts',(44.6393983237826,4.69673585831531,47.3159985829072));
#262045=CARTESIAN_POINT('Ctrl Pts',(44.5943903813102,4.29625205794682,46.1431750279315));
#262046=CARTESIAN_POINT('Ctrl Pts',(44.5719923468965,3.98640446044065,45.6053143854802));
#262047=CARTESIAN_POINT('Ctrl Pts',(44.5292586718744,3.17320321784598,44.6710894566896));
#262048=CARTESIAN_POINT('Ctrl Pts',(44.5080322394463,2.67510132706706,44.2859131457229));
#262049=CARTESIAN_POINT('Ctrl Pts',(44.463056127013,1.56603926024906,43.7337811473309));
#262050=CARTESIAN_POINT('Ctrl Pts',(44.4406301826481,0.967183012352598,
43.5691858099602));
#262051=CARTESIAN_POINT('Ctrl Pts',(44.4152792766867,0.235766499055907,
43.5145836208336));
#262052=CARTESIAN_POINT('Ctrl Pts',(44.4112527733547,0.117818553244039,
43.5102));
#262053=CARTESIAN_POINT('Ctrl Pts',(44.4072916666655,-7.47318873450808E-14,
43.5102));
#262054=CARTESIAN_POINT('Ctrl Pts',(43.3854166666658,-1.37945210809676E-13,
43.5102));
#262055=CARTESIAN_POINT('Ctrl Pts',(43.3939205687891,0.252938767799535,
43.5102));
#262056=CARTESIAN_POINT('Ctrl Pts',(43.4027110535074,0.506033130485796,
43.530403283693));
#262057=CARTESIAN_POINT('Ctrl Pts',(43.4336826313524,1.3695165685671,43.6697769184864));
#262058=CARTESIAN_POINT('Ctrl Pts',(43.4564661935627,1.95688726194218,43.8877806596037));
#262059=CARTESIAN_POINT('Ctrl Pts',(43.5008325659325,3.00889875965012,44.5338607011944));
#262060=CARTESIAN_POINT('Ctrl Pts',(43.520942739417,3.46485166643091,44.9535835508839));
#262061=CARTESIAN_POINT('Ctrl Pts',(43.5645559399502,4.19533395069807,45.9482322667419));
#262062=CARTESIAN_POINT('Ctrl Pts',(43.5873127911785,4.46097731607732,46.5150754942648));
#262063=CARTESIAN_POINT('Ctrl Pts',(43.6317448550053,4.75813933136105,47.7135674873043));
#262064=CARTESIAN_POINT('Ctrl Pts',(43.6519198657491,4.78885255595582,48.3332802923877));
#262065=CARTESIAN_POINT('Ctrl Pts',(43.6954547796803,4.61172004566973,49.5548054446156));
#262066=CARTESIAN_POINT('Ctrl Pts',(43.7181839244842,4.40368282860139,50.1446858243819));
#262067=CARTESIAN_POINT('Ctrl Pts',(43.7626789442841,3.77496669459671,51.2077161576492));
#262068=CARTESIAN_POINT('Ctrl Pts',(43.7829261062389,3.36166674266077,51.67153927919));
#262069=CARTESIAN_POINT('Ctrl Pts',(43.8263830720853,2.37823063200775,52.4178722866199));
#262070=CARTESIAN_POINT('Ctrl Pts',(43.8490836771301,1.81662634707887,52.6921246523139));
#262071=CARTESIAN_POINT('Ctrl Pts',(43.8936388223165,0.622625619815621,
53.0089677686193));
#262072=CARTESIAN_POINT('Ctrl Pts',(43.9139647275047,0.00191039525560578,
53.0496087451274));
#262073=CARTESIAN_POINT('Ctrl Pts',(43.9573443645712,-1.22275842556398,
52.8912158432986));
#262074=CARTESIAN_POINT('Ctrl Pts',(43.9800157646236,-1.81489342511969,
52.692768295012));
#262075=CARTESIAN_POINT('Ctrl Pts',(44.0246281409167,-2.88836171452507,
52.0808244812212));
#262076=CARTESIAN_POINT('Ctrl Pts',(44.0450386063447,-3.35975143565501,
51.6737076021874));
#262077=CARTESIAN_POINT('Ctrl Pts',(44.0883418029553,-4.12114558046663,
50.7010837075983));
#262078=CARTESIAN_POINT('Ctrl Pts',(44.110983503581,-4.40352124979238,50.1445962492606));
#262079=CARTESIAN_POINT('Ctrl Pts',(44.1556501829778,-4.73911767096824,
48.9550459386729));
#262080=CARTESIAN_POINT('Ctrl Pts',(44.1761502153232,-4.78925197630396,
48.3333793250293));
#262081=CARTESIAN_POINT('Ctrl Pts',(44.2193781136555,-4.64866775580551,
47.1058472006399));
#262082=CARTESIAN_POINT('Ctrl Pts',(44.2419897907381,-4.45933251113791,
46.5117141522488));
#262083=CARTESIAN_POINT('Ctrl Pts',(44.286707839491,-3.86339106873334,45.4284743580556));
#262084=CARTESIAN_POINT('Ctrl Pts',(44.3073016172268,-3.46215786932346,
44.9498969868947));
#262085=CARTESIAN_POINT('Ctrl Pts',(44.3504555952403,-2.49983219569656,
44.1743558263898));
#262086=CARTESIAN_POINT('Ctrl Pts',(44.3730370915411,-1.94827382197323,
43.8844034463062));
#262087=CARTESIAN_POINT('Ctrl Pts',(44.4120410312371,-0.915635083605541,
43.5766189918152));
#262088=CARTESIAN_POINT('Ctrl Pts',(44.428331374608,-0.458609242081003,
43.5102));
#262089=CARTESIAN_POINT('Ctrl Pts',(44.4437499999988,-5.89805981832114E-14,
43.5102));
#262090=CARTESIAN_POINT('Origin',(40.475,-1.41317707189676E-13,48.26));
#262091=CARTESIAN_POINT('',(46.5239583333315,-1.62531318710601E-13,43.5102));
#262092=CARTESIAN_POINT('',(45.5020833333317,-1.42870944908646E-13,43.5102));
#262093=CARTESIAN_POINT('',(40.475,-1.40736024453017E-13,43.5102));
#262094=CARTESIAN_POINT('Ctrl Pts',(46.5239583333315,-1.62370117351429E-13,
43.5102));
#262095=CARTESIAN_POINT('Ctrl Pts',(46.5036008374102,-0.605510253896953,
43.5102));
#262096=CARTESIAN_POINT('Ctrl Pts',(46.4818076969026,-1.20576070108166,
43.6259890631562));
#262097=CARTESIAN_POINT('Ctrl Pts',(46.4374905918229,-2.33611695352889,
44.0793903497508));
#262098=CARTESIAN_POINT('Ctrl Pts',(46.4153861300924,-2.85467272875886,
44.4147631522864));
#262099=CARTESIAN_POINT('Ctrl Pts',(46.3732591906852,-3.75030468937599,
45.2775675910213));
#262100=CARTESIAN_POINT('Ctrl Pts',(46.350867950729,-4.11332423204566,45.8022845225455));
#262101=CARTESIAN_POINT('Ctrl Pts',(46.3056097860154,-4.60492983715441,
46.9448067623493));
#262102=CARTESIAN_POINT('Ctrl Pts',(46.283490643379,-4.73591436814603,47.5484595982699));
#262103=CARTESIAN_POINT('Ctrl Pts',(46.2413346731749,-4.76199965834225,
48.7915354657041));
#262104=CARTESIAN_POINT('Ctrl Pts',(46.2190049601663,-4.64927095256036,
49.4191198129382));
#262105=CARTESIAN_POINT('Ctrl Pts',(46.1737580864563,-4.19207402121399,
50.5755587541874));
#262106=CARTESIAN_POINT('Ctrl Pts',(46.1516233565398,-3.85907637047691,
51.0959986418156));
#262107=CARTESIAN_POINT('Ctrl Pts',(46.1094364386808,-3.00095705659985,
51.9953552346118));
#262108=CARTESIAN_POINT('Ctrl Pts',(46.0871717251068,-2.47879870234449,
52.3605222090012));
#262109=CARTESIAN_POINT('Ctrl Pts',(46.0419371201451,-1.33940444906901,
52.8579876629451));
#262110=CARTESIAN_POINT('Ctrl Pts',(46.01978586708,-0.736131320341421,52.9921946738508));
#262111=CARTESIAN_POINT('Ctrl Pts',(45.9775659990635,0.506210804173913,
53.0246397502708));
#262112=CARTESIAN_POINT('Ctrl Pts',(45.9553698123262,1.13348286507559,52.9154651892213));
#262113=CARTESIAN_POINT('Ctrl Pts',(45.9101485354608,2.29197503236145,52.4650632422377));
#262114=CARTESIAN_POINT('Ctrl Pts',(45.8879797972532,2.81455697175497,52.1347948945605));
#262115=CARTESIAN_POINT('Ctrl Pts',(45.8457248934765,3.71815798027413,51.2820405739011));
#262116=CARTESIAN_POINT('Ctrl Pts',(45.8236007922176,4.08576925695497,50.7628005139269));
#262117=CARTESIAN_POINT('Ctrl Pts',(45.7783939899705,4.58990752858193,49.6269971919372));
#262118=CARTESIAN_POINT('Ctrl Pts',(45.7562067826859,4.72779263414618,49.0241781630782));
#262119=CARTESIAN_POINT('Ctrl Pts',(45.713914678184,4.76748967906392,47.782691311264));
#262120=CARTESIAN_POINT('Ctrl Pts',(45.6918662243994,4.6623560474797,47.155778630674));
#262121=CARTESIAN_POINT('Ctrl Pts',(45.6466751360762,4.21969723649481,45.9949770748332));
#262122=CARTESIAN_POINT('Ctrl Pts',(45.6244684589117,3.892553992568,45.469972224536));
#262123=CARTESIAN_POINT('Ctrl Pts',(45.5821369144204,3.04591872211625,44.5615570327062));
#262124=CARTESIAN_POINT('Ctrl Pts',(45.5601676411215,2.52999210496053,44.1911767212705));
#262125=CARTESIAN_POINT('Ctrl Pts',(45.5149936043689,1.39829579747449,43.6794760641619));
#262126=CARTESIAN_POINT('Ctrl Pts',(45.4927664456731,0.796019569018646,
43.5374116915684));
#262127=CARTESIAN_POINT('Ctrl Pts',(45.4697508383311,0.122230094171664,
43.5113786479076));
#262128=CARTESIAN_POINT('Ctrl Pts',(45.4676789441933,0.0610922028778175,
43.5102));
#262129=CARTESIAN_POINT('Ctrl Pts',(45.4656249999985,-1.43470754738992E-13,
43.5102));
#262130=CARTESIAN_POINT('Ctrl Pts',(44.4437499999988,-5.99173488602389E-14,
43.5102));
#262131=CARTESIAN_POINT('Ctrl Pts',(44.4490830245783,0.158624669738691,
43.5102));
#262132=CARTESIAN_POINT('Ctrl Pts',(44.4545328214474,0.317431308338911,
43.5181458728695));
#262133=CARTESIAN_POINT('Ctrl Pts',(44.4815761187494,1.08959979877602,43.5958913234831));
#262134=CARTESIAN_POINT('Ctrl Pts',(44.5041274378078,1.68548201395458,43.7766695169645));
#262135=CARTESIAN_POINT('Ctrl Pts',(44.5489395260635,2.77776933644252,44.3575210824724));
#262136=CARTESIAN_POINT('Ctrl Pts',(44.5697300255303,3.26309684251997,44.7532169626168));
#262137=CARTESIAN_POINT('Ctrl Pts',(44.612741135947,4.0517839323666,45.705847982011));
#262138=CARTESIAN_POINT('Ctrl Pts',(44.6352624336814,4.34872785466118,46.2527198271492));
#262139=CARTESIAN_POINT('Ctrl Pts',(44.6801172971881,4.71843598020359,47.4337379266194));
#262140=CARTESIAN_POINT('Ctrl Pts',(44.7010091685603,4.78593419842796,48.0571184351156));
#262141=CARTESIAN_POINT('Ctrl Pts',(44.743951694488,4.67763124679665,49.2895338255994));
#262142=CARTESIAN_POINT('Ctrl Pts',(44.7664432688965,4.50480069578187,49.8869310263233));
#262143=CARTESIAN_POINT('Ctrl Pts',(44.8113381781625,3.93802269070928,50.9875112239144));
#262144=CARTESIAN_POINT('Ctrl Pts',(44.832332415779,3.54748413748238,51.4791104293721));
#262145=CARTESIAN_POINT('Ctrl Pts',(44.8752084588664,2.60388019462774,52.279891895045));
#262146=CARTESIAN_POINT('Ctrl Pts',(44.8976707382443,2.06141002983677,52.5832244235893));
#262147=CARTESIAN_POINT('Ctrl Pts',(44.9420768352923,0.898155571040059,
52.9635927494964));
#262148=CARTESIAN_POINT('Ctrl Pts',(44.9627764100013,0.289169763904942,
53.039833984679));
#262149=CARTESIAN_POINT('Ctrl Pts',(45.005495989191,-0.94715505118126,52.9569785783005));
#262150=CARTESIAN_POINT('Ctrl Pts',(45.0284962665617,-1.56201031345564,
52.7897665739478));
#262151=CARTESIAN_POINT('Ctrl Pts',(45.0734758495259,-2.6701092429633,52.2350601445217));
#262152=CARTESIAN_POINT('Ctrl Pts',(45.0942529077285,-3.1566752646787,51.8608257934969));
#262153=CARTESIAN_POINT('Ctrl Pts',(45.1369115840167,-3.97741086967365,
50.9319524507001));
#262154=CARTESIAN_POINT('Ctrl Pts',(45.1599088389435,-4.29692068711041,
50.3802709072346));
#262155=CARTESIAN_POINT('Ctrl Pts',(45.2049197616781,-4.69422254308849,
49.2060407032733));
#262156=CARTESIAN_POINT('Ctrl Pts',(45.2257736105639,-4.77667886664448,
48.5976543478092));
#262157=CARTESIAN_POINT('Ctrl Pts',(45.2683740367194,-4.70627373513496,
47.3597165296944));
#262158=CARTESIAN_POINT('Ctrl Pts',(45.2913678851307,-4.54499228938495,
46.7425959716021));
#262159=CARTESIAN_POINT('Ctrl Pts',(45.3364080181532,-4.00068514395075,
45.6283885259276));
#262160=CARTESIAN_POINT('Ctrl Pts',(45.3573375096765,-3.63101697737368,
45.138057673055));
#262161=CARTESIAN_POINT('Ctrl Pts',(45.3998823651131,-2.70942297072614,
44.3079214437151));
#262162=CARTESIAN_POINT('Ctrl Pts',(45.4228725062249,-2.16022155508338,
43.982934896878));
#262163=CARTESIAN_POINT('Ctrl Pts',(45.4651887079935,-1.06039337333246,
43.5995131929409));
#262164=CARTESIAN_POINT('Ctrl Pts',(45.4842039863065,-0.531800571084733,
43.5102));
#262165=CARTESIAN_POINT('Ctrl Pts',(45.5020833333318,-1.29618538124987E-13,
43.5102));
#262166=CARTESIAN_POINT('Origin',(40.475,-1.41317707189676E-13,48.26));
#262167=CARTESIAN_POINT('',(47.5822916659101,-1.12196777507983E-8,43.5102));
#262168=CARTESIAN_POINT('',(46.5604166666648,-1.64744021012041E-13,43.5102));
#262169=CARTESIAN_POINT('',(40.475,-1.40736024453017E-13,43.5102));
#262170=CARTESIAN_POINT('Ctrl Pts',(47.5822916662868,-1.12323599033015E-8,
43.5102));
#262171=CARTESIAN_POINT('Ctrl Pts',(47.5619423247769,-0.605267720969552,
43.5102000014313));
#262172=CARTESIAN_POINT('Ctrl Pts',(47.5401645011038,-1.20510137850486,
43.625895412559));
#262173=CARTESIAN_POINT('Ctrl Pts',(47.4950292970466,-2.35644830837556,
44.0873667724118));
#262174=CARTESIAN_POINT('Ctrl Pts',(47.4721044817229,-2.89251300407696,
44.4393772525012));
#262175=CARTESIAN_POINT('Ctrl Pts',(47.4301570353803,-3.77706893480709,
45.3160325548263));
#262176=CARTESIAN_POINT('Ctrl Pts',(47.4082806115085,-4.12379833993764,
45.8253303490187));
#262177=CARTESIAN_POINT('Ctrl Pts',(47.3629657401008,-4.61505081519561,
46.9696855352567));
#262178=CARTESIAN_POINT('Ctrl Pts',(47.3400383819616,-4.7460112676243,47.5973877834964));
#262179=CARTESIAN_POINT('Ctrl Pts',(47.298073272432,-4.75328333135358,48.8425794136922));
#262180=CARTESIAN_POINT('Ctrl Pts',(47.2762280767327,-4.63917883647766,
49.4479616397681));
#262181=CARTESIAN_POINT('Ctrl Pts',(47.2309203610855,-4.17905205326832,
50.6049966699415));
#262182=CARTESIAN_POINT('Ctrl Pts',(47.207990303116,-3.82862449556926,51.1418729700229));
#262183=CARTESIAN_POINT('Ctrl Pts',(47.1660061719569,-2.95470207981842,
52.0286520470236));
#262184=CARTESIAN_POINT('Ctrl Pts',(47.144194401308,-2.44653487105249,52.3767460972433));
#262185=CARTESIAN_POINT('Ctrl Pts',(47.0988944542651,-1.30394588441433,
52.8711908667363));
#262186=CARTESIAN_POINT('Ctrl Pts',(47.0759615361057,-0.676834674480039,
53.0039774657885));
#262187=CARTESIAN_POINT('Ctrl Pts',(47.0339569365298,0.567965482807333,
53.0150303299691));
#262188=CARTESIAN_POINT('Ctrl Pts',(47.0121808943154,1.17352631992653,52.9028288165141));
#262189=CARTESIAN_POINT('Ctrl Pts',(46.9668893795248,2.33164582654647,52.4464835421591));
#262190=CARTESIAN_POINT('Ctrl Pts',(46.9439534386922,2.8694611262,52.0979004933294));
#262191=CARTESIAN_POINT('Ctrl Pts',(46.9019268325604,3.75882201964883,51.2271610910262));
#262192=CARTESIAN_POINT('Ctrl Pts',(46.8801889252566,4.10850263838954,50.7203080174567));
#262193=CARTESIAN_POINT('Ctrl Pts',(46.8349065609813,4.60665335937256,49.5797770653415));
#262194=CARTESIAN_POINT('Ctrl Pts',(46.8119674343812,4.7415598214872,48.9533592685245));
#262195=CARTESIAN_POINT('Ctrl Pts',(46.7699171895906,4.75700467169273,47.70902066711));
#262196=CARTESIAN_POINT('Ctrl Pts',(46.7482199214303,4.64701236019363,47.1032521937931));
#262197=CARTESIAN_POINT('Ctrl Pts',(46.7029474845507,4.19505684768359,45.9438818387573));
#262198=CARTESIAN_POINT('Ctrl Pts',(46.6800050103184,3.84861779247109,45.4049841394255));
#262199=CARTESIAN_POINT('Ctrl Pts',(46.6379293986921,2.98157626632718,44.5126339235632));
#262200=CARTESIAN_POINT('Ctrl Pts',(46.6162753641057,2.47624632147946,44.1611138927456));
#262201=CARTESIAN_POINT('Ctrl Pts',(46.5710136942996,1.33810750007012,43.6586740858176));
#262202=CARTESIAN_POINT('Ctrl Pts',(46.5480677140097,0.71250200241092,43.5213144103002));
#262203=CARTESIAN_POINT('Ctrl Pts',(46.5257182038233,0.0522560520112886,
43.5104155107889));
#262204=CARTESIAN_POINT('Ctrl Pts',(46.5248366067607,0.0261232309295294,
43.5102));
#262205=CARTESIAN_POINT('Ctrl Pts',(46.5239583333315,-1.6320678782792E-13,
43.5102));
#262206=CARTESIAN_POINT('Ctrl Pts',(45.5020833333317,-1.27453897717139E-13,
43.5102));
#262207=CARTESIAN_POINT('Ctrl Pts',(45.5046240043241,0.0755693305096932,
43.5102));
#262208=CARTESIAN_POINT('Ctrl Pts',(45.5071919115641,0.151201761329515,
43.5120034428537));
#262209=CARTESIAN_POINT('Ctrl Pts',(45.5314353880609,0.858292825627946,
43.5458101658758));
#262210=CARTESIAN_POINT('Ctrl Pts',(45.5544215964756,1.47739253944832,43.7017648941488));
#262211=CARTESIAN_POINT('Ctrl Pts',(45.5995141893975,2.5970258903536,44.2367397860434));
#262212=CARTESIAN_POINT('Ctrl Pts',(45.6205900058756,3.09072149426274,44.6023308982021));
#262213=CARTESIAN_POINT('Ctrl Pts',(45.663031759178,3.92921331639899,45.5173972508389));
#262214=CARTESIAN_POINT('Ctrl Pts',(45.6860138769148,4.25906430353926,46.0643451032907));
#262215=CARTESIAN_POINT('Ctrl Pts',(45.731129935053,4.67725347513067,47.2330506292525));
#262216=CARTESIAN_POINT('Ctrl Pts',(45.7522758227053,4.77024273033945,47.840428588214));
#262217=CARTESIAN_POINT('Ctrl Pts',(45.7946699987671,4.72090364611286,49.0809575774851));
#262218=CARTESIAN_POINT('Ctrl Pts',(45.8176479274089,4.56969597499951,49.7017773144619));
#262219=CARTESIAN_POINT('Ctrl Pts',(45.8627857499861,4.04303230143915,50.8261985886924));
#262220=CARTESIAN_POINT('Ctrl Pts',(45.8839993325933,3.68105632465102,51.3228801778135));
#262221=CARTESIAN_POINT('Ctrl Pts',(45.9263485235756,2.7717992805151,52.1687501962364));
#262222=CARTESIAN_POINT('Ctrl Pts',(45.9493222166804,2.22687990283323,52.5028933987062));
#262223=CARTESIAN_POINT('Ctrl Pts',(45.9944802071712,1.06053286026028,52.9297875312546));
#262224=CARTESIAN_POINT('Ctrl Pts',(46.0157589354208,0.453572105348301,
53.0271624369284));
#262225=CARTESIAN_POINT('Ctrl Pts',(46.0580656740932,-0.787983361553054,
52.9865801929745));
#262226=CARTESIAN_POINT('Ctrl Pts',(46.0810351299837,-1.41029123865711,
52.8395736212652));
#262227=CARTESIAN_POINT('Ctrl Pts',(46.126211793147,-2.53891297590829,52.3202616976962));
#262228=CARTESIAN_POINT('Ctrl Pts',(46.1475529902292,-3.03822772092515,
51.9614714595661));
#262229=CARTESIAN_POINT('Ctrl Pts',(46.1898197392216,-3.89057513217457,
51.0573495813617));
#262230=CARTESIAN_POINT('Ctrl Pts',(46.2127849942371,-4.22848369300958,
50.5142408474223));
#262231=CARTESIAN_POINT('Ctrl Pts',(46.2579789325657,-4.66303233929073,
49.3499951812442));
#262232=CARTESIAN_POINT('Ctrl Pts',(46.2793798352095,-4.76426216006541,
48.7433999159247));
#262233=CARTESIAN_POINT('Ctrl Pts',(46.32160897825,-4.73136914703602,47.5009674579309));
#262234=CARTESIAN_POINT('Ctrl Pts',(46.3445701005156,-4.58805767250563,
46.877376895531));
#262235=CARTESIAN_POINT('Ctrl Pts',(46.3897800102523,-4.0752097067891,45.7450888182613));
#262236=CARTESIAN_POINT('Ctrl Pts',(46.4112378051486,-3.71921141673633,
45.2434650441401));
#262237=CARTESIAN_POINT('Ctrl Pts',(46.4534316401483,-2.81960171713258,
44.3854600781061));
#262238=CARTESIAN_POINT('Ctrl Pts',(46.4763887238927,-2.27809729632209,
44.0442651253932));
#262239=CARTESIAN_POINT('Ctrl Pts',(46.5204002356443,-1.14689194172171,
43.6148577984356));
#262240=CARTESIAN_POINT('Ctrl Pts',(46.5410623551547,-0.575671689767508,
43.5102));
#262241=CARTESIAN_POINT('Ctrl Pts',(46.5604166666647,-1.66949787328008E-13,
43.5102));
#262242=CARTESIAN_POINT('Origin',(40.475,-1.41317707189676E-13,48.26));
#262243=CARTESIAN_POINT('',(48.640625002023,3.01226086749755E-8,43.5102));
#262244=CARTESIAN_POINT('',(47.6187499976816,-3.44458056410151E-8,43.5102));
#262245=CARTESIAN_POINT('',(40.475,-1.40736024453017E-13,43.5102));
#262246=CARTESIAN_POINT('Ctrl Pts',(48.6406250010114,3.01567474912057E-8,
43.5102));
#262247=CARTESIAN_POINT('Ctrl Pts',(48.6403402808376,-0.00846864324612915,
43.5101999999462));
#262248=CARTESIAN_POINT('Ctrl Pts',(48.6400552091581,-0.0169383903995125,
43.5102226487671));
#262249=CARTESIAN_POINT('Ctrl Pts',(48.6191798718932,-0.636478416209216,
43.5135369343409));
#262250=CARTESIAN_POINT('Ctrl Pts',(48.5971621151167,-1.24118429143203,
43.6346988877366));
#262251=CARTESIAN_POINT('Ctrl Pts',(48.5518367752532,-2.39313666806122,
44.1083618417949));
#262252=CARTESIAN_POINT('Ctrl Pts',(48.5290407974581,-2.92566350708343,
44.4647992630245));
#262253=CARTESIAN_POINT('Ctrl Pts',(48.4870990846606,-3.80266330856524,
45.349041959842));
#262254=CARTESIAN_POINT('Ctrl Pts',(48.4650895774633,-4.14518439984186,
45.8618125037741));
#262255=CARTESIAN_POINT('Ctrl Pts',(48.4197592212302,-4.62633837758331,
47.0108112029288));
#262256=CARTESIAN_POINT('Ctrl Pts',(48.3969299909334,-4.75166011105822,
47.6394713519076));
#262257=CARTESIAN_POINT('Ctrl Pts',(48.3550030935466,-4.74796833627022,
48.8850094101939));
#262258=CARTESIAN_POINT('Ctrl Pts',(48.3330012731708,-4.62830538735032,
49.4898621835297));
#262259=CARTESIAN_POINT('Ctrl Pts',(48.2876663003645,-4.15739165130443,
50.6432398443229));
#262260=CARTESIAN_POINT('Ctrl Pts',(48.2648060457194,-3.80196381608403,
51.1769600772513));
#262261=CARTESIAN_POINT('Ctrl Pts',(48.2228929205492,-2.91946417246145,
52.0561151610514));
#262262=CARTESIAN_POINT('Ctrl Pts',(48.200898257452,-2.40758203843062,52.3997151384207));
#262263=CARTESIAN_POINT('Ctrl Pts',(48.1555590355424,-1.25945421064565,
52.8836082121268));
#262264=CARTESIAN_POINT('Ctrl Pts',(48.1326698594116,-0.630673758570354,
53.0103761234247));
#262265=CARTESIAN_POINT('Ctrl Pts',(48.0907695298135,0.615133469116345,
53.0092419608279));
#262266=CARTESIAN_POINT('Ctrl Pts',(48.0687815264716,1.22010977350227,52.8908694158124));
#262267=CARTESIAN_POINT('Ctrl Pts',(48.023441724036,2.3746266275441,52.4223591295305));
#262268=CARTESIAN_POINT('Ctrl Pts',(48.0005256061278,2.90939118846583,52.0678343904391));
#262269=CARTESIAN_POINT('Ctrl Pts',(47.9586368751837,3.79040161835962,51.1868357272435));
#262270=CARTESIAN_POINT('Ctrl Pts',(47.936655342557,4.13495748899571,50.6757367096215));
#262271=CARTESIAN_POINT('Ctrl Pts',(47.8913170826427,4.62111654763343,49.5285760969697));
#262272=CARTESIAN_POINT('Ctrl Pts',(47.8683990003311,4.74916318677365,48.8999428065474));
#262273=CARTESIAN_POINT('Ctrl Pts',(47.8264972255023,4.75040751120774,47.6541382226684));
#262274=CARTESIAN_POINT('Ctrl Pts',(47.804539214751,4.6332666990795,47.0490405340912));
#262275=CARTESIAN_POINT('Ctrl Pts',(47.7592060980522,4.1671060394343,45.8937492923668));
#262276=CARTESIAN_POINT('Ctrl Pts',(47.7362859153077,3.81374001495502,45.3583838722651));
#262277=CARTESIAN_POINT('Ctrl Pts',(47.694370056637,2.93474341586611,44.4757372773047));
#262278=CARTESIAN_POINT('Ctrl Pts',(47.6724373335368,2.4244753413614,44.1301787960157));
#262279=CARTESIAN_POINT('Ctrl Pts',(47.6271098037818,1.27860763790808,43.64166888973));
#262280=CARTESIAN_POINT('Ctrl Pts',(47.6041873785707,0.650402238452378,
43.5122773754931));
#262281=CARTESIAN_POINT('Ctrl Pts',(47.5826358605589,0.0102342257254587,
43.5102082686246));
#262282=CARTESIAN_POINT('Ctrl Pts',(47.5824636994493,0.00511691691828377,
43.5101999999879));
#262283=CARTESIAN_POINT('Ctrl Pts',(47.5822916662868,-1.12323625723863E-8,
43.5102));
#262284=CARTESIAN_POINT('Ctrl Pts',(46.5604166666647,-1.63817944252533E-13,
43.5102));
#262285=CARTESIAN_POINT('Ctrl Pts',(46.5615367790316,0.0333164514072579,
43.5102));
#262286=CARTESIAN_POINT('Ctrl Pts',(46.5626622633208,0.0666474877714339,
43.5105505358004));
#262287=CARTESIAN_POINT('Ctrl Pts',(46.5852859802539,0.733745769366106,
43.5245966824768));
#262288=CARTESIAN_POINT('Ctrl Pts',(46.6082391406889,1.35843845899938,43.6646756633591));
#262289=CARTESIAN_POINT('Ctrl Pts',(46.6534774353482,2.49391246938954,44.1718703706478));
#262290=CARTESIAN_POINT('Ctrl Pts',(46.6750405296683,2.99755105650663,44.5254336623452));
#262291=CARTESIAN_POINT('Ctrl Pts',(46.7171702744803,3.86047541902424,45.4210993924374));
#262292=CARTESIAN_POINT('Ctrl Pts',(46.7401196432355,4.20452601484771,45.9611914936831));
#262293=CARTESIAN_POINT('Ctrl Pts',(46.7853705168101,4.65159836673637,47.1219431444179));
#262294=CARTESIAN_POINT('Ctrl Pts',(46.8069820603205,4.75913295039603,47.7279429848354));
#262295=CARTESIAN_POINT('Ctrl Pts',(46.8490828312042,4.73879860375925,48.97175913092));
#262296=CARTESIAN_POINT('Ctrl Pts',(46.8720285523032,4.60153407961332,49.5973963322325));
#262297=CARTESIAN_POINT('Ctrl Pts',(46.9172910317213,4.09926063963386,50.7356281460643));
#262298=CARTESIAN_POINT('Ctrl Pts',(46.9389482871538,3.74781202136899,51.241017215303));
#262299=CARTESIAN_POINT('Ctrl Pts',(46.9810220010193,2.85557778140817,52.1082024576298));
#262300=CARTESIAN_POINT('Ctrl Pts',(47.0039642273676,2.31672197870589,52.454724860202));
#262301=CARTESIAN_POINT('Ctrl Pts',(47.0492374108295,1.15740005626358,52.9068509099196));
#262302=CARTESIAN_POINT('Ctrl Pts',(47.0709377090647,0.551639655500766,
53.0169290494785));
#262303=CARTESIAN_POINT('Ctrl Pts',(47.1129861845493,-0.692717019939179,
53.0016548841548));
#262304=CARTESIAN_POINT('Ctrl Pts',(47.1359250749044,-1.31916190183093,
52.8668307754803));
#262305=CARTESIAN_POINT('Ctrl Pts',(47.1812081274254,-2.45977296165277,
52.368824030063));
#262306=CARTESIAN_POINT('Ctrl Pts',(47.2029488802598,-2.9666771221035,52.0192050967237));
#262307=CARTESIAN_POINT('Ctrl Pts',(47.2449738385226,-3.83754039304243,
51.1299445253089));
#262308=CARTESIAN_POINT('Ctrl Pts',(47.2679095549076,-4.18619523897315,
50.5921656409207));
#262309=CARTESIAN_POINT('Ctrl Pts',(47.313201703992,-4.64268762188745,49.4340882023249));
#262310=CARTESIAN_POINT('Ctrl Pts',(47.3349804140488,-4.75496316694576,
48.8285343178715));
#262311=CARTESIAN_POINT('Ctrl Pts',(47.3769834803082,-4.74405742910946,
47.5837188255888));
#262312=CARTESIAN_POINT('Ctrl Pts',(47.3999161858311,-4.61134187087903,
46.9565845142116));
#262313=CARTESIAN_POINT('Ctrl Pts',(47.4452167173044,-4.11702129093329,
45.8139267033697));
#262314=CARTESIAN_POINT('Ctrl Pts',(47.4670309854212,-3.76898036413851,
45.3057154872926));
#262315=CARTESIAN_POINT('Ctrl Pts',(47.5090136911057,-2.88228778831692,
44.4316865997071));
#262316=CARTESIAN_POINT('Ctrl Pts',(47.5319435481428,-2.34544301461709,
44.081197359138));
#262317=CARTESIAN_POINT('Ctrl Pts',(47.5769211080058,-1.19688904259089,
43.6243033168787));
#262318=CARTESIAN_POINT('Ctrl Pts',(47.5985411648686,-0.60108850816148,
43.5102000043641));
#262319=CARTESIAN_POINT('Ctrl Pts',(47.6187499988384,-3.44848784250562E-8,
43.5102));
#262320=CARTESIAN_POINT('Origin',(40.475,-1.41317707189676E-13,48.26));
#262321=CARTESIAN_POINT('',(49.238,-1.71331875425299E-13,43.5102));
#262322=CARTESIAN_POINT('',(48.6770833340043,1.00166031396858E-8,43.5102));
#262323=CARTESIAN_POINT('',(40.475,-1.40736024453017E-13,43.5102));
#262324=CARTESIAN_POINT('',(49.238,-1.86990303000829,52.6262412551721));
#262325=CARTESIAN_POINT('Origin',(49.238,-1.71913558161958E-13,48.26));
#262326=CARTESIAN_POINT('Ctrl Pts',(49.238,-1.86990303000829,52.6262412551721));
#262327=CARTESIAN_POINT('Ctrl Pts',(49.2258845683299,-1.56383729601022,
52.7573181265444));
#262328=CARTESIAN_POINT('Ctrl Pts',(49.2137876533848,-1.24484153160789,
52.8558494941654));
#262329=CARTESIAN_POINT('Ctrl Pts',(49.1902689990312,-0.598087148393598,
52.9832738225069));
#262330=CARTESIAN_POINT('Ctrl Pts',(49.1789970034025,-0.272399227164311,
53.0131869119213));
#262331=CARTESIAN_POINT('Ctrl Pts',(49.1473284546882,0.665150328710388,
53.0025766190358));
#262332=CARTESIAN_POINT('Ctrl Pts',(49.1252713731853,1.26947276028809,52.8776651208351));
#262333=CARTESIAN_POINT('Ctrl Pts',(49.0799708480804,2.41784395231669,52.3971383205351));
#262334=CARTESIAN_POINT('Ctrl Pts',(49.0573327453722,2.9473875112117,52.0381816129474));
#262335=CARTESIAN_POINT('Ctrl Pts',(49.0153198975399,3.8189835138927,51.1495847597557));
#262336=CARTESIAN_POINT('Ctrl Pts',(48.9932736680055,4.15879206820481,50.6345983826297));
#262337=CARTESIAN_POINT('Ctrl Pts',(48.9479661434789,4.63308233656798,49.4834357447573));
#262338=CARTESIAN_POINT('Ctrl Pts',(48.9252845812558,4.7547860276341,48.8550795761242));
#262339=CARTESIAN_POINT('Ctrl Pts',(48.8832914499036,4.74468294064032,47.6102271173403));
#262340=CARTESIAN_POINT('Ctrl Pts',(48.8612553675669,4.62178279031756,47.0056961541918));
#262341=CARTESIAN_POINT('Ctrl Pts',(48.8159414036286,4.1449356425251,45.8554010775775));
#262342=CARTESIAN_POINT('Ctrl Pts',(48.7932191294468,3.78732928008337,45.3242575343515));
#262343=CARTESIAN_POINT('Ctrl Pts',(48.7512443740699,2.90106707411043,44.4497605377253));
#262344=CARTESIAN_POINT('Ctrl Pts',(48.7292177706584,2.38726818569485,44.1084944446942));
#262345=CARTESIAN_POINT('Ctrl Pts',(48.6842061952532,1.24508730776226,43.6337718041888));
#262346=CARTESIAN_POINT('Ctrl Pts',(48.6616555802689,0.625530370510131,
43.5102000039716));
#262347=CARTESIAN_POINT('Ctrl Pts',(48.6406250010114,3.01567516791668E-8,
43.5102));
#262348=CARTESIAN_POINT('Ctrl Pts',(47.6187499988384,-3.44848800534558E-8,
43.5102));
#262349=CARTESIAN_POINT('Ctrl Pts',(47.6190554156344,0.00908423608770984,
43.510199999934));
#262350=CARTESIAN_POINT('Ctrl Pts',(47.6193612351469,0.0181696901690511,
43.5102260611622));
#262351=CARTESIAN_POINT('Ctrl Pts',(47.6410631179697,0.662136500170199,
43.5139214564747));
#262352=CARTESIAN_POINT('Ctrl Pts',(47.6639902866763,1.28985842539487,43.6448208016816));
#262353=CARTESIAN_POINT('Ctrl Pts',(47.7093056539373,2.43427260627935,44.1359664574964));
#262354=CARTESIAN_POINT('Ctrl Pts',(47.7311842575743,2.94360820937294,44.4826502313436));
#262355=CARTESIAN_POINT('Ctrl Pts',(47.7731304748416,3.82035481584508,45.3671317852305));
#262356=CARTESIAN_POINT('Ctrl Pts',(47.7960551119496,4.17241816830255,45.903169279661));
#262357=CARTESIAN_POINT('Ctrl Pts',(47.8413770300831,4.63590244033921,47.0592360290128));
#262358=CARTESIAN_POINT('Ctrl Pts',(47.8632846262197,4.7516964766686,47.6644598597278));
#262359=CARTESIAN_POINT('Ctrl Pts',(47.9052145427422,4.74777924465977,48.909994331287));
#262360=CARTESIAN_POINT('Ctrl Pts',(47.9281368006109,4.61844016403251,49.5382164720474));
#262361=CARTESIAN_POINT('Ctrl Pts',(47.9734647507917,4.13002191265737,50.6841346452895));
#262362=CARTESIAN_POINT('Ctrl Pts',(47.9953993673612,3.78450253960707,51.1944351295972));
#262363=CARTESIAN_POINT('Ctrl Pts',(48.037314169267,2.9019197434865,52.0735098685421));
#262364=CARTESIAN_POINT('Ctrl Pts',(48.0602341951523,2.36657772452769,52.4269211246324));
#262365=CARTESIAN_POINT('Ctrl Pts',(48.1055676989055,1.21131348071787,52.8931747566165));
#262366=CARTESIAN_POINT('Ctrl Pts',(48.1275274716682,0.606220172191773,
53.0103623527895));
#262367=CARTESIAN_POINT('Ctrl Pts',(48.1694282675115,-0.639593744248682,
53.0092108581361));
#262368=CARTESIAN_POINT('Ctrl Pts',(48.1923462030236,-1.26824126499063,
52.8812091154099));
#262369=CARTESIAN_POINT('Ctrl Pts',(48.2376816627341,-2.41536511316516,
52.395162376501));
#262370=CARTESIAN_POINT('Ctrl Pts',(48.2596639329102,-2.92650865236691,
52.0506691843566));
#262371=CARTESIAN_POINT('Ctrl Pts',(48.3015532619484,-3.80756031737948,
51.1697271236059));
#262372=CARTESIAN_POINT('Ctrl Pts',(48.3244673767911,-4.16214899822476,
50.6350159036455));
#262373=CARTESIAN_POINT('Ctrl Pts',(48.3698102209431,-4.63077827583694,
49.4804578650764));
#262374=CARTESIAN_POINT('Ctrl Pts',(48.3917987188872,-4.74919686669791,
48.8754859221348));
#262375=CARTESIAN_POINT('Ctrl Pts',(48.4336999981435,-4.75042231280389,
47.6296882588265));
#262376=CARTESIAN_POINT('Ctrl Pts',(48.4565870245828,-4.62370604511379,
47.0009120908299));
#262377=CARTESIAN_POINT('Ctrl Pts',(48.5019259324576,-4.13991074199294,
45.8527531057449));
#262378=CARTESIAN_POINT('Ctrl Pts',(48.523921127265,-3.79634923939758,45.3408392198344));
#262379=CARTESIAN_POINT('Ctrl Pts',(48.5658352748235,-2.91727107546747,
44.4582773051979));
#262380=CARTESIAN_POINT('Ctrl Pts',(48.5886932226241,-2.38359346820029,
44.1028133915142));
#262381=CARTESIAN_POINT('Ctrl Pts',(48.6340278542553,-1.23026664392626,
43.6318014243508));
#262382=CARTESIAN_POINT('Ctrl Pts',(48.6560302458644,-0.625419053718888,
43.5120849431333));
#262383=CARTESIAN_POINT('Ctrl Pts',(48.6767586264633,-0.00965498329010137,
43.510207359137));
#262384=CARTESIAN_POINT('Ctrl Pts',(48.6769210372467,-0.00482730997555823,
43.5101999999898));
#262385=CARTESIAN_POINT('Ctrl Pts',(48.6770833336679,1.00279621503562E-8,
43.5102));
#262386=CARTESIAN_POINT('Origin',(42.09425,-1.46971288347598E-13,48.26));
#262387=CARTESIAN_POINT('',(42.0671867061318,-4.66579641623079,47.5288462557477));
#262388=CARTESIAN_POINT('Origin',(42.0904940530805,0.0419539454483869,48.1587073448045));
#262389=CARTESIAN_POINT('',(42.0671867061318,-4.68628896694512,47.6743911597878));
#262390=CARTESIAN_POINT('Origin',(42.0671867060951,-1.1101650337908E-6,
48.259999841405));
#262391=CARTESIAN_POINT('Origin',(42.1434096703743,0.157122447872717,47.8795110986836));
#262392=CARTESIAN_POINT('',(40.475,-1.40934325385969E-13,45.12945));
#262393=CARTESIAN_POINT('',(42.09425,-1.46389605610939E-13,43.5102));
#262394=CARTESIAN_POINT('Origin',(40.475,-1.41317707189676E-13,48.26));
#262395=CARTESIAN_POINT('Origin',(50.,-1.74574066942157E-13,48.26));
#262396=CARTESIAN_POINT('',(49.238,-0.908077042619528,52.9221879117714));
#262397=CARTESIAN_POINT('',(49.238,-1.71331875425299E-13,53.0098));
#262398=CARTESIAN_POINT('Origin',(49.238,-1.71913558161958E-13,48.26));
#262399=CARTESIAN_POINT('Origin',(49.2622522741381,0.101290884806737,48.3019587266361));
#262400=CARTESIAN_POINT('Origin',(49.2681001647118,0.380373159827433,48.418111922516));
#262401=CARTESIAN_POINT('Origin',(49.238,-1.71913558161958E-13,48.26));
#262402=CARTESIAN_POINT('',(50.,-1.74085702291593E-13,52.2478));
#262403=CARTESIAN_POINT('',(50.,-1.74085702291593E-13,52.2478));
#262404=CARTESIAN_POINT('Origin',(50.,-1.74574066942157E-13,48.26));
#262405=CARTESIAN_POINT('Origin',(40.475,-1.41317707189676E-13,48.26));
#262406=CARTESIAN_POINT('Ctrl Pts',(48.6770833336679,1.00279587411656E-8,
43.5102));
#262407=CARTESIAN_POINT('Ctrl Pts',(48.698253182187,0.629672755148532,43.5102000013294));
#262408=CARTESIAN_POINT('Ctrl Pts',(48.7209607258464,1.25321726916315,43.6354136739498));
#262409=CARTESIAN_POINT('Ctrl Pts',(48.7661149856871,2.39779765933032,44.1145892634239));
#262410=CARTESIAN_POINT('Ctrl Pts',(48.7881251061508,2.91060499549462,44.4570655678307));
#262411=CARTESIAN_POINT('Ctrl Pts',(48.8300680020356,3.7949199110413,45.3339759730068));
#262412=CARTESIAN_POINT('Ctrl Pts',(48.852861329914,4.15139914838053,45.8664533561614));
#262413=CARTESIAN_POINT('Ctrl Pts',(48.89818626695,4.62517599058976,47.0183465771308));
#262414=CARTESIAN_POINT('Ctrl Pts',(48.9202046816237,4.74640007620399,47.6230462847423));
#262415=CARTESIAN_POINT('Ctrl Pts',(48.9621635943343,4.75318456347128,48.8682555584822));
#262416=CARTESIAN_POINT('Ctrl Pts',(48.9849211271637,4.62960939173084,49.4967694962158));
#262417=CARTESIAN_POINT('Ctrl Pts',(49.0302405779038,4.15176681390732,50.6468154508066));
#262418=CARTESIAN_POINT('Ctrl Pts',(49.0522678865187,3.81055277871214,51.1606568777459));
#262419=CARTESIAN_POINT('Ctrl Pts',(49.0942440076311,2.93615950038779,52.0470026674728));
#262420=CARTESIAN_POINT('Ctrl Pts',(49.1169632491864,2.40507322360049,52.4046573926883));
#262421=CARTESIAN_POINT('Ctrl Pts',(49.1570831197733,1.38668037730972,52.826967238459));
#262422=CARTESIAN_POINT('Ctrl Pts',(49.1740393274788,0.929744443720402,
52.9414176733626));
#262423=CARTESIAN_POINT('Ctrl Pts',(49.2063727902452,0.00555594936310154,
53.0320305704281));
#262424=CARTESIAN_POINT('Ctrl Pts',(49.2215907184063,-0.45643928208532,
53.0101555976911));
#262425=CARTESIAN_POINT('Ctrl Pts',(49.238,-0.908077042619906,52.9221879117714));
#262426=CARTESIAN_POINT('Origin',(40.475,-1.41317707189676E-13,48.26));
#262427=CARTESIAN_POINT('Origin',(50.,-1.74574066942157E-13,48.26));
#262428=CARTESIAN_POINT('',(50.,-1.77392992590619E-13,51.0096306570156));
#262429=CARTESIAN_POINT('',(50.,-2.38125000000018,49.6348153285078));
#262430=CARTESIAN_POINT('Origin',(50.,-1.74574066942157E-13,48.26));
#262431=CARTESIAN_POINT('',(50.,2.38124999999983,49.6348153285078));
#262432=CARTESIAN_POINT('Origin',(50.,-1.74574066942157E-13,48.26));
#262433=CARTESIAN_POINT('',(50.,2.38124999999983,46.8851846714922));
#262434=CARTESIAN_POINT('Origin',(50.,-1.74574066942157E-13,48.26));
#262435=CARTESIAN_POINT('',(50.,-1.77392992590619E-13,45.5103693429844));
#262436=CARTESIAN_POINT('Origin',(50.,-1.74574066942157E-13,48.26));
#262437=CARTESIAN_POINT('',(50.,-2.38125000000018,46.8851846714922));
#262438=CARTESIAN_POINT('Origin',(50.,-1.74574066942157E-13,48.26));
#262439=CARTESIAN_POINT('Origin',(50.,-1.74574066942157E-13,48.26));
#262440=CARTESIAN_POINT('Origin',(50.,-1.74574066942157E-13,48.26));
#262441=CARTESIAN_POINT('Ctrl Pts',(50.0000000000005,6.90208666923676E-13,
51.0096306570161));
#262442=CARTESIAN_POINT('Ctrl Pts',(49.3125923357457,-1.19062500000018,
50.3222229927617));
#262443=CARTESIAN_POINT('Ctrl Pts',(50.0000000000005,-2.38125000000105,
49.6348153285073));
#262444=CARTESIAN_POINT('Origin',(50.,-1.74574066942157E-13,48.26));
#262445=CARTESIAN_POINT('Ctrl Pts',(50.0000000000005,-2.38125000000017,
49.6348153285088));
#262446=CARTESIAN_POINT('Ctrl Pts',(49.3125923357457,-2.38125000000017,
48.26));
#262447=CARTESIAN_POINT('Ctrl Pts',(50.0000000000005,-2.38125000000017,
46.8851846714912));
#262448=CARTESIAN_POINT('Origin',(50.,-1.74574066942157E-13,48.26));
#262449=CARTESIAN_POINT('Ctrl Pts',(50.0000000000005,-2.38125000000103,
46.8851846714927));
#262450=CARTESIAN_POINT('Ctrl Pts',(49.3125923357457,-1.19062500000017,
46.1977770072383));
#262451=CARTESIAN_POINT('Ctrl Pts',(50.0000000000005,6.88211024554572E-13,
45.5103693429839));
#262452=CARTESIAN_POINT('Origin',(50.,-1.74574066942157E-13,48.26));
#262453=CARTESIAN_POINT('Ctrl Pts',(50.0000000000005,-1.01963383062804E-12,
45.5103693429839));
#262454=CARTESIAN_POINT('Ctrl Pts',(49.3125923357457,1.19062499999984,46.1977770072383));
#262455=CARTESIAN_POINT('Ctrl Pts',(50.0000000000005,2.3812500000007,46.8851846714927));
#262456=CARTESIAN_POINT('Origin',(50.,-1.74574066942157E-13,48.26));
#262457=CARTESIAN_POINT('Ctrl Pts',(50.0000000000005,2.38124999999983,46.8851846714912));
#262458=CARTESIAN_POINT('Ctrl Pts',(49.3125923357457,2.38124999999983,48.26));
#262459=CARTESIAN_POINT('Ctrl Pts',(50.0000000000005,2.38124999999983,49.6348153285088));
#262460=CARTESIAN_POINT('Origin',(50.,-1.74574066942157E-13,48.26));
#262461=CARTESIAN_POINT('Ctrl Pts',(50.0000000000005,2.38125000000067,49.6348153285073));
#262462=CARTESIAN_POINT('Ctrl Pts',(49.3125923357458,1.19062499999982,50.3222229927617));
#262463=CARTESIAN_POINT('Ctrl Pts',(50.0000000000005,-1.03770552554851E-12,
51.0096306570161));
#262464=CARTESIAN_POINT('Origin',(46.428125,2.38124999999984,49.6348153285078));
#262465=CARTESIAN_POINT('',(46.428125,2.38124999999984,49.6348153285078));
#262466=CARTESIAN_POINT('',(46.428125,-1.62265562360849E-13,51.0096306570156));
#262467=CARTESIAN_POINT('',(46.428125,-1.62265562360849E-13,51.0096306570156));
#262468=CARTESIAN_POINT('',(46.428125,-2.38125000000016,49.6348153285078));
#262469=CARTESIAN_POINT('',(46.428125,-2.38125000000016,49.6348153285078));
#262470=CARTESIAN_POINT('',(46.428125,-2.38125000000016,46.8851846714922));
#262471=CARTESIAN_POINT('',(46.428125,-2.38125000000016,46.8851846714922));
#262472=CARTESIAN_POINT('',(46.428125,-1.62265562360849E-13,45.5103693429844));
#262473=CARTESIAN_POINT('',(46.428125,-1.62265562360849E-13,45.5103693429844));
#262474=CARTESIAN_POINT('',(46.428125,2.38124999999984,46.8851846714922));
#262475=CARTESIAN_POINT('',(46.428125,2.38124999999984,46.8851846714922));
#262476=CARTESIAN_POINT('',(46.428125,2.38124999999984,49.6348153285078));
#262477=CARTESIAN_POINT('Origin',(46.428125,-2.38125000000016,49.6348153285078));
#262478=CARTESIAN_POINT('',(46.428125,-1.62265562360849E-13,51.0096306570156));
#262479=CARTESIAN_POINT('',(46.428125,-2.38125000000016,49.6348153285078));
#262480=CARTESIAN_POINT('Origin',(46.428125,-2.38125000000016,46.8851846714922));
#262481=CARTESIAN_POINT('',(46.428125,-2.38125000000016,46.8851846714922));
#262482=CARTESIAN_POINT('Origin',(46.428125,-1.62265562360849E-13,45.5103693429844));
#262483=CARTESIAN_POINT('',(46.428125,-1.62265562360849E-13,45.5103693429844));
#262484=CARTESIAN_POINT('Origin',(46.428125,2.38124999999984,46.8851846714922));
#262485=CARTESIAN_POINT('',(46.428125,2.38124999999984,46.8851846714922));
#262486=CARTESIAN_POINT('Origin',(46.428125,2.38124999999984,49.6348153285078));
#262487=CARTESIAN_POINT('',(46.428125,2.38124999999984,49.6348153285078));
#262488=CARTESIAN_POINT('Origin',(46.428125,-1.62265562360849E-13,51.0096306570156));
#262489=CARTESIAN_POINT('Ctrl Pts',(40.4593750000001,4.72273670613168,48.26));
#262490=CARTESIAN_POINT('Ctrl Pts',(40.5255208333334,4.72273670613168,50.216221595197));
#262491=CARTESIAN_POINT('Ctrl Pts',(40.5916666666667,3.33947915066429,51.5994791506644));
#262492=CARTESIAN_POINT('Ctrl Pts',(40.6578125,1.9562215951969,52.9827367061318));
#262493=CARTESIAN_POINT('Ctrl Pts',(40.7239583333333,-1.4189775634514E-13,
52.9827367061318));
#262494=CARTESIAN_POINT('Ctrl Pts',(40.7901041666666,-1.95622159519718,
52.9827367061318));
#262495=CARTESIAN_POINT('Ctrl Pts',(40.8562499999999,-3.33947915066458,
51.5994791506644));
#262496=CARTESIAN_POINT('Ctrl Pts',(40.9223958333332,-4.72273670613197,
50.216221595197));
#262497=CARTESIAN_POINT('Ctrl Pts',(40.9885416666665,-4.72273670613197,
48.26));
#262498=CARTESIAN_POINT('Ctrl Pts',(41.0546874999999,-4.72273670613197,
46.303778404803));
#262499=CARTESIAN_POINT('Ctrl Pts',(41.1208333333332,-3.33947915066458,
44.9205208493356));
#262500=CARTESIAN_POINT('Ctrl Pts',(41.1869791666665,-1.95622159519719,
43.5372632938682));
#262501=CARTESIAN_POINT('Ctrl Pts',(41.2531249999998,-1.44902068765019E-13,
43.5372632938682));
#262502=CARTESIAN_POINT('Ctrl Pts',(41.3192708333331,1.9562215951969,43.5372632938682));
#262503=CARTESIAN_POINT('Ctrl Pts',(41.3854166666664,3.33947915066429,44.9205208493356));
#262504=CARTESIAN_POINT('Ctrl Pts',(41.4515624999997,4.72273670613168,46.303778404803));
#262505=CARTESIAN_POINT('Ctrl Pts',(41.5177083333331,4.72273670613168,48.26));
#262506=CARTESIAN_POINT('Ctrl Pts',(41.5838541666664,4.72273670613168,50.216221595197));
#262507=CARTESIAN_POINT('Ctrl Pts',(41.6499999999997,3.33947915066429,51.5994791506644));
#262508=CARTESIAN_POINT('Ctrl Pts',(41.716145833333,1.9562215951969,52.9827367061318));
#262509=CARTESIAN_POINT('Ctrl Pts',(41.7822916666663,-1.45592907428747E-13,
52.9827367061318));
#262510=CARTESIAN_POINT('Ctrl Pts',(41.8484374999996,-1.95622159519719,
52.9827367061318));
#262511=CARTESIAN_POINT('Ctrl Pts',(41.9145833333329,-3.33947915066458,
51.5994791506644));
#262512=CARTESIAN_POINT('Ctrl Pts',(41.9807291666662,-4.72273670613197,
50.216221595197));
#262513=CARTESIAN_POINT('Ctrl Pts',(42.0468749999995,-4.72273670613197,
48.26));
#262514=CARTESIAN_POINT('Ctrl Pts',(42.1130208333329,-4.72273670613197,
46.303778404803));
#262515=CARTESIAN_POINT('Ctrl Pts',(42.1791666666662,-3.33947915066458,
44.9205208493356));
#262516=CARTESIAN_POINT('Ctrl Pts',(42.2453124999995,-1.95622159519719,
43.5372632938682));
#262517=CARTESIAN_POINT('Ctrl Pts',(42.3114583333328,-1.48597219848627E-13,
43.5372632938682));
#262518=CARTESIAN_POINT('Ctrl Pts',(42.3776041666661,1.95622159519689,43.5372632938682));
#262519=CARTESIAN_POINT('Ctrl Pts',(42.4437499999994,3.33947915066428,44.9205208493356));
#262520=CARTESIAN_POINT('Ctrl Pts',(42.5098958333328,4.72273670613168,46.303778404803));
#262521=CARTESIAN_POINT('Ctrl Pts',(42.5760416666661,4.72273670613168,48.26));
#262522=CARTESIAN_POINT('Ctrl Pts',(42.6421874999994,4.72273670613168,50.216221595197));
#262523=CARTESIAN_POINT('Ctrl Pts',(42.7083333333327,3.33947915066428,51.5994791506644));
#262524=CARTESIAN_POINT('Ctrl Pts',(42.774479166666,1.95622159519689,52.9827367061318));
#262525=CARTESIAN_POINT('Ctrl Pts',(42.8406249999993,-1.49288058512355E-13,
52.9827367061318));
#262526=CARTESIAN_POINT('Ctrl Pts',(42.9067708333326,-1.95622159519719,
52.9827367061318));
#262527=CARTESIAN_POINT('Ctrl Pts',(42.9729166666659,-3.33947915066458,
51.5994791506644));
#262528=CARTESIAN_POINT('Ctrl Pts',(43.0390624999992,-4.72273670613198,
50.216221595197));
#262529=CARTESIAN_POINT('Ctrl Pts',(43.1052083333325,-4.72273670613198,
48.26));
#262530=CARTESIAN_POINT('Ctrl Pts',(43.1713541666659,-4.72273670613198,
46.303778404803));
#262531=CARTESIAN_POINT('Ctrl Pts',(43.2374999999992,-3.33947915066458,
44.9205208493356));
#262532=CARTESIAN_POINT('Ctrl Pts',(43.3036458333325,-1.95622159519719,
43.5372632938682));
#262533=CARTESIAN_POINT('Ctrl Pts',(43.3697916666658,-1.52292370932235E-13,
43.5372632938682));
#262534=CARTESIAN_POINT('Ctrl Pts',(43.4359374999991,1.95622159519689,43.5372632938682));
#262535=CARTESIAN_POINT('Ctrl Pts',(43.5020833333324,3.33947915066428,44.9205208493356));
#262536=CARTESIAN_POINT('Ctrl Pts',(43.5682291666658,4.72273670613167,46.303778404803));
#262537=CARTESIAN_POINT('Ctrl Pts',(43.6343749999991,4.72273670613167,48.26));
#262538=CARTESIAN_POINT('Ctrl Pts',(43.7005208333324,4.72273670613167,50.216221595197));
#262539=CARTESIAN_POINT('Ctrl Pts',(43.7666666666657,3.33947915066428,51.5994791506644));
#262540=CARTESIAN_POINT('Ctrl Pts',(43.832812499999,1.95622159519689,52.9827367061318));
#262541=CARTESIAN_POINT('Ctrl Pts',(43.8989583333323,-1.52983209595963E-13,
52.9827367061318));
#262542=CARTESIAN_POINT('Ctrl Pts',(43.9651041666656,-1.95622159519719,
52.9827367061318));
#262543=CARTESIAN_POINT('Ctrl Pts',(44.0312499999989,-3.33947915066459,
51.5994791506644));
#262544=CARTESIAN_POINT('Ctrl Pts',(44.0973958333322,-4.72273670613198,
50.216221595197));
#262545=CARTESIAN_POINT('Ctrl Pts',(44.1635416666655,-4.72273670613198,
48.26));
#262546=CARTESIAN_POINT('Ctrl Pts',(44.2296874999989,-4.72273670613198,
46.303778404803));
#262547=CARTESIAN_POINT('Ctrl Pts',(44.2958333333322,-3.33947915066459,
44.9205208493356));
#262548=CARTESIAN_POINT('Ctrl Pts',(44.3619791666655,-1.9562215951972,43.5372632938682));
#262549=CARTESIAN_POINT('Ctrl Pts',(44.4281249999988,-1.55987522015843E-13,
43.5372632938682));
#262550=CARTESIAN_POINT('Ctrl Pts',(44.4942708333321,1.95622159519689,43.5372632938682));
#262551=CARTESIAN_POINT('Ctrl Pts',(44.5604166666654,3.33947915066428,44.9205208493356));
#262552=CARTESIAN_POINT('Ctrl Pts',(44.6265624999988,4.72273670613167,46.303778404803));
#262553=CARTESIAN_POINT('Ctrl Pts',(44.6927083333321,4.72273670613167,48.26));
#262554=CARTESIAN_POINT('Ctrl Pts',(44.7588541666654,4.72273670613167,50.216221595197));
#262555=CARTESIAN_POINT('Ctrl Pts',(44.8249999999987,3.33947915066428,51.5994791506644));
#262556=CARTESIAN_POINT('Ctrl Pts',(44.891145833332,1.95622159519688,52.9827367061318));
#262557=CARTESIAN_POINT('Ctrl Pts',(44.9572916666653,-1.56678360679571E-13,
52.9827367061318));
#262558=CARTESIAN_POINT('Ctrl Pts',(45.0234374999986,-1.9562215951972,52.9827367061318));
#262559=CARTESIAN_POINT('Ctrl Pts',(45.0895833333319,-3.33947915066459,
51.5994791506644));
#262560=CARTESIAN_POINT('Ctrl Pts',(45.1557291666652,-4.72273670613198,
50.216221595197));
#262561=CARTESIAN_POINT('Ctrl Pts',(45.2218749999985,-4.72273670613198,
48.26));
#262562=CARTESIAN_POINT('Ctrl Pts',(45.2880208333319,-4.72273670613199,
46.303778404803));
#262563=CARTESIAN_POINT('Ctrl Pts',(45.3541666666652,-3.33947915066459,
44.9205208493356));
#262564=CARTESIAN_POINT('Ctrl Pts',(45.4203124999985,-1.9562215951972,43.5372632938682));
#262565=CARTESIAN_POINT('Ctrl Pts',(45.4864583333318,-1.59682673099451E-13,
43.5372632938682));
#262566=CARTESIAN_POINT('Ctrl Pts',(45.5526041666651,1.95622159519688,43.5372632938682));
#262567=CARTESIAN_POINT('Ctrl Pts',(45.6187499999984,3.33947915066427,44.9205208493356));
#262568=CARTESIAN_POINT('Ctrl Pts',(45.6848958333318,4.72273670613167,46.303778404803));
#262569=CARTESIAN_POINT('Ctrl Pts',(45.7510416666651,4.72273670613167,48.26));
#262570=CARTESIAN_POINT('Ctrl Pts',(45.8171874999984,4.72273670613167,50.216221595197));
#262571=CARTESIAN_POINT('Ctrl Pts',(45.8833333333317,3.33947915066427,51.5994791506644));
#262572=CARTESIAN_POINT('Ctrl Pts',(45.949479166665,1.95622159519688,52.9827367061318));
#262573=CARTESIAN_POINT('Ctrl Pts',(46.0156249999983,-1.60373511763179E-13,
52.9827367061318));
#262574=CARTESIAN_POINT('Ctrl Pts',(46.0817708333316,-1.9562215951972,52.9827367061318));
#262575=CARTESIAN_POINT('Ctrl Pts',(46.1479166666649,-3.33947915066459,
51.5994791506644));
#262576=CARTESIAN_POINT('Ctrl Pts',(46.2140624999982,-4.72273670613199,
50.216221595197));
#262577=CARTESIAN_POINT('Ctrl Pts',(46.2802083333315,-4.72273670613199,
48.26));
#262578=CARTESIAN_POINT('Ctrl Pts',(46.3463541666649,-4.72273670613199,
46.303778404803));
#262579=CARTESIAN_POINT('Ctrl Pts',(46.4124999999982,-3.3394791506646,44.9205208493356));
#262580=CARTESIAN_POINT('Ctrl Pts',(46.4786458333315,-1.95622159519721,
43.5372632938682));
#262581=CARTESIAN_POINT('Ctrl Pts',(46.5447916666648,-1.63377824183059E-13,
43.5372632938682));
#262582=CARTESIAN_POINT('Ctrl Pts',(46.6109374999981,1.95622159519688,43.5372632938682));
#262583=CARTESIAN_POINT('Ctrl Pts',(46.6770833333314,3.33947915066427,44.9205208493356));
#262584=CARTESIAN_POINT('Ctrl Pts',(46.7432291666648,4.72273670613166,46.303778404803));
#262585=CARTESIAN_POINT('Ctrl Pts',(46.8093749999981,4.72273670613166,48.26));
#262586=CARTESIAN_POINT('Ctrl Pts',(46.8755208333314,4.72273670613166,50.216221595197));
#262587=CARTESIAN_POINT('Ctrl Pts',(46.9416666666647,3.33947915066427,51.5994791506644));
#262588=CARTESIAN_POINT('Ctrl Pts',(47.007812499998,1.95622159519688,52.9827367061318));
#262589=CARTESIAN_POINT('Ctrl Pts',(47.0739583333313,-1.64068662846786E-13,
52.9827367061318));
#262590=CARTESIAN_POINT('Ctrl Pts',(47.1401041666646,-1.95622159519721,
52.9827367061318));
#262591=CARTESIAN_POINT('Ctrl Pts',(47.2062499999979,-3.3394791506646,51.5994791506644));
#262592=CARTESIAN_POINT('Ctrl Pts',(47.2723958333312,-4.72273670613199,
50.216221595197));
#262593=CARTESIAN_POINT('Ctrl Pts',(47.3385416666645,-4.72273670613199,
48.26));
#262594=CARTESIAN_POINT('Ctrl Pts',(47.4046874999979,-4.72273670613199,
46.303778404803));
#262595=CARTESIAN_POINT('Ctrl Pts',(47.4708333333312,-3.3394791506646,44.9205208493356));
#262596=CARTESIAN_POINT('Ctrl Pts',(47.5369791666645,-1.95622159519721,
43.5372632938682));
#262597=CARTESIAN_POINT('Ctrl Pts',(47.6031249999978,-1.67072975266666E-13,
43.5372632938682));
#262598=CARTESIAN_POINT('Ctrl Pts',(47.6692708333311,1.95622159519688,43.5372632938682));
#262599=CARTESIAN_POINT('Ctrl Pts',(47.7354166666644,3.33947915066426,44.9205208493356));
#262600=CARTESIAN_POINT('Ctrl Pts',(47.8015624999978,4.72273670613166,46.303778404803));
#262601=CARTESIAN_POINT('Ctrl Pts',(47.8677083333311,4.72273670613166,48.26));
#262602=CARTESIAN_POINT('Ctrl Pts',(47.9338541666644,4.72273670613166,50.216221595197));
#262603=CARTESIAN_POINT('Ctrl Pts',(47.9999999999977,3.33947915066427,51.5994791506644));
#262604=CARTESIAN_POINT('Ctrl Pts',(48.066145833331,1.95622159519687,52.9827367061318));
#262605=CARTESIAN_POINT('Ctrl Pts',(48.1322916666643,-1.67763813930394E-13,
52.9827367061318));
#262606=CARTESIAN_POINT('Ctrl Pts',(48.1984374999976,-1.95622159519721,
52.9827367061318));
#262607=CARTESIAN_POINT('Ctrl Pts',(48.2645833333309,-3.3394791506646,51.5994791506644));
#262608=CARTESIAN_POINT('Ctrl Pts',(48.3307291666642,-4.722736706132,50.216221595197));
#262609=CARTESIAN_POINT('Ctrl Pts',(48.3968749999976,-4.72273670613199,
48.26));
#262610=CARTESIAN_POINT('Ctrl Pts',(48.4630208333309,-4.722736706132,46.303778404803));
#262611=CARTESIAN_POINT('Ctrl Pts',(48.5291666666642,-3.3394791506646,44.9205208493356));
#262612=CARTESIAN_POINT('Ctrl Pts',(48.5953124999975,-1.95622159519721,
43.5372632938682));
#262613=CARTESIAN_POINT('Ctrl Pts',(48.6614583333308,-1.70768126350274E-13,
43.5372632938682));
#262614=CARTESIAN_POINT('Ctrl Pts',(48.7276041666641,1.95622159519687,43.5372632938682));
#262615=CARTESIAN_POINT('Ctrl Pts',(48.7937499999974,3.33947915066426,44.9205208493356));
#262616=CARTESIAN_POINT('Ctrl Pts',(48.8598958333308,4.72273670613165,46.303778404803));
#262617=CARTESIAN_POINT('Ctrl Pts',(48.9260416666641,4.72273670613165,48.26));
#262618=CARTESIAN_POINT('Ctrl Pts',(48.9921874999974,4.72273670613165,50.216221595197));
#262619=CARTESIAN_POINT('Ctrl Pts',(49.0583333333307,3.33947915066426,51.5994791506644));
#262620=CARTESIAN_POINT('Ctrl Pts',(49.124479166664,1.95622159519687,52.9827367061318));
#262621=CARTESIAN_POINT('Ctrl Pts',(49.1906249999973,-1.71458965014002E-13,
52.9827367061318));
#262622=CARTESIAN_POINT('Ctrl Pts',(49.2567708333306,-1.95622159519721,
52.9827367061318));
#262623=CARTESIAN_POINT('Ctrl Pts',(49.3229166666639,-3.33947915066461,
51.5994791506644));
#262624=CARTESIAN_POINT('Ctrl Pts',(49.3890624999972,-4.722736706132,50.216221595197));
#262625=CARTESIAN_POINT('Ctrl Pts',(49.4552083333306,-4.722736706132,48.26));
#262626=CARTESIAN_POINT('Ctrl Pts',(49.5213541666639,-4.722736706132,46.303778404803));
#262627=CARTESIAN_POINT('Ctrl Pts',(49.5874999999972,-3.33947915066461,
44.9205208493356));
#262628=CARTESIAN_POINT('Ctrl Pts',(49.6536458333305,-1.95622159519722,
43.5372632938682));
#262629=CARTESIAN_POINT('Ctrl Pts',(49.7197916666638,-1.74463277433882E-13,
43.5372632938682));
#262630=CARTESIAN_POINT('Ctrl Pts',(49.7859374999971,1.95622159519687,43.5372632938682));
#262631=CARTESIAN_POINT('Ctrl Pts',(49.8520833333304,3.33947915066426,44.9205208493356));
#262632=CARTESIAN_POINT('Ctrl Pts',(49.9182291666638,4.72273670613165,46.303778404803));
#262633=CARTESIAN_POINT('Ctrl Pts',(49.9843749999971,4.72273670613165,48.26));
#262634=CARTESIAN_POINT('Ctrl Pts',(50.0505208333304,4.72273670613165,50.216221595197));
#262635=CARTESIAN_POINT('Ctrl Pts',(50.1166666666637,3.33947915066426,51.5994791506644));
#262636=CARTESIAN_POINT('Ctrl Pts',(50.182812499997,1.95622159519687,52.9827367061318));
#262637=CARTESIAN_POINT('Ctrl Pts',(50.2489583333303,-1.7515411609761E-13,
52.9827367061318));
#262638=CARTESIAN_POINT('Ctrl Pts',(50.3151041666636,-1.95622159519722,
52.9827367061318));
#262639=CARTESIAN_POINT('Ctrl Pts',(50.3812499999969,-3.33947915066461,
51.5994791506644));
#262640=CARTESIAN_POINT('Ctrl Pts',(50.4473958333302,-4.722736706132,50.216221595197));
#262641=CARTESIAN_POINT('Ctrl Pts',(50.5135416666635,-4.722736706132,48.26));
#262642=CARTESIAN_POINT('Ctrl Pts',(50.5796874999969,-4.722736706132,46.303778404803));
#262643=CARTESIAN_POINT('Ctrl Pts',(50.6458333333302,-3.33947915066461,
44.9205208493356));
#262644=CARTESIAN_POINT('Ctrl Pts',(50.7119791666635,-1.95622159519722,
43.5372632938682));
#262645=CARTESIAN_POINT('Ctrl Pts',(50.7781249999968,-1.7815842851749E-13,
43.5372632938682));
#262646=CARTESIAN_POINT('Ctrl Pts',(50.8442708333301,1.95622159519686,43.5372632938682));
#262647=CARTESIAN_POINT('Ctrl Pts',(50.9104166666634,3.33947915066425,44.9205208493356));
#262648=CARTESIAN_POINT('Ctrl Pts',(50.9765624999968,4.72273670613165,46.303778404803));
#262649=CARTESIAN_POINT('Ctrl Pts',(51.0427083333301,4.72273670613165,48.26));
#262650=CARTESIAN_POINT('Ctrl Pts',(40.4763020833334,4.7520552744889,48.26));
#262651=CARTESIAN_POINT('Ctrl Pts',(40.5424479166667,4.7520552744889,50.22836574384));
#262652=CARTESIAN_POINT('Ctrl Pts',(40.60859375,3.36021050916436,51.6202105091645));
#262653=CARTESIAN_POINT('Ctrl Pts',(40.6747395833333,1.96836574383982,53.0120552744891));
#262654=CARTESIAN_POINT('Ctrl Pts',(40.7408854166666,-1.41955061696174E-13,
53.012055274489));
#262655=CARTESIAN_POINT('Ctrl Pts',(40.8070312499999,-1.96836574384011,
53.0120552744891));
#262656=CARTESIAN_POINT('Ctrl Pts',(40.8731770833332,-3.36021050916465,
51.6202105091645));
#262657=CARTESIAN_POINT('Ctrl Pts',(40.9393229166665,-4.75205527448919,
50.22836574384));
#262658=CARTESIAN_POINT('Ctrl Pts',(41.0054687499998,-4.75205527448919,
48.26));
#262659=CARTESIAN_POINT('Ctrl Pts',(41.0716145833332,-4.75205527448919,
46.29163425616));
#262660=CARTESIAN_POINT('Ctrl Pts',(41.1377604166665,-3.36021050916465,
44.8997894908355));
#262661=CARTESIAN_POINT('Ctrl Pts',(41.2039062499998,-1.96836574384011,
43.507944725511));
#262662=CARTESIAN_POINT('Ctrl Pts',(41.2700520833331,-1.44966555094233E-13,
43.507944725511));
#262663=CARTESIAN_POINT('Ctrl Pts',(41.3361979166664,1.96836574383982,43.507944725511));
#262664=CARTESIAN_POINT('Ctrl Pts',(41.4023437499997,3.36021050916436,44.8997894908355));
#262665=CARTESIAN_POINT('Ctrl Pts',(41.468489583333,4.7520552744889,46.29163425616));
#262666=CARTESIAN_POINT('Ctrl Pts',(41.5346354166664,4.7520552744889,48.26));
#262667=CARTESIAN_POINT('Ctrl Pts',(41.6007812499997,4.7520552744889,50.22836574384));
#262668=CARTESIAN_POINT('Ctrl Pts',(41.666927083333,3.36021050916436,51.6202105091645));
#262669=CARTESIAN_POINT('Ctrl Pts',(41.7330729166663,1.96836574383982,53.0120552744891));
#262670=CARTESIAN_POINT('Ctrl Pts',(41.7992187499996,-1.45650212779782E-13,
53.012055274489));
#262671=CARTESIAN_POINT('Ctrl Pts',(41.8653645833329,-1.96836574384011,
53.0120552744891));
#262672=CARTESIAN_POINT('Ctrl Pts',(41.9315104166662,-3.36021050916465,
51.6202105091645));
#262673=CARTESIAN_POINT('Ctrl Pts',(41.9976562499995,-4.75205527448919,
50.22836574384));
#262674=CARTESIAN_POINT('Ctrl Pts',(42.0638020833328,-4.75205527448919,
48.26));
#262675=CARTESIAN_POINT('Ctrl Pts',(42.1299479166662,-4.75205527448919,
46.29163425616));
#262676=CARTESIAN_POINT('Ctrl Pts',(42.1960937499995,-3.36021050916465,
44.8997894908355));
#262677=CARTESIAN_POINT('Ctrl Pts',(42.2622395833328,-1.96836574384011,
43.507944725511));
#262678=CARTESIAN_POINT('Ctrl Pts',(42.3283854166661,-1.48661706177841E-13,
43.507944725511));
#262679=CARTESIAN_POINT('Ctrl Pts',(42.3945312499994,1.96836574383982,43.507944725511));
#262680=CARTESIAN_POINT('Ctrl Pts',(42.4606770833327,3.36021050916436,44.8997894908355));
#262681=CARTESIAN_POINT('Ctrl Pts',(42.526822916666,4.7520552744889,46.29163425616));
#262682=CARTESIAN_POINT('Ctrl Pts',(42.5929687499994,4.7520552744889,48.26));
#262683=CARTESIAN_POINT('Ctrl Pts',(42.6591145833327,4.7520552744889,50.22836574384));
#262684=CARTESIAN_POINT('Ctrl Pts',(42.725260416666,3.36021050916436,51.6202105091645));
#262685=CARTESIAN_POINT('Ctrl Pts',(42.7914062499993,1.96836574383981,53.0120552744891));
#262686=CARTESIAN_POINT('Ctrl Pts',(42.8575520833326,-1.4934536386339E-13,
53.012055274489));
#262687=CARTESIAN_POINT('Ctrl Pts',(42.9236979166659,-1.96836574384011,
53.0120552744891));
#262688=CARTESIAN_POINT('Ctrl Pts',(42.9898437499992,-3.36021050916465,
51.6202105091645));
#262689=CARTESIAN_POINT('Ctrl Pts',(43.0559895833325,-4.7520552744892,50.22836574384));
#262690=CARTESIAN_POINT('Ctrl Pts',(43.1221354166658,-4.7520552744892,48.26));
#262691=CARTESIAN_POINT('Ctrl Pts',(43.1882812499991,-4.7520552744892,46.29163425616));
#262692=CARTESIAN_POINT('Ctrl Pts',(43.2544270833325,-3.36021050916466,
44.8997894908355));
#262693=CARTESIAN_POINT('Ctrl Pts',(43.3205729166658,-1.96836574384012,
43.507944725511));
#262694=CARTESIAN_POINT('Ctrl Pts',(43.3867187499991,-1.52356857261448E-13,
43.507944725511));
#262695=CARTESIAN_POINT('Ctrl Pts',(43.4528645833324,1.96836574383981,43.507944725511));
#262696=CARTESIAN_POINT('Ctrl Pts',(43.5190104166657,3.36021050916435,44.8997894908355));
#262697=CARTESIAN_POINT('Ctrl Pts',(43.5851562499991,4.75205527448889,46.29163425616));
#262698=CARTESIAN_POINT('Ctrl Pts',(43.6513020833324,4.75205527448889,48.26));
#262699=CARTESIAN_POINT('Ctrl Pts',(43.7174479166657,4.75205527448889,50.22836574384));
#262700=CARTESIAN_POINT('Ctrl Pts',(43.783593749999,3.36021050916435,51.6202105091645));
#262701=CARTESIAN_POINT('Ctrl Pts',(43.8497395833323,1.96836574383981,53.0120552744891));
#262702=CARTESIAN_POINT('Ctrl Pts',(43.9158854166656,-1.53040514946997E-13,
53.012055274489));
#262703=CARTESIAN_POINT('Ctrl Pts',(43.9820312499989,-1.96836574384012,
53.0120552744891));
#262704=CARTESIAN_POINT('Ctrl Pts',(44.0481770833322,-3.36021050916466,
51.6202105091645));
#262705=CARTESIAN_POINT('Ctrl Pts',(44.1143229166655,-4.7520552744892,50.22836574384));
#262706=CARTESIAN_POINT('Ctrl Pts',(44.1804687499988,-4.7520552744892,48.26));
#262707=CARTESIAN_POINT('Ctrl Pts',(44.2466145833321,-4.7520552744892,46.29163425616));
#262708=CARTESIAN_POINT('Ctrl Pts',(44.3127604166655,-3.36021050916466,
44.8997894908355));
#262709=CARTESIAN_POINT('Ctrl Pts',(44.3789062499988,-1.96836574384012,
43.507944725511));
#262710=CARTESIAN_POINT('Ctrl Pts',(44.4450520833321,-1.56052008345056E-13,
43.507944725511));
#262711=CARTESIAN_POINT('Ctrl Pts',(44.5111979166654,1.96836574383981,43.507944725511));
#262712=CARTESIAN_POINT('Ctrl Pts',(44.5773437499987,3.36021050916435,44.8997894908355));
#262713=CARTESIAN_POINT('Ctrl Pts',(44.643489583332,4.75205527448889,46.29163425616));
#262714=CARTESIAN_POINT('Ctrl Pts',(44.7096354166654,4.75205527448889,48.26));
#262715=CARTESIAN_POINT('Ctrl Pts',(44.7757812499987,4.75205527448889,50.22836574384));
#262716=CARTESIAN_POINT('Ctrl Pts',(44.841927083332,3.36021050916435,51.6202105091645));
#262717=CARTESIAN_POINT('Ctrl Pts',(44.9080729166653,1.96836574383981,53.0120552744891));
#262718=CARTESIAN_POINT('Ctrl Pts',(44.9742187499986,-1.56735666030605E-13,
53.012055274489));
#262719=CARTESIAN_POINT('Ctrl Pts',(45.0403645833319,-1.96836574384012,
53.0120552744891));
#262720=CARTESIAN_POINT('Ctrl Pts',(45.1065104166652,-3.36021050916466,
51.6202105091645));
#262721=CARTESIAN_POINT('Ctrl Pts',(45.1726562499985,-4.7520552744892,50.22836574384));
#262722=CARTESIAN_POINT('Ctrl Pts',(45.2388020833318,-4.7520552744892,48.26));
#262723=CARTESIAN_POINT('Ctrl Pts',(45.3049479166651,-4.75205527448921,
46.29163425616));
#262724=CARTESIAN_POINT('Ctrl Pts',(45.3710937499985,-3.36021050916466,
44.8997894908355));
#262725=CARTESIAN_POINT('Ctrl Pts',(45.4372395833318,-1.96836574384013,
43.507944725511));
#262726=CARTESIAN_POINT('Ctrl Pts',(45.5033854166651,-1.59747159428664E-13,
43.507944725511));
#262727=CARTESIAN_POINT('Ctrl Pts',(45.5695312499984,1.96836574383981,43.507944725511));
#262728=CARTESIAN_POINT('Ctrl Pts',(45.6356770833317,3.36021050916434,44.8997894908355));
#262729=CARTESIAN_POINT('Ctrl Pts',(45.701822916665,4.75205527448889,46.29163425616));
#262730=CARTESIAN_POINT('Ctrl Pts',(45.7679687499984,4.75205527448889,48.26));
#262731=CARTESIAN_POINT('Ctrl Pts',(45.8341145833317,4.75205527448889,50.22836574384));
#262732=CARTESIAN_POINT('Ctrl Pts',(45.900260416665,3.36021050916434,51.6202105091645));
#262733=CARTESIAN_POINT('Ctrl Pts',(45.9664062499983,1.9683657438398,53.0120552744891));
#262734=CARTESIAN_POINT('Ctrl Pts',(46.0325520833316,-1.60430817114213E-13,
53.012055274489));
#262735=CARTESIAN_POINT('Ctrl Pts',(46.0986979166649,-1.96836574384012,
53.0120552744891));
#262736=CARTESIAN_POINT('Ctrl Pts',(46.1648437499982,-3.36021050916467,
51.6202105091645));
#262737=CARTESIAN_POINT('Ctrl Pts',(46.2309895833315,-4.75205527448921,
50.22836574384));
#262738=CARTESIAN_POINT('Ctrl Pts',(46.2971354166648,-4.75205527448921,
48.26));
#262739=CARTESIAN_POINT('Ctrl Pts',(46.3632812499981,-4.75205527448921,
46.29163425616));
#262740=CARTESIAN_POINT('Ctrl Pts',(46.4294270833315,-3.36021050916467,
44.8997894908355));
#262741=CARTESIAN_POINT('Ctrl Pts',(46.4955729166648,-1.96836574384013,
43.507944725511));
#262742=CARTESIAN_POINT('Ctrl Pts',(46.5617187499981,-1.63442310512272E-13,
43.507944725511));
#262743=CARTESIAN_POINT('Ctrl Pts',(46.6278645833314,1.9683657438398,43.507944725511));
#262744=CARTESIAN_POINT('Ctrl Pts',(46.6940104166647,3.36021050916434,44.8997894908355));
#262745=CARTESIAN_POINT('Ctrl Pts',(46.7601562499981,4.75205527448888,46.29163425616));
#262746=CARTESIAN_POINT('Ctrl Pts',(46.8263020833314,4.75205527448888,48.26));
#262747=CARTESIAN_POINT('Ctrl Pts',(46.8924479166647,4.75205527448888,50.22836574384));
#262748=CARTESIAN_POINT('Ctrl Pts',(46.958593749998,3.36021050916434,51.6202105091645));
#262749=CARTESIAN_POINT('Ctrl Pts',(47.0247395833313,1.9683657438398,53.0120552744891));
#262750=CARTESIAN_POINT('Ctrl Pts',(47.0908854166646,-1.64125968197821E-13,
53.012055274489));
#262751=CARTESIAN_POINT('Ctrl Pts',(47.1570312499979,-1.96836574384013,
53.0120552744891));
#262752=CARTESIAN_POINT('Ctrl Pts',(47.2231770833312,-3.36021050916467,
51.6202105091645));
#262753=CARTESIAN_POINT('Ctrl Pts',(47.2893229166645,-4.75205527448921,
50.22836574384));
#262754=CARTESIAN_POINT('Ctrl Pts',(47.3554687499978,-4.75205527448921,
48.26));
#262755=CARTESIAN_POINT('Ctrl Pts',(47.4216145833312,-4.75205527448921,
46.29163425616));
#262756=CARTESIAN_POINT('Ctrl Pts',(47.4877604166645,-3.36021050916467,
44.8997894908355));
#262757=CARTESIAN_POINT('Ctrl Pts',(47.5539062499978,-1.96836574384013,
43.507944725511));
#262758=CARTESIAN_POINT('Ctrl Pts',(47.6200520833311,-1.6713746159588E-13,
43.507944725511));
#262759=CARTESIAN_POINT('Ctrl Pts',(47.6861979166644,1.9683657438398,43.507944725511));
#262760=CARTESIAN_POINT('Ctrl Pts',(47.7523437499977,3.36021050916434,44.8997894908355));
#262761=CARTESIAN_POINT('Ctrl Pts',(47.818489583331,4.75205527448888,46.29163425616));
#262762=CARTESIAN_POINT('Ctrl Pts',(47.8846354166644,4.75205527448888,48.26));
#262763=CARTESIAN_POINT('Ctrl Pts',(47.9507812499977,4.75205527448888,50.22836574384));
#262764=CARTESIAN_POINT('Ctrl Pts',(48.016927083331,3.36021050916434,51.6202105091645));
#262765=CARTESIAN_POINT('Ctrl Pts',(48.0830729166643,1.9683657438398,53.0120552744891));
#262766=CARTESIAN_POINT('Ctrl Pts',(48.1492187499976,-1.67821119281429E-13,
53.012055274489));
#262767=CARTESIAN_POINT('Ctrl Pts',(48.2153645833309,-1.96836574384013,
53.0120552744891));
#262768=CARTESIAN_POINT('Ctrl Pts',(48.2815104166642,-3.36021050916467,
51.6202105091645));
#262769=CARTESIAN_POINT('Ctrl Pts',(48.3476562499975,-4.75205527448922,
50.22836574384));
#262770=CARTESIAN_POINT('Ctrl Pts',(48.4138020833308,-4.75205527448921,
48.26));
#262771=CARTESIAN_POINT('Ctrl Pts',(48.4799479166642,-4.75205527448922,
46.29163425616));
#262772=CARTESIAN_POINT('Ctrl Pts',(48.5460937499975,-3.36021050916468,
44.8997894908355));
#262773=CARTESIAN_POINT('Ctrl Pts',(48.6122395833308,-1.96836574384014,
43.507944725511));
#262774=CARTESIAN_POINT('Ctrl Pts',(48.6783854166641,-1.70832612679488E-13,
43.507944725511));
#262775=CARTESIAN_POINT('Ctrl Pts',(48.7445312499974,1.96836574383979,43.507944725511));
#262776=CARTESIAN_POINT('Ctrl Pts',(48.8106770833307,3.36021050916433,44.8997894908355));
#262777=CARTESIAN_POINT('Ctrl Pts',(48.876822916664,4.75205527448887,46.29163425616));
#262778=CARTESIAN_POINT('Ctrl Pts',(48.9429687499974,4.75205527448887,48.26));
#262779=CARTESIAN_POINT('Ctrl Pts',(49.0091145833307,4.75205527448887,50.22836574384));
#262780=CARTESIAN_POINT('Ctrl Pts',(49.075260416664,3.36021050916433,51.6202105091645));
#262781=CARTESIAN_POINT('Ctrl Pts',(49.1414062499973,1.96836574383979,53.0120552744891));
#262782=CARTESIAN_POINT('Ctrl Pts',(49.2075520833306,-1.71516270365037E-13,
53.012055274489));
#262783=CARTESIAN_POINT('Ctrl Pts',(49.2736979166639,-1.96836574384014,
53.0120552744891));
#262784=CARTESIAN_POINT('Ctrl Pts',(49.3398437499972,-3.36021050916468,
51.6202105091645));
#262785=CARTESIAN_POINT('Ctrl Pts',(49.4059895833305,-4.75205527448922,
50.22836574384));
#262786=CARTESIAN_POINT('Ctrl Pts',(49.4721354166638,-4.75205527448922,
48.26));
#262787=CARTESIAN_POINT('Ctrl Pts',(49.5382812499972,-4.75205527448922,
46.29163425616));
#262788=CARTESIAN_POINT('Ctrl Pts',(49.6044270833305,-3.36021050916468,
44.8997894908355));
#262789=CARTESIAN_POINT('Ctrl Pts',(49.6705729166638,-1.96836574384014,
43.507944725511));
#262790=CARTESIAN_POINT('Ctrl Pts',(49.7367187499971,-1.74527763763095E-13,
43.507944725511));
#262791=CARTESIAN_POINT('Ctrl Pts',(49.8028645833304,1.96836574383979,43.507944725511));
#262792=CARTESIAN_POINT('Ctrl Pts',(49.8690104166637,3.36021050916433,44.8997894908355));
#262793=CARTESIAN_POINT('Ctrl Pts',(49.935156249997,4.75205527448887,46.29163425616));
#262794=CARTESIAN_POINT('Ctrl Pts',(50.0013020833304,4.75205527448887,48.26));
#262795=CARTESIAN_POINT('Ctrl Pts',(50.0674479166637,4.75205527448887,50.22836574384));
#262796=CARTESIAN_POINT('Ctrl Pts',(50.133593749997,3.36021050916433,51.6202105091645));
#262797=CARTESIAN_POINT('Ctrl Pts',(50.1997395833303,1.96836574383979,53.0120552744891));
#262798=CARTESIAN_POINT('Ctrl Pts',(50.2658854166636,-1.75211421448644E-13,
53.012055274489));
#262799=CARTESIAN_POINT('Ctrl Pts',(50.3320312499969,-1.96836574384014,
53.0120552744891));
#262800=CARTESIAN_POINT('Ctrl Pts',(50.3981770833302,-3.36021050916468,
51.6202105091645));
#262801=CARTESIAN_POINT('Ctrl Pts',(50.4643229166635,-4.75205527448922,
50.22836574384));
#262802=CARTESIAN_POINT('Ctrl Pts',(50.5304687499968,-4.75205527448922,
48.26));
#262803=CARTESIAN_POINT('Ctrl Pts',(50.5966145833301,-4.75205527448922,
46.29163425616));
#262804=CARTESIAN_POINT('Ctrl Pts',(50.6627604166635,-3.36021050916468,
44.8997894908355));
#262805=CARTESIAN_POINT('Ctrl Pts',(50.7289062499968,-1.96836574384014,
43.507944725511));
#262806=CARTESIAN_POINT('Ctrl Pts',(50.7950520833301,-1.78222914846703E-13,
43.507944725511));
#262807=CARTESIAN_POINT('Ctrl Pts',(50.8611979166634,1.96836574383979,43.507944725511));
#262808=CARTESIAN_POINT('Ctrl Pts',(50.9273437499967,3.36021050916433,44.8997894908355));
#262809=CARTESIAN_POINT('Ctrl Pts',(50.99348958333,4.75205527448887,46.29163425616));
#262810=CARTESIAN_POINT('Ctrl Pts',(51.0596354166634,4.75205527448887,48.26));
#262811=CARTESIAN_POINT('Ctrl Pts',(42.0671867061318,-4.68628896694512,
47.6743911597878));
#262812=CARTESIAN_POINT('Ctrl Pts',(42.1243724082372,-4.48534984498616,
46.0663915436572));
#262813=CARTESIAN_POINT('Ctrl Pts',(42.1791666666662,-3.33947915066458,
44.9205208493356));
#262814=CARTESIAN_POINT('Ctrl Pts',(42.2453124999995,-1.95622159519719,
43.5372632938682));
#262815=CARTESIAN_POINT('Ctrl Pts',(42.3114583333328,-1.48597219848627E-13,
43.5372632938682));
#262816=CARTESIAN_POINT('Ctrl Pts',(42.3776041666661,1.95622159519689,43.5372632938682));
#262817=CARTESIAN_POINT('Ctrl Pts',(42.4437499999994,3.33947915066428,44.9205208493356));
#262818=CARTESIAN_POINT('Ctrl Pts',(42.5098958333328,4.72273670613168,46.303778404803));
#262819=CARTESIAN_POINT('Ctrl Pts',(42.5760416666661,4.72273670613168,48.26));
#262820=CARTESIAN_POINT('Ctrl Pts',(42.6421874999994,4.72273670613168,50.216221595197));
#262821=CARTESIAN_POINT('Ctrl Pts',(42.7083333333327,3.33947915066428,51.5994791506644));
#262822=CARTESIAN_POINT('Ctrl Pts',(42.774479166666,1.95622159519689,52.9827367061318));
#262823=CARTESIAN_POINT('Ctrl Pts',(42.8406249999993,-1.49288058512355E-13,
52.9827367061318));
#262824=CARTESIAN_POINT('Ctrl Pts',(42.9067708333326,-1.95622159519719,
52.9827367061318));
#262825=CARTESIAN_POINT('Ctrl Pts',(42.9729166666659,-3.33947915066458,
51.5994791506644));
#262826=CARTESIAN_POINT('Ctrl Pts',(43.0390624999992,-4.72273670613198,
50.216221595197));
#262827=CARTESIAN_POINT('Ctrl Pts',(43.1052083333325,-4.72273670613198,
48.26));
#262828=CARTESIAN_POINT('Origin',(40.4567708333334,-1.14908083048704E-13,
48.26));
#262829=CARTESIAN_POINT('Ctrl Pts',(42.0671867061318,-4.66579641623079,
47.5288462557477));
#262830=CARTESIAN_POINT('Ctrl Pts',(42.1219271548081,-4.4275676543112,46.0086093529822));
#262831=CARTESIAN_POINT('Ctrl Pts',(42.1739583333328,-3.33947915066458,
44.9205208493356));
#262832=CARTESIAN_POINT('Ctrl Pts',(42.2401041666661,-1.95622159519719,
43.5372632938682));
#262833=CARTESIAN_POINT('Ctrl Pts',(42.3062499999994,-1.48579035049987E-13,
43.5372632938682));
#262834=CARTESIAN_POINT('Ctrl Pts',(42.3723958333328,1.95622159519689,43.5372632938682));
#262835=CARTESIAN_POINT('Ctrl Pts',(42.4385416666661,3.33947915066428,44.9205208493356));
#262836=CARTESIAN_POINT('Ctrl Pts',(42.5046874999994,4.72273670613168,46.303778404803));
#262837=CARTESIAN_POINT('Ctrl Pts',(42.5708333333327,4.72273670613168,48.26));
#262838=CARTESIAN_POINT('Ctrl Pts',(42.636979166666,4.72273670613168,50.216221595197));
#262839=CARTESIAN_POINT('Ctrl Pts',(42.7031249999993,3.33947915066428,51.5994791506644));
#262840=CARTESIAN_POINT('Ctrl Pts',(42.7692708333326,1.95622159519689,52.9827367061318));
#262841=CARTESIAN_POINT('Ctrl Pts',(42.8354166666659,-1.49269873713715E-13,
52.9827367061318));
#262842=CARTESIAN_POINT('Ctrl Pts',(42.9015624999992,-1.95622159519719,
52.9827367061318));
#262843=CARTESIAN_POINT('Ctrl Pts',(42.9677083333325,-3.33947915066458,
51.5994791506644));
#262844=CARTESIAN_POINT('Ctrl Pts',(43.0338541666658,-4.72273670613198,
50.216221595197));
#262845=CARTESIAN_POINT('Ctrl Pts',(43.0999999999992,-4.72273670613198,
48.26));
#262846=CARTESIAN_POINT('Ctrl Pts',(40.4372395833334,4.75205527448891,48.26));
#262847=CARTESIAN_POINT('Ctrl Pts',(40.5033854166667,4.75205527448891,50.22836574384));
#262848=CARTESIAN_POINT('Ctrl Pts',(40.56953125,3.36021050916437,51.6202105091645));
#262849=CARTESIAN_POINT('Ctrl Pts',(40.6356770833333,1.96836574383982,53.0120552744891));
#262850=CARTESIAN_POINT('Ctrl Pts',(40.7018229166666,-1.41818675706376E-13,
53.012055274489));
#262851=CARTESIAN_POINT('Ctrl Pts',(40.7679687499999,-1.96836574384011,
53.0120552744891));
#262852=CARTESIAN_POINT('Ctrl Pts',(40.8341145833332,-3.36021050916465,
51.6202105091645));
#262853=CARTESIAN_POINT('Ctrl Pts',(40.9002604166665,-4.75205527448919,
50.22836574384));
#262854=CARTESIAN_POINT('Ctrl Pts',(40.9664062499999,-4.75205527448919,
48.26));
#262855=CARTESIAN_POINT('Ctrl Pts',(41.0325520833332,-4.75205527448919,
46.29163425616));
#262856=CARTESIAN_POINT('Ctrl Pts',(41.0986979166665,-3.36021050916465,
44.8997894908355));
#262857=CARTESIAN_POINT('Ctrl Pts',(41.1648437499998,-1.96836574384011,
43.507944725511));
#262858=CARTESIAN_POINT('Ctrl Pts',(41.2309895833331,-1.44830169104434E-13,
43.507944725511));
#262859=CARTESIAN_POINT('Ctrl Pts',(41.2971354166664,1.96836574383982,43.507944725511));
#262860=CARTESIAN_POINT('Ctrl Pts',(41.3632812499998,3.36021050916436,44.8997894908355));
#262861=CARTESIAN_POINT('Ctrl Pts',(41.4294270833331,4.7520552744889,46.29163425616));
#262862=CARTESIAN_POINT('Ctrl Pts',(41.4955729166664,4.7520552744889,48.26));
#262863=CARTESIAN_POINT('Ctrl Pts',(41.5617187499997,4.7520552744889,50.22836574384));
#262864=CARTESIAN_POINT('Ctrl Pts',(41.627864583333,3.36021050916436,51.6202105091645));
#262865=CARTESIAN_POINT('Ctrl Pts',(41.6940104166663,1.96836574383982,53.0120552744891));
#262866=CARTESIAN_POINT('Ctrl Pts',(41.7601562499996,-1.45513826789983E-13,
53.012055274489));
#262867=CARTESIAN_POINT('Ctrl Pts',(41.8263020833329,-1.96836574384011,
53.0120552744891));
#262868=CARTESIAN_POINT('Ctrl Pts',(41.8924479166662,-3.36021050916465,
51.6202105091645));
#262869=CARTESIAN_POINT('Ctrl Pts',(41.9585937499996,-4.7520552744892,50.22836574384));
#262870=CARTESIAN_POINT('Ctrl Pts',(42.0247395833329,-4.7520552744892,48.26));
#262871=CARTESIAN_POINT('Ctrl Pts',(42.0908854166662,-4.7520552744892,46.29163425616));
#262872=CARTESIAN_POINT('Ctrl Pts',(42.1570312499995,-3.36021050916466,
44.8997894908355));
#262873=CARTESIAN_POINT('Ctrl Pts',(42.2231770833328,-1.96836574384011,
43.507944725511));
#262874=CARTESIAN_POINT('Ctrl Pts',(42.2893229166661,-1.48525320188042E-13,
43.507944725511));
#262875=CARTESIAN_POINT('Ctrl Pts',(42.3554687499994,1.96836574383982,43.507944725511));
#262876=CARTESIAN_POINT('Ctrl Pts',(42.4216145833328,3.36021050916436,44.8997894908355));
#262877=CARTESIAN_POINT('Ctrl Pts',(42.4877604166661,4.7520552744889,46.29163425616));
#262878=CARTESIAN_POINT('Ctrl Pts',(42.5539062499994,4.7520552744889,48.26));
#262879=CARTESIAN_POINT('Ctrl Pts',(42.6200520833327,4.7520552744889,50.22836574384));
#262880=CARTESIAN_POINT('Ctrl Pts',(42.686197916666,3.36021050916436,51.6202105091645));
#262881=CARTESIAN_POINT('Ctrl Pts',(42.7523437499993,1.96836574383982,53.0120552744891));
#262882=CARTESIAN_POINT('Ctrl Pts',(42.8184895833326,-1.49208977873591E-13,
53.012055274489));
#262883=CARTESIAN_POINT('Ctrl Pts',(42.8846354166659,-1.96836574384011,
53.0120552744891));
#262884=CARTESIAN_POINT('Ctrl Pts',(42.9507812499992,-3.36021050916466,
51.6202105091645));
#262885=CARTESIAN_POINT('Ctrl Pts',(43.0169270833326,-4.7520552744892,50.22836574384));
#262886=CARTESIAN_POINT('Ctrl Pts',(43.0830729166659,-4.7520552744892,48.26));
#262887=CARTESIAN_POINT('Ctrl Pts',(43.1492187499992,-4.7520552744892,46.29163425616));
#262888=CARTESIAN_POINT('Ctrl Pts',(43.2153645833325,-3.36021050916466,
44.8997894908355));
#262889=CARTESIAN_POINT('Ctrl Pts',(43.2815104166658,-1.96836574384012,
43.507944725511));
#262890=CARTESIAN_POINT('Ctrl Pts',(43.3476562499991,-1.5222047127165E-13,
43.507944725511));
#262891=CARTESIAN_POINT('Ctrl Pts',(43.4138020833324,1.96836574383981,43.507944725511));
#262892=CARTESIAN_POINT('Ctrl Pts',(43.4799479166658,3.36021050916435,44.8997894908355));
#262893=CARTESIAN_POINT('Ctrl Pts',(43.5460937499991,4.7520552744889,46.29163425616));
#262894=CARTESIAN_POINT('Ctrl Pts',(43.6122395833324,4.7520552744889,48.26));
#262895=CARTESIAN_POINT('Ctrl Pts',(43.6783854166657,4.7520552744889,50.22836574384));
#262896=CARTESIAN_POINT('Ctrl Pts',(43.744531249999,3.36021050916435,51.6202105091645));
#262897=CARTESIAN_POINT('Ctrl Pts',(43.8106770833323,1.96836574383981,53.0120552744891));
#262898=CARTESIAN_POINT('Ctrl Pts',(43.8768229166656,-1.52904128957199E-13,
53.012055274489));
#262899=CARTESIAN_POINT('Ctrl Pts',(43.9429687499989,-1.96836574384012,
53.0120552744891));
#262900=CARTESIAN_POINT('Ctrl Pts',(44.0091145833323,-3.36021050916466,
51.6202105091645));
#262901=CARTESIAN_POINT('Ctrl Pts',(44.0752604166656,-4.7520552744892,50.22836574384));
#262902=CARTESIAN_POINT('Ctrl Pts',(44.1414062499989,-4.7520552744892,48.26));
#262903=CARTESIAN_POINT('Ctrl Pts',(44.2075520833322,-4.75205527448921,
46.29163425616));
#262904=CARTESIAN_POINT('Ctrl Pts',(44.2736979166655,-3.36021050916466,
44.8997894908355));
#262905=CARTESIAN_POINT('Ctrl Pts',(44.3398437499988,-1.96836574384012,
43.507944725511));
#262906=CARTESIAN_POINT('Ctrl Pts',(44.4059895833321,-1.55915622355258E-13,
43.507944725511));
#262907=CARTESIAN_POINT('Ctrl Pts',(44.4721354166655,1.96836574383981,43.507944725511));
#262908=CARTESIAN_POINT('Ctrl Pts',(44.5382812499988,3.36021050916435,44.8997894908355));
#262909=CARTESIAN_POINT('Ctrl Pts',(44.6044270833321,4.75205527448889,46.29163425616));
#262910=CARTESIAN_POINT('Ctrl Pts',(44.6705729166654,4.75205527448889,48.26));
#262911=CARTESIAN_POINT('Ctrl Pts',(44.7367187499987,4.75205527448889,50.22836574384));
#262912=CARTESIAN_POINT('Ctrl Pts',(44.802864583332,3.36021050916435,51.6202105091645));
#262913=CARTESIAN_POINT('Ctrl Pts',(44.8690104166653,1.96836574383981,53.0120552744891));
#262914=CARTESIAN_POINT('Ctrl Pts',(44.9351562499986,-1.56599280040807E-13,
53.012055274489));
#262915=CARTESIAN_POINT('Ctrl Pts',(45.001302083332,-1.96836574384012,53.0120552744891));
#262916=CARTESIAN_POINT('Ctrl Pts',(45.0674479166652,-3.36021050916466,
51.6202105091645));
#262917=CARTESIAN_POINT('Ctrl Pts',(45.1335937499986,-4.75205527448921,
50.22836574384));
#262918=CARTESIAN_POINT('Ctrl Pts',(45.1997395833319,-4.75205527448921,
48.26));
#262919=CARTESIAN_POINT('Ctrl Pts',(45.2658854166652,-4.75205527448921,
46.29163425616));
#262920=CARTESIAN_POINT('Ctrl Pts',(45.3320312499985,-3.36021050916467,
44.8997894908355));
#262921=CARTESIAN_POINT('Ctrl Pts',(45.3981770833318,-1.96836574384013,
43.507944725511));
#262922=CARTESIAN_POINT('Ctrl Pts',(45.4643229166651,-1.59610773438866E-13,
43.507944725511));
#262923=CARTESIAN_POINT('Ctrl Pts',(45.5304687499984,1.96836574383981,43.507944725511));
#262924=CARTESIAN_POINT('Ctrl Pts',(45.5966145833318,3.36021050916435,44.8997894908355));
#262925=CARTESIAN_POINT('Ctrl Pts',(45.6627604166651,4.75205527448889,46.29163425616));
#262926=CARTESIAN_POINT('Ctrl Pts',(45.7289062499984,4.75205527448889,48.26));
#262927=CARTESIAN_POINT('Ctrl Pts',(45.7950520833317,4.75205527448889,50.22836574384));
#262928=CARTESIAN_POINT('Ctrl Pts',(45.861197916665,3.36021050916435,51.6202105091645));
#262929=CARTESIAN_POINT('Ctrl Pts',(45.9273437499983,1.96836574383981,53.0120552744891));
#262930=CARTESIAN_POINT('Ctrl Pts',(45.9934895833316,-1.60294431124415E-13,
53.012055274489));
#262931=CARTESIAN_POINT('Ctrl Pts',(46.0596354166649,-1.96836574384013,
53.0120552744891));
#262932=CARTESIAN_POINT('Ctrl Pts',(46.1257812499982,-3.36021050916467,
51.6202105091645));
#262933=CARTESIAN_POINT('Ctrl Pts',(46.1919270833316,-4.75205527448921,
50.22836574384));
#262934=CARTESIAN_POINT('Ctrl Pts',(46.2580729166649,-4.75205527448921,
48.26));
#262935=CARTESIAN_POINT('Ctrl Pts',(46.3242187499982,-4.75205527448921,
46.29163425616));
#262936=CARTESIAN_POINT('Ctrl Pts',(46.3903645833315,-3.36021050916467,
44.8997894908355));
#262937=CARTESIAN_POINT('Ctrl Pts',(46.4565104166648,-1.96836574384013,
43.507944725511));
#262938=CARTESIAN_POINT('Ctrl Pts',(46.5226562499981,-1.63305924522473E-13,
43.507944725511));
#262939=CARTESIAN_POINT('Ctrl Pts',(46.5888020833314,1.9683657438398,43.507944725511));
#262940=CARTESIAN_POINT('Ctrl Pts',(46.6549479166648,3.36021050916434,44.8997894908355));
#262941=CARTESIAN_POINT('Ctrl Pts',(46.7210937499981,4.75205527448889,46.29163425616));
#262942=CARTESIAN_POINT('Ctrl Pts',(46.7872395833314,4.75205527448888,48.26));
#262943=CARTESIAN_POINT('Ctrl Pts',(46.8533854166647,4.75205527448889,50.22836574384));
#262944=CARTESIAN_POINT('Ctrl Pts',(46.919531249998,3.36021050916434,51.6202105091645));
#262945=CARTESIAN_POINT('Ctrl Pts',(46.9856770833313,1.9683657438398,53.0120552744891));
#262946=CARTESIAN_POINT('Ctrl Pts',(47.0518229166646,-1.63989582208022E-13,
53.012055274489));
#262947=CARTESIAN_POINT('Ctrl Pts',(47.1179687499979,-1.96836574384013,
53.0120552744891));
#262948=CARTESIAN_POINT('Ctrl Pts',(47.1841145833313,-3.36021050916467,
51.6202105091645));
#262949=CARTESIAN_POINT('Ctrl Pts',(47.2502604166646,-4.75205527448921,
50.22836574384));
#262950=CARTESIAN_POINT('Ctrl Pts',(47.3164062499979,-4.75205527448921,
48.26));
#262951=CARTESIAN_POINT('Ctrl Pts',(47.3825520833312,-4.75205527448922,
46.29163425616));
#262952=CARTESIAN_POINT('Ctrl Pts',(47.4486979166645,-3.36021050916467,
44.8997894908355));
#262953=CARTESIAN_POINT('Ctrl Pts',(47.5148437499978,-1.96836574384013,
43.507944725511));
#262954=CARTESIAN_POINT('Ctrl Pts',(47.5809895833311,-1.67001075606081E-13,
43.507944725511));
#262955=CARTESIAN_POINT('Ctrl Pts',(47.6471354166645,1.9683657438398,43.507944725511));
#262956=CARTESIAN_POINT('Ctrl Pts',(47.7132812499978,3.36021050916434,44.8997894908355));
#262957=CARTESIAN_POINT('Ctrl Pts',(47.7794270833311,4.75205527448888,46.29163425616));
#262958=CARTESIAN_POINT('Ctrl Pts',(47.8455729166644,4.75205527448888,48.26));
#262959=CARTESIAN_POINT('Ctrl Pts',(47.9117187499977,4.75205527448888,50.22836574384));
#262960=CARTESIAN_POINT('Ctrl Pts',(47.977864583331,3.36021050916434,51.6202105091645));
#262961=CARTESIAN_POINT('Ctrl Pts',(48.0440104166643,1.9683657438398,53.0120552744891));
#262962=CARTESIAN_POINT('Ctrl Pts',(48.1101562499976,-1.6768473329163E-13,
53.012055274489));
#262963=CARTESIAN_POINT('Ctrl Pts',(48.1763020833309,-1.96836574384013,
53.0120552744891));
#262964=CARTESIAN_POINT('Ctrl Pts',(48.2424479166642,-3.36021050916468,
51.6202105091645));
#262965=CARTESIAN_POINT('Ctrl Pts',(48.3085937499975,-4.75205527448922,
50.22836574384));
#262966=CARTESIAN_POINT('Ctrl Pts',(48.3747395833309,-4.75205527448922,
48.26));
#262967=CARTESIAN_POINT('Ctrl Pts',(48.4408854166642,-4.75205527448922,
46.29163425616));
#262968=CARTESIAN_POINT('Ctrl Pts',(48.5070312499975,-3.36021050916468,
44.8997894908355));
#262969=CARTESIAN_POINT('Ctrl Pts',(48.5731770833308,-1.96836574384014,
43.507944725511));
#262970=CARTESIAN_POINT('Ctrl Pts',(48.6393229166641,-1.70696226689689E-13,
43.507944725511));
#262971=CARTESIAN_POINT('Ctrl Pts',(48.7054687499974,1.9683657438398,43.507944725511));
#262972=CARTESIAN_POINT('Ctrl Pts',(48.7716145833308,3.36021050916434,44.8997894908355));
#262973=CARTESIAN_POINT('Ctrl Pts',(48.8377604166641,4.75205527448888,46.29163425616));
#262974=CARTESIAN_POINT('Ctrl Pts',(48.9039062499974,4.75205527448888,48.26));
#262975=CARTESIAN_POINT('Ctrl Pts',(48.9700520833307,4.75205527448888,50.22836574384));
#262976=CARTESIAN_POINT('Ctrl Pts',(49.036197916664,3.36021050916434,51.6202105091645));
#262977=CARTESIAN_POINT('Ctrl Pts',(49.1023437499973,1.96836574383979,53.0120552744891));
#262978=CARTESIAN_POINT('Ctrl Pts',(49.1684895833306,-1.71379884375238E-13,
53.012055274489));
#262979=CARTESIAN_POINT('Ctrl Pts',(49.2346354166639,-1.96836574384014,
53.0120552744891));
#262980=CARTESIAN_POINT('Ctrl Pts',(49.3007812499973,-3.36021050916468,
51.6202105091645));
#262981=CARTESIAN_POINT('Ctrl Pts',(49.3669270833306,-4.75205527448922,
50.22836574384));
#262982=CARTESIAN_POINT('Ctrl Pts',(49.4330729166639,-4.75205527448922,
48.26));
#262983=CARTESIAN_POINT('Ctrl Pts',(49.4992187499972,-4.75205527448922,
46.29163425616));
#262984=CARTESIAN_POINT('Ctrl Pts',(49.5653645833305,-3.36021050916468,
44.8997894908355));
#262985=CARTESIAN_POINT('Ctrl Pts',(49.6315104166638,-1.96836574384014,
43.507944725511));
#262986=CARTESIAN_POINT('Ctrl Pts',(49.6976562499971,-1.74391377773297E-13,
43.507944725511));
#262987=CARTESIAN_POINT('Ctrl Pts',(49.7638020833305,1.96836574383979,43.507944725511));
#262988=CARTESIAN_POINT('Ctrl Pts',(49.8299479166638,3.36021050916433,44.8997894908355));
#262989=CARTESIAN_POINT('Ctrl Pts',(49.8960937499971,4.75205527448887,46.29163425616));
#262990=CARTESIAN_POINT('Ctrl Pts',(49.9622395833304,4.75205527448887,48.26));
#262991=CARTESIAN_POINT('Ctrl Pts',(50.0283854166637,4.75205527448887,50.22836574384));
#262992=CARTESIAN_POINT('Ctrl Pts',(50.094531249997,3.36021050916433,51.6202105091645));
#262993=CARTESIAN_POINT('Ctrl Pts',(50.1606770833303,1.96836574383979,53.0120552744891));
#262994=CARTESIAN_POINT('Ctrl Pts',(50.2268229166636,-1.75075035458846E-13,
53.012055274489));
#262995=CARTESIAN_POINT('Ctrl Pts',(50.2929687499969,-1.96836574384014,
53.0120552744891));
#262996=CARTESIAN_POINT('Ctrl Pts',(50.3591145833302,-3.36021050916468,
51.6202105091645));
#262997=CARTESIAN_POINT('Ctrl Pts',(50.4252604166636,-4.75205527448922,
50.22836574384));
#262998=CARTESIAN_POINT('Ctrl Pts',(50.4914062499969,-4.75205527448922,
48.26));
#262999=CARTESIAN_POINT('Ctrl Pts',(50.5575520833302,-4.75205527448923,
46.29163425616));
#263000=CARTESIAN_POINT('Ctrl Pts',(50.6236979166635,-3.36021050916468,
44.8997894908355));
#263001=CARTESIAN_POINT('Ctrl Pts',(50.6898437499968,-1.96836574384015,
43.507944725511));
#263002=CARTESIAN_POINT('Ctrl Pts',(50.7559895833301,-1.78086528856905E-13,
43.507944725511));
#263003=CARTESIAN_POINT('Ctrl Pts',(50.8221354166634,1.96836574383979,43.507944725511));
#263004=CARTESIAN_POINT('Ctrl Pts',(50.8882812499968,3.36021050916433,44.8997894908355));
#263005=CARTESIAN_POINT('Ctrl Pts',(50.9544270833301,4.75205527448887,46.29163425616));
#263006=CARTESIAN_POINT('Ctrl Pts',(51.0205729166634,4.75205527448887,48.26));
#263007=CARTESIAN_POINT('Ctrl Pts',(40.4541666666667,4.72273670613168,48.26));
#263008=CARTESIAN_POINT('Ctrl Pts',(40.5203125,4.72273670613168,50.216221595197));
#263009=CARTESIAN_POINT('Ctrl Pts',(40.5864583333333,3.33947915066429,51.5994791506644));
#263010=CARTESIAN_POINT('Ctrl Pts',(40.6526041666666,1.9562215951969,52.9827367061318));
#263011=CARTESIAN_POINT('Ctrl Pts',(40.7187499999999,-1.418795715465E-13,
52.9827367061318));
#263012=CARTESIAN_POINT('Ctrl Pts',(40.7848958333332,-1.95622159519718,
52.9827367061318));
#263013=CARTESIAN_POINT('Ctrl Pts',(40.8510416666665,-3.33947915066458,
51.5994791506644));
#263014=CARTESIAN_POINT('Ctrl Pts',(40.9171874999998,-4.72273670613197,
50.216221595197));
#263015=CARTESIAN_POINT('Ctrl Pts',(40.9833333333332,-4.72273670613197,
48.26));
#263016=CARTESIAN_POINT('Ctrl Pts',(41.0494791666665,-4.72273670613197,
46.303778404803));
#263017=CARTESIAN_POINT('Ctrl Pts',(41.1156249999998,-3.33947915066458,
44.9205208493356));
#263018=CARTESIAN_POINT('Ctrl Pts',(41.1817708333331,-1.95622159519719,
43.5372632938682));
#263019=CARTESIAN_POINT('Ctrl Pts',(41.2479166666664,-1.44883883966379E-13,
43.5372632938682));
#263020=CARTESIAN_POINT('Ctrl Pts',(41.3140624999997,1.9562215951969,43.5372632938682));
#263021=CARTESIAN_POINT('Ctrl Pts',(41.3802083333331,3.33947915066429,44.9205208493356));
#263022=CARTESIAN_POINT('Ctrl Pts',(41.4463541666664,4.72273670613168,46.303778404803));
#263023=CARTESIAN_POINT('Ctrl Pts',(41.5124999999997,4.72273670613168,48.26));
#263024=CARTESIAN_POINT('Ctrl Pts',(41.578645833333,4.72273670613168,50.216221595197));
#263025=CARTESIAN_POINT('Ctrl Pts',(41.6447916666663,3.33947915066429,51.5994791506644));
#263026=CARTESIAN_POINT('Ctrl Pts',(41.7109374999996,1.9562215951969,52.9827367061318));
#263027=CARTESIAN_POINT('Ctrl Pts',(41.7770833333329,-1.45574722630107E-13,
52.9827367061318));
#263028=CARTESIAN_POINT('Ctrl Pts',(41.8432291666662,-1.95622159519719,
52.9827367061318));
#263029=CARTESIAN_POINT('Ctrl Pts',(41.9093749999995,-3.33947915066458,
51.5994791506644));
#263030=CARTESIAN_POINT('Ctrl Pts',(41.9755208333328,-4.72273670613197,
50.216221595197));
#263031=CARTESIAN_POINT('Ctrl Pts',(42.0416666666662,-4.72273670613197,
48.26));
#263032=CARTESIAN_POINT('Ctrl Pts',(42.1078124999995,-4.72273670613197,
46.303778404803));
#263033=CARTESIAN_POINT('Ctrl Pts',(42.1739583333328,-3.33947915066458,
44.9205208493356));
#263034=CARTESIAN_POINT('Ctrl Pts',(42.2401041666661,-1.95622159519719,
43.5372632938682));
#263035=CARTESIAN_POINT('Ctrl Pts',(42.3062499999994,-1.48579035049987E-13,
43.5372632938682));
#263036=CARTESIAN_POINT('Ctrl Pts',(42.3723958333328,1.95622159519689,43.5372632938682));
#263037=CARTESIAN_POINT('Ctrl Pts',(42.4385416666661,3.33947915066428,44.9205208493356));
#263038=CARTESIAN_POINT('Ctrl Pts',(42.5046874999994,4.72273670613168,46.303778404803));
#263039=CARTESIAN_POINT('Ctrl Pts',(42.5708333333327,4.72273670613168,48.26));
#263040=CARTESIAN_POINT('Ctrl Pts',(42.636979166666,4.72273670613168,50.216221595197));
#263041=CARTESIAN_POINT('Ctrl Pts',(42.7031249999993,3.33947915066428,51.5994791506644));
#263042=CARTESIAN_POINT('Ctrl Pts',(42.7692708333326,1.95622159519689,52.9827367061318));
#263043=CARTESIAN_POINT('Ctrl Pts',(42.8354166666659,-1.49269873713715E-13,
52.9827367061318));
#263044=CARTESIAN_POINT('Ctrl Pts',(42.9015624999992,-1.95622159519719,
52.9827367061318));
#263045=CARTESIAN_POINT('Ctrl Pts',(42.9677083333325,-3.33947915066458,
51.5994791506644));
#263046=CARTESIAN_POINT('Ctrl Pts',(43.0338541666658,-4.72273670613198,
50.216221595197));
#263047=CARTESIAN_POINT('Ctrl Pts',(43.0999999999992,-4.72273670613198,
48.26));
#263048=CARTESIAN_POINT('Ctrl Pts',(43.1661458333325,-4.72273670613198,
46.303778404803));
#263049=CARTESIAN_POINT('Ctrl Pts',(43.2322916666658,-3.33947915066458,
44.9205208493356));
#263050=CARTESIAN_POINT('Ctrl Pts',(43.2984374999991,-1.95622159519719,
43.5372632938682));
#263051=CARTESIAN_POINT('Ctrl Pts',(43.3645833333324,-1.52274186133595E-13,
43.5372632938682));
#263052=CARTESIAN_POINT('Ctrl Pts',(43.4307291666657,1.95622159519689,43.5372632938682));
#263053=CARTESIAN_POINT('Ctrl Pts',(43.4968749999991,3.33947915066428,44.9205208493356));
#263054=CARTESIAN_POINT('Ctrl Pts',(43.5630208333324,4.72273670613167,46.303778404803));
#263055=CARTESIAN_POINT('Ctrl Pts',(43.6291666666657,4.72273670613167,48.26));
#263056=CARTESIAN_POINT('Ctrl Pts',(43.695312499999,4.72273670613167,50.216221595197));
#263057=CARTESIAN_POINT('Ctrl Pts',(43.7614583333323,3.33947915066428,51.5994791506644));
#263058=CARTESIAN_POINT('Ctrl Pts',(43.8276041666656,1.95622159519689,52.9827367061318));
#263059=CARTESIAN_POINT('Ctrl Pts',(43.8937499999989,-1.52965024797323E-13,
52.9827367061318));
#263060=CARTESIAN_POINT('Ctrl Pts',(43.9598958333322,-1.95622159519719,
52.9827367061318));
#263061=CARTESIAN_POINT('Ctrl Pts',(44.0260416666655,-3.33947915066459,
51.5994791506644));
#263062=CARTESIAN_POINT('Ctrl Pts',(44.0921874999988,-4.72273670613198,
50.216221595197));
#263063=CARTESIAN_POINT('Ctrl Pts',(44.1583333333322,-4.72273670613198,
48.26));
#263064=CARTESIAN_POINT('Ctrl Pts',(44.2244791666655,-4.72273670613198,
46.303778404803));
#263065=CARTESIAN_POINT('Ctrl Pts',(44.2906249999988,-3.33947915066459,
44.9205208493356));
#263066=CARTESIAN_POINT('Ctrl Pts',(44.3567708333321,-1.9562215951972,43.5372632938682));
#263067=CARTESIAN_POINT('Ctrl Pts',(44.4229166666654,-1.55969337217203E-13,
43.5372632938682));
#263068=CARTESIAN_POINT('Ctrl Pts',(44.4890624999988,1.95622159519689,43.5372632938682));
#263069=CARTESIAN_POINT('Ctrl Pts',(44.5552083333321,3.33947915066428,44.9205208493356));
#263070=CARTESIAN_POINT('Ctrl Pts',(44.6213541666654,4.72273670613167,46.303778404803));
#263071=CARTESIAN_POINT('Ctrl Pts',(44.6874999999987,4.72273670613167,48.26));
#263072=CARTESIAN_POINT('Ctrl Pts',(44.753645833332,4.72273670613167,50.216221595197));
#263073=CARTESIAN_POINT('Ctrl Pts',(44.8197916666653,3.33947915066428,51.5994791506644));
#263074=CARTESIAN_POINT('Ctrl Pts',(44.8859374999986,1.95622159519688,52.9827367061318));
#263075=CARTESIAN_POINT('Ctrl Pts',(44.9520833333319,-1.56660175880931E-13,
52.9827367061318));
#263076=CARTESIAN_POINT('Ctrl Pts',(45.0182291666652,-1.9562215951972,52.9827367061318));
#263077=CARTESIAN_POINT('Ctrl Pts',(45.0843749999985,-3.33947915066459,
51.5994791506644));
#263078=CARTESIAN_POINT('Ctrl Pts',(45.1505208333318,-4.72273670613198,
50.216221595197));
#263079=CARTESIAN_POINT('Ctrl Pts',(45.2166666666652,-4.72273670613198,
48.26));
#263080=CARTESIAN_POINT('Ctrl Pts',(45.2828124999985,-4.72273670613199,
46.303778404803));
#263081=CARTESIAN_POINT('Ctrl Pts',(45.3489583333318,-3.33947915066459,
44.9205208493356));
#263082=CARTESIAN_POINT('Ctrl Pts',(45.4151041666651,-1.9562215951972,43.5372632938682));
#263083=CARTESIAN_POINT('Ctrl Pts',(45.4812499999984,-1.59664488300811E-13,
43.5372632938682));
#263084=CARTESIAN_POINT('Ctrl Pts',(45.5473958333317,1.95622159519688,43.5372632938682));
#263085=CARTESIAN_POINT('Ctrl Pts',(45.6135416666651,3.33947915066427,44.9205208493356));
#263086=CARTESIAN_POINT('Ctrl Pts',(45.6796874999984,4.72273670613167,46.303778404803));
#263087=CARTESIAN_POINT('Ctrl Pts',(45.7458333333317,4.72273670613167,48.26));
#263088=CARTESIAN_POINT('Ctrl Pts',(45.811979166665,4.72273670613167,50.216221595197));
#263089=CARTESIAN_POINT('Ctrl Pts',(45.8781249999983,3.33947915066427,51.5994791506644));
#263090=CARTESIAN_POINT('Ctrl Pts',(45.9442708333316,1.95622159519688,52.9827367061318));
#263091=CARTESIAN_POINT('Ctrl Pts',(46.0104166666649,-1.60355326964539E-13,
52.9827367061318));
#263092=CARTESIAN_POINT('Ctrl Pts',(46.0765624999982,-1.9562215951972,52.9827367061318));
#263093=CARTESIAN_POINT('Ctrl Pts',(46.1427083333315,-3.33947915066459,
51.5994791506644));
#263094=CARTESIAN_POINT('Ctrl Pts',(46.2088541666649,-4.72273670613199,
50.216221595197));
#263095=CARTESIAN_POINT('Ctrl Pts',(46.2749999999982,-4.72273670613199,
48.26));
#263096=CARTESIAN_POINT('Ctrl Pts',(46.3411458333315,-4.72273670613199,
46.303778404803));
#263097=CARTESIAN_POINT('Ctrl Pts',(46.4072916666648,-3.3394791506646,44.9205208493356));
#263098=CARTESIAN_POINT('Ctrl Pts',(46.4734374999981,-1.95622159519721,
43.5372632938682));
#263099=CARTESIAN_POINT('Ctrl Pts',(46.5395833333314,-1.63359639384419E-13,
43.5372632938682));
#263100=CARTESIAN_POINT('Ctrl Pts',(46.6057291666647,1.95622159519688,43.5372632938682));
#263101=CARTESIAN_POINT('Ctrl Pts',(46.6718749999981,3.33947915066427,44.9205208493356));
#263102=CARTESIAN_POINT('Ctrl Pts',(46.7380208333314,4.72273670613166,46.303778404803));
#263103=CARTESIAN_POINT('Ctrl Pts',(46.8041666666647,4.72273670613166,48.26));
#263104=CARTESIAN_POINT('Ctrl Pts',(46.870312499998,4.72273670613166,50.216221595197));
#263105=CARTESIAN_POINT('Ctrl Pts',(46.9364583333313,3.33947915066427,51.5994791506644));
#263106=CARTESIAN_POINT('Ctrl Pts',(47.0026041666646,1.95622159519688,52.9827367061318));
#263107=CARTESIAN_POINT('Ctrl Pts',(47.0687499999979,-1.64050478048146E-13,
52.9827367061318));
#263108=CARTESIAN_POINT('Ctrl Pts',(47.1348958333312,-1.95622159519721,
52.9827367061318));
#263109=CARTESIAN_POINT('Ctrl Pts',(47.2010416666646,-3.3394791506646,51.5994791506644));
#263110=CARTESIAN_POINT('Ctrl Pts',(47.2671874999979,-4.72273670613199,
50.216221595197));
#263111=CARTESIAN_POINT('Ctrl Pts',(47.3333333333312,-4.72273670613199,
48.26));
#263112=CARTESIAN_POINT('Ctrl Pts',(47.3994791666645,-4.72273670613199,
46.303778404803));
#263113=CARTESIAN_POINT('Ctrl Pts',(47.4656249999978,-3.3394791506646,44.9205208493356));
#263114=CARTESIAN_POINT('Ctrl Pts',(47.5317708333311,-1.95622159519721,
43.5372632938682));
#263115=CARTESIAN_POINT('Ctrl Pts',(47.5979166666644,-1.67054790468026E-13,
43.5372632938682));
#263116=CARTESIAN_POINT('Ctrl Pts',(47.6640624999977,1.95622159519688,43.5372632938682));
#263117=CARTESIAN_POINT('Ctrl Pts',(47.7302083333311,3.33947915066426,44.9205208493356));
#263118=CARTESIAN_POINT('Ctrl Pts',(47.7963541666644,4.72273670613166,46.303778404803));
#263119=CARTESIAN_POINT('Ctrl Pts',(47.8624999999977,4.72273670613166,48.26));
#263120=CARTESIAN_POINT('Ctrl Pts',(47.928645833331,4.72273670613166,50.216221595197));
#263121=CARTESIAN_POINT('Ctrl Pts',(47.9947916666643,3.33947915066427,51.5994791506644));
#263122=CARTESIAN_POINT('Ctrl Pts',(48.0609374999976,1.95622159519687,52.9827367061318));
#263123=CARTESIAN_POINT('Ctrl Pts',(48.1270833333309,-1.67745629131754E-13,
52.9827367061318));
#263124=CARTESIAN_POINT('Ctrl Pts',(48.1932291666642,-1.95622159519721,
52.9827367061318));
#263125=CARTESIAN_POINT('Ctrl Pts',(48.2593749999975,-3.3394791506646,51.5994791506644));
#263126=CARTESIAN_POINT('Ctrl Pts',(48.3255208333308,-4.722736706132,50.216221595197));
#263127=CARTESIAN_POINT('Ctrl Pts',(48.3916666666642,-4.72273670613199,
48.26));
#263128=CARTESIAN_POINT('Ctrl Pts',(48.4578124999975,-4.722736706132,46.303778404803));
#263129=CARTESIAN_POINT('Ctrl Pts',(48.5239583333308,-3.3394791506646,44.9205208493356));
#263130=CARTESIAN_POINT('Ctrl Pts',(48.5901041666641,-1.95622159519721,
43.5372632938682));
#263131=CARTESIAN_POINT('Ctrl Pts',(48.6562499999974,-1.70749941551634E-13,
43.5372632938682));
#263132=CARTESIAN_POINT('Ctrl Pts',(48.7223958333307,1.95622159519687,43.5372632938682));
#263133=CARTESIAN_POINT('Ctrl Pts',(48.7885416666641,3.33947915066426,44.9205208493356));
#263134=CARTESIAN_POINT('Ctrl Pts',(48.8546874999974,4.72273670613165,46.303778404803));
#263135=CARTESIAN_POINT('Ctrl Pts',(48.9208333333307,4.72273670613165,48.26));
#263136=CARTESIAN_POINT('Ctrl Pts',(48.986979166664,4.72273670613165,50.216221595197));
#263137=CARTESIAN_POINT('Ctrl Pts',(49.0531249999973,3.33947915066426,51.5994791506644));
#263138=CARTESIAN_POINT('Ctrl Pts',(49.1192708333306,1.95622159519687,52.9827367061318));
#263139=CARTESIAN_POINT('Ctrl Pts',(49.1854166666639,-1.71440780215362E-13,
52.9827367061318));
#263140=CARTESIAN_POINT('Ctrl Pts',(49.2515624999972,-1.95622159519721,
52.9827367061318));
#263141=CARTESIAN_POINT('Ctrl Pts',(49.3177083333305,-3.33947915066461,
51.5994791506644));
#263142=CARTESIAN_POINT('Ctrl Pts',(49.3838541666639,-4.722736706132,50.216221595197));
#263143=CARTESIAN_POINT('Ctrl Pts',(49.4499999999972,-4.722736706132,48.26));
#263144=CARTESIAN_POINT('Ctrl Pts',(49.5161458333305,-4.722736706132,46.303778404803));
#263145=CARTESIAN_POINT('Ctrl Pts',(49.5822916666638,-3.33947915066461,
44.9205208493356));
#263146=CARTESIAN_POINT('Ctrl Pts',(49.6484374999971,-1.95622159519722,
43.5372632938682));
#263147=CARTESIAN_POINT('Ctrl Pts',(49.7145833333304,-1.74445092635242E-13,
43.5372632938682));
#263148=CARTESIAN_POINT('Ctrl Pts',(49.7807291666637,1.95622159519687,43.5372632938682));
#263149=CARTESIAN_POINT('Ctrl Pts',(49.8468749999971,3.33947915066426,44.9205208493356));
#263150=CARTESIAN_POINT('Ctrl Pts',(49.9130208333304,4.72273670613165,46.303778404803));
#263151=CARTESIAN_POINT('Ctrl Pts',(49.9791666666637,4.72273670613165,48.26));
#263152=CARTESIAN_POINT('Ctrl Pts',(50.045312499997,4.72273670613165,50.216221595197));
#263153=CARTESIAN_POINT('Ctrl Pts',(50.1114583333303,3.33947915066426,51.5994791506644));
#263154=CARTESIAN_POINT('Ctrl Pts',(50.1776041666636,1.95622159519687,52.9827367061318));
#263155=CARTESIAN_POINT('Ctrl Pts',(50.2437499999969,-1.7513593129897E-13,
52.9827367061318));
#263156=CARTESIAN_POINT('Ctrl Pts',(50.3098958333302,-1.95622159519722,
52.9827367061318));
#263157=CARTESIAN_POINT('Ctrl Pts',(50.3760416666635,-3.33947915066461,
51.5994791506644));
#263158=CARTESIAN_POINT('Ctrl Pts',(50.4421874999969,-4.722736706132,50.216221595197));
#263159=CARTESIAN_POINT('Ctrl Pts',(50.5083333333302,-4.722736706132,48.26));
#263160=CARTESIAN_POINT('Ctrl Pts',(50.5744791666635,-4.722736706132,46.303778404803));
#263161=CARTESIAN_POINT('Ctrl Pts',(50.6406249999968,-3.33947915066461,
44.9205208493356));
#263162=CARTESIAN_POINT('Ctrl Pts',(50.7067708333301,-1.95622159519722,
43.5372632938682));
#263163=CARTESIAN_POINT('Ctrl Pts',(50.7729166666634,-1.7814024371885E-13,
43.5372632938682));
#263164=CARTESIAN_POINT('Ctrl Pts',(50.8390624999967,1.95622159519686,43.5372632938682));
#263165=CARTESIAN_POINT('Ctrl Pts',(50.9052083333301,3.33947915066425,44.9205208493356));
#263166=CARTESIAN_POINT('Ctrl Pts',(50.9713541666634,4.72273670613165,46.303778404803));
#263167=CARTESIAN_POINT('Ctrl Pts',(51.0374999999967,4.72273670613165,48.26));
#263168=CARTESIAN_POINT('Origin',(-3.05311331771918E-14,40.4567708333334,
48.26));
#263169=CARTESIAN_POINT('',(4.72273670613183,48.3916666666642,48.26));
#263170=CARTESIAN_POINT('',(4.72273670613183,48.3968749999976,48.26));
#263171=CARTESIAN_POINT('',(4.72273670613176,40.4567708333334,48.26));
#263172=CARTESIAN_POINT('',(2.14259623628819,49.2650632938682,52.4687436799701));
#263173=CARTESIAN_POINT('Ctrl Pts',(4.72273670613183,48.3916666666642,48.26));
#263174=CARTESIAN_POINT('Ctrl Pts',(4.72273670613183,48.4578124999975,46.303778404803));
#263175=CARTESIAN_POINT('Ctrl Pts',(3.33947915066444,48.5239583333308,44.9205208493356));
#263176=CARTESIAN_POINT('Ctrl Pts',(1.95622159519705,48.5901041666641,43.5372632938682));
#263177=CARTESIAN_POINT('Ctrl Pts',(6.99833541005117E-15,48.6562499999974,
43.5372632938682));
#263178=CARTESIAN_POINT('Ctrl Pts',(-1.95622159519704,48.7223958333307,
43.5372632938682));
#263179=CARTESIAN_POINT('Ctrl Pts',(-3.33947915066443,48.788541666664,44.9205208493356));
#263180=CARTESIAN_POINT('Ctrl Pts',(-4.72273670613182,48.8546874999974,
46.303778404803));
#263181=CARTESIAN_POINT('Ctrl Pts',(-4.72273670613182,48.9208333333307,
48.26));
#263182=CARTESIAN_POINT('Ctrl Pts',(-4.72273670613182,48.986979166664,50.216221595197));
#263183=CARTESIAN_POINT('Ctrl Pts',(-3.33947915066443,49.0531249999973,
51.5994791506644));
#263184=CARTESIAN_POINT('Ctrl Pts',(-1.95622159519703,49.1192708333306,
52.9827367061318));
#263185=CARTESIAN_POINT('Ctrl Pts',(7.17168088200102E-15,49.1854166666639,
52.9827367061318));
#263186=CARTESIAN_POINT('Ctrl Pts',(1.13294968517018,49.2237251595434,52.9827367061318));
#263187=CARTESIAN_POINT('Ctrl Pts',(2.14259623628819,49.2650632938682,52.4687436799701));
#263188=CARTESIAN_POINT('',(2.01456111142411,49.2650632938682,52.5315085770466));
#263189=CARTESIAN_POINT('Origin',(-4.11914963277527E-6,49.2650632939072,
48.2599916315336));
#263190=CARTESIAN_POINT('Ctrl Pts',(4.72273670613183,48.3968749999976,48.26));
#263191=CARTESIAN_POINT('Ctrl Pts',(4.72273670613183,48.4630208333309,46.303778404803));
#263192=CARTESIAN_POINT('Ctrl Pts',(3.33947915066444,48.5291666666642,44.9205208493356));
#263193=CARTESIAN_POINT('Ctrl Pts',(1.95622159519705,48.5953124999975,43.5372632938682));
#263194=CARTESIAN_POINT('Ctrl Pts',(6.99833541005117E-15,48.6614583333308,
43.5372632938682));
#263195=CARTESIAN_POINT('Ctrl Pts',(-1.95622159519704,48.7276041666641,
43.5372632938682));
#263196=CARTESIAN_POINT('Ctrl Pts',(-3.33947915066443,48.7937499999974,
44.9205208493356));
#263197=CARTESIAN_POINT('Ctrl Pts',(-4.72273670613182,48.8598958333307,
46.303778404803));
#263198=CARTESIAN_POINT('Ctrl Pts',(-4.72273670613182,48.9260416666641,
48.26));
#263199=CARTESIAN_POINT('Ctrl Pts',(-4.72273670613182,48.9921874999974,
50.216221595197));
#263200=CARTESIAN_POINT('Ctrl Pts',(-3.33947915066443,49.0583333333307,
51.5994791506644));
#263201=CARTESIAN_POINT('Ctrl Pts',(-1.95622159519703,49.124479166664,52.9827367061318));
#263202=CARTESIAN_POINT('Ctrl Pts',(7.17168088200102E-15,49.1906249999973,
52.9827367061318));
#263203=CARTESIAN_POINT('Ctrl Pts',(1.05781434774328,49.2263929373901,52.9827367061318));
#263204=CARTESIAN_POINT('Ctrl Pts',(2.01456111142411,49.2650632938682,52.5315085770466));
#263205=CARTESIAN_POINT('Origin',(-3.05311331771918E-14,40.4567708333334,
48.26));
#263206=CARTESIAN_POINT('',(4.72273670613183,47.3333333333312,48.26));
#263207=CARTESIAN_POINT('',(4.72273670613183,47.3385416666645,48.26));
#263208=CARTESIAN_POINT('',(4.72273670613176,40.4567708333334,48.26));
#263209=CARTESIAN_POINT('Ctrl Pts',(4.72273670613183,47.3333333333312,48.26));
#263210=CARTESIAN_POINT('Ctrl Pts',(4.72273670613183,47.3994791666645,46.303778404803));
#263211=CARTESIAN_POINT('Ctrl Pts',(3.33947915066444,47.4656249999978,44.9205208493356));
#263212=CARTESIAN_POINT('Ctrl Pts',(1.95622159519705,47.5317708333311,43.5372632938682));
#263213=CARTESIAN_POINT('Ctrl Pts',(6.99833541005117E-15,47.5979166666644,
43.5372632938682));
#263214=CARTESIAN_POINT('Ctrl Pts',(-1.95622159519704,47.6640624999977,
43.5372632938682));
#263215=CARTESIAN_POINT('Ctrl Pts',(-3.33947915066443,47.730208333331,44.9205208493356));
#263216=CARTESIAN_POINT('Ctrl Pts',(-4.72273670613182,47.7963541666644,
46.303778404803));
#263217=CARTESIAN_POINT('Ctrl Pts',(-4.72273670613182,47.8624999999977,
48.26));
#263218=CARTESIAN_POINT('Ctrl Pts',(-4.72273670613182,47.928645833331,50.216221595197));
#263219=CARTESIAN_POINT('Ctrl Pts',(-3.33947915066443,47.9947916666643,
51.5994791506644));
#263220=CARTESIAN_POINT('Ctrl Pts',(-1.95622159519703,48.0609374999976,
52.9827367061318));
#263221=CARTESIAN_POINT('Ctrl Pts',(7.17168088200102E-15,48.1270833333309,
52.9827367061318));
#263222=CARTESIAN_POINT('Ctrl Pts',(1.95622159519705,48.1932291666642,52.9827367061318));
#263223=CARTESIAN_POINT('Ctrl Pts',(3.33947915066444,48.2593749999975,51.5994791506644));
#263224=CARTESIAN_POINT('Ctrl Pts',(4.72273670613183,48.3255208333309,50.216221595197));
#263225=CARTESIAN_POINT('Ctrl Pts',(4.72273670613183,48.3916666666642,48.26));
#263226=CARTESIAN_POINT('Ctrl Pts',(4.72273670613183,47.3385416666645,48.26));
#263227=CARTESIAN_POINT('Ctrl Pts',(4.72273670613183,47.4046874999979,46.303778404803));
#263228=CARTESIAN_POINT('Ctrl Pts',(3.33947915066444,47.4708333333312,44.9205208493356));
#263229=CARTESIAN_POINT('Ctrl Pts',(1.95622159519705,47.5369791666645,43.5372632938682));
#263230=CARTESIAN_POINT('Ctrl Pts',(6.99833541005117E-15,47.6031249999978,
43.5372632938682));
#263231=CARTESIAN_POINT('Ctrl Pts',(-1.95622159519704,47.6692708333311,
43.5372632938682));
#263232=CARTESIAN_POINT('Ctrl Pts',(-3.33947915066443,47.7354166666644,
44.9205208493356));
#263233=CARTESIAN_POINT('Ctrl Pts',(-4.72273670613182,47.8015624999977,
46.303778404803));
#263234=CARTESIAN_POINT('Ctrl Pts',(-4.72273670613182,47.867708333331,48.26));
#263235=CARTESIAN_POINT('Ctrl Pts',(-4.72273670613182,47.9338541666644,
50.216221595197));
#263236=CARTESIAN_POINT('Ctrl Pts',(-3.33947915066443,47.9999999999977,
51.5994791506644));
#263237=CARTESIAN_POINT('Ctrl Pts',(-1.95622159519703,48.066145833331,52.9827367061318));
#263238=CARTESIAN_POINT('Ctrl Pts',(7.17168088200104E-15,48.1322916666643,
52.9827367061318));
#263239=CARTESIAN_POINT('Ctrl Pts',(1.95622159519705,48.1984374999976,52.9827367061318));
#263240=CARTESIAN_POINT('Ctrl Pts',(3.33947915066444,48.2645833333309,51.5994791506644));
#263241=CARTESIAN_POINT('Ctrl Pts',(4.72273670613183,48.3307291666642,50.216221595197));
#263242=CARTESIAN_POINT('Ctrl Pts',(4.72273670613183,48.3968749999976,48.26));
#263243=CARTESIAN_POINT('Origin',(-3.05311331771918E-14,40.4567708333334,
48.26));
#263244=CARTESIAN_POINT('',(4.72273670613183,46.2749999999982,48.26));
#263245=CARTESIAN_POINT('',(4.72273670613183,46.2802083333315,48.26));
#263246=CARTESIAN_POINT('',(4.72273670613176,40.4567708333334,48.26));
#263247=CARTESIAN_POINT('Ctrl Pts',(4.72273670613183,46.2749999999982,48.26));
#263248=CARTESIAN_POINT('Ctrl Pts',(4.72273670613183,46.3411458333315,46.303778404803));
#263249=CARTESIAN_POINT('Ctrl Pts',(3.33947915066444,46.4072916666648,44.9205208493356));
#263250=CARTESIAN_POINT('Ctrl Pts',(1.95622159519705,46.4734374999981,43.5372632938682));
#263251=CARTESIAN_POINT('Ctrl Pts',(6.99833541005117E-15,46.5395833333314,
43.5372632938682));
#263252=CARTESIAN_POINT('Ctrl Pts',(-1.95622159519704,46.6057291666647,
43.5372632938682));
#263253=CARTESIAN_POINT('Ctrl Pts',(-3.33947915066443,46.671874999998,44.9205208493356));
#263254=CARTESIAN_POINT('Ctrl Pts',(-4.72273670613182,46.7380208333314,
46.303778404803));
#263255=CARTESIAN_POINT('Ctrl Pts',(-4.72273670613182,46.8041666666647,
48.26));
#263256=CARTESIAN_POINT('Ctrl Pts',(-4.72273670613182,46.870312499998,50.216221595197));
#263257=CARTESIAN_POINT('Ctrl Pts',(-3.33947915066443,46.9364583333313,
51.5994791506644));
#263258=CARTESIAN_POINT('Ctrl Pts',(-1.95622159519703,47.0026041666646,
52.9827367061318));
#263259=CARTESIAN_POINT('Ctrl Pts',(7.17168088200104E-15,47.0687499999979,
52.9827367061318));
#263260=CARTESIAN_POINT('Ctrl Pts',(1.95622159519705,47.1348958333312,52.9827367061318));
#263261=CARTESIAN_POINT('Ctrl Pts',(3.33947915066444,47.2010416666646,51.5994791506644));
#263262=CARTESIAN_POINT('Ctrl Pts',(4.72273670613183,47.2671874999979,50.216221595197));
#263263=CARTESIAN_POINT('Ctrl Pts',(4.72273670613183,47.3333333333312,48.26));
#263264=CARTESIAN_POINT('Ctrl Pts',(4.72273670613183,46.2802083333315,48.26));
#263265=CARTESIAN_POINT('Ctrl Pts',(4.72273670613183,46.3463541666649,46.303778404803));
#263266=CARTESIAN_POINT('Ctrl Pts',(3.33947915066444,46.4124999999982,44.9205208493356));
#263267=CARTESIAN_POINT('Ctrl Pts',(1.95622159519705,46.4786458333315,43.5372632938682));
#263268=CARTESIAN_POINT('Ctrl Pts',(6.99833541005117E-15,46.5447916666648,
43.5372632938682));
#263269=CARTESIAN_POINT('Ctrl Pts',(-1.95622159519704,46.6109374999981,
43.5372632938682));
#263270=CARTESIAN_POINT('Ctrl Pts',(-3.33947915066443,46.6770833333314,
44.9205208493356));
#263271=CARTESIAN_POINT('Ctrl Pts',(-4.72273670613182,46.7432291666647,
46.303778404803));
#263272=CARTESIAN_POINT('Ctrl Pts',(-4.72273670613182,46.8093749999981,
48.26));
#263273=CARTESIAN_POINT('Ctrl Pts',(-4.72273670613182,46.8755208333314,
50.216221595197));
#263274=CARTESIAN_POINT('Ctrl Pts',(-3.33947915066443,46.9416666666647,
51.5994791506644));
#263275=CARTESIAN_POINT('Ctrl Pts',(-1.95622159519703,47.007812499998,52.9827367061318));
#263276=CARTESIAN_POINT('Ctrl Pts',(7.17168088200104E-15,47.0739583333313,
52.9827367061318));
#263277=CARTESIAN_POINT('Ctrl Pts',(1.95622159519705,47.1401041666646,52.9827367061318));
#263278=CARTESIAN_POINT('Ctrl Pts',(3.33947915066444,47.2062499999979,51.5994791506644));
#263279=CARTESIAN_POINT('Ctrl Pts',(4.72273670613183,47.2723958333312,50.216221595197));
#263280=CARTESIAN_POINT('Ctrl Pts',(4.72273670613183,47.3385416666645,48.26));
#263281=CARTESIAN_POINT('Origin',(-3.05311331771918E-14,40.4567708333334,
48.26));
#263282=CARTESIAN_POINT('',(4.72273670613183,45.2166666666652,48.26));
#263283=CARTESIAN_POINT('',(4.72273670613183,45.2218749999985,48.26));
#263284=CARTESIAN_POINT('',(4.72273670613176,40.4567708333334,48.26));
#263285=CARTESIAN_POINT('Ctrl Pts',(4.72273670613183,45.2166666666652,48.26));
#263286=CARTESIAN_POINT('Ctrl Pts',(4.72273670613183,45.2828124999985,46.303778404803));
#263287=CARTESIAN_POINT('Ctrl Pts',(3.33947915066444,45.3489583333318,44.9205208493356));
#263288=CARTESIAN_POINT('Ctrl Pts',(1.95622159519705,45.4151041666651,43.5372632938682));
#263289=CARTESIAN_POINT('Ctrl Pts',(6.99833541005117E-15,45.4812499999984,
43.5372632938682));
#263290=CARTESIAN_POINT('Ctrl Pts',(-1.95622159519704,45.5473958333317,
43.5372632938682));
#263291=CARTESIAN_POINT('Ctrl Pts',(-3.33947915066443,45.613541666665,44.9205208493356));
#263292=CARTESIAN_POINT('Ctrl Pts',(-4.72273670613182,45.6796874999984,
46.303778404803));
#263293=CARTESIAN_POINT('Ctrl Pts',(-4.72273670613182,45.7458333333317,
48.26));
#263294=CARTESIAN_POINT('Ctrl Pts',(-4.72273670613182,45.811979166665,50.216221595197));
#263295=CARTESIAN_POINT('Ctrl Pts',(-3.33947915066443,45.8781249999983,
51.5994791506644));
#263296=CARTESIAN_POINT('Ctrl Pts',(-1.95622159519703,45.9442708333316,
52.9827367061318));
#263297=CARTESIAN_POINT('Ctrl Pts',(7.17168088200104E-15,46.0104166666649,
52.9827367061318));
#263298=CARTESIAN_POINT('Ctrl Pts',(1.95622159519705,46.0765624999982,52.9827367061318));
#263299=CARTESIAN_POINT('Ctrl Pts',(3.33947915066444,46.1427083333315,51.5994791506644));
#263300=CARTESIAN_POINT('Ctrl Pts',(4.72273670613183,46.2088541666649,50.216221595197));
#263301=CARTESIAN_POINT('Ctrl Pts',(4.72273670613183,46.2749999999982,48.26));
#263302=CARTESIAN_POINT('Ctrl Pts',(4.72273670613183,45.2218749999985,48.26));
#263303=CARTESIAN_POINT('Ctrl Pts',(4.72273670613183,45.2880208333319,46.303778404803));
#263304=CARTESIAN_POINT('Ctrl Pts',(3.33947915066444,45.3541666666652,44.9205208493356));
#263305=CARTESIAN_POINT('Ctrl Pts',(1.95622159519705,45.4203124999985,43.5372632938682));
#263306=CARTESIAN_POINT('Ctrl Pts',(6.99833541005117E-15,45.4864583333318,
43.5372632938682));
#263307=CARTESIAN_POINT('Ctrl Pts',(-1.95622159519704,45.5526041666651,
43.5372632938682));
#263308=CARTESIAN_POINT('Ctrl Pts',(-3.33947915066443,45.6187499999984,
44.9205208493356));
#263309=CARTESIAN_POINT('Ctrl Pts',(-4.72273670613182,45.6848958333317,
46.303778404803));
#263310=CARTESIAN_POINT('Ctrl Pts',(-4.72273670613182,45.7510416666651,
48.26));
#263311=CARTESIAN_POINT('Ctrl Pts',(-4.72273670613182,45.8171874999984,
50.216221595197));
#263312=CARTESIAN_POINT('Ctrl Pts',(-3.33947915066443,45.8833333333317,
51.5994791506644));
#263313=CARTESIAN_POINT('Ctrl Pts',(-1.95622159519703,45.949479166665,52.9827367061318));
#263314=CARTESIAN_POINT('Ctrl Pts',(7.17168088200107E-15,46.0156249999983,
52.9827367061318));
#263315=CARTESIAN_POINT('Ctrl Pts',(1.95622159519705,46.0817708333316,52.9827367061318));
#263316=CARTESIAN_POINT('Ctrl Pts',(3.33947915066444,46.1479166666649,51.5994791506644));
#263317=CARTESIAN_POINT('Ctrl Pts',(4.72273670613183,46.2140624999982,50.216221595197));
#263318=CARTESIAN_POINT('Ctrl Pts',(4.72273670613183,46.2802083333315,48.26));
#263319=CARTESIAN_POINT('Origin',(-3.05311331771918E-14,40.4567708333334,
48.26));
#263320=CARTESIAN_POINT('',(4.72273670613183,44.1583333333322,48.26));
#263321=CARTESIAN_POINT('',(4.72273670613183,44.1635416666656,48.26));
#263322=CARTESIAN_POINT('',(4.72273670613176,40.4567708333334,48.26));
#263323=CARTESIAN_POINT('Ctrl Pts',(4.72273670613183,44.1583333333322,48.26));
#263324=CARTESIAN_POINT('Ctrl Pts',(4.72273670613183,44.2244791666655,46.303778404803));
#263325=CARTESIAN_POINT('Ctrl Pts',(3.33947915066444,44.2906249999988,44.9205208493356));
#263326=CARTESIAN_POINT('Ctrl Pts',(1.95622159519705,44.3567708333321,43.5372632938682));
#263327=CARTESIAN_POINT('Ctrl Pts',(6.99833541005117E-15,44.4229166666654,
43.5372632938682));
#263328=CARTESIAN_POINT('Ctrl Pts',(-1.95622159519704,44.4890624999987,
43.5372632938682));
#263329=CARTESIAN_POINT('Ctrl Pts',(-3.33947915066443,44.555208333332,44.9205208493356));
#263330=CARTESIAN_POINT('Ctrl Pts',(-4.72273670613182,44.6213541666654,
46.303778404803));
#263331=CARTESIAN_POINT('Ctrl Pts',(-4.72273670613182,44.6874999999987,
48.26));
#263332=CARTESIAN_POINT('Ctrl Pts',(-4.72273670613182,44.753645833332,50.216221595197));
#263333=CARTESIAN_POINT('Ctrl Pts',(-3.33947915066443,44.8197916666653,
51.5994791506644));
#263334=CARTESIAN_POINT('Ctrl Pts',(-1.95622159519703,44.8859374999986,
52.9827367061318));
#263335=CARTESIAN_POINT('Ctrl Pts',(7.17168088200107E-15,44.9520833333319,
52.9827367061318));
#263336=CARTESIAN_POINT('Ctrl Pts',(1.95622159519705,45.0182291666652,52.9827367061318));
#263337=CARTESIAN_POINT('Ctrl Pts',(3.33947915066444,45.0843749999985,51.5994791506644));
#263338=CARTESIAN_POINT('Ctrl Pts',(4.72273670613183,45.1505208333318,50.216221595197));
#263339=CARTESIAN_POINT('Ctrl Pts',(4.72273670613183,45.2166666666652,48.26));
#263340=CARTESIAN_POINT('Ctrl Pts',(4.72273670613183,44.1635416666656,48.26));
#263341=CARTESIAN_POINT('Ctrl Pts',(4.72273670613183,44.2296874999989,46.303778404803));
#263342=CARTESIAN_POINT('Ctrl Pts',(3.33947915066444,44.2958333333322,44.9205208493356));
#263343=CARTESIAN_POINT('Ctrl Pts',(1.95622159519705,44.3619791666655,43.5372632938682));
#263344=CARTESIAN_POINT('Ctrl Pts',(6.99833541005117E-15,44.4281249999988,
43.5372632938682));
#263345=CARTESIAN_POINT('Ctrl Pts',(-1.95622159519704,44.4942708333321,
43.5372632938682));
#263346=CARTESIAN_POINT('Ctrl Pts',(-3.33947915066443,44.5604166666654,
44.9205208493356));
#263347=CARTESIAN_POINT('Ctrl Pts',(-4.72273670613182,44.6265624999987,
46.303778404803));
#263348=CARTESIAN_POINT('Ctrl Pts',(-4.72273670613182,44.692708333332,48.26));
#263349=CARTESIAN_POINT('Ctrl Pts',(-4.72273670613182,44.7588541666654,
50.216221595197));
#263350=CARTESIAN_POINT('Ctrl Pts',(-3.33947915066443,44.8249999999987,
51.5994791506644));
#263351=CARTESIAN_POINT('Ctrl Pts',(-1.95622159519703,44.891145833332,52.9827367061318));
#263352=CARTESIAN_POINT('Ctrl Pts',(7.17168088200107E-15,44.9572916666653,
52.9827367061318));
#263353=CARTESIAN_POINT('Ctrl Pts',(1.95622159519705,45.0234374999986,52.9827367061318));
#263354=CARTESIAN_POINT('Ctrl Pts',(3.33947915066444,45.0895833333319,51.5994791506644));
#263355=CARTESIAN_POINT('Ctrl Pts',(4.72273670613183,45.1557291666652,50.216221595197));
#263356=CARTESIAN_POINT('Ctrl Pts',(4.72273670613183,45.2218749999985,48.26));
#263357=CARTESIAN_POINT('Origin',(-3.05311331771918E-14,40.4567708333334,
48.26));
#263358=CARTESIAN_POINT('',(4.72273670613183,43.0999999999992,48.26));
#263359=CARTESIAN_POINT('',(4.72273670613183,43.1052083333326,48.26));
#263360=CARTESIAN_POINT('',(4.72273670613176,40.4567708333334,48.26));
#263361=CARTESIAN_POINT('Ctrl Pts',(4.72273670613183,43.0999999999992,48.26));
#263362=CARTESIAN_POINT('Ctrl Pts',(4.72273670613183,43.1661458333325,46.303778404803));
#263363=CARTESIAN_POINT('Ctrl Pts',(3.33947915066444,43.2322916666658,44.9205208493356));
#263364=CARTESIAN_POINT('Ctrl Pts',(1.95622159519705,43.2984374999991,43.5372632938682));
#263365=CARTESIAN_POINT('Ctrl Pts',(6.99833541005117E-15,43.3645833333324,
43.5372632938682));
#263366=CARTESIAN_POINT('Ctrl Pts',(-1.95622159519704,43.4307291666657,
43.5372632938682));
#263367=CARTESIAN_POINT('Ctrl Pts',(-3.33947915066443,43.496874999999,44.9205208493356));
#263368=CARTESIAN_POINT('Ctrl Pts',(-4.72273670613182,43.5630208333324,
46.303778404803));
#263369=CARTESIAN_POINT('Ctrl Pts',(-4.72273670613182,43.6291666666657,
48.26));
#263370=CARTESIAN_POINT('Ctrl Pts',(-4.72273670613182,43.695312499999,50.216221595197));
#263371=CARTESIAN_POINT('Ctrl Pts',(-3.33947915066443,43.7614583333323,
51.5994791506644));
#263372=CARTESIAN_POINT('Ctrl Pts',(-1.95622159519703,43.8276041666656,
52.9827367061318));
#263373=CARTESIAN_POINT('Ctrl Pts',(7.17168088200102E-15,43.8937499999989,
52.9827367061318));
#263374=CARTESIAN_POINT('Ctrl Pts',(1.95622159519705,43.9598958333322,52.9827367061318));
#263375=CARTESIAN_POINT('Ctrl Pts',(3.33947915066444,44.0260416666656,51.5994791506644));
#263376=CARTESIAN_POINT('Ctrl Pts',(4.72273670613183,44.0921874999989,50.216221595197));
#263377=CARTESIAN_POINT('Ctrl Pts',(4.72273670613183,44.1583333333322,48.26));
#263378=CARTESIAN_POINT('Ctrl Pts',(4.72273670613183,43.1052083333326,48.26));
#263379=CARTESIAN_POINT('Ctrl Pts',(4.72273670613183,43.1713541666659,46.303778404803));
#263380=CARTESIAN_POINT('Ctrl Pts',(3.33947915066444,43.2374999999992,44.9205208493356));
#263381=CARTESIAN_POINT('Ctrl Pts',(1.95622159519705,43.3036458333325,43.5372632938682));
#263382=CARTESIAN_POINT('Ctrl Pts',(6.99833541005117E-15,43.3697916666658,
43.5372632938682));
#263383=CARTESIAN_POINT('Ctrl Pts',(-1.95622159519704,43.4359374999991,
43.5372632938682));
#263384=CARTESIAN_POINT('Ctrl Pts',(-3.33947915066443,43.5020833333324,
44.9205208493356));
#263385=CARTESIAN_POINT('Ctrl Pts',(-4.72273670613182,43.5682291666657,
46.303778404803));
#263386=CARTESIAN_POINT('Ctrl Pts',(-4.72273670613182,43.634374999999,48.26));
#263387=CARTESIAN_POINT('Ctrl Pts',(-4.72273670613182,43.7005208333324,
50.216221595197));
#263388=CARTESIAN_POINT('Ctrl Pts',(-3.33947915066443,43.7666666666657,
51.5994791506644));
#263389=CARTESIAN_POINT('Ctrl Pts',(-1.95622159519703,43.832812499999,52.9827367061318));
#263390=CARTESIAN_POINT('Ctrl Pts',(7.17168088200102E-15,43.8989583333323,
52.9827367061318));
#263391=CARTESIAN_POINT('Ctrl Pts',(1.95622159519705,43.9651041666656,52.9827367061318));
#263392=CARTESIAN_POINT('Ctrl Pts',(3.33947915066444,44.0312499999989,51.5994791506644));
#263393=CARTESIAN_POINT('Ctrl Pts',(4.72273670613183,44.0973958333322,50.216221595197));
#263394=CARTESIAN_POINT('Ctrl Pts',(4.72273670613183,44.1635416666656,48.26));
#263395=CARTESIAN_POINT('Origin',(6.7958239265071E-15,40.475,48.26));
#263396=CARTESIAN_POINT('',(4.40328459016939E-15,42.2906249999995,43.5102));
#263397=CARTESIAN_POINT('',(5.54528904550239E-15,42.09425,43.5102));
#263398=CARTESIAN_POINT('',(5.54528904550239E-15,40.475,43.5102));
#263399=CARTESIAN_POINT('',(4.36624125519644,42.09425,46.3900969700488));
#263400=CARTESIAN_POINT('Ctrl Pts',(7.7715611723761E-15,42.2906249999995,
43.5102));
#263401=CARTESIAN_POINT('Ctrl Pts',(0.306312377613604,42.2803266558546,
43.5102));
#263402=CARTESIAN_POINT('Ctrl Pts',(0.612600594710301,42.2696165070132,
43.539829200288));
#263403=CARTESIAN_POINT('Ctrl Pts',(1.5259625148491,42.2364131029764,43.719048502412));
#263404=CARTESIAN_POINT('Ctrl Pts',(2.10782424211785,42.2135208891992,43.9581541159287));
#263405=CARTESIAN_POINT('Ctrl Pts',(3.00697611076785,42.1749789086954,44.5550320160162));
#263406=CARTESIAN_POINT('Ctrl Pts',(3.34869201888086,42.15983788401,44.8607436451307));
#263407=CARTESIAN_POINT('Ctrl Pts',(3.93944645506913,42.1278937490674,45.5661866234649));
#263408=CARTESIAN_POINT('Ctrl Pts',(4.18359566378164,42.1111319270672,45.9636177871491));
#263409=CARTESIAN_POINT('Ctrl Pts',(4.36624125519659,42.09425,46.3900969700491));
#263410=CARTESIAN_POINT('Origin',(6.7958239265071E-15,42.09425,48.26));
#263411=CARTESIAN_POINT('Origin',(6.7958239265071E-15,40.475,48.26));
#263412=CARTESIAN_POINT('',(-1.95879410825898E-14,43.3489583333325,43.5102));
#263413=CARTESIAN_POINT('',(1.07523725122445E-14,42.3270833333327,43.5102));
#263414=CARTESIAN_POINT('',(5.54528904550239E-15,40.475,43.5102));
#263415=CARTESIAN_POINT('Ctrl Pts',(-4.29517532651857E-14,43.3489583333325,
43.5102));
#263416=CARTESIAN_POINT('Ctrl Pts',(0.413798530172926,43.3350462619249,
43.5102));
#263417=CARTESIAN_POINT('Ctrl Pts',(0.826670368688511,43.3204123302741,
43.5642725719141));
#263418=CARTESIAN_POINT('Ctrl Pts',(1.8259494112998,43.2830916071325,43.831726042004));
#263419=CARTESIAN_POINT('Ctrl Pts',(2.38686058154301,43.2603987577855,44.1070948134215));
#263420=CARTESIAN_POINT('Ctrl Pts',(3.36882436692966,43.2169625534067,44.8554914890216));
#263421=CARTESIAN_POINT('Ctrl Pts',(3.78128185410638,43.1966949382382,45.3203462387152));
#263422=CARTESIAN_POINT('Ctrl Pts',(4.40771574233544,43.1521835512767,46.3848087314939));
#263423=CARTESIAN_POINT('Ctrl Pts',(4.61444584304911,43.1294619675453,46.9750056411953));
#263424=CARTESIAN_POINT('Ctrl Pts',(4.78902391945517,43.0859479536866,48.1969672260116));
#263425=CARTESIAN_POINT('Ctrl Pts',(4.75696102960572,43.0657543266859,48.8168166627164));
#263426=CARTESIAN_POINT('Ctrl Pts',(4.45711948033121,43.0213051463692,50.0147078667033));
#263427=CARTESIAN_POINT('Ctrl Pts',(4.1902990760171,42.998555617062,50.5808457666307));
#263428=CARTESIAN_POINT('Ctrl Pts',(3.45765603924985,42.9549633791373,51.5739759608694));
#263429=CARTESIAN_POINT('Ctrl Pts',(3.00063580575679,42.9348366133039,51.9928281298175));
#263430=CARTESIAN_POINT('Ctrl Pts',(1.94712039905175,42.8904524036952,52.6365582703685));
#263431=CARTESIAN_POINT('Ctrl Pts',(1.35939952094681,42.8676758816576,52.8532110500321));
#263432=CARTESIAN_POINT('Ctrl Pts',(0.140814301271115,42.824005292089,53.0471837815253));
#263433=CARTESIAN_POINT('Ctrl Pts',(-0.477998516061079,42.803937588497,
53.0253408551151));
#263434=CARTESIAN_POINT('Ctrl Pts',(-1.68036223673691,42.7596209950149,
52.7458177117107));
#263435=CARTESIAN_POINT('Ctrl Pts',(-2.25178562281166,42.7368185887116,
52.4879606083977));
#263436=CARTESIAN_POINT('Ctrl Pts',(-3.25636757408644,42.6930698118832,
51.7717238131873));
#263437=CARTESIAN_POINT('Ctrl Pts',(-3.68179377358298,42.673052782406,51.3227646567329));
#263438=CARTESIAN_POINT('Ctrl Pts',(-4.3432329780399,42.6288062995307,50.280681107429));
#263439=CARTESIAN_POINT('Ctrl Pts',(-4.57008234897582,42.6059792614027,
49.6956812528296));
#263440=CARTESIAN_POINT('Ctrl Pts',(-4.783998273458,42.5621527543215,48.48071918745));
#263441=CARTESIAN_POINT('Ctrl Pts',(-4.77260115723503,42.5421775196058,
47.8629689153103));
#263442=CARTESIAN_POINT('Ctrl Pts',(-4.51390729703972,42.4980034591323,
46.656216903107));
#263443=CARTESIAN_POINT('Ctrl Pts',(-4.26532764079846,42.4751531709417,
46.079526481079));
#263444=CARTESIAN_POINT('Ctrl Pts',(-3.56596209792685,42.4312496794982,
45.0633544203556));
#263445=CARTESIAN_POINT('Ctrl Pts',(-3.1251912266916,42.4113069799741,44.6312525735305));
#263446=CARTESIAN_POINT('Ctrl Pts',(-2.09489088525855,42.3672074406395,
43.9519179106002));
#263447=CARTESIAN_POINT('Ctrl Pts',(-1.5128344495972,42.3443353961348,43.7147306798431));
#263448=CARTESIAN_POINT('Ctrl Pts',(-0.603833353133009,42.3113269822488,
43.5389852708177));
#263449=CARTESIAN_POINT('Ctrl Pts',(-0.301918536111969,42.3007756214429,
43.5102));
#263450=CARTESIAN_POINT('Ctrl Pts',(6.17561557447743E-15,42.2906249999995,
43.5102));
#263451=CARTESIAN_POINT('',(4.66218791181207,42.0942499999981,47.3519229575834));
#263452=CARTESIAN_POINT('Origin',(6.7958239265071E-15,42.09425,48.26));
#263453=CARTESIAN_POINT('Ctrl Pts',(4.66218791181102,42.0942499999949,47.3519229575838));
#263454=CARTESIAN_POINT('Ctrl Pts',(4.5947983082204,42.1068206953643,47.0059357994833));
#263455=CARTESIAN_POINT('Ctrl Pts',(4.48910763172072,42.1196360322442,46.6685368854553));
#263456=CARTESIAN_POINT('Ctrl Pts',(4.20537339562347,42.145252195001,46.0241402159205));
#263457=CARTESIAN_POINT('Ctrl Pts',(4.0283811118818,42.1579739998848,45.7190573960589));
#263458=CARTESIAN_POINT('Ctrl Pts',(3.45736524908729,42.1918930242663,44.9466976226496));
#263459=CARTESIAN_POINT('Ctrl Pts',(3.00461394812578,42.2118479691886,44.5312412852076));
#263460=CARTESIAN_POINT('Ctrl Pts',(1.95293188099643,42.2562007886002,43.8853391386656));
#263461=CARTESIAN_POINT('Ctrl Pts',(1.36067932860232,42.2791600006444,43.6665081845346));
#263462=CARTESIAN_POINT('Ctrl Pts',(0.496745708221664,42.3101114315127,
43.5296681000585));
#263463=CARTESIAN_POINT('Ctrl Pts',(0.248293869613903,42.3187355945366,
43.5102));
#263464=CARTESIAN_POINT('Ctrl Pts',(1.48492329543615E-14,42.3270833333328,
43.5102));
#263465=CARTESIAN_POINT('Origin',(6.7958239265071E-15,40.475,48.26));
#263466=CARTESIAN_POINT('',(-3.7455592885151E-14,44.4072916666655,43.5102));
#263467=CARTESIAN_POINT('',(2.32161641899723E-15,43.3854166666658,43.5102));
#263468=CARTESIAN_POINT('',(5.54528904550239E-15,40.475,43.5102));
#263469=CARTESIAN_POINT('Ctrl Pts',(-7.39686090156511E-14,44.4072916666655,
43.5102));
#263470=CARTESIAN_POINT('Ctrl Pts',(0.503221800043281,44.390373149306,43.5102));
#263471=CARTESIAN_POINT('Ctrl Pts',(1.00400848126672,44.3724228202082,43.5901712341933));
#263472=CARTESIAN_POINT('Ctrl Pts',(2.06827713231742,44.3317689812627,43.9400702898139));
#263473=CARTESIAN_POINT('Ctrl Pts',(2.61018179015456,44.3093144518143,44.2442115659869));
#263474=CARTESIAN_POINT('Ctrl Pts',(3.55263113629528,44.2664558238078,45.046529932576));
#263475=CARTESIAN_POINT('Ctrl Pts',(3.94250983519217,44.2454341206351,45.5389303845267));
#263476=CARTESIAN_POINT('Ctrl Pts',(4.50748616977274,44.2005289482455,46.6405621232504));
#263477=CARTESIAN_POINT('Ctrl Pts',(4.67930167148437,44.1780452588232,47.2381452413361));
#263478=CARTESIAN_POINT('Ctrl Pts',(4.78561759298189,44.1351207318422,48.4708483287254));
#263479=CARTESIAN_POINT('Ctrl Pts',(4.71704371069774,44.1142015396868,49.0943336232476));
#263480=CARTESIAN_POINT('Ctrl Pts',(4.34523111346103,44.0693356980773,50.2748065530144));
#263481=CARTESIAN_POINT('Ctrl Pts',(4.04739745399867,44.0468223876693,50.8210722831364));
#263482=CARTESIAN_POINT('Ctrl Pts',(3.25703080618358,44.003829825242,51.7724559182719));
#263483=CARTESIAN_POINT('Ctrl Pts',(2.77083588879443,43.9830123427014,52.1674392770568));
#263484=CARTESIAN_POINT('Ctrl Pts',(1.67739508145102,43.9381885376627,52.7463474425373));
#263485=CARTESIAN_POINT('Ctrl Pts',(1.08129701659115,43.9156452722035,52.9260262159432));
#263486=CARTESIAN_POINT('Ctrl Pts',(-0.149139245221289,43.8725826769129,
53.0477291476657));
#263487=CARTESIAN_POINT('Ctrl Pts',(-0.771810656405107,43.8518653644044,
52.9874638415032));
#263488=CARTESIAN_POINT('Ctrl Pts',(-1.95644428853647,43.8070863850711,
52.6319334746697));
#263489=CARTESIAN_POINT('Ctrl Pts',(-2.50736060681273,43.7845129695506,
52.3410113002899));
#263490=CARTESIAN_POINT('Ctrl Pts',(-3.46835273705026,43.7413785072399,
51.563652064836));
#263491=CARTESIAN_POINT('Ctrl Pts',(-3.86882423653969,43.7207590458096,
51.0841452638547));
#263492=CARTESIAN_POINT('Ctrl Pts',(-4.46269147748995,43.676027748612,49.9996522475679));
#263493=CARTESIAN_POINT('Ctrl Pts',(-4.65084839767155,43.6534241378127,
49.4052710434929));
#263494=CARTESIAN_POINT('Ctrl Pts',(-4.7891292849171,43.6102161612666,48.177377397803));
#263495=CARTESIAN_POINT('Ctrl Pts',(-4.73776279420127,43.5896914222037,
47.555587940092));
#263496=CARTESIAN_POINT('Ctrl Pts',(-4.39973740307815,43.5450107117975,
46.3666264055941));
#263497=CARTESIAN_POINT('Ctrl Pts',(-4.11631541613004,43.5223770192419,
45.810810537023));
#263498=CARTESIAN_POINT('Ctrl Pts',(-3.35297349292649,43.4790940907976,
44.8395962919083));
#263499=CARTESIAN_POINT('Ctrl Pts',(-2.88059882280507,43.4586601181008,
44.4332850148773));
#263500=CARTESIAN_POINT('Ctrl Pts',(-1.80578318535429,43.4140329253292,
43.8235300453175));
#263501=CARTESIAN_POINT('Ctrl Pts',(-1.21336611326443,43.3913694300323,
43.6263311050534));
#263502=CARTESIAN_POINT('Ctrl Pts',(-0.400469824454208,43.3625984281871,
43.5228482498025));
#263503=CARTESIAN_POINT('Ctrl Pts',(-0.200132489240207,43.355686867337,
43.5102));
#263504=CARTESIAN_POINT('Ctrl Pts',(-3.99680288865056E-14,43.3489583333325,
43.5102));
#263505=CARTESIAN_POINT('Ctrl Pts',(1.54737334057131E-14,42.3270833333327,
43.5102));
#263506=CARTESIAN_POINT('Ctrl Pts',(-0.35821960567291,42.3391268191606,
43.5102));
#263507=CARTESIAN_POINT('Ctrl Pts',(-0.71607214488095,42.3517222752217,
43.5507220553509));
#263508=CARTESIAN_POINT('Ctrl Pts',(-1.67550713467282,42.3870580817763,
43.7718346878538));
#263509=CARTESIAN_POINT('Ctrl Pts',(-2.25071018064137,42.4100044194961,
44.030902312143));
#263510=CARTESIAN_POINT('Ctrl Pts',(-3.25541035828551,42.4537685521362,
44.7479563537761));
#263511=CARTESIAN_POINT('Ctrl Pts',(-3.67877054229274,42.473679910113,45.1942548346965));
#263512=CARTESIAN_POINT('Ctrl Pts',(-4.34157757558856,42.5178973195809,
46.234907055749));
#263513=CARTESIAN_POINT('Ctrl Pts',(-4.56986676456883,42.5408290503086,
46.822424478906));
#263514=CARTESIAN_POINT('Ctrl Pts',(-4.78365346537154,42.5846736373392,
48.0379778377428));
#263515=CARTESIAN_POINT('Ctrl Pts',(-4.77261296903176,42.6045767469765,
48.6534449009694));
#263516=CARTESIAN_POINT('Ctrl Pts',(-4.51547977408878,42.648723303151,49.8600252782126));
#263517=CARTESIAN_POINT('Ctrl Pts',(-4.26657920474278,42.6716386916767,
50.4385191081198));
#263518=CARTESIAN_POINT('Ctrl Pts',(-3.56702886072932,42.7155628202327,
51.4552284488307));
#263519=CARTESIAN_POINT('Ctrl Pts',(-3.1273415287299,42.7354671391827,51.8866946633162));
#263520=CARTESIAN_POINT('Ctrl Pts',(-2.09805709470288,42.7795410052046,
52.56663839445));
#263521=CARTESIAN_POINT('Ctrl Pts',(-1.51551485278494,42.802438336214,52.8044685584775));
#263522=CARTESIAN_POINT('Ctrl Pts',(-0.303969126029313,42.8464407839499,
53.0392662005286));
#263523=CARTESIAN_POINT('Ctrl Pts',(0.312565072830679,42.8663559369633,
53.0387117164387));
#263524=CARTESIAN_POINT('Ctrl Pts',(1.52316486227975,42.9103555026468,52.8018373341285));
#263525=CARTESIAN_POINT('Ctrl Pts',(2.10481239179041,42.9332331024555,52.5632640013275));
#263526=CARTESIAN_POINT('Ctrl Pts',(3.13351782190229,42.9773123779918,51.881533984683));
#263527=CARTESIAN_POINT('Ctrl Pts',(3.57318933199809,42.9972479789684,51.4485358355));
#263528=CARTESIAN_POINT('Ctrl Pts',(4.27027386259732,43.0411719049498,50.4308111467803));
#263529=CARTESIAN_POINT('Ctrl Pts',(4.51759478199226,43.0640281646244,49.8534217239699));
#263530=CARTESIAN_POINT('Ctrl Pts',(4.77347759941231,43.1081824830165,48.646092545179));
#263531=CARTESIAN_POINT('Ctrl Pts',(4.78346712714521,43.1281480926501,48.0284855337845));
#263532=CARTESIAN_POINT('Ctrl Pts',(4.5668549003962,43.1719952818795,46.814025146711));
#263533=CARTESIAN_POINT('Ctrl Pts',(4.33862772648812,43.194828680947,46.2294067979757));
#263534=CARTESIAN_POINT('Ctrl Pts',(3.67480020981176,43.2390560053493,45.188882366683));
#263535=CARTESIAN_POINT('Ctrl Pts',(3.24848507963304,43.2590609647294,44.7410135082327));
#263536=CARTESIAN_POINT('Ctrl Pts',(2.24235732065186,43.3028305952222,44.0270111630162));
#263537=CARTESIAN_POINT('Ctrl Pts',(1.6702265530796,43.3256397201586,43.7703793781061));
#263538=CARTESIAN_POINT('Ctrl Pts',(0.714876476894768,43.360819833794,43.5505848889169));
#263539=CARTESIAN_POINT('Ctrl Pts',(0.357612817399793,43.3733935813014,
43.5102));
#263540=CARTESIAN_POINT('Ctrl Pts',(-6.45317133063372E-15,43.3854166666658,
43.5102));
#263541=CARTESIAN_POINT('Origin',(6.7958239265071E-15,40.475,48.26));
#263542=CARTESIAN_POINT('',(-9.87175814600512E-15,45.4656249999985,43.5102));
#263543=CARTESIAN_POINT('',(-3.83749963274187E-14,44.4437499999987,43.5102));
#263544=CARTESIAN_POINT('',(5.54528904550239E-15,40.475,43.5102));
#263545=CARTESIAN_POINT('Ctrl Pts',(-2.48412401759879E-14,45.4656249999985,
43.5102));
#263546=CARTESIAN_POINT('Ctrl Pts',(0.566167174768376,45.4465902340685,
43.5102));
#263547=CARTESIAN_POINT('Ctrl Pts',(1.12831666969806,45.4262808000092,43.6114309061969));
#263548=CARTESIAN_POINT('Ctrl Pts',(2.23435532889598,45.3833509845901,44.0239215602639));
#263549=CARTESIAN_POINT('Ctrl Pts',(2.76208488292739,45.3611023288806,44.3475011828489));
#263550=CARTESIAN_POINT('Ctrl Pts',(3.67593158760873,45.3186849235856,45.1871891138991));
#263551=CARTESIAN_POINT('Ctrl Pts',(4.04943203210943,45.2968843047985,45.699373099574));
#263552=CARTESIAN_POINT('Ctrl Pts',(4.5696569085592,45.2517488041455,46.8263923479328));
#263553=CARTESIAN_POINT('Ctrl Pts',(4.71644566319283,45.2294776401571,47.4280205599865));
#263554=CARTESIAN_POINT('Ctrl Pts',(4.77366924022708,45.1870137044427,48.6673586058741));
#263555=CARTESIAN_POINT('Ctrl Pts',(4.67825065771643,45.1653022980402,49.2933896217085));
#263556=CARTESIAN_POINT('Ctrl Pts',(4.25428195262986,45.1201885041776,50.4596338382421));
#263557=CARTESIAN_POINT('Ctrl Pts',(3.93474684068767,45.097893833954,50.9904073321232));
#263558=CARTESIAN_POINT('Ctrl Pts',(3.10290584598736,45.055380912789,51.9103453537361));
#263559=CARTESIAN_POINT('Ctrl Pts',(2.59492452463815,45.0337617192976,52.2873404412948));
#263560=CARTESIAN_POINT('Ctrl Pts',(1.47320517645446,44.9886714132759,52.8171150725373));
#263561=CARTESIAN_POINT('Ctrl Pts',(0.872348912097263,44.9663522622886,
52.9692133241848));
#263562=CARTESIAN_POINT('Ctrl Pts',(-0.365654927903947,44.9237878756165,
53.0368711415338));
#263563=CARTESIAN_POINT('Ctrl Pts',(-0.991153230745437,44.9022636356118,
52.9472027181653));
#263564=CARTESIAN_POINT('Ctrl Pts',(-2.16054571570856,44.8571987189914,
52.5343443824203));
#263565=CARTESIAN_POINT('Ctrl Pts',(-2.69469457492828,44.8348541472401,
52.2193747943595));
#263566=CARTESIAN_POINT('Ctrl Pts',(-3.62141790896547,44.7922358051748,
51.3963449289355));
#263567=CARTESIAN_POINT('Ctrl Pts',(-4.00230089366418,44.7708089405814,
50.8930517722628));
#263568=CARTESIAN_POINT('Ctrl Pts',(-4.5427009304037,44.7257714374295,49.7773041716474));
#263569=CARTESIAN_POINT('Ctrl Pts',(-4.70072700271712,44.7034005514389,
49.1773644929565));
#263570=CARTESIAN_POINT('Ctrl Pts',(-4.7800207424564,44.6607257712771,47.9408968826995));
#263571=CARTESIAN_POINT('Ctrl Pts',(-4.69673585831553,44.6393983237826,
47.3159985829078));
#263572=CARTESIAN_POINT('Ctrl Pts',(-4.29625205794725,44.5943903813102,
46.1431750279321));
#263573=CARTESIAN_POINT('Ctrl Pts',(-3.98640446044117,44.5719923468965,
45.6053143854807));
#263574=CARTESIAN_POINT('Ctrl Pts',(-3.17320321784656,44.5292586718744,
44.67108945669));
#263575=CARTESIAN_POINT('Ctrl Pts',(-2.67510132706769,44.5080322394464,
44.2859131457232));
#263576=CARTESIAN_POINT('Ctrl Pts',(-1.5660392602498,44.463056127013,43.7337811473311));
#263577=CARTESIAN_POINT('Ctrl Pts',(-0.967183012353343,44.4406301826481,
43.5691858099604));
#263578=CARTESIAN_POINT('Ctrl Pts',(-0.235766499056439,44.4152792766867,
43.5145836208336));
#263579=CARTESIAN_POINT('Ctrl Pts',(-0.117818553244376,44.4112527733547,
43.5102));
#263580=CARTESIAN_POINT('Ctrl Pts',(-7.35869698509362E-14,44.4072916666655,
43.5102));
#263581=CARTESIAN_POINT('Ctrl Pts',(-7.56339435525888E-15,43.3854166666658,
43.5102));
#263582=CARTESIAN_POINT('Ctrl Pts',(-0.252938767796752,43.393920568789,
43.5102));
#263583=CARTESIAN_POINT('Ctrl Pts',(-0.506033130480092,43.4027110535072,
43.5304032836925));
#263584=CARTESIAN_POINT('Ctrl Pts',(-1.36951656855858,43.433682631352,43.6697769184839));
#263585=CARTESIAN_POINT('Ctrl Pts',(-1.95688726193394,43.4564661935624,
43.8877806596));
#263586=CARTESIAN_POINT('Ctrl Pts',(-3.0088987596432,43.5008325659322,44.5338607011886));
#263587=CARTESIAN_POINT('Ctrl Pts',(-3.46485166642493,43.5209427394167,
44.9535835508775));
#263588=CARTESIAN_POINT('Ctrl Pts',(-4.19533395069392,43.5645559399498,
45.9482322667341));
#263589=CARTESIAN_POINT('Ctrl Pts',(-4.46097731607419,43.5873127911782,
46.5150754942565));
#263590=CARTESIAN_POINT('Ctrl Pts',(-4.75813933136021,43.631744855005,47.7135674872954));
#263591=CARTESIAN_POINT('Ctrl Pts',(-4.78885255595613,43.6519198657488,
48.333280292379));
#263592=CARTESIAN_POINT('Ctrl Pts',(-4.61172004567221,43.69545477968,49.5548054446073));
#263593=CARTESIAN_POINT('Ctrl Pts',(-4.40368282860499,43.7181839244839,
50.1446858243739));
#263594=CARTESIAN_POINT('Ctrl Pts',(-3.77496669460223,43.7626789442838,
51.2077161576424));
#263595=CARTESIAN_POINT('Ctrl Pts',(-3.36166674266701,43.7829261062386,
51.6715392791841));
#263596=CARTESIAN_POINT('Ctrl Pts',(-2.37823063201529,43.826383072085,52.4178722866157));
#263597=CARTESIAN_POINT('Ctrl Pts',(-1.81662634708705,43.8490836771297,
52.6921246523106));
#263598=CARTESIAN_POINT('Ctrl Pts',(-0.622625619824168,43.8936388223162,
53.0089677686183));
#263599=CARTESIAN_POINT('Ctrl Pts',(-0.00191039526407429,43.9139647275044,
53.0496087451274));
#263600=CARTESIAN_POINT('Ctrl Pts',(1.22275842555576,43.9573443645708,52.8912158433007));
#263601=CARTESIAN_POINT('Ctrl Pts',(1.81489342511168,43.9800157646233,52.6927682950152));
#263602=CARTESIAN_POINT('Ctrl Pts',(2.88836171451833,44.0246281409164,52.0808244812262));
#263603=CARTESIAN_POINT('Ctrl Pts',(3.35975143564909,44.0450386063444,51.6737076021931));
#263604=CARTESIAN_POINT('Ctrl Pts',(4.12114558046236,44.088341802955,50.7010837076052));
#263605=CARTESIAN_POINT('Ctrl Pts',(4.40352124978901,44.1109835035808,50.1445962492681));
#263606=CARTESIAN_POINT('Ctrl Pts',(4.73911767096697,44.1556501829775,48.9550459386809));
#263607=CARTESIAN_POINT('Ctrl Pts',(4.78925197630372,44.1761502153229,48.3333793250371));
#263608=CARTESIAN_POINT('Ctrl Pts',(4.64866775580724,44.2193781136552,47.1058472006474));
#263609=CARTESIAN_POINT('Ctrl Pts',(4.45933251114065,44.2419897907378,46.5117141522562));
#263610=CARTESIAN_POINT('Ctrl Pts',(3.86339106873776,44.2867078394907,45.4284743580617));
#263611=CARTESIAN_POINT('Ctrl Pts',(3.46215786932851,44.3073016172265,44.9498969869002));
#263612=CARTESIAN_POINT('Ctrl Pts',(2.49983219570281,44.35045559524,44.1743558263937));
#263613=CARTESIAN_POINT('Ctrl Pts',(1.94827382198002,44.3730370915408,43.8844034463094));
#263614=CARTESIAN_POINT('Ctrl Pts',(0.915635083610503,44.4120410312369,
43.5766189918159));
#263615=CARTESIAN_POINT('Ctrl Pts',(0.458609242083433,44.4283313746079,
43.5102));
#263616=CARTESIAN_POINT('Ctrl Pts',(-9.20097331658098E-14,44.4437499999987,
43.5102));
#263617=CARTESIAN_POINT('Origin',(6.7958239265071E-15,40.475,48.26));
#263618=CARTESIAN_POINT('',(6.38086935278296E-15,46.5239583333315,43.5102));
#263619=CARTESIAN_POINT('',(-9.87175814600512E-15,45.5020833333317,43.5102));
#263620=CARTESIAN_POINT('',(5.54528904550239E-15,40.475,43.5102));
#263621=CARTESIAN_POINT('Ctrl Pts',(6.38378239159465E-15,46.5239583333315,
43.5102));
#263622=CARTESIAN_POINT('Ctrl Pts',(0.605510253896708,46.5036008374102,
43.5102));
#263623=CARTESIAN_POINT('Ctrl Pts',(1.20576070108133,46.4818076969026,43.6259890631561));
#263624=CARTESIAN_POINT('Ctrl Pts',(2.33611695352849,46.4374905918229,44.0793903497507));
#263625=CARTESIAN_POINT('Ctrl Pts',(2.8546727287585,46.4153861300924,44.4147631522863));
#263626=CARTESIAN_POINT('Ctrl Pts',(3.75030468937568,46.3732591906852,45.277567591021));
#263627=CARTESIAN_POINT('Ctrl Pts',(4.11332423204537,46.350867950729,45.8022845225452));
#263628=CARTESIAN_POINT('Ctrl Pts',(4.60492983715419,46.3056097860154,46.944806762349));
#263629=CARTESIAN_POINT('Ctrl Pts',(4.73591436814583,46.283490643379,47.5484595982696));
#263630=CARTESIAN_POINT('Ctrl Pts',(4.76199965834213,46.2413346731749,48.7915354657038));
#263631=CARTESIAN_POINT('Ctrl Pts',(4.6492709525603,46.2190049601663,49.4191198129379));
#263632=CARTESIAN_POINT('Ctrl Pts',(4.19207402121399,46.1737580864564,50.5755587541872));
#263633=CARTESIAN_POINT('Ctrl Pts',(3.85907637047694,46.1516233565398,51.0959986418154));
#263634=CARTESIAN_POINT('Ctrl Pts',(3.00095705659992,46.1094364386808,51.9953552346117));
#263635=CARTESIAN_POINT('Ctrl Pts',(2.47879870234457,46.0871717251068,52.3605222090011));
#263636=CARTESIAN_POINT('Ctrl Pts',(1.33940444906917,46.0419371201451,52.857987662945));
#263637=CARTESIAN_POINT('Ctrl Pts',(0.736131320341591,46.01978586708,52.9921946738508));
#263638=CARTESIAN_POINT('Ctrl Pts',(-0.506210804173773,45.9775659990635,
53.0246397502708));
#263639=CARTESIAN_POINT('Ctrl Pts',(-1.13348286507548,45.9553698123262,
52.9154651892213));
#263640=CARTESIAN_POINT('Ctrl Pts',(-2.29197503236124,45.9101485354608,
52.4650632422378));
#263641=CARTESIAN_POINT('Ctrl Pts',(-2.81455697175483,45.8879797972532,
52.1347948945607));
#263642=CARTESIAN_POINT('Ctrl Pts',(-3.71815798027405,45.8457248934765,
51.2820405739014));
#263643=CARTESIAN_POINT('Ctrl Pts',(-4.08576925695492,45.8236007922176,
50.7628005139273));
#263644=CARTESIAN_POINT('Ctrl Pts',(-4.58990752858198,45.7783939899705,
49.6269971919376));
#263645=CARTESIAN_POINT('Ctrl Pts',(-4.72779263414628,45.7562067826859,
49.0241781630785));
#263646=CARTESIAN_POINT('Ctrl Pts',(-4.76748967906412,45.713914678184,47.7826913112644));
#263647=CARTESIAN_POINT('Ctrl Pts',(-4.66235604747994,45.6918662243994,
47.1557786306744));
#263648=CARTESIAN_POINT('Ctrl Pts',(-4.21969723649514,45.6466751360762,
45.9949770748335));
#263649=CARTESIAN_POINT('Ctrl Pts',(-3.89255399256836,45.6244684589117,
45.4699722245363));
#263650=CARTESIAN_POINT('Ctrl Pts',(-3.04591872211673,45.5821369144204,
44.5615570327065));
#263651=CARTESIAN_POINT('Ctrl Pts',(-2.52999210496112,45.5601676411215,
44.1911767212708));
#263652=CARTESIAN_POINT('Ctrl Pts',(-1.39829579747494,45.5149936043689,
43.6794760641619));
#263653=CARTESIAN_POINT('Ctrl Pts',(-0.796019569019148,45.4927664456731,
43.5374116915685));
#263654=CARTESIAN_POINT('Ctrl Pts',(-0.12223009417209,45.4697508383311,
43.5113786479076));
#263655=CARTESIAN_POINT('Ctrl Pts',(-0.061092202878116,45.4676789441933,
43.5102));
#263656=CARTESIAN_POINT('Ctrl Pts',(-2.52888053375127E-14,45.4656249999985,
43.5102));
#263657=CARTESIAN_POINT('Ctrl Pts',(-9.15240105925363E-14,44.4437499999988,
43.5102));
#263658=CARTESIAN_POINT('Ctrl Pts',(-0.158624669736482,44.4490830245783,
43.5102));
#263659=CARTESIAN_POINT('Ctrl Pts',(-0.317431308334336,44.4545328214472,
43.5181458728693));
#263660=CARTESIAN_POINT('Ctrl Pts',(-1.08959979876912,44.4815761187491,
43.5958913234815));
#263661=CARTESIAN_POINT('Ctrl Pts',(-1.68548201394787,44.5041274378075,
43.7766695169619));
#263662=CARTESIAN_POINT('Ctrl Pts',(-2.77776933643676,44.5489395260632,
44.3575210824682));
#263663=CARTESIAN_POINT('Ctrl Pts',(-3.26309684251495,44.56973002553,44.753216962612));
#263664=CARTESIAN_POINT('Ctrl Pts',(-4.051783932363,44.6127411359467,45.7058479820052));
#263665=CARTESIAN_POINT('Ctrl Pts',(-4.34872785465835,44.6352624336811,
46.2527198271428));
#263666=CARTESIAN_POINT('Ctrl Pts',(-4.71843598020254,44.6801172971878,
47.4337379266126));
#263667=CARTESIAN_POINT('Ctrl Pts',(-4.78593419842782,44.7010091685601,
48.0571184351088));
#263668=CARTESIAN_POINT('Ctrl Pts',(-4.6776312467982,44.7439516944877,49.2895338255929));
#263669=CARTESIAN_POINT('Ctrl Pts',(-4.50480069578428,44.7664432688962,
49.886931026317));
#263670=CARTESIAN_POINT('Ctrl Pts',(-3.93802269071322,44.8113381781622,
50.987511223909));
#263671=CARTESIAN_POINT('Ctrl Pts',(-3.54748413748688,44.8323324157788,
51.4791104293673));
#263672=CARTESIAN_POINT('Ctrl Pts',(-2.6038801946333,44.8752084588662,52.2798918950414));
#263673=CARTESIAN_POINT('Ctrl Pts',(-2.06141002984294,44.897670738244,52.5832244235865));
#263674=CARTESIAN_POINT('Ctrl Pts',(-0.898155571046601,44.942076835292,
52.9635927494952));
#263675=CARTESIAN_POINT('Ctrl Pts',(-0.289169763911568,44.9627764100011,
53.0398339846786));
#263676=CARTESIAN_POINT('Ctrl Pts',(0.947155051174923,45.0054959891908,
52.9569785783018));
#263677=CARTESIAN_POINT('Ctrl Pts',(1.56201031344966,45.0284962665614,52.7897665739497));
#263678=CARTESIAN_POINT('Ctrl Pts',(2.67010924295794,45.0734758495257,52.2350601445252));
#263679=CARTESIAN_POINT('Ctrl Pts',(3.1566752646739,45.0942529077283,51.860825793501));
#263680=CARTESIAN_POINT('Ctrl Pts',(3.97741086967013,45.1369115840165,50.9319524507052));
#263681=CARTESIAN_POINT('Ctrl Pts',(4.29692068710763,45.1599088389433,50.3802709072399));
#263682=CARTESIAN_POINT('Ctrl Pts',(4.69422254308719,45.2049197616779,49.2060407032791));
#263683=CARTESIAN_POINT('Ctrl Pts',(4.77667886664393,45.2257736105637,48.5976543478151));
#263684=CARTESIAN_POINT('Ctrl Pts',(4.7062737351359,45.2683740367192,47.3597165297));
#263685=CARTESIAN_POINT('Ctrl Pts',(4.54499228938658,45.2913678851305,46.7425959716075));
#263686=CARTESIAN_POINT('Ctrl Pts',(4.00068514395364,45.336408018153,45.6283885259323));
#263687=CARTESIAN_POINT('Ctrl Pts',(3.63101697737713,45.3573375096764,45.1380576730592));
#263688=CARTESIAN_POINT('Ctrl Pts',(2.70942297073046,45.3998823651129,44.3079214437182));
#263689=CARTESIAN_POINT('Ctrl Pts',(2.16022155508803,45.4228725062247,43.9829348968804));
#263690=CARTESIAN_POINT('Ctrl Pts',(1.06039337333579,45.4651887079934,43.5995131929415));
#263691=CARTESIAN_POINT('Ctrl Pts',(0.531800571086339,45.4842039863064,
43.5102));
#263692=CARTESIAN_POINT('Ctrl Pts',(-2.62290189567693E-14,45.5020833333317,
43.5102));
#263693=CARTESIAN_POINT('Origin',(6.7958239265071E-15,40.475,48.26));
#263694=CARTESIAN_POINT('',(1.12195103872683E-8,47.58229166591,43.5102));
#263695=CARTESIAN_POINT('',(6.10331359662667E-15,46.5604166666648,43.5102));
#263696=CARTESIAN_POINT('',(5.54528904550239E-15,40.475,43.5102));
#263697=CARTESIAN_POINT('Ctrl Pts',(1.12322018352984E-8,47.5822916662868,
43.5102));
#263698=CARTESIAN_POINT('Ctrl Pts',(0.605267720969338,47.5619423247769,
43.5102000014313));
#263699=CARTESIAN_POINT('Ctrl Pts',(1.20510137850458,47.5401645011038,43.625895412559));
#263700=CARTESIAN_POINT('Ctrl Pts',(2.35644830837524,47.4950292970466,44.0873667724117));
#263701=CARTESIAN_POINT('Ctrl Pts',(2.89251300407666,47.472104481723,44.4393772525011));
#263702=CARTESIAN_POINT('Ctrl Pts',(3.77706893480681,47.4301570353803,45.3160325548261));
#263703=CARTESIAN_POINT('Ctrl Pts',(4.12379833993738,47.4082806115086,45.8253303490186));
#263704=CARTESIAN_POINT('Ctrl Pts',(4.6150508151954,47.3629657401008,46.9696855352565));
#263705=CARTESIAN_POINT('Ctrl Pts',(4.74601126762411,47.3400383819616,47.5973877834963));
#263706=CARTESIAN_POINT('Ctrl Pts',(4.75328333135343,47.298073272432,48.842579413692));
#263707=CARTESIAN_POINT('Ctrl Pts',(4.63917883647753,47.2762280767327,49.447961639768));
#263708=CARTESIAN_POINT('Ctrl Pts',(4.17905205326823,47.2309203610855,50.6049966699414));
#263709=CARTESIAN_POINT('Ctrl Pts',(3.82862449556919,47.207990303116,51.1418729700227));
#263710=CARTESIAN_POINT('Ctrl Pts',(2.95470207981838,47.1660061719569,52.0286520470234));
#263711=CARTESIAN_POINT('Ctrl Pts',(2.44653487105245,47.144194401308,52.3767460972432));
#263712=CARTESIAN_POINT('Ctrl Pts',(1.30394588441443,47.0988944542651,52.8711908667362));
#263713=CARTESIAN_POINT('Ctrl Pts',(0.676834674480104,47.0759615361057,
53.0039774657885));
#263714=CARTESIAN_POINT('Ctrl Pts',(-0.567965482807374,47.0339569365298,
53.0150303299691));
#263715=CARTESIAN_POINT('Ctrl Pts',(-1.17352631992661,47.0121808943154,
52.9028288165141));
#263716=CARTESIAN_POINT('Ctrl Pts',(-2.33164582654648,46.9668893795248,
52.4464835421592));
#263717=CARTESIAN_POINT('Ctrl Pts',(-2.86946112620001,46.9439534386922,
52.0979004933295));
#263718=CARTESIAN_POINT('Ctrl Pts',(-3.75882201964882,46.9019268325604,
51.2271610910263));
#263719=CARTESIAN_POINT('Ctrl Pts',(-4.10850263838956,46.8801889252566,
50.7203080174569));
#263720=CARTESIAN_POINT('Ctrl Pts',(-4.60665335937267,46.8349065609813,
49.5797770653417));
#263721=CARTESIAN_POINT('Ctrl Pts',(-4.74155982148733,46.8119674343811,
48.9533592685247));
#263722=CARTESIAN_POINT('Ctrl Pts',(-4.75700467169291,46.7699171895905,
47.7090206671102));
#263723=CARTESIAN_POINT('Ctrl Pts',(-4.64701236019383,46.7482199214303,
47.1032521937933));
#263724=CARTESIAN_POINT('Ctrl Pts',(-4.19505684768385,46.7029474845507,
45.9438818387575));
#263725=CARTESIAN_POINT('Ctrl Pts',(-3.84861779247138,46.6800050103184,
45.4049841394257));
#263726=CARTESIAN_POINT('Ctrl Pts',(-2.98157626632749,46.6379293986921,
44.5126339235633));
#263727=CARTESIAN_POINT('Ctrl Pts',(-2.47624632147977,46.6162753641057,
44.1611138927457));
#263728=CARTESIAN_POINT('Ctrl Pts',(-1.33810750007046,46.5710136942996,
43.6586740858177));
#263729=CARTESIAN_POINT('Ctrl Pts',(-0.712502002411283,46.5480677140097,
43.5213144103002));
#263730=CARTESIAN_POINT('Ctrl Pts',(-0.0522560520115934,46.5257182038233,
43.5104155107889));
#263731=CARTESIAN_POINT('Ctrl Pts',(-0.0261232309297634,46.5248366067607,
43.5102));
#263732=CARTESIAN_POINT('Ctrl Pts',(7.21644966006352E-15,46.5239583333315,
43.5102));
#263733=CARTESIAN_POINT('Ctrl Pts',(-2.52888053375126E-14,45.5020833333317,
43.5102));
#263734=CARTESIAN_POINT('Ctrl Pts',(-0.0755693305081445,45.504624004324,
43.5102));
#263735=CARTESIAN_POINT('Ctrl Pts',(-0.151201761326261,45.507191911564,
43.5120034428536));
#263736=CARTESIAN_POINT('Ctrl Pts',(-0.858292825623087,45.5314353880608,
43.5458101658749));
#263737=CARTESIAN_POINT('Ctrl Pts',(-1.4773925394437,45.5544215964754,43.7017648941472));
#263738=CARTESIAN_POINT('Ctrl Pts',(-2.59702589034967,45.5995141893973,
44.2367397860407));
#263739=CARTESIAN_POINT('Ctrl Pts',(-3.09072149425917,45.6205900058754,
44.6023308981989));
#263740=CARTESIAN_POINT('Ctrl Pts',(-3.9292133163964,45.6630317591778,45.517397250835));
#263741=CARTESIAN_POINT('Ctrl Pts',(-4.25906430353724,45.6860138769146,
46.0643451032865));
#263742=CARTESIAN_POINT('Ctrl Pts',(-4.67725347512983,45.7311299350528,
47.2330506292479));
#263743=CARTESIAN_POINT('Ctrl Pts',(-4.7702427303392,45.7522758227052,47.8404285882094));
#263744=CARTESIAN_POINT('Ctrl Pts',(-4.72090364611379,45.7946699987669,
49.0809575774807));
#263745=CARTESIAN_POINT('Ctrl Pts',(-4.56969597500102,45.8176479274087,
49.7017773144576));
#263746=CARTESIAN_POINT('Ctrl Pts',(-4.04303230144165,45.862785749986,50.8261985886888));
#263747=CARTESIAN_POINT('Ctrl Pts',(-3.68105632465394,45.8839993325931,
51.3228801778102));
#263748=CARTESIAN_POINT('Ctrl Pts',(-2.7717992805187,45.9263485235755,52.168750196234));
#263749=CARTESIAN_POINT('Ctrl Pts',(-2.22687990283705,45.9493222166802,
52.5028933987043));
#263750=CARTESIAN_POINT('Ctrl Pts',(-1.06053286026439,45.994480207171,52.9297875312537));
#263751=CARTESIAN_POINT('Ctrl Pts',(-0.453572105352478,46.0157589354207,
53.027162436928));
#263752=CARTESIAN_POINT('Ctrl Pts',(0.787983361548988,46.0580656740931,
52.9865801929752));
#263753=CARTESIAN_POINT('Ctrl Pts',(1.41029123865322,46.0810351299836,52.8395736212663));
#263754=CARTESIAN_POINT('Ctrl Pts',(2.53891297590485,46.1262117931469,52.3202616976982));
#263755=CARTESIAN_POINT('Ctrl Pts',(3.03822772092204,46.147552990229,51.9614714595685));
#263756=CARTESIAN_POINT('Ctrl Pts',(3.89057513217224,46.1898197392215,51.0573495813647));
#263757=CARTESIAN_POINT('Ctrl Pts',(4.22848369300769,46.212784994237,50.5142408474255));
#263758=CARTESIAN_POINT('Ctrl Pts',(4.66303233928975,46.2579789325656,49.3499951812477));
#263759=CARTESIAN_POINT('Ctrl Pts',(4.76426216006489,46.2793798352094,48.7433999159282));
#263760=CARTESIAN_POINT('Ctrl Pts',(4.73136914703641,46.3216089782499,47.5009674579344));
#263761=CARTESIAN_POINT('Ctrl Pts',(4.58805767250648,46.3445701005154,46.8773768955343));
#263762=CARTESIAN_POINT('Ctrl Pts',(4.07520970679068,46.3897800102521,45.7450888182641));
#263763=CARTESIAN_POINT('Ctrl Pts',(3.71921141673823,46.4112378051485,45.2434650441426));
#263764=CARTESIAN_POINT('Ctrl Pts',(2.819601717135,46.4534316401482,44.385460078108));
#263765=CARTESIAN_POINT('Ctrl Pts',(2.27809729632468,46.4763887238926,44.0442651253947));
#263766=CARTESIAN_POINT('Ctrl Pts',(1.14689194172361,46.5204002356443,43.6148577984359));
#263767=CARTESIAN_POINT('Ctrl Pts',(0.575671689768406,46.5410623551547,
43.5102));
#263768=CARTESIAN_POINT('Ctrl Pts',(8.04911692853238E-15,46.5604166666648,
43.5102));
#263769=CARTESIAN_POINT('Origin',(6.7958239265071E-15,40.475,48.26));
#263770=CARTESIAN_POINT('',(-3.0122773445189E-8,48.6406250020229,43.5102));
#263771=CARTESIAN_POINT('',(3.44456304422771E-8,47.6187499976816,43.5102));
#263772=CARTESIAN_POINT('',(5.54528904550239E-15,40.475,43.5102));
#263773=CARTESIAN_POINT('Ctrl Pts',(-3.01569111920684E-8,48.6406250010114,
43.5102));
#263774=CARTESIAN_POINT('Ctrl Pts',(0.00846864324595446,48.6403402808376,
43.5101999999462));
#263775=CARTESIAN_POINT('Ctrl Pts',(0.0169383903993272,48.6400552091581,
43.5102226487671));
#263776=CARTESIAN_POINT('Ctrl Pts',(0.636478416209048,48.6191798718932,
43.5135369343409));
#263777=CARTESIAN_POINT('Ctrl Pts',(1.24118429143188,48.5971621151167,43.6346988877366));
#263778=CARTESIAN_POINT('Ctrl Pts',(2.39313666806093,48.5518367752532,44.1083618417949));
#263779=CARTESIAN_POINT('Ctrl Pts',(2.9256635070832,48.5290407974581,44.4647992630245));
#263780=CARTESIAN_POINT('Ctrl Pts',(3.80266330856505,48.4870990846606,45.349041959842));
#263781=CARTESIAN_POINT('Ctrl Pts',(4.14518439984167,48.4650895774633,45.8618125037741));
#263782=CARTESIAN_POINT('Ctrl Pts',(4.62633837758311,48.4197592212302,47.0108112029287));
#263783=CARTESIAN_POINT('Ctrl Pts',(4.75166011105805,48.3969299909334,47.6394713519075));
#263784=CARTESIAN_POINT('Ctrl Pts',(4.74796833627008,48.3550030935466,48.8850094101938));
#263785=CARTESIAN_POINT('Ctrl Pts',(4.62830538735018,48.3330012731708,49.4898621835296));
#263786=CARTESIAN_POINT('Ctrl Pts',(4.15739165130435,48.2876663003646,50.6432398443227));
#263787=CARTESIAN_POINT('Ctrl Pts',(3.80196381608398,48.2648060457194,51.1769600772512));
#263788=CARTESIAN_POINT('Ctrl Pts',(2.91946417246134,48.2228929205492,52.0561151610514));
#263789=CARTESIAN_POINT('Ctrl Pts',(2.40758203843045,48.200898257452,52.3997151384207));
#263790=CARTESIAN_POINT('Ctrl Pts',(1.25945421064558,48.1555590355424,52.8836082121267));
#263791=CARTESIAN_POINT('Ctrl Pts',(0.630673758570287,48.1326698594116,
53.0103761234246));
#263792=CARTESIAN_POINT('Ctrl Pts',(-0.615133469116459,48.0907695298135,
53.0092419608279));
#263793=CARTESIAN_POINT('Ctrl Pts',(-1.22010977350242,48.0687815264716,
52.8908694158124));
#263794=CARTESIAN_POINT('Ctrl Pts',(-2.37462662754409,48.0234417240359,
52.4223591295305));
#263795=CARTESIAN_POINT('Ctrl Pts',(-2.90939118846586,48.0005256061278,
52.0678343904392));
#263796=CARTESIAN_POINT('Ctrl Pts',(-3.7904016183597,47.9586368751837,51.1868357272436));
#263797=CARTESIAN_POINT('Ctrl Pts',(-4.13495748899581,47.9366553425569,
50.6757367096216));
#263798=CARTESIAN_POINT('Ctrl Pts',(-4.62111654763354,47.8913170826427,
49.5285760969698));
#263799=CARTESIAN_POINT('Ctrl Pts',(-4.74916318677378,47.868399000331,48.8999428065475));
#263800=CARTESIAN_POINT('Ctrl Pts',(-4.7504075112079,47.8264972255023,47.6541382226685));
#263801=CARTESIAN_POINT('Ctrl Pts',(-4.6332666990797,47.8045392147509,47.0490405340914));
#263802=CARTESIAN_POINT('Ctrl Pts',(-4.16710603943454,47.7592060980522,
45.893749292367));
#263803=CARTESIAN_POINT('Ctrl Pts',(-3.8137400149553,47.7362859153077,45.3583838722653));
#263804=CARTESIAN_POINT('Ctrl Pts',(-2.93474341586644,47.694370056637,44.4757372773048));
#263805=CARTESIAN_POINT('Ctrl Pts',(-2.42447534136177,47.6724373335368,
44.1301787960158));
#263806=CARTESIAN_POINT('Ctrl Pts',(-1.27860763790831,47.6271098037818,
43.64166888973));
#263807=CARTESIAN_POINT('Ctrl Pts',(-0.650402238452651,47.6041873785707,
43.5122773754931));
#263808=CARTESIAN_POINT('Ctrl Pts',(-0.0102342257257289,47.5826358605589,
43.5102082686246));
#263809=CARTESIAN_POINT('Ctrl Pts',(-0.0051169169184957,47.5824636994492,
43.5101999999879));
#263810=CARTESIAN_POINT('Ctrl Pts',(1.12322026959339E-8,47.5822916662868,
43.5102));
#263811=CARTESIAN_POINT('Ctrl Pts',(6.66133814775094E-15,46.5604166666648,
43.5102));
#263812=CARTESIAN_POINT('Ctrl Pts',(-0.0333164514064297,46.5615367790316,
43.5102));
#263813=CARTESIAN_POINT('Ctrl Pts',(-0.0666474877696299,46.5626622633207,
43.5105505358004));
#263814=CARTESIAN_POINT('Ctrl Pts',(-0.733745769363326,46.5852859802539,
43.5245966824763));
#263815=CARTESIAN_POINT('Ctrl Pts',(-1.35843845899671,46.6082391406888,
43.6646756633582));
#263816=CARTESIAN_POINT('Ctrl Pts',(-2.4939124693873,46.6534774353481,44.1718703706464));
#263817=CARTESIAN_POINT('Ctrl Pts',(-2.99755105650462,46.6750405296682,
44.5254336623435));
#263818=CARTESIAN_POINT('Ctrl Pts',(-3.86047541902279,46.7171702744801,
45.4210993924352));
#263819=CARTESIAN_POINT('Ctrl Pts',(-4.20452601484658,46.7401196432354,
45.9611914936807));
#263820=CARTESIAN_POINT('Ctrl Pts',(-4.65159836673592,46.7853705168099,
47.1219431444154));
#263821=CARTESIAN_POINT('Ctrl Pts',(-4.75913295039592,46.8069820603204,
47.7279429848328));
#263822=CARTESIAN_POINT('Ctrl Pts',(-4.73879860375981,46.849082831204,48.9717591309175));
#263823=CARTESIAN_POINT('Ctrl Pts',(-4.60153407961421,46.8720285523031,
49.5973963322301));
#263824=CARTESIAN_POINT('Ctrl Pts',(-4.09926063963529,46.9172910317212,
50.7356281460623));
#263825=CARTESIAN_POINT('Ctrl Pts',(-3.74781202137065,46.9389482871537,
51.2410172153012));
#263826=CARTESIAN_POINT('Ctrl Pts',(-2.85557778141026,46.9810220010192,
52.1082024576284));
#263827=CARTESIAN_POINT('Ctrl Pts',(-2.31672197870818,47.0039642273675,
52.4547248602009));
#263828=CARTESIAN_POINT('Ctrl Pts',(-1.15740005626589,47.0492374108295,
52.9068509099192));
#263829=CARTESIAN_POINT('Ctrl Pts',(-0.551639655503142,47.0709377090647,
53.0169290494783));
#263830=CARTESIAN_POINT('Ctrl Pts',(0.692717019936865,47.1129861845493,
53.0016548841551));
#263831=CARTESIAN_POINT('Ctrl Pts',(1.31916190182874,47.1359250749043,52.8668307754809));
#263832=CARTESIAN_POINT('Ctrl Pts',(2.45977296165077,47.1812081274254,52.3688240300641));
#263833=CARTESIAN_POINT('Ctrl Pts',(2.96667712210168,47.2029488802598,52.019205096725));
#263834=CARTESIAN_POINT('Ctrl Pts',(3.83754039304105,47.2449738385225,51.1299445253105));
#263835=CARTESIAN_POINT('Ctrl Pts',(4.18619523897202,47.2679095549076,50.5921656409225));
#263836=CARTESIAN_POINT('Ctrl Pts',(4.6426876218868,47.3132017039919,49.4340882023268));
#263837=CARTESIAN_POINT('Ctrl Pts',(4.75496316694537,47.3349804140488,48.8285343178734));
#263838=CARTESIAN_POINT('Ctrl Pts',(4.74405742910957,47.3769834803082,47.5837188255907));
#263839=CARTESIAN_POINT('Ctrl Pts',(4.61134187087939,47.3999161858311,46.9565845142134));
#263840=CARTESIAN_POINT('Ctrl Pts',(4.11702129093406,47.4452167173043,45.8139267033713));
#263841=CARTESIAN_POINT('Ctrl Pts',(3.76898036413946,47.4670309854212,45.305715487294));
#263842=CARTESIAN_POINT('Ctrl Pts',(2.88228778831814,47.5090136911056,44.4316865997081));
#263843=CARTESIAN_POINT('Ctrl Pts',(2.34544301461838,47.5319435481428,44.0811973591388));
#263844=CARTESIAN_POINT('Ctrl Pts',(1.19688904259188,47.5769211080058,43.6243033168789));
#263845=CARTESIAN_POINT('Ctrl Pts',(0.601088508161882,47.5985411648686,
43.5102000043641));
#263846=CARTESIAN_POINT('Ctrl Pts',(3.44846856625836E-8,47.6187499988384,
43.5102));
#263847=CARTESIAN_POINT('Origin',(6.7958239265071E-15,40.475,48.26));
#263848=CARTESIAN_POINT('',(5.54528904550239E-15,49.238,43.5102));
#263849=CARTESIAN_POINT('',(-1.00167620060974E-8,48.6770833340043,43.5102));
#263850=CARTESIAN_POINT('',(5.54528904550239E-15,40.475,43.5102));
#263851=CARTESIAN_POINT('',(1.86990303000813,49.238,52.6262412551721));
#263852=CARTESIAN_POINT('Origin',(6.7958239265071E-15,49.238,48.26));
#263853=CARTESIAN_POINT('Ctrl Pts',(1.86990303000838,49.238,52.626241255172));
#263854=CARTESIAN_POINT('Ctrl Pts',(1.56383729601047,49.2258845683299,52.7573181265442));
#263855=CARTESIAN_POINT('Ctrl Pts',(1.24484153160777,49.2137876533848,52.8558494941654));
#263856=CARTESIAN_POINT('Ctrl Pts',(0.598087148393397,49.1902689990312,
52.9832738225069));
#263857=CARTESIAN_POINT('Ctrl Pts',(0.272399227164127,49.1789970034025,
53.0131869119213));
#263858=CARTESIAN_POINT('Ctrl Pts',(-0.665150328710527,49.1473284546882,
53.0025766190358));
#263859=CARTESIAN_POINT('Ctrl Pts',(-1.26947276028821,49.1252713731853,
52.8776651208351));
#263860=CARTESIAN_POINT('Ctrl Pts',(-2.4178439523169,49.0799708480804,52.3971383205351));
#263861=CARTESIAN_POINT('Ctrl Pts',(-2.94738751121186,49.0573327453721,
52.0381816129474));
#263862=CARTESIAN_POINT('Ctrl Pts',(-3.81898351389284,49.0153198975399,
51.1495847597557));
#263863=CARTESIAN_POINT('Ctrl Pts',(-4.15879206820495,48.9932736680055,
50.6345983826297));
#263864=CARTESIAN_POINT('Ctrl Pts',(-4.63308233656813,48.9479661434788,
49.4834357447574));
#263865=CARTESIAN_POINT('Ctrl Pts',(-4.75478602763426,48.9252845812558,
48.8550795761242));
#263866=CARTESIAN_POINT('Ctrl Pts',(-4.74468294064049,48.8832914499036,
47.6102271173403));
#263867=CARTESIAN_POINT('Ctrl Pts',(-4.62178279031773,48.8612553675669,
47.0056961541918));
#263868=CARTESIAN_POINT('Ctrl Pts',(-4.14493564252529,48.8159414036286,
45.8554010775775));
#263869=CARTESIAN_POINT('Ctrl Pts',(-3.78732928008356,48.7932191294468,
45.3242575343515));
#263870=CARTESIAN_POINT('Ctrl Pts',(-2.90106707411062,48.7512443740699,
44.4497605377253));
#263871=CARTESIAN_POINT('Ctrl Pts',(-2.38726818569504,48.7292177706584,
44.1084944446942));
#263872=CARTESIAN_POINT('Ctrl Pts',(-1.24508730776246,48.6842061952532,
43.6337718041888));
#263873=CARTESIAN_POINT('Ctrl Pts',(-0.625530370510309,48.6616555802689,
43.5102000039715));
#263874=CARTESIAN_POINT('Ctrl Pts',(-3.0156908498169E-8,48.6406250010113,
43.5102));
#263875=CARTESIAN_POINT('Ctrl Pts',(3.44846877406766E-8,47.6187499988384,
43.5102));
#263876=CARTESIAN_POINT('Ctrl Pts',(-0.00908423608736038,47.6190554156343,
43.510199999934));
#263877=CARTESIAN_POINT('Ctrl Pts',(-0.0181696901681403,47.6193612351469,
43.5102260611621));
#263878=CARTESIAN_POINT('Ctrl Pts',(-0.662136500168755,47.6410631179696,
43.5139214564745));
#263879=CARTESIAN_POINT('Ctrl Pts',(-1.28985842539348,47.6639902866762,
43.6448208016811));
#263880=CARTESIAN_POINT('Ctrl Pts',(-2.43427260627819,47.7093056539372,
44.1359664574956));
#263881=CARTESIAN_POINT('Ctrl Pts',(-2.94360820937189,47.7311842575742,
44.4826502313427));
#263882=CARTESIAN_POINT('Ctrl Pts',(-3.82035481584433,47.7731304748415,
45.3671317852293));
#263883=CARTESIAN_POINT('Ctrl Pts',(-4.17241816830197,47.7960551119495,
45.9031692796597));
#263884=CARTESIAN_POINT('Ctrl Pts',(-4.63590244033901,47.841377030083,47.0592360290114));
#263885=CARTESIAN_POINT('Ctrl Pts',(-4.75169647666858,47.8632846262196,
47.6644598597264));
#263886=CARTESIAN_POINT('Ctrl Pts',(-4.74777924466011,47.9052145427421,
48.9099943312856));
#263887=CARTESIAN_POINT('Ctrl Pts',(-4.61844016403301,47.9281368006108,
49.5382164720461));
#263888=CARTESIAN_POINT('Ctrl Pts',(-4.13002191265821,47.9734647507916,
50.6841346452883));
#263889=CARTESIAN_POINT('Ctrl Pts',(-3.78450253960804,47.9953993673611,
51.1944351295961));
#263890=CARTESIAN_POINT('Ctrl Pts',(-2.90191974348767,48.037314169267,52.0735098685414));
#263891=CARTESIAN_POINT('Ctrl Pts',(-2.36657772452895,48.0602341951522,
52.4269211246317));
#263892=CARTESIAN_POINT('Ctrl Pts',(-1.21131348071913,48.1055676989055,
52.8931747566162));
#263893=CARTESIAN_POINT('Ctrl Pts',(-0.606220172193079,48.1275274716681,
53.0103623527893));
#263894=CARTESIAN_POINT('Ctrl Pts',(0.639593744247375,48.1694282675114,
53.0092108581362));
#263895=CARTESIAN_POINT('Ctrl Pts',(1.26824126498937,48.1923462030235,52.8812091154102));
#263896=CARTESIAN_POINT('Ctrl Pts',(2.41536511316397,48.237681662734,52.3951623765016));
#263897=CARTESIAN_POINT('Ctrl Pts',(2.92650865236586,48.2596639329101,52.0506691843573));
#263898=CARTESIAN_POINT('Ctrl Pts',(3.80756031737863,48.3015532619483,51.1697271236068));
#263899=CARTESIAN_POINT('Ctrl Pts',(4.16214899822401,48.3244673767911,50.6350159036465));
#263900=CARTESIAN_POINT('Ctrl Pts',(4.63077827583646,48.3698102209431,49.4804578650776));
#263901=CARTESIAN_POINT('Ctrl Pts',(4.7491968666976,48.3917987188872,48.875485922136));
#263902=CARTESIAN_POINT('Ctrl Pts',(4.75042231280387,48.4336999981435,47.6296882588277));
#263903=CARTESIAN_POINT('Ctrl Pts',(4.62370604511392,48.4565870245828,47.0009120908311));
#263904=CARTESIAN_POINT('Ctrl Pts',(4.13991074199344,48.5019259324576,45.8527531057461));
#263905=CARTESIAN_POINT('Ctrl Pts',(3.79634923939821,48.523921127265,45.3408392198354));
#263906=CARTESIAN_POINT('Ctrl Pts',(2.91727107546832,48.5658352748234,44.4582773051987));
#263907=CARTESIAN_POINT('Ctrl Pts',(2.38359346820129,48.588693222624,44.1028133915149));
#263908=CARTESIAN_POINT('Ctrl Pts',(1.23026664392749,48.6340278542552,43.6318014243512));
#263909=CARTESIAN_POINT('Ctrl Pts',(0.625419053720088,48.6560302458643,
43.5120849431335));
#263910=CARTESIAN_POINT('Ctrl Pts',(0.00965498329080251,48.6767586264632,
43.510207359137));
#263911=CARTESIAN_POINT('Ctrl Pts',(0.00482730997582324,48.6769210372467,
43.5101999999898));
#263912=CARTESIAN_POINT('Ctrl Pts',(-1.00281259683004E-8,48.6770833336679,
43.5102));
#263913=CARTESIAN_POINT('Origin',(6.7958239265071E-15,42.09425,48.26));
#263914=CARTESIAN_POINT('',(4.66579641623065,42.0671867061318,47.5288462557477));
#263915=CARTESIAN_POINT('Origin',(-0.0419539454484924,42.0904940530822,
48.1587073448045));
#263916=CARTESIAN_POINT('',(4.68628896694498,42.0671867061318,47.6743911597878));
#263917=CARTESIAN_POINT('Origin',(1.58033521102663E-6,42.0671867060952,
48.2599997745674));
#263918=CARTESIAN_POINT('Origin',(-0.157122447866724,42.1434096703623,47.879511098682));
#263919=CARTESIAN_POINT('',(5.97160775493582E-15,40.475,45.12945));
#263920=CARTESIAN_POINT('',(5.54528904550239E-15,42.09425,43.5102));
#263921=CARTESIAN_POINT('Origin',(6.7958239265071E-15,40.475,48.26));
#263922=CARTESIAN_POINT('Origin',(6.7958239265071E-15,50.,48.26));
#263923=CARTESIAN_POINT('',(0.908077042619364,49.238,52.9221879117715));
#263924=CARTESIAN_POINT('',(6.88299333419379E-15,49.238,53.0098));
#263925=CARTESIAN_POINT('Origin',(6.7958239265071E-15,49.238,48.26));
#263926=CARTESIAN_POINT('Origin',(-0.101290884807203,49.2622522741402,48.3019587266354));
#263927=CARTESIAN_POINT('Origin',(-0.380373159828188,49.2681001647224,48.4181119225168));
#263928=CARTESIAN_POINT('Origin',(6.7958239265071E-15,49.238,48.26));
#263929=CARTESIAN_POINT('',(6.86900893723871E-15,50.,52.2478));
#263930=CARTESIAN_POINT('',(6.86900893723871E-15,50.,52.2478));
#263931=CARTESIAN_POINT('Origin',(6.7958239265071E-15,50.,48.26));
#263932=CARTESIAN_POINT('Origin',(6.7958239265071E-15,40.475,48.26));
#263933=CARTESIAN_POINT('Ctrl Pts',(-1.00281261072865E-8,48.6770833336679,
43.5102));
#263934=CARTESIAN_POINT('Ctrl Pts',(-0.629672755148192,48.6982531821869,
43.5102000013294));
#263935=CARTESIAN_POINT('Ctrl Pts',(-1.25321726916232,48.7209607258464,
43.6354136739496));
#263936=CARTESIAN_POINT('Ctrl Pts',(-2.39779765932932,48.766114985687,44.1145892634232));
#263937=CARTESIAN_POINT('Ctrl Pts',(-2.91060499549369,48.7881251061508,
44.4570655678299));
#263938=CARTESIAN_POINT('Ctrl Pts',(-3.79491991104055,48.8300680020356,
45.3339759730056));
#263939=CARTESIAN_POINT('Ctrl Pts',(-4.15139914837991,48.8528613299139,
45.86645335616));
#263940=CARTESIAN_POINT('Ctrl Pts',(-4.62517599058953,48.8981862669499,
47.0183465771293));
#263941=CARTESIAN_POINT('Ctrl Pts',(-4.74640007620397,48.9202046816236,
47.6230462847408));
#263942=CARTESIAN_POINT('Ctrl Pts',(-4.75318456347165,48.9621635943342,
48.8682555584807));
#263943=CARTESIAN_POINT('Ctrl Pts',(-4.62960939173144,48.9849211271636,
49.4967694962143));
#263944=CARTESIAN_POINT('Ctrl Pts',(-4.15176681390835,49.0302405779038,
50.6468154508051));
#263945=CARTESIAN_POINT('Ctrl Pts',(-3.81055277871335,49.0522678865187,
51.1606568777446));
#263946=CARTESIAN_POINT('Ctrl Pts',(-2.93615950038935,49.094244007631,52.0470026674717));
#263947=CARTESIAN_POINT('Ctrl Pts',(-2.40507322360229,49.1169632491863,
52.4046573926874));
#263948=CARTESIAN_POINT('Ctrl Pts',(-1.38668037731136,49.1570831197733,
52.8269672384587));
#263949=CARTESIAN_POINT('Ctrl Pts',(-0.929744443721774,49.1740393274787,
52.9414176733624));
#263950=CARTESIAN_POINT('Ctrl Pts',(-0.00555594936379633,49.2063727902452,
53.0320305704281));
#263951=CARTESIAN_POINT('Ctrl Pts',(0.456439282085028,49.2215907184063,
53.0101555976912));
#263952=CARTESIAN_POINT('Ctrl Pts',(0.908077042619743,49.238,52.9221879117714));
#263953=CARTESIAN_POINT('Origin',(6.7958239265071E-15,40.475,48.26));
#263954=CARTESIAN_POINT('Origin',(6.7958239265071E-15,50.,48.26));
#263955=CARTESIAN_POINT('',(1.000194405918E-14,50.,51.0096306570156));
#263956=CARTESIAN_POINT('',(2.38125000000001,50.,49.6348153285078));
#263957=CARTESIAN_POINT('Origin',(6.7958239265071E-15,50.,48.26));
#263958=CARTESIAN_POINT('',(-2.38124999999999,50.,49.6348153285078));
#263959=CARTESIAN_POINT('Origin',(6.7958239265071E-15,50.,48.26));
#263960=CARTESIAN_POINT('',(-2.38125,50.,46.8851846714922));
#263961=CARTESIAN_POINT('Origin',(6.7958239265071E-15,50.,48.26));
#263962=CARTESIAN_POINT('',(9.22755509075881E-15,50.,45.5103693429844));
#263963=CARTESIAN_POINT('Origin',(6.7958239265071E-15,50.,48.26));
#263964=CARTESIAN_POINT('',(2.38125000000001,50.,46.8851846714922));
#263965=CARTESIAN_POINT('Origin',(6.7958239265071E-15,50.,48.26));
#263966=CARTESIAN_POINT('Origin',(6.7958239265071E-15,50.,48.26));
#263967=CARTESIAN_POINT('Origin',(6.7958239265071E-15,50.,48.26));
#263968=CARTESIAN_POINT('Ctrl Pts',(-8.35153880681623E-13,50.0000000000005,
51.0096306570161));
#263969=CARTESIAN_POINT('Ctrl Pts',(1.19062500000002,49.3125923357457,50.3222229927617));
#263970=CARTESIAN_POINT('Ctrl Pts',(2.38125000000088,50.0000000000005,49.6348153285073));
#263971=CARTESIAN_POINT('Origin',(6.7958239265071E-15,50.,48.26));
#263972=CARTESIAN_POINT('Ctrl Pts',(2.38125000000001,50.0000000000005,49.6348153285088));
#263973=CARTESIAN_POINT('Ctrl Pts',(2.38125000000001,49.3125923357457,48.26));
#263974=CARTESIAN_POINT('Ctrl Pts',(2.38125000000001,50.0000000000005,46.8851846714912));
#263975=CARTESIAN_POINT('Origin',(6.7958239265071E-15,50.,48.26));
#263976=CARTESIAN_POINT('Ctrl Pts',(2.38125000000087,50.0000000000005,46.8851846714927));
#263977=CARTESIAN_POINT('Ctrl Pts',(1.19062500000001,49.3125923357457,46.1977770072383));
#263978=CARTESIAN_POINT('Ctrl Pts',(-8.54108254788434E-13,50.0000000000005,
45.5103693429839));
#263979=CARTESIAN_POINT('Origin',(6.7958239265071E-15,50.,48.26));
#263980=CARTESIAN_POINT('Ctrl Pts',(8.99821745281327E-13,50.0000000000005,
45.5103693429839));
#263981=CARTESIAN_POINT('Ctrl Pts',(-1.19062499999999,49.3125923357457,
46.1977770072383));
#263982=CARTESIAN_POINT('Ctrl Pts',(-2.38125000000087,50.0000000000005,
46.8851846714927));
#263983=CARTESIAN_POINT('Origin',(6.7958239265071E-15,50.,48.26));
#263984=CARTESIAN_POINT('Ctrl Pts',(-2.38124999999999,50.0000000000005,
46.8851846714912));
#263985=CARTESIAN_POINT('Ctrl Pts',(-2.38124999999999,49.3125923357457,
48.26));
#263986=CARTESIAN_POINT('Ctrl Pts',(-2.38124999999999,50.0000000000005,
49.6348153285088));
#263987=CARTESIAN_POINT('Origin',(6.7958239265071E-15,50.,48.26));
#263988=CARTESIAN_POINT('Ctrl Pts',(-2.38125000000084,50.0000000000005,
49.6348153285073));
#263989=CARTESIAN_POINT('Ctrl Pts',(-1.19062499999998,49.3125923357457,
50.3222229927617));
#263990=CARTESIAN_POINT('Ctrl Pts',(8.74084678479433E-13,50.0000000000005,
51.0096306570161));
#263991=CARTESIAN_POINT('Origin',(-2.38124999999999,46.428125,49.6348153285078));
#263992=CARTESIAN_POINT('',(-2.38124999999999,46.428125,49.6348153285078));
#263993=CARTESIAN_POINT('',(7.34564873659056E-15,46.428125,51.0096306570156));
#263994=CARTESIAN_POINT('',(7.34564873659056E-15,46.428125,51.0096306570156));
#263995=CARTESIAN_POINT('',(2.38125000000001,46.428125,49.6348153285078));
#263996=CARTESIAN_POINT('',(2.38125000000001,46.428125,49.6348153285078));
#263997=CARTESIAN_POINT('',(2.38125000000001,46.428125,46.8851846714922));
#263998=CARTESIAN_POINT('',(2.38125000000001,46.428125,46.8851846714922));
#263999=CARTESIAN_POINT('',(6.57125976816934E-15,46.428125,45.5103693429844));
#264000=CARTESIAN_POINT('',(6.57125976816934E-15,46.428125,45.5103693429844));
#264001=CARTESIAN_POINT('',(-2.38124999999999,46.428125,46.8851846714922));
#264002=CARTESIAN_POINT('',(-2.38124999999999,46.428125,46.8851846714922));
#264003=CARTESIAN_POINT('',(-2.38124999999999,46.428125,49.6348153285078));
#264004=CARTESIAN_POINT('Origin',(2.38125000000001,46.428125,49.6348153285078));
#264005=CARTESIAN_POINT('',(7.34564873659056E-15,46.428125,51.0096306570156));
#264006=CARTESIAN_POINT('',(2.38125000000001,46.428125,49.6348153285078));
#264007=CARTESIAN_POINT('Origin',(2.38125000000001,46.428125,46.8851846714922));
#264008=CARTESIAN_POINT('',(2.38125000000001,46.428125,46.8851846714922));
#264009=CARTESIAN_POINT('Origin',(6.57125976816934E-15,46.428125,45.5103693429844));
#264010=CARTESIAN_POINT('',(6.57125976816934E-15,46.428125,45.5103693429844));
#264011=CARTESIAN_POINT('Origin',(-2.38124999999999,46.428125,46.8851846714922));
#264012=CARTESIAN_POINT('',(-2.38124999999999,46.428125,46.8851846714922));
#264013=CARTESIAN_POINT('Origin',(-2.38124999999999,46.428125,49.6348153285078));
#264014=CARTESIAN_POINT('',(-2.38124999999999,46.428125,49.6348153285078));
#264015=CARTESIAN_POINT('Origin',(7.34564873659056E-15,46.428125,51.0096306570156));
#264016=CARTESIAN_POINT('Ctrl Pts',(-4.72273670613182,40.459375,48.26));
#264017=CARTESIAN_POINT('Ctrl Pts',(-4.72273670613182,40.5255208333334,
50.216221595197));
#264018=CARTESIAN_POINT('Ctrl Pts',(-3.33947915066443,40.5916666666667,
51.5994791506644));
#264019=CARTESIAN_POINT('Ctrl Pts',(-1.95622159519703,40.6578125,52.9827367061318));
#264020=CARTESIAN_POINT('Ctrl Pts',(7.17168088200107E-15,40.7239583333333,
52.9827367061318));
#264021=CARTESIAN_POINT('Ctrl Pts',(1.95622159519705,40.7901041666666,52.9827367061318));
#264022=CARTESIAN_POINT('Ctrl Pts',(3.33947915066444,40.8562499999999,51.5994791506644));
#264023=CARTESIAN_POINT('Ctrl Pts',(4.72273670613183,40.9223958333332,50.216221595197));
#264024=CARTESIAN_POINT('Ctrl Pts',(4.72273670613183,40.9885416666665,48.26));
#264025=CARTESIAN_POINT('Ctrl Pts',(4.72273670613183,41.0546874999999,46.303778404803));
#264026=CARTESIAN_POINT('Ctrl Pts',(3.33947915066444,41.1208333333332,44.9205208493356));
#264027=CARTESIAN_POINT('Ctrl Pts',(1.95622159519705,41.1869791666665,43.5372632938682));
#264028=CARTESIAN_POINT('Ctrl Pts',(6.99833541005117E-15,41.2531249999998,
43.5372632938682));
#264029=CARTESIAN_POINT('Ctrl Pts',(-1.95622159519704,41.3192708333331,
43.5372632938682));
#264030=CARTESIAN_POINT('Ctrl Pts',(-3.33947915066443,41.3854166666664,
44.9205208493356));
#264031=CARTESIAN_POINT('Ctrl Pts',(-4.72273670613182,41.4515624999997,
46.303778404803));
#264032=CARTESIAN_POINT('Ctrl Pts',(-4.72273670613182,41.517708333333,48.26));
#264033=CARTESIAN_POINT('Ctrl Pts',(-4.72273670613182,41.5838541666664,
50.216221595197));
#264034=CARTESIAN_POINT('Ctrl Pts',(-3.33947915066443,41.6499999999997,
51.5994791506644));
#264035=CARTESIAN_POINT('Ctrl Pts',(-1.95622159519703,41.716145833333,52.9827367061318));
#264036=CARTESIAN_POINT('Ctrl Pts',(7.17168088200104E-15,41.7822916666663,
52.9827367061318));
#264037=CARTESIAN_POINT('Ctrl Pts',(1.95622159519705,41.8484374999996,52.9827367061318));
#264038=CARTESIAN_POINT('Ctrl Pts',(3.33947915066444,41.9145833333329,51.5994791506644));
#264039=CARTESIAN_POINT('Ctrl Pts',(4.72273670613183,41.9807291666662,50.216221595197));
#264040=CARTESIAN_POINT('Ctrl Pts',(4.72273670613183,42.0468749999996,48.26));
#264041=CARTESIAN_POINT('Ctrl Pts',(4.72273670613183,42.1130208333329,46.303778404803));
#264042=CARTESIAN_POINT('Ctrl Pts',(3.33947915066444,42.1791666666662,44.9205208493356));
#264043=CARTESIAN_POINT('Ctrl Pts',(1.95622159519705,42.2453124999995,43.5372632938682));
#264044=CARTESIAN_POINT('Ctrl Pts',(6.9983354100512E-15,42.3114583333328,
43.5372632938682));
#264045=CARTESIAN_POINT('Ctrl Pts',(-1.95622159519704,42.3776041666661,
43.5372632938682));
#264046=CARTESIAN_POINT('Ctrl Pts',(-3.33947915066443,42.4437499999994,
44.9205208493356));
#264047=CARTESIAN_POINT('Ctrl Pts',(-4.72273670613182,42.5098958333327,
46.303778404803));
#264048=CARTESIAN_POINT('Ctrl Pts',(-4.72273670613182,42.5760416666661,
48.26));
#264049=CARTESIAN_POINT('Ctrl Pts',(-4.72273670613182,42.6421874999994,
50.216221595197));
#264050=CARTESIAN_POINT('Ctrl Pts',(-3.33947915066443,42.7083333333327,
51.5994791506644));
#264051=CARTESIAN_POINT('Ctrl Pts',(-1.95622159519703,42.774479166666,52.9827367061318));
#264052=CARTESIAN_POINT('Ctrl Pts',(7.17168088200104E-15,42.8406249999993,
52.9827367061318));
#264053=CARTESIAN_POINT('Ctrl Pts',(1.95622159519705,42.9067708333326,52.9827367061318));
#264054=CARTESIAN_POINT('Ctrl Pts',(3.33947915066444,42.9729166666659,51.5994791506644));
#264055=CARTESIAN_POINT('Ctrl Pts',(4.72273670613183,43.0390624999992,50.216221595197));
#264056=CARTESIAN_POINT('Ctrl Pts',(4.72273670613183,43.1052083333326,48.26));
#264057=CARTESIAN_POINT('Ctrl Pts',(4.72273670613183,43.1713541666659,46.303778404803));
#264058=CARTESIAN_POINT('Ctrl Pts',(3.33947915066444,43.2374999999992,44.9205208493356));
#264059=CARTESIAN_POINT('Ctrl Pts',(1.95622159519705,43.3036458333325,43.5372632938682));
#264060=CARTESIAN_POINT('Ctrl Pts',(6.99833541005117E-15,43.3697916666658,
43.5372632938682));
#264061=CARTESIAN_POINT('Ctrl Pts',(-1.95622159519704,43.4359374999991,
43.5372632938682));
#264062=CARTESIAN_POINT('Ctrl Pts',(-3.33947915066443,43.5020833333324,
44.9205208493356));
#264063=CARTESIAN_POINT('Ctrl Pts',(-4.72273670613182,43.5682291666657,
46.303778404803));
#264064=CARTESIAN_POINT('Ctrl Pts',(-4.72273670613182,43.634374999999,48.26));
#264065=CARTESIAN_POINT('Ctrl Pts',(-4.72273670613182,43.7005208333324,
50.216221595197));
#264066=CARTESIAN_POINT('Ctrl Pts',(-3.33947915066443,43.7666666666657,
51.5994791506644));
#264067=CARTESIAN_POINT('Ctrl Pts',(-1.95622159519703,43.832812499999,52.9827367061318));
#264068=CARTESIAN_POINT('Ctrl Pts',(7.17168088200102E-15,43.8989583333323,
52.9827367061318));
#264069=CARTESIAN_POINT('Ctrl Pts',(1.95622159519705,43.9651041666656,52.9827367061318));
#264070=CARTESIAN_POINT('Ctrl Pts',(3.33947915066444,44.0312499999989,51.5994791506644));
#264071=CARTESIAN_POINT('Ctrl Pts',(4.72273670613183,44.0973958333322,50.216221595197));
#264072=CARTESIAN_POINT('Ctrl Pts',(4.72273670613183,44.1635416666656,48.26));
#264073=CARTESIAN_POINT('Ctrl Pts',(4.72273670613183,44.2296874999989,46.303778404803));
#264074=CARTESIAN_POINT('Ctrl Pts',(3.33947915066444,44.2958333333322,44.9205208493356));
#264075=CARTESIAN_POINT('Ctrl Pts',(1.95622159519705,44.3619791666655,43.5372632938682));
#264076=CARTESIAN_POINT('Ctrl Pts',(6.99833541005117E-15,44.4281249999988,
43.5372632938682));
#264077=CARTESIAN_POINT('Ctrl Pts',(-1.95622159519704,44.4942708333321,
43.5372632938682));
#264078=CARTESIAN_POINT('Ctrl Pts',(-3.33947915066443,44.5604166666654,
44.9205208493356));
#264079=CARTESIAN_POINT('Ctrl Pts',(-4.72273670613182,44.6265624999987,
46.303778404803));
#264080=CARTESIAN_POINT('Ctrl Pts',(-4.72273670613182,44.692708333332,48.26));
#264081=CARTESIAN_POINT('Ctrl Pts',(-4.72273670613182,44.7588541666654,
50.216221595197));
#264082=CARTESIAN_POINT('Ctrl Pts',(-3.33947915066443,44.8249999999987,
51.5994791506644));
#264083=CARTESIAN_POINT('Ctrl Pts',(-1.95622159519703,44.891145833332,52.9827367061318));
#264084=CARTESIAN_POINT('Ctrl Pts',(7.17168088200107E-15,44.9572916666653,
52.9827367061318));
#264085=CARTESIAN_POINT('Ctrl Pts',(1.95622159519705,45.0234374999986,52.9827367061318));
#264086=CARTESIAN_POINT('Ctrl Pts',(3.33947915066444,45.0895833333319,51.5994791506644));
#264087=CARTESIAN_POINT('Ctrl Pts',(4.72273670613183,45.1557291666652,50.216221595197));
#264088=CARTESIAN_POINT('Ctrl Pts',(4.72273670613183,45.2218749999985,48.26));
#264089=CARTESIAN_POINT('Ctrl Pts',(4.72273670613183,45.2880208333319,46.303778404803));
#264090=CARTESIAN_POINT('Ctrl Pts',(3.33947915066444,45.3541666666652,44.9205208493356));
#264091=CARTESIAN_POINT('Ctrl Pts',(1.95622159519705,45.4203124999985,43.5372632938682));
#264092=CARTESIAN_POINT('Ctrl Pts',(6.99833541005117E-15,45.4864583333318,
43.5372632938682));
#264093=CARTESIAN_POINT('Ctrl Pts',(-1.95622159519704,45.5526041666651,
43.5372632938682));
#264094=CARTESIAN_POINT('Ctrl Pts',(-3.33947915066443,45.6187499999984,
44.9205208493356));
#264095=CARTESIAN_POINT('Ctrl Pts',(-4.72273670613182,45.6848958333317,
46.303778404803));
#264096=CARTESIAN_POINT('Ctrl Pts',(-4.72273670613182,45.7510416666651,
48.26));
#264097=CARTESIAN_POINT('Ctrl Pts',(-4.72273670613182,45.8171874999984,
50.216221595197));
#264098=CARTESIAN_POINT('Ctrl Pts',(-3.33947915066443,45.8833333333317,
51.5994791506644));
#264099=CARTESIAN_POINT('Ctrl Pts',(-1.95622159519703,45.949479166665,52.9827367061318));
#264100=CARTESIAN_POINT('Ctrl Pts',(7.17168088200107E-15,46.0156249999983,
52.9827367061318));
#264101=CARTESIAN_POINT('Ctrl Pts',(1.95622159519705,46.0817708333316,52.9827367061318));
#264102=CARTESIAN_POINT('Ctrl Pts',(3.33947915066444,46.1479166666649,51.5994791506644));
#264103=CARTESIAN_POINT('Ctrl Pts',(4.72273670613183,46.2140624999982,50.216221595197));
#264104=CARTESIAN_POINT('Ctrl Pts',(4.72273670613183,46.2802083333315,48.26));
#264105=CARTESIAN_POINT('Ctrl Pts',(4.72273670613183,46.3463541666649,46.303778404803));
#264106=CARTESIAN_POINT('Ctrl Pts',(3.33947915066444,46.4124999999982,44.9205208493356));
#264107=CARTESIAN_POINT('Ctrl Pts',(1.95622159519705,46.4786458333315,43.5372632938682));
#264108=CARTESIAN_POINT('Ctrl Pts',(6.99833541005117E-15,46.5447916666648,
43.5372632938682));
#264109=CARTESIAN_POINT('Ctrl Pts',(-1.95622159519704,46.6109374999981,
43.5372632938682));
#264110=CARTESIAN_POINT('Ctrl Pts',(-3.33947915066443,46.6770833333314,
44.9205208493356));
#264111=CARTESIAN_POINT('Ctrl Pts',(-4.72273670613182,46.7432291666647,
46.303778404803));
#264112=CARTESIAN_POINT('Ctrl Pts',(-4.72273670613182,46.8093749999981,
48.26));
#264113=CARTESIAN_POINT('Ctrl Pts',(-4.72273670613182,46.8755208333314,
50.216221595197));
#264114=CARTESIAN_POINT('Ctrl Pts',(-3.33947915066443,46.9416666666647,
51.5994791506644));
#264115=CARTESIAN_POINT('Ctrl Pts',(-1.95622159519703,47.007812499998,52.9827367061318));
#264116=CARTESIAN_POINT('Ctrl Pts',(7.17168088200104E-15,47.0739583333313,
52.9827367061318));
#264117=CARTESIAN_POINT('Ctrl Pts',(1.95622159519705,47.1401041666646,52.9827367061318));
#264118=CARTESIAN_POINT('Ctrl Pts',(3.33947915066444,47.2062499999979,51.5994791506644));
#264119=CARTESIAN_POINT('Ctrl Pts',(4.72273670613183,47.2723958333312,50.216221595197));
#264120=CARTESIAN_POINT('Ctrl Pts',(4.72273670613183,47.3385416666645,48.26));
#264121=CARTESIAN_POINT('Ctrl Pts',(4.72273670613183,47.4046874999979,46.303778404803));
#264122=CARTESIAN_POINT('Ctrl Pts',(3.33947915066444,47.4708333333312,44.9205208493356));
#264123=CARTESIAN_POINT('Ctrl Pts',(1.95622159519705,47.5369791666645,43.5372632938682));
#264124=CARTESIAN_POINT('Ctrl Pts',(6.99833541005117E-15,47.6031249999978,
43.5372632938682));
#264125=CARTESIAN_POINT('Ctrl Pts',(-1.95622159519704,47.6692708333311,
43.5372632938682));
#264126=CARTESIAN_POINT('Ctrl Pts',(-3.33947915066443,47.7354166666644,
44.9205208493356));
#264127=CARTESIAN_POINT('Ctrl Pts',(-4.72273670613182,47.8015624999977,
46.303778404803));
#264128=CARTESIAN_POINT('Ctrl Pts',(-4.72273670613182,47.867708333331,48.26));
#264129=CARTESIAN_POINT('Ctrl Pts',(-4.72273670613182,47.9338541666644,
50.216221595197));
#264130=CARTESIAN_POINT('Ctrl Pts',(-3.33947915066443,47.9999999999977,
51.5994791506644));
#264131=CARTESIAN_POINT('Ctrl Pts',(-1.95622159519703,48.066145833331,52.9827367061318));
#264132=CARTESIAN_POINT('Ctrl Pts',(7.17168088200104E-15,48.1322916666643,
52.9827367061318));
#264133=CARTESIAN_POINT('Ctrl Pts',(1.95622159519705,48.1984374999976,52.9827367061318));
#264134=CARTESIAN_POINT('Ctrl Pts',(3.33947915066444,48.2645833333309,51.5994791506644));
#264135=CARTESIAN_POINT('Ctrl Pts',(4.72273670613183,48.3307291666642,50.216221595197));
#264136=CARTESIAN_POINT('Ctrl Pts',(4.72273670613183,48.3968749999976,48.26));
#264137=CARTESIAN_POINT('Ctrl Pts',(4.72273670613183,48.4630208333309,46.303778404803));
#264138=CARTESIAN_POINT('Ctrl Pts',(3.33947915066444,48.5291666666642,44.9205208493356));
#264139=CARTESIAN_POINT('Ctrl Pts',(1.95622159519705,48.5953124999975,43.5372632938682));
#264140=CARTESIAN_POINT('Ctrl Pts',(6.99833541005117E-15,48.6614583333308,
43.5372632938682));
#264141=CARTESIAN_POINT('Ctrl Pts',(-1.95622159519704,48.7276041666641,
43.5372632938682));
#264142=CARTESIAN_POINT('Ctrl Pts',(-3.33947915066443,48.7937499999974,
44.9205208493356));
#264143=CARTESIAN_POINT('Ctrl Pts',(-4.72273670613182,48.8598958333307,
46.303778404803));
#264144=CARTESIAN_POINT('Ctrl Pts',(-4.72273670613182,48.9260416666641,
48.26));
#264145=CARTESIAN_POINT('Ctrl Pts',(-4.72273670613182,48.9921874999974,
50.216221595197));
#264146=CARTESIAN_POINT('Ctrl Pts',(-3.33947915066443,49.0583333333307,
51.5994791506644));
#264147=CARTESIAN_POINT('Ctrl Pts',(-1.95622159519703,49.124479166664,52.9827367061318));
#264148=CARTESIAN_POINT('Ctrl Pts',(7.17168088200102E-15,49.1906249999973,
52.9827367061318));
#264149=CARTESIAN_POINT('Ctrl Pts',(1.95622159519705,49.2567708333306,52.9827367061318));
#264150=CARTESIAN_POINT('Ctrl Pts',(3.33947915066444,49.3229166666639,51.5994791506644));
#264151=CARTESIAN_POINT('Ctrl Pts',(4.72273670613183,49.3890624999972,50.216221595197));
#264152=CARTESIAN_POINT('Ctrl Pts',(4.72273670613183,49.4552083333306,48.26));
#264153=CARTESIAN_POINT('Ctrl Pts',(4.72273670613183,49.5213541666639,46.303778404803));
#264154=CARTESIAN_POINT('Ctrl Pts',(3.33947915066444,49.5874999999972,44.9205208493356));
#264155=CARTESIAN_POINT('Ctrl Pts',(1.95622159519705,49.6536458333305,43.5372632938682));
#264156=CARTESIAN_POINT('Ctrl Pts',(6.99833541005115E-15,49.7197916666638,
43.5372632938682));
#264157=CARTESIAN_POINT('Ctrl Pts',(-1.95622159519704,49.7859374999971,
43.5372632938682));
#264158=CARTESIAN_POINT('Ctrl Pts',(-3.33947915066443,49.8520833333304,
44.9205208493356));
#264159=CARTESIAN_POINT('Ctrl Pts',(-4.72273670613182,49.9182291666637,
46.303778404803));
#264160=CARTESIAN_POINT('Ctrl Pts',(-4.72273670613182,49.9843749999971,
48.26));
#264161=CARTESIAN_POINT('Ctrl Pts',(-4.72273670613182,50.0505208333304,
50.216221595197));
#264162=CARTESIAN_POINT('Ctrl Pts',(-3.33947915066443,50.1166666666637,
51.5994791506644));
#264163=CARTESIAN_POINT('Ctrl Pts',(-1.95622159519703,50.182812499997,52.9827367061318));
#264164=CARTESIAN_POINT('Ctrl Pts',(7.17168088200107E-15,50.2489583333303,
52.9827367061318));
#264165=CARTESIAN_POINT('Ctrl Pts',(1.95622159519705,50.3151041666636,52.9827367061318));
#264166=CARTESIAN_POINT('Ctrl Pts',(3.33947915066444,50.3812499999969,51.5994791506644));
#264167=CARTESIAN_POINT('Ctrl Pts',(4.72273670613183,50.4473958333302,50.216221595197));
#264168=CARTESIAN_POINT('Ctrl Pts',(4.72273670613183,50.5135416666636,48.26));
#264169=CARTESIAN_POINT('Ctrl Pts',(4.72273670613183,50.5796874999969,46.303778404803));
#264170=CARTESIAN_POINT('Ctrl Pts',(3.33947915066444,50.6458333333302,44.9205208493356));
#264171=CARTESIAN_POINT('Ctrl Pts',(1.95622159519705,50.7119791666635,43.5372632938682));
#264172=CARTESIAN_POINT('Ctrl Pts',(6.99833541005117E-15,50.7781249999968,
43.5372632938682));
#264173=CARTESIAN_POINT('Ctrl Pts',(-1.95622159519704,50.8442708333301,
43.5372632938682));
#264174=CARTESIAN_POINT('Ctrl Pts',(-3.33947915066443,50.9104166666634,
44.9205208493356));
#264175=CARTESIAN_POINT('Ctrl Pts',(-4.72273670613182,50.9765624999967,
46.303778404803));
#264176=CARTESIAN_POINT('Ctrl Pts',(-4.72273670613182,51.04270833333,48.26));
#264177=CARTESIAN_POINT('Ctrl Pts',(-4.75205527448904,40.4763020833333,
48.26));
#264178=CARTESIAN_POINT('Ctrl Pts',(-4.75205527448904,40.5424479166667,
50.22836574384));
#264179=CARTESIAN_POINT('Ctrl Pts',(-3.3602105091645,40.60859375,51.6202105091645));
#264180=CARTESIAN_POINT('Ctrl Pts',(-1.96836574383996,40.6747395833333,
53.0120552744891));
#264181=CARTESIAN_POINT('Ctrl Pts',(7.17401418756681E-15,40.7408854166666,
53.0120552744891));
#264182=CARTESIAN_POINT('Ctrl Pts',(1.96836574383997,40.8070312499999,53.0120552744891));
#264183=CARTESIAN_POINT('Ctrl Pts',(3.36021050916451,40.8731770833332,51.6202105091645));
#264184=CARTESIAN_POINT('Ctrl Pts',(4.75205527448905,40.9393229166665,50.22836574384));
#264185=CARTESIAN_POINT('Ctrl Pts',(4.75205527448905,41.0054687499998,48.26));
#264186=CARTESIAN_POINT('Ctrl Pts',(4.75205527448905,41.0716145833332,46.29163425616));
#264187=CARTESIAN_POINT('Ctrl Pts',(3.36021050916451,41.1377604166665,44.8997894908355));
#264188=CARTESIAN_POINT('Ctrl Pts',(1.96836574383997,41.2039062499998,43.507944725511));
#264189=CARTESIAN_POINT('Ctrl Pts',(6.99959259357482E-15,41.2700520833331,
43.507944725511));
#264190=CARTESIAN_POINT('Ctrl Pts',(-1.96836574383996,41.3361979166664,
43.507944725511));
#264191=CARTESIAN_POINT('Ctrl Pts',(-3.3602105091645,41.4023437499997,44.8997894908355));
#264192=CARTESIAN_POINT('Ctrl Pts',(-4.75205527448904,41.468489583333,46.29163425616));
#264193=CARTESIAN_POINT('Ctrl Pts',(-4.75205527448904,41.5346354166663,
48.26));
#264194=CARTESIAN_POINT('Ctrl Pts',(-4.75205527448904,41.6007812499997,
50.22836574384));
#264195=CARTESIAN_POINT('Ctrl Pts',(-3.3602105091645,41.666927083333,51.6202105091645));
#264196=CARTESIAN_POINT('Ctrl Pts',(-1.96836574383996,41.7330729166663,
53.0120552744891));
#264197=CARTESIAN_POINT('Ctrl Pts',(7.17401418756681E-15,41.7992187499996,
53.0120552744891));
#264198=CARTESIAN_POINT('Ctrl Pts',(1.96836574383997,41.8653645833329,53.0120552744891));
#264199=CARTESIAN_POINT('Ctrl Pts',(3.36021050916451,41.9315104166662,51.6202105091645));
#264200=CARTESIAN_POINT('Ctrl Pts',(4.75205527448905,41.9976562499995,50.22836574384));
#264201=CARTESIAN_POINT('Ctrl Pts',(4.75205527448905,42.0638020833328,48.26));
#264202=CARTESIAN_POINT('Ctrl Pts',(4.75205527448905,42.1299479166662,46.29163425616));
#264203=CARTESIAN_POINT('Ctrl Pts',(3.36021050916451,42.1960937499995,44.8997894908355));
#264204=CARTESIAN_POINT('Ctrl Pts',(1.96836574383997,42.2622395833328,43.507944725511));
#264205=CARTESIAN_POINT('Ctrl Pts',(6.99959259357482E-15,42.3283854166661,
43.507944725511));
#264206=CARTESIAN_POINT('Ctrl Pts',(-1.96836574383996,42.3945312499994,
43.507944725511));
#264207=CARTESIAN_POINT('Ctrl Pts',(-3.3602105091645,42.4606770833327,44.8997894908355));
#264208=CARTESIAN_POINT('Ctrl Pts',(-4.75205527448904,42.526822916666,46.29163425616));
#264209=CARTESIAN_POINT('Ctrl Pts',(-4.75205527448904,42.5929687499993,
48.26));
#264210=CARTESIAN_POINT('Ctrl Pts',(-4.75205527448904,42.6591145833326,
50.22836574384));
#264211=CARTESIAN_POINT('Ctrl Pts',(-3.3602105091645,42.725260416666,51.6202105091645));
#264212=CARTESIAN_POINT('Ctrl Pts',(-1.96836574383996,42.7914062499993,
53.0120552744891));
#264213=CARTESIAN_POINT('Ctrl Pts',(7.17401418756679E-15,42.8575520833326,
53.0120552744891));
#264214=CARTESIAN_POINT('Ctrl Pts',(1.96836574383997,42.9236979166659,53.0120552744891));
#264215=CARTESIAN_POINT('Ctrl Pts',(3.36021050916451,42.9898437499992,51.6202105091645));
#264216=CARTESIAN_POINT('Ctrl Pts',(4.75205527448905,43.0559895833325,50.22836574384));
#264217=CARTESIAN_POINT('Ctrl Pts',(4.75205527448905,43.1221354166658,48.26));
#264218=CARTESIAN_POINT('Ctrl Pts',(4.75205527448905,43.1882812499991,46.29163425616));
#264219=CARTESIAN_POINT('Ctrl Pts',(3.36021050916451,43.2544270833325,44.8997894908355));
#264220=CARTESIAN_POINT('Ctrl Pts',(1.96836574383997,43.3205729166658,43.507944725511));
#264221=CARTESIAN_POINT('Ctrl Pts',(6.99959259357482E-15,43.3867187499991,
43.507944725511));
#264222=CARTESIAN_POINT('Ctrl Pts',(-1.96836574383996,43.4528645833324,
43.507944725511));
#264223=CARTESIAN_POINT('Ctrl Pts',(-3.3602105091645,43.5190104166657,44.8997894908355));
#264224=CARTESIAN_POINT('Ctrl Pts',(-4.75205527448904,43.585156249999,46.29163425616));
#264225=CARTESIAN_POINT('Ctrl Pts',(-4.75205527448904,43.6513020833323,
48.26));
#264226=CARTESIAN_POINT('Ctrl Pts',(-4.75205527448904,43.7174479166656,
50.22836574384));
#264227=CARTESIAN_POINT('Ctrl Pts',(-3.3602105091645,43.783593749999,51.6202105091645));
#264228=CARTESIAN_POINT('Ctrl Pts',(-1.96836574383996,43.8497395833323,
53.0120552744891));
#264229=CARTESIAN_POINT('Ctrl Pts',(7.17401418756679E-15,43.9158854166656,
53.0120552744891));
#264230=CARTESIAN_POINT('Ctrl Pts',(1.96836574383997,43.9820312499989,53.0120552744891));
#264231=CARTESIAN_POINT('Ctrl Pts',(3.36021050916451,44.0481770833322,51.6202105091645));
#264232=CARTESIAN_POINT('Ctrl Pts',(4.75205527448905,44.1143229166655,50.22836574384));
#264233=CARTESIAN_POINT('Ctrl Pts',(4.75205527448905,44.1804687499988,48.26));
#264234=CARTESIAN_POINT('Ctrl Pts',(4.75205527448905,44.2466145833322,46.29163425616));
#264235=CARTESIAN_POINT('Ctrl Pts',(3.36021050916451,44.3127604166655,44.8997894908355));
#264236=CARTESIAN_POINT('Ctrl Pts',(1.96836574383997,44.3789062499988,43.507944725511));
#264237=CARTESIAN_POINT('Ctrl Pts',(6.99959259357479E-15,44.4450520833321,
43.507944725511));
#264238=CARTESIAN_POINT('Ctrl Pts',(-1.96836574383996,44.5111979166654,
43.507944725511));
#264239=CARTESIAN_POINT('Ctrl Pts',(-3.3602105091645,44.5773437499987,44.8997894908355));
#264240=CARTESIAN_POINT('Ctrl Pts',(-4.75205527448904,44.643489583332,46.29163425616));
#264241=CARTESIAN_POINT('Ctrl Pts',(-4.75205527448904,44.7096354166653,
48.26));
#264242=CARTESIAN_POINT('Ctrl Pts',(-4.75205527448904,44.7757812499987,
50.22836574384));
#264243=CARTESIAN_POINT('Ctrl Pts',(-3.3602105091645,44.841927083332,51.6202105091645));
#264244=CARTESIAN_POINT('Ctrl Pts',(-1.96836574383996,44.9080729166653,
53.0120552744891));
#264245=CARTESIAN_POINT('Ctrl Pts',(7.17401418756681E-15,44.9742187499986,
53.0120552744891));
#264246=CARTESIAN_POINT('Ctrl Pts',(1.96836574383997,45.0403645833319,53.0120552744891));
#264247=CARTESIAN_POINT('Ctrl Pts',(3.36021050916451,45.1065104166652,51.6202105091645));
#264248=CARTESIAN_POINT('Ctrl Pts',(4.75205527448905,45.1726562499985,50.22836574384));
#264249=CARTESIAN_POINT('Ctrl Pts',(4.75205527448905,45.2388020833318,48.26));
#264250=CARTESIAN_POINT('Ctrl Pts',(4.75205527448905,45.3049479166652,46.29163425616));
#264251=CARTESIAN_POINT('Ctrl Pts',(3.36021050916451,45.3710937499985,44.8997894908355));
#264252=CARTESIAN_POINT('Ctrl Pts',(1.96836574383997,45.4372395833318,43.507944725511));
#264253=CARTESIAN_POINT('Ctrl Pts',(6.99959259357482E-15,45.5033854166651,
43.507944725511));
#264254=CARTESIAN_POINT('Ctrl Pts',(-1.96836574383996,45.5695312499984,
43.507944725511));
#264255=CARTESIAN_POINT('Ctrl Pts',(-3.3602105091645,45.6356770833317,44.8997894908355));
#264256=CARTESIAN_POINT('Ctrl Pts',(-4.75205527448904,45.701822916665,46.29163425616));
#264257=CARTESIAN_POINT('Ctrl Pts',(-4.75205527448904,45.7679687499983,
48.26));
#264258=CARTESIAN_POINT('Ctrl Pts',(-4.75205527448904,45.8341145833317,
50.22836574384));
#264259=CARTESIAN_POINT('Ctrl Pts',(-3.3602105091645,45.900260416665,51.6202105091645));
#264260=CARTESIAN_POINT('Ctrl Pts',(-1.96836574383996,45.9664062499983,
53.0120552744891));
#264261=CARTESIAN_POINT('Ctrl Pts',(7.17401418756681E-15,46.0325520833316,
53.0120552744891));
#264262=CARTESIAN_POINT('Ctrl Pts',(1.96836574383997,46.0986979166649,53.0120552744891));
#264263=CARTESIAN_POINT('Ctrl Pts',(3.36021050916451,46.1648437499982,51.6202105091645));
#264264=CARTESIAN_POINT('Ctrl Pts',(4.75205527448905,46.2309895833315,50.22836574384));
#264265=CARTESIAN_POINT('Ctrl Pts',(4.75205527448905,46.2971354166648,48.26));
#264266=CARTESIAN_POINT('Ctrl Pts',(4.75205527448905,46.3632812499982,46.29163425616));
#264267=CARTESIAN_POINT('Ctrl Pts',(3.36021050916451,46.4294270833315,44.8997894908355));
#264268=CARTESIAN_POINT('Ctrl Pts',(1.96836574383997,46.4955729166648,43.507944725511));
#264269=CARTESIAN_POINT('Ctrl Pts',(6.99959259357482E-15,46.5617187499981,
43.507944725511));
#264270=CARTESIAN_POINT('Ctrl Pts',(-1.96836574383996,46.6278645833314,
43.507944725511));
#264271=CARTESIAN_POINT('Ctrl Pts',(-3.3602105091645,46.6940104166647,44.8997894908355));
#264272=CARTESIAN_POINT('Ctrl Pts',(-4.75205527448904,46.760156249998,46.29163425616));
#264273=CARTESIAN_POINT('Ctrl Pts',(-4.75205527448904,46.8263020833313,
48.26));
#264274=CARTESIAN_POINT('Ctrl Pts',(-4.75205527448904,46.8924479166647,
50.22836574384));
#264275=CARTESIAN_POINT('Ctrl Pts',(-3.3602105091645,46.958593749998,51.6202105091645));
#264276=CARTESIAN_POINT('Ctrl Pts',(-1.96836574383996,47.0247395833313,
53.0120552744891));
#264277=CARTESIAN_POINT('Ctrl Pts',(7.17401418756681E-15,47.0908854166646,
53.0120552744891));
#264278=CARTESIAN_POINT('Ctrl Pts',(1.96836574383997,47.1570312499979,53.0120552744891));
#264279=CARTESIAN_POINT('Ctrl Pts',(3.36021050916451,47.2231770833312,51.6202105091645));
#264280=CARTESIAN_POINT('Ctrl Pts',(4.75205527448905,47.2893229166645,50.22836574384));
#264281=CARTESIAN_POINT('Ctrl Pts',(4.75205527448905,47.3554687499978,48.26));
#264282=CARTESIAN_POINT('Ctrl Pts',(4.75205527448905,47.4216145833312,46.29163425616));
#264283=CARTESIAN_POINT('Ctrl Pts',(3.36021050916451,47.4877604166645,44.8997894908355));
#264284=CARTESIAN_POINT('Ctrl Pts',(1.96836574383997,47.5539062499978,43.507944725511));
#264285=CARTESIAN_POINT('Ctrl Pts',(6.99959259357482E-15,47.6200520833311,
43.507944725511));
#264286=CARTESIAN_POINT('Ctrl Pts',(-1.96836574383996,47.6861979166644,
43.507944725511));
#264287=CARTESIAN_POINT('Ctrl Pts',(-3.3602105091645,47.7523437499977,44.8997894908355));
#264288=CARTESIAN_POINT('Ctrl Pts',(-4.75205527448904,47.818489583331,46.29163425616));
#264289=CARTESIAN_POINT('Ctrl Pts',(-4.75205527448904,47.8846354166643,
48.26));
#264290=CARTESIAN_POINT('Ctrl Pts',(-4.75205527448904,47.9507812499977,
50.22836574384));
#264291=CARTESIAN_POINT('Ctrl Pts',(-3.3602105091645,48.016927083331,51.6202105091645));
#264292=CARTESIAN_POINT('Ctrl Pts',(-1.96836574383996,48.0830729166643,
53.0120552744891));
#264293=CARTESIAN_POINT('Ctrl Pts',(7.17401418756679E-15,48.1492187499976,
53.0120552744891));
#264294=CARTESIAN_POINT('Ctrl Pts',(1.96836574383997,48.2153645833309,53.0120552744891));
#264295=CARTESIAN_POINT('Ctrl Pts',(3.36021050916451,48.2815104166642,51.6202105091645));
#264296=CARTESIAN_POINT('Ctrl Pts',(4.75205527448905,48.3476562499975,50.22836574384));
#264297=CARTESIAN_POINT('Ctrl Pts',(4.75205527448905,48.4138020833309,48.26));
#264298=CARTESIAN_POINT('Ctrl Pts',(4.75205527448905,48.4799479166642,46.29163425616));
#264299=CARTESIAN_POINT('Ctrl Pts',(3.36021050916451,48.5460937499975,44.8997894908355));
#264300=CARTESIAN_POINT('Ctrl Pts',(1.96836574383997,48.6122395833308,43.507944725511));
#264301=CARTESIAN_POINT('Ctrl Pts',(6.99959259357482E-15,48.6783854166641,
43.507944725511));
#264302=CARTESIAN_POINT('Ctrl Pts',(-1.96836574383996,48.7445312499974,
43.507944725511));
#264303=CARTESIAN_POINT('Ctrl Pts',(-3.3602105091645,48.8106770833307,44.8997894908355));
#264304=CARTESIAN_POINT('Ctrl Pts',(-4.75205527448904,48.876822916664,46.29163425616));
#264305=CARTESIAN_POINT('Ctrl Pts',(-4.75205527448904,48.9429687499973,
48.26));
#264306=CARTESIAN_POINT('Ctrl Pts',(-4.75205527448904,49.0091145833307,
50.22836574384));
#264307=CARTESIAN_POINT('Ctrl Pts',(-3.3602105091645,49.075260416664,51.6202105091645));
#264308=CARTESIAN_POINT('Ctrl Pts',(-1.96836574383996,49.1414062499973,
53.0120552744891));
#264309=CARTESIAN_POINT('Ctrl Pts',(7.17401418756684E-15,49.2075520833306,
53.0120552744891));
#264310=CARTESIAN_POINT('Ctrl Pts',(1.96836574383997,49.2736979166639,53.0120552744891));
#264311=CARTESIAN_POINT('Ctrl Pts',(3.36021050916451,49.3398437499972,51.6202105091645));
#264312=CARTESIAN_POINT('Ctrl Pts',(4.75205527448905,49.4059895833305,50.22836574384));
#264313=CARTESIAN_POINT('Ctrl Pts',(4.75205527448905,49.4721354166639,48.26));
#264314=CARTESIAN_POINT('Ctrl Pts',(4.75205527448905,49.5382812499972,46.29163425616));
#264315=CARTESIAN_POINT('Ctrl Pts',(3.36021050916451,49.6044270833305,44.8997894908355));
#264316=CARTESIAN_POINT('Ctrl Pts',(1.96836574383997,49.6705729166638,43.507944725511));
#264317=CARTESIAN_POINT('Ctrl Pts',(6.99959259357482E-15,49.7367187499971,
43.507944725511));
#264318=CARTESIAN_POINT('Ctrl Pts',(-1.96836574383996,49.8028645833304,
43.507944725511));
#264319=CARTESIAN_POINT('Ctrl Pts',(-3.3602105091645,49.8690104166637,44.8997894908355));
#264320=CARTESIAN_POINT('Ctrl Pts',(-4.75205527448904,49.935156249997,46.29163425616));
#264321=CARTESIAN_POINT('Ctrl Pts',(-4.75205527448904,50.0013020833303,
48.26));
#264322=CARTESIAN_POINT('Ctrl Pts',(-4.75205527448904,50.0674479166637,
50.22836574384));
#264323=CARTESIAN_POINT('Ctrl Pts',(-3.3602105091645,50.133593749997,51.6202105091645));
#264324=CARTESIAN_POINT('Ctrl Pts',(-1.96836574383996,50.1997395833303,
53.0120552744891));
#264325=CARTESIAN_POINT('Ctrl Pts',(7.17401418756681E-15,50.2658854166636,
53.0120552744891));
#264326=CARTESIAN_POINT('Ctrl Pts',(1.96836574383997,50.3320312499969,53.0120552744891));
#264327=CARTESIAN_POINT('Ctrl Pts',(3.36021050916451,50.3981770833302,51.6202105091645));
#264328=CARTESIAN_POINT('Ctrl Pts',(4.75205527448905,50.4643229166635,50.22836574384));
#264329=CARTESIAN_POINT('Ctrl Pts',(4.75205527448905,50.5304687499968,48.26));
#264330=CARTESIAN_POINT('Ctrl Pts',(4.75205527448905,50.5966145833302,46.29163425616));
#264331=CARTESIAN_POINT('Ctrl Pts',(3.36021050916451,50.6627604166635,44.8997894908355));
#264332=CARTESIAN_POINT('Ctrl Pts',(1.96836574383997,50.7289062499968,43.507944725511));
#264333=CARTESIAN_POINT('Ctrl Pts',(6.99959259357482E-15,50.7950520833301,
43.507944725511));
#264334=CARTESIAN_POINT('Ctrl Pts',(-1.96836574383996,50.8611979166634,
43.507944725511));
#264335=CARTESIAN_POINT('Ctrl Pts',(-3.3602105091645,50.9273437499967,44.8997894908355));
#264336=CARTESIAN_POINT('Ctrl Pts',(-4.75205527448904,50.99348958333,46.29163425616));
#264337=CARTESIAN_POINT('Ctrl Pts',(-4.75205527448904,51.0596354166633,
48.26));
#264338=CARTESIAN_POINT('Ctrl Pts',(4.68628896694498,42.0671867061318,47.6743911597878));
#264339=CARTESIAN_POINT('Ctrl Pts',(4.48534984498601,42.1243724082372,46.0663915436572));
#264340=CARTESIAN_POINT('Ctrl Pts',(3.33947915066444,42.1791666666662,44.9205208493356));
#264341=CARTESIAN_POINT('Ctrl Pts',(1.95622159519705,42.2453124999995,43.5372632938682));
#264342=CARTESIAN_POINT('Ctrl Pts',(6.9983354100512E-15,42.3114583333328,
43.5372632938682));
#264343=CARTESIAN_POINT('Ctrl Pts',(-1.95622159519704,42.3776041666661,
43.5372632938682));
#264344=CARTESIAN_POINT('Ctrl Pts',(-3.33947915066443,42.4437499999994,
44.9205208493356));
#264345=CARTESIAN_POINT('Ctrl Pts',(-4.72273670613182,42.5098958333327,
46.303778404803));
#264346=CARTESIAN_POINT('Ctrl Pts',(-4.72273670613182,42.5760416666661,
48.26));
#264347=CARTESIAN_POINT('Ctrl Pts',(-4.72273670613182,42.6421874999994,
50.216221595197));
#264348=CARTESIAN_POINT('Ctrl Pts',(-3.33947915066443,42.7083333333327,
51.5994791506644));
#264349=CARTESIAN_POINT('Ctrl Pts',(-1.95622159519703,42.774479166666,52.9827367061318));
#264350=CARTESIAN_POINT('Ctrl Pts',(7.17168088200104E-15,42.8406249999993,
52.9827367061318));
#264351=CARTESIAN_POINT('Ctrl Pts',(1.95622159519705,42.9067708333326,52.9827367061318));
#264352=CARTESIAN_POINT('Ctrl Pts',(3.33947915066444,42.9729166666659,51.5994791506644));
#264353=CARTESIAN_POINT('Ctrl Pts',(4.72273670613183,43.0390624999992,50.216221595197));
#264354=CARTESIAN_POINT('Ctrl Pts',(4.72273670613183,43.1052083333326,48.26));
#264355=CARTESIAN_POINT('Origin',(-3.05311331771918E-14,40.4567708333334,
48.26));
#264356=CARTESIAN_POINT('Ctrl Pts',(4.66579641623065,42.0671867061318,47.5288462557477));
#264357=CARTESIAN_POINT('Ctrl Pts',(4.42756765431106,42.1219271548081,46.0086093529822));
#264358=CARTESIAN_POINT('Ctrl Pts',(3.33947915066444,42.1739583333328,44.9205208493356));
#264359=CARTESIAN_POINT('Ctrl Pts',(1.95622159519705,42.2401041666661,43.5372632938682));
#264360=CARTESIAN_POINT('Ctrl Pts',(6.99833541005117E-15,42.3062499999994,
43.5372632938682));
#264361=CARTESIAN_POINT('Ctrl Pts',(-1.95622159519704,42.3723958333327,
43.5372632938682));
#264362=CARTESIAN_POINT('Ctrl Pts',(-3.33947915066443,42.438541666666,44.9205208493356));
#264363=CARTESIAN_POINT('Ctrl Pts',(-4.72273670613182,42.5046874999994,
46.303778404803));
#264364=CARTESIAN_POINT('Ctrl Pts',(-4.72273670613182,42.5708333333327,
48.26));
#264365=CARTESIAN_POINT('Ctrl Pts',(-4.72273670613182,42.636979166666,50.216221595197));
#264366=CARTESIAN_POINT('Ctrl Pts',(-3.33947915066443,42.7031249999993,
51.5994791506644));
#264367=CARTESIAN_POINT('Ctrl Pts',(-1.95622159519703,42.7692708333326,
52.9827367061318));
#264368=CARTESIAN_POINT('Ctrl Pts',(7.17168088200104E-15,42.8354166666659,
52.9827367061318));
#264369=CARTESIAN_POINT('Ctrl Pts',(1.95622159519705,42.9015624999992,52.9827367061318));
#264370=CARTESIAN_POINT('Ctrl Pts',(3.33947915066444,42.9677083333326,51.5994791506644));
#264371=CARTESIAN_POINT('Ctrl Pts',(4.72273670613183,43.0338541666659,50.216221595197));
#264372=CARTESIAN_POINT('Ctrl Pts',(4.72273670613183,43.0999999999992,48.26));
#264373=CARTESIAN_POINT('Ctrl Pts',(-4.75205527448904,40.4372395833334,
48.26));
#264374=CARTESIAN_POINT('Ctrl Pts',(-4.75205527448904,40.5033854166667,
50.22836574384));
#264375=CARTESIAN_POINT('Ctrl Pts',(-3.3602105091645,40.56953125,51.6202105091645));
#264376=CARTESIAN_POINT('Ctrl Pts',(-1.96836574383996,40.6356770833333,
53.0120552744891));
#264377=CARTESIAN_POINT('Ctrl Pts',(7.17401418756681E-15,40.7018229166666,
53.0120552744891));
#264378=CARTESIAN_POINT('Ctrl Pts',(1.96836574383997,40.7679687499999,53.0120552744891));
#264379=CARTESIAN_POINT('Ctrl Pts',(3.36021050916451,40.8341145833332,51.6202105091645));
#264380=CARTESIAN_POINT('Ctrl Pts',(4.75205527448906,40.9002604166666,50.22836574384));
#264381=CARTESIAN_POINT('Ctrl Pts',(4.75205527448906,40.9664062499999,48.26));
#264382=CARTESIAN_POINT('Ctrl Pts',(4.75205527448906,41.0325520833332,46.29163425616));
#264383=CARTESIAN_POINT('Ctrl Pts',(3.36021050916451,41.0986979166665,44.8997894908355));
#264384=CARTESIAN_POINT('Ctrl Pts',(1.96836574383997,41.1648437499998,43.507944725511));
#264385=CARTESIAN_POINT('Ctrl Pts',(6.99959259357479E-15,41.2309895833331,
43.507944725511));
#264386=CARTESIAN_POINT('Ctrl Pts',(-1.96836574383996,41.2971354166664,
43.507944725511));
#264387=CARTESIAN_POINT('Ctrl Pts',(-3.3602105091645,41.3632812499997,44.8997894908355));
#264388=CARTESIAN_POINT('Ctrl Pts',(-4.75205527448904,41.4294270833331,
46.29163425616));
#264389=CARTESIAN_POINT('Ctrl Pts',(-4.75205527448904,41.4955729166664,
48.26));
#264390=CARTESIAN_POINT('Ctrl Pts',(-4.75205527448904,41.5617187499997,
50.22836574384));
#264391=CARTESIAN_POINT('Ctrl Pts',(-3.3602105091645,41.627864583333,51.6202105091645));
#264392=CARTESIAN_POINT('Ctrl Pts',(-1.96836574383996,41.6940104166663,
53.0120552744891));
#264393=CARTESIAN_POINT('Ctrl Pts',(7.17401418756681E-15,41.7601562499996,
53.0120552744891));
#264394=CARTESIAN_POINT('Ctrl Pts',(1.96836574383997,41.8263020833329,53.0120552744891));
#264395=CARTESIAN_POINT('Ctrl Pts',(3.36021050916451,41.8924479166662,51.6202105091645));
#264396=CARTESIAN_POINT('Ctrl Pts',(4.75205527448906,41.9585937499996,50.22836574384));
#264397=CARTESIAN_POINT('Ctrl Pts',(4.75205527448906,42.0247395833329,48.26));
#264398=CARTESIAN_POINT('Ctrl Pts',(4.75205527448906,42.0908854166662,46.29163425616));
#264399=CARTESIAN_POINT('Ctrl Pts',(3.36021050916451,42.1570312499995,44.8997894908355));
#264400=CARTESIAN_POINT('Ctrl Pts',(1.96836574383997,42.2231770833328,43.507944725511));
#264401=CARTESIAN_POINT('Ctrl Pts',(6.99959259357482E-15,42.2893229166661,
43.507944725511));
#264402=CARTESIAN_POINT('Ctrl Pts',(-1.96836574383996,42.3554687499994,
43.507944725511));
#264403=CARTESIAN_POINT('Ctrl Pts',(-3.3602105091645,42.4216145833327,44.8997894908355));
#264404=CARTESIAN_POINT('Ctrl Pts',(-4.75205527448904,42.4877604166661,
46.29163425616));
#264405=CARTESIAN_POINT('Ctrl Pts',(-4.75205527448904,42.5539062499994,
48.26));
#264406=CARTESIAN_POINT('Ctrl Pts',(-4.75205527448904,42.6200520833327,
50.22836574384));
#264407=CARTESIAN_POINT('Ctrl Pts',(-3.3602105091645,42.686197916666,51.6202105091645));
#264408=CARTESIAN_POINT('Ctrl Pts',(-1.96836574383996,42.7523437499993,
53.0120552744891));
#264409=CARTESIAN_POINT('Ctrl Pts',(7.17401418756679E-15,42.8184895833326,
53.0120552744891));
#264410=CARTESIAN_POINT('Ctrl Pts',(1.96836574383997,42.8846354166659,53.0120552744891));
#264411=CARTESIAN_POINT('Ctrl Pts',(3.36021050916451,42.9507812499993,51.6202105091645));
#264412=CARTESIAN_POINT('Ctrl Pts',(4.75205527448906,43.0169270833326,50.22836574384));
#264413=CARTESIAN_POINT('Ctrl Pts',(4.75205527448906,43.0830729166659,48.26));
#264414=CARTESIAN_POINT('Ctrl Pts',(4.75205527448906,43.1492187499992,46.29163425616));
#264415=CARTESIAN_POINT('Ctrl Pts',(3.36021050916451,43.2153645833325,44.8997894908355));
#264416=CARTESIAN_POINT('Ctrl Pts',(1.96836574383997,43.2815104166658,43.507944725511));
#264417=CARTESIAN_POINT('Ctrl Pts',(6.99959259357479E-15,43.3476562499991,
43.507944725511));
#264418=CARTESIAN_POINT('Ctrl Pts',(-1.96836574383996,43.4138020833324,
43.507944725511));
#264419=CARTESIAN_POINT('Ctrl Pts',(-3.3602105091645,43.4799479166657,44.8997894908355));
#264420=CARTESIAN_POINT('Ctrl Pts',(-4.75205527448904,43.5460937499991,
46.29163425616));
#264421=CARTESIAN_POINT('Ctrl Pts',(-4.75205527448904,43.6122395833324,
48.26));
#264422=CARTESIAN_POINT('Ctrl Pts',(-4.75205527448904,43.6783854166657,
50.22836574384));
#264423=CARTESIAN_POINT('Ctrl Pts',(-3.3602105091645,43.744531249999,51.6202105091645));
#264424=CARTESIAN_POINT('Ctrl Pts',(-1.96836574383996,43.8106770833323,
53.0120552744891));
#264425=CARTESIAN_POINT('Ctrl Pts',(7.17401418756679E-15,43.8768229166656,
53.0120552744891));
#264426=CARTESIAN_POINT('Ctrl Pts',(1.96836574383997,43.9429687499989,53.0120552744891));
#264427=CARTESIAN_POINT('Ctrl Pts',(3.36021050916451,44.0091145833323,51.6202105091645));
#264428=CARTESIAN_POINT('Ctrl Pts',(4.75205527448906,44.0752604166656,50.22836574384));
#264429=CARTESIAN_POINT('Ctrl Pts',(4.75205527448906,44.1414062499989,48.26));
#264430=CARTESIAN_POINT('Ctrl Pts',(4.75205527448906,44.2075520833322,46.29163425616));
#264431=CARTESIAN_POINT('Ctrl Pts',(3.36021050916451,44.2736979166655,44.8997894908355));
#264432=CARTESIAN_POINT('Ctrl Pts',(1.96836574383997,44.3398437499988,43.507944725511));
#264433=CARTESIAN_POINT('Ctrl Pts',(6.99959259357479E-15,44.4059895833321,
43.507944725511));
#264434=CARTESIAN_POINT('Ctrl Pts',(-1.96836574383996,44.4721354166654,
43.507944725511));
#264435=CARTESIAN_POINT('Ctrl Pts',(-3.3602105091645,44.5382812499987,44.8997894908355));
#264436=CARTESIAN_POINT('Ctrl Pts',(-4.75205527448904,44.6044270833321,
46.29163425616));
#264437=CARTESIAN_POINT('Ctrl Pts',(-4.75205527448904,44.6705729166654,
48.26));
#264438=CARTESIAN_POINT('Ctrl Pts',(-4.75205527448904,44.7367187499987,
50.22836574384));
#264439=CARTESIAN_POINT('Ctrl Pts',(-3.3602105091645,44.802864583332,51.6202105091645));
#264440=CARTESIAN_POINT('Ctrl Pts',(-1.96836574383996,44.8690104166653,
53.0120552744891));
#264441=CARTESIAN_POINT('Ctrl Pts',(7.17401418756679E-15,44.9351562499986,
53.0120552744891));
#264442=CARTESIAN_POINT('Ctrl Pts',(1.96836574383997,45.001302083332,53.0120552744891));
#264443=CARTESIAN_POINT('Ctrl Pts',(3.36021050916451,45.0674479166652,51.6202105091645));
#264444=CARTESIAN_POINT('Ctrl Pts',(4.75205527448906,45.1335937499986,50.22836574384));
#264445=CARTESIAN_POINT('Ctrl Pts',(4.75205527448906,45.1997395833319,48.26));
#264446=CARTESIAN_POINT('Ctrl Pts',(4.75205527448906,45.2658854166652,46.29163425616));
#264447=CARTESIAN_POINT('Ctrl Pts',(3.36021050916451,45.3320312499985,44.8997894908355));
#264448=CARTESIAN_POINT('Ctrl Pts',(1.96836574383997,45.3981770833318,43.507944725511));
#264449=CARTESIAN_POINT('Ctrl Pts',(6.99959259357482E-15,45.4643229166651,
43.507944725511));
#264450=CARTESIAN_POINT('Ctrl Pts',(-1.96836574383996,45.5304687499984,
43.507944725511));
#264451=CARTESIAN_POINT('Ctrl Pts',(-3.3602105091645,45.5966145833317,44.8997894908355));
#264452=CARTESIAN_POINT('Ctrl Pts',(-4.75205527448904,45.6627604166651,
46.29163425616));
#264453=CARTESIAN_POINT('Ctrl Pts',(-4.75205527448904,45.7289062499984,
48.26));
#264454=CARTESIAN_POINT('Ctrl Pts',(-4.75205527448904,45.7950520833317,
50.22836574384));
#264455=CARTESIAN_POINT('Ctrl Pts',(-3.3602105091645,45.861197916665,51.6202105091645));
#264456=CARTESIAN_POINT('Ctrl Pts',(-1.96836574383996,45.9273437499983,
53.0120552744891));
#264457=CARTESIAN_POINT('Ctrl Pts',(7.17401418756681E-15,45.9934895833316,
53.0120552744891));
#264458=CARTESIAN_POINT('Ctrl Pts',(1.96836574383997,46.0596354166649,53.0120552744891));
#264459=CARTESIAN_POINT('Ctrl Pts',(3.36021050916451,46.1257812499982,51.6202105091645));
#264460=CARTESIAN_POINT('Ctrl Pts',(4.75205527448906,46.1919270833316,50.22836574384));
#264461=CARTESIAN_POINT('Ctrl Pts',(4.75205527448906,46.2580729166649,48.26));
#264462=CARTESIAN_POINT('Ctrl Pts',(4.75205527448906,46.3242187499982,46.29163425616));
#264463=CARTESIAN_POINT('Ctrl Pts',(3.36021050916451,46.3903645833315,44.8997894908355));
#264464=CARTESIAN_POINT('Ctrl Pts',(1.96836574383997,46.4565104166648,43.507944725511));
#264465=CARTESIAN_POINT('Ctrl Pts',(6.99959259357479E-15,46.5226562499981,
43.507944725511));
#264466=CARTESIAN_POINT('Ctrl Pts',(-1.96836574383996,46.5888020833314,
43.507944725511));
#264467=CARTESIAN_POINT('Ctrl Pts',(-3.3602105091645,46.6549479166647,44.8997894908355));
#264468=CARTESIAN_POINT('Ctrl Pts',(-4.75205527448904,46.7210937499981,
46.29163425616));
#264469=CARTESIAN_POINT('Ctrl Pts',(-4.75205527448904,46.7872395833314,
48.26));
#264470=CARTESIAN_POINT('Ctrl Pts',(-4.75205527448904,46.8533854166647,
50.22836574384));
#264471=CARTESIAN_POINT('Ctrl Pts',(-3.3602105091645,46.919531249998,51.6202105091645));
#264472=CARTESIAN_POINT('Ctrl Pts',(-1.96836574383996,46.9856770833313,
53.0120552744891));
#264473=CARTESIAN_POINT('Ctrl Pts',(7.17401418756679E-15,47.0518229166646,
53.0120552744891));
#264474=CARTESIAN_POINT('Ctrl Pts',(1.96836574383997,47.1179687499979,53.0120552744891));
#264475=CARTESIAN_POINT('Ctrl Pts',(3.36021050916451,47.1841145833313,51.6202105091645));
#264476=CARTESIAN_POINT('Ctrl Pts',(4.75205527448906,47.2502604166646,50.22836574384));
#264477=CARTESIAN_POINT('Ctrl Pts',(4.75205527448906,47.3164062499979,48.26));
#264478=CARTESIAN_POINT('Ctrl Pts',(4.75205527448906,47.3825520833312,46.29163425616));
#264479=CARTESIAN_POINT('Ctrl Pts',(3.36021050916451,47.4486979166645,44.8997894908355));
#264480=CARTESIAN_POINT('Ctrl Pts',(1.96836574383997,47.5148437499978,43.507944725511));
#264481=CARTESIAN_POINT('Ctrl Pts',(6.99959259357482E-15,47.5809895833311,
43.507944725511));
#264482=CARTESIAN_POINT('Ctrl Pts',(-1.96836574383996,47.6471354166644,
43.507944725511));
#264483=CARTESIAN_POINT('Ctrl Pts',(-3.3602105091645,47.7132812499977,44.8997894908355));
#264484=CARTESIAN_POINT('Ctrl Pts',(-4.75205527448904,47.7794270833311,
46.29163425616));
#264485=CARTESIAN_POINT('Ctrl Pts',(-4.75205527448904,47.8455729166644,
48.26));
#264486=CARTESIAN_POINT('Ctrl Pts',(-4.75205527448904,47.9117187499977,
50.22836574384));
#264487=CARTESIAN_POINT('Ctrl Pts',(-3.3602105091645,47.977864583331,51.6202105091645));
#264488=CARTESIAN_POINT('Ctrl Pts',(-1.96836574383996,48.0440104166643,
53.0120552744891));
#264489=CARTESIAN_POINT('Ctrl Pts',(7.17401418756679E-15,48.1101562499976,
53.0120552744891));
#264490=CARTESIAN_POINT('Ctrl Pts',(1.96836574383997,48.1763020833309,53.0120552744891));
#264491=CARTESIAN_POINT('Ctrl Pts',(3.36021050916451,48.2424479166643,51.6202105091645));
#264492=CARTESIAN_POINT('Ctrl Pts',(4.75205527448906,48.3085937499975,50.22836574384));
#264493=CARTESIAN_POINT('Ctrl Pts',(4.75205527448906,48.3747395833309,48.26));
#264494=CARTESIAN_POINT('Ctrl Pts',(4.75205527448906,48.4408854166642,46.29163425616));
#264495=CARTESIAN_POINT('Ctrl Pts',(3.36021050916451,48.5070312499975,44.8997894908355));
#264496=CARTESIAN_POINT('Ctrl Pts',(1.96836574383997,48.5731770833308,43.507944725511));
#264497=CARTESIAN_POINT('Ctrl Pts',(6.99959259357479E-15,48.6393229166641,
43.507944725511));
#264498=CARTESIAN_POINT('Ctrl Pts',(-1.96836574383996,48.7054687499974,
43.507944725511));
#264499=CARTESIAN_POINT('Ctrl Pts',(-3.3602105091645,48.7716145833307,44.8997894908355));
#264500=CARTESIAN_POINT('Ctrl Pts',(-4.75205527448904,48.8377604166641,
46.29163425616));
#264501=CARTESIAN_POINT('Ctrl Pts',(-4.75205527448904,48.9039062499974,
48.26));
#264502=CARTESIAN_POINT('Ctrl Pts',(-4.75205527448904,48.9700520833307,
50.22836574384));
#264503=CARTESIAN_POINT('Ctrl Pts',(-3.3602105091645,49.036197916664,51.6202105091645));
#264504=CARTESIAN_POINT('Ctrl Pts',(-1.96836574383996,49.1023437499973,
53.0120552744891));
#264505=CARTESIAN_POINT('Ctrl Pts',(7.17401418756679E-15,49.1684895833306,
53.0120552744891));
#264506=CARTESIAN_POINT('Ctrl Pts',(1.96836574383997,49.2346354166639,53.0120552744891));
#264507=CARTESIAN_POINT('Ctrl Pts',(3.36021050916451,49.3007812499973,51.6202105091645));
#264508=CARTESIAN_POINT('Ctrl Pts',(4.75205527448906,49.3669270833306,50.22836574384));
#264509=CARTESIAN_POINT('Ctrl Pts',(4.75205527448906,49.4330729166639,48.26));
#264510=CARTESIAN_POINT('Ctrl Pts',(4.75205527448906,49.4992187499972,46.29163425616));
#264511=CARTESIAN_POINT('Ctrl Pts',(3.36021050916451,49.5653645833305,44.8997894908355));
#264512=CARTESIAN_POINT('Ctrl Pts',(1.96836574383997,49.6315104166638,43.507944725511));
#264513=CARTESIAN_POINT('Ctrl Pts',(6.99959259357482E-15,49.6976562499971,
43.507944725511));
#264514=CARTESIAN_POINT('Ctrl Pts',(-1.96836574383996,49.7638020833304,
43.507944725511));
#264515=CARTESIAN_POINT('Ctrl Pts',(-3.3602105091645,49.8299479166637,44.8997894908355));
#264516=CARTESIAN_POINT('Ctrl Pts',(-4.75205527448904,49.8960937499971,
46.29163425616));
#264517=CARTESIAN_POINT('Ctrl Pts',(-4.75205527448904,49.9622395833304,
48.26));
#264518=CARTESIAN_POINT('Ctrl Pts',(-4.75205527448904,50.0283854166637,
50.22836574384));
#264519=CARTESIAN_POINT('Ctrl Pts',(-3.3602105091645,50.094531249997,51.6202105091645));
#264520=CARTESIAN_POINT('Ctrl Pts',(-1.96836574383996,50.1606770833303,
53.0120552744891));
#264521=CARTESIAN_POINT('Ctrl Pts',(7.17401418756681E-15,50.2268229166636,
53.0120552744891));
#264522=CARTESIAN_POINT('Ctrl Pts',(1.96836574383997,50.2929687499969,53.0120552744891));
#264523=CARTESIAN_POINT('Ctrl Pts',(3.36021050916451,50.3591145833303,51.6202105091645));
#264524=CARTESIAN_POINT('Ctrl Pts',(4.75205527448906,50.4252604166636,50.22836574384));
#264525=CARTESIAN_POINT('Ctrl Pts',(4.75205527448906,50.4914062499969,48.26));
#264526=CARTESIAN_POINT('Ctrl Pts',(4.75205527448906,50.5575520833302,46.29163425616));
#264527=CARTESIAN_POINT('Ctrl Pts',(3.36021050916451,50.6236979166635,44.8997894908355));
#264528=CARTESIAN_POINT('Ctrl Pts',(1.96836574383997,50.6898437499968,43.507944725511));
#264529=CARTESIAN_POINT('Ctrl Pts',(6.99959259357482E-15,50.7559895833301,
43.507944725511));
#264530=CARTESIAN_POINT('Ctrl Pts',(-1.96836574383996,50.8221354166634,
43.507944725511));
#264531=CARTESIAN_POINT('Ctrl Pts',(-3.3602105091645,50.8882812499967,44.8997894908355));
#264532=CARTESIAN_POINT('Ctrl Pts',(-4.75205527448904,50.9544270833301,
46.29163425616));
#264533=CARTESIAN_POINT('Ctrl Pts',(-4.75205527448904,51.0205729166634,
48.26));
#264534=CARTESIAN_POINT('Ctrl Pts',(-4.72273670613182,40.4541666666667,
48.26));
#264535=CARTESIAN_POINT('Ctrl Pts',(-4.72273670613182,40.5203125,50.216221595197));
#264536=CARTESIAN_POINT('Ctrl Pts',(-3.33947915066443,40.5864583333333,
51.5994791506644));
#264537=CARTESIAN_POINT('Ctrl Pts',(-1.95622159519703,40.6526041666666,
52.9827367061318));
#264538=CARTESIAN_POINT('Ctrl Pts',(7.17168088200107E-15,40.7187499999999,
52.9827367061318));
#264539=CARTESIAN_POINT('Ctrl Pts',(1.95622159519705,40.7848958333332,52.9827367061318));
#264540=CARTESIAN_POINT('Ctrl Pts',(3.33947915066444,40.8510416666665,51.5994791506644));
#264541=CARTESIAN_POINT('Ctrl Pts',(4.72273670613183,40.9171874999999,50.216221595197));
#264542=CARTESIAN_POINT('Ctrl Pts',(4.72273670613183,40.9833333333332,48.26));
#264543=CARTESIAN_POINT('Ctrl Pts',(4.72273670613183,41.0494791666665,46.303778404803));
#264544=CARTESIAN_POINT('Ctrl Pts',(3.33947915066444,41.1156249999998,44.9205208493356));
#264545=CARTESIAN_POINT('Ctrl Pts',(1.95622159519705,41.1817708333331,43.5372632938682));
#264546=CARTESIAN_POINT('Ctrl Pts',(6.99833541005117E-15,41.2479166666664,
43.5372632938682));
#264547=CARTESIAN_POINT('Ctrl Pts',(-1.95622159519704,41.3140624999997,
43.5372632938682));
#264548=CARTESIAN_POINT('Ctrl Pts',(-3.33947915066443,41.380208333333,44.9205208493356));
#264549=CARTESIAN_POINT('Ctrl Pts',(-4.72273670613182,41.4463541666663,
46.303778404803));
#264550=CARTESIAN_POINT('Ctrl Pts',(-4.72273670613182,41.5124999999997,
48.26));
#264551=CARTESIAN_POINT('Ctrl Pts',(-4.72273670613182,41.578645833333,50.216221595197));
#264552=CARTESIAN_POINT('Ctrl Pts',(-3.33947915066443,41.6447916666663,
51.5994791506644));
#264553=CARTESIAN_POINT('Ctrl Pts',(-1.95622159519703,41.7109374999996,
52.9827367061318));
#264554=CARTESIAN_POINT('Ctrl Pts',(7.17168088200104E-15,41.7770833333329,
52.9827367061318));
#264555=CARTESIAN_POINT('Ctrl Pts',(1.95622159519705,41.8432291666662,52.9827367061318));
#264556=CARTESIAN_POINT('Ctrl Pts',(3.33947915066444,41.9093749999995,51.5994791506644));
#264557=CARTESIAN_POINT('Ctrl Pts',(4.72273670613183,41.9755208333329,50.216221595197));
#264558=CARTESIAN_POINT('Ctrl Pts',(4.72273670613183,42.0416666666662,48.26));
#264559=CARTESIAN_POINT('Ctrl Pts',(4.72273670613183,42.1078124999995,46.303778404803));
#264560=CARTESIAN_POINT('Ctrl Pts',(3.33947915066444,42.1739583333328,44.9205208493356));
#264561=CARTESIAN_POINT('Ctrl Pts',(1.95622159519705,42.2401041666661,43.5372632938682));
#264562=CARTESIAN_POINT('Ctrl Pts',(6.99833541005117E-15,42.3062499999994,
43.5372632938682));
#264563=CARTESIAN_POINT('Ctrl Pts',(-1.95622159519704,42.3723958333327,
43.5372632938682));
#264564=CARTESIAN_POINT('Ctrl Pts',(-3.33947915066443,42.438541666666,44.9205208493356));
#264565=CARTESIAN_POINT('Ctrl Pts',(-4.72273670613182,42.5046874999994,
46.303778404803));
#264566=CARTESIAN_POINT('Ctrl Pts',(-4.72273670613182,42.5708333333327,
48.26));
#264567=CARTESIAN_POINT('Ctrl Pts',(-4.72273670613182,42.636979166666,50.216221595197));
#264568=CARTESIAN_POINT('Ctrl Pts',(-3.33947915066443,42.7031249999993,
51.5994791506644));
#264569=CARTESIAN_POINT('Ctrl Pts',(-1.95622159519703,42.7692708333326,
52.9827367061318));
#264570=CARTESIAN_POINT('Ctrl Pts',(7.17168088200104E-15,42.8354166666659,
52.9827367061318));
#264571=CARTESIAN_POINT('Ctrl Pts',(1.95622159519705,42.9015624999992,52.9827367061318));
#264572=CARTESIAN_POINT('Ctrl Pts',(3.33947915066444,42.9677083333326,51.5994791506644));
#264573=CARTESIAN_POINT('Ctrl Pts',(4.72273670613183,43.0338541666659,50.216221595197));
#264574=CARTESIAN_POINT('Ctrl Pts',(4.72273670613183,43.0999999999992,48.26));
#264575=CARTESIAN_POINT('Ctrl Pts',(4.72273670613183,43.1661458333325,46.303778404803));
#264576=CARTESIAN_POINT('Ctrl Pts',(3.33947915066444,43.2322916666658,44.9205208493356));
#264577=CARTESIAN_POINT('Ctrl Pts',(1.95622159519705,43.2984374999991,43.5372632938682));
#264578=CARTESIAN_POINT('Ctrl Pts',(6.99833541005117E-15,43.3645833333324,
43.5372632938682));
#264579=CARTESIAN_POINT('Ctrl Pts',(-1.95622159519704,43.4307291666657,
43.5372632938682));
#264580=CARTESIAN_POINT('Ctrl Pts',(-3.33947915066443,43.496874999999,44.9205208493356));
#264581=CARTESIAN_POINT('Ctrl Pts',(-4.72273670613182,43.5630208333324,
46.303778404803));
#264582=CARTESIAN_POINT('Ctrl Pts',(-4.72273670613182,43.6291666666657,
48.26));
#264583=CARTESIAN_POINT('Ctrl Pts',(-4.72273670613182,43.695312499999,50.216221595197));
#264584=CARTESIAN_POINT('Ctrl Pts',(-3.33947915066443,43.7614583333323,
51.5994791506644));
#264585=CARTESIAN_POINT('Ctrl Pts',(-1.95622159519703,43.8276041666656,
52.9827367061318));
#264586=CARTESIAN_POINT('Ctrl Pts',(7.17168088200102E-15,43.8937499999989,
52.9827367061318));
#264587=CARTESIAN_POINT('Ctrl Pts',(1.95622159519705,43.9598958333322,52.9827367061318));
#264588=CARTESIAN_POINT('Ctrl Pts',(3.33947915066444,44.0260416666656,51.5994791506644));
#264589=CARTESIAN_POINT('Ctrl Pts',(4.72273670613183,44.0921874999989,50.216221595197));
#264590=CARTESIAN_POINT('Ctrl Pts',(4.72273670613183,44.1583333333322,48.26));
#264591=CARTESIAN_POINT('Ctrl Pts',(4.72273670613183,44.2244791666655,46.303778404803));
#264592=CARTESIAN_POINT('Ctrl Pts',(3.33947915066444,44.2906249999988,44.9205208493356));
#264593=CARTESIAN_POINT('Ctrl Pts',(1.95622159519705,44.3567708333321,43.5372632938682));
#264594=CARTESIAN_POINT('Ctrl Pts',(6.99833541005117E-15,44.4229166666654,
43.5372632938682));
#264595=CARTESIAN_POINT('Ctrl Pts',(-1.95622159519704,44.4890624999988,
43.5372632938682));
#264596=CARTESIAN_POINT('Ctrl Pts',(-3.33947915066443,44.555208333332,44.9205208493356));
#264597=CARTESIAN_POINT('Ctrl Pts',(-4.72273670613182,44.6213541666654,
46.303778404803));
#264598=CARTESIAN_POINT('Ctrl Pts',(-4.72273670613182,44.6874999999987,
48.26));
#264599=CARTESIAN_POINT('Ctrl Pts',(-4.72273670613182,44.753645833332,50.216221595197));
#264600=CARTESIAN_POINT('Ctrl Pts',(-3.33947915066443,44.8197916666653,
51.5994791506644));
#264601=CARTESIAN_POINT('Ctrl Pts',(-1.95622159519703,44.8859374999986,
52.9827367061318));
#264602=CARTESIAN_POINT('Ctrl Pts',(7.17168088200107E-15,44.9520833333319,
52.9827367061318));
#264603=CARTESIAN_POINT('Ctrl Pts',(1.95622159519705,45.0182291666652,52.9827367061318));
#264604=CARTESIAN_POINT('Ctrl Pts',(3.33947915066444,45.0843749999985,51.5994791506644));
#264605=CARTESIAN_POINT('Ctrl Pts',(4.72273670613183,45.1505208333318,50.216221595197));
#264606=CARTESIAN_POINT('Ctrl Pts',(4.72273670613183,45.2166666666652,48.26));
#264607=CARTESIAN_POINT('Ctrl Pts',(4.72273670613183,45.2828124999985,46.303778404803));
#264608=CARTESIAN_POINT('Ctrl Pts',(3.33947915066444,45.3489583333318,44.9205208493356));
#264609=CARTESIAN_POINT('Ctrl Pts',(1.95622159519705,45.4151041666651,43.5372632938682));
#264610=CARTESIAN_POINT('Ctrl Pts',(6.99833541005117E-15,45.4812499999984,
43.5372632938682));
#264611=CARTESIAN_POINT('Ctrl Pts',(-1.95622159519704,45.5473958333317,
43.5372632938682));
#264612=CARTESIAN_POINT('Ctrl Pts',(-3.33947915066443,45.613541666665,44.9205208493356));
#264613=CARTESIAN_POINT('Ctrl Pts',(-4.72273670613182,45.6796874999984,
46.303778404803));
#264614=CARTESIAN_POINT('Ctrl Pts',(-4.72273670613182,45.7458333333317,
48.26));
#264615=CARTESIAN_POINT('Ctrl Pts',(-4.72273670613182,45.811979166665,50.216221595197));
#264616=CARTESIAN_POINT('Ctrl Pts',(-3.33947915066443,45.8781249999983,
51.5994791506644));
#264617=CARTESIAN_POINT('Ctrl Pts',(-1.95622159519703,45.9442708333316,
52.9827367061318));
#264618=CARTESIAN_POINT('Ctrl Pts',(7.17168088200104E-15,46.0104166666649,
52.9827367061318));
#264619=CARTESIAN_POINT('Ctrl Pts',(1.95622159519705,46.0765624999982,52.9827367061318));
#264620=CARTESIAN_POINT('Ctrl Pts',(3.33947915066444,46.1427083333315,51.5994791506644));
#264621=CARTESIAN_POINT('Ctrl Pts',(4.72273670613183,46.2088541666649,50.216221595197));
#264622=CARTESIAN_POINT('Ctrl Pts',(4.72273670613183,46.2749999999982,48.26));
#264623=CARTESIAN_POINT('Ctrl Pts',(4.72273670613183,46.3411458333315,46.303778404803));
#264624=CARTESIAN_POINT('Ctrl Pts',(3.33947915066444,46.4072916666648,44.9205208493356));
#264625=CARTESIAN_POINT('Ctrl Pts',(1.95622159519705,46.4734374999981,43.5372632938682));
#264626=CARTESIAN_POINT('Ctrl Pts',(6.99833541005117E-15,46.5395833333314,
43.5372632938682));
#264627=CARTESIAN_POINT('Ctrl Pts',(-1.95622159519704,46.6057291666647,
43.5372632938682));
#264628=CARTESIAN_POINT('Ctrl Pts',(-3.33947915066443,46.671874999998,44.9205208493356));
#264629=CARTESIAN_POINT('Ctrl Pts',(-4.72273670613182,46.7380208333314,
46.303778404803));
#264630=CARTESIAN_POINT('Ctrl Pts',(-4.72273670613182,46.8041666666647,
48.26));
#264631=CARTESIAN_POINT('Ctrl Pts',(-4.72273670613182,46.870312499998,50.216221595197));
#264632=CARTESIAN_POINT('Ctrl Pts',(-3.33947915066443,46.9364583333313,
51.5994791506644));
#264633=CARTESIAN_POINT('Ctrl Pts',(-1.95622159519703,47.0026041666646,
52.9827367061318));
#264634=CARTESIAN_POINT('Ctrl Pts',(7.17168088200104E-15,47.0687499999979,
52.9827367061318));
#264635=CARTESIAN_POINT('Ctrl Pts',(1.95622159519705,47.1348958333312,52.9827367061318));
#264636=CARTESIAN_POINT('Ctrl Pts',(3.33947915066444,47.2010416666646,51.5994791506644));
#264637=CARTESIAN_POINT('Ctrl Pts',(4.72273670613183,47.2671874999979,50.216221595197));
#264638=CARTESIAN_POINT('Ctrl Pts',(4.72273670613183,47.3333333333312,48.26));
#264639=CARTESIAN_POINT('Ctrl Pts',(4.72273670613183,47.3994791666645,46.303778404803));
#264640=CARTESIAN_POINT('Ctrl Pts',(3.33947915066444,47.4656249999978,44.9205208493356));
#264641=CARTESIAN_POINT('Ctrl Pts',(1.95622159519705,47.5317708333311,43.5372632938682));
#264642=CARTESIAN_POINT('Ctrl Pts',(6.99833541005117E-15,47.5979166666644,
43.5372632938682));
#264643=CARTESIAN_POINT('Ctrl Pts',(-1.95622159519704,47.6640624999977,
43.5372632938682));
#264644=CARTESIAN_POINT('Ctrl Pts',(-3.33947915066443,47.730208333331,44.9205208493356));
#264645=CARTESIAN_POINT('Ctrl Pts',(-4.72273670613182,47.7963541666644,
46.303778404803));
#264646=CARTESIAN_POINT('Ctrl Pts',(-4.72273670613182,47.8624999999977,
48.26));
#264647=CARTESIAN_POINT('Ctrl Pts',(-4.72273670613182,47.928645833331,50.216221595197));
#264648=CARTESIAN_POINT('Ctrl Pts',(-3.33947915066443,47.9947916666643,
51.5994791506644));
#264649=CARTESIAN_POINT('Ctrl Pts',(-1.95622159519703,48.0609374999976,
52.9827367061318));
#264650=CARTESIAN_POINT('Ctrl Pts',(7.17168088200102E-15,48.1270833333309,
52.9827367061318));
#264651=CARTESIAN_POINT('Ctrl Pts',(1.95622159519705,48.1932291666642,52.9827367061318));
#264652=CARTESIAN_POINT('Ctrl Pts',(3.33947915066444,48.2593749999975,51.5994791506644));
#264653=CARTESIAN_POINT('Ctrl Pts',(4.72273670613183,48.3255208333309,50.216221595197));
#264654=CARTESIAN_POINT('Ctrl Pts',(4.72273670613183,48.3916666666642,48.26));
#264655=CARTESIAN_POINT('Ctrl Pts',(4.72273670613183,48.4578124999975,46.303778404803));
#264656=CARTESIAN_POINT('Ctrl Pts',(3.33947915066444,48.5239583333308,44.9205208493356));
#264657=CARTESIAN_POINT('Ctrl Pts',(1.95622159519705,48.5901041666641,43.5372632938682));
#264658=CARTESIAN_POINT('Ctrl Pts',(6.99833541005117E-15,48.6562499999974,
43.5372632938682));
#264659=CARTESIAN_POINT('Ctrl Pts',(-1.95622159519704,48.7223958333307,
43.5372632938682));
#264660=CARTESIAN_POINT('Ctrl Pts',(-3.33947915066443,48.788541666664,44.9205208493356));
#264661=CARTESIAN_POINT('Ctrl Pts',(-4.72273670613182,48.8546874999974,
46.303778404803));
#264662=CARTESIAN_POINT('Ctrl Pts',(-4.72273670613182,48.9208333333307,
48.26));
#264663=CARTESIAN_POINT('Ctrl Pts',(-4.72273670613182,48.986979166664,50.216221595197));
#264664=CARTESIAN_POINT('Ctrl Pts',(-3.33947915066443,49.0531249999973,
51.5994791506644));
#264665=CARTESIAN_POINT('Ctrl Pts',(-1.95622159519703,49.1192708333306,
52.9827367061318));
#264666=CARTESIAN_POINT('Ctrl Pts',(7.17168088200102E-15,49.1854166666639,
52.9827367061318));
#264667=CARTESIAN_POINT('Ctrl Pts',(1.95622159519705,49.2515624999972,52.9827367061318));
#264668=CARTESIAN_POINT('Ctrl Pts',(3.33947915066444,49.3177083333306,51.5994791506644));
#264669=CARTESIAN_POINT('Ctrl Pts',(4.72273670613183,49.3838541666639,50.216221595197));
#264670=CARTESIAN_POINT('Ctrl Pts',(4.72273670613183,49.4499999999972,48.26));
#264671=CARTESIAN_POINT('Ctrl Pts',(4.72273670613183,49.5161458333305,46.303778404803));
#264672=CARTESIAN_POINT('Ctrl Pts',(3.33947915066444,49.5822916666638,44.9205208493356));
#264673=CARTESIAN_POINT('Ctrl Pts',(1.95622159519705,49.6484374999971,43.5372632938682));
#264674=CARTESIAN_POINT('Ctrl Pts',(6.99833541005115E-15,49.7145833333304,
43.5372632938682));
#264675=CARTESIAN_POINT('Ctrl Pts',(-1.95622159519704,49.7807291666637,
43.5372632938682));
#264676=CARTESIAN_POINT('Ctrl Pts',(-3.33947915066443,49.846874999997,44.9205208493356));
#264677=CARTESIAN_POINT('Ctrl Pts',(-4.72273670613182,49.9130208333304,
46.303778404803));
#264678=CARTESIAN_POINT('Ctrl Pts',(-4.72273670613182,49.9791666666637,
48.26));
#264679=CARTESIAN_POINT('Ctrl Pts',(-4.72273670613182,50.045312499997,50.216221595197));
#264680=CARTESIAN_POINT('Ctrl Pts',(-3.33947915066443,50.1114583333303,
51.5994791506644));
#264681=CARTESIAN_POINT('Ctrl Pts',(-1.95622159519703,50.1776041666636,
52.9827367061318));
#264682=CARTESIAN_POINT('Ctrl Pts',(7.17168088200107E-15,50.2437499999969,
52.9827367061318));
#264683=CARTESIAN_POINT('Ctrl Pts',(1.95622159519705,50.3098958333302,52.9827367061318));
#264684=CARTESIAN_POINT('Ctrl Pts',(3.33947915066444,50.3760416666636,51.5994791506644));
#264685=CARTESIAN_POINT('Ctrl Pts',(4.72273670613183,50.4421874999969,50.216221595197));
#264686=CARTESIAN_POINT('Ctrl Pts',(4.72273670613183,50.5083333333302,48.26));
#264687=CARTESIAN_POINT('Ctrl Pts',(4.72273670613183,50.5744791666635,46.303778404803));
#264688=CARTESIAN_POINT('Ctrl Pts',(3.33947915066444,50.6406249999968,44.9205208493356));
#264689=CARTESIAN_POINT('Ctrl Pts',(1.95622159519705,50.7067708333301,43.5372632938682));
#264690=CARTESIAN_POINT('Ctrl Pts',(6.99833541005117E-15,50.7729166666634,
43.5372632938682));
#264691=CARTESIAN_POINT('Ctrl Pts',(-1.95622159519704,50.8390624999967,
43.5372632938682));
#264692=CARTESIAN_POINT('Ctrl Pts',(-3.33947915066443,50.90520833333,44.9205208493356));
#264693=CARTESIAN_POINT('Ctrl Pts',(-4.72273670613182,50.9713541666634,
46.303778404803));
#264694=CARTESIAN_POINT('Ctrl Pts',(-4.72273670613182,51.0374999999967,
48.26));
#264695=CARTESIAN_POINT('Origin',(-1.38777878078145E-14,-1.38777878078145E-14,
4.05352706259476));
#264696=CARTESIAN_POINT('',(40.,-1.87763750044039E-14,4.05352706259477));
#264697=CARTESIAN_POINT('Origin',(-1.38777878078145E-14,-1.38777878078145E-14,
4.05352706259476));
#264698=CARTESIAN_POINT('',(41.2700000000001,-1.89319051478956E-14,2.54));
#264699=CARTESIAN_POINT('',(40.,-1.87763750044039E-14,4.05352706259476));
#264700=CARTESIAN_POINT('Origin',(-1.38777878078145E-14,-1.38777878078145E-14,
2.54));
#264701=CARTESIAN_POINT('Origin',(-1.38777878078145E-14,-1.38777878078145E-14,
61.9864729374053));
#264702=CARTESIAN_POINT('',(40.,-8.97920061122505E-15,61.9864729374053));
#264703=CARTESIAN_POINT('',(-40.,-1.87763750044039E-14,61.9864729374053));
#264704=CARTESIAN_POINT('Origin',(-1.38777878078145E-14,-1.38777878078145E-14,
61.9864729374053));
#264705=CARTESIAN_POINT('Origin',(-1.38777878078145E-14,-1.38777878078145E-14,
61.9864729374053));
#264706=CARTESIAN_POINT('',(-41.2700000000001,-1.89319051478956E-14,63.5));
#264707=CARTESIAN_POINT('',(-40.,-1.87763750044039E-14,61.9864729374053));
#264708=CARTESIAN_POINT('Origin',(-1.38777878078145E-14,-1.38777878078145E-14,
63.5));
#264709=CARTESIAN_POINT('Origin',(-1.38777878078145E-14,-1.38777878078145E-14,
63.5));
#264710=CARTESIAN_POINT('',(50.,-2.00010218035512E-14,62.2300000000001));
#264711=CARTESIAN_POINT('Origin',(-1.38777878078145E-14,-1.38777878078145E-14,
62.2300000000001));
#264712=CARTESIAN_POINT('',(48.4864729374054,-1.98156681962883E-14,63.5));
#264713=CARTESIAN_POINT('',(48.4864729374054,-1.98156681962883E-14,63.5));
#264714=CARTESIAN_POINT('Origin',(-1.38777878078145E-14,-1.38777878078145E-14,
63.5));
#264715=CARTESIAN_POINT('Origin',(-1.38777878078145E-14,-1.38777878078145E-14,
2.53999999999999));
#264716=CARTESIAN_POINT('',(50.,-7.75455381207769E-15,3.80999999999998));
#264717=CARTESIAN_POINT('',(-50.,-2.00010218035512E-14,3.80999999999998));
#264718=CARTESIAN_POINT('Origin',(-1.38777878078145E-14,-1.38777878078145E-14,
3.80999999999998));
#264719=CARTESIAN_POINT('Origin',(-1.38777878078145E-14,-1.38777878078145E-14,
3.80999999999998));
#264720=CARTESIAN_POINT('',(-48.4864729374054,-1.98156681962883E-14,2.54));
#264721=CARTESIAN_POINT('',(-48.4864729374054,-1.98156681962883E-14,2.53999999999999));
#264722=CARTESIAN_POINT('Origin',(-1.38777878078145E-14,-1.38777878078145E-14,
2.54));
#264723=CARTESIAN_POINT('Origin',(-1.38777878078145E-14,-1.38777878078145E-14,
268.42135623731));
#264724=CARTESIAN_POINT('',(50.,-9.74305740910067E-14,43.4975));
#264725=CARTESIAN_POINT('',(50.,-2.00010218035512E-14,268.42135623731));
#264726=CARTESIAN_POINT('',(50.,-1.75157305013873E-13,53.0225));
#264727=CARTESIAN_POINT('Ctrl Pts',(50.,-1.7499890425654E-13,53.0225));
#264728=CARTESIAN_POINT('Ctrl Pts',(50.,-0.598378688298317,53.0225));
#264729=CARTESIAN_POINT('Ctrl Pts',(49.9881578769847,-1.23639552071279,
52.9028396534865));
#264730=CARTESIAN_POINT('Ctrl Pts',(49.9453510199711,-2.40967078999247,
52.4166958716389));
#264731=CARTESIAN_POINT('Ctrl Pts',(49.9149942232673,-2.94495962679791,
52.0502324640042));
#264732=CARTESIAN_POINT('Ctrl Pts',(49.8579338261974,-3.79023364706856,
51.2049584437335));
#264733=CARTESIAN_POINT('Ctrl Pts',(49.8275167150177,-4.15669613276604,
50.6696701266124));
#264734=CARTESIAN_POINT('Ctrl Pts',(49.7845717960014,-4.64283922274571,
49.4963965934443));
#264735=CARTESIAN_POINT('Ctrl Pts',(49.7726691443205,-4.76250000000018,
48.8583803633087));
#264736=CARTESIAN_POINT('Ctrl Pts',(49.7726691443205,-4.76250000000018,
47.6616196366914));
#264737=CARTESIAN_POINT('Ctrl Pts',(49.7845717960014,-4.64283922274571,
47.0236034065557));
#264738=CARTESIAN_POINT('Ctrl Pts',(49.8275167150177,-4.15669613276604,
45.8503298733876));
#264739=CARTESIAN_POINT('Ctrl Pts',(49.8579338261974,-3.79023364706856,
45.3150415562665));
#264740=CARTESIAN_POINT('Ctrl Pts',(49.9149942232673,-2.94495962679791,
44.4697675359959));
#264741=CARTESIAN_POINT('Ctrl Pts',(49.9453510199711,-2.40967078999247,
44.1033041283611));
#264742=CARTESIAN_POINT('Ctrl Pts',(49.9881578769847,-1.23639552071278,
43.6171603465136));
#264743=CARTESIAN_POINT('Ctrl Pts',(50.,-0.598378688298317,43.4975));
#264744=CARTESIAN_POINT('Ctrl Pts',(50.,-1.74860126378462E-13,43.4975));
#264745=CARTESIAN_POINT('',(50.,-2.00010218035512E-14,268.42135623731));
#264746=CARTESIAN_POINT('Ctrl Pts',(50.,-1.74582570622306E-13,43.4975));
#264747=CARTESIAN_POINT('Ctrl Pts',(50.,0.598378688297968,43.4975));
#264748=CARTESIAN_POINT('Ctrl Pts',(49.9881578769847,1.23639552071243,43.6171603465136));
#264749=CARTESIAN_POINT('Ctrl Pts',(49.9453510199711,2.40967078999212,44.1033041283611));
#264750=CARTESIAN_POINT('Ctrl Pts',(49.9149942232673,2.94495962679757,44.4697675359959));
#264751=CARTESIAN_POINT('Ctrl Pts',(49.8579338261974,3.79023364706821,45.3150415562665));
#264752=CARTESIAN_POINT('Ctrl Pts',(49.8275167150177,4.15669613276569,45.8503298733876));
#264753=CARTESIAN_POINT('Ctrl Pts',(49.7845717960014,4.64283922274536,47.0236034065557));
#264754=CARTESIAN_POINT('Ctrl Pts',(49.7726691443206,4.76249999999983,47.6616196366914));
#264755=CARTESIAN_POINT('Ctrl Pts',(49.7726691443206,4.76249999999983,48.26));
#264756=CARTESIAN_POINT('Ctrl Pts',(49.7726691443206,4.76249999999983,48.8583803633087));
#264757=CARTESIAN_POINT('Ctrl Pts',(49.7845717960014,4.64283922274536,49.4963965934443));
#264758=CARTESIAN_POINT('Ctrl Pts',(49.8275167150177,4.15669613276569,50.6696701266124));
#264759=CARTESIAN_POINT('Ctrl Pts',(49.8579338261974,3.79023364706821,51.2049584437335));
#264760=CARTESIAN_POINT('Ctrl Pts',(49.9149942232673,2.94495962679757,52.0502324640042));
#264761=CARTESIAN_POINT('Ctrl Pts',(49.9453510199711,2.40967078999212,52.4166958716389));
#264762=CARTESIAN_POINT('Ctrl Pts',(49.9881578769847,1.23639552071243,52.9028396534865));
#264763=CARTESIAN_POINT('Ctrl Pts',(50.,0.598378688297967,53.0225));
#264764=CARTESIAN_POINT('Ctrl Pts',(50.,-1.75276460012697E-13,53.0225));
#264765=CARTESIAN_POINT('',(1.31536147873854E-15,50.,43.4975));
#264766=CARTESIAN_POINT('',(-5.83238038093927E-16,50.,53.0225));
#264767=CARTESIAN_POINT('Ctrl Pts',(4.16333634234434E-16,50.,43.4975));
#264768=CARTESIAN_POINT('Ctrl Pts',(-0.598378688298142,50.,43.4975));
#264769=CARTESIAN_POINT('Ctrl Pts',(-1.23639552071261,49.9881578769847,
43.6171603465136));
#264770=CARTESIAN_POINT('Ctrl Pts',(-2.40967078999229,49.9453510199711,
44.1033041283611));
#264771=CARTESIAN_POINT('Ctrl Pts',(-2.94495962679774,49.9149942232673,
44.4697675359959));
#264772=CARTESIAN_POINT('Ctrl Pts',(-3.79023364706838,49.8579338261974,
45.3150415562665));
#264773=CARTESIAN_POINT('Ctrl Pts',(-4.15669613276586,49.8275167150177,
45.8503298733876));
#264774=CARTESIAN_POINT('Ctrl Pts',(-4.64283922274554,49.7845717960014,
47.0236034065557));
#264775=CARTESIAN_POINT('Ctrl Pts',(-4.7625,49.7726691443205,47.6616196366914));
#264776=CARTESIAN_POINT('Ctrl Pts',(-4.7625,49.7726691443205,48.26));
#264777=CARTESIAN_POINT('Ctrl Pts',(-4.7625,49.7726691443205,48.8583803633087));
#264778=CARTESIAN_POINT('Ctrl Pts',(-4.64283922274554,49.7845717960014,
49.4963965934443));
#264779=CARTESIAN_POINT('Ctrl Pts',(-4.15669613276586,49.8275167150177,
50.6696701266124));
#264780=CARTESIAN_POINT('Ctrl Pts',(-3.79023364706839,49.8579338261974,
51.2049584437335));
#264781=CARTESIAN_POINT('Ctrl Pts',(-2.94495962679774,49.9149942232673,
52.0502324640042));
#264782=CARTESIAN_POINT('Ctrl Pts',(-2.4096707899923,49.9453510199711,52.4166958716389));
#264783=CARTESIAN_POINT('Ctrl Pts',(-1.23639552071261,49.9881578769847,
52.9028396534865));
#264784=CARTESIAN_POINT('Ctrl Pts',(-0.598378688298142,50.,53.0225));
#264785=CARTESIAN_POINT('Ctrl Pts',(1.38777878078145E-16,50.,53.0225));
#264786=CARTESIAN_POINT('Ctrl Pts',(-5.55111512312578E-16,50.,53.0225));
#264787=CARTESIAN_POINT('Ctrl Pts',(0.598378688298142,50.,53.0225));
#264788=CARTESIAN_POINT('Ctrl Pts',(1.23639552071261,49.9881578769847,52.9028396534865));
#264789=CARTESIAN_POINT('Ctrl Pts',(2.40967078999229,49.9453510199711,52.4166958716389));
#264790=CARTESIAN_POINT('Ctrl Pts',(2.94495962679774,49.9149942232673,52.0502324640042));
#264791=CARTESIAN_POINT('Ctrl Pts',(3.79023364706838,49.8579338261974,51.2049584437335));
#264792=CARTESIAN_POINT('Ctrl Pts',(4.15669613276586,49.8275167150177,50.6696701266124));
#264793=CARTESIAN_POINT('Ctrl Pts',(4.64283922274554,49.7845717960014,49.4963965934443));
#264794=CARTESIAN_POINT('Ctrl Pts',(4.7625,49.7726691443205,48.8583803633087));
#264795=CARTESIAN_POINT('Ctrl Pts',(4.7625,49.7726691443205,47.6616196366914));
#264796=CARTESIAN_POINT('Ctrl Pts',(4.64283922274554,49.7845717960014,47.0236034065557));
#264797=CARTESIAN_POINT('Ctrl Pts',(4.15669613276586,49.8275167150177,45.8503298733876));
#264798=CARTESIAN_POINT('Ctrl Pts',(3.79023364706839,49.8579338261974,45.3150415562665));
#264799=CARTESIAN_POINT('Ctrl Pts',(2.94495962679774,49.9149942232673,44.4697675359959));
#264800=CARTESIAN_POINT('Ctrl Pts',(2.4096707899923,49.9453510199711,44.1033041283611));
#264801=CARTESIAN_POINT('Ctrl Pts',(1.23639552071261,49.9881578769847,43.6171603465136));
#264802=CARTESIAN_POINT('Ctrl Pts',(0.598378688298144,50.,43.4975));
#264803=CARTESIAN_POINT('Ctrl Pts',(1.11022302462516E-15,50.,43.4975));
#264804=CARTESIAN_POINT('Origin',(0.,115.,48.26));
#264805=CARTESIAN_POINT('',(5.83238094526905E-16,40.,53.0225));
#264806=CARTESIAN_POINT('',(-5.83238038093927E-16,115.,53.0225));
#264807=CARTESIAN_POINT('Ctrl Pts',(-4.7625,39.7154704586261,48.26));
#264808=CARTESIAN_POINT('Ctrl Pts',(-4.7625,39.7154704586261,48.8586021223598));
#264809=CARTESIAN_POINT('Ctrl Pts',(-4.64275284127331,39.7303998106907,
49.4967123644842));
#264810=CARTESIAN_POINT('Ctrl Pts',(-4.15654655972588,39.7842046972333,
50.6699237637271));
#264811=CARTESIAN_POINT('Ctrl Pts',(-3.79011828934085,39.8222902757623,
51.205073801461));
#264812=CARTESIAN_POINT('Ctrl Pts',(-2.94507670291011,39.8936877237352,
52.0501153878918));
#264813=CARTESIAN_POINT('Ctrl Pts',(-2.40992540144616,39.9316551722397,
52.416545929979));
#264814=CARTESIAN_POINT('Ctrl Pts',(-1.23670973303352,39.9851894363656,
52.9027538828458));
#264815=CARTESIAN_POINT('Ctrl Pts',(-0.598598011774796,40.,53.0225));
#264816=CARTESIAN_POINT('Ctrl Pts',(0.598598011774795,40.,53.0225));
#264817=CARTESIAN_POINT('Ctrl Pts',(1.23670973303352,39.9851894363656,52.9027538828458));
#264818=CARTESIAN_POINT('Ctrl Pts',(2.40992540144616,39.9316551722397,52.416545929979));
#264819=CARTESIAN_POINT('Ctrl Pts',(2.94507670291011,39.8936877237352,52.0501153878918));
#264820=CARTESIAN_POINT('Ctrl Pts',(3.79011828934085,39.8222902757623,51.205073801461));
#264821=CARTESIAN_POINT('Ctrl Pts',(4.15654655972588,39.7842046972333,50.6699237637271));
#264822=CARTESIAN_POINT('Ctrl Pts',(4.64275284127331,39.7303998106907,49.4967123644842));
#264823=CARTESIAN_POINT('Ctrl Pts',(4.7625,39.7154704586261,48.8586021223598));
#264824=CARTESIAN_POINT('Ctrl Pts',(4.7625,39.7154704586261,47.6613978776402));
#264825=CARTESIAN_POINT('Ctrl Pts',(4.64275284127331,39.7303998106907,47.0232876355158));
#264826=CARTESIAN_POINT('Ctrl Pts',(4.15654655972588,39.7842046972333,45.8500762362729));
#264827=CARTESIAN_POINT('Ctrl Pts',(3.79011828934085,39.8222902757623,45.314926198539));
#264828=CARTESIAN_POINT('Ctrl Pts',(2.94507670291011,39.8936877237352,44.4698846121082));
#264829=CARTESIAN_POINT('Ctrl Pts',(2.40992540144616,39.9316551722397,44.103454070021));
#264830=CARTESIAN_POINT('Ctrl Pts',(1.23670973303352,39.9851894363656,43.6172461171542));
#264831=CARTESIAN_POINT('Ctrl Pts',(0.598598011774796,40.,43.4975));
#264832=CARTESIAN_POINT('Ctrl Pts',(-0.598598011774794,40.,43.4975));
#264833=CARTESIAN_POINT('Ctrl Pts',(-1.23670973303352,39.9851894363656,
43.6172461171542));
#264834=CARTESIAN_POINT('Ctrl Pts',(-2.40992540144616,39.9316551722397,
44.103454070021));
#264835=CARTESIAN_POINT('Ctrl Pts',(-2.94507670291011,39.8936877237352,
44.4698846121082));
#264836=CARTESIAN_POINT('Ctrl Pts',(-3.79011828934085,39.8222902757623,
45.314926198539));
#264837=CARTESIAN_POINT('Ctrl Pts',(-4.15654655972588,39.7842046972333,
45.8500762362729));
#264838=CARTESIAN_POINT('Ctrl Pts',(-4.64275284127331,39.7303998106907,
47.0232876355158));
#264839=CARTESIAN_POINT('Ctrl Pts',(-4.7625,39.7154704586261,47.6613978776402));
#264840=CARTESIAN_POINT('Ctrl Pts',(-4.7625,39.7154704586261,48.26));
#264841=CARTESIAN_POINT('Origin',(115.,-4.0152035396696E-13,48.26));
#264842=CARTESIAN_POINT('',(40.,-8.97920066765691E-15,53.0225));
#264843=CARTESIAN_POINT('',(115.,-4.00937115928867E-13,53.0225));
#264844=CARTESIAN_POINT('',(40.,-7.98179606268603E-14,43.4975));
#264845=CARTESIAN_POINT('Ctrl Pts',(40.,-1.40998324127395E-13,43.4975));
#264846=CARTESIAN_POINT('Ctrl Pts',(40.,0.598598011774654,43.4975));
#264847=CARTESIAN_POINT('Ctrl Pts',(39.9851894363656,1.23670973303338,43.6172461171542));
#264848=CARTESIAN_POINT('Ctrl Pts',(39.9316551722397,2.40992540144602,44.103454070021));
#264849=CARTESIAN_POINT('Ctrl Pts',(39.8936877237352,2.94507670290997,44.4698846121082));
#264850=CARTESIAN_POINT('Ctrl Pts',(39.8222902757623,3.79011828934071,45.314926198539));
#264851=CARTESIAN_POINT('Ctrl Pts',(39.7842046972333,4.15654655972574,45.8500762362729));
#264852=CARTESIAN_POINT('Ctrl Pts',(39.7303998106907,4.64275284127317,47.0232876355158));
#264853=CARTESIAN_POINT('Ctrl Pts',(39.7154704586261,4.76249999999986,47.6613978776402));
#264854=CARTESIAN_POINT('Ctrl Pts',(39.7154704586261,4.76249999999986,48.26));
#264855=CARTESIAN_POINT('Ctrl Pts',(39.7154704586261,4.76249999999986,48.8586021223598));
#264856=CARTESIAN_POINT('Ctrl Pts',(39.7303998106907,4.64275284127317,49.4967123644842));
#264857=CARTESIAN_POINT('Ctrl Pts',(39.7842046972333,4.15654655972574,50.6699237637271));
#264858=CARTESIAN_POINT('Ctrl Pts',(39.8222902757623,3.79011828934071,51.205073801461));
#264859=CARTESIAN_POINT('Ctrl Pts',(39.8936877237352,2.94507670290997,52.0501153878918));
#264860=CARTESIAN_POINT('Ctrl Pts',(39.9316551722397,2.40992540144602,52.416545929979));
#264861=CARTESIAN_POINT('Ctrl Pts',(39.9851894363656,1.23670973303338,52.9027538828458));
#264862=CARTESIAN_POINT('Ctrl Pts',(40.,0.598598011774656,53.0225));
#264863=CARTESIAN_POINT('Ctrl Pts',(40.,-1.39471767468535E-13,53.0225));
#264864=CARTESIAN_POINT('Ctrl Pts',(40.,-1.38777878078145E-13,53.0225));
#264865=CARTESIAN_POINT('Ctrl Pts',(40.,-0.598598011774934,53.0225));
#264866=CARTESIAN_POINT('Ctrl Pts',(39.9851894363656,-1.23670973303366,
52.9027538828458));
#264867=CARTESIAN_POINT('Ctrl Pts',(39.9316551722397,-2.4099254014463,52.416545929979));
#264868=CARTESIAN_POINT('Ctrl Pts',(39.8936877237351,-2.94507670291025,
52.0501153878918));
#264869=CARTESIAN_POINT('Ctrl Pts',(39.8222902757623,-3.79011828934099,
51.205073801461));
#264870=CARTESIAN_POINT('Ctrl Pts',(39.7842046972333,-4.15654655972601,
50.6699237637271));
#264871=CARTESIAN_POINT('Ctrl Pts',(39.7303998106907,-4.64275284127345,
49.4967123644842));
#264872=CARTESIAN_POINT('Ctrl Pts',(39.715470458626,-4.76250000000014,48.8586021223598));
#264873=CARTESIAN_POINT('Ctrl Pts',(39.715470458626,-4.76250000000014,47.6613978776402));
#264874=CARTESIAN_POINT('Ctrl Pts',(39.7303998106907,-4.64275284127345,
47.0232876355158));
#264875=CARTESIAN_POINT('Ctrl Pts',(39.7842046972333,-4.15654655972602,
45.850076236273));
#264876=CARTESIAN_POINT('Ctrl Pts',(39.8222902757623,-3.79011828934099,
45.314926198539));
#264877=CARTESIAN_POINT('Ctrl Pts',(39.8936877237351,-2.94507670291025,
44.4698846121082));
#264878=CARTESIAN_POINT('Ctrl Pts',(39.9316551722397,-2.4099254014463,44.103454070021));
#264879=CARTESIAN_POINT('Ctrl Pts',(39.9851894363656,-1.23670973303366,
43.6172461171542));
#264880=CARTESIAN_POINT('Ctrl Pts',(40.,-0.598598011774937,43.4975));
#264881=CARTESIAN_POINT('Ctrl Pts',(40.,-1.41414657761629E-13,43.4975));
#264882=CARTESIAN_POINT('Origin',(-1.38777878078145E-14,-1.38777878078145E-14,
268.42135623731));
#264883=CARTESIAN_POINT('',(40.,-1.87763750044039E-14,268.42135623731));
#264884=CARTESIAN_POINT('',(40.,-1.87763750044039E-14,268.42135623731));
#264885=CARTESIAN_POINT('Origin',(-90.,-90.,63.5));
#264886=CARTESIAN_POINT('Origin',(-90.,-90.,2.54));
#264887=CARTESIAN_POINT('Origin',(0.,0.,0.));
#264888=CARTESIAN_POINT('',(65.0000000000002,-7.96020419445782E-15,4.08753198860307));
#264889=CARTESIAN_POINT('Origin',(5.7559361144865E-16,0.,4.08753198860308));
#264890=CARTESIAN_POINT('',(65.0000000000002,-7.96020419445782E-15,7.62));
#264891=CARTESIAN_POINT('',(65.0000000000002,-7.96020419445782E-15,-9.15309894784421E-15));
#264892=CARTESIAN_POINT('Origin',(8.94187358750932E-16,0.,7.62));
#264893=CARTESIAN_POINT('Origin',(0.,0.,-195.421614460986));
#264894=CARTESIAN_POINT('',(-56.875,-6.96517867015057E-15,4.08753198860303));
#264895=CARTESIAN_POINT('Origin',(5.75593611448643E-16,0.,4.08753198860302));
#264896=CARTESIAN_POINT('',(-56.875,-6.96517867015057E-15,17.4625));
#264897=CARTESIAN_POINT('',(-56.875,-6.96517867015057E-15,-195.421614460986));
#264898=CARTESIAN_POINT('Origin',(0.,0.,17.4625));
#264899=CARTESIAN_POINT('Origin',(0.,0.,0.952499999999995));
#264900=CARTESIAN_POINT('',(74.8702478255888,-9.16896093509764E-15,2.54));
#264901=CARTESIAN_POINT('Origin',(0.,0.,2.54));
#264902=CARTESIAN_POINT('',(76.4577478255888,-9.36337361446228E-15,0.952499999999995));
#264903=CARTESIAN_POINT('Origin',(74.8702478255888,-9.16896093509764E-15,
0.952499999999995));
#264904=CARTESIAN_POINT('',(-76.4577478255888,9.36337361446228E-15,0.952499999999995));
#264905=CARTESIAN_POINT('Origin',(0.,0.,0.952499999999995));
#264906=CARTESIAN_POINT('Origin',(0.,0.,0.952499999999995));
#264907=CARTESIAN_POINT('Origin',(0.,0.,-216.614378091742));
#264908=CARTESIAN_POINT('',(-76.4577478255888,-9.36337361446228E-15,0.));
#264909=CARTESIAN_POINT('Origin',(0.,0.,0.));
#264910=CARTESIAN_POINT('',(-76.4577478255888,-9.36337361446228E-15,-216.614378091742));
#264911=CARTESIAN_POINT('Origin',(0.,0.,-195.421614460986));
#264912=CARTESIAN_POINT('',(17.3379110419349,64.705964905612,2.54));
#264913=CARTESIAN_POINT('',(17.3379110419349,-64.705964905612,2.54));
#264914=CARTESIAN_POINT('Origin',(0.,0.,2.53999999999999));
#264915=CARTESIAN_POINT('',(17.3379110419349,-64.705964905612,7.62));
#264916=CARTESIAN_POINT('',(17.3379110419349,-64.705964905612,7.62));
#264917=CARTESIAN_POINT('',(17.3379110419349,64.705964905612,7.62));
#264918=CARTESIAN_POINT('Origin',(0.,0.,7.62));
#264919=CARTESIAN_POINT('',(17.3379110419349,64.705964905612,7.62));
#264920=CARTESIAN_POINT('Origin',(0.,0.,-197.2176656852));
#264921=CARTESIAN_POINT('',(-70.625,-8.64906801897818E-15,17.4625));
#264922=CARTESIAN_POINT('Origin',(0.,0.,17.4625));
#264923=CARTESIAN_POINT('',(-70.625,-8.64906801897818E-15,8.25500000000002));
#264924=CARTESIAN_POINT('',(-70.625,-8.64906801897818E-15,-197.2176656852));
#264925=CARTESIAN_POINT('Origin',(0.,0.,8.255));
#264926=CARTESIAN_POINT('Origin',(0.,0.,228.814169979695));
#264927=CARTESIAN_POINT('',(76.5847478255888,-9.37892662881146E-15,0.));
#264928=CARTESIAN_POINT('Origin',(0.,0.,0.));
#264929=CARTESIAN_POINT('',(76.5847478255888,-9.37892662881146E-15,-8.00000000000001));
#264930=CARTESIAN_POINT('',(76.5847478255888,-9.37892662881146E-15,228.814169979695));
#264931=CARTESIAN_POINT('Origin',(0.,0.,-8.));
#264932=CARTESIAN_POINT('Origin',(-90.,-90.,63.5));
#264933=CARTESIAN_POINT('',(-81.5545,-90.,8.255));
#264934=CARTESIAN_POINT('Origin',(-90.,-90.,8.255));
#264935=CARTESIAN_POINT('',(-81.5545,-90.,3.175));
#264936=CARTESIAN_POINT('',(-81.5545,-90.,63.5));
#264937=CARTESIAN_POINT('Origin',(-90.,-90.,3.175));
#264938=CARTESIAN_POINT('Origin',(-90.,90.,63.5));
#264939=CARTESIAN_POINT('',(-81.5545,90.,8.255));
#264940=CARTESIAN_POINT('Origin',(-90.,90.,8.255));
#264941=CARTESIAN_POINT('',(-81.5545,90.,3.175));
#264942=CARTESIAN_POINT('',(-81.5545,90.,63.5));
#264943=CARTESIAN_POINT('Origin',(-90.,90.,3.175));
#264944=CARTESIAN_POINT('Origin',(90.,90.,63.5));
#264945=CARTESIAN_POINT('',(98.4455,90.,8.255));
#264946=CARTESIAN_POINT('Origin',(90.,90.,8.255));
#264947=CARTESIAN_POINT('',(98.4455,90.,3.175));
#264948=CARTESIAN_POINT('',(98.4455,90.,63.5));
#264949=CARTESIAN_POINT('Origin',(90.,90.,3.175));
#264950=CARTESIAN_POINT('Origin',(90.,-90.,63.5));
#264951=CARTESIAN_POINT('',(98.4455,-90.,8.255));
#264952=CARTESIAN_POINT('Origin',(90.,-90.,8.255));
#264953=CARTESIAN_POINT('',(98.4455,-90.,3.175));
#264954=CARTESIAN_POINT('',(98.4455,-90.,63.5));
#264955=CARTESIAN_POINT('Origin',(90.,-90.,3.175));
#264956=CARTESIAN_POINT('Origin',(90.,-90.,0.));
#264957=CARTESIAN_POINT('',(82.0625,-90.,-8.));
#264958=CARTESIAN_POINT('Origin',(90.,-90.,-8.));
#264959=CARTESIAN_POINT('',(82.0625,-90.,3.175));
#264960=CARTESIAN_POINT('',(82.0625,-90.,0.));
#264961=CARTESIAN_POINT('Origin',(90.,-90.,3.175));
#264962=CARTESIAN_POINT('Origin',(90.,90.,0.));
#264963=CARTESIAN_POINT('',(82.0625,90.,-8.));
#264964=CARTESIAN_POINT('Origin',(90.,90.,-8.));
#264965=CARTESIAN_POINT('',(82.0625,90.,3.175));
#264966=CARTESIAN_POINT('',(82.0625,90.,0.));
#264967=CARTESIAN_POINT('Origin',(90.,90.,3.175));
#264968=CARTESIAN_POINT('Origin',(-90.,90.,0.));
#264969=CARTESIAN_POINT('',(-97.9375,90.,-8.));
#264970=CARTESIAN_POINT('Origin',(-90.,90.,-8.));
#264971=CARTESIAN_POINT('',(-97.9375,90.,3.175));
#264972=CARTESIAN_POINT('',(-97.9375,90.,0.));
#264973=CARTESIAN_POINT('Origin',(-90.,90.,3.175));
#264974=CARTESIAN_POINT('Origin',(-90.,-90.,0.));
#264975=CARTESIAN_POINT('',(-97.9375,-90.,-8.));
#264976=CARTESIAN_POINT('Origin',(-90.,-90.,-8.));
#264977=CARTESIAN_POINT('',(-97.9375,-90.,3.175));
#264978=CARTESIAN_POINT('',(-97.9375,-90.,0.));
#264979=CARTESIAN_POINT('Origin',(-90.,-90.,3.175));
#264980=CARTESIAN_POINT('Origin',(-90.,-90.,0.));
#264981=CARTESIAN_POINT('',(-90.,-114.492,0.0381));
#264982=CARTESIAN_POINT('',(-90.,-114.492,7.493));
#264983=CARTESIAN_POINT('',(-90.,-114.492,0.));
#264984=CARTESIAN_POINT('',(-114.492,-90.,7.493));
#264985=CARTESIAN_POINT('Origin',(-90.,-90.,7.493));
#264986=CARTESIAN_POINT('',(-114.492,-90.,0.0381));
#264987=CARTESIAN_POINT('',(-114.492,-90.,0.));
#264988=CARTESIAN_POINT('Origin',(-90.,-90.,0.0381));
#264989=CARTESIAN_POINT('Origin',(-114.492,-90.,0.));
#264990=CARTESIAN_POINT('',(-114.492,90.,7.493));
#264991=CARTESIAN_POINT('',(-114.492,-90.,7.493));
#264992=CARTESIAN_POINT('',(-114.492,90.,0.0381));
#264993=CARTESIAN_POINT('',(-114.492,90.,0.));
#264994=CARTESIAN_POINT('',(-114.492,-90.,0.0381));
#264995=CARTESIAN_POINT('Origin',(-90.,90.,0.));
#264996=CARTESIAN_POINT('',(-90.,114.492,7.493));
#264997=CARTESIAN_POINT('Origin',(-90.,90.,7.493));
#264998=CARTESIAN_POINT('',(-90.,114.492,0.0381));
#264999=CARTESIAN_POINT('',(-90.,114.492,0.));
#265000=CARTESIAN_POINT('Origin',(-90.,90.,0.0381));
#265001=CARTESIAN_POINT('Origin',(-90.,114.492,0.));
#265002=CARTESIAN_POINT('',(90.,114.492,7.493));
#265003=CARTESIAN_POINT('',(-90.,114.492,7.493));
#265004=CARTESIAN_POINT('',(90.,114.492,0.0381));
#265005=CARTESIAN_POINT('',(90.,114.492,0.));
#265006=CARTESIAN_POINT('',(-90.,114.492,0.0381));
#265007=CARTESIAN_POINT('Origin',(90.,90.,0.));
#265008=CARTESIAN_POINT('',(114.492,90.,7.493));
#265009=CARTESIAN_POINT('Origin',(90.,90.,7.493));
#265010=CARTESIAN_POINT('',(114.492,90.,0.0381));
#265011=CARTESIAN_POINT('',(114.492,90.,0.));
#265012=CARTESIAN_POINT('Origin',(90.,90.,0.0381));
#265013=CARTESIAN_POINT('Origin',(114.492,90.,0.));
#265014=CARTESIAN_POINT('',(114.492,-90.,7.493));
#265015=CARTESIAN_POINT('',(114.492,90.,7.493));
#265016=CARTESIAN_POINT('',(114.492,-90.,0.0381));
#265017=CARTESIAN_POINT('',(114.492,-90.,0.));
#265018=CARTESIAN_POINT('',(114.492,90.,0.0381));
#265019=CARTESIAN_POINT('Origin',(90.,-90.,0.));
#265020=CARTESIAN_POINT('',(90.,-114.492,7.493));
#265021=CARTESIAN_POINT('Origin',(90.,-90.,7.493));
#265022=CARTESIAN_POINT('',(90.,-114.492,0.0381));
#265023=CARTESIAN_POINT('',(90.,-114.492,0.));
#265024=CARTESIAN_POINT('Origin',(90.,-90.,0.0381));
#265025=CARTESIAN_POINT('Origin',(90.,-114.492,0.));
#265026=CARTESIAN_POINT('',(90.,-114.492,7.493));
#265027=CARTESIAN_POINT('',(90.,-114.492,0.0381));
#265028=CARTESIAN_POINT('Origin',(-90.,-90.,8.255));
#265029=CARTESIAN_POINT('',(-113.73,90.,8.255));
#265030=CARTESIAN_POINT('',(-113.73,-90.,8.255));
#265031=CARTESIAN_POINT('',(-113.73,-90.,8.255));
#265032=CARTESIAN_POINT('',(-90.,-113.73,8.255));
#265033=CARTESIAN_POINT('Origin',(-90.,-90.,8.255));
#265034=CARTESIAN_POINT('',(90.,-113.73,8.255));
#265035=CARTESIAN_POINT('',(-90.,-113.73,8.255));
#265036=CARTESIAN_POINT('',(113.73,-90.,8.255));
#265037=CARTESIAN_POINT('Origin',(90.,-90.,8.255));
#265038=CARTESIAN_POINT('',(113.73,90.,8.255));
#265039=CARTESIAN_POINT('',(113.73,-90.0000000000001,8.255));
#265040=CARTESIAN_POINT('',(90.,113.73,8.255));
#265041=CARTESIAN_POINT('Origin',(90.,90.,8.255));
#265042=CARTESIAN_POINT('',(-90.,113.73,8.255));
#265043=CARTESIAN_POINT('',(-90.,113.73,8.255));
#265044=CARTESIAN_POINT('Origin',(-90.,90.,8.255));
#265045=CARTESIAN_POINT('Origin',(90.,-90.,3.175));
#265046=CARTESIAN_POINT('Origin',(90.,90.,3.175));
#265047=CARTESIAN_POINT('Origin',(-90.,90.,3.175));
#265048=CARTESIAN_POINT('Origin',(-90.,-90.,3.175));
#265049=CARTESIAN_POINT('Origin',(90.,90.,0.0381));
#265050=CARTESIAN_POINT('',(90.,115.,0.0381));
#265051=CARTESIAN_POINT('',(115.,90.,0.0381));
#265052=CARTESIAN_POINT('Origin',(90.,90.,0.0381));
#265053=CARTESIAN_POINT('',(-90.,115.,0.0381));
#265054=CARTESIAN_POINT('',(-90.,115.,0.0381));
#265055=CARTESIAN_POINT('',(-115.,90.,0.0381));
#265056=CARTESIAN_POINT('Origin',(-90.,90.,0.0381));
#265057=CARTESIAN_POINT('',(-115.,-90.,0.0381));
#265058=CARTESIAN_POINT('',(-115.,-90.,0.0381));
#265059=CARTESIAN_POINT('',(-90.,-115.,0.0381));
#265060=CARTESIAN_POINT('Origin',(-90.,-90.,0.0381));
#265061=CARTESIAN_POINT('',(90.,-115.,0.0381));
#265062=CARTESIAN_POINT('',(90.,-115.,0.0381));
#265063=CARTESIAN_POINT('',(115.,-90.,0.0381));
#265064=CARTESIAN_POINT('Origin',(90.,-90.,0.0381));
#265065=CARTESIAN_POINT('',(115.,90.,0.0381));
#265066=CARTESIAN_POINT('Origin',(90.,90.,0.));
#265067=CARTESIAN_POINT('',(115.,90.,-8.));
#265068=CARTESIAN_POINT('',(115.,90.,0.));
#265069=CARTESIAN_POINT('',(90.,115.,-8.));
#265070=CARTESIAN_POINT('Origin',(90.,90.,-8.));
#265071=CARTESIAN_POINT('',(90.,115.,0.));
#265072=CARTESIAN_POINT('Origin',(115.,90.,0.));
#265073=CARTESIAN_POINT('',(115.,-90.,-8.));
#265074=CARTESIAN_POINT('',(115.,-90.,0.));
#265075=CARTESIAN_POINT('',(115.,90.,-8.));
#265076=CARTESIAN_POINT('Origin',(90.,-90.,0.));
#265077=CARTESIAN_POINT('',(90.,-115.,-8.));
#265078=CARTESIAN_POINT('',(90.,-115.,0.));
#265079=CARTESIAN_POINT('Origin',(90.,-90.,-8.));
#265080=CARTESIAN_POINT('Origin',(90.,-115.,0.));
#265081=CARTESIAN_POINT('',(-90.,-115.,-8.));
#265082=CARTESIAN_POINT('',(-90.,-115.,0.));
#265083=CARTESIAN_POINT('',(90.,-115.,-8.));
#265084=CARTESIAN_POINT('Origin',(-90.,-90.,0.));
#265085=CARTESIAN_POINT('',(-115.,-90.,-8.));
#265086=CARTESIAN_POINT('',(-115.,-90.,0.));
#265087=CARTESIAN_POINT('Origin',(-90.,-90.,-8.));
#265088=CARTESIAN_POINT('Origin',(-115.,-90.,0.));
#265089=CARTESIAN_POINT('',(-115.,90.,-8.));
#265090=CARTESIAN_POINT('',(-115.,90.,0.));
#265091=CARTESIAN_POINT('',(-115.,-90.,-8.));
#265092=CARTESIAN_POINT('Origin',(-90.,90.,0.));
#265093=CARTESIAN_POINT('',(-90.,115.,-8.));
#265094=CARTESIAN_POINT('',(-90.,115.,0.));
#265095=CARTESIAN_POINT('Origin',(-90.,90.,-8.));
#265096=CARTESIAN_POINT('Origin',(-90.,115.,0.));
#265097=CARTESIAN_POINT('',(-90.,115.,-8.));
#265098=CARTESIAN_POINT('Origin',(90.,90.,7.493));
#265099=CARTESIAN_POINT('Origin',(90.,113.73,7.493));
#265100=CARTESIAN_POINT('Origin',(113.73,90.,7.493));
#265101=CARTESIAN_POINT('Origin',(113.73,90.,7.493));
#265102=CARTESIAN_POINT('Origin',(113.73,-90.,7.493));
#265103=CARTESIAN_POINT('Origin',(-90.,113.73,7.493));
#265104=CARTESIAN_POINT('Origin',(-90.,113.73,7.493));
#265105=CARTESIAN_POINT('Origin',(90.,-90.,7.493));
#265106=CARTESIAN_POINT('Origin',(90.,-113.73,7.493));
#265107=CARTESIAN_POINT('Origin',(-90.,90.,7.493));
#265108=CARTESIAN_POINT('Origin',(-113.73,90.,7.493));
#265109=CARTESIAN_POINT('Origin',(90.,-113.73,7.493));
#265110=CARTESIAN_POINT('Origin',(-90.,-113.73,7.493));
#265111=CARTESIAN_POINT('Origin',(-113.73,-90.,7.493));
#265112=CARTESIAN_POINT('Origin',(-113.73,-90.,7.493));
#265113=CARTESIAN_POINT('Origin',(-90.,-90.,7.493));
#265114=CARTESIAN_POINT('Origin',(90.,90.,-8.));
#265115=CARTESIAN_POINT('Origin',(0.,0.,-195.421614460986));
#265116=CARTESIAN_POINT('',(-17.3379110419348,-64.705964905612,7.62));
#265117=CARTESIAN_POINT('',(-17.3379110419348,-64.705964905612,2.54));
#265118=CARTESIAN_POINT('',(-17.3379110419348,-64.705964905612,7.62));
#265119=CARTESIAN_POINT('',(-17.3379110419348,64.705964905612,2.54));
#265120=CARTESIAN_POINT('Origin',(0.,0.,2.53999999999999));
#265121=CARTESIAN_POINT('',(-17.3379110419348,64.705964905612,7.62));
#265122=CARTESIAN_POINT('',(-17.3379110419348,64.705964905612,7.62));
#265123=CARTESIAN_POINT('Origin',(0.,0.,7.62));
#265124=CARTESIAN_POINT('Origin',(-90.,-90.,2.54));
#265125=CARTESIAN_POINT('',(-17.3379110419348,-71.5863792036332,2.54));
#265126=CARTESIAN_POINT('',(-17.3379110419348,-71.5863792036332,2.54));
#265127=CARTESIAN_POINT('',(17.3379110419348,-71.5863792036332,2.54));
#265128=CARTESIAN_POINT('Origin',(0.,0.,2.54));
#265129=CARTESIAN_POINT('',(17.3379110419348,-71.5863792036332,2.54));
#265130=CARTESIAN_POINT('',(17.3379110419348,71.5863792036332,2.54));
#265131=CARTESIAN_POINT('',(17.3379110419348,71.5863792036332,2.54));
#265132=CARTESIAN_POINT('',(-17.3379110419348,71.5863792036332,2.54));
#265133=CARTESIAN_POINT('Origin',(0.,0.,2.54));
#265134=CARTESIAN_POINT('',(-17.3379110419348,71.5863792036332,2.54));
#265135=CARTESIAN_POINT('Origin',(0.,0.,17.4625));
#265136=CARTESIAN_POINT('Origin',(90.,90.,0.));
#265137=CARTESIAN_POINT('Origin',(5.94817889868156E-29,-2.83629507977407E-14,
4.08753198860305));
#265138=CARTESIAN_POINT('Origin',(0.,0.,7.62));
#265139=CARTESIAN_POINT('',(17.3379110419348,71.5863792036332,7.62));
#265140=CARTESIAN_POINT('',(17.3379110419348,71.5863792036332,7.62));
#265141=CARTESIAN_POINT('',(-17.3379110419348,71.5863792036332,7.62));
#265142=CARTESIAN_POINT('Origin',(0.,0.,7.62));
#265143=CARTESIAN_POINT('',(-17.3379110419348,71.5863792036332,7.62));
#265144=CARTESIAN_POINT('Origin',(-17.3379110419348,71.5863792036332,7.62));
#265145=CARTESIAN_POINT('',(-17.3379110419348,71.5863792036332,7.62));
#265146=CARTESIAN_POINT('Origin',(17.3379110419348,71.5863792036332,7.62));
#265147=CARTESIAN_POINT('',(17.3379110419348,71.5863792036332,7.62));
#265148=CARTESIAN_POINT('Origin',(0.,0.,7.62));
#265149=CARTESIAN_POINT('',(17.3379110419348,-71.5863792036332,7.62));
#265150=CARTESIAN_POINT('',(17.3379110419348,-71.5863792036332,7.62));
#265151=CARTESIAN_POINT('',(-17.3379110419348,-71.5863792036332,7.62));
#265152=CARTESIAN_POINT('Origin',(0.,0.,7.62));
#265153=CARTESIAN_POINT('',(-17.3379110419348,-71.5863792036332,7.62));
#265154=CARTESIAN_POINT('Origin',(0.,0.,7.62));
#265155=CARTESIAN_POINT('',(-17.3379110419348,-71.5863792036332,7.62));
#265156=CARTESIAN_POINT('',(17.3379110419348,-71.5863792036332,7.62));
#265157=CARTESIAN_POINT('Origin',(-17.3379110419348,-71.5863792036332,7.62));
#265158=CARTESIAN_POINT('Origin',(17.3379110419348,-71.5863792036332,7.62));
#265159=CARTESIAN_POINT('',(0.,0.,0.));
#265160=CARTESIAN_POINT('Ctrl Pts',(160.,4.30813900827813,372.462296651428));
#265161=CARTESIAN_POINT('Ctrl Pts',(160.339057893189,-8.28413408366083,
370.462296651428));
#265162=CARTESIAN_POINT('Ctrl Pts',(158.704075916301,-20.7744157382975,
368.462296651428));
#265163=CARTESIAN_POINT('Ctrl Pts',(157.069093939413,-33.2646973929343,
366.462296651428));
#265164=CARTESIAN_POINT('Ctrl Pts',(153.500330774912,-45.3454354230633,
364.462296651428));
#265165=CARTESIAN_POINT('Ctrl Pts',(149.931567610412,-57.4261734531924,
362.462296651428));
#265166=CARTESIAN_POINT('Ctrl Pts',(144.516898051455,-68.7998999948413,
360.462296651428));
#265167=CARTESIAN_POINT('Ctrl Pts',(139.102228492497,-80.1736265364901,
358.462296651428));
#265168=CARTESIAN_POINT('Ctrl Pts',(131.974979673883,-90.5602826949691,
356.462296651428));
#265169=CARTESIAN_POINT('Ctrl Pts',(124.847730855269,-100.946938853448,
354.462296651428));
#265170=CARTESIAN_POINT('Ctrl Pts',(116.183399296895,-110.0907706828,352.462296651428));
#265171=CARTESIAN_POINT('Ctrl Pts',(107.519067738521,-119.234602512152,
350.462296651428));
#265172=CARTESIAN_POINT('Ctrl Pts',(97.5309980386224,-126.9104585261,348.462296651428));
#265173=CARTESIAN_POINT('Ctrl Pts',(87.5429283387234,-134.586314540048,
346.462296651428));
#265174=CARTESIAN_POINT('Ctrl Pts',(76.4770599218137,-140.605189688823,
344.462296651428));
#265175=CARTESIAN_POINT('Ctrl Pts',(65.4111915049041,-146.624064837599,
342.462296651428));
#265176=CARTESIAN_POINT('Ctrl Pts',(53.5400027769198,-150.837754439537,
340.462296651428));
#265177=CARTESIAN_POINT('Ctrl Pts',(41.6688140489356,-155.051444041475,
338.462296651428));
#265178=CARTESIAN_POINT('Ctrl Pts',(29.2846130745764,-157.356193074143,
336.462296651428));
#265179=CARTESIAN_POINT('Ctrl Pts',(16.9004121002171,-159.660942106811,
334.462296651428));
#265180=CARTESIAN_POINT('Ctrl Pts',(4.30813900827814,-160.,332.462296651428));
#265181=CARTESIAN_POINT('Ctrl Pts',(-8.28413408366082,-160.339057893189,
330.462296651428));
#265182=CARTESIAN_POINT('Ctrl Pts',(-20.7744157382975,-158.704075916301,
328.462296651428));
#265183=CARTESIAN_POINT('Ctrl Pts',(-33.2646973929342,-157.069093939413,
326.462296651428));
#265184=CARTESIAN_POINT('Ctrl Pts',(-45.3454354230633,-153.500330774912,
324.462296651428));
#265185=CARTESIAN_POINT('Ctrl Pts',(-57.4261734531924,-149.931567610412,
322.462296651428));
#265186=CARTESIAN_POINT('Ctrl Pts',(-68.7998999948413,-144.516898051455,
320.462296651428));
#265187=CARTESIAN_POINT('Ctrl Pts',(-80.1736265364901,-139.102228492497,
318.462296651428));
#265188=CARTESIAN_POINT('Ctrl Pts',(-90.5602826949691,-131.974979673883,
316.462296651428));
#265189=CARTESIAN_POINT('Ctrl Pts',(-100.946938853448,-124.847730855269,
314.462296651428));
#265190=CARTESIAN_POINT('Ctrl Pts',(-110.0907706828,-116.183399296895,312.462296651428));
#265191=CARTESIAN_POINT('Ctrl Pts',(-119.234602512152,-107.519067738521,
310.462296651428));
#265192=CARTESIAN_POINT('Ctrl Pts',(-126.9104585261,-97.5309980386224,308.462296651428));
#265193=CARTESIAN_POINT('Ctrl Pts',(-134.586314540048,-87.5429283387234,
306.462296651428));
#265194=CARTESIAN_POINT('Ctrl Pts',(-140.605189688823,-76.4770599218137,
304.462296651428));
#265195=CARTESIAN_POINT('Ctrl Pts',(-146.624064837599,-65.4111915049041,
302.462296651428));
#265196=CARTESIAN_POINT('Ctrl Pts',(-150.837754439537,-53.5400027769199,
300.462296651428));
#265197=CARTESIAN_POINT('Ctrl Pts',(-155.051444041475,-41.6688140489356,
298.462296651428));
#265198=CARTESIAN_POINT('Ctrl Pts',(-157.356193074143,-29.2846130745764,
296.462296651428));
#265199=CARTESIAN_POINT('Ctrl Pts',(-159.660942106811,-16.9004121002171,
294.462296651428));
#265200=CARTESIAN_POINT('Ctrl Pts',(-160.,-4.30813900827815,292.462296651428));
#265201=CARTESIAN_POINT('Ctrl Pts',(-160.339057893189,8.28413408366081,
290.462296651428));
#265202=CARTESIAN_POINT('Ctrl Pts',(-158.704075916301,20.7744157382975,
288.462296651428));
#265203=CARTESIAN_POINT('Ctrl Pts',(-157.069093939413,33.2646973929342,
286.462296651428));
#265204=CARTESIAN_POINT('Ctrl Pts',(-153.500330774912,45.3454354230633,
284.462296651428));
#265205=CARTESIAN_POINT('Ctrl Pts',(-149.931567610412,57.4261734531924,
282.462296651428));
#265206=CARTESIAN_POINT('Ctrl Pts',(-144.516898051455,68.7998999948413,
280.462296651428));
#265207=CARTESIAN_POINT('Ctrl Pts',(-139.102228492497,80.1736265364901,
278.462296651428));
#265208=CARTESIAN_POINT('Ctrl Pts',(-131.974979673883,90.5602826949691,
276.462296651428));
#265209=CARTESIAN_POINT('Ctrl Pts',(-124.847730855269,100.946938853448,
274.462296651428));
#265210=CARTESIAN_POINT('Ctrl Pts',(-116.183399296895,110.0907706828,272.462296651428));
#265211=CARTESIAN_POINT('Ctrl Pts',(-107.519067738521,119.234602512152,
270.462296651428));
#265212=CARTESIAN_POINT('Ctrl Pts',(-97.5309980386224,126.9104585261,268.462296651428));
#265213=CARTESIAN_POINT('Ctrl Pts',(-87.5429283387233,134.586314540048,
266.462296651428));
#265214=CARTESIAN_POINT('Ctrl Pts',(-76.4770599218137,140.605189688823,
264.462296651428));
#265215=CARTESIAN_POINT('Ctrl Pts',(-65.4111915049042,146.624064837599,
262.462296651428));
#265216=CARTESIAN_POINT('Ctrl Pts',(-53.5400027769199,150.837754439537,
260.462296651428));
#265217=CARTESIAN_POINT('Ctrl Pts',(-41.6688140489356,155.051444041475,
258.462296651428));
#265218=CARTESIAN_POINT('Ctrl Pts',(-29.2846130745764,157.356193074143,
256.462296651428));
#265219=CARTESIAN_POINT('Ctrl Pts',(-16.9004121002172,159.660942106811,
254.462296651428));
#265220=CARTESIAN_POINT('Ctrl Pts',(-4.30813900827816,160.,252.462296651428));
#265221=CARTESIAN_POINT('Ctrl Pts',(8.28413408366087,160.339057893189,250.462296651428));
#265222=CARTESIAN_POINT('Ctrl Pts',(20.7744157382975,158.704075916301,248.462296651428));
#265223=CARTESIAN_POINT('Ctrl Pts',(33.2646973929342,157.069093939413,246.462296651428));
#265224=CARTESIAN_POINT('Ctrl Pts',(45.3454354230633,153.500330774912,244.462296651428));
#265225=CARTESIAN_POINT('Ctrl Pts',(57.4261734531925,149.931567610412,242.462296651428));
#265226=CARTESIAN_POINT('Ctrl Pts',(68.7998999948413,144.516898051455,240.462296651428));
#265227=CARTESIAN_POINT('Ctrl Pts',(80.1736265364901,139.102228492498,238.462296651428));
#265228=CARTESIAN_POINT('Ctrl Pts',(90.560282694969,131.974979673883,236.462296651428));
#265229=CARTESIAN_POINT('Ctrl Pts',(100.946938853448,124.847730855269,234.462296651428));
#265230=CARTESIAN_POINT('Ctrl Pts',(110.0907706828,116.183399296895,232.462296651428));
#265231=CARTESIAN_POINT('Ctrl Pts',(119.234602512152,107.519067738521,230.462296651428));
#265232=CARTESIAN_POINT('Ctrl Pts',(126.9104585261,97.5309980386224,228.462296651428));
#265233=CARTESIAN_POINT('Ctrl Pts',(134.586314540048,87.5429283387233,226.462296651428));
#265234=CARTESIAN_POINT('Ctrl Pts',(140.605189688823,76.4770599218137,224.462296651428));
#265235=CARTESIAN_POINT('Ctrl Pts',(146.624064837599,65.4111915049042,222.462296651428));
#265236=CARTESIAN_POINT('Ctrl Pts',(150.837754439537,53.5400027769199,220.462296651428));
#265237=CARTESIAN_POINT('Ctrl Pts',(155.051444041475,41.6688140489356,218.462296651428));
#265238=CARTESIAN_POINT('Ctrl Pts',(157.356193074143,29.2846130745764,216.462296651428));
#265239=CARTESIAN_POINT('Ctrl Pts',(159.660942106811,16.9004121002172,214.462296651428));
#265240=CARTESIAN_POINT('Ctrl Pts',(160.,4.30813900827813,212.462296651428));
#265241=CARTESIAN_POINT('Ctrl Pts',(160.,-4.30813900827805,377.537703348572));
#265242=CARTESIAN_POINT('Ctrl Pts',(159.660942106811,-16.900412100217,375.537703348572));
#265243=CARTESIAN_POINT('Ctrl Pts',(157.356193074143,-29.2846130745763,
373.537703348572));
#265244=CARTESIAN_POINT('Ctrl Pts',(155.051444041475,-41.6688140489355,
371.537703348572));
#265245=CARTESIAN_POINT('Ctrl Pts',(150.837754439537,-53.5400027769198,
369.537703348572));
#265246=CARTESIAN_POINT('Ctrl Pts',(146.624064837599,-65.411191504904,367.537703348572));
#265247=CARTESIAN_POINT('Ctrl Pts',(140.605189688823,-76.4770599218136,
365.537703348572));
#265248=CARTESIAN_POINT('Ctrl Pts',(134.586314540048,-87.5429283387233,
363.537703348572));
#265249=CARTESIAN_POINT('Ctrl Pts',(126.9104585261,-97.5309980386223,361.537703348572));
#265250=CARTESIAN_POINT('Ctrl Pts',(119.234602512152,-107.519067738521,
359.537703348572));
#265251=CARTESIAN_POINT('Ctrl Pts',(110.0907706828,-116.183399296895,357.537703348572));
#265252=CARTESIAN_POINT('Ctrl Pts',(100.946938853448,-124.847730855269,
355.537703348572));
#265253=CARTESIAN_POINT('Ctrl Pts',(90.5602826949691,-131.974979673883,
353.537703348572));
#265254=CARTESIAN_POINT('Ctrl Pts',(80.1736265364902,-139.102228492497,
351.537703348572));
#265255=CARTESIAN_POINT('Ctrl Pts',(68.7998999948414,-144.516898051454,
349.537703348572));
#265256=CARTESIAN_POINT('Ctrl Pts',(57.4261734531925,-149.931567610412,
347.537703348572));
#265257=CARTESIAN_POINT('Ctrl Pts',(45.3454354230634,-153.500330774912,
345.537703348572));
#265258=CARTESIAN_POINT('Ctrl Pts',(33.2646973929343,-157.069093939413,
343.537703348572));
#265259=CARTESIAN_POINT('Ctrl Pts',(20.7744157382976,-158.704075916301,
341.537703348572));
#265260=CARTESIAN_POINT('Ctrl Pts',(8.28413408366091,-160.339057893189,
339.537703348572));
#265261=CARTESIAN_POINT('Ctrl Pts',(-4.30813900827804,-160.,337.537703348572));
#265262=CARTESIAN_POINT('Ctrl Pts',(-16.900412100217,-159.660942106811,
335.537703348572));
#265263=CARTESIAN_POINT('Ctrl Pts',(-29.2846130745763,-157.356193074143,
333.537703348572));
#265264=CARTESIAN_POINT('Ctrl Pts',(-41.6688140489355,-155.051444041475,
331.537703348572));
#265265=CARTESIAN_POINT('Ctrl Pts',(-53.5400027769198,-150.837754439537,
329.537703348572));
#265266=CARTESIAN_POINT('Ctrl Pts',(-65.411191504904,-146.624064837599,
327.537703348572));
#265267=CARTESIAN_POINT('Ctrl Pts',(-76.4770599218136,-140.605189688823,
325.537703348572));
#265268=CARTESIAN_POINT('Ctrl Pts',(-87.5429283387233,-134.586314540048,
323.537703348572));
#265269=CARTESIAN_POINT('Ctrl Pts',(-97.5309980386223,-126.9104585261,321.537703348572));
#265270=CARTESIAN_POINT('Ctrl Pts',(-107.519067738521,-119.234602512152,
319.537703348572));
#265271=CARTESIAN_POINT('Ctrl Pts',(-116.183399296895,-110.0907706828,317.537703348572));
#265272=CARTESIAN_POINT('Ctrl Pts',(-124.847730855269,-100.946938853448,
315.537703348572));
#265273=CARTESIAN_POINT('Ctrl Pts',(-131.974979673883,-90.5602826949692,
313.537703348572));
#265274=CARTESIAN_POINT('Ctrl Pts',(-139.102228492497,-80.1736265364902,
311.537703348572));
#265275=CARTESIAN_POINT('Ctrl Pts',(-144.516898051454,-68.7998999948414,
309.537703348572));
#265276=CARTESIAN_POINT('Ctrl Pts',(-149.931567610412,-57.4261734531925,
307.537703348572));
#265277=CARTESIAN_POINT('Ctrl Pts',(-153.500330774912,-45.3454354230634,
305.537703348572));
#265278=CARTESIAN_POINT('Ctrl Pts',(-157.069093939413,-33.2646973929344,
303.537703348572));
#265279=CARTESIAN_POINT('Ctrl Pts',(-158.704075916301,-20.7744157382976,
301.537703348572));
#265280=CARTESIAN_POINT('Ctrl Pts',(-160.339057893189,-8.28413408366092,
299.537703348572));
#265281=CARTESIAN_POINT('Ctrl Pts',(-160.,4.30813900827803,297.537703348572));
#265282=CARTESIAN_POINT('Ctrl Pts',(-159.660942106811,16.900412100217,295.537703348572));
#265283=CARTESIAN_POINT('Ctrl Pts',(-157.356193074143,29.2846130745763,
293.537703348572));
#265284=CARTESIAN_POINT('Ctrl Pts',(-155.051444041475,41.6688140489355,
291.537703348572));
#265285=CARTESIAN_POINT('Ctrl Pts',(-150.837754439537,53.5400027769198,
289.537703348572));
#265286=CARTESIAN_POINT('Ctrl Pts',(-146.624064837599,65.411191504904,287.537703348572));
#265287=CARTESIAN_POINT('Ctrl Pts',(-140.605189688823,76.4770599218136,
285.537703348572));
#265288=CARTESIAN_POINT('Ctrl Pts',(-134.586314540048,87.5429283387233,
283.537703348572));
#265289=CARTESIAN_POINT('Ctrl Pts',(-126.9104585261,97.5309980386223,281.537703348572));
#265290=CARTESIAN_POINT('Ctrl Pts',(-119.234602512152,107.519067738521,
279.537703348572));
#265291=CARTESIAN_POINT('Ctrl Pts',(-110.0907706828,116.183399296895,277.537703348572));
#265292=CARTESIAN_POINT('Ctrl Pts',(-100.946938853448,124.847730855269,
275.537703348572));
#265293=CARTESIAN_POINT('Ctrl Pts',(-90.5602826949692,131.974979673883,
273.537703348572));
#265294=CARTESIAN_POINT('Ctrl Pts',(-80.1736265364901,139.102228492497,
271.537703348572));
#265295=CARTESIAN_POINT('Ctrl Pts',(-68.7998999948414,144.516898051454,
269.537703348572));
#265296=CARTESIAN_POINT('Ctrl Pts',(-57.4261734531926,149.931567610412,
267.537703348572));
#265297=CARTESIAN_POINT('Ctrl Pts',(-45.3454354230634,153.500330774912,
265.537703348572));
#265298=CARTESIAN_POINT('Ctrl Pts',(-33.2646973929343,157.069093939413,
263.537703348572));
#265299=CARTESIAN_POINT('Ctrl Pts',(-20.7744157382976,158.704075916301,
261.537703348572));
#265300=CARTESIAN_POINT('Ctrl Pts',(-8.284134083661,160.339057893189,259.537703348572));
#265301=CARTESIAN_POINT('Ctrl Pts',(4.30813900827803,160.,257.537703348572));
#265302=CARTESIAN_POINT('Ctrl Pts',(16.9004121002171,159.660942106811,255.537703348572));
#265303=CARTESIAN_POINT('Ctrl Pts',(29.2846130745762,157.356193074143,253.537703348572));
#265304=CARTESIAN_POINT('Ctrl Pts',(41.6688140489354,155.051444041476,251.537703348572));
#265305=CARTESIAN_POINT('Ctrl Pts',(53.5400027769198,150.837754439537,249.537703348572));
#265306=CARTESIAN_POINT('Ctrl Pts',(65.4111915049041,146.624064837599,247.537703348572));
#265307=CARTESIAN_POINT('Ctrl Pts',(76.4770599218136,140.605189688823,245.537703348572));
#265308=CARTESIAN_POINT('Ctrl Pts',(87.5429283387232,134.586314540048,243.537703348572));
#265309=CARTESIAN_POINT('Ctrl Pts',(97.5309980386223,126.9104585261,241.537703348572));
#265310=CARTESIAN_POINT('Ctrl Pts',(107.519067738521,119.234602512152,239.537703348572));
#265311=CARTESIAN_POINT('Ctrl Pts',(116.183399296895,110.0907706828,237.537703348572));
#265312=CARTESIAN_POINT('Ctrl Pts',(124.847730855269,100.946938853448,235.537703348572));
#265313=CARTESIAN_POINT('Ctrl Pts',(131.974979673883,90.5602826949692,233.537703348572));
#265314=CARTESIAN_POINT('Ctrl Pts',(139.102228492497,80.1736265364902,231.537703348572));
#265315=CARTESIAN_POINT('Ctrl Pts',(144.516898051454,68.7998999948414,229.537703348572));
#265316=CARTESIAN_POINT('Ctrl Pts',(149.931567610412,57.4261734531926,227.537703348572));
#265317=CARTESIAN_POINT('Ctrl Pts',(153.500330774912,45.3454354230634,225.537703348572));
#265318=CARTESIAN_POINT('Ctrl Pts',(157.069093939413,33.2646973929343,223.537703348572));
#265319=CARTESIAN_POINT('Ctrl Pts',(158.704075916301,20.7744157382976,221.537703348572));
#265320=CARTESIAN_POINT('Ctrl Pts',(160.339057893189,8.28413408366101,219.537703348572));
#265321=CARTESIAN_POINT('Ctrl Pts',(160.,-4.30813900827805,217.537703348572));
#265322=CARTESIAN_POINT('',(157.805088795962,-26.7603066464731,367.5));
#265323=CARTESIAN_POINT('',(146.075461400194,-65.4256802672709,367.500000000001));
#265324=CARTESIAN_POINT('Ctrl Pts',(157.805088795962,-26.7603066464731,
367.5));
#265325=CARTESIAN_POINT('Ctrl Pts',(156.638532817878,-33.4083424416554,
367.5));
#265326=CARTESIAN_POINT('Ctrl Pts',(155.071407572055,-39.9802096740409,
367.5));
#265327=CARTESIAN_POINT('Ctrl Pts',(152.131501324444,-49.6731919343085,
367.5));
#265328=CARTESIAN_POINT('Ctrl Pts',(151.053085052425,-52.8765297093718,
367.499999999997));
#265329=CARTESIAN_POINT('Ctrl Pts',(148.705612539596,-59.2094688002808,
367.499999999997));
#265330=CARTESIAN_POINT('Ctrl Pts',(147.437304082636,-62.3378048444613,
367.5));
#265331=CARTESIAN_POINT('Ctrl Pts',(146.075461400194,-65.4256802672709,
367.5));
#265332=CARTESIAN_POINT('',(160.,4.30813900827813,372.462296651428));
#265333=CARTESIAN_POINT('Ctrl Pts',(160.,4.30813900827813,372.462296651428));
#265334=CARTESIAN_POINT('Ctrl Pts',(160.339057893189,-8.28413408366083,
370.462296651428));
#265335=CARTESIAN_POINT('Ctrl Pts',(158.704075916301,-20.7744157382975,
368.462296651428));
#265336=CARTESIAN_POINT('Ctrl Pts',(158.311185598564,-23.7758621134173,
367.981691576521));
#265337=CARTESIAN_POINT('Ctrl Pts',(157.805088795962,-26.7603066464731,
367.5));
#265338=CARTESIAN_POINT('',(160.,-4.30813900827805,377.537703348572));
#265339=CARTESIAN_POINT('',(160.,3.64291929955129E-14,375.));
#265340=CARTESIAN_POINT('Ctrl Pts',(160.,-4.30813900827805,377.537703348572));
#265341=CARTESIAN_POINT('Ctrl Pts',(159.660942106811,-16.900412100217,375.537703348572));
#265342=CARTESIAN_POINT('Ctrl Pts',(157.356193074143,-29.2846130745763,
373.537703348572));
#265343=CARTESIAN_POINT('Ctrl Pts',(155.051444041475,-41.6688140489355,
371.537703348572));
#265344=CARTESIAN_POINT('Ctrl Pts',(150.837754439537,-53.5400027769198,
369.537703348572));
#265345=CARTESIAN_POINT('Ctrl Pts',(148.694504587761,-59.5781607537096,
368.520423931127));
#265346=CARTESIAN_POINT('Ctrl Pts',(146.075461400194,-65.4256802672709,
367.5));
#265347=CARTESIAN_POINT('Ctrl Pts',(130.,4.30813900827812,372.462296651428));
#265348=CARTESIAN_POINT('Ctrl Pts',(130.339057893189,-5.92308287892228,
370.462296651428));
#265349=CARTESIAN_POINT('Ctrl Pts',(129.073425698447,-16.0813817870906,
368.462296651428));
#265350=CARTESIAN_POINT('Ctrl Pts',(127.807793503704,-26.2396806952589,
366.462296651428));
#265351=CARTESIAN_POINT('Ctrl Pts',(124.968635286058,-36.0749255918149,
364.462296651428));
#265352=CARTESIAN_POINT('Ctrl Pts',(122.129477068411,-45.9101704883709,
362.462296651428));
#265353=CARTESIAN_POINT('Ctrl Pts',(117.786702325803,-55.1801850026549,
360.462296651428));
#265354=CARTESIAN_POINT('Ctrl Pts',(113.443927583196,-64.4501995169389,
358.462296651428));
#265355=CARTESIAN_POINT('Ctrl Pts',(107.704469842635,-72.9267251261949,
356.462296651428));
#265356=CARTESIAN_POINT('Ctrl Pts',(101.965012102074,-81.4032507354509,
354.462296651428));
#265357=CARTESIAN_POINT('Ctrl Pts',(94.9701958612989,-88.8775672472035,
352.462296651428));
#265358=CARTESIAN_POINT('Ctrl Pts',(87.9753796205242,-96.351883758956,350.462296651428));
#265359=CARTESIAN_POINT('Ctrl Pts',(79.8974404698481,-102.639948694851,
348.462296651428));
#265360=CARTESIAN_POINT('Ctrl Pts',(71.8195013191721,-108.928013630747,
346.462296651428));
#265361=CARTESIAN_POINT('Ctrl Pts',(62.8573449296273,-113.874993963172,
344.462296651428));
#265362=CARTESIAN_POINT('Ctrl Pts',(53.8951885400825,-118.821974295598,
342.462296651428));
#265363=CARTESIAN_POINT('Ctrl Pts',(44.2694929456714,-122.306058950682,
340.462296651428));
#265364=CARTESIAN_POINT('Ctrl Pts',(34.6437973512603,-125.790143605767,
338.462296651428));
#265365=CARTESIAN_POINT('Ctrl Pts',(24.5915791233694,-127.725542856289,
336.462296651428));
#265366=CARTESIAN_POINT('Ctrl Pts',(14.5393608954785,-129.660942106811,
334.462296651428));
#265367=CARTESIAN_POINT('Ctrl Pts',(4.30813900827813,-130.,332.462296651428));
#265368=CARTESIAN_POINT('Ctrl Pts',(-5.92308287892227,-130.339057893189,
330.462296651428));
#265369=CARTESIAN_POINT('Ctrl Pts',(-16.0813817870906,-129.073425698447,
328.462296651428));
#265370=CARTESIAN_POINT('Ctrl Pts',(-26.2396806952589,-127.807793503705,
326.462296651428));
#265371=CARTESIAN_POINT('Ctrl Pts',(-36.0749255918149,-124.968635286058,
324.462296651428));
#265372=CARTESIAN_POINT('Ctrl Pts',(-45.9101704883709,-122.129477068411,
322.462296651428));
#265373=CARTESIAN_POINT('Ctrl Pts',(-55.1801850026549,-117.786702325803,
320.462296651428));
#265374=CARTESIAN_POINT('Ctrl Pts',(-64.4501995169389,-113.443927583196,
318.462296651428));
#265375=CARTESIAN_POINT('Ctrl Pts',(-72.9267251261949,-107.704469842635,
316.462296651428));
#265376=CARTESIAN_POINT('Ctrl Pts',(-81.4032507354509,-101.965012102074,
314.462296651428));
#265377=CARTESIAN_POINT('Ctrl Pts',(-88.8775672472034,-94.9701958612989,
312.462296651428));
#265378=CARTESIAN_POINT('Ctrl Pts',(-96.351883758956,-87.9753796205242,
310.462296651428));
#265379=CARTESIAN_POINT('Ctrl Pts',(-102.639948694851,-79.8974404698482,
308.462296651428));
#265380=CARTESIAN_POINT('Ctrl Pts',(-108.928013630747,-71.8195013191721,
306.462296651428));
#265381=CARTESIAN_POINT('Ctrl Pts',(-113.874993963172,-62.8573449296273,
304.462296651428));
#265382=CARTESIAN_POINT('Ctrl Pts',(-118.821974295598,-53.8951885400825,
302.462296651428));
#265383=CARTESIAN_POINT('Ctrl Pts',(-122.306058950682,-44.2694929456714,
300.462296651428));
#265384=CARTESIAN_POINT('Ctrl Pts',(-125.790143605767,-34.6437973512603,
298.462296651428));
#265385=CARTESIAN_POINT('Ctrl Pts',(-127.725542856289,-24.5915791233694,
296.462296651428));
#265386=CARTESIAN_POINT('Ctrl Pts',(-129.660942106811,-14.5393608954785,
294.462296651428));
#265387=CARTESIAN_POINT('Ctrl Pts',(-130.,-4.30813900827813,292.462296651428));
#265388=CARTESIAN_POINT('Ctrl Pts',(-130.339057893189,5.92308287892227,
290.462296651428));
#265389=CARTESIAN_POINT('Ctrl Pts',(-129.073425698447,16.0813817870906,
288.462296651428));
#265390=CARTESIAN_POINT('Ctrl Pts',(-127.807793503705,26.2396806952589,
286.462296651428));
#265391=CARTESIAN_POINT('Ctrl Pts',(-124.968635286058,36.0749255918149,
284.462296651428));
#265392=CARTESIAN_POINT('Ctrl Pts',(-122.129477068411,45.9101704883709,
282.462296651428));
#265393=CARTESIAN_POINT('Ctrl Pts',(-117.786702325803,55.1801850026549,
280.462296651428));
#265394=CARTESIAN_POINT('Ctrl Pts',(-113.443927583196,64.4501995169388,
278.462296651428));
#265395=CARTESIAN_POINT('Ctrl Pts',(-107.704469842635,72.9267251261949,
276.462296651428));
#265396=CARTESIAN_POINT('Ctrl Pts',(-101.965012102074,81.4032507354509,
274.462296651428));
#265397=CARTESIAN_POINT('Ctrl Pts',(-94.9701958612989,88.8775672472034,
272.462296651428));
#265398=CARTESIAN_POINT('Ctrl Pts',(-87.9753796205243,96.3518837589559,
270.462296651428));
#265399=CARTESIAN_POINT('Ctrl Pts',(-79.8974404698482,102.639948694851,
268.462296651428));
#265400=CARTESIAN_POINT('Ctrl Pts',(-71.819501319172,108.928013630747,266.462296651428));
#265401=CARTESIAN_POINT('Ctrl Pts',(-62.8573449296273,113.874993963172,
264.462296651428));
#265402=CARTESIAN_POINT('Ctrl Pts',(-53.8951885400826,118.821974295598,
262.462296651428));
#265403=CARTESIAN_POINT('Ctrl Pts',(-44.2694929456714,122.306058950682,
260.462296651428));
#265404=CARTESIAN_POINT('Ctrl Pts',(-34.6437973512603,125.790143605767,
258.462296651428));
#265405=CARTESIAN_POINT('Ctrl Pts',(-24.5915791233694,127.725542856289,
256.462296651428));
#265406=CARTESIAN_POINT('Ctrl Pts',(-14.5393608954786,129.660942106811,
254.462296651428));
#265407=CARTESIAN_POINT('Ctrl Pts',(-4.30813900827814,130.,252.462296651428));
#265408=CARTESIAN_POINT('Ctrl Pts',(5.92308287892232,130.339057893189,250.462296651428));
#265409=CARTESIAN_POINT('Ctrl Pts',(16.0813817870906,129.073425698447,248.462296651428));
#265410=CARTESIAN_POINT('Ctrl Pts',(26.2396806952589,127.807793503705,246.462296651428));
#265411=CARTESIAN_POINT('Ctrl Pts',(36.0749255918149,124.968635286058,244.462296651428));
#265412=CARTESIAN_POINT('Ctrl Pts',(45.9101704883709,122.129477068411,242.462296651428));
#265413=CARTESIAN_POINT('Ctrl Pts',(55.1801850026549,117.786702325803,240.462296651428));
#265414=CARTESIAN_POINT('Ctrl Pts',(64.4501995169388,113.443927583196,238.462296651428));
#265415=CARTESIAN_POINT('Ctrl Pts',(72.9267251261949,107.704469842635,236.462296651428));
#265416=CARTESIAN_POINT('Ctrl Pts',(81.4032507354509,101.965012102074,234.462296651428));
#265417=CARTESIAN_POINT('Ctrl Pts',(88.8775672472034,94.9701958612989,232.462296651428));
#265418=CARTESIAN_POINT('Ctrl Pts',(96.3518837589559,87.9753796205243,230.462296651428));
#265419=CARTESIAN_POINT('Ctrl Pts',(102.639948694851,79.8974404698482,228.462296651428));
#265420=CARTESIAN_POINT('Ctrl Pts',(108.928013630747,71.819501319172,226.462296651428));
#265421=CARTESIAN_POINT('Ctrl Pts',(113.874993963172,62.8573449296273,224.462296651428));
#265422=CARTESIAN_POINT('Ctrl Pts',(118.821974295598,53.8951885400826,222.462296651428));
#265423=CARTESIAN_POINT('Ctrl Pts',(122.306058950682,44.2694929456714,220.462296651428));
#265424=CARTESIAN_POINT('Ctrl Pts',(125.790143605767,34.6437973512603,218.462296651428));
#265425=CARTESIAN_POINT('Ctrl Pts',(127.725542856289,24.5915791233694,216.462296651428));
#265426=CARTESIAN_POINT('Ctrl Pts',(129.660942106811,14.5393608954786,214.462296651428));
#265427=CARTESIAN_POINT('Ctrl Pts',(130.,4.30813900827812,212.462296651428));
#265428=CARTESIAN_POINT('Ctrl Pts',(160.,4.30813900827813,372.462296651428));
#265429=CARTESIAN_POINT('Ctrl Pts',(160.339057893189,-8.28413408366083,
370.462296651428));
#265430=CARTESIAN_POINT('Ctrl Pts',(158.704075916301,-20.7744157382975,
368.462296651428));
#265431=CARTESIAN_POINT('Ctrl Pts',(157.069093939413,-33.2646973929343,
366.462296651428));
#265432=CARTESIAN_POINT('Ctrl Pts',(153.500330774912,-45.3454354230633,
364.462296651428));
#265433=CARTESIAN_POINT('Ctrl Pts',(149.931567610412,-57.4261734531924,
362.462296651428));
#265434=CARTESIAN_POINT('Ctrl Pts',(144.516898051455,-68.7998999948413,
360.462296651428));
#265435=CARTESIAN_POINT('Ctrl Pts',(139.102228492497,-80.1736265364901,
358.462296651428));
#265436=CARTESIAN_POINT('Ctrl Pts',(131.974979673883,-90.5602826949691,
356.462296651428));
#265437=CARTESIAN_POINT('Ctrl Pts',(124.847730855269,-100.946938853448,
354.462296651428));
#265438=CARTESIAN_POINT('Ctrl Pts',(116.183399296895,-110.0907706828,352.462296651428));
#265439=CARTESIAN_POINT('Ctrl Pts',(107.519067738521,-119.234602512152,
350.462296651428));
#265440=CARTESIAN_POINT('Ctrl Pts',(97.5309980386224,-126.9104585261,348.462296651428));
#265441=CARTESIAN_POINT('Ctrl Pts',(87.5429283387234,-134.586314540048,
346.462296651428));
#265442=CARTESIAN_POINT('Ctrl Pts',(76.4770599218137,-140.605189688823,
344.462296651428));
#265443=CARTESIAN_POINT('Ctrl Pts',(65.4111915049041,-146.624064837599,
342.462296651428));
#265444=CARTESIAN_POINT('Ctrl Pts',(53.5400027769198,-150.837754439537,
340.462296651428));
#265445=CARTESIAN_POINT('Ctrl Pts',(41.6688140489356,-155.051444041475,
338.462296651428));
#265446=CARTESIAN_POINT('Ctrl Pts',(29.2846130745764,-157.356193074143,
336.462296651428));
#265447=CARTESIAN_POINT('Ctrl Pts',(16.9004121002171,-159.660942106811,
334.462296651428));
#265448=CARTESIAN_POINT('Ctrl Pts',(4.30813900827814,-160.,332.462296651428));
#265449=CARTESIAN_POINT('Ctrl Pts',(-8.28413408366082,-160.339057893189,
330.462296651428));
#265450=CARTESIAN_POINT('Ctrl Pts',(-20.7744157382975,-158.704075916301,
328.462296651428));
#265451=CARTESIAN_POINT('Ctrl Pts',(-33.2646973929342,-157.069093939413,
326.462296651428));
#265452=CARTESIAN_POINT('Ctrl Pts',(-45.3454354230633,-153.500330774912,
324.462296651428));
#265453=CARTESIAN_POINT('Ctrl Pts',(-57.4261734531924,-149.931567610412,
322.462296651428));
#265454=CARTESIAN_POINT('Ctrl Pts',(-68.7998999948413,-144.516898051455,
320.462296651428));
#265455=CARTESIAN_POINT('Ctrl Pts',(-80.1736265364901,-139.102228492497,
318.462296651428));
#265456=CARTESIAN_POINT('Ctrl Pts',(-90.5602826949691,-131.974979673883,
316.462296651428));
#265457=CARTESIAN_POINT('Ctrl Pts',(-100.946938853448,-124.847730855269,
314.462296651428));
#265458=CARTESIAN_POINT('Ctrl Pts',(-110.0907706828,-116.183399296895,312.462296651428));
#265459=CARTESIAN_POINT('Ctrl Pts',(-119.234602512152,-107.519067738521,
310.462296651428));
#265460=CARTESIAN_POINT('Ctrl Pts',(-126.9104585261,-97.5309980386224,308.462296651428));
#265461=CARTESIAN_POINT('Ctrl Pts',(-134.586314540048,-87.5429283387234,
306.462296651428));
#265462=CARTESIAN_POINT('Ctrl Pts',(-140.605189688823,-76.4770599218137,
304.462296651428));
#265463=CARTESIAN_POINT('Ctrl Pts',(-146.624064837599,-65.4111915049041,
302.462296651428));
#265464=CARTESIAN_POINT('Ctrl Pts',(-150.837754439537,-53.5400027769199,
300.462296651428));
#265465=CARTESIAN_POINT('Ctrl Pts',(-155.051444041475,-41.6688140489356,
298.462296651428));
#265466=CARTESIAN_POINT('Ctrl Pts',(-157.356193074143,-29.2846130745764,
296.462296651428));
#265467=CARTESIAN_POINT('Ctrl Pts',(-159.660942106811,-16.9004121002171,
294.462296651428));
#265468=CARTESIAN_POINT('Ctrl Pts',(-160.,-4.30813900827815,292.462296651428));
#265469=CARTESIAN_POINT('Ctrl Pts',(-160.339057893189,8.28413408366081,
290.462296651428));
#265470=CARTESIAN_POINT('Ctrl Pts',(-158.704075916301,20.7744157382975,
288.462296651428));
#265471=CARTESIAN_POINT('Ctrl Pts',(-157.069093939413,33.2646973929342,
286.462296651428));
#265472=CARTESIAN_POINT('Ctrl Pts',(-153.500330774912,45.3454354230633,
284.462296651428));
#265473=CARTESIAN_POINT('Ctrl Pts',(-149.931567610412,57.4261734531924,
282.462296651428));
#265474=CARTESIAN_POINT('Ctrl Pts',(-144.516898051455,68.7998999948413,
280.462296651428));
#265475=CARTESIAN_POINT('Ctrl Pts',(-139.102228492497,80.1736265364901,
278.462296651428));
#265476=CARTESIAN_POINT('Ctrl Pts',(-131.974979673883,90.5602826949691,
276.462296651428));
#265477=CARTESIAN_POINT('Ctrl Pts',(-124.847730855269,100.946938853448,
274.462296651428));
#265478=CARTESIAN_POINT('Ctrl Pts',(-116.183399296895,110.0907706828,272.462296651428));
#265479=CARTESIAN_POINT('Ctrl Pts',(-107.519067738521,119.234602512152,
270.462296651428));
#265480=CARTESIAN_POINT('Ctrl Pts',(-97.5309980386224,126.9104585261,268.462296651428));
#265481=CARTESIAN_POINT('Ctrl Pts',(-87.5429283387233,134.586314540048,
266.462296651428));
#265482=CARTESIAN_POINT('Ctrl Pts',(-76.4770599218137,140.605189688823,
264.462296651428));
#265483=CARTESIAN_POINT('Ctrl Pts',(-65.4111915049042,146.624064837599,
262.462296651428));
#265484=CARTESIAN_POINT('Ctrl Pts',(-53.5400027769199,150.837754439537,
260.462296651428));
#265485=CARTESIAN_POINT('Ctrl Pts',(-41.6688140489356,155.051444041475,
258.462296651428));
#265486=CARTESIAN_POINT('Ctrl Pts',(-29.2846130745764,157.356193074143,
256.462296651428));
#265487=CARTESIAN_POINT('Ctrl Pts',(-16.9004121002172,159.660942106811,
254.462296651428));
#265488=CARTESIAN_POINT('Ctrl Pts',(-4.30813900827816,160.,252.462296651428));
#265489=CARTESIAN_POINT('Ctrl Pts',(8.28413408366087,160.339057893189,250.462296651428));
#265490=CARTESIAN_POINT('Ctrl Pts',(20.7744157382975,158.704075916301,248.462296651428));
#265491=CARTESIAN_POINT('Ctrl Pts',(33.2646973929342,157.069093939413,246.462296651428));
#265492=CARTESIAN_POINT('Ctrl Pts',(45.3454354230633,153.500330774912,244.462296651428));
#265493=CARTESIAN_POINT('Ctrl Pts',(57.4261734531925,149.931567610412,242.462296651428));
#265494=CARTESIAN_POINT('Ctrl Pts',(68.7998999948413,144.516898051455,240.462296651428));
#265495=CARTESIAN_POINT('Ctrl Pts',(80.1736265364901,139.102228492498,238.462296651428));
#265496=CARTESIAN_POINT('Ctrl Pts',(90.560282694969,131.974979673883,236.462296651428));
#265497=CARTESIAN_POINT('Ctrl Pts',(100.946938853448,124.847730855269,234.462296651428));
#265498=CARTESIAN_POINT('Ctrl Pts',(110.0907706828,116.183399296895,232.462296651428));
#265499=CARTESIAN_POINT('Ctrl Pts',(119.234602512152,107.519067738521,230.462296651428));
#265500=CARTESIAN_POINT('Ctrl Pts',(126.9104585261,97.5309980386224,228.462296651428));
#265501=CARTESIAN_POINT('Ctrl Pts',(134.586314540048,87.5429283387233,226.462296651428));
#265502=CARTESIAN_POINT('Ctrl Pts',(140.605189688823,76.4770599218137,224.462296651428));
#265503=CARTESIAN_POINT('Ctrl Pts',(146.624064837599,65.4111915049042,222.462296651428));
#265504=CARTESIAN_POINT('Ctrl Pts',(150.837754439537,53.5400027769199,220.462296651428));
#265505=CARTESIAN_POINT('Ctrl Pts',(155.051444041475,41.6688140489356,218.462296651428));
#265506=CARTESIAN_POINT('Ctrl Pts',(157.356193074143,29.2846130745764,216.462296651428));
#265507=CARTESIAN_POINT('Ctrl Pts',(159.660942106811,16.9004121002172,214.462296651428));
#265508=CARTESIAN_POINT('Ctrl Pts',(160.,4.30813900827813,212.462296651428));
#265509=CARTESIAN_POINT('',(128.373075022505,-20.9502666088245,367.5));
#265510=CARTESIAN_POINT('',(128.373075022505,-20.9502666088245,367.5));
#265511=CARTESIAN_POINT('',(130.,4.30813900827812,372.462296651428));
#265512=CARTESIAN_POINT('Ctrl Pts',(130.,4.30813900827812,372.462296651428));
#265513=CARTESIAN_POINT('Ctrl Pts',(130.339057893189,-5.92308287892229,
370.462296651428));
#265514=CARTESIAN_POINT('Ctrl Pts',(129.073425698447,-16.0813817870906,
368.462296651428));
#265515=CARTESIAN_POINT('Ctrl Pts',(128.769291070567,-18.522446790936,367.981691576521));
#265516=CARTESIAN_POINT('Ctrl Pts',(128.373075022505,-20.9502666088245,
367.5));
#265517=CARTESIAN_POINT('',(145.,4.30813900827812,372.462296651428));
#265518=CARTESIAN_POINT('Ctrl Pts',(130.,-4.30813900827807,377.537703348572));
#265519=CARTESIAN_POINT('Ctrl Pts',(129.660942106811,-14.5393608954785,
375.537703348572));
#265520=CARTESIAN_POINT('Ctrl Pts',(127.725542856289,-24.5915791233694,
373.537703348572));
#265521=CARTESIAN_POINT('Ctrl Pts',(125.790143605767,-34.6437973512603,
371.537703348572));
#265522=CARTESIAN_POINT('Ctrl Pts',(122.306058950682,-44.2694929456714,
369.537703348572));
#265523=CARTESIAN_POINT('Ctrl Pts',(118.821974295598,-53.8951885400825,
367.537703348572));
#265524=CARTESIAN_POINT('Ctrl Pts',(113.874993963172,-62.8573449296272,
365.537703348572));
#265525=CARTESIAN_POINT('Ctrl Pts',(108.928013630747,-71.819501319172,363.537703348572));
#265526=CARTESIAN_POINT('Ctrl Pts',(102.639948694851,-79.8974404698481,
361.537703348572));
#265527=CARTESIAN_POINT('Ctrl Pts',(96.351883758956,-87.9753796205242,359.537703348572));
#265528=CARTESIAN_POINT('Ctrl Pts',(88.8775672472035,-94.9701958612989,
357.537703348572));
#265529=CARTESIAN_POINT('Ctrl Pts',(81.403250735451,-101.965012102074,355.537703348572));
#265530=CARTESIAN_POINT('Ctrl Pts',(72.9267251261949,-107.704469842635,
353.537703348572));
#265531=CARTESIAN_POINT('Ctrl Pts',(64.4501995169389,-113.443927583196,
351.537703348572));
#265532=CARTESIAN_POINT('Ctrl Pts',(55.1801850026549,-117.786702325803,
349.537703348572));
#265533=CARTESIAN_POINT('Ctrl Pts',(45.910170488371,-122.129477068411,347.537703348572));
#265534=CARTESIAN_POINT('Ctrl Pts',(36.074925591815,-124.968635286058,345.537703348572));
#265535=CARTESIAN_POINT('Ctrl Pts',(26.239680695259,-127.807793503704,343.537703348572));
#265536=CARTESIAN_POINT('Ctrl Pts',(16.0813817870907,-129.073425698447,
341.537703348572));
#265537=CARTESIAN_POINT('Ctrl Pts',(5.92308287892234,-130.339057893189,
339.537703348572));
#265538=CARTESIAN_POINT('Ctrl Pts',(-4.30813900827806,-130.,337.537703348572));
#265539=CARTESIAN_POINT('Ctrl Pts',(-14.5393608954785,-129.660942106811,
335.537703348572));
#265540=CARTESIAN_POINT('Ctrl Pts',(-24.5915791233694,-127.725542856289,
333.537703348572));
#265541=CARTESIAN_POINT('Ctrl Pts',(-34.6437973512603,-125.790143605767,
331.537703348572));
#265542=CARTESIAN_POINT('Ctrl Pts',(-44.2694929456713,-122.306058950682,
329.537703348572));
#265543=CARTESIAN_POINT('Ctrl Pts',(-53.8951885400825,-118.821974295598,
327.537703348572));
#265544=CARTESIAN_POINT('Ctrl Pts',(-62.8573449296272,-113.874993963172,
325.537703348572));
#265545=CARTESIAN_POINT('Ctrl Pts',(-71.819501319172,-108.928013630747,
323.537703348572));
#265546=CARTESIAN_POINT('Ctrl Pts',(-79.8974404698481,-102.639948694851,
321.537703348572));
#265547=CARTESIAN_POINT('Ctrl Pts',(-87.9753796205242,-96.351883758956,
319.537703348572));
#265548=CARTESIAN_POINT('Ctrl Pts',(-94.9701958612989,-88.8775672472035,
317.537703348572));
#265549=CARTESIAN_POINT('Ctrl Pts',(-101.965012102074,-81.403250735451,
315.537703348572));
#265550=CARTESIAN_POINT('Ctrl Pts',(-107.704469842635,-72.9267251261949,
313.537703348572));
#265551=CARTESIAN_POINT('Ctrl Pts',(-113.443927583196,-64.4501995169389,
311.537703348572));
#265552=CARTESIAN_POINT('Ctrl Pts',(-117.786702325803,-55.1801850026549,
309.537703348572));
#265553=CARTESIAN_POINT('Ctrl Pts',(-122.129477068411,-45.910170488371,
307.537703348572));
#265554=CARTESIAN_POINT('Ctrl Pts',(-124.968635286058,-36.074925591815,
305.537703348572));
#265555=CARTESIAN_POINT('Ctrl Pts',(-127.807793503704,-26.239680695259,
303.537703348572));
#265556=CARTESIAN_POINT('Ctrl Pts',(-129.073425698447,-16.0813817870907,
301.537703348572));
#265557=CARTESIAN_POINT('Ctrl Pts',(-130.339057893189,-5.92308287892235,
299.537703348572));
#265558=CARTESIAN_POINT('Ctrl Pts',(-130.,4.30813900827805,297.537703348572));
#265559=CARTESIAN_POINT('Ctrl Pts',(-129.660942106811,14.5393608954784,
295.537703348572));
#265560=CARTESIAN_POINT('Ctrl Pts',(-127.725542856289,24.5915791233693,
293.537703348572));
#265561=CARTESIAN_POINT('Ctrl Pts',(-125.790143605767,34.6437973512602,
291.537703348572));
#265562=CARTESIAN_POINT('Ctrl Pts',(-122.306058950682,44.2694929456713,
289.537703348572));
#265563=CARTESIAN_POINT('Ctrl Pts',(-118.821974295598,53.8951885400825,
287.537703348572));
#265564=CARTESIAN_POINT('Ctrl Pts',(-113.874993963172,62.8573449296272,
285.537703348572));
#265565=CARTESIAN_POINT('Ctrl Pts',(-108.928013630747,71.819501319172,283.537703348572));
#265566=CARTESIAN_POINT('Ctrl Pts',(-102.639948694851,79.8974404698481,
281.537703348572));
#265567=CARTESIAN_POINT('Ctrl Pts',(-96.3518837589561,87.9753796205242,
279.537703348572));
#265568=CARTESIAN_POINT('Ctrl Pts',(-88.8775672472035,94.9701958612989,
277.537703348572));
#265569=CARTESIAN_POINT('Ctrl Pts',(-81.403250735451,101.965012102074,275.537703348572));
#265570=CARTESIAN_POINT('Ctrl Pts',(-72.9267251261949,107.704469842635,
273.537703348572));
#265571=CARTESIAN_POINT('Ctrl Pts',(-64.4501995169389,113.443927583196,
271.537703348572));
#265572=CARTESIAN_POINT('Ctrl Pts',(-55.1801850026549,117.786702325803,
269.537703348572));
#265573=CARTESIAN_POINT('Ctrl Pts',(-45.910170488371,122.129477068411,267.537703348572));
#265574=CARTESIAN_POINT('Ctrl Pts',(-36.074925591815,124.968635286058,265.537703348572));
#265575=CARTESIAN_POINT('Ctrl Pts',(-26.239680695259,127.807793503704,263.537703348572));
#265576=CARTESIAN_POINT('Ctrl Pts',(-16.0813817870907,129.073425698447,
261.537703348572));
#265577=CARTESIAN_POINT('Ctrl Pts',(-5.92308287892242,130.339057893189,
259.537703348572));
#265578=CARTESIAN_POINT('Ctrl Pts',(4.30813900827804,130.,257.537703348572));
#265579=CARTESIAN_POINT('Ctrl Pts',(14.5393608954785,129.660942106811,255.537703348572));
#265580=CARTESIAN_POINT('Ctrl Pts',(24.5915791233693,127.725542856289,253.537703348572));
#265581=CARTESIAN_POINT('Ctrl Pts',(34.6437973512602,125.790143605767,251.537703348572));
#265582=CARTESIAN_POINT('Ctrl Pts',(44.2694929456713,122.306058950682,249.537703348572));
#265583=CARTESIAN_POINT('Ctrl Pts',(53.8951885400825,118.821974295598,247.537703348572));
#265584=CARTESIAN_POINT('Ctrl Pts',(62.8573449296272,113.874993963172,245.537703348572));
#265585=CARTESIAN_POINT('Ctrl Pts',(71.819501319172,108.928013630747,243.537703348572));
#265586=CARTESIAN_POINT('Ctrl Pts',(79.8974404698481,102.639948694851,241.537703348572));
#265587=CARTESIAN_POINT('Ctrl Pts',(87.9753796205242,96.351883758956,239.537703348572));
#265588=CARTESIAN_POINT('Ctrl Pts',(94.9701958612989,88.8775672472035,237.537703348572));
#265589=CARTESIAN_POINT('Ctrl Pts',(101.965012102074,81.403250735451,235.537703348572));
#265590=CARTESIAN_POINT('Ctrl Pts',(107.704469842635,72.926725126195,233.537703348572));
#265591=CARTESIAN_POINT('Ctrl Pts',(113.443927583196,64.4501995169389,231.537703348572));
#265592=CARTESIAN_POINT('Ctrl Pts',(117.786702325803,55.1801850026549,229.537703348572));
#265593=CARTESIAN_POINT('Ctrl Pts',(122.129477068411,45.910170488371,227.537703348572));
#265594=CARTESIAN_POINT('Ctrl Pts',(124.968635286058,36.074925591815,225.537703348572));
#265595=CARTESIAN_POINT('Ctrl Pts',(127.807793503704,26.239680695259,223.537703348572));
#265596=CARTESIAN_POINT('Ctrl Pts',(129.073425698447,16.0813817870907,221.537703348572));
#265597=CARTESIAN_POINT('Ctrl Pts',(130.339057893189,5.92308287892242,219.537703348572));
#265598=CARTESIAN_POINT('Ctrl Pts',(130.,-4.30813900827807,217.537703348572));
#265599=CARTESIAN_POINT('Ctrl Pts',(130.,4.30813900827812,372.462296651428));
#265600=CARTESIAN_POINT('Ctrl Pts',(130.339057893189,-5.92308287892228,
370.462296651428));
#265601=CARTESIAN_POINT('Ctrl Pts',(129.073425698447,-16.0813817870906,
368.462296651428));
#265602=CARTESIAN_POINT('Ctrl Pts',(127.807793503704,-26.2396806952589,
366.462296651428));
#265603=CARTESIAN_POINT('Ctrl Pts',(124.968635286058,-36.0749255918149,
364.462296651428));
#265604=CARTESIAN_POINT('Ctrl Pts',(122.129477068411,-45.9101704883709,
362.462296651428));
#265605=CARTESIAN_POINT('Ctrl Pts',(117.786702325803,-55.1801850026549,
360.462296651428));
#265606=CARTESIAN_POINT('Ctrl Pts',(113.443927583196,-64.4501995169389,
358.462296651428));
#265607=CARTESIAN_POINT('Ctrl Pts',(107.704469842635,-72.9267251261949,
356.462296651428));
#265608=CARTESIAN_POINT('Ctrl Pts',(101.965012102074,-81.4032507354509,
354.462296651428));
#265609=CARTESIAN_POINT('Ctrl Pts',(94.9701958612989,-88.8775672472035,
352.462296651428));
#265610=CARTESIAN_POINT('Ctrl Pts',(87.9753796205242,-96.351883758956,350.462296651428));
#265611=CARTESIAN_POINT('Ctrl Pts',(79.8974404698481,-102.639948694851,
348.462296651428));
#265612=CARTESIAN_POINT('Ctrl Pts',(71.8195013191721,-108.928013630747,
346.462296651428));
#265613=CARTESIAN_POINT('Ctrl Pts',(62.8573449296273,-113.874993963172,
344.462296651428));
#265614=CARTESIAN_POINT('Ctrl Pts',(53.8951885400825,-118.821974295598,
342.462296651428));
#265615=CARTESIAN_POINT('Ctrl Pts',(44.2694929456714,-122.306058950682,
340.462296651428));
#265616=CARTESIAN_POINT('Ctrl Pts',(34.6437973512603,-125.790143605767,
338.462296651428));
#265617=CARTESIAN_POINT('Ctrl Pts',(24.5915791233694,-127.725542856289,
336.462296651428));
#265618=CARTESIAN_POINT('Ctrl Pts',(14.5393608954785,-129.660942106811,
334.462296651428));
#265619=CARTESIAN_POINT('Ctrl Pts',(4.30813900827813,-130.,332.462296651428));
#265620=CARTESIAN_POINT('Ctrl Pts',(-5.92308287892227,-130.339057893189,
330.462296651428));
#265621=CARTESIAN_POINT('Ctrl Pts',(-16.0813817870906,-129.073425698447,
328.462296651428));
#265622=CARTESIAN_POINT('Ctrl Pts',(-26.2396806952589,-127.807793503705,
326.462296651428));
#265623=CARTESIAN_POINT('Ctrl Pts',(-36.0749255918149,-124.968635286058,
324.462296651428));
#265624=CARTESIAN_POINT('Ctrl Pts',(-45.9101704883709,-122.129477068411,
322.462296651428));
#265625=CARTESIAN_POINT('Ctrl Pts',(-55.1801850026549,-117.786702325803,
320.462296651428));
#265626=CARTESIAN_POINT('Ctrl Pts',(-64.4501995169389,-113.443927583196,
318.462296651428));
#265627=CARTESIAN_POINT('Ctrl Pts',(-72.9267251261949,-107.704469842635,
316.462296651428));
#265628=CARTESIAN_POINT('Ctrl Pts',(-81.4032507354509,-101.965012102074,
314.462296651428));
#265629=CARTESIAN_POINT('Ctrl Pts',(-88.8775672472034,-94.9701958612989,
312.462296651428));
#265630=CARTESIAN_POINT('Ctrl Pts',(-96.351883758956,-87.9753796205242,
310.462296651428));
#265631=CARTESIAN_POINT('Ctrl Pts',(-102.639948694851,-79.8974404698482,
308.462296651428));
#265632=CARTESIAN_POINT('Ctrl Pts',(-108.928013630747,-71.8195013191721,
306.462296651428));
#265633=CARTESIAN_POINT('Ctrl Pts',(-113.874993963172,-62.8573449296273,
304.462296651428));
#265634=CARTESIAN_POINT('Ctrl Pts',(-118.821974295598,-53.8951885400825,
302.462296651428));
#265635=CARTESIAN_POINT('Ctrl Pts',(-122.306058950682,-44.2694929456714,
300.462296651428));
#265636=CARTESIAN_POINT('Ctrl Pts',(-125.790143605767,-34.6437973512603,
298.462296651428));
#265637=CARTESIAN_POINT('Ctrl Pts',(-127.725542856289,-24.5915791233694,
296.462296651428));
#265638=CARTESIAN_POINT('Ctrl Pts',(-129.660942106811,-14.5393608954785,
294.462296651428));
#265639=CARTESIAN_POINT('Ctrl Pts',(-130.,-4.30813900827813,292.462296651428));
#265640=CARTESIAN_POINT('Ctrl Pts',(-130.339057893189,5.92308287892227,
290.462296651428));
#265641=CARTESIAN_POINT('Ctrl Pts',(-129.073425698447,16.0813817870906,
288.462296651428));
#265642=CARTESIAN_POINT('Ctrl Pts',(-127.807793503705,26.2396806952589,
286.462296651428));
#265643=CARTESIAN_POINT('Ctrl Pts',(-124.968635286058,36.0749255918149,
284.462296651428));
#265644=CARTESIAN_POINT('Ctrl Pts',(-122.129477068411,45.9101704883709,
282.462296651428));
#265645=CARTESIAN_POINT('Ctrl Pts',(-117.786702325803,55.1801850026549,
280.462296651428));
#265646=CARTESIAN_POINT('Ctrl Pts',(-113.443927583196,64.4501995169388,
278.462296651428));
#265647=CARTESIAN_POINT('Ctrl Pts',(-107.704469842635,72.9267251261949,
276.462296651428));
#265648=CARTESIAN_POINT('Ctrl Pts',(-101.965012102074,81.4032507354509,
274.462296651428));
#265649=CARTESIAN_POINT('Ctrl Pts',(-94.9701958612989,88.8775672472034,
272.462296651428));
#265650=CARTESIAN_POINT('Ctrl Pts',(-87.9753796205243,96.3518837589559,
270.462296651428));
#265651=CARTESIAN_POINT('Ctrl Pts',(-79.8974404698482,102.639948694851,
268.462296651428));
#265652=CARTESIAN_POINT('Ctrl Pts',(-71.819501319172,108.928013630747,266.462296651428));
#265653=CARTESIAN_POINT('Ctrl Pts',(-62.8573449296273,113.874993963172,
264.462296651428));
#265654=CARTESIAN_POINT('Ctrl Pts',(-53.8951885400826,118.821974295598,
262.462296651428));
#265655=CARTESIAN_POINT('Ctrl Pts',(-44.2694929456714,122.306058950682,
260.462296651428));
#265656=CARTESIAN_POINT('Ctrl Pts',(-34.6437973512603,125.790143605767,
258.462296651428));
#265657=CARTESIAN_POINT('Ctrl Pts',(-24.5915791233694,127.725542856289,
256.462296651428));
#265658=CARTESIAN_POINT('Ctrl Pts',(-14.5393608954786,129.660942106811,
254.462296651428));
#265659=CARTESIAN_POINT('Ctrl Pts',(-4.30813900827814,130.,252.462296651428));
#265660=CARTESIAN_POINT('Ctrl Pts',(5.92308287892232,130.339057893189,250.462296651428));
#265661=CARTESIAN_POINT('Ctrl Pts',(16.0813817870906,129.073425698447,248.462296651428));
#265662=CARTESIAN_POINT('Ctrl Pts',(26.2396806952589,127.807793503705,246.462296651428));
#265663=CARTESIAN_POINT('Ctrl Pts',(36.0749255918149,124.968635286058,244.462296651428));
#265664=CARTESIAN_POINT('Ctrl Pts',(45.9101704883709,122.129477068411,242.462296651428));
#265665=CARTESIAN_POINT('Ctrl Pts',(55.1801850026549,117.786702325803,240.462296651428));
#265666=CARTESIAN_POINT('Ctrl Pts',(64.4501995169388,113.443927583196,238.462296651428));
#265667=CARTESIAN_POINT('Ctrl Pts',(72.9267251261949,107.704469842635,236.462296651428));
#265668=CARTESIAN_POINT('Ctrl Pts',(81.4032507354509,101.965012102074,234.462296651428));
#265669=CARTESIAN_POINT('Ctrl Pts',(88.8775672472034,94.9701958612989,232.462296651428));
#265670=CARTESIAN_POINT('Ctrl Pts',(96.3518837589559,87.9753796205243,230.462296651428));
#265671=CARTESIAN_POINT('Ctrl Pts',(102.639948694851,79.8974404698482,228.462296651428));
#265672=CARTESIAN_POINT('Ctrl Pts',(108.928013630747,71.819501319172,226.462296651428));
#265673=CARTESIAN_POINT('Ctrl Pts',(113.874993963172,62.8573449296273,224.462296651428));
#265674=CARTESIAN_POINT('Ctrl Pts',(118.821974295598,53.8951885400826,222.462296651428));
#265675=CARTESIAN_POINT('Ctrl Pts',(122.306058950682,44.2694929456714,220.462296651428));
#265676=CARTESIAN_POINT('Ctrl Pts',(125.790143605767,34.6437973512603,218.462296651428));
#265677=CARTESIAN_POINT('Ctrl Pts',(127.725542856289,24.5915791233694,216.462296651428));
#265678=CARTESIAN_POINT('Ctrl Pts',(129.660942106811,14.5393608954786,214.462296651428));
#265679=CARTESIAN_POINT('Ctrl Pts',(130.,4.30813900827812,212.462296651428));
#265680=CARTESIAN_POINT('',(118.376086385729,-53.9041949546879,367.5));
#265681=CARTESIAN_POINT('Ctrl Pts',(118.376086385729,-53.9041949546878,
367.5));
#265682=CARTESIAN_POINT('Ctrl Pts',(119.546342407814,-51.276867586873,367.5));
#265683=CARTESIAN_POINT('Ctrl Pts',(120.634616850713,-48.6137313363232,
367.499999999997));
#265684=CARTESIAN_POINT('Ctrl Pts',(122.645087654721,-43.2205933565688,
367.499999999997));
#265685=CARTESIAN_POINT('Ctrl Pts',(123.566638088336,-40.4917272023246,
367.5));
#265686=CARTESIAN_POINT('Ctrl Pts',(126.073121396906,-32.2286687868894,
367.5));
#265687=CARTESIAN_POINT('Ctrl Pts',(127.399213018599,-26.6223327935022,
367.5));
#265688=CARTESIAN_POINT('Ctrl Pts',(128.373075022505,-20.9502666088246,
367.5));
#265689=CARTESIAN_POINT('',(130.,-4.30813900827807,377.537703348572));
#265690=CARTESIAN_POINT('Ctrl Pts',(130.,-4.30813900827807,377.537703348572));
#265691=CARTESIAN_POINT('Ctrl Pts',(129.660942106811,-14.5393608954785,
375.537703348572));
#265692=CARTESIAN_POINT('Ctrl Pts',(127.725542856289,-24.5915791233694,
373.537703348572));
#265693=CARTESIAN_POINT('Ctrl Pts',(125.790143605767,-34.6437973512603,
371.537703348572));
#265694=CARTESIAN_POINT('Ctrl Pts',(122.306058950682,-44.2694929456714,
369.537703348572));
#265695=CARTESIAN_POINT('Ctrl Pts',(120.533915146556,-49.1655039490629,
368.520423931127));
#265696=CARTESIAN_POINT('Ctrl Pts',(118.376086385729,-53.9041949546879,
367.5));
#265697=CARTESIAN_POINT('',(130.,2.68882138776405E-14,375.));
#265698=CARTESIAN_POINT('Ctrl Pts',(160.,-4.30813900827805,377.537703348572));
#265699=CARTESIAN_POINT('Ctrl Pts',(159.660942106811,-16.900412100217,375.537703348572));
#265700=CARTESIAN_POINT('Ctrl Pts',(157.356193074143,-29.2846130745763,
373.537703348572));
#265701=CARTESIAN_POINT('Ctrl Pts',(155.051444041475,-41.6688140489355,
371.537703348572));
#265702=CARTESIAN_POINT('Ctrl Pts',(150.837754439537,-53.5400027769198,
369.537703348572));
#265703=CARTESIAN_POINT('Ctrl Pts',(146.624064837599,-65.411191504904,367.537703348572));
#265704=CARTESIAN_POINT('Ctrl Pts',(140.605189688823,-76.4770599218136,
365.537703348572));
#265705=CARTESIAN_POINT('Ctrl Pts',(134.586314540048,-87.5429283387233,
363.537703348572));
#265706=CARTESIAN_POINT('Ctrl Pts',(126.9104585261,-97.5309980386223,361.537703348572));
#265707=CARTESIAN_POINT('Ctrl Pts',(119.234602512152,-107.519067738521,
359.537703348572));
#265708=CARTESIAN_POINT('Ctrl Pts',(110.0907706828,-116.183399296895,357.537703348572));
#265709=CARTESIAN_POINT('Ctrl Pts',(100.946938853448,-124.847730855269,
355.537703348572));
#265710=CARTESIAN_POINT('Ctrl Pts',(90.5602826949691,-131.974979673883,
353.537703348572));
#265711=CARTESIAN_POINT('Ctrl Pts',(80.1736265364902,-139.102228492497,
351.537703348572));
#265712=CARTESIAN_POINT('Ctrl Pts',(68.7998999948414,-144.516898051454,
349.537703348572));
#265713=CARTESIAN_POINT('Ctrl Pts',(57.4261734531925,-149.931567610412,
347.537703348572));
#265714=CARTESIAN_POINT('Ctrl Pts',(45.3454354230634,-153.500330774912,
345.537703348572));
#265715=CARTESIAN_POINT('Ctrl Pts',(33.2646973929343,-157.069093939413,
343.537703348572));
#265716=CARTESIAN_POINT('Ctrl Pts',(20.7744157382976,-158.704075916301,
341.537703348572));
#265717=CARTESIAN_POINT('Ctrl Pts',(8.28413408366091,-160.339057893189,
339.537703348572));
#265718=CARTESIAN_POINT('Ctrl Pts',(-4.30813900827804,-160.,337.537703348572));
#265719=CARTESIAN_POINT('Ctrl Pts',(-16.900412100217,-159.660942106811,
335.537703348572));
#265720=CARTESIAN_POINT('Ctrl Pts',(-29.2846130745763,-157.356193074143,
333.537703348572));
#265721=CARTESIAN_POINT('Ctrl Pts',(-41.6688140489355,-155.051444041475,
331.537703348572));
#265722=CARTESIAN_POINT('Ctrl Pts',(-53.5400027769198,-150.837754439537,
329.537703348572));
#265723=CARTESIAN_POINT('Ctrl Pts',(-65.411191504904,-146.624064837599,
327.537703348572));
#265724=CARTESIAN_POINT('Ctrl Pts',(-76.4770599218136,-140.605189688823,
325.537703348572));
#265725=CARTESIAN_POINT('Ctrl Pts',(-87.5429283387233,-134.586314540048,
323.537703348572));
#265726=CARTESIAN_POINT('Ctrl Pts',(-97.5309980386223,-126.9104585261,321.537703348572));
#265727=CARTESIAN_POINT('Ctrl Pts',(-107.519067738521,-119.234602512152,
319.537703348572));
#265728=CARTESIAN_POINT('Ctrl Pts',(-116.183399296895,-110.0907706828,317.537703348572));
#265729=CARTESIAN_POINT('Ctrl Pts',(-124.847730855269,-100.946938853448,
315.537703348572));
#265730=CARTESIAN_POINT('Ctrl Pts',(-131.974979673883,-90.5602826949692,
313.537703348572));
#265731=CARTESIAN_POINT('Ctrl Pts',(-139.102228492497,-80.1736265364902,
311.537703348572));
#265732=CARTESIAN_POINT('Ctrl Pts',(-144.516898051454,-68.7998999948414,
309.537703348572));
#265733=CARTESIAN_POINT('Ctrl Pts',(-149.931567610412,-57.4261734531925,
307.537703348572));
#265734=CARTESIAN_POINT('Ctrl Pts',(-153.500330774912,-45.3454354230634,
305.537703348572));
#265735=CARTESIAN_POINT('Ctrl Pts',(-157.069093939413,-33.2646973929344,
303.537703348572));
#265736=CARTESIAN_POINT('Ctrl Pts',(-158.704075916301,-20.7744157382976,
301.537703348572));
#265737=CARTESIAN_POINT('Ctrl Pts',(-160.339057893189,-8.28413408366092,
299.537703348572));
#265738=CARTESIAN_POINT('Ctrl Pts',(-160.,4.30813900827803,297.537703348572));
#265739=CARTESIAN_POINT('Ctrl Pts',(-159.660942106811,16.900412100217,295.537703348572));
#265740=CARTESIAN_POINT('Ctrl Pts',(-157.356193074143,29.2846130745763,
293.537703348572));
#265741=CARTESIAN_POINT('Ctrl Pts',(-155.051444041475,41.6688140489355,
291.537703348572));
#265742=CARTESIAN_POINT('Ctrl Pts',(-150.837754439537,53.5400027769198,
289.537703348572));
#265743=CARTESIAN_POINT('Ctrl Pts',(-146.624064837599,65.411191504904,287.537703348572));
#265744=CARTESIAN_POINT('Ctrl Pts',(-140.605189688823,76.4770599218136,
285.537703348572));
#265745=CARTESIAN_POINT('Ctrl Pts',(-134.586314540048,87.5429283387233,
283.537703348572));
#265746=CARTESIAN_POINT('Ctrl Pts',(-126.9104585261,97.5309980386223,281.537703348572));
#265747=CARTESIAN_POINT('Ctrl Pts',(-119.234602512152,107.519067738521,
279.537703348572));
#265748=CARTESIAN_POINT('Ctrl Pts',(-110.0907706828,116.183399296895,277.537703348572));
#265749=CARTESIAN_POINT('Ctrl Pts',(-100.946938853448,124.847730855269,
275.537703348572));
#265750=CARTESIAN_POINT('Ctrl Pts',(-90.5602826949692,131.974979673883,
273.537703348572));
#265751=CARTESIAN_POINT('Ctrl Pts',(-80.1736265364901,139.102228492497,
271.537703348572));
#265752=CARTESIAN_POINT('Ctrl Pts',(-68.7998999948414,144.516898051454,
269.537703348572));
#265753=CARTESIAN_POINT('Ctrl Pts',(-57.4261734531926,149.931567610412,
267.537703348572));
#265754=CARTESIAN_POINT('Ctrl Pts',(-45.3454354230634,153.500330774912,
265.537703348572));
#265755=CARTESIAN_POINT('Ctrl Pts',(-33.2646973929343,157.069093939413,
263.537703348572));
#265756=CARTESIAN_POINT('Ctrl Pts',(-20.7744157382976,158.704075916301,
261.537703348572));
#265757=CARTESIAN_POINT('Ctrl Pts',(-8.284134083661,160.339057893189,259.537703348572));
#265758=CARTESIAN_POINT('Ctrl Pts',(4.30813900827803,160.,257.537703348572));
#265759=CARTESIAN_POINT('Ctrl Pts',(16.9004121002171,159.660942106811,255.537703348572));
#265760=CARTESIAN_POINT('Ctrl Pts',(29.2846130745762,157.356193074143,253.537703348572));
#265761=CARTESIAN_POINT('Ctrl Pts',(41.6688140489354,155.051444041476,251.537703348572));
#265762=CARTESIAN_POINT('Ctrl Pts',(53.5400027769198,150.837754439537,249.537703348572));
#265763=CARTESIAN_POINT('Ctrl Pts',(65.4111915049041,146.624064837599,247.537703348572));
#265764=CARTESIAN_POINT('Ctrl Pts',(76.4770599218136,140.605189688823,245.537703348572));
#265765=CARTESIAN_POINT('Ctrl Pts',(87.5429283387232,134.586314540048,243.537703348572));
#265766=CARTESIAN_POINT('Ctrl Pts',(97.5309980386223,126.9104585261,241.537703348572));
#265767=CARTESIAN_POINT('Ctrl Pts',(107.519067738521,119.234602512152,239.537703348572));
#265768=CARTESIAN_POINT('Ctrl Pts',(116.183399296895,110.0907706828,237.537703348572));
#265769=CARTESIAN_POINT('Ctrl Pts',(124.847730855269,100.946938853448,235.537703348572));
#265770=CARTESIAN_POINT('Ctrl Pts',(131.974979673883,90.5602826949692,233.537703348572));
#265771=CARTESIAN_POINT('Ctrl Pts',(139.102228492497,80.1736265364902,231.537703348572));
#265772=CARTESIAN_POINT('Ctrl Pts',(144.516898051454,68.7998999948414,229.537703348572));
#265773=CARTESIAN_POINT('Ctrl Pts',(149.931567610412,57.4261734531926,227.537703348572));
#265774=CARTESIAN_POINT('Ctrl Pts',(153.500330774912,45.3454354230634,225.537703348572));
#265775=CARTESIAN_POINT('Ctrl Pts',(157.069093939413,33.2646973929343,223.537703348572));
#265776=CARTESIAN_POINT('Ctrl Pts',(158.704075916301,20.7744157382976,221.537703348572));
#265777=CARTESIAN_POINT('Ctrl Pts',(160.339057893189,8.28413408366101,219.537703348572));
#265778=CARTESIAN_POINT('Ctrl Pts',(160.,-4.30813900827805,217.537703348572));
#265779=CARTESIAN_POINT('Ctrl Pts',(130.,-4.30813900827807,377.537703348572));
#265780=CARTESIAN_POINT('Ctrl Pts',(129.660942106811,-14.5393608954785,
375.537703348572));
#265781=CARTESIAN_POINT('Ctrl Pts',(127.725542856289,-24.5915791233694,
373.537703348572));
#265782=CARTESIAN_POINT('Ctrl Pts',(125.790143605767,-34.6437973512603,
371.537703348572));
#265783=CARTESIAN_POINT('Ctrl Pts',(122.306058950682,-44.2694929456714,
369.537703348572));
#265784=CARTESIAN_POINT('Ctrl Pts',(118.821974295598,-53.8951885400825,
367.537703348572));
#265785=CARTESIAN_POINT('Ctrl Pts',(113.874993963172,-62.8573449296272,
365.537703348572));
#265786=CARTESIAN_POINT('Ctrl Pts',(108.928013630747,-71.819501319172,363.537703348572));
#265787=CARTESIAN_POINT('Ctrl Pts',(102.639948694851,-79.8974404698481,
361.537703348572));
#265788=CARTESIAN_POINT('Ctrl Pts',(96.351883758956,-87.9753796205242,359.537703348572));
#265789=CARTESIAN_POINT('Ctrl Pts',(88.8775672472035,-94.9701958612989,
357.537703348572));
#265790=CARTESIAN_POINT('Ctrl Pts',(81.403250735451,-101.965012102074,355.537703348572));
#265791=CARTESIAN_POINT('Ctrl Pts',(72.9267251261949,-107.704469842635,
353.537703348572));
#265792=CARTESIAN_POINT('Ctrl Pts',(64.4501995169389,-113.443927583196,
351.537703348572));
#265793=CARTESIAN_POINT('Ctrl Pts',(55.1801850026549,-117.786702325803,
349.537703348572));
#265794=CARTESIAN_POINT('Ctrl Pts',(45.910170488371,-122.129477068411,347.537703348572));
#265795=CARTESIAN_POINT('Ctrl Pts',(36.074925591815,-124.968635286058,345.537703348572));
#265796=CARTESIAN_POINT('Ctrl Pts',(26.239680695259,-127.807793503704,343.537703348572));
#265797=CARTESIAN_POINT('Ctrl Pts',(16.0813817870907,-129.073425698447,
341.537703348572));
#265798=CARTESIAN_POINT('Ctrl Pts',(5.92308287892234,-130.339057893189,
339.537703348572));
#265799=CARTESIAN_POINT('Ctrl Pts',(-4.30813900827806,-130.,337.537703348572));
#265800=CARTESIAN_POINT('Ctrl Pts',(-14.5393608954785,-129.660942106811,
335.537703348572));
#265801=CARTESIAN_POINT('Ctrl Pts',(-24.5915791233694,-127.725542856289,
333.537703348572));
#265802=CARTESIAN_POINT('Ctrl Pts',(-34.6437973512603,-125.790143605767,
331.537703348572));
#265803=CARTESIAN_POINT('Ctrl Pts',(-44.2694929456713,-122.306058950682,
329.537703348572));
#265804=CARTESIAN_POINT('Ctrl Pts',(-53.8951885400825,-118.821974295598,
327.537703348572));
#265805=CARTESIAN_POINT('Ctrl Pts',(-62.8573449296272,-113.874993963172,
325.537703348572));
#265806=CARTESIAN_POINT('Ctrl Pts',(-71.819501319172,-108.928013630747,
323.537703348572));
#265807=CARTESIAN_POINT('Ctrl Pts',(-79.8974404698481,-102.639948694851,
321.537703348572));
#265808=CARTESIAN_POINT('Ctrl Pts',(-87.9753796205242,-96.351883758956,
319.537703348572));
#265809=CARTESIAN_POINT('Ctrl Pts',(-94.9701958612989,-88.8775672472035,
317.537703348572));
#265810=CARTESIAN_POINT('Ctrl Pts',(-101.965012102074,-81.403250735451,
315.537703348572));
#265811=CARTESIAN_POINT('Ctrl Pts',(-107.704469842635,-72.9267251261949,
313.537703348572));
#265812=CARTESIAN_POINT('Ctrl Pts',(-113.443927583196,-64.4501995169389,
311.537703348572));
#265813=CARTESIAN_POINT('Ctrl Pts',(-117.786702325803,-55.1801850026549,
309.537703348572));
#265814=CARTESIAN_POINT('Ctrl Pts',(-122.129477068411,-45.910170488371,
307.537703348572));
#265815=CARTESIAN_POINT('Ctrl Pts',(-124.968635286058,-36.074925591815,
305.537703348572));
#265816=CARTESIAN_POINT('Ctrl Pts',(-127.807793503704,-26.239680695259,
303.537703348572));
#265817=CARTESIAN_POINT('Ctrl Pts',(-129.073425698447,-16.0813817870907,
301.537703348572));
#265818=CARTESIAN_POINT('Ctrl Pts',(-130.339057893189,-5.92308287892235,
299.537703348572));
#265819=CARTESIAN_POINT('Ctrl Pts',(-130.,4.30813900827805,297.537703348572));
#265820=CARTESIAN_POINT('Ctrl Pts',(-129.660942106811,14.5393608954784,
295.537703348572));
#265821=CARTESIAN_POINT('Ctrl Pts',(-127.725542856289,24.5915791233693,
293.537703348572));
#265822=CARTESIAN_POINT('Ctrl Pts',(-125.790143605767,34.6437973512602,
291.537703348572));
#265823=CARTESIAN_POINT('Ctrl Pts',(-122.306058950682,44.2694929456713,
289.537703348572));
#265824=CARTESIAN_POINT('Ctrl Pts',(-118.821974295598,53.8951885400825,
287.537703348572));
#265825=CARTESIAN_POINT('Ctrl Pts',(-113.874993963172,62.8573449296272,
285.537703348572));
#265826=CARTESIAN_POINT('Ctrl Pts',(-108.928013630747,71.819501319172,283.537703348572));
#265827=CARTESIAN_POINT('Ctrl Pts',(-102.639948694851,79.8974404698481,
281.537703348572));
#265828=CARTESIAN_POINT('Ctrl Pts',(-96.3518837589561,87.9753796205242,
279.537703348572));
#265829=CARTESIAN_POINT('Ctrl Pts',(-88.8775672472035,94.9701958612989,
277.537703348572));
#265830=CARTESIAN_POINT('Ctrl Pts',(-81.403250735451,101.965012102074,275.537703348572));
#265831=CARTESIAN_POINT('Ctrl Pts',(-72.9267251261949,107.704469842635,
273.537703348572));
#265832=CARTESIAN_POINT('Ctrl Pts',(-64.4501995169389,113.443927583196,
271.537703348572));
#265833=CARTESIAN_POINT('Ctrl Pts',(-55.1801850026549,117.786702325803,
269.537703348572));
#265834=CARTESIAN_POINT('Ctrl Pts',(-45.910170488371,122.129477068411,267.537703348572));
#265835=CARTESIAN_POINT('Ctrl Pts',(-36.074925591815,124.968635286058,265.537703348572));
#265836=CARTESIAN_POINT('Ctrl Pts',(-26.239680695259,127.807793503704,263.537703348572));
#265837=CARTESIAN_POINT('Ctrl Pts',(-16.0813817870907,129.073425698447,
261.537703348572));
#265838=CARTESIAN_POINT('Ctrl Pts',(-5.92308287892242,130.339057893189,
259.537703348572));
#265839=CARTESIAN_POINT('Ctrl Pts',(4.30813900827804,130.,257.537703348572));
#265840=CARTESIAN_POINT('Ctrl Pts',(14.5393608954785,129.660942106811,255.537703348572));
#265841=CARTESIAN_POINT('Ctrl Pts',(24.5915791233693,127.725542856289,253.537703348572));
#265842=CARTESIAN_POINT('Ctrl Pts',(34.6437973512602,125.790143605767,251.537703348572));
#265843=CARTESIAN_POINT('Ctrl Pts',(44.2694929456713,122.306058950682,249.537703348572));
#265844=CARTESIAN_POINT('Ctrl Pts',(53.8951885400825,118.821974295598,247.537703348572));
#265845=CARTESIAN_POINT('Ctrl Pts',(62.8573449296272,113.874993963172,245.537703348572));
#265846=CARTESIAN_POINT('Ctrl Pts',(71.819501319172,108.928013630747,243.537703348572));
#265847=CARTESIAN_POINT('Ctrl Pts',(79.8974404698481,102.639948694851,241.537703348572));
#265848=CARTESIAN_POINT('Ctrl Pts',(87.9753796205242,96.351883758956,239.537703348572));
#265849=CARTESIAN_POINT('Ctrl Pts',(94.9701958612989,88.8775672472035,237.537703348572));
#265850=CARTESIAN_POINT('Ctrl Pts',(101.965012102074,81.403250735451,235.537703348572));
#265851=CARTESIAN_POINT('Ctrl Pts',(107.704469842635,72.926725126195,233.537703348572));
#265852=CARTESIAN_POINT('Ctrl Pts',(113.443927583196,64.4501995169389,231.537703348572));
#265853=CARTESIAN_POINT('Ctrl Pts',(117.786702325803,55.1801850026549,229.537703348572));
#265854=CARTESIAN_POINT('Ctrl Pts',(122.129477068411,45.910170488371,227.537703348572));
#265855=CARTESIAN_POINT('Ctrl Pts',(124.968635286058,36.074925591815,225.537703348572));
#265856=CARTESIAN_POINT('Ctrl Pts',(127.807793503704,26.239680695259,223.537703348572));
#265857=CARTESIAN_POINT('Ctrl Pts',(129.073425698447,16.0813817870907,221.537703348572));
#265858=CARTESIAN_POINT('Ctrl Pts',(130.339057893189,5.92308287892242,219.537703348572));
#265859=CARTESIAN_POINT('Ctrl Pts',(130.,-4.30813900827807,217.537703348572));
#265860=CARTESIAN_POINT('',(146.075461400194,-65.4256802672709,367.5));
#265861=CARTESIAN_POINT('',(145.,-4.30813900827806,377.537703348572));
#265862=CARTESIAN_POINT('Origin',(160.,3.64291929955129E-14,375.));
#265863=CARTESIAN_POINT('Origin',(-160.,-160.339057893189,367.5));
#265864=CARTESIAN_POINT('Ctrl Pts',(-130.,4.30813900827773,377.537703348572));
#265865=CARTESIAN_POINT('Ctrl Pts',(-129.660942106811,14.5393608954781,
375.537703348572));
#265866=CARTESIAN_POINT('Ctrl Pts',(-127.725542856289,24.591579123369,373.537703348572));
#265867=CARTESIAN_POINT('Ctrl Pts',(-125.790143605767,34.6437973512599,
371.537703348572));
#265868=CARTESIAN_POINT('Ctrl Pts',(-122.306058950683,44.269492945671,369.537703348572));
#265869=CARTESIAN_POINT('Ctrl Pts',(-118.821974295598,53.8951885400822,
367.537703348572));
#265870=CARTESIAN_POINT('Ctrl Pts',(-113.874993963172,62.8573449296269,
365.537703348572));
#265871=CARTESIAN_POINT('Ctrl Pts',(-108.928013630747,71.8195013191717,
363.537703348572));
#265872=CARTESIAN_POINT('Ctrl Pts',(-102.639948694852,79.8974404698478,
361.537703348572));
#265873=CARTESIAN_POINT('Ctrl Pts',(-96.3518837589562,87.9753796205239,
359.537703348572));
#265874=CARTESIAN_POINT('Ctrl Pts',(-88.8775672472037,94.9701958612987,
357.537703348572));
#265875=CARTESIAN_POINT('Ctrl Pts',(-81.4032507354512,101.965012102073,
355.537703348572));
#265876=CARTESIAN_POINT('Ctrl Pts',(-72.9267251261952,107.704469842635,
353.537703348572));
#265877=CARTESIAN_POINT('Ctrl Pts',(-64.4501995169392,113.443927583196,
351.537703348572));
#265878=CARTESIAN_POINT('Ctrl Pts',(-55.1801850026552,117.786702325803,
349.537703348572));
#265879=CARTESIAN_POINT('Ctrl Pts',(-45.9101704883713,122.12947706841,347.537703348572));
#265880=CARTESIAN_POINT('Ctrl Pts',(-36.0749255918153,124.968635286057,
345.537703348572));
#265881=CARTESIAN_POINT('Ctrl Pts',(-26.2396806952593,127.807793503704,
343.537703348572));
#265882=CARTESIAN_POINT('Ctrl Pts',(-16.081381787091,129.073425698447,341.537703348572));
#265883=CARTESIAN_POINT('Ctrl Pts',(-5.92308287892268,130.339057893189,
339.537703348572));
#265884=CARTESIAN_POINT('Ctrl Pts',(4.30813900827772,130.,337.537703348572));
#265885=CARTESIAN_POINT('Ctrl Pts',(14.5393608954781,129.660942106811,335.537703348572));
#265886=CARTESIAN_POINT('Ctrl Pts',(24.591579123369,127.725542856289,333.537703348572));
#265887=CARTESIAN_POINT('Ctrl Pts',(34.6437973512599,125.790143605767,331.537703348572));
#265888=CARTESIAN_POINT('Ctrl Pts',(44.269492945671,122.306058950683,329.537703348572));
#265889=CARTESIAN_POINT('Ctrl Pts',(53.8951885400822,118.821974295598,327.537703348572));
#265890=CARTESIAN_POINT('Ctrl Pts',(62.8573449296269,113.874993963172,325.537703348572));
#265891=CARTESIAN_POINT('Ctrl Pts',(71.8195013191717,108.928013630747,323.537703348572));
#265892=CARTESIAN_POINT('Ctrl Pts',(79.8974404698478,102.639948694852,321.537703348572));
#265893=CARTESIAN_POINT('Ctrl Pts',(87.9753796205239,96.3518837589562,319.537703348572));
#265894=CARTESIAN_POINT('Ctrl Pts',(94.9701958612986,88.8775672472037,317.537703348572));
#265895=CARTESIAN_POINT('Ctrl Pts',(101.965012102073,81.4032507354512,315.537703348572));
#265896=CARTESIAN_POINT('Ctrl Pts',(107.704469842635,72.9267251261952,313.537703348572));
#265897=CARTESIAN_POINT('Ctrl Pts',(113.443927583196,64.4501995169392,311.537703348572));
#265898=CARTESIAN_POINT('Ctrl Pts',(117.786702325803,55.1801850026552,309.537703348572));
#265899=CARTESIAN_POINT('Ctrl Pts',(122.12947706841,45.9101704883713,307.537703348572));
#265900=CARTESIAN_POINT('Ctrl Pts',(124.968635286057,36.0749255918153,305.537703348572));
#265901=CARTESIAN_POINT('Ctrl Pts',(127.807793503704,26.2396806952593,303.537703348572));
#265902=CARTESIAN_POINT('Ctrl Pts',(129.073425698447,16.081381787091,301.537703348572));
#265903=CARTESIAN_POINT('Ctrl Pts',(130.339057893189,5.92308287892268,299.537703348572));
#265904=CARTESIAN_POINT('Ctrl Pts',(130.,-4.30813900827772,297.537703348572));
#265905=CARTESIAN_POINT('Ctrl Pts',(129.660942106811,-14.5393608954781,
295.537703348572));
#265906=CARTESIAN_POINT('Ctrl Pts',(127.725542856289,-24.591579123369,293.537703348572));
#265907=CARTESIAN_POINT('Ctrl Pts',(125.790143605767,-34.6437973512599,
291.537703348572));
#265908=CARTESIAN_POINT('Ctrl Pts',(122.306058950683,-44.269492945671,289.537703348572));
#265909=CARTESIAN_POINT('Ctrl Pts',(118.821974295598,-53.8951885400822,
287.537703348572));
#265910=CARTESIAN_POINT('Ctrl Pts',(113.874993963172,-62.8573449296269,
285.537703348572));
#265911=CARTESIAN_POINT('Ctrl Pts',(108.928013630747,-71.8195013191717,
283.537703348572));
#265912=CARTESIAN_POINT('Ctrl Pts',(102.639948694852,-79.8974404698478,
281.537703348572));
#265913=CARTESIAN_POINT('Ctrl Pts',(96.3518837589563,-87.9753796205239,
279.537703348572));
#265914=CARTESIAN_POINT('Ctrl Pts',(88.8775672472037,-94.9701958612986,
277.537703348572));
#265915=CARTESIAN_POINT('Ctrl Pts',(81.4032507354513,-101.965012102073,
275.537703348572));
#265916=CARTESIAN_POINT('Ctrl Pts',(72.9267251261952,-107.704469842635,
273.537703348572));
#265917=CARTESIAN_POINT('Ctrl Pts',(64.4501995169392,-113.443927583196,
271.537703348572));
#265918=CARTESIAN_POINT('Ctrl Pts',(55.1801850026552,-117.786702325803,
269.537703348572));
#265919=CARTESIAN_POINT('Ctrl Pts',(45.9101704883713,-122.12947706841,267.537703348572));
#265920=CARTESIAN_POINT('Ctrl Pts',(36.0749255918153,-124.968635286057,
265.537703348572));
#265921=CARTESIAN_POINT('Ctrl Pts',(26.2396806952593,-127.807793503704,
263.537703348572));
#265922=CARTESIAN_POINT('Ctrl Pts',(16.081381787091,-129.073425698447,261.537703348572));
#265923=CARTESIAN_POINT('Ctrl Pts',(5.92308287892275,-130.339057893189,
259.537703348572));
#265924=CARTESIAN_POINT('Ctrl Pts',(-4.30813900827771,-130.,257.537703348572));
#265925=CARTESIAN_POINT('Ctrl Pts',(-14.5393608954782,-129.660942106811,
255.537703348572));
#265926=CARTESIAN_POINT('Ctrl Pts',(-24.591579123369,-127.725542856289,
253.537703348572));
#265927=CARTESIAN_POINT('Ctrl Pts',(-34.6437973512598,-125.790143605767,
251.537703348572));
#265928=CARTESIAN_POINT('Ctrl Pts',(-44.269492945671,-122.306058950683,
249.537703348572));
#265929=CARTESIAN_POINT('Ctrl Pts',(-53.8951885400822,-118.821974295598,
247.537703348572));
#265930=CARTESIAN_POINT('Ctrl Pts',(-62.8573449296269,-113.874993963172,
245.537703348572));
#265931=CARTESIAN_POINT('Ctrl Pts',(-71.8195013191717,-108.928013630747,
243.537703348572));
#265932=CARTESIAN_POINT('Ctrl Pts',(-79.8974404698478,-102.639948694852,
241.537703348572));
#265933=CARTESIAN_POINT('Ctrl Pts',(-87.975379620524,-96.3518837589562,
239.537703348572));
#265934=CARTESIAN_POINT('Ctrl Pts',(-94.9701958612986,-88.8775672472037,
237.537703348572));
#265935=CARTESIAN_POINT('Ctrl Pts',(-101.965012102073,-81.4032507354513,
235.537703348572));
#265936=CARTESIAN_POINT('Ctrl Pts',(-107.704469842635,-72.9267251261952,
233.537703348572));
#265937=CARTESIAN_POINT('Ctrl Pts',(-113.443927583196,-64.4501995169392,
231.537703348572));
#265938=CARTESIAN_POINT('Ctrl Pts',(-117.786702325803,-55.1801850026553,
229.537703348572));
#265939=CARTESIAN_POINT('Ctrl Pts',(-122.12947706841,-45.9101704883713,
227.537703348572));
#265940=CARTESIAN_POINT('Ctrl Pts',(-124.968635286057,-36.0749255918153,
225.537703348572));
#265941=CARTESIAN_POINT('Ctrl Pts',(-127.807793503704,-26.2396806952593,
223.537703348572));
#265942=CARTESIAN_POINT('Ctrl Pts',(-129.073425698447,-16.081381787091,
221.537703348572));
#265943=CARTESIAN_POINT('Ctrl Pts',(-130.339057893189,-5.92308287892275,
219.537703348572));
#265944=CARTESIAN_POINT('Ctrl Pts',(-130.,4.30813900827773,217.537703348572));
#265945=CARTESIAN_POINT('Ctrl Pts',(-130.,-4.30813900827845,372.462296651428));
#265946=CARTESIAN_POINT('Ctrl Pts',(-130.339057893189,5.92308287892195,
370.462296651428));
#265947=CARTESIAN_POINT('Ctrl Pts',(-129.073425698447,16.0813817870903,
368.462296651429));
#265948=CARTESIAN_POINT('Ctrl Pts',(-127.807793503705,26.2396806952586,
366.462296651429));
#265949=CARTESIAN_POINT('Ctrl Pts',(-124.968635286058,36.0749255918146,
364.462296651428));
#265950=CARTESIAN_POINT('Ctrl Pts',(-122.129477068411,45.9101704883706,
362.462296651428));
#265951=CARTESIAN_POINT('Ctrl Pts',(-117.786702325804,55.1801850026546,
360.462296651428));
#265952=CARTESIAN_POINT('Ctrl Pts',(-113.443927583196,64.4501995169386,
358.462296651428));
#265953=CARTESIAN_POINT('Ctrl Pts',(-107.704469842635,72.9267251261946,
356.462296651428));
#265954=CARTESIAN_POINT('Ctrl Pts',(-101.965012102074,81.4032507354507,
354.462296651428));
#265955=CARTESIAN_POINT('Ctrl Pts',(-94.9701958612992,88.8775672472032,
352.462296651428));
#265956=CARTESIAN_POINT('Ctrl Pts',(-87.9753796205245,96.3518837589558,
350.462296651428));
#265957=CARTESIAN_POINT('Ctrl Pts',(-79.8974404698484,102.639948694851,
348.462296651428));
#265958=CARTESIAN_POINT('Ctrl Pts',(-71.8195013191724,108.928013630747,
346.462296651428));
#265959=CARTESIAN_POINT('Ctrl Pts',(-62.8573449296276,113.874993963172,
344.462296651428));
#265960=CARTESIAN_POINT('Ctrl Pts',(-53.8951885400828,118.821974295598,
342.462296651428));
#265961=CARTESIAN_POINT('Ctrl Pts',(-44.2694929456717,122.306058950682,
340.462296651428));
#265962=CARTESIAN_POINT('Ctrl Pts',(-34.6437973512606,125.790143605767,
338.462296651428));
#265963=CARTESIAN_POINT('Ctrl Pts',(-24.5915791233697,127.725542856289,
336.462296651428));
#265964=CARTESIAN_POINT('Ctrl Pts',(-14.5393608954789,129.660942106811,
334.462296651428));
#265965=CARTESIAN_POINT('Ctrl Pts',(-4.30813900827846,130.,332.462296651428));
#265966=CARTESIAN_POINT('Ctrl Pts',(5.92308287892194,130.339057893189,330.462296651429));
#265967=CARTESIAN_POINT('Ctrl Pts',(16.0813817870903,129.073425698447,328.462296651428));
#265968=CARTESIAN_POINT('Ctrl Pts',(26.2396806952586,127.807793503705,326.462296651428));
#265969=CARTESIAN_POINT('Ctrl Pts',(36.0749255918146,124.968635286058,324.462296651428));
#265970=CARTESIAN_POINT('Ctrl Pts',(45.9101704883706,122.129477068411,322.462296651428));
#265971=CARTESIAN_POINT('Ctrl Pts',(55.1801850026546,117.786702325804,320.462296651428));
#265972=CARTESIAN_POINT('Ctrl Pts',(64.4501995169386,113.443927583196,318.462296651428));
#265973=CARTESIAN_POINT('Ctrl Pts',(72.9267251261946,107.704469842635,316.462296651428));
#265974=CARTESIAN_POINT('Ctrl Pts',(81.4032507354506,101.965012102074,314.462296651428));
#265975=CARTESIAN_POINT('Ctrl Pts',(88.8775672472032,94.9701958612992,312.462296651428));
#265976=CARTESIAN_POINT('Ctrl Pts',(96.3518837589558,87.9753796205245,310.462296651428));
#265977=CARTESIAN_POINT('Ctrl Pts',(102.639948694851,79.8974404698484,308.462296651428));
#265978=CARTESIAN_POINT('Ctrl Pts',(108.928013630747,71.8195013191724,306.462296651428));
#265979=CARTESIAN_POINT('Ctrl Pts',(113.874993963172,62.8573449296276,304.462296651428));
#265980=CARTESIAN_POINT('Ctrl Pts',(118.821974295598,53.8951885400829,302.462296651428));
#265981=CARTESIAN_POINT('Ctrl Pts',(122.306058950682,44.2694929456717,300.462296651428));
#265982=CARTESIAN_POINT('Ctrl Pts',(125.790143605767,34.6437973512606,298.462296651428));
#265983=CARTESIAN_POINT('Ctrl Pts',(127.725542856289,24.5915791233698,296.462296651428));
#265984=CARTESIAN_POINT('Ctrl Pts',(129.660942106811,14.5393608954789,294.462296651429));
#265985=CARTESIAN_POINT('Ctrl Pts',(130.,4.30813900827846,292.462296651428));
#265986=CARTESIAN_POINT('Ctrl Pts',(130.339057893189,-5.92308287892194,
290.462296651428));
#265987=CARTESIAN_POINT('Ctrl Pts',(129.073425698447,-16.0813817870903,
288.462296651428));
#265988=CARTESIAN_POINT('Ctrl Pts',(127.807793503705,-26.2396806952586,
286.462296651428));
#265989=CARTESIAN_POINT('Ctrl Pts',(124.968635286058,-36.0749255918146,
284.462296651428));
#265990=CARTESIAN_POINT('Ctrl Pts',(122.129477068411,-45.9101704883706,
282.462296651428));
#265991=CARTESIAN_POINT('Ctrl Pts',(117.786702325804,-55.1801850026546,
280.462296651428));
#265992=CARTESIAN_POINT('Ctrl Pts',(113.443927583196,-64.4501995169386,
278.462296651428));
#265993=CARTESIAN_POINT('Ctrl Pts',(107.704469842635,-72.9267251261946,
276.462296651428));
#265994=CARTESIAN_POINT('Ctrl Pts',(101.965012102074,-81.4032507354506,
274.462296651428));
#265995=CARTESIAN_POINT('Ctrl Pts',(94.9701958612992,-88.8775672472032,
272.462296651428));
#265996=CARTESIAN_POINT('Ctrl Pts',(87.9753796205246,-96.3518837589557,
270.462296651428));
#265997=CARTESIAN_POINT('Ctrl Pts',(79.8974404698484,-102.639948694851,
268.462296651428));
#265998=CARTESIAN_POINT('Ctrl Pts',(71.8195013191723,-108.928013630747,
266.462296651428));
#265999=CARTESIAN_POINT('Ctrl Pts',(62.8573449296276,-113.874993963172,
264.462296651428));
#266000=CARTESIAN_POINT('Ctrl Pts',(53.8951885400829,-118.821974295598,
262.462296651428));
#266001=CARTESIAN_POINT('Ctrl Pts',(44.2694929456717,-122.306058950682,
260.462296651428));
#266002=CARTESIAN_POINT('Ctrl Pts',(34.6437973512606,-125.790143605767,
258.462296651428));
#266003=CARTESIAN_POINT('Ctrl Pts',(24.5915791233698,-127.725542856289,
256.462296651428));
#266004=CARTESIAN_POINT('Ctrl Pts',(14.5393608954789,-129.660942106811,
254.462296651428));
#266005=CARTESIAN_POINT('Ctrl Pts',(4.30813900827847,-130.,252.462296651428));
#266006=CARTESIAN_POINT('Ctrl Pts',(-5.92308287892199,-130.339057893189,
250.462296651428));
#266007=CARTESIAN_POINT('Ctrl Pts',(-16.0813817870903,-129.073425698447,
248.462296651428));
#266008=CARTESIAN_POINT('Ctrl Pts',(-26.2396806952585,-127.807793503705,
246.462296651428));
#266009=CARTESIAN_POINT('Ctrl Pts',(-36.0749255918146,-124.968635286058,
244.462296651428));
#266010=CARTESIAN_POINT('Ctrl Pts',(-45.9101704883706,-122.129477068411,
242.462296651428));
#266011=CARTESIAN_POINT('Ctrl Pts',(-55.1801850026546,-117.786702325804,
240.462296651428));
#266012=CARTESIAN_POINT('Ctrl Pts',(-64.4501995169385,-113.443927583197,
238.462296651429));
#266013=CARTESIAN_POINT('Ctrl Pts',(-72.9267251261946,-107.704469842635,
236.462296651428));
#266014=CARTESIAN_POINT('Ctrl Pts',(-81.4032507354507,-101.965012102074,
234.462296651428));
#266015=CARTESIAN_POINT('Ctrl Pts',(-88.8775672472032,-94.9701958612992,
232.462296651428));
#266016=CARTESIAN_POINT('Ctrl Pts',(-96.3518837589557,-87.9753796205246,
230.462296651428));
#266017=CARTESIAN_POINT('Ctrl Pts',(-102.639948694851,-79.8974404698484,
228.462296651428));
#266018=CARTESIAN_POINT('Ctrl Pts',(-108.928013630747,-71.8195013191723,
226.462296651428));
#266019=CARTESIAN_POINT('Ctrl Pts',(-113.874993963172,-62.8573449296276,
224.462296651428));
#266020=CARTESIAN_POINT('Ctrl Pts',(-118.821974295598,-53.8951885400829,
222.462296651428));
#266021=CARTESIAN_POINT('Ctrl Pts',(-122.306058950682,-44.2694929456718,
220.462296651428));
#266022=CARTESIAN_POINT('Ctrl Pts',(-125.790143605767,-34.6437973512606,
218.462296651428));
#266023=CARTESIAN_POINT('Ctrl Pts',(-127.725542856289,-24.5915791233698,
216.462296651428));
#266024=CARTESIAN_POINT('Ctrl Pts',(-129.660942106811,-14.5393608954789,
214.462296651428));
#266025=CARTESIAN_POINT('Ctrl Pts',(-130.,-4.30813900827845,212.462296651428));
#266026=CARTESIAN_POINT('',(-118.376086385729,53.9041949546877,367.5));
#266027=CARTESIAN_POINT('',(-128.373075022505,20.9502666088252,367.5));
#266028=CARTESIAN_POINT('Ctrl Pts',(-118.376086385729,53.9041949546877,
367.5));
#266029=CARTESIAN_POINT('Ctrl Pts',(-119.546342407814,51.276867586874,367.5));
#266030=CARTESIAN_POINT('Ctrl Pts',(-120.634616850713,48.6137313363238,
367.499999999997));
#266031=CARTESIAN_POINT('Ctrl Pts',(-122.645087654721,43.2205933565672,
367.499999999997));
#266032=CARTESIAN_POINT('Ctrl Pts',(-123.566638088337,40.491727202324,367.5));
#266033=CARTESIAN_POINT('Ctrl Pts',(-126.073121396906,32.2286687868899,
367.5));
#266034=CARTESIAN_POINT('Ctrl Pts',(-127.399213018598,26.6223327935032,
367.5));
#266035=CARTESIAN_POINT('Ctrl Pts',(-128.373075022505,20.9502666088252,
367.5));
#266036=CARTESIAN_POINT('',(-130.,4.30813900827773,377.537703348572));
#266037=CARTESIAN_POINT('Ctrl Pts',(-130.,4.30813900827773,377.537703348572));
#266038=CARTESIAN_POINT('Ctrl Pts',(-129.660942106811,14.5393608954781,
375.537703348572));
#266039=CARTESIAN_POINT('Ctrl Pts',(-127.725542856289,24.591579123369,373.537703348572));
#266040=CARTESIAN_POINT('Ctrl Pts',(-125.790143605767,34.6437973512599,
371.537703348572));
#266041=CARTESIAN_POINT('Ctrl Pts',(-122.306058950683,44.269492945671,369.537703348572));
#266042=CARTESIAN_POINT('Ctrl Pts',(-120.533915146556,49.1655039490626,
368.520423931127));
#266043=CARTESIAN_POINT('Ctrl Pts',(-118.376086385729,53.9041949546877,
367.5));
#266044=CARTESIAN_POINT('',(-130.,-4.30813900827845,372.462296651428));
#266045=CARTESIAN_POINT('',(-130.,-3.57353036051222E-13,375.));
#266046=CARTESIAN_POINT('Ctrl Pts',(-130.,-4.30813900827845,372.462296651428));
#266047=CARTESIAN_POINT('Ctrl Pts',(-130.339057893189,5.92308287892196,
370.462296651428));
#266048=CARTESIAN_POINT('Ctrl Pts',(-129.073425698447,16.0813817870903,
368.462296651429));
#266049=CARTESIAN_POINT('Ctrl Pts',(-128.769291070567,18.5224467909361,
367.981691576521));
#266050=CARTESIAN_POINT('Ctrl Pts',(-128.373075022505,20.9502666088252,
367.5));
#266051=CARTESIAN_POINT('Ctrl Pts',(-160.,4.30813900827767,377.537703348572));
#266052=CARTESIAN_POINT('Ctrl Pts',(-159.660942106811,16.9004121002166,
375.537703348572));
#266053=CARTESIAN_POINT('Ctrl Pts',(-157.356193074143,29.2846130745759,
373.537703348572));
#266054=CARTESIAN_POINT('Ctrl Pts',(-155.051444041476,41.6688140489352,
371.537703348572));
#266055=CARTESIAN_POINT('Ctrl Pts',(-150.837754439537,53.5400027769194,
369.537703348572));
#266056=CARTESIAN_POINT('Ctrl Pts',(-146.624064837599,65.4111915049037,
367.537703348572));
#266057=CARTESIAN_POINT('Ctrl Pts',(-140.605189688823,76.4770599218133,
365.537703348572));
#266058=CARTESIAN_POINT('Ctrl Pts',(-134.586314540048,87.542928338723,363.537703348572));
#266059=CARTESIAN_POINT('Ctrl Pts',(-126.9104585261,97.530998038622,361.537703348572));
#266060=CARTESIAN_POINT('Ctrl Pts',(-119.234602512152,107.519067738521,
359.537703348572));
#266061=CARTESIAN_POINT('Ctrl Pts',(-110.0907706828,116.183399296895,357.537703348572));
#266062=CARTESIAN_POINT('Ctrl Pts',(-100.946938853448,124.847730855269,
355.537703348572));
#266063=CARTESIAN_POINT('Ctrl Pts',(-90.5602826949695,131.974979673883,
353.537703348572));
#266064=CARTESIAN_POINT('Ctrl Pts',(-80.1736265364906,139.102228492497,
351.537703348572));
#266065=CARTESIAN_POINT('Ctrl Pts',(-68.7998999948417,144.516898051454,
349.537703348572));
#266066=CARTESIAN_POINT('Ctrl Pts',(-57.4261734531929,149.931567610411,
347.537703348572));
#266067=CARTESIAN_POINT('Ctrl Pts',(-45.3454354230638,153.500330774912,
345.537703348572));
#266068=CARTESIAN_POINT('Ctrl Pts',(-33.2646973929347,157.069093939413,
343.537703348572));
#266069=CARTESIAN_POINT('Ctrl Pts',(-20.774415738298,158.704075916301,341.537703348572));
#266070=CARTESIAN_POINT('Ctrl Pts',(-8.28413408366129,160.339057893189,
339.537703348572));
#266071=CARTESIAN_POINT('Ctrl Pts',(4.30813900827766,160.,337.537703348572));
#266072=CARTESIAN_POINT('Ctrl Pts',(16.9004121002166,159.660942106811,335.537703348572));
#266073=CARTESIAN_POINT('Ctrl Pts',(29.2846130745759,157.356193074143,333.537703348572));
#266074=CARTESIAN_POINT('Ctrl Pts',(41.6688140489352,155.051444041476,331.537703348572));
#266075=CARTESIAN_POINT('Ctrl Pts',(53.5400027769194,150.837754439537,329.537703348572));
#266076=CARTESIAN_POINT('Ctrl Pts',(65.4111915049037,146.624064837599,327.537703348572));
#266077=CARTESIAN_POINT('Ctrl Pts',(76.4770599218133,140.605189688823,325.537703348572));
#266078=CARTESIAN_POINT('Ctrl Pts',(87.542928338723,134.586314540048,323.537703348572));
#266079=CARTESIAN_POINT('Ctrl Pts',(97.530998038622,126.9104585261,321.537703348572));
#266080=CARTESIAN_POINT('Ctrl Pts',(107.519067738521,119.234602512152,319.537703348572));
#266081=CARTESIAN_POINT('Ctrl Pts',(116.183399296895,110.0907706828,317.537703348572));
#266082=CARTESIAN_POINT('Ctrl Pts',(124.847730855269,100.946938853448,315.537703348572));
#266083=CARTESIAN_POINT('Ctrl Pts',(131.974979673883,90.5602826949695,313.537703348572));
#266084=CARTESIAN_POINT('Ctrl Pts',(139.102228492497,80.1736265364906,311.537703348572));
#266085=CARTESIAN_POINT('Ctrl Pts',(144.516898051454,68.7998999948417,309.537703348572));
#266086=CARTESIAN_POINT('Ctrl Pts',(149.931567610411,57.4261734531929,307.537703348572));
#266087=CARTESIAN_POINT('Ctrl Pts',(153.500330774912,45.3454354230638,305.537703348572));
#266088=CARTESIAN_POINT('Ctrl Pts',(157.069093939413,33.2646973929347,303.537703348572));
#266089=CARTESIAN_POINT('Ctrl Pts',(158.704075916301,20.774415738298,301.537703348572));
#266090=CARTESIAN_POINT('Ctrl Pts',(160.339057893189,8.28413408366131,299.537703348572));
#266091=CARTESIAN_POINT('Ctrl Pts',(160.,-4.30813900827765,297.537703348572));
#266092=CARTESIAN_POINT('Ctrl Pts',(159.660942106811,-16.9004121002166,
295.537703348572));
#266093=CARTESIAN_POINT('Ctrl Pts',(157.356193074143,-29.2846130745759,
293.537703348572));
#266094=CARTESIAN_POINT('Ctrl Pts',(155.051444041476,-41.6688140489352,
291.537703348572));
#266095=CARTESIAN_POINT('Ctrl Pts',(150.837754439537,-53.5400027769194,
289.537703348572));
#266096=CARTESIAN_POINT('Ctrl Pts',(146.624064837599,-65.4111915049036,
287.537703348572));
#266097=CARTESIAN_POINT('Ctrl Pts',(140.605189688823,-76.4770599218133,
285.537703348572));
#266098=CARTESIAN_POINT('Ctrl Pts',(134.586314540048,-87.5429283387229,
283.537703348572));
#266099=CARTESIAN_POINT('Ctrl Pts',(126.9104585261,-97.530998038622,281.537703348572));
#266100=CARTESIAN_POINT('Ctrl Pts',(119.234602512152,-107.519067738521,
279.537703348572));
#266101=CARTESIAN_POINT('Ctrl Pts',(110.0907706828,-116.183399296895,277.537703348572));
#266102=CARTESIAN_POINT('Ctrl Pts',(100.946938853448,-124.847730855269,
275.537703348572));
#266103=CARTESIAN_POINT('Ctrl Pts',(90.5602826949695,-131.974979673883,
273.537703348572));
#266104=CARTESIAN_POINT('Ctrl Pts',(80.1736265364905,-139.102228492497,
271.537703348572));
#266105=CARTESIAN_POINT('Ctrl Pts',(68.7998999948417,-144.516898051454,
269.537703348572));
#266106=CARTESIAN_POINT('Ctrl Pts',(57.426173453193,-149.931567610411,267.537703348572));
#266107=CARTESIAN_POINT('Ctrl Pts',(45.3454354230638,-153.500330774912,
265.537703348572));
#266108=CARTESIAN_POINT('Ctrl Pts',(33.2646973929347,-157.069093939413,
263.537703348572));
#266109=CARTESIAN_POINT('Ctrl Pts',(20.774415738298,-158.704075916301,261.537703348572));
#266110=CARTESIAN_POINT('Ctrl Pts',(8.28413408366139,-160.339057893189,
259.537703348572));
#266111=CARTESIAN_POINT('Ctrl Pts',(-4.30813900827764,-160.,257.537703348572));
#266112=CARTESIAN_POINT('Ctrl Pts',(-16.9004121002167,-159.660942106811,
255.537703348572));
#266113=CARTESIAN_POINT('Ctrl Pts',(-29.2846130745759,-157.356193074143,
253.537703348572));
#266114=CARTESIAN_POINT('Ctrl Pts',(-41.6688140489351,-155.051444041476,
251.537703348572));
#266115=CARTESIAN_POINT('Ctrl Pts',(-53.5400027769194,-150.837754439537,
249.537703348572));
#266116=CARTESIAN_POINT('Ctrl Pts',(-65.4111915049037,-146.624064837599,
247.537703348572));
#266117=CARTESIAN_POINT('Ctrl Pts',(-76.4770599218133,-140.605189688823,
245.537703348572));
#266118=CARTESIAN_POINT('Ctrl Pts',(-87.5429283387229,-134.586314540048,
243.537703348572));
#266119=CARTESIAN_POINT('Ctrl Pts',(-97.530998038622,-126.9104585261,241.537703348572));
#266120=CARTESIAN_POINT('Ctrl Pts',(-107.519067738521,-119.234602512152,
239.537703348572));
#266121=CARTESIAN_POINT('Ctrl Pts',(-116.183399296895,-110.0907706828,237.537703348572));
#266122=CARTESIAN_POINT('Ctrl Pts',(-124.847730855269,-100.946938853448,
235.537703348572));
#266123=CARTESIAN_POINT('Ctrl Pts',(-131.974979673883,-90.5602826949695,
233.537703348572));
#266124=CARTESIAN_POINT('Ctrl Pts',(-139.102228492497,-80.1736265364905,
231.537703348572));
#266125=CARTESIAN_POINT('Ctrl Pts',(-144.516898051454,-68.7998999948417,
229.537703348572));
#266126=CARTESIAN_POINT('Ctrl Pts',(-149.931567610411,-57.426173453193,
227.537703348572));
#266127=CARTESIAN_POINT('Ctrl Pts',(-153.500330774912,-45.3454354230638,
225.537703348572));
#266128=CARTESIAN_POINT('Ctrl Pts',(-157.069093939413,-33.2646973929347,
223.537703348572));
#266129=CARTESIAN_POINT('Ctrl Pts',(-158.704075916301,-20.774415738298,
221.537703348572));
#266130=CARTESIAN_POINT('Ctrl Pts',(-160.339057893189,-8.2841340836614,
219.537703348572));
#266131=CARTESIAN_POINT('Ctrl Pts',(-160.,4.30813900827767,217.537703348572));
#266132=CARTESIAN_POINT('Ctrl Pts',(-130.,4.30813900827773,377.537703348572));
#266133=CARTESIAN_POINT('Ctrl Pts',(-129.660942106811,14.5393608954781,
375.537703348572));
#266134=CARTESIAN_POINT('Ctrl Pts',(-127.725542856289,24.591579123369,373.537703348572));
#266135=CARTESIAN_POINT('Ctrl Pts',(-125.790143605767,34.6437973512599,
371.537703348572));
#266136=CARTESIAN_POINT('Ctrl Pts',(-122.306058950683,44.269492945671,369.537703348572));
#266137=CARTESIAN_POINT('Ctrl Pts',(-118.821974295598,53.8951885400822,
367.537703348572));
#266138=CARTESIAN_POINT('Ctrl Pts',(-113.874993963172,62.8573449296269,
365.537703348572));
#266139=CARTESIAN_POINT('Ctrl Pts',(-108.928013630747,71.8195013191717,
363.537703348572));
#266140=CARTESIAN_POINT('Ctrl Pts',(-102.639948694852,79.8974404698478,
361.537703348572));
#266141=CARTESIAN_POINT('Ctrl Pts',(-96.3518837589562,87.9753796205239,
359.537703348572));
#266142=CARTESIAN_POINT('Ctrl Pts',(-88.8775672472037,94.9701958612987,
357.537703348572));
#266143=CARTESIAN_POINT('Ctrl Pts',(-81.4032507354512,101.965012102073,
355.537703348572));
#266144=CARTESIAN_POINT('Ctrl Pts',(-72.9267251261952,107.704469842635,
353.537703348572));
#266145=CARTESIAN_POINT('Ctrl Pts',(-64.4501995169392,113.443927583196,
351.537703348572));
#266146=CARTESIAN_POINT('Ctrl Pts',(-55.1801850026552,117.786702325803,
349.537703348572));
#266147=CARTESIAN_POINT('Ctrl Pts',(-45.9101704883713,122.12947706841,347.537703348572));
#266148=CARTESIAN_POINT('Ctrl Pts',(-36.0749255918153,124.968635286057,
345.537703348572));
#266149=CARTESIAN_POINT('Ctrl Pts',(-26.2396806952593,127.807793503704,
343.537703348572));
#266150=CARTESIAN_POINT('Ctrl Pts',(-16.081381787091,129.073425698447,341.537703348572));
#266151=CARTESIAN_POINT('Ctrl Pts',(-5.92308287892268,130.339057893189,
339.537703348572));
#266152=CARTESIAN_POINT('Ctrl Pts',(4.30813900827772,130.,337.537703348572));
#266153=CARTESIAN_POINT('Ctrl Pts',(14.5393608954781,129.660942106811,335.537703348572));
#266154=CARTESIAN_POINT('Ctrl Pts',(24.591579123369,127.725542856289,333.537703348572));
#266155=CARTESIAN_POINT('Ctrl Pts',(34.6437973512599,125.790143605767,331.537703348572));
#266156=CARTESIAN_POINT('Ctrl Pts',(44.269492945671,122.306058950683,329.537703348572));
#266157=CARTESIAN_POINT('Ctrl Pts',(53.8951885400822,118.821974295598,327.537703348572));
#266158=CARTESIAN_POINT('Ctrl Pts',(62.8573449296269,113.874993963172,325.537703348572));
#266159=CARTESIAN_POINT('Ctrl Pts',(71.8195013191717,108.928013630747,323.537703348572));
#266160=CARTESIAN_POINT('Ctrl Pts',(79.8974404698478,102.639948694852,321.537703348572));
#266161=CARTESIAN_POINT('Ctrl Pts',(87.9753796205239,96.3518837589562,319.537703348572));
#266162=CARTESIAN_POINT('Ctrl Pts',(94.9701958612986,88.8775672472037,317.537703348572));
#266163=CARTESIAN_POINT('Ctrl Pts',(101.965012102073,81.4032507354512,315.537703348572));
#266164=CARTESIAN_POINT('Ctrl Pts',(107.704469842635,72.9267251261952,313.537703348572));
#266165=CARTESIAN_POINT('Ctrl Pts',(113.443927583196,64.4501995169392,311.537703348572));
#266166=CARTESIAN_POINT('Ctrl Pts',(117.786702325803,55.1801850026552,309.537703348572));
#266167=CARTESIAN_POINT('Ctrl Pts',(122.12947706841,45.9101704883713,307.537703348572));
#266168=CARTESIAN_POINT('Ctrl Pts',(124.968635286057,36.0749255918153,305.537703348572));
#266169=CARTESIAN_POINT('Ctrl Pts',(127.807793503704,26.2396806952593,303.537703348572));
#266170=CARTESIAN_POINT('Ctrl Pts',(129.073425698447,16.081381787091,301.537703348572));
#266171=CARTESIAN_POINT('Ctrl Pts',(130.339057893189,5.92308287892268,299.537703348572));
#266172=CARTESIAN_POINT('Ctrl Pts',(130.,-4.30813900827772,297.537703348572));
#266173=CARTESIAN_POINT('Ctrl Pts',(129.660942106811,-14.5393608954781,
295.537703348572));
#266174=CARTESIAN_POINT('Ctrl Pts',(127.725542856289,-24.591579123369,293.537703348572));
#266175=CARTESIAN_POINT('Ctrl Pts',(125.790143605767,-34.6437973512599,
291.537703348572));
#266176=CARTESIAN_POINT('Ctrl Pts',(122.306058950683,-44.269492945671,289.537703348572));
#266177=CARTESIAN_POINT('Ctrl Pts',(118.821974295598,-53.8951885400822,
287.537703348572));
#266178=CARTESIAN_POINT('Ctrl Pts',(113.874993963172,-62.8573449296269,
285.537703348572));
#266179=CARTESIAN_POINT('Ctrl Pts',(108.928013630747,-71.8195013191717,
283.537703348572));
#266180=CARTESIAN_POINT('Ctrl Pts',(102.639948694852,-79.8974404698478,
281.537703348572));
#266181=CARTESIAN_POINT('Ctrl Pts',(96.3518837589563,-87.9753796205239,
279.537703348572));
#266182=CARTESIAN_POINT('Ctrl Pts',(88.8775672472037,-94.9701958612986,
277.537703348572));
#266183=CARTESIAN_POINT('Ctrl Pts',(81.4032507354513,-101.965012102073,
275.537703348572));
#266184=CARTESIAN_POINT('Ctrl Pts',(72.9267251261952,-107.704469842635,
273.537703348572));
#266185=CARTESIAN_POINT('Ctrl Pts',(64.4501995169392,-113.443927583196,
271.537703348572));
#266186=CARTESIAN_POINT('Ctrl Pts',(55.1801850026552,-117.786702325803,
269.537703348572));
#266187=CARTESIAN_POINT('Ctrl Pts',(45.9101704883713,-122.12947706841,267.537703348572));
#266188=CARTESIAN_POINT('Ctrl Pts',(36.0749255918153,-124.968635286057,
265.537703348572));
#266189=CARTESIAN_POINT('Ctrl Pts',(26.2396806952593,-127.807793503704,
263.537703348572));
#266190=CARTESIAN_POINT('Ctrl Pts',(16.081381787091,-129.073425698447,261.537703348572));
#266191=CARTESIAN_POINT('Ctrl Pts',(5.92308287892275,-130.339057893189,
259.537703348572));
#266192=CARTESIAN_POINT('Ctrl Pts',(-4.30813900827771,-130.,257.537703348572));
#266193=CARTESIAN_POINT('Ctrl Pts',(-14.5393608954782,-129.660942106811,
255.537703348572));
#266194=CARTESIAN_POINT('Ctrl Pts',(-24.591579123369,-127.725542856289,
253.537703348572));
#266195=CARTESIAN_POINT('Ctrl Pts',(-34.6437973512598,-125.790143605767,
251.537703348572));
#266196=CARTESIAN_POINT('Ctrl Pts',(-44.269492945671,-122.306058950683,
249.537703348572));
#266197=CARTESIAN_POINT('Ctrl Pts',(-53.8951885400822,-118.821974295598,
247.537703348572));
#266198=CARTESIAN_POINT('Ctrl Pts',(-62.8573449296269,-113.874993963172,
245.537703348572));
#266199=CARTESIAN_POINT('Ctrl Pts',(-71.8195013191717,-108.928013630747,
243.537703348572));
#266200=CARTESIAN_POINT('Ctrl Pts',(-79.8974404698478,-102.639948694852,
241.537703348572));
#266201=CARTESIAN_POINT('Ctrl Pts',(-87.975379620524,-96.3518837589562,
239.537703348572));
#266202=CARTESIAN_POINT('Ctrl Pts',(-94.9701958612986,-88.8775672472037,
237.537703348572));
#266203=CARTESIAN_POINT('Ctrl Pts',(-101.965012102073,-81.4032507354513,
235.537703348572));
#266204=CARTESIAN_POINT('Ctrl Pts',(-107.704469842635,-72.9267251261952,
233.537703348572));
#266205=CARTESIAN_POINT('Ctrl Pts',(-113.443927583196,-64.4501995169392,
231.537703348572));
#266206=CARTESIAN_POINT('Ctrl Pts',(-117.786702325803,-55.1801850026553,
229.537703348572));
#266207=CARTESIAN_POINT('Ctrl Pts',(-122.12947706841,-45.9101704883713,
227.537703348572));
#266208=CARTESIAN_POINT('Ctrl Pts',(-124.968635286057,-36.0749255918153,
225.537703348572));
#266209=CARTESIAN_POINT('Ctrl Pts',(-127.807793503704,-26.2396806952593,
223.537703348572));
#266210=CARTESIAN_POINT('Ctrl Pts',(-129.073425698447,-16.081381787091,
221.537703348572));
#266211=CARTESIAN_POINT('Ctrl Pts',(-130.339057893189,-5.92308287892275,
219.537703348572));
#266212=CARTESIAN_POINT('Ctrl Pts',(-130.,4.30813900827773,217.537703348572));
#266213=CARTESIAN_POINT('',(-146.075461400193,65.4256802672723,367.5));
#266214=CARTESIAN_POINT('',(-146.075461400193,65.4256802672722,367.5));
#266215=CARTESIAN_POINT('',(-160.,4.30813900827767,377.537703348572));
#266216=CARTESIAN_POINT('Ctrl Pts',(-160.,4.30813900827767,377.537703348572));
#266217=CARTESIAN_POINT('Ctrl Pts',(-159.660942106811,16.9004121002166,
375.537703348572));
#266218=CARTESIAN_POINT('Ctrl Pts',(-157.356193074143,29.2846130745759,
373.537703348572));
#266219=CARTESIAN_POINT('Ctrl Pts',(-155.051444041476,41.6688140489352,
371.537703348572));
#266220=CARTESIAN_POINT('Ctrl Pts',(-150.837754439537,53.5400027769194,
369.537703348572));
#266221=CARTESIAN_POINT('Ctrl Pts',(-148.694504587761,59.5781607537101,
368.520423931127));
#266222=CARTESIAN_POINT('Ctrl Pts',(-146.075461400193,65.4256802672722,
367.5));
#266223=CARTESIAN_POINT('',(-145.,4.3081390082777,377.537703348572));
#266224=CARTESIAN_POINT('Ctrl Pts',(-160.,-4.30813900827851,372.462296651429));
#266225=CARTESIAN_POINT('Ctrl Pts',(-160.339057893189,8.28413408366045,
370.462296651429));
#266226=CARTESIAN_POINT('Ctrl Pts',(-158.704075916301,20.7744157382972,
368.462296651429));
#266227=CARTESIAN_POINT('Ctrl Pts',(-157.069093939413,33.2646973929339,
366.462296651429));
#266228=CARTESIAN_POINT('Ctrl Pts',(-153.500330774912,45.345435423063,364.462296651429));
#266229=CARTESIAN_POINT('Ctrl Pts',(-149.931567610412,57.4261734531921,
362.462296651429));
#266230=CARTESIAN_POINT('Ctrl Pts',(-144.516898051455,68.7998999948409,
360.462296651429));
#266231=CARTESIAN_POINT('Ctrl Pts',(-139.102228492498,80.1736265364898,
358.462296651429));
#266232=CARTESIAN_POINT('Ctrl Pts',(-131.974979673884,90.5602826949688,
356.462296651429));
#266233=CARTESIAN_POINT('Ctrl Pts',(-124.84773085527,100.946938853448,354.462296651429));
#266234=CARTESIAN_POINT('Ctrl Pts',(-116.183399296896,110.0907706828,352.462296651429));
#266235=CARTESIAN_POINT('Ctrl Pts',(-107.519067738522,119.234602512151,
350.462296651429));
#266236=CARTESIAN_POINT('Ctrl Pts',(-97.5309980386227,126.9104585261,348.462296651429));
#266237=CARTESIAN_POINT('Ctrl Pts',(-87.5429283387237,134.586314540048,
346.462296651428));
#266238=CARTESIAN_POINT('Ctrl Pts',(-76.4770599218141,140.605189688823,
344.462296651429));
#266239=CARTESIAN_POINT('Ctrl Pts',(-65.4111915049045,146.624064837598,
342.462296651429));
#266240=CARTESIAN_POINT('Ctrl Pts',(-53.5400027769202,150.837754439537,
340.462296651429));
#266241=CARTESIAN_POINT('Ctrl Pts',(-41.668814048936,155.051444041475,338.462296651429));
#266242=CARTESIAN_POINT('Ctrl Pts',(-29.2846130745767,157.356193074143,
336.462296651429));
#266243=CARTESIAN_POINT('Ctrl Pts',(-16.9004121002175,159.660942106811,
334.462296651428));
#266244=CARTESIAN_POINT('Ctrl Pts',(-4.30813900827852,160.,332.462296651429));
#266245=CARTESIAN_POINT('Ctrl Pts',(8.28413408366043,160.339057893189,330.462296651429));
#266246=CARTESIAN_POINT('Ctrl Pts',(20.7744157382972,158.704075916301,328.462296651429));
#266247=CARTESIAN_POINT('Ctrl Pts',(33.2646973929339,157.069093939413,326.462296651428));
#266248=CARTESIAN_POINT('Ctrl Pts',(45.345435423063,153.500330774912,324.462296651429));
#266249=CARTESIAN_POINT('Ctrl Pts',(57.4261734531921,149.931567610412,322.462296651428));
#266250=CARTESIAN_POINT('Ctrl Pts',(68.7998999948409,144.516898051455,320.462296651429));
#266251=CARTESIAN_POINT('Ctrl Pts',(80.1736265364898,139.102228492498,318.462296651429));
#266252=CARTESIAN_POINT('Ctrl Pts',(90.5602826949688,131.974979673884,316.462296651429));
#266253=CARTESIAN_POINT('Ctrl Pts',(100.946938853448,124.84773085527,314.462296651429));
#266254=CARTESIAN_POINT('Ctrl Pts',(110.0907706828,116.183399296896,312.462296651429));
#266255=CARTESIAN_POINT('Ctrl Pts',(119.234602512151,107.519067738522,310.462296651429));
#266256=CARTESIAN_POINT('Ctrl Pts',(126.9104585261,97.5309980386227,308.462296651429));
#266257=CARTESIAN_POINT('Ctrl Pts',(134.586314540048,87.5429283387237,306.462296651429));
#266258=CARTESIAN_POINT('Ctrl Pts',(140.605189688823,76.4770599218141,304.462296651429));
#266259=CARTESIAN_POINT('Ctrl Pts',(146.624064837598,65.4111915049045,302.462296651429));
#266260=CARTESIAN_POINT('Ctrl Pts',(150.837754439537,53.5400027769202,300.462296651429));
#266261=CARTESIAN_POINT('Ctrl Pts',(155.051444041475,41.668814048936,298.462296651429));
#266262=CARTESIAN_POINT('Ctrl Pts',(157.356193074143,29.2846130745767,296.462296651429));
#266263=CARTESIAN_POINT('Ctrl Pts',(159.660942106811,16.9004121002175,294.462296651429));
#266264=CARTESIAN_POINT('Ctrl Pts',(160.,4.30813900827853,292.462296651429));
#266265=CARTESIAN_POINT('Ctrl Pts',(160.339057893189,-8.28413408366043,
290.462296651429));
#266266=CARTESIAN_POINT('Ctrl Pts',(158.704075916301,-20.7744157382971,
288.462296651429));
#266267=CARTESIAN_POINT('Ctrl Pts',(157.069093939413,-33.2646973929339,
286.462296651429));
#266268=CARTESIAN_POINT('Ctrl Pts',(153.500330774912,-45.345435423063,284.462296651429));
#266269=CARTESIAN_POINT('Ctrl Pts',(149.931567610412,-57.4261734531921,
282.462296651429));
#266270=CARTESIAN_POINT('Ctrl Pts',(144.516898051455,-68.7998999948409,
280.462296651429));
#266271=CARTESIAN_POINT('Ctrl Pts',(139.102228492498,-80.1736265364898,
278.462296651429));
#266272=CARTESIAN_POINT('Ctrl Pts',(131.974979673884,-90.5602826949688,
276.462296651429));
#266273=CARTESIAN_POINT('Ctrl Pts',(124.84773085527,-100.946938853448,274.462296651429));
#266274=CARTESIAN_POINT('Ctrl Pts',(116.183399296896,-110.0907706828,272.462296651429));
#266275=CARTESIAN_POINT('Ctrl Pts',(107.519067738522,-119.234602512151,
270.462296651429));
#266276=CARTESIAN_POINT('Ctrl Pts',(97.5309980386227,-126.9104585261,268.462296651429));
#266277=CARTESIAN_POINT('Ctrl Pts',(87.5429283387236,-134.586314540048,
266.462296651429));
#266278=CARTESIAN_POINT('Ctrl Pts',(76.4770599218141,-140.605189688823,
264.462296651429));
#266279=CARTESIAN_POINT('Ctrl Pts',(65.4111915049046,-146.624064837598,
262.462296651429));
#266280=CARTESIAN_POINT('Ctrl Pts',(53.5400027769202,-150.837754439537,
260.462296651429));
#266281=CARTESIAN_POINT('Ctrl Pts',(41.6688140489359,-155.051444041475,
258.462296651429));
#266282=CARTESIAN_POINT('Ctrl Pts',(29.2846130745768,-157.356193074143,
256.462296651429));
#266283=CARTESIAN_POINT('Ctrl Pts',(16.9004121002176,-159.660942106811,
254.462296651429));
#266284=CARTESIAN_POINT('Ctrl Pts',(4.30813900827854,-160.,252.462296651429));
#266285=CARTESIAN_POINT('Ctrl Pts',(-8.28413408366049,-160.339057893189,
250.462296651429));
#266286=CARTESIAN_POINT('Ctrl Pts',(-20.7744157382971,-158.704075916301,
248.462296651429));
#266287=CARTESIAN_POINT('Ctrl Pts',(-33.2646973929338,-157.069093939413,
246.462296651429));
#266288=CARTESIAN_POINT('Ctrl Pts',(-45.345435423063,-153.500330774912,
244.462296651429));
#266289=CARTESIAN_POINT('Ctrl Pts',(-57.4261734531921,-149.931567610412,
242.462296651429));
#266290=CARTESIAN_POINT('Ctrl Pts',(-68.7998999948409,-144.516898051455,
240.462296651429));
#266291=CARTESIAN_POINT('Ctrl Pts',(-80.1736265364897,-139.102228492498,
238.462296651429));
#266292=CARTESIAN_POINT('Ctrl Pts',(-90.5602826949688,-131.974979673884,
236.462296651429));
#266293=CARTESIAN_POINT('Ctrl Pts',(-100.946938853448,-124.84773085527,
234.462296651429));
#266294=CARTESIAN_POINT('Ctrl Pts',(-110.0907706828,-116.183399296896,232.462296651429));
#266295=CARTESIAN_POINT('Ctrl Pts',(-119.234602512151,-107.519067738522,
230.462296651429));
#266296=CARTESIAN_POINT('Ctrl Pts',(-126.9104585261,-97.5309980386227,228.462296651429));
#266297=CARTESIAN_POINT('Ctrl Pts',(-134.586314540048,-87.5429283387236,
226.462296651429));
#266298=CARTESIAN_POINT('Ctrl Pts',(-140.605189688823,-76.4770599218141,
224.462296651429));
#266299=CARTESIAN_POINT('Ctrl Pts',(-146.624064837598,-65.4111915049046,
222.462296651429));
#266300=CARTESIAN_POINT('Ctrl Pts',(-150.837754439537,-53.5400027769203,
220.462296651429));
#266301=CARTESIAN_POINT('Ctrl Pts',(-155.051444041475,-41.668814048936,
218.462296651429));
#266302=CARTESIAN_POINT('Ctrl Pts',(-157.356193074143,-29.2846130745768,
216.462296651429));
#266303=CARTESIAN_POINT('Ctrl Pts',(-159.660942106811,-16.9004121002176,
214.462296651429));
#266304=CARTESIAN_POINT('Ctrl Pts',(-160.,-4.30813900827851,212.462296651429));
#266305=CARTESIAN_POINT('Ctrl Pts',(-160.,4.30813900827767,377.537703348572));
#266306=CARTESIAN_POINT('Ctrl Pts',(-159.660942106811,16.9004121002166,
375.537703348572));
#266307=CARTESIAN_POINT('Ctrl Pts',(-157.356193074143,29.2846130745759,
373.537703348572));
#266308=CARTESIAN_POINT('Ctrl Pts',(-155.051444041476,41.6688140489352,
371.537703348572));
#266309=CARTESIAN_POINT('Ctrl Pts',(-150.837754439537,53.5400027769194,
369.537703348572));
#266310=CARTESIAN_POINT('Ctrl Pts',(-146.624064837599,65.4111915049037,
367.537703348572));
#266311=CARTESIAN_POINT('Ctrl Pts',(-140.605189688823,76.4770599218133,
365.537703348572));
#266312=CARTESIAN_POINT('Ctrl Pts',(-134.586314540048,87.542928338723,363.537703348572));
#266313=CARTESIAN_POINT('Ctrl Pts',(-126.9104585261,97.530998038622,361.537703348572));
#266314=CARTESIAN_POINT('Ctrl Pts',(-119.234602512152,107.519067738521,
359.537703348572));
#266315=CARTESIAN_POINT('Ctrl Pts',(-110.0907706828,116.183399296895,357.537703348572));
#266316=CARTESIAN_POINT('Ctrl Pts',(-100.946938853448,124.847730855269,
355.537703348572));
#266317=CARTESIAN_POINT('Ctrl Pts',(-90.5602826949695,131.974979673883,
353.537703348572));
#266318=CARTESIAN_POINT('Ctrl Pts',(-80.1736265364906,139.102228492497,
351.537703348572));
#266319=CARTESIAN_POINT('Ctrl Pts',(-68.7998999948417,144.516898051454,
349.537703348572));
#266320=CARTESIAN_POINT('Ctrl Pts',(-57.4261734531929,149.931567610411,
347.537703348572));
#266321=CARTESIAN_POINT('Ctrl Pts',(-45.3454354230638,153.500330774912,
345.537703348572));
#266322=CARTESIAN_POINT('Ctrl Pts',(-33.2646973929347,157.069093939413,
343.537703348572));
#266323=CARTESIAN_POINT('Ctrl Pts',(-20.774415738298,158.704075916301,341.537703348572));
#266324=CARTESIAN_POINT('Ctrl Pts',(-8.28413408366129,160.339057893189,
339.537703348572));
#266325=CARTESIAN_POINT('Ctrl Pts',(4.30813900827766,160.,337.537703348572));
#266326=CARTESIAN_POINT('Ctrl Pts',(16.9004121002166,159.660942106811,335.537703348572));
#266327=CARTESIAN_POINT('Ctrl Pts',(29.2846130745759,157.356193074143,333.537703348572));
#266328=CARTESIAN_POINT('Ctrl Pts',(41.6688140489352,155.051444041476,331.537703348572));
#266329=CARTESIAN_POINT('Ctrl Pts',(53.5400027769194,150.837754439537,329.537703348572));
#266330=CARTESIAN_POINT('Ctrl Pts',(65.4111915049037,146.624064837599,327.537703348572));
#266331=CARTESIAN_POINT('Ctrl Pts',(76.4770599218133,140.605189688823,325.537703348572));
#266332=CARTESIAN_POINT('Ctrl Pts',(87.542928338723,134.586314540048,323.537703348572));
#266333=CARTESIAN_POINT('Ctrl Pts',(97.530998038622,126.9104585261,321.537703348572));
#266334=CARTESIAN_POINT('Ctrl Pts',(107.519067738521,119.234602512152,319.537703348572));
#266335=CARTESIAN_POINT('Ctrl Pts',(116.183399296895,110.0907706828,317.537703348572));
#266336=CARTESIAN_POINT('Ctrl Pts',(124.847730855269,100.946938853448,315.537703348572));
#266337=CARTESIAN_POINT('Ctrl Pts',(131.974979673883,90.5602826949695,313.537703348572));
#266338=CARTESIAN_POINT('Ctrl Pts',(139.102228492497,80.1736265364906,311.537703348572));
#266339=CARTESIAN_POINT('Ctrl Pts',(144.516898051454,68.7998999948417,309.537703348572));
#266340=CARTESIAN_POINT('Ctrl Pts',(149.931567610411,57.4261734531929,307.537703348572));
#266341=CARTESIAN_POINT('Ctrl Pts',(153.500330774912,45.3454354230638,305.537703348572));
#266342=CARTESIAN_POINT('Ctrl Pts',(157.069093939413,33.2646973929347,303.537703348572));
#266343=CARTESIAN_POINT('Ctrl Pts',(158.704075916301,20.774415738298,301.537703348572));
#266344=CARTESIAN_POINT('Ctrl Pts',(160.339057893189,8.28413408366131,299.537703348572));
#266345=CARTESIAN_POINT('Ctrl Pts',(160.,-4.30813900827765,297.537703348572));
#266346=CARTESIAN_POINT('Ctrl Pts',(159.660942106811,-16.9004121002166,
295.537703348572));
#266347=CARTESIAN_POINT('Ctrl Pts',(157.356193074143,-29.2846130745759,
293.537703348572));
#266348=CARTESIAN_POINT('Ctrl Pts',(155.051444041476,-41.6688140489352,
291.537703348572));
#266349=CARTESIAN_POINT('Ctrl Pts',(150.837754439537,-53.5400027769194,
289.537703348572));
#266350=CARTESIAN_POINT('Ctrl Pts',(146.624064837599,-65.4111915049036,
287.537703348572));
#266351=CARTESIAN_POINT('Ctrl Pts',(140.605189688823,-76.4770599218133,
285.537703348572));
#266352=CARTESIAN_POINT('Ctrl Pts',(134.586314540048,-87.5429283387229,
283.537703348572));
#266353=CARTESIAN_POINT('Ctrl Pts',(126.9104585261,-97.530998038622,281.537703348572));
#266354=CARTESIAN_POINT('Ctrl Pts',(119.234602512152,-107.519067738521,
279.537703348572));
#266355=CARTESIAN_POINT('Ctrl Pts',(110.0907706828,-116.183399296895,277.537703348572));
#266356=CARTESIAN_POINT('Ctrl Pts',(100.946938853448,-124.847730855269,
275.537703348572));
#266357=CARTESIAN_POINT('Ctrl Pts',(90.5602826949695,-131.974979673883,
273.537703348572));
#266358=CARTESIAN_POINT('Ctrl Pts',(80.1736265364905,-139.102228492497,
271.537703348572));
#266359=CARTESIAN_POINT('Ctrl Pts',(68.7998999948417,-144.516898051454,
269.537703348572));
#266360=CARTESIAN_POINT('Ctrl Pts',(57.426173453193,-149.931567610411,267.537703348572));
#266361=CARTESIAN_POINT('Ctrl Pts',(45.3454354230638,-153.500330774912,
265.537703348572));
#266362=CARTESIAN_POINT('Ctrl Pts',(33.2646973929347,-157.069093939413,
263.537703348572));
#266363=CARTESIAN_POINT('Ctrl Pts',(20.774415738298,-158.704075916301,261.537703348572));
#266364=CARTESIAN_POINT('Ctrl Pts',(8.28413408366139,-160.339057893189,
259.537703348572));
#266365=CARTESIAN_POINT('Ctrl Pts',(-4.30813900827764,-160.,257.537703348572));
#266366=CARTESIAN_POINT('Ctrl Pts',(-16.9004121002167,-159.660942106811,
255.537703348572));
#266367=CARTESIAN_POINT('Ctrl Pts',(-29.2846130745759,-157.356193074143,
253.537703348572));
#266368=CARTESIAN_POINT('Ctrl Pts',(-41.6688140489351,-155.051444041476,
251.537703348572));
#266369=CARTESIAN_POINT('Ctrl Pts',(-53.5400027769194,-150.837754439537,
249.537703348572));
#266370=CARTESIAN_POINT('Ctrl Pts',(-65.4111915049037,-146.624064837599,
247.537703348572));
#266371=CARTESIAN_POINT('Ctrl Pts',(-76.4770599218133,-140.605189688823,
245.537703348572));
#266372=CARTESIAN_POINT('Ctrl Pts',(-87.5429283387229,-134.586314540048,
243.537703348572));
#266373=CARTESIAN_POINT('Ctrl Pts',(-97.530998038622,-126.9104585261,241.537703348572));
#266374=CARTESIAN_POINT('Ctrl Pts',(-107.519067738521,-119.234602512152,
239.537703348572));
#266375=CARTESIAN_POINT('Ctrl Pts',(-116.183399296895,-110.0907706828,237.537703348572));
#266376=CARTESIAN_POINT('Ctrl Pts',(-124.847730855269,-100.946938853448,
235.537703348572));
#266377=CARTESIAN_POINT('Ctrl Pts',(-131.974979673883,-90.5602826949695,
233.537703348572));
#266378=CARTESIAN_POINT('Ctrl Pts',(-139.102228492497,-80.1736265364905,
231.537703348572));
#266379=CARTESIAN_POINT('Ctrl Pts',(-144.516898051454,-68.7998999948417,
229.537703348572));
#266380=CARTESIAN_POINT('Ctrl Pts',(-149.931567610411,-57.426173453193,
227.537703348572));
#266381=CARTESIAN_POINT('Ctrl Pts',(-153.500330774912,-45.3454354230638,
225.537703348572));
#266382=CARTESIAN_POINT('Ctrl Pts',(-157.069093939413,-33.2646973929347,
223.537703348572));
#266383=CARTESIAN_POINT('Ctrl Pts',(-158.704075916301,-20.774415738298,
221.537703348572));
#266384=CARTESIAN_POINT('Ctrl Pts',(-160.339057893189,-8.2841340836614,
219.537703348572));
#266385=CARTESIAN_POINT('Ctrl Pts',(-160.,4.30813900827767,217.537703348572));
#266386=CARTESIAN_POINT('',(-157.805088795962,26.7603066464745,367.5));
#266387=CARTESIAN_POINT('Ctrl Pts',(-157.805088795962,26.7603066464745,
367.5));
#266388=CARTESIAN_POINT('Ctrl Pts',(-156.638532817877,33.4083424416569,
367.5));
#266389=CARTESIAN_POINT('Ctrl Pts',(-155.071407572055,39.9802096740424,
367.5));
#266390=CARTESIAN_POINT('Ctrl Pts',(-152.131501324444,49.6731919343096,
367.5));
#266391=CARTESIAN_POINT('Ctrl Pts',(-151.053085052424,52.8765297093725,
367.499999999997));
#266392=CARTESIAN_POINT('Ctrl Pts',(-148.705612539595,59.2094688002817,
367.499999999997));
#266393=CARTESIAN_POINT('Ctrl Pts',(-147.437304082636,62.3378048444623,
367.5));
#266394=CARTESIAN_POINT('Ctrl Pts',(-146.075461400193,65.4256802672723,
367.5));
#266395=CARTESIAN_POINT('',(-160.,-4.30813900827851,372.462296651429));
#266396=CARTESIAN_POINT('Ctrl Pts',(-160.,-4.30813900827851,372.462296651429));
#266397=CARTESIAN_POINT('Ctrl Pts',(-160.339057893189,8.28413408366045,
370.462296651429));
#266398=CARTESIAN_POINT('Ctrl Pts',(-158.704075916301,20.7744157382972,
368.462296651429));
#266399=CARTESIAN_POINT('Ctrl Pts',(-158.311185598564,23.7758621134177,
367.981691576521));
#266400=CARTESIAN_POINT('Ctrl Pts',(-157.805088795962,26.7603066464745,
367.5));
#266401=CARTESIAN_POINT('',(-160.,-4.21537804662364E-13,375.));
#266402=CARTESIAN_POINT('Ctrl Pts',(-130.,-4.30813900827845,372.462296651428));
#266403=CARTESIAN_POINT('Ctrl Pts',(-130.339057893189,5.92308287892195,
370.462296651428));
#266404=CARTESIAN_POINT('Ctrl Pts',(-129.073425698447,16.0813817870903,
368.462296651429));
#266405=CARTESIAN_POINT('Ctrl Pts',(-127.807793503705,26.2396806952586,
366.462296651429));
#266406=CARTESIAN_POINT('Ctrl Pts',(-124.968635286058,36.0749255918146,
364.462296651428));
#266407=CARTESIAN_POINT('Ctrl Pts',(-122.129477068411,45.9101704883706,
362.462296651428));
#266408=CARTESIAN_POINT('Ctrl Pts',(-117.786702325804,55.1801850026546,
360.462296651428));
#266409=CARTESIAN_POINT('Ctrl Pts',(-113.443927583196,64.4501995169386,
358.462296651428));
#266410=CARTESIAN_POINT('Ctrl Pts',(-107.704469842635,72.9267251261946,
356.462296651428));
#266411=CARTESIAN_POINT('Ctrl Pts',(-101.965012102074,81.4032507354507,
354.462296651428));
#266412=CARTESIAN_POINT('Ctrl Pts',(-94.9701958612992,88.8775672472032,
352.462296651428));
#266413=CARTESIAN_POINT('Ctrl Pts',(-87.9753796205245,96.3518837589558,
350.462296651428));
#266414=CARTESIAN_POINT('Ctrl Pts',(-79.8974404698484,102.639948694851,
348.462296651428));
#266415=CARTESIAN_POINT('Ctrl Pts',(-71.8195013191724,108.928013630747,
346.462296651428));
#266416=CARTESIAN_POINT('Ctrl Pts',(-62.8573449296276,113.874993963172,
344.462296651428));
#266417=CARTESIAN_POINT('Ctrl Pts',(-53.8951885400828,118.821974295598,
342.462296651428));
#266418=CARTESIAN_POINT('Ctrl Pts',(-44.2694929456717,122.306058950682,
340.462296651428));
#266419=CARTESIAN_POINT('Ctrl Pts',(-34.6437973512606,125.790143605767,
338.462296651428));
#266420=CARTESIAN_POINT('Ctrl Pts',(-24.5915791233697,127.725542856289,
336.462296651428));
#266421=CARTESIAN_POINT('Ctrl Pts',(-14.5393608954789,129.660942106811,
334.462296651428));
#266422=CARTESIAN_POINT('Ctrl Pts',(-4.30813900827846,130.,332.462296651428));
#266423=CARTESIAN_POINT('Ctrl Pts',(5.92308287892194,130.339057893189,330.462296651429));
#266424=CARTESIAN_POINT('Ctrl Pts',(16.0813817870903,129.073425698447,328.462296651428));
#266425=CARTESIAN_POINT('Ctrl Pts',(26.2396806952586,127.807793503705,326.462296651428));
#266426=CARTESIAN_POINT('Ctrl Pts',(36.0749255918146,124.968635286058,324.462296651428));
#266427=CARTESIAN_POINT('Ctrl Pts',(45.9101704883706,122.129477068411,322.462296651428));
#266428=CARTESIAN_POINT('Ctrl Pts',(55.1801850026546,117.786702325804,320.462296651428));
#266429=CARTESIAN_POINT('Ctrl Pts',(64.4501995169386,113.443927583196,318.462296651428));
#266430=CARTESIAN_POINT('Ctrl Pts',(72.9267251261946,107.704469842635,316.462296651428));
#266431=CARTESIAN_POINT('Ctrl Pts',(81.4032507354506,101.965012102074,314.462296651428));
#266432=CARTESIAN_POINT('Ctrl Pts',(88.8775672472032,94.9701958612992,312.462296651428));
#266433=CARTESIAN_POINT('Ctrl Pts',(96.3518837589558,87.9753796205245,310.462296651428));
#266434=CARTESIAN_POINT('Ctrl Pts',(102.639948694851,79.8974404698484,308.462296651428));
#266435=CARTESIAN_POINT('Ctrl Pts',(108.928013630747,71.8195013191724,306.462296651428));
#266436=CARTESIAN_POINT('Ctrl Pts',(113.874993963172,62.8573449296276,304.462296651428));
#266437=CARTESIAN_POINT('Ctrl Pts',(118.821974295598,53.8951885400829,302.462296651428));
#266438=CARTESIAN_POINT('Ctrl Pts',(122.306058950682,44.2694929456717,300.462296651428));
#266439=CARTESIAN_POINT('Ctrl Pts',(125.790143605767,34.6437973512606,298.462296651428));
#266440=CARTESIAN_POINT('Ctrl Pts',(127.725542856289,24.5915791233698,296.462296651428));
#266441=CARTESIAN_POINT('Ctrl Pts',(129.660942106811,14.5393608954789,294.462296651429));
#266442=CARTESIAN_POINT('Ctrl Pts',(130.,4.30813900827846,292.462296651428));
#266443=CARTESIAN_POINT('Ctrl Pts',(130.339057893189,-5.92308287892194,
290.462296651428));
#266444=CARTESIAN_POINT('Ctrl Pts',(129.073425698447,-16.0813817870903,
288.462296651428));
#266445=CARTESIAN_POINT('Ctrl Pts',(127.807793503705,-26.2396806952586,
286.462296651428));
#266446=CARTESIAN_POINT('Ctrl Pts',(124.968635286058,-36.0749255918146,
284.462296651428));
#266447=CARTESIAN_POINT('Ctrl Pts',(122.129477068411,-45.9101704883706,
282.462296651428));
#266448=CARTESIAN_POINT('Ctrl Pts',(117.786702325804,-55.1801850026546,
280.462296651428));
#266449=CARTESIAN_POINT('Ctrl Pts',(113.443927583196,-64.4501995169386,
278.462296651428));
#266450=CARTESIAN_POINT('Ctrl Pts',(107.704469842635,-72.9267251261946,
276.462296651428));
#266451=CARTESIAN_POINT('Ctrl Pts',(101.965012102074,-81.4032507354506,
274.462296651428));
#266452=CARTESIAN_POINT('Ctrl Pts',(94.9701958612992,-88.8775672472032,
272.462296651428));
#266453=CARTESIAN_POINT('Ctrl Pts',(87.9753796205246,-96.3518837589557,
270.462296651428));
#266454=CARTESIAN_POINT('Ctrl Pts',(79.8974404698484,-102.639948694851,
268.462296651428));
#266455=CARTESIAN_POINT('Ctrl Pts',(71.8195013191723,-108.928013630747,
266.462296651428));
#266456=CARTESIAN_POINT('Ctrl Pts',(62.8573449296276,-113.874993963172,
264.462296651428));
#266457=CARTESIAN_POINT('Ctrl Pts',(53.8951885400829,-118.821974295598,
262.462296651428));
#266458=CARTESIAN_POINT('Ctrl Pts',(44.2694929456717,-122.306058950682,
260.462296651428));
#266459=CARTESIAN_POINT('Ctrl Pts',(34.6437973512606,-125.790143605767,
258.462296651428));
#266460=CARTESIAN_POINT('Ctrl Pts',(24.5915791233698,-127.725542856289,
256.462296651428));
#266461=CARTESIAN_POINT('Ctrl Pts',(14.5393608954789,-129.660942106811,
254.462296651428));
#266462=CARTESIAN_POINT('Ctrl Pts',(4.30813900827847,-130.,252.462296651428));
#266463=CARTESIAN_POINT('Ctrl Pts',(-5.92308287892199,-130.339057893189,
250.462296651428));
#266464=CARTESIAN_POINT('Ctrl Pts',(-16.0813817870903,-129.073425698447,
248.462296651428));
#266465=CARTESIAN_POINT('Ctrl Pts',(-26.2396806952585,-127.807793503705,
246.462296651428));
#266466=CARTESIAN_POINT('Ctrl Pts',(-36.0749255918146,-124.968635286058,
244.462296651428));
#266467=CARTESIAN_POINT('Ctrl Pts',(-45.9101704883706,-122.129477068411,
242.462296651428));
#266468=CARTESIAN_POINT('Ctrl Pts',(-55.1801850026546,-117.786702325804,
240.462296651428));
#266469=CARTESIAN_POINT('Ctrl Pts',(-64.4501995169385,-113.443927583197,
238.462296651429));
#266470=CARTESIAN_POINT('Ctrl Pts',(-72.9267251261946,-107.704469842635,
236.462296651428));
#266471=CARTESIAN_POINT('Ctrl Pts',(-81.4032507354507,-101.965012102074,
234.462296651428));
#266472=CARTESIAN_POINT('Ctrl Pts',(-88.8775672472032,-94.9701958612992,
232.462296651428));
#266473=CARTESIAN_POINT('Ctrl Pts',(-96.3518837589557,-87.9753796205246,
230.462296651428));
#266474=CARTESIAN_POINT('Ctrl Pts',(-102.639948694851,-79.8974404698484,
228.462296651428));
#266475=CARTESIAN_POINT('Ctrl Pts',(-108.928013630747,-71.8195013191723,
226.462296651428));
#266476=CARTESIAN_POINT('Ctrl Pts',(-113.874993963172,-62.8573449296276,
224.462296651428));
#266477=CARTESIAN_POINT('Ctrl Pts',(-118.821974295598,-53.8951885400829,
222.462296651428));
#266478=CARTESIAN_POINT('Ctrl Pts',(-122.306058950682,-44.2694929456718,
220.462296651428));
#266479=CARTESIAN_POINT('Ctrl Pts',(-125.790143605767,-34.6437973512606,
218.462296651428));
#266480=CARTESIAN_POINT('Ctrl Pts',(-127.725542856289,-24.5915791233698,
216.462296651428));
#266481=CARTESIAN_POINT('Ctrl Pts',(-129.660942106811,-14.5393608954789,
214.462296651428));
#266482=CARTESIAN_POINT('Ctrl Pts',(-130.,-4.30813900827845,212.462296651428));
#266483=CARTESIAN_POINT('Ctrl Pts',(-160.,-4.30813900827851,372.462296651429));
#266484=CARTESIAN_POINT('Ctrl Pts',(-160.339057893189,8.28413408366045,
370.462296651429));
#266485=CARTESIAN_POINT('Ctrl Pts',(-158.704075916301,20.7744157382972,
368.462296651429));
#266486=CARTESIAN_POINT('Ctrl Pts',(-157.069093939413,33.2646973929339,
366.462296651429));
#266487=CARTESIAN_POINT('Ctrl Pts',(-153.500330774912,45.345435423063,364.462296651429));
#266488=CARTESIAN_POINT('Ctrl Pts',(-149.931567610412,57.4261734531921,
362.462296651429));
#266489=CARTESIAN_POINT('Ctrl Pts',(-144.516898051455,68.7998999948409,
360.462296651429));
#266490=CARTESIAN_POINT('Ctrl Pts',(-139.102228492498,80.1736265364898,
358.462296651429));
#266491=CARTESIAN_POINT('Ctrl Pts',(-131.974979673884,90.5602826949688,
356.462296651429));
#266492=CARTESIAN_POINT('Ctrl Pts',(-124.84773085527,100.946938853448,354.462296651429));
#266493=CARTESIAN_POINT('Ctrl Pts',(-116.183399296896,110.0907706828,352.462296651429));
#266494=CARTESIAN_POINT('Ctrl Pts',(-107.519067738522,119.234602512151,
350.462296651429));
#266495=CARTESIAN_POINT('Ctrl Pts',(-97.5309980386227,126.9104585261,348.462296651429));
#266496=CARTESIAN_POINT('Ctrl Pts',(-87.5429283387237,134.586314540048,
346.462296651428));
#266497=CARTESIAN_POINT('Ctrl Pts',(-76.4770599218141,140.605189688823,
344.462296651429));
#266498=CARTESIAN_POINT('Ctrl Pts',(-65.4111915049045,146.624064837598,
342.462296651429));
#266499=CARTESIAN_POINT('Ctrl Pts',(-53.5400027769202,150.837754439537,
340.462296651429));
#266500=CARTESIAN_POINT('Ctrl Pts',(-41.668814048936,155.051444041475,338.462296651429));
#266501=CARTESIAN_POINT('Ctrl Pts',(-29.2846130745767,157.356193074143,
336.462296651429));
#266502=CARTESIAN_POINT('Ctrl Pts',(-16.9004121002175,159.660942106811,
334.462296651428));
#266503=CARTESIAN_POINT('Ctrl Pts',(-4.30813900827852,160.,332.462296651429));
#266504=CARTESIAN_POINT('Ctrl Pts',(8.28413408366043,160.339057893189,330.462296651429));
#266505=CARTESIAN_POINT('Ctrl Pts',(20.7744157382972,158.704075916301,328.462296651429));
#266506=CARTESIAN_POINT('Ctrl Pts',(33.2646973929339,157.069093939413,326.462296651428));
#266507=CARTESIAN_POINT('Ctrl Pts',(45.345435423063,153.500330774912,324.462296651429));
#266508=CARTESIAN_POINT('Ctrl Pts',(57.4261734531921,149.931567610412,322.462296651428));
#266509=CARTESIAN_POINT('Ctrl Pts',(68.7998999948409,144.516898051455,320.462296651429));
#266510=CARTESIAN_POINT('Ctrl Pts',(80.1736265364898,139.102228492498,318.462296651429));
#266511=CARTESIAN_POINT('Ctrl Pts',(90.5602826949688,131.974979673884,316.462296651429));
#266512=CARTESIAN_POINT('Ctrl Pts',(100.946938853448,124.84773085527,314.462296651429));
#266513=CARTESIAN_POINT('Ctrl Pts',(110.0907706828,116.183399296896,312.462296651429));
#266514=CARTESIAN_POINT('Ctrl Pts',(119.234602512151,107.519067738522,310.462296651429));
#266515=CARTESIAN_POINT('Ctrl Pts',(126.9104585261,97.5309980386227,308.462296651429));
#266516=CARTESIAN_POINT('Ctrl Pts',(134.586314540048,87.5429283387237,306.462296651429));
#266517=CARTESIAN_POINT('Ctrl Pts',(140.605189688823,76.4770599218141,304.462296651429));
#266518=CARTESIAN_POINT('Ctrl Pts',(146.624064837598,65.4111915049045,302.462296651429));
#266519=CARTESIAN_POINT('Ctrl Pts',(150.837754439537,53.5400027769202,300.462296651429));
#266520=CARTESIAN_POINT('Ctrl Pts',(155.051444041475,41.668814048936,298.462296651429));
#266521=CARTESIAN_POINT('Ctrl Pts',(157.356193074143,29.2846130745767,296.462296651429));
#266522=CARTESIAN_POINT('Ctrl Pts',(159.660942106811,16.9004121002175,294.462296651429));
#266523=CARTESIAN_POINT('Ctrl Pts',(160.,4.30813900827853,292.462296651429));
#266524=CARTESIAN_POINT('Ctrl Pts',(160.339057893189,-8.28413408366043,
290.462296651429));
#266525=CARTESIAN_POINT('Ctrl Pts',(158.704075916301,-20.7744157382971,
288.462296651429));
#266526=CARTESIAN_POINT('Ctrl Pts',(157.069093939413,-33.2646973929339,
286.462296651429));
#266527=CARTESIAN_POINT('Ctrl Pts',(153.500330774912,-45.345435423063,284.462296651429));
#266528=CARTESIAN_POINT('Ctrl Pts',(149.931567610412,-57.4261734531921,
282.462296651429));
#266529=CARTESIAN_POINT('Ctrl Pts',(144.516898051455,-68.7998999948409,
280.462296651429));
#266530=CARTESIAN_POINT('Ctrl Pts',(139.102228492498,-80.1736265364898,
278.462296651429));
#266531=CARTESIAN_POINT('Ctrl Pts',(131.974979673884,-90.5602826949688,
276.462296651429));
#266532=CARTESIAN_POINT('Ctrl Pts',(124.84773085527,-100.946938853448,274.462296651429));
#266533=CARTESIAN_POINT('Ctrl Pts',(116.183399296896,-110.0907706828,272.462296651429));
#266534=CARTESIAN_POINT('Ctrl Pts',(107.519067738522,-119.234602512151,
270.462296651429));
#266535=CARTESIAN_POINT('Ctrl Pts',(97.5309980386227,-126.9104585261,268.462296651429));
#266536=CARTESIAN_POINT('Ctrl Pts',(87.5429283387236,-134.586314540048,
266.462296651429));
#266537=CARTESIAN_POINT('Ctrl Pts',(76.4770599218141,-140.605189688823,
264.462296651429));
#266538=CARTESIAN_POINT('Ctrl Pts',(65.4111915049046,-146.624064837598,
262.462296651429));
#266539=CARTESIAN_POINT('Ctrl Pts',(53.5400027769202,-150.837754439537,
260.462296651429));
#266540=CARTESIAN_POINT('Ctrl Pts',(41.6688140489359,-155.051444041475,
258.462296651429));
#266541=CARTESIAN_POINT('Ctrl Pts',(29.2846130745768,-157.356193074143,
256.462296651429));
#266542=CARTESIAN_POINT('Ctrl Pts',(16.9004121002176,-159.660942106811,
254.462296651429));
#266543=CARTESIAN_POINT('Ctrl Pts',(4.30813900827854,-160.,252.462296651429));
#266544=CARTESIAN_POINT('Ctrl Pts',(-8.28413408366049,-160.339057893189,
250.462296651429));
#266545=CARTESIAN_POINT('Ctrl Pts',(-20.7744157382971,-158.704075916301,
248.462296651429));
#266546=CARTESIAN_POINT('Ctrl Pts',(-33.2646973929338,-157.069093939413,
246.462296651429));
#266547=CARTESIAN_POINT('Ctrl Pts',(-45.345435423063,-153.500330774912,
244.462296651429));
#266548=CARTESIAN_POINT('Ctrl Pts',(-57.4261734531921,-149.931567610412,
242.462296651429));
#266549=CARTESIAN_POINT('Ctrl Pts',(-68.7998999948409,-144.516898051455,
240.462296651429));
#266550=CARTESIAN_POINT('Ctrl Pts',(-80.1736265364897,-139.102228492498,
238.462296651429));
#266551=CARTESIAN_POINT('Ctrl Pts',(-90.5602826949688,-131.974979673884,
236.462296651429));
#266552=CARTESIAN_POINT('Ctrl Pts',(-100.946938853448,-124.84773085527,
234.462296651429));
#266553=CARTESIAN_POINT('Ctrl Pts',(-110.0907706828,-116.183399296896,232.462296651429));
#266554=CARTESIAN_POINT('Ctrl Pts',(-119.234602512151,-107.519067738522,
230.462296651429));
#266555=CARTESIAN_POINT('Ctrl Pts',(-126.9104585261,-97.5309980386227,228.462296651429));
#266556=CARTESIAN_POINT('Ctrl Pts',(-134.586314540048,-87.5429283387236,
226.462296651429));
#266557=CARTESIAN_POINT('Ctrl Pts',(-140.605189688823,-76.4770599218141,
224.462296651429));
#266558=CARTESIAN_POINT('Ctrl Pts',(-146.624064837598,-65.4111915049046,
222.462296651429));
#266559=CARTESIAN_POINT('Ctrl Pts',(-150.837754439537,-53.5400027769203,
220.462296651429));
#266560=CARTESIAN_POINT('Ctrl Pts',(-155.051444041475,-41.668814048936,
218.462296651429));
#266561=CARTESIAN_POINT('Ctrl Pts',(-157.356193074143,-29.2846130745768,
216.462296651429));
#266562=CARTESIAN_POINT('Ctrl Pts',(-159.660942106811,-16.9004121002176,
214.462296651429));
#266563=CARTESIAN_POINT('Ctrl Pts',(-160.,-4.30813900827851,212.462296651429));
#266564=CARTESIAN_POINT('',(-128.373075022505,20.9502666088252,367.5));
#266565=CARTESIAN_POINT('',(-145.,-4.30813900827848,372.462296651428));
#266566=CARTESIAN_POINT('Origin',(-130.,-3.57353036051222E-13,375.));
#266567=CARTESIAN_POINT('Origin',(-160.,-160.339057893189,367.5));
#266568=CARTESIAN_POINT('Origin',(0.,0.,848.));
#266569=CARTESIAN_POINT('',(-3.4,-4.163799117101E-16,828.));
#266570=CARTESIAN_POINT('Origin',(0.,0.,828.));
#266571=CARTESIAN_POINT('',(-3.4,-4.163799117101E-16,848.));
#266572=CARTESIAN_POINT('',(-3.4,-4.163799117101E-16,848.));
#266573=CARTESIAN_POINT('Origin',(0.,0.,848.));
#266574=CARTESIAN_POINT('Origin',(0.,0.,828.));
#266575=CARTESIAN_POINT('',(-5.33250671116729E-15,0.,825.957073895307));
#266576=CARTESIAN_POINT('',(-3.4,-4.163799117101E-16,828.));
#266577=CARTESIAN_POINT('Origin',(-160.,-1.08084483543429E-12,695.));
#266578=CARTESIAN_POINT('',(-15.,3.28589693438513E-15,702.5));
#266579=CARTESIAN_POINT('Ctrl Pts',(-12.990381056766,-7.50000000000104,
695.));
#266580=CARTESIAN_POINT('Ctrl Pts',(-12.990381056766,-7.50000000000104,
694.037711997797));
#266581=CARTESIAN_POINT('Ctrl Pts',(-13.1086907696464,-7.30414188357672,
693.026460490526));
#266582=CARTESIAN_POINT('Ctrl Pts',(-13.5089700934546,-6.5342153230227,
691.185632303692));
#266583=CARTESIAN_POINT('Ctrl Pts',(-13.7827535066158,-5.9606687109838,
690.354066993185));
#266584=CARTESIAN_POINT('Ctrl Pts',(-14.2789995755284,-4.64772502354804,
689.041123305749));
#266585=CARTESIAN_POINT('Ctrl Pts',(-14.5369863077958,-3.8155556858589,
688.466261900566));
#266586=CARTESIAN_POINT('Ctrl Pts',(-14.8994397626298,-1.97208806616749,
687.695270705982));
#266587=CARTESIAN_POINT('Ctrl Pts',(-14.9999999999999,-0.959664758316259,
687.5));
#266588=CARTESIAN_POINT('Ctrl Pts',(-15.0000000000001,0.959664758314065,
687.5));
#266589=CARTESIAN_POINT('Ctrl Pts',(-14.8994397626301,1.97208806616529,
687.695270705982));
#266590=CARTESIAN_POINT('Ctrl Pts',(-14.5369863077964,3.81555568585669,
688.466261900566));
#266591=CARTESIAN_POINT('Ctrl Pts',(-14.2789995755291,4.64772502354583,
689.041123305749));
#266592=CARTESIAN_POINT('Ctrl Pts',(-13.7827535066168,5.96066871098163,
690.354066993185));
#266593=CARTESIAN_POINT('Ctrl Pts',(-13.5089700934557,6.53421532302054,
691.185632303692));
#266594=CARTESIAN_POINT('Ctrl Pts',(-13.1086907696476,7.30414188357456,
693.026460490526));
#266595=CARTESIAN_POINT('Ctrl Pts',(-12.9903810567672,7.49999999999887,
694.037711997797));
#266596=CARTESIAN_POINT('Ctrl Pts',(-12.9903810567672,7.49999999999887,
695.962288002204));
#266597=CARTESIAN_POINT('Ctrl Pts',(-13.1086907696476,7.30414188357456,
696.973539509475));
#266598=CARTESIAN_POINT('Ctrl Pts',(-13.5089700934557,6.53421532302054,
698.814367696309));
#266599=CARTESIAN_POINT('Ctrl Pts',(-13.7827535066168,5.96066871098163,
699.645933006816));
#266600=CARTESIAN_POINT('Ctrl Pts',(-14.2789995755291,4.64772502354583,
700.958876694252));
#266601=CARTESIAN_POINT('Ctrl Pts',(-14.5369863077964,3.81555568585669,
701.533738099435));
#266602=CARTESIAN_POINT('Ctrl Pts',(-14.8994397626301,1.97208806616529,
702.304729294019));
#266603=CARTESIAN_POINT('Ctrl Pts',(-15.0000000000001,0.959664758314061,
702.5));
#266604=CARTESIAN_POINT('Ctrl Pts',(-14.9999999999999,-0.959664758316262,
702.5));
#266605=CARTESIAN_POINT('Ctrl Pts',(-14.8994397626298,-1.9720880661675,
702.304729294019));
#266606=CARTESIAN_POINT('Ctrl Pts',(-14.5369863077958,-3.8155556858589,
701.533738099435));
#266607=CARTESIAN_POINT('Ctrl Pts',(-14.2789995755284,-4.64772502354804,
700.958876694251));
#266608=CARTESIAN_POINT('Ctrl Pts',(-13.7827535066158,-5.9606687109838,
699.645933006816));
#266609=CARTESIAN_POINT('Ctrl Pts',(-13.5089700934546,-6.5342153230227,
698.814367696309));
#266610=CARTESIAN_POINT('Ctrl Pts',(-13.1086907696464,-7.30414188357672,
696.973539509475));
#266611=CARTESIAN_POINT('Ctrl Pts',(-12.990381056766,-7.50000000000103,
695.962288002204));
#266612=CARTESIAN_POINT('Ctrl Pts',(-12.990381056766,-7.50000000000103,
695.));
#266613=CARTESIAN_POINT('',(-160.,-1.08176332053365E-12,702.5));
#266614=CARTESIAN_POINT('',(-160.,-1.08176332053365E-12,702.5));
#266615=CARTESIAN_POINT('Origin',(-160.,-1.08084483543429E-12,695.));
#266616=CARTESIAN_POINT('',(-159.937609420477,6.20654127332979,690.789436448355));
#266617=CARTESIAN_POINT('',(-129.934615416877,5.96286660784587,690.450909781394));
#266618=CARTESIAN_POINT('Ctrl Pts',(-159.937609420477,6.20654127332982,
690.789436448355));
#266619=CARTESIAN_POINT('Ctrl Pts',(-154.948459738842,6.17458452188821,
690.742330901948));
#266620=CARTESIAN_POINT('Ctrl Pts',(-149.926082303016,6.1390213471184,690.691039620133));
#266621=CARTESIAN_POINT('Ctrl Pts',(-139.949152040579,6.05906103115091,
690.579310542064));
#266622=CARTESIAN_POINT('Ctrl Pts',(-134.922635902319,6.0141024887776,690.518068863507));
#266623=CARTESIAN_POINT('Ctrl Pts',(-129.934615416877,5.96286660784588,
690.450909781394));
#266624=CARTESIAN_POINT('',(-129.869812400585,7.23822414349888,696.964207537012));
#266625=CARTESIAN_POINT('Ctrl Pts',(-129.934615416877,5.96286660784597,
690.450909781394));
#266626=CARTESIAN_POINT('Ctrl Pts',(-129.895497332176,6.3198742880004,690.918869103464));
#266627=CARTESIAN_POINT('Ctrl Pts',(-129.861734938059,6.62077691231157,
691.427509497858));
#266628=CARTESIAN_POINT('Ctrl Pts',(-129.813111426559,7.08500706130328,
692.477209818207));
#266629=CARTESIAN_POINT('Ctrl Pts',(-129.797530023073,7.25319087208374,
693.011645223298));
#266630=CARTESIAN_POINT('Ctrl Pts',(-129.785399163032,7.46764113789919,
694.107885119514));
#266631=CARTESIAN_POINT('Ctrl Pts',(-129.788874868863,7.51329980358179,
694.66573759385));
#266632=CARTESIAN_POINT('Ctrl Pts',(-129.814956867898,7.47911407824289,
695.812263009751));
#266633=CARTESIAN_POINT('Ctrl Pts',(-129.838507736136,7.39229580419887,
696.396444104027));
#266634=CARTESIAN_POINT('Ctrl Pts',(-129.869812400585,7.23822414349893,
696.964207537012));
#266635=CARTESIAN_POINT('',(-159.895664541343,7.20669984090177,697.076891283416));
#266636=CARTESIAN_POINT('Ctrl Pts',(-129.869812400585,7.23822414349889,
696.964207537012));
#266637=CARTESIAN_POINT('Ctrl Pts',(-134.859218204142,7.23191213146821,
696.987467684941));
#266638=CARTESIAN_POINT('Ctrl Pts',(-139.89584879553,7.22618364101929,697.008143200778));
#266639=CARTESIAN_POINT('Ctrl Pts',(-149.874856564711,7.21579485641644,
697.045158795903));
#266640=CARTESIAN_POINT('Ctrl Pts',(-154.905389260016,7.21104308929451,
697.061820447619));
#266641=CARTESIAN_POINT('Ctrl Pts',(-159.895664541343,7.20669984090182,
697.076891283416));
#266642=CARTESIAN_POINT('Ctrl Pts',(-159.895664541343,7.2066998409018,697.076891283416));
#266643=CARTESIAN_POINT('Ctrl Pts',(-159.870103993811,7.36226817270387,
696.537077629712));
#266644=CARTESIAN_POINT('Ctrl Pts',(-159.850674352115,7.45675253696311,
695.981314356345));
#266645=CARTESIAN_POINT('Ctrl Pts',(-159.828240589408,7.51820614028886,
694.885484288732));
#266646=CARTESIAN_POINT('Ctrl Pts',(-159.824566877554,7.4908836067602,694.349379238582));
#266647=CARTESIAN_POINT('Ctrl Pts',(-159.832377964382,7.32254333391787,
693.292150424693));
#266648=CARTESIAN_POINT('Ctrl Pts',(-159.843827611085,7.18211047599033,
692.774384904098));
#266649=CARTESIAN_POINT('Ctrl Pts',(-159.880789425704,6.78379176451796,
691.752562621326));
#266650=CARTESIAN_POINT('Ctrl Pts',(-159.906846253054,6.52166889429016,
691.253947329587));
#266651=CARTESIAN_POINT('Ctrl Pts',(-159.937609420477,6.20654127332982,
690.789436448355));
#266652=CARTESIAN_POINT('Origin',(-160.,3.64291929955129E-14,375.));
#266653=CARTESIAN_POINT('',(-15.,0.,382.5));
#266654=CARTESIAN_POINT('',(-15.,3.64291929955129E-14,367.5));
#266655=CARTESIAN_POINT('Ctrl Pts',(-15.,3.55965257270441E-14,382.5));
#266656=CARTESIAN_POINT('Ctrl Pts',(-15.,-0.959664758315123,382.5));
#266657=CARTESIAN_POINT('Ctrl Pts',(-14.8994397626299,-1.97208806616638,
382.304729294019));
#266658=CARTESIAN_POINT('Ctrl Pts',(-14.5369863077961,-3.81555568585776,
381.533738099434));
#266659=CARTESIAN_POINT('Ctrl Pts',(-14.2789995755288,-4.64772502354691,
380.958876694251));
#266660=CARTESIAN_POINT('Ctrl Pts',(-13.7827535066163,-5.96066871098269,
379.645933006816));
#266661=CARTESIAN_POINT('Ctrl Pts',(-13.5089700934551,-6.53421532302163,
378.814367696309));
#266662=CARTESIAN_POINT('Ctrl Pts',(-13.1086907696471,-7.30414188357562,
376.973539509475));
#266663=CARTESIAN_POINT('Ctrl Pts',(-12.9903810567666,-7.49999999999991,
375.962288002204));
#266664=CARTESIAN_POINT('Ctrl Pts',(-12.9903810567666,-7.49999999999991,
375.));
#266665=CARTESIAN_POINT('Ctrl Pts',(-12.9903810567666,-7.49999999999991,
374.037711997797));
#266666=CARTESIAN_POINT('Ctrl Pts',(-13.1086907696471,-7.30414188357562,
373.026460490526));
#266667=CARTESIAN_POINT('Ctrl Pts',(-13.5089700934551,-6.53421532302163,
371.185632303692));
#266668=CARTESIAN_POINT('Ctrl Pts',(-13.7827535066163,-5.96066871098269,
370.354066993185));
#266669=CARTESIAN_POINT('Ctrl Pts',(-14.2789995755288,-4.64772502354691,
369.041123305749));
#266670=CARTESIAN_POINT('Ctrl Pts',(-14.5369863077961,-3.81555568585776,
368.466261900566));
#266671=CARTESIAN_POINT('Ctrl Pts',(-14.8994397626299,-1.97208806616638,
367.695270705982));
#266672=CARTESIAN_POINT('Ctrl Pts',(-15.,-0.959664758315121,367.5));
#266673=CARTESIAN_POINT('Ctrl Pts',(-15.,3.82333054105288E-14,367.5));
#266674=CARTESIAN_POINT('',(-160.,3.55107078961524E-14,382.5));
#266675=CARTESIAN_POINT('',(-160.,3.55107078961524E-14,382.5));
#266676=CARTESIAN_POINT('Origin',(-160.,3.64291929955129E-14,375.));
#266677=CARTESIAN_POINT('Ctrl Pts',(-15.,3.64291929955129E-14,367.5));
#266678=CARTESIAN_POINT('Ctrl Pts',(-15.,0.959664758315196,367.5));
#266679=CARTESIAN_POINT('Ctrl Pts',(-14.8994397626299,1.97208806616645,
367.695270705982));
#266680=CARTESIAN_POINT('Ctrl Pts',(-14.5369863077961,3.81555568585784,
368.466261900566));
#266681=CARTESIAN_POINT('Ctrl Pts',(-14.2789995755287,4.64772502354698,
369.041123305749));
#266682=CARTESIAN_POINT('Ctrl Pts',(-13.7827535066163,5.96066871098276,
370.354066993185));
#266683=CARTESIAN_POINT('Ctrl Pts',(-13.5089700934551,6.5342153230217,371.185632303692));
#266684=CARTESIAN_POINT('Ctrl Pts',(-13.108690769647,7.30414188357569,373.026460490526));
#266685=CARTESIAN_POINT('Ctrl Pts',(-12.9903810567666,7.49999999999999,
374.037711997797));
#266686=CARTESIAN_POINT('Ctrl Pts',(-12.9903810567666,7.49999999999999,
375.962288002204));
#266687=CARTESIAN_POINT('Ctrl Pts',(-13.108690769647,7.30414188357565,376.973539509475));
#266688=CARTESIAN_POINT('Ctrl Pts',(-13.5089700934551,6.53421532302163,
378.814367696309));
#266689=CARTESIAN_POINT('Ctrl Pts',(-13.7827535066163,5.96066871098276,
379.645933006816));
#266690=CARTESIAN_POINT('Ctrl Pts',(-14.2789995755287,4.64772502354698,
380.958876694251));
#266691=CARTESIAN_POINT('Ctrl Pts',(-14.5369863077961,3.81555568585784,
381.533738099434));
#266692=CARTESIAN_POINT('Ctrl Pts',(-14.8994397626299,1.97208806616646,
382.304729294019));
#266693=CARTESIAN_POINT('Ctrl Pts',(-15.,0.959664758315197,382.5));
#266694=CARTESIAN_POINT('Ctrl Pts',(-15.,3.7470027081099E-14,382.5));
#266695=CARTESIAN_POINT('',(-159.937609420477,-6.20654127333065,379.210563551645));
#266696=CARTESIAN_POINT('',(-129.934615416877,-5.96286660784699,379.549090218607));
#266697=CARTESIAN_POINT('Ctrl Pts',(-159.937609420477,-6.20654127333066,
379.210563551645));
#266698=CARTESIAN_POINT('Ctrl Pts',(-154.948459738633,-6.17458452188773,
379.257669098055));
#266699=CARTESIAN_POINT('Ctrl Pts',(-149.926082302936,-6.13902134711856,
379.308960379868));
#266700=CARTESIAN_POINT('Ctrl Pts',(-139.949152040766,-6.05906103115325,
379.420689457935));
#266701=CARTESIAN_POINT('Ctrl Pts',(-134.92263590239,-6.01410248877932,
379.481931136493));
#266702=CARTESIAN_POINT('Ctrl Pts',(-129.934615416877,-5.9628666078469,
379.549090218607));
#266703=CARTESIAN_POINT('',(-129.869812400585,-7.23822414349998,373.035792462989));
#266704=CARTESIAN_POINT('Ctrl Pts',(-129.934615416877,-5.962866607847,379.549090218607));
#266705=CARTESIAN_POINT('Ctrl Pts',(-129.895497332176,-6.3198742880009,
379.081130896537));
#266706=CARTESIAN_POINT('Ctrl Pts',(-129.861734938059,-6.62077691231253,
378.572490502143));
#266707=CARTESIAN_POINT('Ctrl Pts',(-129.813111426559,-7.085007061304,377.522790181794));
#266708=CARTESIAN_POINT('Ctrl Pts',(-129.797530023073,-7.25319087208486,
376.988354776703));
#266709=CARTESIAN_POINT('Ctrl Pts',(-129.785399163032,-7.46764113790054,
375.892114880486));
#266710=CARTESIAN_POINT('Ctrl Pts',(-129.788874868863,-7.51329980358274,
375.334262406149));
#266711=CARTESIAN_POINT('Ctrl Pts',(-129.814956867898,-7.47911407824392,
374.18773699025));
#266712=CARTESIAN_POINT('Ctrl Pts',(-129.838507736136,-7.39229580420003,
373.603555895973));
#266713=CARTESIAN_POINT('Ctrl Pts',(-129.869812400585,-7.23822414349998,
373.035792462989));
#266714=CARTESIAN_POINT('',(-159.895664541343,-7.20669984090295,372.923108716584));
#266715=CARTESIAN_POINT('Ctrl Pts',(-129.869812400585,-7.23822414349996,
373.035792462989));
#266716=CARTESIAN_POINT('Ctrl Pts',(-134.859218204139,-7.23191213146929,
373.01253231506));
#266717=CARTESIAN_POINT('Ctrl Pts',(-139.89584879552,-7.22618364102027,
372.991856799222));
#266718=CARTESIAN_POINT('Ctrl Pts',(-149.874856564524,-7.21579485641762,
372.954841204098));
#266719=CARTESIAN_POINT('Ctrl Pts',(-154.905389259528,-7.21104308929605,
372.938179552383));
#266720=CARTESIAN_POINT('Ctrl Pts',(-159.895664541343,-7.20669984090294,
372.923108716584));
#266721=CARTESIAN_POINT('Ctrl Pts',(-159.895664541343,-7.20669984090288,
372.923108716584));
#266722=CARTESIAN_POINT('Ctrl Pts',(-159.870103993811,-7.3622681727049,
373.462922370288));
#266723=CARTESIAN_POINT('Ctrl Pts',(-159.850674352115,-7.45675253696417,
374.018685643656));
#266724=CARTESIAN_POINT('Ctrl Pts',(-159.828240589408,-7.51820614028992,
375.114515711268));
#266725=CARTESIAN_POINT('Ctrl Pts',(-159.824566877554,-7.49088360676129,
375.650620761418));
#266726=CARTESIAN_POINT('Ctrl Pts',(-159.832377964382,-7.32254333391888,
376.707849575308));
#266727=CARTESIAN_POINT('Ctrl Pts',(-159.843827611085,-7.18211047599103,
377.225615095903));
#266728=CARTESIAN_POINT('Ctrl Pts',(-159.880789425704,-6.78379176451862,
378.247437378675));
#266729=CARTESIAN_POINT('Ctrl Pts',(-159.906846253054,-6.52166889429029,
378.746052670415));
#266730=CARTESIAN_POINT('Ctrl Pts',(-159.937609420477,-6.20654127333069,
379.210563551645));
#266731=CARTESIAN_POINT('Origin',(160.,-1.08084483543429E-12,695.));
#266732=CARTESIAN_POINT('',(15.,-1.072837590456E-12,702.5));
#266733=CARTESIAN_POINT('',(15.,-1.08280927416198E-12,687.5));
#266734=CARTESIAN_POINT('Ctrl Pts',(15.,-1.07913677993565E-12,702.5));
#266735=CARTESIAN_POINT('Ctrl Pts',(14.9999999999999,-0.959664758316259,
702.5));
#266736=CARTESIAN_POINT('Ctrl Pts',(14.8994397626298,-1.97208806616749,
702.304729294019));
#266737=CARTESIAN_POINT('Ctrl Pts',(14.5369863077958,-3.8155556858589,701.533738099435));
#266738=CARTESIAN_POINT('Ctrl Pts',(14.2789995755284,-4.64772502354804,
700.958876694251));
#266739=CARTESIAN_POINT('Ctrl Pts',(13.7827535066158,-5.9606687109838,699.645933006816));
#266740=CARTESIAN_POINT('Ctrl Pts',(13.5089700934546,-6.5342153230227,698.814367696309));
#266741=CARTESIAN_POINT('Ctrl Pts',(13.1086907696464,-7.30414188357672,
696.973539509475));
#266742=CARTESIAN_POINT('Ctrl Pts',(12.990381056766,-7.50000000000103,695.962288002204));
#266743=CARTESIAN_POINT('Ctrl Pts',(12.990381056766,-7.50000000000103,694.037711997797));
#266744=CARTESIAN_POINT('Ctrl Pts',(13.1086907696464,-7.30414188357672,
693.026460490526));
#266745=CARTESIAN_POINT('Ctrl Pts',(13.5089700934546,-6.5342153230227,691.185632303692));
#266746=CARTESIAN_POINT('Ctrl Pts',(13.7827535066158,-5.9606687109838,690.354066993185));
#266747=CARTESIAN_POINT('Ctrl Pts',(14.2789995755284,-4.64772502354804,
689.041123305749));
#266748=CARTESIAN_POINT('Ctrl Pts',(14.5369863077958,-3.8155556858589,688.466261900566));
#266749=CARTESIAN_POINT('Ctrl Pts',(14.8994397626298,-1.97208806616749,
687.695270705982));
#266750=CARTESIAN_POINT('Ctrl Pts',(14.9999999999999,-0.959664758316263,
687.5));
#266751=CARTESIAN_POINT('Ctrl Pts',(15.,-1.08385522779031E-12,687.5));
#266752=CARTESIAN_POINT('',(160.,-1.08176332053365E-12,687.5));
#266753=CARTESIAN_POINT('',(160.,-1.08176332053365E-12,687.5));
#266754=CARTESIAN_POINT('Origin',(160.,-1.08084483543429E-12,695.));
#266755=CARTESIAN_POINT('Ctrl Pts',(15.,-1.0845491171807E-12,687.5));
#266756=CARTESIAN_POINT('Ctrl Pts',(15.0000000000001,0.959664758314058,
687.5));
#266757=CARTESIAN_POINT('Ctrl Pts',(14.8994397626301,1.97208806616529,687.695270705982));
#266758=CARTESIAN_POINT('Ctrl Pts',(14.5369863077964,3.81555568585669,688.466261900566));
#266759=CARTESIAN_POINT('Ctrl Pts',(14.2789995755291,4.64772502354583,689.041123305749));
#266760=CARTESIAN_POINT('Ctrl Pts',(13.7827535066168,5.96066871098163,690.354066993185));
#266761=CARTESIAN_POINT('Ctrl Pts',(13.5089700934557,6.53421532302054,691.185632303692));
#266762=CARTESIAN_POINT('Ctrl Pts',(13.1086907696476,7.30414188357456,693.026460490526));
#266763=CARTESIAN_POINT('Ctrl Pts',(12.9903810567672,7.49999999999887,694.037711997797));
#266764=CARTESIAN_POINT('Ctrl Pts',(12.9903810567672,7.49999999999887,695.));
#266765=CARTESIAN_POINT('Ctrl Pts',(12.9903810567672,7.49999999999887,695.962288002204));
#266766=CARTESIAN_POINT('Ctrl Pts',(13.1086907696476,7.30414188357456,696.973539509475));
#266767=CARTESIAN_POINT('Ctrl Pts',(13.5089700934557,6.53421532302054,698.814367696309));
#266768=CARTESIAN_POINT('Ctrl Pts',(13.7827535066168,5.96066871098163,699.645933006816));
#266769=CARTESIAN_POINT('Ctrl Pts',(14.2789995755291,4.64772502354583,700.958876694252));
#266770=CARTESIAN_POINT('Ctrl Pts',(14.5369863077964,3.81555568585669,701.533738099435));
#266771=CARTESIAN_POINT('Ctrl Pts',(14.8994397626301,1.97208806616529,702.304729294019));
#266772=CARTESIAN_POINT('Ctrl Pts',(15.0000000000001,0.959664758314059,
702.5));
#266773=CARTESIAN_POINT('Ctrl Pts',(15.,-1.08468789505878E-12,702.5));
#266774=CARTESIAN_POINT('',(159.937609420477,-6.20654127333164,690.789436448355));
#266775=CARTESIAN_POINT('',(159.895664541343,-7.20669984090406,697.076891283416));
#266776=CARTESIAN_POINT('Ctrl Pts',(159.937609420477,-6.20654127333163,
690.789436448355));
#266777=CARTESIAN_POINT('Ctrl Pts',(159.906834643176,-6.52178782200797,
691.254122633859));
#266778=CARTESIAN_POINT('Ctrl Pts',(159.880769856038,-6.78398922241133,
691.752938404992));
#266779=CARTESIAN_POINT('Ctrl Pts',(159.843804521963,-7.18237209951024,
692.775180680853));
#266780=CARTESIAN_POINT('Ctrl Pts',(159.832358861788,-7.32279367879376,
693.293160677924));
#266781=CARTESIAN_POINT('Ctrl Pts',(159.824570869009,-7.49095925222209,
694.350417431358));
#266782=CARTESIAN_POINT('Ctrl Pts',(159.82825204698,-7.51820444472976,694.8863221477));
#266783=CARTESIAN_POINT('Ctrl Pts',(159.850688911066,-7.45668143260721,
695.981732982313));
#266784=CARTESIAN_POINT('Ctrl Pts',(159.870113636375,-7.36220948547999,
696.537281271196));
#266785=CARTESIAN_POINT('Ctrl Pts',(159.895664541343,-7.2066998409041,697.076891283416));
#266786=CARTESIAN_POINT('',(129.934615416877,-5.96286660784778,690.450909781393));
#266787=CARTESIAN_POINT('Ctrl Pts',(129.934615416877,-5.96286660784775,
690.450909781393));
#266788=CARTESIAN_POINT('Ctrl Pts',(134.922636022201,-6.01410249001088,
690.518068865121));
#266789=CARTESIAN_POINT('Ctrl Pts',(139.949152283076,-6.05906103332323,
690.579310545018));
#266790=CARTESIAN_POINT('Ctrl Pts',(149.926082545137,-6.13902134883337,
690.691039622605));
#266791=CARTESIAN_POINT('Ctrl Pts',(154.948459858584,-6.17458452265701,
690.742330903078));
#266792=CARTESIAN_POINT('Ctrl Pts',(159.937609420477,-6.20654127333165,
690.789436448355));
#266793=CARTESIAN_POINT('',(129.869812400585,-7.23822414350117,696.964207537011));
#266794=CARTESIAN_POINT('Ctrl Pts',(129.869812400585,-7.23822414350118,
696.964207537011));
#266795=CARTESIAN_POINT('Ctrl Pts',(129.838465947162,-7.3925014763172,696.39568618978));
#266796=CARTESIAN_POINT('Ctrl Pts',(129.814894504108,-7.4793450036484,695.810706203687));
#266797=CARTESIAN_POINT('Ctrl Pts',(129.788829961956,-7.5132167397021,694.662636602978));
#266798=CARTESIAN_POINT('Ctrl Pts',(129.785389515462,-7.46723834799325,
694.104054596373));
#266799=CARTESIAN_POINT('Ctrl Pts',(129.797623339578,-7.25211847571097,
693.007946909601));
#266800=CARTESIAN_POINT('Ctrl Pts',(129.813220504589,-7.08391429791459,
692.474308019488));
#266801=CARTESIAN_POINT('Ctrl Pts',(129.861824504594,-6.61997620179538,
691.426155633436));
#266802=CARTESIAN_POINT('Ctrl Pts',(129.895549481156,-6.31939835503028,
690.918245258983));
#266803=CARTESIAN_POINT('Ctrl Pts',(129.934615416877,-5.96286660784783,
690.450909781393));
#266804=CARTESIAN_POINT('Ctrl Pts',(159.895664541343,-7.20669984090407,
697.076891283416));
#266805=CARTESIAN_POINT('Ctrl Pts',(154.905389419006,-7.21104308915838,
697.061820448099));
#266806=CARTESIAN_POINT('Ctrl Pts',(149.874856855226,-7.21579485612801,
697.04515879687));
#266807=CARTESIAN_POINT('Ctrl Pts',(139.895849065302,-7.22618364069772,
697.008143201895));
#266808=CARTESIAN_POINT('Ctrl Pts',(134.859218339046,-7.2319121312998,696.98746768557));
#266809=CARTESIAN_POINT('Ctrl Pts',(129.869812400585,-7.23822414350115,
696.964207537012));
#266810=CARTESIAN_POINT('Origin',(160.,3.64291929955129E-14,375.));
#266811=CARTESIAN_POINT('',(15.,1.83697019872103E-15,382.5));
#266812=CARTESIAN_POINT('',(15.,3.64291929155445E-14,367.5));
#266813=CARTESIAN_POINT('Ctrl Pts',(15.,3.64291929955129E-14,382.5));
#266814=CARTESIAN_POINT('Ctrl Pts',(15.,-0.959664758315123,382.5));
#266815=CARTESIAN_POINT('Ctrl Pts',(14.8994397626299,-1.97208806616638,
382.304729294019));
#266816=CARTESIAN_POINT('Ctrl Pts',(14.5369863077961,-3.81555568585776,
381.533738099434));
#266817=CARTESIAN_POINT('Ctrl Pts',(14.2789995755288,-4.64772502354691,
380.958876694251));
#266818=CARTESIAN_POINT('Ctrl Pts',(13.7827535066163,-5.96066871098269,
379.645933006816));
#266819=CARTESIAN_POINT('Ctrl Pts',(13.5089700934552,-6.53421532302156,
378.814367696309));
#266820=CARTESIAN_POINT('Ctrl Pts',(13.1086907696471,-7.30414188357558,
376.973539509475));
#266821=CARTESIAN_POINT('Ctrl Pts',(12.9903810567666,-7.49999999999991,
375.962288002204));
#266822=CARTESIAN_POINT('Ctrl Pts',(12.9903810567666,-7.49999999999991,
374.037711997797));
#266823=CARTESIAN_POINT('Ctrl Pts',(13.1086907696471,-7.30414188357562,
373.026460490526));
#266824=CARTESIAN_POINT('Ctrl Pts',(13.5089700934551,-6.53421532302163,
371.185632303692));
#266825=CARTESIAN_POINT('Ctrl Pts',(13.7827535066163,-5.96066871098269,
370.354066993185));
#266826=CARTESIAN_POINT('Ctrl Pts',(14.2789995755288,-4.64772502354691,
369.041123305749));
#266827=CARTESIAN_POINT('Ctrl Pts',(14.5369863077961,-3.81555568585776,
368.466261900566));
#266828=CARTESIAN_POINT('Ctrl Pts',(14.8994397626299,-1.97208806616638,
367.695270705982));
#266829=CARTESIAN_POINT('Ctrl Pts',(15.,-0.959664758315123,367.5));
#266830=CARTESIAN_POINT('Ctrl Pts',(15.,3.60822483003176E-14,367.5));
#266831=CARTESIAN_POINT('',(160.,3.55107078961524E-14,367.5));
#266832=CARTESIAN_POINT('',(160.,3.55107078961524E-14,367.5));
#266833=CARTESIAN_POINT('Origin',(160.,3.64291929955129E-14,375.));
#266834=CARTESIAN_POINT('Ctrl Pts',(15.,3.73312492030209E-14,367.5));
#266835=CARTESIAN_POINT('Ctrl Pts',(15.,0.959664758315197,367.5));
#266836=CARTESIAN_POINT('Ctrl Pts',(14.8994397626299,1.97208806616646,367.695270705982));
#266837=CARTESIAN_POINT('Ctrl Pts',(14.5369863077961,3.81555568585784,368.466261900566));
#266838=CARTESIAN_POINT('Ctrl Pts',(14.2789995755287,4.64772502354698,369.041123305749));
#266839=CARTESIAN_POINT('Ctrl Pts',(13.7827535066163,5.96066871098276,370.354066993185));
#266840=CARTESIAN_POINT('Ctrl Pts',(13.5089700934551,6.5342153230217,371.185632303692));
#266841=CARTESIAN_POINT('Ctrl Pts',(13.108690769647,7.30414188357569,373.026460490526));
#266842=CARTESIAN_POINT('Ctrl Pts',(12.9903810567666,7.49999999999999,374.037711997797));
#266843=CARTESIAN_POINT('Ctrl Pts',(12.9903810567666,7.49999999999999,375.));
#266844=CARTESIAN_POINT('Ctrl Pts',(12.9903810567666,7.49999999999999,375.962288002204));
#266845=CARTESIAN_POINT('Ctrl Pts',(13.108690769647,7.30414188357569,376.973539509475));
#266846=CARTESIAN_POINT('Ctrl Pts',(13.5089700934551,6.5342153230217,378.814367696309));
#266847=CARTESIAN_POINT('Ctrl Pts',(13.7827535066163,5.96066871098276,379.645933006816));
#266848=CARTESIAN_POINT('Ctrl Pts',(14.2789995755287,4.64772502354698,380.958876694251));
#266849=CARTESIAN_POINT('Ctrl Pts',(14.5369863077961,3.81555568585778,381.533738099435));
#266850=CARTESIAN_POINT('Ctrl Pts',(14.8994397626299,1.97208806616639,382.304729294019));
#266851=CARTESIAN_POINT('Ctrl Pts',(15.,0.959664758315195,382.5));
#266852=CARTESIAN_POINT('Ctrl Pts',(15.,3.46944695195361E-14,382.5));
#266853=CARTESIAN_POINT('',(129.869812400585,7.23822414350007,373.035792462989));
#266854=CARTESIAN_POINT('',(129.934615416877,5.96286660784696,379.549090218607));
#266855=CARTESIAN_POINT('Ctrl Pts',(129.869812400585,7.23822414350003,373.035792462989));
#266856=CARTESIAN_POINT('Ctrl Pts',(129.838465947162,7.39250147631606,373.60431381022));
#266857=CARTESIAN_POINT('Ctrl Pts',(129.814894504108,7.47934500364732,374.189293796313));
#266858=CARTESIAN_POINT('Ctrl Pts',(129.788829961956,7.51321673970108,375.337363397022));
#266859=CARTESIAN_POINT('Ctrl Pts',(129.785389515462,7.4672383479923,375.895945403626));
#266860=CARTESIAN_POINT('Ctrl Pts',(129.797623339578,7.25211847571004,376.9920530904));
#266861=CARTESIAN_POINT('Ctrl Pts',(129.813220504589,7.08391429791338,377.525691980513));
#266862=CARTESIAN_POINT('Ctrl Pts',(129.861824504594,6.61997620179469,378.573844366563));
#266863=CARTESIAN_POINT('Ctrl Pts',(129.895549481156,6.31939835502988,379.081754741017));
#266864=CARTESIAN_POINT('Ctrl Pts',(129.934615416877,5.96286660784708,379.549090218607));
#266865=CARTESIAN_POINT('',(159.895664541343,7.20669984090294,372.923108716584));
#266866=CARTESIAN_POINT('Ctrl Pts',(159.895664541343,7.20669984090292,372.923108716584));
#266867=CARTESIAN_POINT('Ctrl Pts',(154.905389418371,7.21104308915779,372.938179551903));
#266868=CARTESIAN_POINT('Ctrl Pts',(149.874856854973,7.21579485612699,372.954841203131));
#266869=CARTESIAN_POINT('Ctrl Pts',(139.895849065092,7.22618364069654,372.991856798107));
#266870=CARTESIAN_POINT('Ctrl Pts',(134.85921833898,7.23191213129876,373.012532314431));
#266871=CARTESIAN_POINT('Ctrl Pts',(129.869812400585,7.23822414350003,373.035792462989));
#266872=CARTESIAN_POINT('',(159.937609420477,6.20654127333073,379.210563551645));
#266873=CARTESIAN_POINT('Ctrl Pts',(159.937609420477,6.20654127333081,379.210563551645));
#266874=CARTESIAN_POINT('Ctrl Pts',(159.906834643176,6.52178782200678,378.745877366142));
#266875=CARTESIAN_POINT('Ctrl Pts',(159.880769856038,6.78398922241033,378.247061595009));
#266876=CARTESIAN_POINT('Ctrl Pts',(159.843804521963,7.18237209951068,377.224819319144));
#266877=CARTESIAN_POINT('Ctrl Pts',(159.832358861788,7.32279367879272,376.706839322075));
#266878=CARTESIAN_POINT('Ctrl Pts',(159.824570869009,7.49095925222048,375.649582568643));
#266879=CARTESIAN_POINT('Ctrl Pts',(159.82825204698,7.51820444472885,375.113677852303));
#266880=CARTESIAN_POINT('Ctrl Pts',(159.850688911066,7.45668143260609,374.018267017687));
#266881=CARTESIAN_POINT('Ctrl Pts',(159.870113636375,7.36220948547902,373.462718728805));
#266882=CARTESIAN_POINT('Ctrl Pts',(159.895664541343,7.20669984090294,372.923108716584));
#266883=CARTESIAN_POINT('Ctrl Pts',(129.934615416877,5.96286660784695,379.549090218607));
#266884=CARTESIAN_POINT('Ctrl Pts',(134.922636022203,6.01410249001008,379.48193113488));
#266885=CARTESIAN_POINT('Ctrl Pts',(139.949152283082,6.05906103332244,379.420689454983));
#266886=CARTESIAN_POINT('Ctrl Pts',(149.926082545118,6.13902134883237,379.308960377395));
#266887=CARTESIAN_POINT('Ctrl Pts',(154.948459858534,6.17458452265582,379.257669096923));
#266888=CARTESIAN_POINT('Ctrl Pts',(159.937609420477,6.20654127333077,379.210563551645));
#266889=CARTESIAN_POINT('Origin',(160.,3.64291929955129E-14,535.));
#266890=CARTESIAN_POINT('',(15.,1.83697027874617E-15,527.5));
#266891=CARTESIAN_POINT('',(15.,1.64287496604076E-14,542.5));
#266892=CARTESIAN_POINT('Ctrl Pts',(15.,2.99760216648792E-14,527.5));
#266893=CARTESIAN_POINT('Ctrl Pts',(15.,-0.959664758315129,527.5));
#266894=CARTESIAN_POINT('Ctrl Pts',(14.8994397626299,-1.97208806616637,
527.695270705982));
#266895=CARTESIAN_POINT('Ctrl Pts',(14.5369863077961,-3.81555568585775,
528.466261900566));
#266896=CARTESIAN_POINT('Ctrl Pts',(14.2789995755288,-4.64772502354691,
529.041123305749));
#266897=CARTESIAN_POINT('Ctrl Pts',(13.7827535066163,-5.96066871098269,
530.354066993185));
#266898=CARTESIAN_POINT('Ctrl Pts',(13.5089700934551,-6.53421532302163,
531.185632303692));
#266899=CARTESIAN_POINT('Ctrl Pts',(13.1086907696471,-7.30414188357563,
533.026460490526));
#266900=CARTESIAN_POINT('Ctrl Pts',(12.9903810567666,-7.49999999999991,
534.037711997796));
#266901=CARTESIAN_POINT('Ctrl Pts',(12.9903810567666,-7.49999999999991,
535.962288002204));
#266902=CARTESIAN_POINT('Ctrl Pts',(13.1086907696471,-7.3041418835756,536.973539509475));
#266903=CARTESIAN_POINT('Ctrl Pts',(13.5089700934552,-6.53421532302157,
538.814367696309));
#266904=CARTESIAN_POINT('Ctrl Pts',(13.7827535066163,-5.96066871098269,
539.645933006816));
#266905=CARTESIAN_POINT('Ctrl Pts',(14.2789995755288,-4.64772502354691,
540.958876694251));
#266906=CARTESIAN_POINT('Ctrl Pts',(14.5369863077961,-3.81555568585775,
541.533738099434));
#266907=CARTESIAN_POINT('Ctrl Pts',(14.8994397626299,-1.97208806616637,
542.304729294019));
#266908=CARTESIAN_POINT('Ctrl Pts',(15.,-0.959664758315122,542.5));
#266909=CARTESIAN_POINT('Ctrl Pts',(15.,3.77475828372553E-14,542.5));
#266910=CARTESIAN_POINT('',(160.,3.55107078961524E-14,527.5));
#266911=CARTESIAN_POINT('',(160.,3.55107078961524E-14,527.5));
#266912=CARTESIAN_POINT('Origin',(160.,3.64291929955129E-14,535.));
#266913=CARTESIAN_POINT('Ctrl Pts',(15.,3.44169137633799E-14,542.5));
#266914=CARTESIAN_POINT('Ctrl Pts',(15.,0.959664758315194,542.5));
#266915=CARTESIAN_POINT('Ctrl Pts',(14.8994397626299,1.97208806616644,542.304729294019));
#266916=CARTESIAN_POINT('Ctrl Pts',(14.5369863077961,3.81555568585783,541.533738099434));
#266917=CARTESIAN_POINT('Ctrl Pts',(14.2789995755287,4.64772502354698,540.958876694251));
#266918=CARTESIAN_POINT('Ctrl Pts',(13.7827535066163,5.96066871098276,539.645933006816));
#266919=CARTESIAN_POINT('Ctrl Pts',(13.5089700934551,6.53421532302171,538.814367696309));
#266920=CARTESIAN_POINT('Ctrl Pts',(13.108690769647,7.30414188357571,536.973539509475));
#266921=CARTESIAN_POINT('Ctrl Pts',(12.9903810567666,7.49999999999999,535.962288002204));
#266922=CARTESIAN_POINT('Ctrl Pts',(12.9903810567666,7.49999999999999,535.));
#266923=CARTESIAN_POINT('Ctrl Pts',(12.9903810567666,7.49999999999999,534.037711997796));
#266924=CARTESIAN_POINT('Ctrl Pts',(13.108690769647,7.30414188357571,533.026460490526));
#266925=CARTESIAN_POINT('Ctrl Pts',(13.5089700934551,6.53421532302171,531.185632303692));
#266926=CARTESIAN_POINT('Ctrl Pts',(13.7827535066163,5.96066871098276,530.354066993185));
#266927=CARTESIAN_POINT('Ctrl Pts',(14.2789995755287,4.64772502354698,529.041123305749));
#266928=CARTESIAN_POINT('Ctrl Pts',(14.5369863077961,3.81555568585783,528.466261900566));
#266929=CARTESIAN_POINT('Ctrl Pts',(14.8994397626299,1.97208806616644,527.695270705982));
#266930=CARTESIAN_POINT('Ctrl Pts',(15.,0.959664758315196,527.5));
#266931=CARTESIAN_POINT('Ctrl Pts',(15.,3.71924713249427E-14,527.5));
#266932=CARTESIAN_POINT('',(129.869812400585,-7.23822414349995,536.964207537012));
#266933=CARTESIAN_POINT('',(159.895664541343,-7.20669984090288,537.076891283416));
#266934=CARTESIAN_POINT('Ctrl Pts',(129.869812400585,-7.23822414349994,
536.964207537012));
#266935=CARTESIAN_POINT('Ctrl Pts',(134.859218204053,-7.23191213146938,
536.98746768494));
#266936=CARTESIAN_POINT('Ctrl Pts',(139.895848795289,-7.22618364102058,
537.008143200777));
#266937=CARTESIAN_POINT('Ctrl Pts',(149.874856564741,-7.21579485641745,
537.045158795903));
#266938=CARTESIAN_POINT('Ctrl Pts',(154.905389260097,-7.21104308929549,
537.061820447619));
#266939=CARTESIAN_POINT('Ctrl Pts',(159.895664541343,-7.20669984090287,
537.076891283416));
#266940=CARTESIAN_POINT('',(159.937609420477,-6.20654127333069,530.789436448355));
#266941=CARTESIAN_POINT('Ctrl Pts',(159.895664541343,-7.20669984090287,
537.076891283416));
#266942=CARTESIAN_POINT('Ctrl Pts',(159.870103993811,-7.36226817270497,
536.537077629712));
#266943=CARTESIAN_POINT('Ctrl Pts',(159.850674352115,-7.45675253696416,
535.981314356344));
#266944=CARTESIAN_POINT('Ctrl Pts',(159.828240589408,-7.51820614028994,
534.885484288732));
#266945=CARTESIAN_POINT('Ctrl Pts',(159.824566877554,-7.4908836067612,534.349379238582));
#266946=CARTESIAN_POINT('Ctrl Pts',(159.832377964382,-7.32254333391886,
533.292150424692));
#266947=CARTESIAN_POINT('Ctrl Pts',(159.843827611085,-7.18211047599137,
532.774384904098));
#266948=CARTESIAN_POINT('Ctrl Pts',(159.880789425704,-6.78379176451867,
531.752562621325));
#266949=CARTESIAN_POINT('Ctrl Pts',(159.906846253054,-6.52166889429031,
531.253947329586));
#266950=CARTESIAN_POINT('Ctrl Pts',(159.937609420477,-6.20654127333076,
530.789436448355));
#266951=CARTESIAN_POINT('',(129.934615416877,-5.96286660784692,530.450909781393));
#266952=CARTESIAN_POINT('Ctrl Pts',(159.937609420477,-6.20654127333072,
530.789436448355));
#266953=CARTESIAN_POINT('Ctrl Pts',(154.948459738742,-6.17458452188848,
530.742330901947));
#266954=CARTESIAN_POINT('Ctrl Pts',(149.926082302978,-6.13902134711897,
530.691039620133));
#266955=CARTESIAN_POINT('Ctrl Pts',(139.949152040648,-6.05906103115236,
530.579310542064));
#266956=CARTESIAN_POINT('Ctrl Pts',(134.922635902346,-6.0141024887789,530.518068863507));
#266957=CARTESIAN_POINT('Ctrl Pts',(129.934615416877,-5.96286660784692,
530.450909781393));
#266958=CARTESIAN_POINT('Ctrl Pts',(129.934615416877,-5.96286660784692,
530.450909781393));
#266959=CARTESIAN_POINT('Ctrl Pts',(129.895497332176,-6.3198742880018,530.918869103465));
#266960=CARTESIAN_POINT('Ctrl Pts',(129.861734938059,-6.62077691231277,
531.427509497859));
#266961=CARTESIAN_POINT('Ctrl Pts',(129.813111426559,-7.0850070613043,532.477209818207));
#266962=CARTESIAN_POINT('Ctrl Pts',(129.797530023073,-7.25319087208485,
533.011645223299));
#266963=CARTESIAN_POINT('Ctrl Pts',(129.785399163032,-7.46764113790021,
534.107885119514));
#266964=CARTESIAN_POINT('Ctrl Pts',(129.788874868863,-7.51329980358284,
534.66573759385));
#266965=CARTESIAN_POINT('Ctrl Pts',(129.814956867898,-7.47911407824392,
535.812263009751));
#266966=CARTESIAN_POINT('Ctrl Pts',(129.838507736136,-7.39229580419984,
536.396444104028));
#266967=CARTESIAN_POINT('Ctrl Pts',(129.869812400585,-7.23822414349995,
536.964207537012));
#266968=CARTESIAN_POINT('',(159.937609420477,6.20654127333082,539.210563551645));
#266969=CARTESIAN_POINT('',(159.895664541343,7.20669984090288,532.923108716584));
#266970=CARTESIAN_POINT('Ctrl Pts',(159.937609420477,6.20654127333076,539.210563551645));
#266971=CARTESIAN_POINT('Ctrl Pts',(159.906834643176,6.52178782200697,538.745877366142));
#266972=CARTESIAN_POINT('Ctrl Pts',(159.880769856038,6.78398922241032,538.247061595009));
#266973=CARTESIAN_POINT('Ctrl Pts',(159.843804521963,7.18237209950917,537.224819319147));
#266974=CARTESIAN_POINT('Ctrl Pts',(159.832358861788,7.32279367879273,536.706839322077));
#266975=CARTESIAN_POINT('Ctrl Pts',(159.824570869009,7.49095925222104,535.649582568642));
#266976=CARTESIAN_POINT('Ctrl Pts',(159.82825204698,7.51820444472875,535.113677852301));
#266977=CARTESIAN_POINT('Ctrl Pts',(159.850688911066,7.45668143260613,534.018267017687));
#266978=CARTESIAN_POINT('Ctrl Pts',(159.870113636375,7.36220948547888,533.462718728804));
#266979=CARTESIAN_POINT('Ctrl Pts',(159.895664541343,7.20669984090294,532.923108716584));
#266980=CARTESIAN_POINT('',(129.934615416877,5.96286660784701,539.549090218607));
#266981=CARTESIAN_POINT('Ctrl Pts',(129.934615416877,5.96286660784688,539.549090218607));
#266982=CARTESIAN_POINT('Ctrl Pts',(134.922636022207,6.01410249001005,539.48193113488));
#266983=CARTESIAN_POINT('Ctrl Pts',(139.949152283091,6.05906103332251,539.420689454982));
#266984=CARTESIAN_POINT('Ctrl Pts',(149.926082545092,6.13902134883217,539.308960377395));
#266985=CARTESIAN_POINT('Ctrl Pts',(154.948459858468,6.17458452265536,539.257669096923));
#266986=CARTESIAN_POINT('Ctrl Pts',(159.937609420477,6.20654127333074,539.210563551645));
#266987=CARTESIAN_POINT('',(129.869812400585,7.23822414350004,533.035792462989));
#266988=CARTESIAN_POINT('Ctrl Pts',(129.869812400585,7.23822414350011,533.035792462989));
#266989=CARTESIAN_POINT('Ctrl Pts',(129.838465947162,7.39250147631596,533.60431381022));
#266990=CARTESIAN_POINT('Ctrl Pts',(129.814894504108,7.4793450036473,534.189293796313));
#266991=CARTESIAN_POINT('Ctrl Pts',(129.788829961956,7.51321673970109,535.337363397021));
#266992=CARTESIAN_POINT('Ctrl Pts',(129.785389515462,7.46723834799247,535.895945403626));
#266993=CARTESIAN_POINT('Ctrl Pts',(129.797623339578,7.2521184757102,536.992053090399));
#266994=CARTESIAN_POINT('Ctrl Pts',(129.813220504589,7.08391429791336,537.525691980513));
#266995=CARTESIAN_POINT('Ctrl Pts',(129.861824504594,6.61997620179435,538.573844366564));
#266996=CARTESIAN_POINT('Ctrl Pts',(129.895549481156,6.31939835502854,539.081754741018));
#266997=CARTESIAN_POINT('Ctrl Pts',(129.934615416877,5.96286660784697,539.549090218607));
#266998=CARTESIAN_POINT('Ctrl Pts',(159.895664541343,7.20669984090296,532.923108716584));
#266999=CARTESIAN_POINT('Ctrl Pts',(154.905389417752,7.21104308915837,532.938179551905));
#267000=CARTESIAN_POINT('Ctrl Pts',(149.87485685474,7.21579485612754,532.954841203132));
#267001=CARTESIAN_POINT('Ctrl Pts',(139.895849065202,7.22618364069673,532.991856798106));
#267002=CARTESIAN_POINT('Ctrl Pts',(134.859218339019,7.23191213129876,533.012532314431));
#267003=CARTESIAN_POINT('Ctrl Pts',(129.869812400585,7.23822414350007,533.035792462989));
#267004=CARTESIAN_POINT('Origin',(-160.,3.64291929955129E-14,535.));
#267005=CARTESIAN_POINT('',(-15.,4.80562938205009E-14,527.5));
#267006=CARTESIAN_POINT('',(-15.,3.70454790009383E-14,542.5));
#267007=CARTESIAN_POINT('Ctrl Pts',(-15.,3.1641356201817E-14,527.5));
#267008=CARTESIAN_POINT('Ctrl Pts',(-15.,-0.959664758315127,527.5));
#267009=CARTESIAN_POINT('Ctrl Pts',(-14.8994397626299,-1.97208806616637,
527.695270705982));
#267010=CARTESIAN_POINT('Ctrl Pts',(-14.5369863077961,-3.81555568585775,
528.466261900566));
#267011=CARTESIAN_POINT('Ctrl Pts',(-14.2789995755288,-4.64772502354691,
529.041123305749));
#267012=CARTESIAN_POINT('Ctrl Pts',(-13.7827535066163,-5.96066871098269,
530.354066993185));
#267013=CARTESIAN_POINT('Ctrl Pts',(-13.5089700934551,-6.53421532302163,
531.185632303692));
#267014=CARTESIAN_POINT('Ctrl Pts',(-13.1086907696471,-7.30414188357563,
533.026460490526));
#267015=CARTESIAN_POINT('Ctrl Pts',(-12.9903810567666,-7.49999999999991,
534.037711997796));
#267016=CARTESIAN_POINT('Ctrl Pts',(-12.9903810567666,-7.49999999999991,
535.));
#267017=CARTESIAN_POINT('Ctrl Pts',(-12.9903810567666,-7.49999999999991,
535.962288002204));
#267018=CARTESIAN_POINT('Ctrl Pts',(-13.1086907696471,-7.30414188357563,
536.973539509475));
#267019=CARTESIAN_POINT('Ctrl Pts',(-13.5089700934551,-6.53421532302163,
538.814367696309));
#267020=CARTESIAN_POINT('Ctrl Pts',(-13.7827535066163,-5.96066871098269,
539.645933006816));
#267021=CARTESIAN_POINT('Ctrl Pts',(-14.2789995755288,-4.64772502354691,
540.958876694251));
#267022=CARTESIAN_POINT('Ctrl Pts',(-14.5369863077961,-3.81555568585775,
541.533738099434));
#267023=CARTESIAN_POINT('Ctrl Pts',(-14.8994397626299,-1.97208806616637,
542.304729294019));
#267024=CARTESIAN_POINT('Ctrl Pts',(-15.,-0.959664758315135,542.5));
#267025=CARTESIAN_POINT('Ctrl Pts',(-15.,2.44249065417534E-14,542.5));
#267026=CARTESIAN_POINT('',(-160.,3.55107078961524E-14,542.5));
#267027=CARTESIAN_POINT('',(-160.,3.55107078961524E-14,542.5));
#267028=CARTESIAN_POINT('Origin',(-160.,3.64291929955129E-14,535.));
#267029=CARTESIAN_POINT('Ctrl Pts',(-15.,3.56659146660832E-14,542.5));
#267030=CARTESIAN_POINT('Ctrl Pts',(-15.,0.959664758315195,542.5));
#267031=CARTESIAN_POINT('Ctrl Pts',(-14.8994397626299,1.97208806616644,
542.304729294019));
#267032=CARTESIAN_POINT('Ctrl Pts',(-14.5369863077961,3.81555568585783,
541.533738099434));
#267033=CARTESIAN_POINT('Ctrl Pts',(-14.2789995755287,4.64772502354698,
540.958876694251));
#267034=CARTESIAN_POINT('Ctrl Pts',(-13.7827535066163,5.96066871098276,
539.645933006816));
#267035=CARTESIAN_POINT('Ctrl Pts',(-13.5089700934551,6.53421532302164,
538.814367696309));
#267036=CARTESIAN_POINT('Ctrl Pts',(-13.108690769647,7.30414188357567,536.973539509475));
#267037=CARTESIAN_POINT('Ctrl Pts',(-12.9903810567666,7.49999999999999,
535.962288002204));
#267038=CARTESIAN_POINT('Ctrl Pts',(-12.9903810567666,7.49999999999999,
534.037711997797));
#267039=CARTESIAN_POINT('Ctrl Pts',(-13.108690769647,7.30414188357571,533.026460490526));
#267040=CARTESIAN_POINT('Ctrl Pts',(-13.5089700934551,6.53421532302171,
531.185632303692));
#267041=CARTESIAN_POINT('Ctrl Pts',(-13.7827535066163,5.96066871098276,
530.354066993185));
#267042=CARTESIAN_POINT('Ctrl Pts',(-14.2789995755287,4.64772502354698,
529.041123305749));
#267043=CARTESIAN_POINT('Ctrl Pts',(-14.5369863077961,3.81555568585786,
528.466261900566));
#267044=CARTESIAN_POINT('Ctrl Pts',(-14.8994397626299,1.97208806616648,
527.695270705982));
#267045=CARTESIAN_POINT('Ctrl Pts',(-15.,0.959664758315195,527.5));
#267046=CARTESIAN_POINT('Ctrl Pts',(-15.,3.5527136788005E-14,527.5));
#267047=CARTESIAN_POINT('',(-159.937609420477,-6.20654127333065,539.210563551645));
#267048=CARTESIAN_POINT('',(-129.934615416877,-5.96286660784691,539.549090218607));
#267049=CARTESIAN_POINT('Ctrl Pts',(-159.937609420477,-6.20654127333064,
539.210563551645));
#267050=CARTESIAN_POINT('Ctrl Pts',(-154.948459738632,-6.1745845218877,
539.257669098055));
#267051=CARTESIAN_POINT('Ctrl Pts',(-149.926082302935,-6.13902134711855,
539.308960379868));
#267052=CARTESIAN_POINT('Ctrl Pts',(-139.949152040724,-6.05906103115291,
539.420689457936));
#267053=CARTESIAN_POINT('Ctrl Pts',(-134.922635902374,-6.01410248877916,
539.481931136493));
#267054=CARTESIAN_POINT('Ctrl Pts',(-129.934615416877,-5.9628666078469,
539.549090218607));
#267055=CARTESIAN_POINT('',(-129.869812400585,-7.23822414349998,533.035792462989));
#267056=CARTESIAN_POINT('Ctrl Pts',(-129.934615416877,-5.96286660784695,
539.549090218607));
#267057=CARTESIAN_POINT('Ctrl Pts',(-129.895497332176,-6.31987428800097,
539.081130896537));
#267058=CARTESIAN_POINT('Ctrl Pts',(-129.861734938059,-6.6207769123125,
538.572490502143));
#267059=CARTESIAN_POINT('Ctrl Pts',(-129.813111426559,-7.0850070613043,
537.522790181794));
#267060=CARTESIAN_POINT('Ctrl Pts',(-129.797530023073,-7.25319087208481,
536.988354776702));
#267061=CARTESIAN_POINT('Ctrl Pts',(-129.785399163032,-7.4676411379003,
535.892114880487));
#267062=CARTESIAN_POINT('Ctrl Pts',(-129.788874868863,-7.51329980358279,
535.33426240615));
#267063=CARTESIAN_POINT('Ctrl Pts',(-129.814956867898,-7.47911407824396,
534.18773699025));
#267064=CARTESIAN_POINT('Ctrl Pts',(-129.838507736136,-7.39229580420002,
533.603555895973));
#267065=CARTESIAN_POINT('Ctrl Pts',(-129.869812400585,-7.23822414349999,
533.035792462989));
#267066=CARTESIAN_POINT('',(-159.895664541343,-7.20669984090296,532.923108716584));
#267067=CARTESIAN_POINT('Ctrl Pts',(-129.869812400585,-7.23822414349999,
533.035792462989));
#267068=CARTESIAN_POINT('Ctrl Pts',(-134.85921820423,-7.23191213146921,
533.012532315059));
#267069=CARTESIAN_POINT('Ctrl Pts',(-139.895848795771,-7.22618364102021,
532.991856799222));
#267070=CARTESIAN_POINT('Ctrl Pts',(-149.874856564472,-7.21579485641788,
532.954841204099));
#267071=CARTESIAN_POINT('Ctrl Pts',(-154.905389259385,-7.2110430892962,
532.938179552383));
#267072=CARTESIAN_POINT('Ctrl Pts',(-159.895664541343,-7.20669984090297,
532.923108716584));
#267073=CARTESIAN_POINT('Ctrl Pts',(-159.895664541343,-7.20669984090294,
532.923108716584));
#267074=CARTESIAN_POINT('Ctrl Pts',(-159.870103993811,-7.36226817270499,
533.462922370289));
#267075=CARTESIAN_POINT('Ctrl Pts',(-159.850674352115,-7.45675253696417,
534.018685643656));
#267076=CARTESIAN_POINT('Ctrl Pts',(-159.828240589408,-7.51820614028982,
535.114515711267));
#267077=CARTESIAN_POINT('Ctrl Pts',(-159.824566877554,-7.49088360676147,
535.650620761418));
#267078=CARTESIAN_POINT('Ctrl Pts',(-159.832377964382,-7.3225433339189,
536.707849575309));
#267079=CARTESIAN_POINT('Ctrl Pts',(-159.843827611085,-7.18211047599091,
537.225615095904));
#267080=CARTESIAN_POINT('Ctrl Pts',(-159.880789425704,-6.78379176451848,
538.247437378676));
#267081=CARTESIAN_POINT('Ctrl Pts',(-159.906846253054,-6.52166889428979,
538.746052670415));
#267082=CARTESIAN_POINT('Ctrl Pts',(-159.937609420477,-6.20654127333069,
539.210563551645));
#267083=CARTESIAN_POINT('',(-129.869812400585,7.23822414350004,536.964207537012));
#267084=CARTESIAN_POINT('',(-129.934615416877,5.96286660784693,530.450909781393));
#267085=CARTESIAN_POINT('Ctrl Pts',(-129.869812400585,7.23822414350001,
536.964207537012));
#267086=CARTESIAN_POINT('Ctrl Pts',(-129.838465947162,7.39250147631553,
536.395686189782));
#267087=CARTESIAN_POINT('Ctrl Pts',(-129.814894504108,7.47934500364728,
535.810706203688));
#267088=CARTESIAN_POINT('Ctrl Pts',(-129.788829961956,7.51321673970107,
534.662636602979));
#267089=CARTESIAN_POINT('Ctrl Pts',(-129.785389515462,7.4672383479923,534.104054596374));
#267090=CARTESIAN_POINT('Ctrl Pts',(-129.797623339578,7.25211847571004,
533.007946909601));
#267091=CARTESIAN_POINT('Ctrl Pts',(-129.813220504589,7.08391429791342,
532.474308019487));
#267092=CARTESIAN_POINT('Ctrl Pts',(-129.861824504594,6.61997620179486,
531.426155633437));
#267093=CARTESIAN_POINT('Ctrl Pts',(-129.895549481156,6.31939835503053,
530.918245258985));
#267094=CARTESIAN_POINT('Ctrl Pts',(-129.934615416877,5.96286660784708,
530.450909781394));
#267095=CARTESIAN_POINT('',(-159.895664541343,7.20669984090294,537.076891283416));
#267096=CARTESIAN_POINT('Ctrl Pts',(-159.895664541343,7.20669984090292,
537.076891283416));
#267097=CARTESIAN_POINT('Ctrl Pts',(-154.905389418126,7.21104308915801,
537.061820448097));
#267098=CARTESIAN_POINT('Ctrl Pts',(-149.874856854883,7.2157948561274,537.045158796869));
#267099=CARTESIAN_POINT('Ctrl Pts',(-139.895849065273,7.22618364069668,
537.008143201894));
#267100=CARTESIAN_POINT('Ctrl Pts',(-134.859218339044,7.23191213129869,
536.98746768557));
#267101=CARTESIAN_POINT('Ctrl Pts',(-129.869812400585,7.23822414350004,
536.964207537012));
#267102=CARTESIAN_POINT('',(-159.937609420477,6.2065412733309,530.789436448355));
#267103=CARTESIAN_POINT('Ctrl Pts',(-159.937609420477,6.20654127333087,
530.789436448355));
#267104=CARTESIAN_POINT('Ctrl Pts',(-159.906834643176,6.52178782200749,
531.254122633859));
#267105=CARTESIAN_POINT('Ctrl Pts',(-159.880769856038,6.78398922241062,
531.752938404992));
#267106=CARTESIAN_POINT('Ctrl Pts',(-159.843804521963,7.18237209950937,
532.775180680854));
#267107=CARTESIAN_POINT('Ctrl Pts',(-159.832358861788,7.32279367879286,
533.293160677924));
#267108=CARTESIAN_POINT('Ctrl Pts',(-159.824570869009,7.49095925222109,
534.350417431359));
#267109=CARTESIAN_POINT('Ctrl Pts',(-159.82825204698,7.51820444472876,534.8863221477));
#267110=CARTESIAN_POINT('Ctrl Pts',(-159.850688911066,7.45668143260605,
535.981732982314));
#267111=CARTESIAN_POINT('Ctrl Pts',(-159.870113636375,7.36220948547839,
536.537281271198));
#267112=CARTESIAN_POINT('Ctrl Pts',(-159.895664541343,7.20669984090291,
537.076891283416));
#267113=CARTESIAN_POINT('Ctrl Pts',(-129.934615416877,5.96286660784702,
530.450909781394));
#267114=CARTESIAN_POINT('Ctrl Pts',(-134.922636022182,6.01410249000995,
530.51806886512));
#267115=CARTESIAN_POINT('Ctrl Pts',(-139.949152283026,6.05906103332206,
530.579310545017));
#267116=CARTESIAN_POINT('Ctrl Pts',(-149.926082545109,6.13902134883239,
530.691039622605));
#267117=CARTESIAN_POINT('Ctrl Pts',(-154.948459858512,6.17458452265583,
530.742330903078));
#267118=CARTESIAN_POINT('Ctrl Pts',(-159.937609420477,6.20654127333093,
530.789436448355));
#267119=CARTESIAN_POINT('Origin',(0.,0.,695.));
#267120=CARTESIAN_POINT('Origin',(0.,0.,367.5));
#267121=CARTESIAN_POINT('',(15.,-1.83697019872103E-15,695.));
#267122=CARTESIAN_POINT('',(15.,-1.83697019872103E-15,695.));
#267123=CARTESIAN_POINT('',(15.,-1.83697019872103E-15,848.));
#267124=CARTESIAN_POINT('',(15.,-1.83697019872103E-15,695.));
#267125=CARTESIAN_POINT('Origin',(0.,0.,848.));
#267126=CARTESIAN_POINT('Origin',(0.,0.,367.5));
#267127=CARTESIAN_POINT('Ctrl Pts',(-130.,4.30813900827773,697.537703348572));
#267128=CARTESIAN_POINT('Ctrl Pts',(-129.660942106811,14.5393608954781,
695.537703348572));
#267129=CARTESIAN_POINT('Ctrl Pts',(-127.725542856289,24.591579123369,693.537703348572));
#267130=CARTESIAN_POINT('Ctrl Pts',(-125.790143605767,34.6437973512599,
691.537703348572));
#267131=CARTESIAN_POINT('Ctrl Pts',(-122.306058950683,44.269492945671,689.537703348572));
#267132=CARTESIAN_POINT('Ctrl Pts',(-118.821974295598,53.8951885400822,
687.537703348572));
#267133=CARTESIAN_POINT('Ctrl Pts',(-113.874993963172,62.8573449296269,
685.537703348572));
#267134=CARTESIAN_POINT('Ctrl Pts',(-108.928013630747,71.8195013191717,
683.537703348572));
#267135=CARTESIAN_POINT('Ctrl Pts',(-102.639948694852,79.8974404698478,
681.537703348572));
#267136=CARTESIAN_POINT('Ctrl Pts',(-96.3518837589562,87.9753796205239,
679.537703348572));
#267137=CARTESIAN_POINT('Ctrl Pts',(-88.8775672472037,94.9701958612987,
677.537703348572));
#267138=CARTESIAN_POINT('Ctrl Pts',(-81.4032507354512,101.965012102073,
675.537703348572));
#267139=CARTESIAN_POINT('Ctrl Pts',(-72.9267251261952,107.704469842635,
673.537703348572));
#267140=CARTESIAN_POINT('Ctrl Pts',(-64.4501995169392,113.443927583196,
671.537703348572));
#267141=CARTESIAN_POINT('Ctrl Pts',(-55.1801850026552,117.786702325803,
669.537703348572));
#267142=CARTESIAN_POINT('Ctrl Pts',(-45.9101704883713,122.12947706841,667.537703348572));
#267143=CARTESIAN_POINT('Ctrl Pts',(-36.0749255918153,124.968635286057,
665.537703348572));
#267144=CARTESIAN_POINT('Ctrl Pts',(-26.2396806952593,127.807793503704,
663.537703348572));
#267145=CARTESIAN_POINT('Ctrl Pts',(-16.081381787091,129.073425698447,661.537703348572));
#267146=CARTESIAN_POINT('Ctrl Pts',(-5.92308287892268,130.339057893189,
659.537703348572));
#267147=CARTESIAN_POINT('Ctrl Pts',(4.30813900827772,130.,657.537703348572));
#267148=CARTESIAN_POINT('Ctrl Pts',(14.5393608954781,129.660942106811,655.537703348572));
#267149=CARTESIAN_POINT('Ctrl Pts',(24.591579123369,127.725542856289,653.537703348572));
#267150=CARTESIAN_POINT('Ctrl Pts',(34.6437973512599,125.790143605767,651.537703348572));
#267151=CARTESIAN_POINT('Ctrl Pts',(44.269492945671,122.306058950683,649.537703348572));
#267152=CARTESIAN_POINT('Ctrl Pts',(53.8951885400822,118.821974295598,647.537703348572));
#267153=CARTESIAN_POINT('Ctrl Pts',(62.8573449296269,113.874993963172,645.537703348572));
#267154=CARTESIAN_POINT('Ctrl Pts',(71.8195013191717,108.928013630747,643.537703348572));
#267155=CARTESIAN_POINT('Ctrl Pts',(79.8974404698478,102.639948694852,641.537703348572));
#267156=CARTESIAN_POINT('Ctrl Pts',(87.9753796205239,96.3518837589562,639.537703348572));
#267157=CARTESIAN_POINT('Ctrl Pts',(94.9701958612986,88.8775672472037,637.537703348572));
#267158=CARTESIAN_POINT('Ctrl Pts',(101.965012102073,81.4032507354512,635.537703348572));
#267159=CARTESIAN_POINT('Ctrl Pts',(107.704469842635,72.9267251261952,633.537703348572));
#267160=CARTESIAN_POINT('Ctrl Pts',(113.443927583196,64.4501995169392,631.537703348572));
#267161=CARTESIAN_POINT('Ctrl Pts',(117.786702325803,55.1801850026552,629.537703348572));
#267162=CARTESIAN_POINT('Ctrl Pts',(122.12947706841,45.9101704883713,627.537703348572));
#267163=CARTESIAN_POINT('Ctrl Pts',(124.968635286057,36.0749255918153,625.537703348572));
#267164=CARTESIAN_POINT('Ctrl Pts',(127.807793503704,26.2396806952593,623.537703348572));
#267165=CARTESIAN_POINT('Ctrl Pts',(129.073425698447,16.081381787091,621.537703348572));
#267166=CARTESIAN_POINT('Ctrl Pts',(130.339057893189,5.92308287892268,619.537703348572));
#267167=CARTESIAN_POINT('Ctrl Pts',(130.,-4.30813900827772,617.537703348572));
#267168=CARTESIAN_POINT('Ctrl Pts',(129.660942106811,-14.5393608954781,
615.537703348572));
#267169=CARTESIAN_POINT('Ctrl Pts',(127.725542856289,-24.591579123369,613.537703348572));
#267170=CARTESIAN_POINT('Ctrl Pts',(125.790143605767,-34.6437973512599,
611.537703348572));
#267171=CARTESIAN_POINT('Ctrl Pts',(122.306058950683,-44.269492945671,609.537703348572));
#267172=CARTESIAN_POINT('Ctrl Pts',(118.821974295598,-53.8951885400822,
607.537703348572));
#267173=CARTESIAN_POINT('Ctrl Pts',(113.874993963172,-62.8573449296269,
605.537703348572));
#267174=CARTESIAN_POINT('Ctrl Pts',(108.928013630747,-71.8195013191717,
603.537703348572));
#267175=CARTESIAN_POINT('Ctrl Pts',(102.639948694852,-79.8974404698478,
601.537703348572));
#267176=CARTESIAN_POINT('Ctrl Pts',(96.3518837589563,-87.9753796205239,
599.537703348572));
#267177=CARTESIAN_POINT('Ctrl Pts',(88.8775672472037,-94.9701958612986,
597.537703348572));
#267178=CARTESIAN_POINT('Ctrl Pts',(81.4032507354513,-101.965012102073,
595.537703348572));
#267179=CARTESIAN_POINT('Ctrl Pts',(72.9267251261952,-107.704469842635,
593.537703348572));
#267180=CARTESIAN_POINT('Ctrl Pts',(64.4501995169392,-113.443927583196,
591.537703348572));
#267181=CARTESIAN_POINT('Ctrl Pts',(55.1801850026552,-117.786702325803,
589.537703348572));
#267182=CARTESIAN_POINT('Ctrl Pts',(45.9101704883713,-122.12947706841,587.537703348572));
#267183=CARTESIAN_POINT('Ctrl Pts',(36.0749255918153,-124.968635286057,
585.537703348572));
#267184=CARTESIAN_POINT('Ctrl Pts',(26.2396806952593,-127.807793503704,
583.537703348572));
#267185=CARTESIAN_POINT('Ctrl Pts',(16.081381787091,-129.073425698447,581.537703348572));
#267186=CARTESIAN_POINT('Ctrl Pts',(5.92308287892275,-130.339057893189,
579.537703348572));
#267187=CARTESIAN_POINT('Ctrl Pts',(-4.30813900827771,-130.,577.537703348572));
#267188=CARTESIAN_POINT('Ctrl Pts',(-14.5393608954782,-129.660942106811,
575.537703348572));
#267189=CARTESIAN_POINT('Ctrl Pts',(-24.591579123369,-127.725542856289,
573.537703348572));
#267190=CARTESIAN_POINT('Ctrl Pts',(-34.6437973512598,-125.790143605767,
571.537703348572));
#267191=CARTESIAN_POINT('Ctrl Pts',(-44.269492945671,-122.306058950683,
569.537703348572));
#267192=CARTESIAN_POINT('Ctrl Pts',(-53.8951885400822,-118.821974295598,
567.537703348572));
#267193=CARTESIAN_POINT('Ctrl Pts',(-62.8573449296269,-113.874993963172,
565.537703348572));
#267194=CARTESIAN_POINT('Ctrl Pts',(-71.8195013191717,-108.928013630747,
563.537703348572));
#267195=CARTESIAN_POINT('Ctrl Pts',(-79.8974404698478,-102.639948694852,
561.537703348572));
#267196=CARTESIAN_POINT('Ctrl Pts',(-87.975379620524,-96.3518837589562,
559.537703348572));
#267197=CARTESIAN_POINT('Ctrl Pts',(-94.9701958612986,-88.8775672472037,
557.537703348572));
#267198=CARTESIAN_POINT('Ctrl Pts',(-101.965012102073,-81.4032507354513,
555.537703348572));
#267199=CARTESIAN_POINT('Ctrl Pts',(-107.704469842635,-72.9267251261952,
553.537703348572));
#267200=CARTESIAN_POINT('Ctrl Pts',(-113.443927583196,-64.4501995169392,
551.537703348572));
#267201=CARTESIAN_POINT('Ctrl Pts',(-117.786702325803,-55.1801850026553,
549.537703348572));
#267202=CARTESIAN_POINT('Ctrl Pts',(-122.12947706841,-45.9101704883713,
547.537703348572));
#267203=CARTESIAN_POINT('Ctrl Pts',(-124.968635286057,-36.0749255918153,
545.537703348572));
#267204=CARTESIAN_POINT('Ctrl Pts',(-127.807793503704,-26.2396806952593,
543.537703348572));
#267205=CARTESIAN_POINT('Ctrl Pts',(-129.073425698447,-16.081381787091,
541.537703348572));
#267206=CARTESIAN_POINT('Ctrl Pts',(-130.339057893189,-5.92308287892275,
539.537703348572));
#267207=CARTESIAN_POINT('Ctrl Pts',(-130.,4.30813900827773,537.537703348572));
#267208=CARTESIAN_POINT('Ctrl Pts',(-130.,-4.30813900827845,692.462296651428));
#267209=CARTESIAN_POINT('Ctrl Pts',(-130.339057893189,5.92308287892195,
690.462296651428));
#267210=CARTESIAN_POINT('Ctrl Pts',(-129.073425698447,16.0813817870903,
688.462296651428));
#267211=CARTESIAN_POINT('Ctrl Pts',(-127.807793503705,26.2396806952586,
686.462296651429));
#267212=CARTESIAN_POINT('Ctrl Pts',(-124.968635286058,36.0749255918146,
684.462296651428));
#267213=CARTESIAN_POINT('Ctrl Pts',(-122.129477068411,45.9101704883706,
682.462296651429));
#267214=CARTESIAN_POINT('Ctrl Pts',(-117.786702325804,55.1801850026546,
680.462296651428));
#267215=CARTESIAN_POINT('Ctrl Pts',(-113.443927583196,64.4501995169386,
678.462296651428));
#267216=CARTESIAN_POINT('Ctrl Pts',(-107.704469842635,72.9267251261946,
676.462296651429));
#267217=CARTESIAN_POINT('Ctrl Pts',(-101.965012102074,81.4032507354507,
674.462296651429));
#267218=CARTESIAN_POINT('Ctrl Pts',(-94.9701958612992,88.8775672472032,
672.462296651428));
#267219=CARTESIAN_POINT('Ctrl Pts',(-87.9753796205245,96.3518837589558,
670.462296651429));
#267220=CARTESIAN_POINT('Ctrl Pts',(-79.8974404698484,102.639948694851,
668.462296651428));
#267221=CARTESIAN_POINT('Ctrl Pts',(-71.8195013191724,108.928013630747,
666.462296651428));
#267222=CARTESIAN_POINT('Ctrl Pts',(-62.8573449296276,113.874993963172,
664.462296651428));
#267223=CARTESIAN_POINT('Ctrl Pts',(-53.8951885400828,118.821974295598,
662.462296651429));
#267224=CARTESIAN_POINT('Ctrl Pts',(-44.2694929456717,122.306058950682,
660.462296651428));
#267225=CARTESIAN_POINT('Ctrl Pts',(-34.6437973512606,125.790143605767,
658.462296651428));
#267226=CARTESIAN_POINT('Ctrl Pts',(-24.5915791233697,127.725542856289,
656.462296651429));
#267227=CARTESIAN_POINT('Ctrl Pts',(-14.5393608954789,129.660942106811,
654.462296651428));
#267228=CARTESIAN_POINT('Ctrl Pts',(-4.30813900827846,130.,652.462296651428));
#267229=CARTESIAN_POINT('Ctrl Pts',(5.92308287892194,130.339057893189,650.462296651429));
#267230=CARTESIAN_POINT('Ctrl Pts',(16.0813817870903,129.073425698447,648.462296651428));
#267231=CARTESIAN_POINT('Ctrl Pts',(26.2396806952586,127.807793503705,646.462296651428));
#267232=CARTESIAN_POINT('Ctrl Pts',(36.0749255918146,124.968635286058,644.462296651428));
#267233=CARTESIAN_POINT('Ctrl Pts',(45.9101704883706,122.129477068411,642.462296651428));
#267234=CARTESIAN_POINT('Ctrl Pts',(55.1801850026546,117.786702325804,640.462296651428));
#267235=CARTESIAN_POINT('Ctrl Pts',(64.4501995169386,113.443927583196,638.462296651429));
#267236=CARTESIAN_POINT('Ctrl Pts',(72.9267251261946,107.704469842635,636.462296651428));
#267237=CARTESIAN_POINT('Ctrl Pts',(81.4032507354506,101.965012102074,634.462296651428));
#267238=CARTESIAN_POINT('Ctrl Pts',(88.8775672472032,94.9701958612992,632.462296651428));
#267239=CARTESIAN_POINT('Ctrl Pts',(96.3518837589558,87.9753796205245,630.462296651428));
#267240=CARTESIAN_POINT('Ctrl Pts',(102.639948694851,79.8974404698484,628.462296651428));
#267241=CARTESIAN_POINT('Ctrl Pts',(108.928013630747,71.8195013191724,626.462296651429));
#267242=CARTESIAN_POINT('Ctrl Pts',(113.874993963172,62.8573449296276,624.462296651428));
#267243=CARTESIAN_POINT('Ctrl Pts',(118.821974295598,53.8951885400829,622.462296651428));
#267244=CARTESIAN_POINT('Ctrl Pts',(122.306058950682,44.2694929456717,620.462296651428));
#267245=CARTESIAN_POINT('Ctrl Pts',(125.790143605767,34.6437973512606,618.462296651428));
#267246=CARTESIAN_POINT('Ctrl Pts',(127.725542856289,24.5915791233698,616.462296651428));
#267247=CARTESIAN_POINT('Ctrl Pts',(129.660942106811,14.5393608954789,614.462296651429));
#267248=CARTESIAN_POINT('Ctrl Pts',(130.,4.30813900827846,612.462296651428));
#267249=CARTESIAN_POINT('Ctrl Pts',(130.339057893189,-5.92308287892194,
610.462296651428));
#267250=CARTESIAN_POINT('Ctrl Pts',(129.073425698447,-16.0813817870903,
608.462296651428));
#267251=CARTESIAN_POINT('Ctrl Pts',(127.807793503705,-26.2396806952586,
606.462296651428));
#267252=CARTESIAN_POINT('Ctrl Pts',(124.968635286058,-36.0749255918146,
604.462296651428));
#267253=CARTESIAN_POINT('Ctrl Pts',(122.129477068411,-45.9101704883706,
602.462296651429));
#267254=CARTESIAN_POINT('Ctrl Pts',(117.786702325804,-55.1801850026546,
600.462296651428));
#267255=CARTESIAN_POINT('Ctrl Pts',(113.443927583196,-64.4501995169386,
598.462296651428));
#267256=CARTESIAN_POINT('Ctrl Pts',(107.704469842635,-72.9267251261946,
596.462296651428));
#267257=CARTESIAN_POINT('Ctrl Pts',(101.965012102074,-81.4032507354506,
594.462296651428));
#267258=CARTESIAN_POINT('Ctrl Pts',(94.9701958612992,-88.8775672472032,
592.462296651428));
#267259=CARTESIAN_POINT('Ctrl Pts',(87.9753796205246,-96.3518837589557,
590.462296651429));
#267260=CARTESIAN_POINT('Ctrl Pts',(79.8974404698484,-102.639948694851,
588.462296651428));
#267261=CARTESIAN_POINT('Ctrl Pts',(71.8195013191723,-108.928013630747,
586.462296651428));
#267262=CARTESIAN_POINT('Ctrl Pts',(62.8573449296276,-113.874993963172,
584.462296651428));
#267263=CARTESIAN_POINT('Ctrl Pts',(53.8951885400829,-118.821974295598,
582.462296651428));
#267264=CARTESIAN_POINT('Ctrl Pts',(44.2694929456717,-122.306058950682,
580.462296651428));
#267265=CARTESIAN_POINT('Ctrl Pts',(34.6437973512606,-125.790143605767,
578.462296651429));
#267266=CARTESIAN_POINT('Ctrl Pts',(24.5915791233698,-127.725542856289,
576.462296651428));
#267267=CARTESIAN_POINT('Ctrl Pts',(14.5393608954789,-129.660942106811,
574.462296651428));
#267268=CARTESIAN_POINT('Ctrl Pts',(4.30813900827847,-130.,572.462296651428));
#267269=CARTESIAN_POINT('Ctrl Pts',(-5.92308287892199,-130.339057893189,
570.462296651428));
#267270=CARTESIAN_POINT('Ctrl Pts',(-16.0813817870903,-129.073425698447,
568.462296651428));
#267271=CARTESIAN_POINT('Ctrl Pts',(-26.2396806952585,-127.807793503705,
566.462296651429));
#267272=CARTESIAN_POINT('Ctrl Pts',(-36.0749255918146,-124.968635286058,
564.462296651428));
#267273=CARTESIAN_POINT('Ctrl Pts',(-45.9101704883706,-122.129477068411,
562.462296651428));
#267274=CARTESIAN_POINT('Ctrl Pts',(-55.1801850026546,-117.786702325804,
560.462296651428));
#267275=CARTESIAN_POINT('Ctrl Pts',(-64.4501995169385,-113.443927583197,
558.462296651429));
#267276=CARTESIAN_POINT('Ctrl Pts',(-72.9267251261946,-107.704469842635,
556.462296651428));
#267277=CARTESIAN_POINT('Ctrl Pts',(-81.4032507354507,-101.965012102074,
554.462296651429));
#267278=CARTESIAN_POINT('Ctrl Pts',(-88.8775672472032,-94.9701958612992,
552.462296651428));
#267279=CARTESIAN_POINT('Ctrl Pts',(-96.3518837589557,-87.9753796205246,
550.462296651428));
#267280=CARTESIAN_POINT('Ctrl Pts',(-102.639948694851,-79.8974404698484,
548.462296651428));
#267281=CARTESIAN_POINT('Ctrl Pts',(-108.928013630747,-71.8195013191723,
546.462296651429));
#267282=CARTESIAN_POINT('Ctrl Pts',(-113.874993963172,-62.8573449296276,
544.462296651428));
#267283=CARTESIAN_POINT('Ctrl Pts',(-118.821974295598,-53.8951885400829,
542.462296651429));
#267284=CARTESIAN_POINT('Ctrl Pts',(-122.306058950682,-44.2694929456718,
540.462296651428));
#267285=CARTESIAN_POINT('Ctrl Pts',(-125.790143605767,-34.6437973512606,
538.462296651428));
#267286=CARTESIAN_POINT('Ctrl Pts',(-127.725542856289,-24.5915791233698,
536.462296651428));
#267287=CARTESIAN_POINT('Ctrl Pts',(-129.660942106811,-14.5393608954789,
534.462296651429));
#267288=CARTESIAN_POINT('Ctrl Pts',(-130.,-4.30813900827845,532.462296651428));
#267289=CARTESIAN_POINT('Ctrl Pts',(-129.934615416877,5.96286660784587,
690.450909781394));
#267290=CARTESIAN_POINT('Ctrl Pts',(-129.701667605591,11.038945994198,689.455068342531));
#267291=CARTESIAN_POINT('Ctrl Pts',(-129.073425698447,16.0813817870903,
688.462296651428));
#267292=CARTESIAN_POINT('Ctrl Pts',(-127.807793503705,26.2396806952586,
686.462296651429));
#267293=CARTESIAN_POINT('Ctrl Pts',(-124.968635286058,36.0749255918146,
684.462296651428));
#267294=CARTESIAN_POINT('Ctrl Pts',(-122.129477068411,45.9101704883706,
682.462296651429));
#267295=CARTESIAN_POINT('Ctrl Pts',(-117.786702325804,55.1801850026546,
680.462296651428));
#267296=CARTESIAN_POINT('Ctrl Pts',(-113.443927583196,64.4501995169386,
678.462296651428));
#267297=CARTESIAN_POINT('Ctrl Pts',(-107.704469842635,72.9267251261946,
676.462296651429));
#267298=CARTESIAN_POINT('Ctrl Pts',(-101.965012102074,81.4032507354507,
674.462296651429));
#267299=CARTESIAN_POINT('Ctrl Pts',(-94.9701958612992,88.8775672472032,
672.462296651428));
#267300=CARTESIAN_POINT('Ctrl Pts',(-87.9753796205245,96.3518837589558,
670.462296651429));
#267301=CARTESIAN_POINT('Ctrl Pts',(-79.8974404698484,102.639948694851,
668.462296651428));
#267302=CARTESIAN_POINT('Ctrl Pts',(-71.8195013191724,108.928013630747,
666.462296651429));
#267303=CARTESIAN_POINT('Ctrl Pts',(-62.8573449296276,113.874993963172,
664.462296651428));
#267304=CARTESIAN_POINT('Ctrl Pts',(-53.8951885400828,118.821974295598,
662.462296651429));
#267305=CARTESIAN_POINT('Ctrl Pts',(-44.2694929456717,122.306058950682,
660.462296651428));
#267306=CARTESIAN_POINT('Ctrl Pts',(-34.6437973512606,125.790143605767,
658.462296651429));
#267307=CARTESIAN_POINT('Ctrl Pts',(-24.5915791233697,127.725542856289,
656.462296651429));
#267308=CARTESIAN_POINT('Ctrl Pts',(-14.5393608954789,129.660942106811,
654.462296651428));
#267309=CARTESIAN_POINT('Ctrl Pts',(-4.30813900827846,130.,652.462296651428));
#267310=CARTESIAN_POINT('Ctrl Pts',(5.92308287892194,130.339057893189,650.462296651429));
#267311=CARTESIAN_POINT('Ctrl Pts',(16.0813817870903,129.073425698447,648.462296651428));
#267312=CARTESIAN_POINT('Ctrl Pts',(26.2396806952586,127.807793503705,646.462296651429));
#267313=CARTESIAN_POINT('Ctrl Pts',(36.0749255918146,124.968635286058,644.462296651428));
#267314=CARTESIAN_POINT('Ctrl Pts',(45.9101704883706,122.129477068411,642.462296651428));
#267315=CARTESIAN_POINT('Ctrl Pts',(55.1801850026546,117.786702325804,640.462296651428));
#267316=CARTESIAN_POINT('Ctrl Pts',(64.4501995169386,113.443927583196,638.462296651428));
#267317=CARTESIAN_POINT('Ctrl Pts',(72.9267251261946,107.704469842635,636.462296651428));
#267318=CARTESIAN_POINT('Ctrl Pts',(81.4032507354506,101.965012102074,634.462296651428));
#267319=CARTESIAN_POINT('Ctrl Pts',(88.8775672472032,94.9701958612992,632.462296651428));
#267320=CARTESIAN_POINT('Ctrl Pts',(96.3518837589558,87.9753796205245,630.462296651428));
#267321=CARTESIAN_POINT('Ctrl Pts',(102.639948694851,79.8974404698484,628.462296651428));
#267322=CARTESIAN_POINT('Ctrl Pts',(108.928013630747,71.8195013191724,626.462296651428));
#267323=CARTESIAN_POINT('Ctrl Pts',(113.874993963172,62.8573449296276,624.462296651428));
#267324=CARTESIAN_POINT('Ctrl Pts',(118.821974295598,53.8951885400829,622.462296651428));
#267325=CARTESIAN_POINT('Ctrl Pts',(122.306058950682,44.2694929456717,620.462296651428));
#267326=CARTESIAN_POINT('Ctrl Pts',(125.790143605767,34.6437973512606,618.462296651428));
#267327=CARTESIAN_POINT('Ctrl Pts',(127.725542856289,24.5915791233698,616.462296651428));
#267328=CARTESIAN_POINT('Ctrl Pts',(129.660942106811,14.5393608954789,614.462296651429));
#267329=CARTESIAN_POINT('Ctrl Pts',(130.,4.30813900827846,612.462296651428));
#267330=CARTESIAN_POINT('Ctrl Pts',(130.339057893189,-5.92308287892194,
610.462296651428));
#267331=CARTESIAN_POINT('Ctrl Pts',(129.073425698447,-16.0813817870903,
608.462296651428));
#267332=CARTESIAN_POINT('Ctrl Pts',(127.807793503705,-26.2396806952586,
606.462296651428));
#267333=CARTESIAN_POINT('Ctrl Pts',(124.968635286058,-36.0749255918146,
604.462296651428));
#267334=CARTESIAN_POINT('Ctrl Pts',(122.129477068411,-45.9101704883706,
602.462296651429));
#267335=CARTESIAN_POINT('Ctrl Pts',(117.786702325804,-55.1801850026546,
600.462296651428));
#267336=CARTESIAN_POINT('Ctrl Pts',(113.443927583196,-64.4501995169386,
598.462296651428));
#267337=CARTESIAN_POINT('Ctrl Pts',(107.704469842635,-72.9267251261946,
596.462296651428));
#267338=CARTESIAN_POINT('Ctrl Pts',(101.965012102074,-81.4032507354506,
594.462296651428));
#267339=CARTESIAN_POINT('Ctrl Pts',(94.9701958612992,-88.8775672472032,
592.462296651428));
#267340=CARTESIAN_POINT('Ctrl Pts',(87.9753796205245,-96.3518837589557,
590.462296651429));
#267341=CARTESIAN_POINT('Ctrl Pts',(79.8974404698484,-102.639948694851,
588.462296651428));
#267342=CARTESIAN_POINT('Ctrl Pts',(71.8195013191723,-108.928013630747,
586.462296651428));
#267343=CARTESIAN_POINT('Ctrl Pts',(62.8573449296276,-113.874993963172,
584.462296651428));
#267344=CARTESIAN_POINT('Ctrl Pts',(53.8951885400829,-118.821974295598,
582.462296651428));
#267345=CARTESIAN_POINT('Ctrl Pts',(44.2694929456717,-122.306058950682,
580.462296651428));
#267346=CARTESIAN_POINT('Ctrl Pts',(34.6437973512606,-125.790143605767,
578.462296651429));
#267347=CARTESIAN_POINT('Ctrl Pts',(24.5915791233698,-127.725542856289,
576.462296651428));
#267348=CARTESIAN_POINT('Ctrl Pts',(14.5393608954789,-129.660942106811,
574.462296651428));
#267349=CARTESIAN_POINT('Ctrl Pts',(4.30813900827847,-130.,572.462296651428));
#267350=CARTESIAN_POINT('Ctrl Pts',(-5.92308287892199,-130.339057893189,
570.462296651428));
#267351=CARTESIAN_POINT('Ctrl Pts',(-16.0813817870903,-129.073425698447,
568.462296651428));
#267352=CARTESIAN_POINT('Ctrl Pts',(-26.2396806952585,-127.807793503705,
566.462296651429));
#267353=CARTESIAN_POINT('Ctrl Pts',(-36.0749255918146,-124.968635286058,
564.462296651428));
#267354=CARTESIAN_POINT('Ctrl Pts',(-45.9101704883706,-122.129477068411,
562.462296651428));
#267355=CARTESIAN_POINT('Ctrl Pts',(-55.1801850026546,-117.786702325804,
560.462296651428));
#267356=CARTESIAN_POINT('Ctrl Pts',(-64.4501995169385,-113.443927583197,
558.462296651429));
#267357=CARTESIAN_POINT('Ctrl Pts',(-72.9267251261946,-107.704469842635,
556.462296651428));
#267358=CARTESIAN_POINT('Ctrl Pts',(-81.4032507354507,-101.965012102074,
554.462296651429));
#267359=CARTESIAN_POINT('Ctrl Pts',(-88.8775672472032,-94.9701958612992,
552.462296651428));
#267360=CARTESIAN_POINT('Ctrl Pts',(-96.3518837589557,-87.9753796205245,
550.462296651428));
#267361=CARTESIAN_POINT('Ctrl Pts',(-102.639948694851,-79.8974404698484,
548.462296651428));
#267362=CARTESIAN_POINT('Ctrl Pts',(-108.928013630747,-71.8195013191723,
546.462296651429));
#267363=CARTESIAN_POINT('Ctrl Pts',(-113.874993963172,-62.8573449296276,
544.462296651428));
#267364=CARTESIAN_POINT('Ctrl Pts',(-118.821974295598,-53.8951885400829,
542.462296651429));
#267365=CARTESIAN_POINT('Ctrl Pts',(-122.306058950682,-44.2694929456718,
540.462296651428));
#267366=CARTESIAN_POINT('Ctrl Pts',(-125.790143605767,-34.6437973512606,
538.462296651428));
#267367=CARTESIAN_POINT('Ctrl Pts',(-127.725542856289,-24.5915791233698,
536.462296651428));
#267368=CARTESIAN_POINT('Ctrl Pts',(-129.382196958681,-15.9871278397995,
534.750345898172));
#267369=CARTESIAN_POINT('Ctrl Pts',(-129.869812400585,-7.23822414349998,
533.035792462989));
#267370=CARTESIAN_POINT('Ctrl Pts',(-129.869812400585,7.23822414349888,
696.964207537012));
#267371=CARTESIAN_POINT('Ctrl Pts',(-129.382196958681,15.9871278397986,
695.249654101829));
#267372=CARTESIAN_POINT('Ctrl Pts',(-127.725542856289,24.591579123369,693.537703348572));
#267373=CARTESIAN_POINT('Ctrl Pts',(-125.790143605767,34.6437973512599,
691.537703348572));
#267374=CARTESIAN_POINT('Ctrl Pts',(-122.306058950683,44.269492945671,689.537703348572));
#267375=CARTESIAN_POINT('Ctrl Pts',(-118.821974295598,53.8951885400822,
687.537703348572));
#267376=CARTESIAN_POINT('Ctrl Pts',(-113.874993963172,62.8573449296269,
685.537703348572));
#267377=CARTESIAN_POINT('Ctrl Pts',(-108.928013630747,71.8195013191717,
683.537703348572));
#267378=CARTESIAN_POINT('Ctrl Pts',(-102.639948694852,79.8974404698478,
681.537703348572));
#267379=CARTESIAN_POINT('Ctrl Pts',(-96.3518837589562,87.9753796205239,
679.537703348572));
#267380=CARTESIAN_POINT('Ctrl Pts',(-88.8775672472037,94.9701958612987,
677.537703348572));
#267381=CARTESIAN_POINT('Ctrl Pts',(-81.4032507354512,101.965012102073,
675.537703348572));
#267382=CARTESIAN_POINT('Ctrl Pts',(-72.9267251261952,107.704469842635,
673.537703348572));
#267383=CARTESIAN_POINT('Ctrl Pts',(-64.4501995169392,113.443927583196,
671.537703348572));
#267384=CARTESIAN_POINT('Ctrl Pts',(-55.1801850026552,117.786702325803,
669.537703348572));
#267385=CARTESIAN_POINT('Ctrl Pts',(-45.9101704883713,122.12947706841,667.537703348572));
#267386=CARTESIAN_POINT('Ctrl Pts',(-36.0749255918153,124.968635286057,
665.537703348572));
#267387=CARTESIAN_POINT('Ctrl Pts',(-26.2396806952593,127.807793503704,
663.537703348572));
#267388=CARTESIAN_POINT('Ctrl Pts',(-16.081381787091,129.073425698447,661.537703348572));
#267389=CARTESIAN_POINT('Ctrl Pts',(-5.92308287892268,130.339057893189,
659.537703348572));
#267390=CARTESIAN_POINT('Ctrl Pts',(4.30813900827772,130.,657.537703348572));
#267391=CARTESIAN_POINT('Ctrl Pts',(14.5393608954781,129.660942106811,655.537703348572));
#267392=CARTESIAN_POINT('Ctrl Pts',(24.591579123369,127.725542856289,653.537703348572));
#267393=CARTESIAN_POINT('Ctrl Pts',(34.6437973512599,125.790143605767,651.537703348572));
#267394=CARTESIAN_POINT('Ctrl Pts',(44.269492945671,122.306058950683,649.537703348572));
#267395=CARTESIAN_POINT('Ctrl Pts',(53.8951885400822,118.821974295598,647.537703348572));
#267396=CARTESIAN_POINT('Ctrl Pts',(62.8573449296269,113.874993963172,645.537703348572));
#267397=CARTESIAN_POINT('Ctrl Pts',(71.8195013191717,108.928013630747,643.537703348572));
#267398=CARTESIAN_POINT('Ctrl Pts',(79.8974404698478,102.639948694852,641.537703348572));
#267399=CARTESIAN_POINT('Ctrl Pts',(87.9753796205239,96.3518837589562,639.537703348572));
#267400=CARTESIAN_POINT('Ctrl Pts',(94.9701958612986,88.8775672472037,637.537703348572));
#267401=CARTESIAN_POINT('Ctrl Pts',(101.965012102073,81.4032507354512,635.537703348572));
#267402=CARTESIAN_POINT('Ctrl Pts',(107.704469842635,72.9267251261952,633.537703348572));
#267403=CARTESIAN_POINT('Ctrl Pts',(113.443927583196,64.4501995169392,631.537703348572));
#267404=CARTESIAN_POINT('Ctrl Pts',(117.786702325803,55.1801850026552,629.537703348572));
#267405=CARTESIAN_POINT('Ctrl Pts',(122.12947706841,45.9101704883713,627.537703348572));
#267406=CARTESIAN_POINT('Ctrl Pts',(124.968635286057,36.0749255918153,625.537703348572));
#267407=CARTESIAN_POINT('Ctrl Pts',(127.807793503704,26.2396806952593,623.537703348572));
#267408=CARTESIAN_POINT('Ctrl Pts',(129.073425698447,16.081381787091,621.537703348572));
#267409=CARTESIAN_POINT('Ctrl Pts',(130.339057893189,5.92308287892268,619.537703348572));
#267410=CARTESIAN_POINT('Ctrl Pts',(130.,-4.30813900827772,617.537703348572));
#267411=CARTESIAN_POINT('Ctrl Pts',(129.660942106811,-14.5393608954781,
615.537703348572));
#267412=CARTESIAN_POINT('Ctrl Pts',(127.725542856289,-24.591579123369,613.537703348572));
#267413=CARTESIAN_POINT('Ctrl Pts',(125.790143605767,-34.6437973512599,
611.537703348572));
#267414=CARTESIAN_POINT('Ctrl Pts',(122.306058950683,-44.269492945671,609.537703348572));
#267415=CARTESIAN_POINT('Ctrl Pts',(118.821974295598,-53.8951885400822,
607.537703348572));
#267416=CARTESIAN_POINT('Ctrl Pts',(113.874993963172,-62.8573449296269,
605.537703348572));
#267417=CARTESIAN_POINT('Ctrl Pts',(108.928013630747,-71.8195013191717,
603.537703348572));
#267418=CARTESIAN_POINT('Ctrl Pts',(102.639948694852,-79.8974404698478,
601.537703348572));
#267419=CARTESIAN_POINT('Ctrl Pts',(96.3518837589563,-87.9753796205239,
599.537703348572));
#267420=CARTESIAN_POINT('Ctrl Pts',(88.8775672472037,-94.9701958612986,
597.537703348572));
#267421=CARTESIAN_POINT('Ctrl Pts',(81.4032507354513,-101.965012102073,
595.537703348572));
#267422=CARTESIAN_POINT('Ctrl Pts',(72.9267251261952,-107.704469842635,
593.537703348572));
#267423=CARTESIAN_POINT('Ctrl Pts',(64.4501995169392,-113.443927583196,
591.537703348572));
#267424=CARTESIAN_POINT('Ctrl Pts',(55.1801850026552,-117.786702325803,
589.537703348572));
#267425=CARTESIAN_POINT('Ctrl Pts',(45.9101704883713,-122.12947706841,587.537703348572));
#267426=CARTESIAN_POINT('Ctrl Pts',(36.0749255918153,-124.968635286057,
585.537703348572));
#267427=CARTESIAN_POINT('Ctrl Pts',(26.2396806952593,-127.807793503704,
583.537703348572));
#267428=CARTESIAN_POINT('Ctrl Pts',(16.081381787091,-129.073425698447,581.537703348572));
#267429=CARTESIAN_POINT('Ctrl Pts',(5.92308287892275,-130.339057893189,
579.537703348572));
#267430=CARTESIAN_POINT('Ctrl Pts',(-4.30813900827771,-130.,577.537703348572));
#267431=CARTESIAN_POINT('Ctrl Pts',(-14.5393608954782,-129.660942106811,
575.537703348572));
#267432=CARTESIAN_POINT('Ctrl Pts',(-24.591579123369,-127.725542856289,
573.537703348572));
#267433=CARTESIAN_POINT('Ctrl Pts',(-34.6437973512598,-125.790143605767,
571.537703348572));
#267434=CARTESIAN_POINT('Ctrl Pts',(-44.269492945671,-122.306058950683,
569.537703348572));
#267435=CARTESIAN_POINT('Ctrl Pts',(-53.8951885400822,-118.821974295598,
567.537703348572));
#267436=CARTESIAN_POINT('Ctrl Pts',(-62.8573449296269,-113.874993963172,
565.537703348572));
#267437=CARTESIAN_POINT('Ctrl Pts',(-71.8195013191717,-108.928013630747,
563.537703348572));
#267438=CARTESIAN_POINT('Ctrl Pts',(-79.8974404698478,-102.639948694852,
561.537703348572));
#267439=CARTESIAN_POINT('Ctrl Pts',(-87.975379620524,-96.3518837589562,
559.537703348572));
#267440=CARTESIAN_POINT('Ctrl Pts',(-94.9701958612986,-88.8775672472037,
557.537703348572));
#267441=CARTESIAN_POINT('Ctrl Pts',(-101.965012102073,-81.4032507354513,
555.537703348572));
#267442=CARTESIAN_POINT('Ctrl Pts',(-107.704469842635,-72.9267251261952,
553.537703348572));
#267443=CARTESIAN_POINT('Ctrl Pts',(-113.443927583196,-64.4501995169392,
551.537703348572));
#267444=CARTESIAN_POINT('Ctrl Pts',(-117.786702325803,-55.1801850026553,
549.537703348572));
#267445=CARTESIAN_POINT('Ctrl Pts',(-122.12947706841,-45.9101704883713,
547.537703348572));
#267446=CARTESIAN_POINT('Ctrl Pts',(-124.968635286057,-36.0749255918153,
545.537703348572));
#267447=CARTESIAN_POINT('Ctrl Pts',(-127.807793503704,-26.2396806952593,
543.537703348572));
#267448=CARTESIAN_POINT('Ctrl Pts',(-129.073425698447,-16.081381787091,
541.537703348572));
#267449=CARTESIAN_POINT('Ctrl Pts',(-129.701667605591,-11.038945994199,
540.54493165747));
#267450=CARTESIAN_POINT('Ctrl Pts',(-129.934615416877,-5.96286660784691,
539.549090218607));
#267451=CARTESIAN_POINT('Ctrl Pts',(-160.,4.30813900827767,697.537703348572));
#267452=CARTESIAN_POINT('Ctrl Pts',(-159.660942106811,16.9004121002166,
695.537703348572));
#267453=CARTESIAN_POINT('Ctrl Pts',(-157.356193074143,29.2846130745759,
693.537703348572));
#267454=CARTESIAN_POINT('Ctrl Pts',(-155.051444041476,41.6688140489352,
691.537703348572));
#267455=CARTESIAN_POINT('Ctrl Pts',(-150.837754439537,53.5400027769194,
689.537703348572));
#267456=CARTESIAN_POINT('Ctrl Pts',(-146.624064837599,65.4111915049037,
687.537703348572));
#267457=CARTESIAN_POINT('Ctrl Pts',(-140.605189688823,76.4770599218133,
685.537703348572));
#267458=CARTESIAN_POINT('Ctrl Pts',(-134.586314540048,87.542928338723,683.537703348572));
#267459=CARTESIAN_POINT('Ctrl Pts',(-126.9104585261,97.530998038622,681.537703348572));
#267460=CARTESIAN_POINT('Ctrl Pts',(-119.234602512152,107.519067738521,
679.537703348572));
#267461=CARTESIAN_POINT('Ctrl Pts',(-110.0907706828,116.183399296895,677.537703348572));
#267462=CARTESIAN_POINT('Ctrl Pts',(-100.946938853448,124.847730855269,
675.537703348572));
#267463=CARTESIAN_POINT('Ctrl Pts',(-90.5602826949695,131.974979673883,
673.537703348572));
#267464=CARTESIAN_POINT('Ctrl Pts',(-80.1736265364906,139.102228492497,
671.537703348572));
#267465=CARTESIAN_POINT('Ctrl Pts',(-68.7998999948417,144.516898051454,
669.537703348572));
#267466=CARTESIAN_POINT('Ctrl Pts',(-57.4261734531929,149.931567610411,
667.537703348572));
#267467=CARTESIAN_POINT('Ctrl Pts',(-45.3454354230638,153.500330774912,
665.537703348572));
#267468=CARTESIAN_POINT('Ctrl Pts',(-33.2646973929347,157.069093939413,
663.537703348572));
#267469=CARTESIAN_POINT('Ctrl Pts',(-20.774415738298,158.704075916301,661.537703348572));
#267470=CARTESIAN_POINT('Ctrl Pts',(-8.28413408366129,160.339057893189,
659.537703348572));
#267471=CARTESIAN_POINT('Ctrl Pts',(4.30813900827766,160.,657.537703348572));
#267472=CARTESIAN_POINT('Ctrl Pts',(16.9004121002166,159.660942106811,655.537703348572));
#267473=CARTESIAN_POINT('Ctrl Pts',(29.2846130745759,157.356193074143,653.537703348572));
#267474=CARTESIAN_POINT('Ctrl Pts',(41.6688140489352,155.051444041476,651.537703348572));
#267475=CARTESIAN_POINT('Ctrl Pts',(53.5400027769194,150.837754439537,649.537703348572));
#267476=CARTESIAN_POINT('Ctrl Pts',(65.4111915049037,146.624064837599,647.537703348572));
#267477=CARTESIAN_POINT('Ctrl Pts',(76.4770599218133,140.605189688823,645.537703348572));
#267478=CARTESIAN_POINT('Ctrl Pts',(87.542928338723,134.586314540048,643.537703348572));
#267479=CARTESIAN_POINT('Ctrl Pts',(97.530998038622,126.9104585261,641.537703348572));
#267480=CARTESIAN_POINT('Ctrl Pts',(107.519067738521,119.234602512152,639.537703348572));
#267481=CARTESIAN_POINT('Ctrl Pts',(116.183399296895,110.0907706828,637.537703348572));
#267482=CARTESIAN_POINT('Ctrl Pts',(124.847730855269,100.946938853448,635.537703348572));
#267483=CARTESIAN_POINT('Ctrl Pts',(131.974979673883,90.5602826949695,633.537703348572));
#267484=CARTESIAN_POINT('Ctrl Pts',(139.102228492497,80.1736265364906,631.537703348572));
#267485=CARTESIAN_POINT('Ctrl Pts',(144.516898051454,68.7998999948417,629.537703348572));
#267486=CARTESIAN_POINT('Ctrl Pts',(149.931567610411,57.4261734531929,627.537703348572));
#267487=CARTESIAN_POINT('Ctrl Pts',(153.500330774912,45.3454354230638,625.537703348572));
#267488=CARTESIAN_POINT('Ctrl Pts',(157.069093939413,33.2646973929347,623.537703348572));
#267489=CARTESIAN_POINT('Ctrl Pts',(158.704075916301,20.774415738298,621.537703348572));
#267490=CARTESIAN_POINT('Ctrl Pts',(160.339057893189,8.28413408366131,619.537703348572));
#267491=CARTESIAN_POINT('Ctrl Pts',(160.,-4.30813900827765,617.537703348572));
#267492=CARTESIAN_POINT('Ctrl Pts',(159.660942106811,-16.9004121002166,
615.537703348572));
#267493=CARTESIAN_POINT('Ctrl Pts',(157.356193074143,-29.2846130745759,
613.537703348572));
#267494=CARTESIAN_POINT('Ctrl Pts',(155.051444041476,-41.6688140489352,
611.537703348572));
#267495=CARTESIAN_POINT('Ctrl Pts',(150.837754439537,-53.5400027769194,
609.537703348572));
#267496=CARTESIAN_POINT('Ctrl Pts',(146.624064837599,-65.4111915049036,
607.537703348572));
#267497=CARTESIAN_POINT('Ctrl Pts',(140.605189688823,-76.4770599218133,
605.537703348572));
#267498=CARTESIAN_POINT('Ctrl Pts',(134.586314540048,-87.5429283387229,
603.537703348572));
#267499=CARTESIAN_POINT('Ctrl Pts',(126.9104585261,-97.530998038622,601.537703348572));
#267500=CARTESIAN_POINT('Ctrl Pts',(119.234602512152,-107.519067738521,
599.537703348572));
#267501=CARTESIAN_POINT('Ctrl Pts',(110.0907706828,-116.183399296895,597.537703348572));
#267502=CARTESIAN_POINT('Ctrl Pts',(100.946938853448,-124.847730855269,
595.537703348572));
#267503=CARTESIAN_POINT('Ctrl Pts',(90.5602826949695,-131.974979673883,
593.537703348572));
#267504=CARTESIAN_POINT('Ctrl Pts',(80.1736265364905,-139.102228492497,
591.537703348572));
#267505=CARTESIAN_POINT('Ctrl Pts',(68.7998999948417,-144.516898051454,
589.537703348572));
#267506=CARTESIAN_POINT('Ctrl Pts',(57.426173453193,-149.931567610411,587.537703348572));
#267507=CARTESIAN_POINT('Ctrl Pts',(45.3454354230638,-153.500330774912,
585.537703348572));
#267508=CARTESIAN_POINT('Ctrl Pts',(33.2646973929347,-157.069093939413,
583.537703348572));
#267509=CARTESIAN_POINT('Ctrl Pts',(20.774415738298,-158.704075916301,581.537703348572));
#267510=CARTESIAN_POINT('Ctrl Pts',(8.28413408366139,-160.339057893189,
579.537703348572));
#267511=CARTESIAN_POINT('Ctrl Pts',(-4.30813900827764,-160.,577.537703348572));
#267512=CARTESIAN_POINT('Ctrl Pts',(-16.9004121002167,-159.660942106811,
575.537703348572));
#267513=CARTESIAN_POINT('Ctrl Pts',(-29.2846130745759,-157.356193074143,
573.537703348572));
#267514=CARTESIAN_POINT('Ctrl Pts',(-41.6688140489351,-155.051444041476,
571.537703348572));
#267515=CARTESIAN_POINT('Ctrl Pts',(-53.5400027769194,-150.837754439537,
569.537703348572));
#267516=CARTESIAN_POINT('Ctrl Pts',(-65.4111915049037,-146.624064837599,
567.537703348572));
#267517=CARTESIAN_POINT('Ctrl Pts',(-76.4770599218133,-140.605189688823,
565.537703348572));
#267518=CARTESIAN_POINT('Ctrl Pts',(-87.5429283387229,-134.586314540048,
563.537703348572));
#267519=CARTESIAN_POINT('Ctrl Pts',(-97.530998038622,-126.9104585261,561.537703348572));
#267520=CARTESIAN_POINT('Ctrl Pts',(-107.519067738521,-119.234602512152,
559.537703348572));
#267521=CARTESIAN_POINT('Ctrl Pts',(-116.183399296895,-110.0907706828,557.537703348572));
#267522=CARTESIAN_POINT('Ctrl Pts',(-124.847730855269,-100.946938853448,
555.537703348572));
#267523=CARTESIAN_POINT('Ctrl Pts',(-131.974979673883,-90.5602826949695,
553.537703348572));
#267524=CARTESIAN_POINT('Ctrl Pts',(-139.102228492497,-80.1736265364905,
551.537703348572));
#267525=CARTESIAN_POINT('Ctrl Pts',(-144.516898051454,-68.7998999948417,
549.537703348572));
#267526=CARTESIAN_POINT('Ctrl Pts',(-149.931567610411,-57.426173453193,
547.537703348572));
#267527=CARTESIAN_POINT('Ctrl Pts',(-153.500330774912,-45.3454354230638,
545.537703348572));
#267528=CARTESIAN_POINT('Ctrl Pts',(-157.069093939413,-33.2646973929347,
543.537703348572));
#267529=CARTESIAN_POINT('Ctrl Pts',(-158.704075916301,-20.774415738298,
541.537703348572));
#267530=CARTESIAN_POINT('Ctrl Pts',(-160.339057893189,-8.2841340836614,
539.537703348572));
#267531=CARTESIAN_POINT('Ctrl Pts',(-160.,4.30813900827767,537.537703348572));
#267532=CARTESIAN_POINT('Ctrl Pts',(-130.,4.30813900827773,697.537703348572));
#267533=CARTESIAN_POINT('Ctrl Pts',(-129.660942106811,14.5393608954781,
695.537703348572));
#267534=CARTESIAN_POINT('Ctrl Pts',(-127.725542856289,24.591579123369,693.537703348572));
#267535=CARTESIAN_POINT('Ctrl Pts',(-125.790143605767,34.6437973512599,
691.537703348572));
#267536=CARTESIAN_POINT('Ctrl Pts',(-122.306058950683,44.269492945671,689.537703348572));
#267537=CARTESIAN_POINT('Ctrl Pts',(-118.821974295598,53.8951885400822,
687.537703348572));
#267538=CARTESIAN_POINT('Ctrl Pts',(-113.874993963172,62.8573449296269,
685.537703348572));
#267539=CARTESIAN_POINT('Ctrl Pts',(-108.928013630747,71.8195013191717,
683.537703348572));
#267540=CARTESIAN_POINT('Ctrl Pts',(-102.639948694852,79.8974404698478,
681.537703348572));
#267541=CARTESIAN_POINT('Ctrl Pts',(-96.3518837589562,87.9753796205239,
679.537703348572));
#267542=CARTESIAN_POINT('Ctrl Pts',(-88.8775672472037,94.9701958612987,
677.537703348572));
#267543=CARTESIAN_POINT('Ctrl Pts',(-81.4032507354512,101.965012102073,
675.537703348572));
#267544=CARTESIAN_POINT('Ctrl Pts',(-72.9267251261952,107.704469842635,
673.537703348572));
#267545=CARTESIAN_POINT('Ctrl Pts',(-64.4501995169392,113.443927583196,
671.537703348572));
#267546=CARTESIAN_POINT('Ctrl Pts',(-55.1801850026552,117.786702325803,
669.537703348572));
#267547=CARTESIAN_POINT('Ctrl Pts',(-45.9101704883713,122.12947706841,667.537703348572));
#267548=CARTESIAN_POINT('Ctrl Pts',(-36.0749255918153,124.968635286057,
665.537703348572));
#267549=CARTESIAN_POINT('Ctrl Pts',(-26.2396806952593,127.807793503704,
663.537703348572));
#267550=CARTESIAN_POINT('Ctrl Pts',(-16.081381787091,129.073425698447,661.537703348572));
#267551=CARTESIAN_POINT('Ctrl Pts',(-5.92308287892268,130.339057893189,
659.537703348572));
#267552=CARTESIAN_POINT('Ctrl Pts',(4.30813900827772,130.,657.537703348572));
#267553=CARTESIAN_POINT('Ctrl Pts',(14.5393608954781,129.660942106811,655.537703348572));
#267554=CARTESIAN_POINT('Ctrl Pts',(24.591579123369,127.725542856289,653.537703348572));
#267555=CARTESIAN_POINT('Ctrl Pts',(34.6437973512599,125.790143605767,651.537703348572));
#267556=CARTESIAN_POINT('Ctrl Pts',(44.269492945671,122.306058950683,649.537703348572));
#267557=CARTESIAN_POINT('Ctrl Pts',(53.8951885400822,118.821974295598,647.537703348572));
#267558=CARTESIAN_POINT('Ctrl Pts',(62.8573449296269,113.874993963172,645.537703348572));
#267559=CARTESIAN_POINT('Ctrl Pts',(71.8195013191717,108.928013630747,643.537703348572));
#267560=CARTESIAN_POINT('Ctrl Pts',(79.8974404698478,102.639948694852,641.537703348572));
#267561=CARTESIAN_POINT('Ctrl Pts',(87.9753796205239,96.3518837589562,639.537703348572));
#267562=CARTESIAN_POINT('Ctrl Pts',(94.9701958612986,88.8775672472037,637.537703348572));
#267563=CARTESIAN_POINT('Ctrl Pts',(101.965012102073,81.4032507354512,635.537703348572));
#267564=CARTESIAN_POINT('Ctrl Pts',(107.704469842635,72.9267251261952,633.537703348572));
#267565=CARTESIAN_POINT('Ctrl Pts',(113.443927583196,64.4501995169392,631.537703348572));
#267566=CARTESIAN_POINT('Ctrl Pts',(117.786702325803,55.1801850026552,629.537703348572));
#267567=CARTESIAN_POINT('Ctrl Pts',(122.12947706841,45.9101704883713,627.537703348572));
#267568=CARTESIAN_POINT('Ctrl Pts',(124.968635286057,36.0749255918153,625.537703348572));
#267569=CARTESIAN_POINT('Ctrl Pts',(127.807793503704,26.2396806952593,623.537703348572));
#267570=CARTESIAN_POINT('Ctrl Pts',(129.073425698447,16.081381787091,621.537703348572));
#267571=CARTESIAN_POINT('Ctrl Pts',(130.339057893189,5.92308287892268,619.537703348572));
#267572=CARTESIAN_POINT('Ctrl Pts',(130.,-4.30813900827772,617.537703348572));
#267573=CARTESIAN_POINT('Ctrl Pts',(129.660942106811,-14.5393608954781,
615.537703348572));
#267574=CARTESIAN_POINT('Ctrl Pts',(127.725542856289,-24.591579123369,613.537703348572));
#267575=CARTESIAN_POINT('Ctrl Pts',(125.790143605767,-34.6437973512599,
611.537703348572));
#267576=CARTESIAN_POINT('Ctrl Pts',(122.306058950683,-44.269492945671,609.537703348572));
#267577=CARTESIAN_POINT('Ctrl Pts',(118.821974295598,-53.8951885400822,
607.537703348572));
#267578=CARTESIAN_POINT('Ctrl Pts',(113.874993963172,-62.8573449296269,
605.537703348572));
#267579=CARTESIAN_POINT('Ctrl Pts',(108.928013630747,-71.8195013191717,
603.537703348572));
#267580=CARTESIAN_POINT('Ctrl Pts',(102.639948694852,-79.8974404698478,
601.537703348572));
#267581=CARTESIAN_POINT('Ctrl Pts',(96.3518837589563,-87.9753796205239,
599.537703348572));
#267582=CARTESIAN_POINT('Ctrl Pts',(88.8775672472037,-94.9701958612986,
597.537703348572));
#267583=CARTESIAN_POINT('Ctrl Pts',(81.4032507354513,-101.965012102073,
595.537703348572));
#267584=CARTESIAN_POINT('Ctrl Pts',(72.9267251261952,-107.704469842635,
593.537703348572));
#267585=CARTESIAN_POINT('Ctrl Pts',(64.4501995169392,-113.443927583196,
591.537703348572));
#267586=CARTESIAN_POINT('Ctrl Pts',(55.1801850026552,-117.786702325803,
589.537703348572));
#267587=CARTESIAN_POINT('Ctrl Pts',(45.9101704883713,-122.12947706841,587.537703348572));
#267588=CARTESIAN_POINT('Ctrl Pts',(36.0749255918153,-124.968635286057,
585.537703348572));
#267589=CARTESIAN_POINT('Ctrl Pts',(26.2396806952593,-127.807793503704,
583.537703348572));
#267590=CARTESIAN_POINT('Ctrl Pts',(16.081381787091,-129.073425698447,581.537703348572));
#267591=CARTESIAN_POINT('Ctrl Pts',(5.92308287892275,-130.339057893189,
579.537703348572));
#267592=CARTESIAN_POINT('Ctrl Pts',(-4.30813900827771,-130.,577.537703348572));
#267593=CARTESIAN_POINT('Ctrl Pts',(-14.5393608954782,-129.660942106811,
575.537703348572));
#267594=CARTESIAN_POINT('Ctrl Pts',(-24.591579123369,-127.725542856289,
573.537703348572));
#267595=CARTESIAN_POINT('Ctrl Pts',(-34.6437973512598,-125.790143605767,
571.537703348572));
#267596=CARTESIAN_POINT('Ctrl Pts',(-44.269492945671,-122.306058950683,
569.537703348572));
#267597=CARTESIAN_POINT('Ctrl Pts',(-53.8951885400822,-118.821974295598,
567.537703348572));
#267598=CARTESIAN_POINT('Ctrl Pts',(-62.8573449296269,-113.874993963172,
565.537703348572));
#267599=CARTESIAN_POINT('Ctrl Pts',(-71.8195013191717,-108.928013630747,
563.537703348572));
#267600=CARTESIAN_POINT('Ctrl Pts',(-79.8974404698478,-102.639948694852,
561.537703348572));
#267601=CARTESIAN_POINT('Ctrl Pts',(-87.975379620524,-96.3518837589562,
559.537703348572));
#267602=CARTESIAN_POINT('Ctrl Pts',(-94.9701958612986,-88.8775672472037,
557.537703348572));
#267603=CARTESIAN_POINT('Ctrl Pts',(-101.965012102073,-81.4032507354513,
555.537703348572));
#267604=CARTESIAN_POINT('Ctrl Pts',(-107.704469842635,-72.9267251261952,
553.537703348572));
#267605=CARTESIAN_POINT('Ctrl Pts',(-113.443927583196,-64.4501995169392,
551.537703348572));
#267606=CARTESIAN_POINT('Ctrl Pts',(-117.786702325803,-55.1801850026553,
549.537703348572));
#267607=CARTESIAN_POINT('Ctrl Pts',(-122.12947706841,-45.9101704883713,
547.537703348572));
#267608=CARTESIAN_POINT('Ctrl Pts',(-124.968635286057,-36.0749255918153,
545.537703348572));
#267609=CARTESIAN_POINT('Ctrl Pts',(-127.807793503704,-26.2396806952593,
543.537703348572));
#267610=CARTESIAN_POINT('Ctrl Pts',(-129.073425698447,-16.081381787091,
541.537703348572));
#267611=CARTESIAN_POINT('Ctrl Pts',(-130.339057893189,-5.92308287892275,
539.537703348572));
#267612=CARTESIAN_POINT('Ctrl Pts',(-130.,4.30813900827773,537.537703348572));
#267613=CARTESIAN_POINT('Ctrl Pts',(-159.895664541343,7.20669984090177,
697.076891283416));
#267614=CARTESIAN_POINT('Ctrl Pts',(-159.394142202012,18.3340187941072,
695.306181476978));
#267615=CARTESIAN_POINT('Ctrl Pts',(-157.356193074143,29.2846130745759,
693.537703348572));
#267616=CARTESIAN_POINT('Ctrl Pts',(-155.051444041476,41.6688140489352,
691.537703348572));
#267617=CARTESIAN_POINT('Ctrl Pts',(-150.837754439537,53.5400027769194,
689.537703348572));
#267618=CARTESIAN_POINT('Ctrl Pts',(-146.624064837599,65.4111915049037,
687.537703348572));
#267619=CARTESIAN_POINT('Ctrl Pts',(-140.605189688823,76.4770599218133,
685.537703348572));
#267620=CARTESIAN_POINT('Ctrl Pts',(-134.586314540048,87.542928338723,683.537703348572));
#267621=CARTESIAN_POINT('Ctrl Pts',(-126.9104585261,97.530998038622,681.537703348572));
#267622=CARTESIAN_POINT('Ctrl Pts',(-119.234602512152,107.519067738521,
679.537703348572));
#267623=CARTESIAN_POINT('Ctrl Pts',(-110.0907706828,116.183399296895,677.537703348572));
#267624=CARTESIAN_POINT('Ctrl Pts',(-100.946938853448,124.847730855269,
675.537703348572));
#267625=CARTESIAN_POINT('Ctrl Pts',(-90.5602826949695,131.974979673883,
673.537703348572));
#267626=CARTESIAN_POINT('Ctrl Pts',(-80.1736265364906,139.102228492497,
671.537703348572));
#267627=CARTESIAN_POINT('Ctrl Pts',(-68.7998999948417,144.516898051454,
669.537703348572));
#267628=CARTESIAN_POINT('Ctrl Pts',(-57.4261734531929,149.931567610411,
667.537703348572));
#267629=CARTESIAN_POINT('Ctrl Pts',(-45.3454354230638,153.500330774912,
665.537703348572));
#267630=CARTESIAN_POINT('Ctrl Pts',(-33.2646973929347,157.069093939413,
663.537703348572));
#267631=CARTESIAN_POINT('Ctrl Pts',(-20.774415738298,158.704075916301,661.537703348572));
#267632=CARTESIAN_POINT('Ctrl Pts',(-8.28413408366129,160.339057893189,
659.537703348572));
#267633=CARTESIAN_POINT('Ctrl Pts',(4.30813900827766,160.,657.537703348572));
#267634=CARTESIAN_POINT('Ctrl Pts',(16.9004121002166,159.660942106811,655.537703348572));
#267635=CARTESIAN_POINT('Ctrl Pts',(29.2846130745759,157.356193074143,653.537703348572));
#267636=CARTESIAN_POINT('Ctrl Pts',(41.6688140489352,155.051444041476,651.537703348572));
#267637=CARTESIAN_POINT('Ctrl Pts',(53.5400027769194,150.837754439537,649.537703348572));
#267638=CARTESIAN_POINT('Ctrl Pts',(65.4111915049037,146.624064837599,647.537703348572));
#267639=CARTESIAN_POINT('Ctrl Pts',(76.4770599218133,140.605189688823,645.537703348572));
#267640=CARTESIAN_POINT('Ctrl Pts',(87.542928338723,134.586314540048,643.537703348572));
#267641=CARTESIAN_POINT('Ctrl Pts',(97.530998038622,126.9104585261,641.537703348572));
#267642=CARTESIAN_POINT('Ctrl Pts',(107.519067738521,119.234602512152,639.537703348572));
#267643=CARTESIAN_POINT('Ctrl Pts',(116.183399296895,110.0907706828,637.537703348572));
#267644=CARTESIAN_POINT('Ctrl Pts',(124.847730855269,100.946938853448,635.537703348572));
#267645=CARTESIAN_POINT('Ctrl Pts',(131.974979673883,90.5602826949695,633.537703348572));
#267646=CARTESIAN_POINT('Ctrl Pts',(139.102228492497,80.1736265364906,631.537703348572));
#267647=CARTESIAN_POINT('Ctrl Pts',(144.516898051454,68.7998999948417,629.537703348572));
#267648=CARTESIAN_POINT('Ctrl Pts',(149.931567610411,57.4261734531929,627.537703348572));
#267649=CARTESIAN_POINT('Ctrl Pts',(153.500330774912,45.3454354230638,625.537703348572));
#267650=CARTESIAN_POINT('Ctrl Pts',(157.069093939413,33.2646973929347,623.537703348572));
#267651=CARTESIAN_POINT('Ctrl Pts',(158.704075916301,20.774415738298,621.537703348572));
#267652=CARTESIAN_POINT('Ctrl Pts',(160.339057893189,8.28413408366131,619.537703348572));
#267653=CARTESIAN_POINT('Ctrl Pts',(160.,-4.30813900827765,617.537703348572));
#267654=CARTESIAN_POINT('Ctrl Pts',(159.660942106811,-16.9004121002166,
615.537703348572));
#267655=CARTESIAN_POINT('Ctrl Pts',(157.356193074143,-29.2846130745759,
613.537703348572));
#267656=CARTESIAN_POINT('Ctrl Pts',(155.051444041476,-41.6688140489352,
611.537703348572));
#267657=CARTESIAN_POINT('Ctrl Pts',(150.837754439537,-53.5400027769194,
609.537703348572));
#267658=CARTESIAN_POINT('Ctrl Pts',(146.624064837599,-65.4111915049036,
607.537703348572));
#267659=CARTESIAN_POINT('Ctrl Pts',(140.605189688823,-76.4770599218133,
605.537703348572));
#267660=CARTESIAN_POINT('Ctrl Pts',(134.586314540048,-87.5429283387229,
603.537703348572));
#267661=CARTESIAN_POINT('Ctrl Pts',(126.9104585261,-97.530998038622,601.537703348572));
#267662=CARTESIAN_POINT('Ctrl Pts',(119.234602512152,-107.519067738521,
599.537703348572));
#267663=CARTESIAN_POINT('Ctrl Pts',(110.0907706828,-116.183399296895,597.537703348572));
#267664=CARTESIAN_POINT('Ctrl Pts',(100.946938853448,-124.847730855269,
595.537703348572));
#267665=CARTESIAN_POINT('Ctrl Pts',(90.5602826949695,-131.974979673883,
593.537703348572));
#267666=CARTESIAN_POINT('Ctrl Pts',(80.1736265364905,-139.102228492497,
591.537703348572));
#267667=CARTESIAN_POINT('Ctrl Pts',(68.7998999948417,-144.516898051454,
589.537703348572));
#267668=CARTESIAN_POINT('Ctrl Pts',(57.426173453193,-149.931567610411,587.537703348572));
#267669=CARTESIAN_POINT('Ctrl Pts',(45.3454354230638,-153.500330774912,
585.537703348572));
#267670=CARTESIAN_POINT('Ctrl Pts',(33.2646973929347,-157.069093939413,
583.537703348572));
#267671=CARTESIAN_POINT('Ctrl Pts',(20.774415738298,-158.704075916301,581.537703348572));
#267672=CARTESIAN_POINT('Ctrl Pts',(8.28413408366139,-160.339057893189,
579.537703348572));
#267673=CARTESIAN_POINT('Ctrl Pts',(-4.30813900827764,-160.,577.537703348572));
#267674=CARTESIAN_POINT('Ctrl Pts',(-16.9004121002167,-159.660942106811,
575.537703348572));
#267675=CARTESIAN_POINT('Ctrl Pts',(-29.2846130745759,-157.356193074143,
573.537703348572));
#267676=CARTESIAN_POINT('Ctrl Pts',(-41.6688140489351,-155.051444041476,
571.537703348572));
#267677=CARTESIAN_POINT('Ctrl Pts',(-53.5400027769194,-150.837754439537,
569.537703348572));
#267678=CARTESIAN_POINT('Ctrl Pts',(-65.4111915049037,-146.624064837599,
567.537703348572));
#267679=CARTESIAN_POINT('Ctrl Pts',(-76.4770599218133,-140.605189688823,
565.537703348572));
#267680=CARTESIAN_POINT('Ctrl Pts',(-87.5429283387229,-134.586314540048,
563.537703348572));
#267681=CARTESIAN_POINT('Ctrl Pts',(-97.530998038622,-126.9104585261,561.537703348572));
#267682=CARTESIAN_POINT('Ctrl Pts',(-107.519067738521,-119.234602512152,
559.537703348572));
#267683=CARTESIAN_POINT('Ctrl Pts',(-116.183399296895,-110.0907706828,557.537703348572));
#267684=CARTESIAN_POINT('Ctrl Pts',(-124.847730855269,-100.946938853448,
555.537703348572));
#267685=CARTESIAN_POINT('Ctrl Pts',(-131.974979673883,-90.5602826949695,
553.537703348572));
#267686=CARTESIAN_POINT('Ctrl Pts',(-139.102228492497,-80.1736265364905,
551.537703348572));
#267687=CARTESIAN_POINT('Ctrl Pts',(-144.516898051454,-68.7998999948417,
549.537703348572));
#267688=CARTESIAN_POINT('Ctrl Pts',(-149.931567610411,-57.426173453193,
547.537703348572));
#267689=CARTESIAN_POINT('Ctrl Pts',(-153.500330774912,-45.3454354230638,
545.537703348572));
#267690=CARTESIAN_POINT('Ctrl Pts',(-157.069093939413,-33.2646973929347,
543.537703348572));
#267691=CARTESIAN_POINT('Ctrl Pts',(-158.704075916301,-20.774415738298,
541.537703348572));
#267692=CARTESIAN_POINT('Ctrl Pts',(-159.653854600275,-13.5186762622036,
540.375881753716));
#267693=CARTESIAN_POINT('Ctrl Pts',(-159.937609420477,-6.20654127333065,
539.210563551645));
#267694=CARTESIAN_POINT('Ctrl Pts',(-160.,-4.30813900827851,692.462296651429));
#267695=CARTESIAN_POINT('Ctrl Pts',(-160.339057893189,8.28413408366045,
690.462296651429));
#267696=CARTESIAN_POINT('Ctrl Pts',(-158.704075916301,20.7744157382972,
688.462296651429));
#267697=CARTESIAN_POINT('Ctrl Pts',(-157.069093939413,33.2646973929339,
686.462296651429));
#267698=CARTESIAN_POINT('Ctrl Pts',(-153.500330774912,45.345435423063,684.462296651429));
#267699=CARTESIAN_POINT('Ctrl Pts',(-149.931567610412,57.4261734531921,
682.462296651429));
#267700=CARTESIAN_POINT('Ctrl Pts',(-144.516898051455,68.7998999948409,
680.462296651429));
#267701=CARTESIAN_POINT('Ctrl Pts',(-139.102228492498,80.1736265364898,
678.462296651429));
#267702=CARTESIAN_POINT('Ctrl Pts',(-131.974979673884,90.5602826949688,
676.462296651429));
#267703=CARTESIAN_POINT('Ctrl Pts',(-124.84773085527,100.946938853448,674.462296651429));
#267704=CARTESIAN_POINT('Ctrl Pts',(-116.183399296896,110.0907706828,672.462296651429));
#267705=CARTESIAN_POINT('Ctrl Pts',(-107.519067738522,119.234602512151,
670.462296651429));
#267706=CARTESIAN_POINT('Ctrl Pts',(-97.5309980386227,126.9104585261,668.462296651429));
#267707=CARTESIAN_POINT('Ctrl Pts',(-87.5429283387237,134.586314540048,
666.462296651429));
#267708=CARTESIAN_POINT('Ctrl Pts',(-76.4770599218141,140.605189688823,
664.462296651429));
#267709=CARTESIAN_POINT('Ctrl Pts',(-65.4111915049045,146.624064837598,
662.462296651429));
#267710=CARTESIAN_POINT('Ctrl Pts',(-53.5400027769202,150.837754439537,
660.462296651429));
#267711=CARTESIAN_POINT('Ctrl Pts',(-41.668814048936,155.051444041475,658.462296651429));
#267712=CARTESIAN_POINT('Ctrl Pts',(-29.2846130745767,157.356193074143,
656.462296651429));
#267713=CARTESIAN_POINT('Ctrl Pts',(-16.9004121002175,159.660942106811,
654.462296651428));
#267714=CARTESIAN_POINT('Ctrl Pts',(-4.30813900827852,160.,652.462296651429));
#267715=CARTESIAN_POINT('Ctrl Pts',(8.28413408366043,160.339057893189,650.462296651429));
#267716=CARTESIAN_POINT('Ctrl Pts',(20.7744157382972,158.704075916301,648.462296651428));
#267717=CARTESIAN_POINT('Ctrl Pts',(33.2646973929339,157.069093939413,646.462296651429));
#267718=CARTESIAN_POINT('Ctrl Pts',(45.345435423063,153.500330774912,644.462296651428));
#267719=CARTESIAN_POINT('Ctrl Pts',(57.4261734531921,149.931567610412,642.462296651428));
#267720=CARTESIAN_POINT('Ctrl Pts',(68.7998999948409,144.516898051455,640.462296651428));
#267721=CARTESIAN_POINT('Ctrl Pts',(80.1736265364898,139.102228492498,638.462296651429));
#267722=CARTESIAN_POINT('Ctrl Pts',(90.5602826949688,131.974979673884,636.462296651428));
#267723=CARTESIAN_POINT('Ctrl Pts',(100.946938853448,124.84773085527,634.462296651428));
#267724=CARTESIAN_POINT('Ctrl Pts',(110.0907706828,116.183399296896,632.462296651429));
#267725=CARTESIAN_POINT('Ctrl Pts',(119.234602512151,107.519067738522,630.462296651429));
#267726=CARTESIAN_POINT('Ctrl Pts',(126.9104585261,97.5309980386227,628.462296651429));
#267727=CARTESIAN_POINT('Ctrl Pts',(134.586314540048,87.5429283387237,626.462296651429));
#267728=CARTESIAN_POINT('Ctrl Pts',(140.605189688823,76.4770599218141,624.462296651429));
#267729=CARTESIAN_POINT('Ctrl Pts',(146.624064837598,65.4111915049045,622.462296651429));
#267730=CARTESIAN_POINT('Ctrl Pts',(150.837754439537,53.5400027769202,620.462296651429));
#267731=CARTESIAN_POINT('Ctrl Pts',(155.051444041475,41.668814048936,618.462296651429));
#267732=CARTESIAN_POINT('Ctrl Pts',(157.356193074143,29.2846130745767,616.462296651429));
#267733=CARTESIAN_POINT('Ctrl Pts',(159.660942106811,16.9004121002175,614.462296651429));
#267734=CARTESIAN_POINT('Ctrl Pts',(160.,4.30813900827853,612.462296651429));
#267735=CARTESIAN_POINT('Ctrl Pts',(160.339057893189,-8.28413408366043,
610.462296651429));
#267736=CARTESIAN_POINT('Ctrl Pts',(158.704075916301,-20.7744157382971,
608.462296651429));
#267737=CARTESIAN_POINT('Ctrl Pts',(157.069093939413,-33.2646973929339,
606.462296651429));
#267738=CARTESIAN_POINT('Ctrl Pts',(153.500330774912,-45.345435423063,604.462296651429));
#267739=CARTESIAN_POINT('Ctrl Pts',(149.931567610412,-57.4261734531921,
602.462296651429));
#267740=CARTESIAN_POINT('Ctrl Pts',(144.516898051455,-68.7998999948409,
600.462296651429));
#267741=CARTESIAN_POINT('Ctrl Pts',(139.102228492498,-80.1736265364898,
598.462296651429));
#267742=CARTESIAN_POINT('Ctrl Pts',(131.974979673884,-90.5602826949688,
596.462296651429));
#267743=CARTESIAN_POINT('Ctrl Pts',(124.84773085527,-100.946938853448,594.462296651428));
#267744=CARTESIAN_POINT('Ctrl Pts',(116.183399296896,-110.0907706828,592.462296651429));
#267745=CARTESIAN_POINT('Ctrl Pts',(107.519067738522,-119.234602512151,
590.462296651429));
#267746=CARTESIAN_POINT('Ctrl Pts',(97.5309980386227,-126.9104585261,588.462296651429));
#267747=CARTESIAN_POINT('Ctrl Pts',(87.5429283387236,-134.586314540048,
586.462296651429));
#267748=CARTESIAN_POINT('Ctrl Pts',(76.4770599218141,-140.605189688823,
584.462296651429));
#267749=CARTESIAN_POINT('Ctrl Pts',(65.4111915049046,-146.624064837598,
582.462296651428));
#267750=CARTESIAN_POINT('Ctrl Pts',(53.5400027769202,-150.837754439537,
580.462296651429));
#267751=CARTESIAN_POINT('Ctrl Pts',(41.6688140489359,-155.051444041475,
578.462296651429));
#267752=CARTESIAN_POINT('Ctrl Pts',(29.2846130745768,-157.356193074143,
576.462296651429));
#267753=CARTESIAN_POINT('Ctrl Pts',(16.9004121002176,-159.660942106811,
574.462296651429));
#267754=CARTESIAN_POINT('Ctrl Pts',(4.30813900827854,-160.,572.462296651429));
#267755=CARTESIAN_POINT('Ctrl Pts',(-8.28413408366049,-160.339057893189,
570.462296651428));
#267756=CARTESIAN_POINT('Ctrl Pts',(-20.7744157382971,-158.704075916301,
568.462296651429));
#267757=CARTESIAN_POINT('Ctrl Pts',(-33.2646973929338,-157.069093939413,
566.462296651429));
#267758=CARTESIAN_POINT('Ctrl Pts',(-45.345435423063,-153.500330774912,
564.462296651429));
#267759=CARTESIAN_POINT('Ctrl Pts',(-57.4261734531921,-149.931567610412,
562.462296651429));
#267760=CARTESIAN_POINT('Ctrl Pts',(-68.7998999948409,-144.516898051455,
560.462296651429));
#267761=CARTESIAN_POINT('Ctrl Pts',(-80.1736265364897,-139.102228492498,
558.462296651429));
#267762=CARTESIAN_POINT('Ctrl Pts',(-90.5602826949688,-131.974979673884,
556.462296651429));
#267763=CARTESIAN_POINT('Ctrl Pts',(-100.946938853448,-124.84773085527,
554.462296651429));
#267764=CARTESIAN_POINT('Ctrl Pts',(-110.0907706828,-116.183399296896,552.462296651429));
#267765=CARTESIAN_POINT('Ctrl Pts',(-119.234602512151,-107.519067738522,
550.462296651429));
#267766=CARTESIAN_POINT('Ctrl Pts',(-126.9104585261,-97.5309980386227,548.462296651429));
#267767=CARTESIAN_POINT('Ctrl Pts',(-134.586314540048,-87.5429283387236,
546.462296651429));
#267768=CARTESIAN_POINT('Ctrl Pts',(-140.605189688823,-76.4770599218141,
544.462296651429));
#267769=CARTESIAN_POINT('Ctrl Pts',(-146.624064837598,-65.4111915049046,
542.462296651429));
#267770=CARTESIAN_POINT('Ctrl Pts',(-150.837754439537,-53.5400027769203,
540.462296651429));
#267771=CARTESIAN_POINT('Ctrl Pts',(-155.051444041475,-41.668814048936,
538.462296651429));
#267772=CARTESIAN_POINT('Ctrl Pts',(-157.356193074143,-29.2846130745768,
536.462296651429));
#267773=CARTESIAN_POINT('Ctrl Pts',(-159.660942106811,-16.9004121002176,
534.462296651429));
#267774=CARTESIAN_POINT('Ctrl Pts',(-160.,-4.30813900827851,532.462296651429));
#267775=CARTESIAN_POINT('Ctrl Pts',(-160.,4.30813900827767,697.537703348572));
#267776=CARTESIAN_POINT('Ctrl Pts',(-159.660942106811,16.9004121002166,
695.537703348572));
#267777=CARTESIAN_POINT('Ctrl Pts',(-157.356193074143,29.2846130745759,
693.537703348572));
#267778=CARTESIAN_POINT('Ctrl Pts',(-155.051444041476,41.6688140489352,
691.537703348572));
#267779=CARTESIAN_POINT('Ctrl Pts',(-150.837754439537,53.5400027769194,
689.537703348572));
#267780=CARTESIAN_POINT('Ctrl Pts',(-146.624064837599,65.4111915049037,
687.537703348572));
#267781=CARTESIAN_POINT('Ctrl Pts',(-140.605189688823,76.4770599218133,
685.537703348572));
#267782=CARTESIAN_POINT('Ctrl Pts',(-134.586314540048,87.542928338723,683.537703348572));
#267783=CARTESIAN_POINT('Ctrl Pts',(-126.9104585261,97.530998038622,681.537703348572));
#267784=CARTESIAN_POINT('Ctrl Pts',(-119.234602512152,107.519067738521,
679.537703348572));
#267785=CARTESIAN_POINT('Ctrl Pts',(-110.0907706828,116.183399296895,677.537703348572));
#267786=CARTESIAN_POINT('Ctrl Pts',(-100.946938853448,124.847730855269,
675.537703348572));
#267787=CARTESIAN_POINT('Ctrl Pts',(-90.5602826949695,131.974979673883,
673.537703348572));
#267788=CARTESIAN_POINT('Ctrl Pts',(-80.1736265364906,139.102228492497,
671.537703348572));
#267789=CARTESIAN_POINT('Ctrl Pts',(-68.7998999948417,144.516898051454,
669.537703348572));
#267790=CARTESIAN_POINT('Ctrl Pts',(-57.4261734531929,149.931567610411,
667.537703348572));
#267791=CARTESIAN_POINT('Ctrl Pts',(-45.3454354230638,153.500330774912,
665.537703348572));
#267792=CARTESIAN_POINT('Ctrl Pts',(-33.2646973929347,157.069093939413,
663.537703348572));
#267793=CARTESIAN_POINT('Ctrl Pts',(-20.774415738298,158.704075916301,661.537703348572));
#267794=CARTESIAN_POINT('Ctrl Pts',(-8.28413408366129,160.339057893189,
659.537703348572));
#267795=CARTESIAN_POINT('Ctrl Pts',(4.30813900827766,160.,657.537703348572));
#267796=CARTESIAN_POINT('Ctrl Pts',(16.9004121002166,159.660942106811,655.537703348572));
#267797=CARTESIAN_POINT('Ctrl Pts',(29.2846130745759,157.356193074143,653.537703348572));
#267798=CARTESIAN_POINT('Ctrl Pts',(41.6688140489352,155.051444041476,651.537703348572));
#267799=CARTESIAN_POINT('Ctrl Pts',(53.5400027769194,150.837754439537,649.537703348572));
#267800=CARTESIAN_POINT('Ctrl Pts',(65.4111915049037,146.624064837599,647.537703348572));
#267801=CARTESIAN_POINT('Ctrl Pts',(76.4770599218133,140.605189688823,645.537703348572));
#267802=CARTESIAN_POINT('Ctrl Pts',(87.542928338723,134.586314540048,643.537703348572));
#267803=CARTESIAN_POINT('Ctrl Pts',(97.530998038622,126.9104585261,641.537703348572));
#267804=CARTESIAN_POINT('Ctrl Pts',(107.519067738521,119.234602512152,639.537703348572));
#267805=CARTESIAN_POINT('Ctrl Pts',(116.183399296895,110.0907706828,637.537703348572));
#267806=CARTESIAN_POINT('Ctrl Pts',(124.847730855269,100.946938853448,635.537703348572));
#267807=CARTESIAN_POINT('Ctrl Pts',(131.974979673883,90.5602826949695,633.537703348572));
#267808=CARTESIAN_POINT('Ctrl Pts',(139.102228492497,80.1736265364906,631.537703348572));
#267809=CARTESIAN_POINT('Ctrl Pts',(144.516898051454,68.7998999948417,629.537703348572));
#267810=CARTESIAN_POINT('Ctrl Pts',(149.931567610411,57.4261734531929,627.537703348572));
#267811=CARTESIAN_POINT('Ctrl Pts',(153.500330774912,45.3454354230638,625.537703348572));
#267812=CARTESIAN_POINT('Ctrl Pts',(157.069093939413,33.2646973929347,623.537703348572));
#267813=CARTESIAN_POINT('Ctrl Pts',(158.704075916301,20.774415738298,621.537703348572));
#267814=CARTESIAN_POINT('Ctrl Pts',(160.339057893189,8.28413408366131,619.537703348572));
#267815=CARTESIAN_POINT('Ctrl Pts',(160.,-4.30813900827765,617.537703348572));
#267816=CARTESIAN_POINT('Ctrl Pts',(159.660942106811,-16.9004121002166,
615.537703348572));
#267817=CARTESIAN_POINT('Ctrl Pts',(157.356193074143,-29.2846130745759,
613.537703348572));
#267818=CARTESIAN_POINT('Ctrl Pts',(155.051444041476,-41.6688140489352,
611.537703348572));
#267819=CARTESIAN_POINT('Ctrl Pts',(150.837754439537,-53.5400027769194,
609.537703348572));
#267820=CARTESIAN_POINT('Ctrl Pts',(146.624064837599,-65.4111915049036,
607.537703348572));
#267821=CARTESIAN_POINT('Ctrl Pts',(140.605189688823,-76.4770599218133,
605.537703348572));
#267822=CARTESIAN_POINT('Ctrl Pts',(134.586314540048,-87.5429283387229,
603.537703348572));
#267823=CARTESIAN_POINT('Ctrl Pts',(126.9104585261,-97.530998038622,601.537703348572));
#267824=CARTESIAN_POINT('Ctrl Pts',(119.234602512152,-107.519067738521,
599.537703348572));
#267825=CARTESIAN_POINT('Ctrl Pts',(110.0907706828,-116.183399296895,597.537703348572));
#267826=CARTESIAN_POINT('Ctrl Pts',(100.946938853448,-124.847730855269,
595.537703348572));
#267827=CARTESIAN_POINT('Ctrl Pts',(90.5602826949695,-131.974979673883,
593.537703348572));
#267828=CARTESIAN_POINT('Ctrl Pts',(80.1736265364905,-139.102228492497,
591.537703348572));
#267829=CARTESIAN_POINT('Ctrl Pts',(68.7998999948417,-144.516898051454,
589.537703348572));
#267830=CARTESIAN_POINT('Ctrl Pts',(57.426173453193,-149.931567610411,587.537703348572));
#267831=CARTESIAN_POINT('Ctrl Pts',(45.3454354230638,-153.500330774912,
585.537703348572));
#267832=CARTESIAN_POINT('Ctrl Pts',(33.2646973929347,-157.069093939413,
583.537703348572));
#267833=CARTESIAN_POINT('Ctrl Pts',(20.774415738298,-158.704075916301,581.537703348572));
#267834=CARTESIAN_POINT('Ctrl Pts',(8.28413408366139,-160.339057893189,
579.537703348572));
#267835=CARTESIAN_POINT('Ctrl Pts',(-4.30813900827764,-160.,577.537703348572));
#267836=CARTESIAN_POINT('Ctrl Pts',(-16.9004121002167,-159.660942106811,
575.537703348572));
#267837=CARTESIAN_POINT('Ctrl Pts',(-29.2846130745759,-157.356193074143,
573.537703348572));
#267838=CARTESIAN_POINT('Ctrl Pts',(-41.6688140489351,-155.051444041476,
571.537703348572));
#267839=CARTESIAN_POINT('Ctrl Pts',(-53.5400027769194,-150.837754439537,
569.537703348572));
#267840=CARTESIAN_POINT('Ctrl Pts',(-65.4111915049037,-146.624064837599,
567.537703348572));
#267841=CARTESIAN_POINT('Ctrl Pts',(-76.4770599218133,-140.605189688823,
565.537703348572));
#267842=CARTESIAN_POINT('Ctrl Pts',(-87.5429283387229,-134.586314540048,
563.537703348572));
#267843=CARTESIAN_POINT('Ctrl Pts',(-97.530998038622,-126.9104585261,561.537703348572));
#267844=CARTESIAN_POINT('Ctrl Pts',(-107.519067738521,-119.234602512152,
559.537703348572));
#267845=CARTESIAN_POINT('Ctrl Pts',(-116.183399296895,-110.0907706828,557.537703348572));
#267846=CARTESIAN_POINT('Ctrl Pts',(-124.847730855269,-100.946938853448,
555.537703348572));
#267847=CARTESIAN_POINT('Ctrl Pts',(-131.974979673883,-90.5602826949695,
553.537703348572));
#267848=CARTESIAN_POINT('Ctrl Pts',(-139.102228492497,-80.1736265364905,
551.537703348572));
#267849=CARTESIAN_POINT('Ctrl Pts',(-144.516898051454,-68.7998999948417,
549.537703348572));
#267850=CARTESIAN_POINT('Ctrl Pts',(-149.931567610411,-57.426173453193,
547.537703348572));
#267851=CARTESIAN_POINT('Ctrl Pts',(-153.500330774912,-45.3454354230638,
545.537703348572));
#267852=CARTESIAN_POINT('Ctrl Pts',(-157.069093939413,-33.2646973929347,
543.537703348572));
#267853=CARTESIAN_POINT('Ctrl Pts',(-158.704075916301,-20.774415738298,
541.537703348572));
#267854=CARTESIAN_POINT('Ctrl Pts',(-160.339057893189,-8.2841340836614,
539.537703348572));
#267855=CARTESIAN_POINT('Ctrl Pts',(-160.,4.30813900827767,537.537703348572));
#267856=CARTESIAN_POINT('Ctrl Pts',(-159.937609420477,6.20654127332979,
690.789436448355));
#267857=CARTESIAN_POINT('Ctrl Pts',(-159.653854600276,13.5186762622027,
689.624118246285));
#267858=CARTESIAN_POINT('Ctrl Pts',(-158.704075916301,20.7744157382972,
688.462296651429));
#267859=CARTESIAN_POINT('Ctrl Pts',(-157.069093939413,33.2646973929339,
686.462296651429));
#267860=CARTESIAN_POINT('Ctrl Pts',(-153.500330774912,45.345435423063,684.462296651429));
#267861=CARTESIAN_POINT('Ctrl Pts',(-149.931567610412,57.4261734531921,
682.462296651429));
#267862=CARTESIAN_POINT('Ctrl Pts',(-144.516898051455,68.7998999948409,
680.462296651429));
#267863=CARTESIAN_POINT('Ctrl Pts',(-139.102228492498,80.1736265364898,
678.462296651429));
#267864=CARTESIAN_POINT('Ctrl Pts',(-131.974979673884,90.5602826949688,
676.462296651429));
#267865=CARTESIAN_POINT('Ctrl Pts',(-124.84773085527,100.946938853448,674.462296651429));
#267866=CARTESIAN_POINT('Ctrl Pts',(-116.183399296896,110.0907706828,672.462296651429));
#267867=CARTESIAN_POINT('Ctrl Pts',(-107.519067738522,119.234602512151,
670.462296651429));
#267868=CARTESIAN_POINT('Ctrl Pts',(-97.5309980386227,126.9104585261,668.462296651429));
#267869=CARTESIAN_POINT('Ctrl Pts',(-87.5429283387237,134.586314540048,
666.462296651429));
#267870=CARTESIAN_POINT('Ctrl Pts',(-76.4770599218141,140.605189688823,
664.462296651429));
#267871=CARTESIAN_POINT('Ctrl Pts',(-65.4111915049045,146.624064837598,
662.462296651429));
#267872=CARTESIAN_POINT('Ctrl Pts',(-53.5400027769202,150.837754439537,
660.462296651429));
#267873=CARTESIAN_POINT('Ctrl Pts',(-41.668814048936,155.051444041475,658.462296651429));
#267874=CARTESIAN_POINT('Ctrl Pts',(-29.2846130745767,157.356193074143,
656.462296651429));
#267875=CARTESIAN_POINT('Ctrl Pts',(-16.9004121002175,159.660942106811,
654.462296651429));
#267876=CARTESIAN_POINT('Ctrl Pts',(-4.30813900827852,160.,652.462296651429));
#267877=CARTESIAN_POINT('Ctrl Pts',(8.28413408366043,160.339057893189,650.462296651429));
#267878=CARTESIAN_POINT('Ctrl Pts',(20.7744157382972,158.704075916301,648.462296651428));
#267879=CARTESIAN_POINT('Ctrl Pts',(33.2646973929339,157.069093939413,646.462296651429));
#267880=CARTESIAN_POINT('Ctrl Pts',(45.345435423063,153.500330774912,644.462296651428));
#267881=CARTESIAN_POINT('Ctrl Pts',(57.4261734531921,149.931567610412,642.462296651428));
#267882=CARTESIAN_POINT('Ctrl Pts',(68.7998999948409,144.516898051455,640.462296651428));
#267883=CARTESIAN_POINT('Ctrl Pts',(80.1736265364898,139.102228492498,638.462296651429));
#267884=CARTESIAN_POINT('Ctrl Pts',(90.5602826949688,131.974979673884,636.462296651428));
#267885=CARTESIAN_POINT('Ctrl Pts',(100.946938853448,124.84773085527,634.462296651428));
#267886=CARTESIAN_POINT('Ctrl Pts',(110.0907706828,116.183399296896,632.462296651429));
#267887=CARTESIAN_POINT('Ctrl Pts',(119.234602512151,107.519067738522,630.462296651429));
#267888=CARTESIAN_POINT('Ctrl Pts',(126.9104585261,97.5309980386227,628.462296651429));
#267889=CARTESIAN_POINT('Ctrl Pts',(134.586314540048,87.5429283387237,626.462296651429));
#267890=CARTESIAN_POINT('Ctrl Pts',(140.605189688823,76.4770599218141,624.462296651429));
#267891=CARTESIAN_POINT('Ctrl Pts',(146.624064837598,65.4111915049045,622.462296651429));
#267892=CARTESIAN_POINT('Ctrl Pts',(150.837754439537,53.5400027769202,620.462296651429));
#267893=CARTESIAN_POINT('Ctrl Pts',(155.051444041475,41.668814048936,618.462296651429));
#267894=CARTESIAN_POINT('Ctrl Pts',(157.356193074143,29.2846130745767,616.462296651429));
#267895=CARTESIAN_POINT('Ctrl Pts',(159.660942106811,16.9004121002175,614.462296651429));
#267896=CARTESIAN_POINT('Ctrl Pts',(160.,4.30813900827853,612.462296651429));
#267897=CARTESIAN_POINT('Ctrl Pts',(160.339057893189,-8.28413408366043,
610.462296651429));
#267898=CARTESIAN_POINT('Ctrl Pts',(158.704075916301,-20.7744157382971,
608.462296651429));
#267899=CARTESIAN_POINT('Ctrl Pts',(157.069093939413,-33.2646973929339,
606.462296651429));
#267900=CARTESIAN_POINT('Ctrl Pts',(153.500330774912,-45.345435423063,604.462296651429));
#267901=CARTESIAN_POINT('Ctrl Pts',(149.931567610412,-57.4261734531921,
602.462296651429));
#267902=CARTESIAN_POINT('Ctrl Pts',(144.516898051455,-68.7998999948409,
600.462296651429));
#267903=CARTESIAN_POINT('Ctrl Pts',(139.102228492498,-80.1736265364898,
598.462296651429));
#267904=CARTESIAN_POINT('Ctrl Pts',(131.974979673884,-90.5602826949688,
596.462296651429));
#267905=CARTESIAN_POINT('Ctrl Pts',(124.84773085527,-100.946938853448,594.462296651429));
#267906=CARTESIAN_POINT('Ctrl Pts',(116.183399296896,-110.0907706828,592.462296651429));
#267907=CARTESIAN_POINT('Ctrl Pts',(107.519067738522,-119.234602512151,
590.462296651429));
#267908=CARTESIAN_POINT('Ctrl Pts',(97.5309980386227,-126.9104585261,588.462296651429));
#267909=CARTESIAN_POINT('Ctrl Pts',(87.5429283387236,-134.586314540048,
586.462296651429));
#267910=CARTESIAN_POINT('Ctrl Pts',(76.4770599218141,-140.605189688823,
584.462296651429));
#267911=CARTESIAN_POINT('Ctrl Pts',(65.4111915049045,-146.624064837598,
582.462296651429));
#267912=CARTESIAN_POINT('Ctrl Pts',(53.5400027769202,-150.837754439537,
580.462296651429));
#267913=CARTESIAN_POINT('Ctrl Pts',(41.6688140489359,-155.051444041475,
578.462296651429));
#267914=CARTESIAN_POINT('Ctrl Pts',(29.2846130745768,-157.356193074143,
576.462296651429));
#267915=CARTESIAN_POINT('Ctrl Pts',(16.9004121002176,-159.660942106811,
574.462296651429));
#267916=CARTESIAN_POINT('Ctrl Pts',(4.30813900827854,-160.,572.462296651429));
#267917=CARTESIAN_POINT('Ctrl Pts',(-8.28413408366049,-160.339057893189,
570.462296651429));
#267918=CARTESIAN_POINT('Ctrl Pts',(-20.7744157382971,-158.704075916301,
568.462296651429));
#267919=CARTESIAN_POINT('Ctrl Pts',(-33.2646973929338,-157.069093939413,
566.462296651429));
#267920=CARTESIAN_POINT('Ctrl Pts',(-45.345435423063,-153.500330774912,
564.462296651429));
#267921=CARTESIAN_POINT('Ctrl Pts',(-57.4261734531921,-149.931567610412,
562.462296651429));
#267922=CARTESIAN_POINT('Ctrl Pts',(-68.7998999948409,-144.516898051455,
560.462296651429));
#267923=CARTESIAN_POINT('Ctrl Pts',(-80.1736265364897,-139.102228492498,
558.462296651429));
#267924=CARTESIAN_POINT('Ctrl Pts',(-90.5602826949688,-131.974979673884,
556.462296651429));
#267925=CARTESIAN_POINT('Ctrl Pts',(-100.946938853448,-124.84773085527,
554.462296651429));
#267926=CARTESIAN_POINT('Ctrl Pts',(-110.0907706828,-116.183399296896,552.462296651429));
#267927=CARTESIAN_POINT('Ctrl Pts',(-119.234602512151,-107.519067738522,
550.462296651429));
#267928=CARTESIAN_POINT('Ctrl Pts',(-126.9104585261,-97.5309980386227,548.462296651429));
#267929=CARTESIAN_POINT('Ctrl Pts',(-134.586314540048,-87.5429283387237,
546.462296651429));
#267930=CARTESIAN_POINT('Ctrl Pts',(-140.605189688823,-76.4770599218141,
544.462296651429));
#267931=CARTESIAN_POINT('Ctrl Pts',(-146.624064837598,-65.4111915049046,
542.462296651429));
#267932=CARTESIAN_POINT('Ctrl Pts',(-150.837754439537,-53.5400027769203,
540.462296651429));
#267933=CARTESIAN_POINT('Ctrl Pts',(-155.051444041475,-41.668814048936,
538.462296651429));
#267934=CARTESIAN_POINT('Ctrl Pts',(-157.356193074143,-29.2846130745768,
536.462296651429));
#267935=CARTESIAN_POINT('Ctrl Pts',(-159.394142202012,-18.3340187941084,
534.693818523023));
#267936=CARTESIAN_POINT('Ctrl Pts',(-159.895664541343,-7.20669984090296,
532.923108716584));
#267937=CARTESIAN_POINT('Ctrl Pts',(-130.,-4.30813900827845,692.462296651428));
#267938=CARTESIAN_POINT('Ctrl Pts',(-130.339057893189,5.92308287892195,
690.462296651428));
#267939=CARTESIAN_POINT('Ctrl Pts',(-129.073425698447,16.0813817870903,
688.462296651428));
#267940=CARTESIAN_POINT('Ctrl Pts',(-127.807793503705,26.2396806952586,
686.462296651429));
#267941=CARTESIAN_POINT('Ctrl Pts',(-124.968635286058,36.0749255918146,
684.462296651428));
#267942=CARTESIAN_POINT('Ctrl Pts',(-122.129477068411,45.9101704883706,
682.462296651429));
#267943=CARTESIAN_POINT('Ctrl Pts',(-117.786702325804,55.1801850026546,
680.462296651428));
#267944=CARTESIAN_POINT('Ctrl Pts',(-113.443927583196,64.4501995169386,
678.462296651428));
#267945=CARTESIAN_POINT('Ctrl Pts',(-107.704469842635,72.9267251261946,
676.462296651429));
#267946=CARTESIAN_POINT('Ctrl Pts',(-101.965012102074,81.4032507354507,
674.462296651429));
#267947=CARTESIAN_POINT('Ctrl Pts',(-94.9701958612992,88.8775672472032,
672.462296651428));
#267948=CARTESIAN_POINT('Ctrl Pts',(-87.9753796205245,96.3518837589558,
670.462296651429));
#267949=CARTESIAN_POINT('Ctrl Pts',(-79.8974404698484,102.639948694851,
668.462296651428));
#267950=CARTESIAN_POINT('Ctrl Pts',(-71.8195013191724,108.928013630747,
666.462296651428));
#267951=CARTESIAN_POINT('Ctrl Pts',(-62.8573449296276,113.874993963172,
664.462296651428));
#267952=CARTESIAN_POINT('Ctrl Pts',(-53.8951885400828,118.821974295598,
662.462296651429));
#267953=CARTESIAN_POINT('Ctrl Pts',(-44.2694929456717,122.306058950682,
660.462296651428));
#267954=CARTESIAN_POINT('Ctrl Pts',(-34.6437973512606,125.790143605767,
658.462296651428));
#267955=CARTESIAN_POINT('Ctrl Pts',(-24.5915791233697,127.725542856289,
656.462296651429));
#267956=CARTESIAN_POINT('Ctrl Pts',(-14.5393608954789,129.660942106811,
654.462296651428));
#267957=CARTESIAN_POINT('Ctrl Pts',(-4.30813900827846,130.,652.462296651428));
#267958=CARTESIAN_POINT('Ctrl Pts',(5.92308287892194,130.339057893189,650.462296651429));
#267959=CARTESIAN_POINT('Ctrl Pts',(16.0813817870903,129.073425698447,648.462296651428));
#267960=CARTESIAN_POINT('Ctrl Pts',(26.2396806952586,127.807793503705,646.462296651428));
#267961=CARTESIAN_POINT('Ctrl Pts',(36.0749255918146,124.968635286058,644.462296651428));
#267962=CARTESIAN_POINT('Ctrl Pts',(45.9101704883706,122.129477068411,642.462296651428));
#267963=CARTESIAN_POINT('Ctrl Pts',(55.1801850026546,117.786702325804,640.462296651428));
#267964=CARTESIAN_POINT('Ctrl Pts',(64.4501995169386,113.443927583196,638.462296651429));
#267965=CARTESIAN_POINT('Ctrl Pts',(72.9267251261946,107.704469842635,636.462296651428));
#267966=CARTESIAN_POINT('Ctrl Pts',(81.4032507354506,101.965012102074,634.462296651428));
#267967=CARTESIAN_POINT('Ctrl Pts',(88.8775672472032,94.9701958612992,632.462296651428));
#267968=CARTESIAN_POINT('Ctrl Pts',(96.3518837589558,87.9753796205245,630.462296651428));
#267969=CARTESIAN_POINT('Ctrl Pts',(102.639948694851,79.8974404698484,628.462296651428));
#267970=CARTESIAN_POINT('Ctrl Pts',(108.928013630747,71.8195013191724,626.462296651429));
#267971=CARTESIAN_POINT('Ctrl Pts',(113.874993963172,62.8573449296276,624.462296651428));
#267972=CARTESIAN_POINT('Ctrl Pts',(118.821974295598,53.8951885400829,622.462296651428));
#267973=CARTESIAN_POINT('Ctrl Pts',(122.306058950682,44.2694929456717,620.462296651428));
#267974=CARTESIAN_POINT('Ctrl Pts',(125.790143605767,34.6437973512606,618.462296651428));
#267975=CARTESIAN_POINT('Ctrl Pts',(127.725542856289,24.5915791233698,616.462296651428));
#267976=CARTESIAN_POINT('Ctrl Pts',(129.660942106811,14.5393608954789,614.462296651429));
#267977=CARTESIAN_POINT('Ctrl Pts',(130.,4.30813900827846,612.462296651428));
#267978=CARTESIAN_POINT('Ctrl Pts',(130.339057893189,-5.92308287892194,
610.462296651428));
#267979=CARTESIAN_POINT('Ctrl Pts',(129.073425698447,-16.0813817870903,
608.462296651428));
#267980=CARTESIAN_POINT('Ctrl Pts',(127.807793503705,-26.2396806952586,
606.462296651428));
#267981=CARTESIAN_POINT('Ctrl Pts',(124.968635286058,-36.0749255918146,
604.462296651428));
#267982=CARTESIAN_POINT('Ctrl Pts',(122.129477068411,-45.9101704883706,
602.462296651429));
#267983=CARTESIAN_POINT('Ctrl Pts',(117.786702325804,-55.1801850026546,
600.462296651428));
#267984=CARTESIAN_POINT('Ctrl Pts',(113.443927583196,-64.4501995169386,
598.462296651428));
#267985=CARTESIAN_POINT('Ctrl Pts',(107.704469842635,-72.9267251261946,
596.462296651428));
#267986=CARTESIAN_POINT('Ctrl Pts',(101.965012102074,-81.4032507354506,
594.462296651428));
#267987=CARTESIAN_POINT('Ctrl Pts',(94.9701958612992,-88.8775672472032,
592.462296651428));
#267988=CARTESIAN_POINT('Ctrl Pts',(87.9753796205246,-96.3518837589557,
590.462296651429));
#267989=CARTESIAN_POINT('Ctrl Pts',(79.8974404698484,-102.639948694851,
588.462296651428));
#267990=CARTESIAN_POINT('Ctrl Pts',(71.8195013191723,-108.928013630747,
586.462296651428));
#267991=CARTESIAN_POINT('Ctrl Pts',(62.8573449296276,-113.874993963172,
584.462296651428));
#267992=CARTESIAN_POINT('Ctrl Pts',(53.8951885400829,-118.821974295598,
582.462296651428));
#267993=CARTESIAN_POINT('Ctrl Pts',(44.2694929456717,-122.306058950682,
580.462296651428));
#267994=CARTESIAN_POINT('Ctrl Pts',(34.6437973512606,-125.790143605767,
578.462296651429));
#267995=CARTESIAN_POINT('Ctrl Pts',(24.5915791233698,-127.725542856289,
576.462296651428));
#267996=CARTESIAN_POINT('Ctrl Pts',(14.5393608954789,-129.660942106811,
574.462296651428));
#267997=CARTESIAN_POINT('Ctrl Pts',(4.30813900827847,-130.,572.462296651428));
#267998=CARTESIAN_POINT('Ctrl Pts',(-5.92308287892199,-130.339057893189,
570.462296651428));
#267999=CARTESIAN_POINT('Ctrl Pts',(-16.0813817870903,-129.073425698447,
568.462296651428));
#268000=CARTESIAN_POINT('Ctrl Pts',(-26.2396806952585,-127.807793503705,
566.462296651429));
#268001=CARTESIAN_POINT('Ctrl Pts',(-36.0749255918146,-124.968635286058,
564.462296651428));
#268002=CARTESIAN_POINT('Ctrl Pts',(-45.9101704883706,-122.129477068411,
562.462296651428));
#268003=CARTESIAN_POINT('Ctrl Pts',(-55.1801850026546,-117.786702325804,
560.462296651428));
#268004=CARTESIAN_POINT('Ctrl Pts',(-64.4501995169385,-113.443927583197,
558.462296651429));
#268005=CARTESIAN_POINT('Ctrl Pts',(-72.9267251261946,-107.704469842635,
556.462296651428));
#268006=CARTESIAN_POINT('Ctrl Pts',(-81.4032507354507,-101.965012102074,
554.462296651429));
#268007=CARTESIAN_POINT('Ctrl Pts',(-88.8775672472032,-94.9701958612992,
552.462296651428));
#268008=CARTESIAN_POINT('Ctrl Pts',(-96.3518837589557,-87.9753796205246,
550.462296651428));
#268009=CARTESIAN_POINT('Ctrl Pts',(-102.639948694851,-79.8974404698484,
548.462296651428));
#268010=CARTESIAN_POINT('Ctrl Pts',(-108.928013630747,-71.8195013191723,
546.462296651429));
#268011=CARTESIAN_POINT('Ctrl Pts',(-113.874993963172,-62.8573449296276,
544.462296651428));
#268012=CARTESIAN_POINT('Ctrl Pts',(-118.821974295598,-53.8951885400829,
542.462296651429));
#268013=CARTESIAN_POINT('Ctrl Pts',(-122.306058950682,-44.2694929456718,
540.462296651428));
#268014=CARTESIAN_POINT('Ctrl Pts',(-125.790143605767,-34.6437973512606,
538.462296651428));
#268015=CARTESIAN_POINT('Ctrl Pts',(-127.725542856289,-24.5915791233698,
536.462296651428));
#268016=CARTESIAN_POINT('Ctrl Pts',(-129.660942106811,-14.5393608954789,
534.462296651429));
#268017=CARTESIAN_POINT('Ctrl Pts',(-130.,-4.30813900827845,532.462296651428));
#268018=CARTESIAN_POINT('Ctrl Pts',(-160.,-4.30813900827851,692.462296651429));
#268019=CARTESIAN_POINT('Ctrl Pts',(-160.339057893189,8.28413408366045,
690.462296651429));
#268020=CARTESIAN_POINT('Ctrl Pts',(-158.704075916301,20.7744157382972,
688.462296651429));
#268021=CARTESIAN_POINT('Ctrl Pts',(-157.069093939413,33.2646973929339,
686.462296651429));
#268022=CARTESIAN_POINT('Ctrl Pts',(-153.500330774912,45.345435423063,684.462296651429));
#268023=CARTESIAN_POINT('Ctrl Pts',(-149.931567610412,57.4261734531921,
682.462296651429));
#268024=CARTESIAN_POINT('Ctrl Pts',(-144.516898051455,68.7998999948409,
680.462296651429));
#268025=CARTESIAN_POINT('Ctrl Pts',(-139.102228492498,80.1736265364898,
678.462296651429));
#268026=CARTESIAN_POINT('Ctrl Pts',(-131.974979673884,90.5602826949688,
676.462296651429));
#268027=CARTESIAN_POINT('Ctrl Pts',(-124.84773085527,100.946938853448,674.462296651429));
#268028=CARTESIAN_POINT('Ctrl Pts',(-116.183399296896,110.0907706828,672.462296651429));
#268029=CARTESIAN_POINT('Ctrl Pts',(-107.519067738522,119.234602512151,
670.462296651429));
#268030=CARTESIAN_POINT('Ctrl Pts',(-97.5309980386227,126.9104585261,668.462296651429));
#268031=CARTESIAN_POINT('Ctrl Pts',(-87.5429283387237,134.586314540048,
666.462296651429));
#268032=CARTESIAN_POINT('Ctrl Pts',(-76.4770599218141,140.605189688823,
664.462296651429));
#268033=CARTESIAN_POINT('Ctrl Pts',(-65.4111915049045,146.624064837598,
662.462296651429));
#268034=CARTESIAN_POINT('Ctrl Pts',(-53.5400027769202,150.837754439537,
660.462296651429));
#268035=CARTESIAN_POINT('Ctrl Pts',(-41.668814048936,155.051444041475,658.462296651429));
#268036=CARTESIAN_POINT('Ctrl Pts',(-29.2846130745767,157.356193074143,
656.462296651429));
#268037=CARTESIAN_POINT('Ctrl Pts',(-16.9004121002175,159.660942106811,
654.462296651428));
#268038=CARTESIAN_POINT('Ctrl Pts',(-4.30813900827852,160.,652.462296651429));
#268039=CARTESIAN_POINT('Ctrl Pts',(8.28413408366043,160.339057893189,650.462296651429));
#268040=CARTESIAN_POINT('Ctrl Pts',(20.7744157382972,158.704075916301,648.462296651428));
#268041=CARTESIAN_POINT('Ctrl Pts',(33.2646973929339,157.069093939413,646.462296651429));
#268042=CARTESIAN_POINT('Ctrl Pts',(45.345435423063,153.500330774912,644.462296651428));
#268043=CARTESIAN_POINT('Ctrl Pts',(57.4261734531921,149.931567610412,642.462296651428));
#268044=CARTESIAN_POINT('Ctrl Pts',(68.7998999948409,144.516898051455,640.462296651428));
#268045=CARTESIAN_POINT('Ctrl Pts',(80.1736265364898,139.102228492498,638.462296651429));
#268046=CARTESIAN_POINT('Ctrl Pts',(90.5602826949688,131.974979673884,636.462296651428));
#268047=CARTESIAN_POINT('Ctrl Pts',(100.946938853448,124.84773085527,634.462296651428));
#268048=CARTESIAN_POINT('Ctrl Pts',(110.0907706828,116.183399296896,632.462296651429));
#268049=CARTESIAN_POINT('Ctrl Pts',(119.234602512151,107.519067738522,630.462296651429));
#268050=CARTESIAN_POINT('Ctrl Pts',(126.9104585261,97.5309980386227,628.462296651429));
#268051=CARTESIAN_POINT('Ctrl Pts',(134.586314540048,87.5429283387237,626.462296651429));
#268052=CARTESIAN_POINT('Ctrl Pts',(140.605189688823,76.4770599218141,624.462296651429));
#268053=CARTESIAN_POINT('Ctrl Pts',(146.624064837598,65.4111915049045,622.462296651429));
#268054=CARTESIAN_POINT('Ctrl Pts',(150.837754439537,53.5400027769202,620.462296651429));
#268055=CARTESIAN_POINT('Ctrl Pts',(155.051444041475,41.668814048936,618.462296651429));
#268056=CARTESIAN_POINT('Ctrl Pts',(157.356193074143,29.2846130745767,616.462296651429));
#268057=CARTESIAN_POINT('Ctrl Pts',(159.660942106811,16.9004121002175,614.462296651429));
#268058=CARTESIAN_POINT('Ctrl Pts',(160.,4.30813900827853,612.462296651429));
#268059=CARTESIAN_POINT('Ctrl Pts',(160.339057893189,-8.28413408366043,
610.462296651429));
#268060=CARTESIAN_POINT('Ctrl Pts',(158.704075916301,-20.7744157382971,
608.462296651429));
#268061=CARTESIAN_POINT('Ctrl Pts',(157.069093939413,-33.2646973929339,
606.462296651429));
#268062=CARTESIAN_POINT('Ctrl Pts',(153.500330774912,-45.345435423063,604.462296651429));
#268063=CARTESIAN_POINT('Ctrl Pts',(149.931567610412,-57.4261734531921,
602.462296651429));
#268064=CARTESIAN_POINT('Ctrl Pts',(144.516898051455,-68.7998999948409,
600.462296651429));
#268065=CARTESIAN_POINT('Ctrl Pts',(139.102228492498,-80.1736265364898,
598.462296651429));
#268066=CARTESIAN_POINT('Ctrl Pts',(131.974979673884,-90.5602826949688,
596.462296651429));
#268067=CARTESIAN_POINT('Ctrl Pts',(124.84773085527,-100.946938853448,594.462296651428));
#268068=CARTESIAN_POINT('Ctrl Pts',(116.183399296896,-110.0907706828,592.462296651429));
#268069=CARTESIAN_POINT('Ctrl Pts',(107.519067738522,-119.234602512151,
590.462296651429));
#268070=CARTESIAN_POINT('Ctrl Pts',(97.5309980386227,-126.9104585261,588.462296651429));
#268071=CARTESIAN_POINT('Ctrl Pts',(87.5429283387236,-134.586314540048,
586.462296651429));
#268072=CARTESIAN_POINT('Ctrl Pts',(76.4770599218141,-140.605189688823,
584.462296651429));
#268073=CARTESIAN_POINT('Ctrl Pts',(65.4111915049046,-146.624064837598,
582.462296651428));
#268074=CARTESIAN_POINT('Ctrl Pts',(53.5400027769202,-150.837754439537,
580.462296651429));
#268075=CARTESIAN_POINT('Ctrl Pts',(41.6688140489359,-155.051444041475,
578.462296651429));
#268076=CARTESIAN_POINT('Ctrl Pts',(29.2846130745768,-157.356193074143,
576.462296651429));
#268077=CARTESIAN_POINT('Ctrl Pts',(16.9004121002176,-159.660942106811,
574.462296651429));
#268078=CARTESIAN_POINT('Ctrl Pts',(4.30813900827854,-160.,572.462296651429));
#268079=CARTESIAN_POINT('Ctrl Pts',(-8.28413408366049,-160.339057893189,
570.462296651428));
#268080=CARTESIAN_POINT('Ctrl Pts',(-20.7744157382971,-158.704075916301,
568.462296651429));
#268081=CARTESIAN_POINT('Ctrl Pts',(-33.2646973929338,-157.069093939413,
566.462296651429));
#268082=CARTESIAN_POINT('Ctrl Pts',(-45.345435423063,-153.500330774912,
564.462296651429));
#268083=CARTESIAN_POINT('Ctrl Pts',(-57.4261734531921,-149.931567610412,
562.462296651429));
#268084=CARTESIAN_POINT('Ctrl Pts',(-68.7998999948409,-144.516898051455,
560.462296651429));
#268085=CARTESIAN_POINT('Ctrl Pts',(-80.1736265364897,-139.102228492498,
558.462296651429));
#268086=CARTESIAN_POINT('Ctrl Pts',(-90.5602826949688,-131.974979673884,
556.462296651429));
#268087=CARTESIAN_POINT('Ctrl Pts',(-100.946938853448,-124.84773085527,
554.462296651429));
#268088=CARTESIAN_POINT('Ctrl Pts',(-110.0907706828,-116.183399296896,552.462296651429));
#268089=CARTESIAN_POINT('Ctrl Pts',(-119.234602512151,-107.519067738522,
550.462296651429));
#268090=CARTESIAN_POINT('Ctrl Pts',(-126.9104585261,-97.5309980386227,548.462296651429));
#268091=CARTESIAN_POINT('Ctrl Pts',(-134.586314540048,-87.5429283387236,
546.462296651429));
#268092=CARTESIAN_POINT('Ctrl Pts',(-140.605189688823,-76.4770599218141,
544.462296651429));
#268093=CARTESIAN_POINT('Ctrl Pts',(-146.624064837598,-65.4111915049046,
542.462296651429));
#268094=CARTESIAN_POINT('Ctrl Pts',(-150.837754439537,-53.5400027769203,
540.462296651429));
#268095=CARTESIAN_POINT('Ctrl Pts',(-155.051444041475,-41.668814048936,
538.462296651429));
#268096=CARTESIAN_POINT('Ctrl Pts',(-157.356193074143,-29.2846130745768,
536.462296651429));
#268097=CARTESIAN_POINT('Ctrl Pts',(-159.660942106811,-16.9004121002176,
534.462296651429));
#268098=CARTESIAN_POINT('Ctrl Pts',(-160.,-4.30813900827851,532.462296651429));
#268099=CARTESIAN_POINT('Origin',(-160.,3.64291929955129E-14,535.));
#268100=CARTESIAN_POINT('',(-160.,1.56720635279146E-14,535.));
#268101=CARTESIAN_POINT('',(-160.,-4.30813900827827,538.90811221526));
#268102=CARTESIAN_POINT('Ctrl Pts',(-160.,-2.35367281220533E-13,535.));
#268103=CARTESIAN_POINT('Ctrl Pts',(-160.,-0.0199151703951082,535.01805734453));
#268104=CARTESIAN_POINT('Ctrl Pts',(-160.,-0.039830432424492,535.036114587998));
#268105=CARTESIAN_POINT('Ctrl Pts',(-160.,-0.059745511185169,535.05417203359));
#268106=CARTESIAN_POINT('Ctrl Pts',(-160.,-1.4761797871856,536.338484547738));
#268107=CARTESIAN_POINT('Ctrl Pts',(-160.,-2.89215276710114,537.623305748502));
#268108=CARTESIAN_POINT('Ctrl Pts',(-160.,-4.30813900827838,538.90811221526));
#268109=CARTESIAN_POINT('',(-160.,-4.30813900827851,532.462296651429));
#268110=CARTESIAN_POINT('',(-160.,-4.21537804662364E-13,535.));
#268111=CARTESIAN_POINT('',(-160.,4.30813900827783,531.091887784741));
#268112=CARTESIAN_POINT('Ctrl Pts',(-160.,-4.30813900827851,532.462296651429));
#268113=CARTESIAN_POINT('Ctrl Pts',(-160.,-1.43594781991725,532.006113535419));
#268114=CARTESIAN_POINT('Ctrl Pts',(-160.,1.43604209808292,531.548664093541));
#268115=CARTESIAN_POINT('Ctrl Pts',(-160.,4.30813900827783,531.091887784741));
#268116=CARTESIAN_POINT('Ctrl Pts',(-160.,4.30813900827787,531.091887784741));
#268117=CARTESIAN_POINT('Ctrl Pts',(-160.,2.89215276710099,532.376694251499));
#268118=CARTESIAN_POINT('Ctrl Pts',(-160.,1.47617978720989,533.66151545229));
#268119=CARTESIAN_POINT('Ctrl Pts',(-160.,0.0597455111844823,534.945827966411));
#268120=CARTESIAN_POINT('Ctrl Pts',(-160.,0.0398304324235108,534.963885412002));
#268121=CARTESIAN_POINT('Ctrl Pts',(-160.,0.019915170394957,534.981942655471));
#268122=CARTESIAN_POINT('Ctrl Pts',(-160.,1.72084568816899E-14,535.000000000001));
#268123=CARTESIAN_POINT('',(-160.,4.30813900827767,537.537703348572));
#268124=CARTESIAN_POINT('',(-160.,-4.21537804662364E-13,535.));
#268125=CARTESIAN_POINT('Ctrl Pts',(-160.,-4.30813900827827,538.90811221526));
#268126=CARTESIAN_POINT('Ctrl Pts',(-160.,-1.43604209806711,538.451335906457));
#268127=CARTESIAN_POINT('Ctrl Pts',(-160.,1.43594781992473,537.99388646458));
#268128=CARTESIAN_POINT('Ctrl Pts',(-160.,4.30813900827767,537.537703348572));
#268129=CARTESIAN_POINT('Ctrl Pts',(-160.,-4.30813900827851,692.462296651429));
#268130=CARTESIAN_POINT('Ctrl Pts',(-160.339057893189,8.28413408366045,
690.462296651429));
#268131=CARTESIAN_POINT('Ctrl Pts',(-158.704075916301,20.7744157382972,
688.462296651429));
#268132=CARTESIAN_POINT('Ctrl Pts',(-157.069093939413,33.2646973929339,
686.462296651429));
#268133=CARTESIAN_POINT('Ctrl Pts',(-153.500330774912,45.345435423063,684.462296651429));
#268134=CARTESIAN_POINT('Ctrl Pts',(-149.931567610412,57.4261734531921,
682.462296651429));
#268135=CARTESIAN_POINT('Ctrl Pts',(-144.516898051455,68.7998999948409,
680.462296651429));
#268136=CARTESIAN_POINT('Ctrl Pts',(-139.102228492498,80.1736265364898,
678.462296651429));
#268137=CARTESIAN_POINT('Ctrl Pts',(-131.974979673884,90.5602826949688,
676.462296651429));
#268138=CARTESIAN_POINT('Ctrl Pts',(-124.84773085527,100.946938853448,674.462296651429));
#268139=CARTESIAN_POINT('Ctrl Pts',(-116.183399296896,110.0907706828,672.462296651429));
#268140=CARTESIAN_POINT('Ctrl Pts',(-107.519067738522,119.234602512151,
670.462296651429));
#268141=CARTESIAN_POINT('Ctrl Pts',(-97.5309980386227,126.9104585261,668.462296651429));
#268142=CARTESIAN_POINT('Ctrl Pts',(-87.5429283387237,134.586314540048,
666.462296651429));
#268143=CARTESIAN_POINT('Ctrl Pts',(-76.4770599218141,140.605189688823,
664.462296651429));
#268144=CARTESIAN_POINT('Ctrl Pts',(-65.4111915049045,146.624064837598,
662.462296651429));
#268145=CARTESIAN_POINT('Ctrl Pts',(-53.5400027769202,150.837754439537,
660.462296651429));
#268146=CARTESIAN_POINT('Ctrl Pts',(-41.668814048936,155.051444041475,658.462296651429));
#268147=CARTESIAN_POINT('Ctrl Pts',(-29.2846130745767,157.356193074143,
656.462296651429));
#268148=CARTESIAN_POINT('Ctrl Pts',(-16.9004121002175,159.660942106811,
654.462296651428));
#268149=CARTESIAN_POINT('Ctrl Pts',(-4.30813900827852,160.,652.462296651429));
#268150=CARTESIAN_POINT('Ctrl Pts',(8.28413408366043,160.339057893189,650.462296651429));
#268151=CARTESIAN_POINT('Ctrl Pts',(20.7744157382972,158.704075916301,648.462296651428));
#268152=CARTESIAN_POINT('Ctrl Pts',(33.2646973929339,157.069093939413,646.462296651429));
#268153=CARTESIAN_POINT('Ctrl Pts',(45.345435423063,153.500330774912,644.462296651428));
#268154=CARTESIAN_POINT('Ctrl Pts',(57.4261734531921,149.931567610412,642.462296651428));
#268155=CARTESIAN_POINT('Ctrl Pts',(68.7998999948409,144.516898051455,640.462296651428));
#268156=CARTESIAN_POINT('Ctrl Pts',(80.1736265364898,139.102228492498,638.462296651429));
#268157=CARTESIAN_POINT('Ctrl Pts',(90.5602826949688,131.974979673884,636.462296651428));
#268158=CARTESIAN_POINT('Ctrl Pts',(100.946938853448,124.84773085527,634.462296651428));
#268159=CARTESIAN_POINT('Ctrl Pts',(110.0907706828,116.183399296896,632.462296651429));
#268160=CARTESIAN_POINT('Ctrl Pts',(119.234602512151,107.519067738522,630.462296651429));
#268161=CARTESIAN_POINT('Ctrl Pts',(126.9104585261,97.5309980386227,628.462296651429));
#268162=CARTESIAN_POINT('Ctrl Pts',(134.586314540048,87.5429283387237,626.462296651429));
#268163=CARTESIAN_POINT('Ctrl Pts',(140.605189688823,76.4770599218141,624.462296651429));
#268164=CARTESIAN_POINT('Ctrl Pts',(146.624064837598,65.4111915049045,622.462296651429));
#268165=CARTESIAN_POINT('Ctrl Pts',(150.837754439537,53.5400027769202,620.462296651429));
#268166=CARTESIAN_POINT('Ctrl Pts',(155.051444041475,41.668814048936,618.462296651429));
#268167=CARTESIAN_POINT('Ctrl Pts',(157.356193074143,29.2846130745767,616.462296651429));
#268168=CARTESIAN_POINT('Ctrl Pts',(159.660942106811,16.9004121002175,614.462296651429));
#268169=CARTESIAN_POINT('Ctrl Pts',(160.,4.30813900827853,612.462296651429));
#268170=CARTESIAN_POINT('Ctrl Pts',(160.339057893189,-8.28413408366043,
610.462296651429));
#268171=CARTESIAN_POINT('Ctrl Pts',(158.704075916301,-20.7744157382971,
608.462296651429));
#268172=CARTESIAN_POINT('Ctrl Pts',(157.069093939413,-33.2646973929339,
606.462296651429));
#268173=CARTESIAN_POINT('Ctrl Pts',(153.500330774912,-45.345435423063,604.462296651429));
#268174=CARTESIAN_POINT('Ctrl Pts',(149.931567610412,-57.4261734531921,
602.462296651429));
#268175=CARTESIAN_POINT('Ctrl Pts',(144.516898051455,-68.7998999948409,
600.462296651429));
#268176=CARTESIAN_POINT('Ctrl Pts',(139.102228492498,-80.1736265364898,
598.462296651429));
#268177=CARTESIAN_POINT('Ctrl Pts',(131.974979673884,-90.5602826949688,
596.462296651429));
#268178=CARTESIAN_POINT('Ctrl Pts',(124.84773085527,-100.946938853448,594.462296651428));
#268179=CARTESIAN_POINT('Ctrl Pts',(116.183399296896,-110.0907706828,592.462296651429));
#268180=CARTESIAN_POINT('Ctrl Pts',(107.519067738522,-119.234602512151,
590.462296651429));
#268181=CARTESIAN_POINT('Ctrl Pts',(97.5309980386227,-126.9104585261,588.462296651429));
#268182=CARTESIAN_POINT('Ctrl Pts',(87.5429283387236,-134.586314540048,
586.462296651429));
#268183=CARTESIAN_POINT('Ctrl Pts',(76.4770599218141,-140.605189688823,
584.462296651429));
#268184=CARTESIAN_POINT('Ctrl Pts',(65.4111915049046,-146.624064837598,
582.462296651428));
#268185=CARTESIAN_POINT('Ctrl Pts',(53.5400027769202,-150.837754439537,
580.462296651429));
#268186=CARTESIAN_POINT('Ctrl Pts',(41.6688140489359,-155.051444041475,
578.462296651429));
#268187=CARTESIAN_POINT('Ctrl Pts',(29.2846130745768,-157.356193074143,
576.462296651429));
#268188=CARTESIAN_POINT('Ctrl Pts',(16.9004121002176,-159.660942106811,
574.462296651429));
#268189=CARTESIAN_POINT('Ctrl Pts',(4.30813900827854,-160.,572.462296651429));
#268190=CARTESIAN_POINT('Ctrl Pts',(-8.28413408366049,-160.339057893189,
570.462296651428));
#268191=CARTESIAN_POINT('Ctrl Pts',(-20.7744157382971,-158.704075916301,
568.462296651429));
#268192=CARTESIAN_POINT('Ctrl Pts',(-33.2646973929338,-157.069093939413,
566.462296651429));
#268193=CARTESIAN_POINT('Ctrl Pts',(-45.345435423063,-153.500330774912,
564.462296651429));
#268194=CARTESIAN_POINT('Ctrl Pts',(-57.4261734531921,-149.931567610412,
562.462296651429));
#268195=CARTESIAN_POINT('Ctrl Pts',(-68.7998999948409,-144.516898051455,
560.462296651429));
#268196=CARTESIAN_POINT('Ctrl Pts',(-80.1736265364897,-139.102228492498,
558.462296651429));
#268197=CARTESIAN_POINT('Ctrl Pts',(-90.5602826949688,-131.974979673884,
556.462296651429));
#268198=CARTESIAN_POINT('Ctrl Pts',(-100.946938853448,-124.84773085527,
554.462296651429));
#268199=CARTESIAN_POINT('Ctrl Pts',(-110.0907706828,-116.183399296896,552.462296651429));
#268200=CARTESIAN_POINT('Ctrl Pts',(-119.234602512151,-107.519067738522,
550.462296651429));
#268201=CARTESIAN_POINT('Ctrl Pts',(-126.9104585261,-97.5309980386227,548.462296651429));
#268202=CARTESIAN_POINT('Ctrl Pts',(-134.586314540048,-87.5429283387236,
546.462296651429));
#268203=CARTESIAN_POINT('Ctrl Pts',(-140.605189688823,-76.4770599218141,
544.462296651429));
#268204=CARTESIAN_POINT('Ctrl Pts',(-146.624064837598,-65.4111915049046,
542.462296651429));
#268205=CARTESIAN_POINT('Ctrl Pts',(-150.837754439537,-53.5400027769203,
540.462296651429));
#268206=CARTESIAN_POINT('Ctrl Pts',(-155.051444041475,-41.668814048936,
538.462296651429));
#268207=CARTESIAN_POINT('Ctrl Pts',(-157.356193074143,-29.2846130745768,
536.462296651429));
#268208=CARTESIAN_POINT('Ctrl Pts',(-159.660942106811,-16.9004121002176,
534.462296651429));
#268209=CARTESIAN_POINT('Ctrl Pts',(-160.,-4.30813900827851,532.462296651429));
#268210=CARTESIAN_POINT('Ctrl Pts',(-160.,4.30813900827767,697.537703348572));
#268211=CARTESIAN_POINT('Ctrl Pts',(-159.660942106811,16.9004121002166,
695.537703348572));
#268212=CARTESIAN_POINT('Ctrl Pts',(-157.356193074143,29.2846130745759,
693.537703348572));
#268213=CARTESIAN_POINT('Ctrl Pts',(-155.051444041476,41.6688140489352,
691.537703348572));
#268214=CARTESIAN_POINT('Ctrl Pts',(-150.837754439537,53.5400027769194,
689.537703348572));
#268215=CARTESIAN_POINT('Ctrl Pts',(-146.624064837599,65.4111915049037,
687.537703348572));
#268216=CARTESIAN_POINT('Ctrl Pts',(-140.605189688823,76.4770599218133,
685.537703348572));
#268217=CARTESIAN_POINT('Ctrl Pts',(-134.586314540048,87.542928338723,683.537703348572));
#268218=CARTESIAN_POINT('Ctrl Pts',(-126.9104585261,97.530998038622,681.537703348572));
#268219=CARTESIAN_POINT('Ctrl Pts',(-119.234602512152,107.519067738521,
679.537703348572));
#268220=CARTESIAN_POINT('Ctrl Pts',(-110.0907706828,116.183399296895,677.537703348572));
#268221=CARTESIAN_POINT('Ctrl Pts',(-100.946938853448,124.847730855269,
675.537703348572));
#268222=CARTESIAN_POINT('Ctrl Pts',(-90.5602826949695,131.974979673883,
673.537703348572));
#268223=CARTESIAN_POINT('Ctrl Pts',(-80.1736265364906,139.102228492497,
671.537703348572));
#268224=CARTESIAN_POINT('Ctrl Pts',(-68.7998999948417,144.516898051454,
669.537703348572));
#268225=CARTESIAN_POINT('Ctrl Pts',(-57.4261734531929,149.931567610411,
667.537703348572));
#268226=CARTESIAN_POINT('Ctrl Pts',(-45.3454354230638,153.500330774912,
665.537703348572));
#268227=CARTESIAN_POINT('Ctrl Pts',(-33.2646973929347,157.069093939413,
663.537703348572));
#268228=CARTESIAN_POINT('Ctrl Pts',(-20.774415738298,158.704075916301,661.537703348572));
#268229=CARTESIAN_POINT('Ctrl Pts',(-8.28413408366129,160.339057893189,
659.537703348572));
#268230=CARTESIAN_POINT('Ctrl Pts',(4.30813900827766,160.,657.537703348572));
#268231=CARTESIAN_POINT('Ctrl Pts',(16.9004121002166,159.660942106811,655.537703348572));
#268232=CARTESIAN_POINT('Ctrl Pts',(29.2846130745759,157.356193074143,653.537703348572));
#268233=CARTESIAN_POINT('Ctrl Pts',(41.6688140489352,155.051444041476,651.537703348572));
#268234=CARTESIAN_POINT('Ctrl Pts',(53.5400027769194,150.837754439537,649.537703348572));
#268235=CARTESIAN_POINT('Ctrl Pts',(65.4111915049037,146.624064837599,647.537703348572));
#268236=CARTESIAN_POINT('Ctrl Pts',(76.4770599218133,140.605189688823,645.537703348572));
#268237=CARTESIAN_POINT('Ctrl Pts',(87.542928338723,134.586314540048,643.537703348572));
#268238=CARTESIAN_POINT('Ctrl Pts',(97.530998038622,126.9104585261,641.537703348572));
#268239=CARTESIAN_POINT('Ctrl Pts',(107.519067738521,119.234602512152,639.537703348572));
#268240=CARTESIAN_POINT('Ctrl Pts',(116.183399296895,110.0907706828,637.537703348572));
#268241=CARTESIAN_POINT('Ctrl Pts',(124.847730855269,100.946938853448,635.537703348572));
#268242=CARTESIAN_POINT('Ctrl Pts',(131.974979673883,90.5602826949695,633.537703348572));
#268243=CARTESIAN_POINT('Ctrl Pts',(139.102228492497,80.1736265364906,631.537703348572));
#268244=CARTESIAN_POINT('Ctrl Pts',(144.516898051454,68.7998999948417,629.537703348572));
#268245=CARTESIAN_POINT('Ctrl Pts',(149.931567610411,57.4261734531929,627.537703348572));
#268246=CARTESIAN_POINT('Ctrl Pts',(153.500330774912,45.3454354230638,625.537703348572));
#268247=CARTESIAN_POINT('Ctrl Pts',(157.069093939413,33.2646973929347,623.537703348572));
#268248=CARTESIAN_POINT('Ctrl Pts',(158.704075916301,20.774415738298,621.537703348572));
#268249=CARTESIAN_POINT('Ctrl Pts',(160.339057893189,8.28413408366131,619.537703348572));
#268250=CARTESIAN_POINT('Ctrl Pts',(160.,-4.30813900827765,617.537703348572));
#268251=CARTESIAN_POINT('Ctrl Pts',(159.660942106811,-16.9004121002166,
615.537703348572));
#268252=CARTESIAN_POINT('Ctrl Pts',(157.356193074143,-29.2846130745759,
613.537703348572));
#268253=CARTESIAN_POINT('Ctrl Pts',(155.051444041476,-41.6688140489352,
611.537703348572));
#268254=CARTESIAN_POINT('Ctrl Pts',(150.837754439537,-53.5400027769194,
609.537703348572));
#268255=CARTESIAN_POINT('Ctrl Pts',(146.624064837599,-65.4111915049036,
607.537703348572));
#268256=CARTESIAN_POINT('Ctrl Pts',(140.605189688823,-76.4770599218133,
605.537703348572));
#268257=CARTESIAN_POINT('Ctrl Pts',(134.586314540048,-87.5429283387229,
603.537703348572));
#268258=CARTESIAN_POINT('Ctrl Pts',(126.9104585261,-97.530998038622,601.537703348572));
#268259=CARTESIAN_POINT('Ctrl Pts',(119.234602512152,-107.519067738521,
599.537703348572));
#268260=CARTESIAN_POINT('Ctrl Pts',(110.0907706828,-116.183399296895,597.537703348572));
#268261=CARTESIAN_POINT('Ctrl Pts',(100.946938853448,-124.847730855269,
595.537703348572));
#268262=CARTESIAN_POINT('Ctrl Pts',(90.5602826949695,-131.974979673883,
593.537703348572));
#268263=CARTESIAN_POINT('Ctrl Pts',(80.1736265364905,-139.102228492497,
591.537703348572));
#268264=CARTESIAN_POINT('Ctrl Pts',(68.7998999948417,-144.516898051454,
589.537703348572));
#268265=CARTESIAN_POINT('Ctrl Pts',(57.426173453193,-149.931567610411,587.537703348572));
#268266=CARTESIAN_POINT('Ctrl Pts',(45.3454354230638,-153.500330774912,
585.537703348572));
#268267=CARTESIAN_POINT('Ctrl Pts',(33.2646973929347,-157.069093939413,
583.537703348572));
#268268=CARTESIAN_POINT('Ctrl Pts',(20.774415738298,-158.704075916301,581.537703348572));
#268269=CARTESIAN_POINT('Ctrl Pts',(8.28413408366139,-160.339057893189,
579.537703348572));
#268270=CARTESIAN_POINT('Ctrl Pts',(-4.30813900827764,-160.,577.537703348572));
#268271=CARTESIAN_POINT('Ctrl Pts',(-16.9004121002167,-159.660942106811,
575.537703348572));
#268272=CARTESIAN_POINT('Ctrl Pts',(-29.2846130745759,-157.356193074143,
573.537703348572));
#268273=CARTESIAN_POINT('Ctrl Pts',(-41.6688140489351,-155.051444041476,
571.537703348572));
#268274=CARTESIAN_POINT('Ctrl Pts',(-53.5400027769194,-150.837754439537,
569.537703348572));
#268275=CARTESIAN_POINT('Ctrl Pts',(-65.4111915049037,-146.624064837599,
567.537703348572));
#268276=CARTESIAN_POINT('Ctrl Pts',(-76.4770599218133,-140.605189688823,
565.537703348572));
#268277=CARTESIAN_POINT('Ctrl Pts',(-87.5429283387229,-134.586314540048,
563.537703348572));
#268278=CARTESIAN_POINT('Ctrl Pts',(-97.530998038622,-126.9104585261,561.537703348572));
#268279=CARTESIAN_POINT('Ctrl Pts',(-107.519067738521,-119.234602512152,
559.537703348572));
#268280=CARTESIAN_POINT('Ctrl Pts',(-116.183399296895,-110.0907706828,557.537703348572));
#268281=CARTESIAN_POINT('Ctrl Pts',(-124.847730855269,-100.946938853448,
555.537703348572));
#268282=CARTESIAN_POINT('Ctrl Pts',(-131.974979673883,-90.5602826949695,
553.537703348572));
#268283=CARTESIAN_POINT('Ctrl Pts',(-139.102228492497,-80.1736265364905,
551.537703348572));
#268284=CARTESIAN_POINT('Ctrl Pts',(-144.516898051454,-68.7998999948417,
549.537703348572));
#268285=CARTESIAN_POINT('Ctrl Pts',(-149.931567610411,-57.426173453193,
547.537703348572));
#268286=CARTESIAN_POINT('Ctrl Pts',(-153.500330774912,-45.3454354230638,
545.537703348572));
#268287=CARTESIAN_POINT('Ctrl Pts',(-157.069093939413,-33.2646973929347,
543.537703348572));
#268288=CARTESIAN_POINT('Ctrl Pts',(-158.704075916301,-20.774415738298,
541.537703348572));
#268289=CARTESIAN_POINT('Ctrl Pts',(-160.339057893189,-8.2841340836614,
539.537703348572));
#268290=CARTESIAN_POINT('Ctrl Pts',(-160.,4.30813900827767,537.537703348572));
#268291=CARTESIAN_POINT('Origin',(4.03737035481473,0.209103844008918,539.53762260761));
#268292=CARTESIAN_POINT('Ctrl Pts',(-160.,4.30813900827767,697.537703348572));
#268293=CARTESIAN_POINT('Ctrl Pts',(-159.660942106811,16.9004121002166,
695.537703348572));
#268294=CARTESIAN_POINT('Ctrl Pts',(-157.356193074143,29.2846130745759,
693.537703348572));
#268295=CARTESIAN_POINT('Ctrl Pts',(-155.051444041476,41.6688140489352,
691.537703348572));
#268296=CARTESIAN_POINT('Ctrl Pts',(-150.837754439537,53.5400027769194,
689.537703348572));
#268297=CARTESIAN_POINT('Ctrl Pts',(-146.624064837599,65.4111915049037,
687.537703348572));
#268298=CARTESIAN_POINT('Ctrl Pts',(-140.605189688823,76.4770599218133,
685.537703348572));
#268299=CARTESIAN_POINT('Ctrl Pts',(-134.586314540048,87.542928338723,683.537703348572));
#268300=CARTESIAN_POINT('Ctrl Pts',(-126.9104585261,97.530998038622,681.537703348572));
#268301=CARTESIAN_POINT('Ctrl Pts',(-119.234602512152,107.519067738521,
679.537703348572));
#268302=CARTESIAN_POINT('Ctrl Pts',(-110.0907706828,116.183399296895,677.537703348572));
#268303=CARTESIAN_POINT('Ctrl Pts',(-100.946938853448,124.847730855269,
675.537703348572));
#268304=CARTESIAN_POINT('Ctrl Pts',(-90.5602826949695,131.974979673883,
673.537703348572));
#268305=CARTESIAN_POINT('Ctrl Pts',(-80.1736265364906,139.102228492497,
671.537703348572));
#268306=CARTESIAN_POINT('Ctrl Pts',(-68.7998999948417,144.516898051454,
669.537703348572));
#268307=CARTESIAN_POINT('Ctrl Pts',(-57.4261734531929,149.931567610411,
667.537703348572));
#268308=CARTESIAN_POINT('Ctrl Pts',(-45.3454354230638,153.500330774912,
665.537703348572));
#268309=CARTESIAN_POINT('Ctrl Pts',(-33.2646973929347,157.069093939413,
663.537703348572));
#268310=CARTESIAN_POINT('Ctrl Pts',(-20.774415738298,158.704075916301,661.537703348572));
#268311=CARTESIAN_POINT('Ctrl Pts',(-8.28413408366129,160.339057893189,
659.537703348572));
#268312=CARTESIAN_POINT('Ctrl Pts',(4.30813900827766,160.,657.537703348572));
#268313=CARTESIAN_POINT('Ctrl Pts',(16.9004121002166,159.660942106811,655.537703348572));
#268314=CARTESIAN_POINT('Ctrl Pts',(29.2846130745759,157.356193074143,653.537703348572));
#268315=CARTESIAN_POINT('Ctrl Pts',(41.6688140489352,155.051444041476,651.537703348572));
#268316=CARTESIAN_POINT('Ctrl Pts',(53.5400027769194,150.837754439537,649.537703348572));
#268317=CARTESIAN_POINT('Ctrl Pts',(65.4111915049037,146.624064837599,647.537703348572));
#268318=CARTESIAN_POINT('Ctrl Pts',(76.4770599218133,140.605189688823,645.537703348572));
#268319=CARTESIAN_POINT('Ctrl Pts',(87.542928338723,134.586314540048,643.537703348572));
#268320=CARTESIAN_POINT('Ctrl Pts',(97.530998038622,126.9104585261,641.537703348572));
#268321=CARTESIAN_POINT('Ctrl Pts',(107.519067738521,119.234602512152,639.537703348572));
#268322=CARTESIAN_POINT('Ctrl Pts',(116.183399296895,110.0907706828,637.537703348572));
#268323=CARTESIAN_POINT('Ctrl Pts',(124.847730855269,100.946938853448,635.537703348572));
#268324=CARTESIAN_POINT('Ctrl Pts',(131.974979673883,90.5602826949695,633.537703348572));
#268325=CARTESIAN_POINT('Ctrl Pts',(139.102228492497,80.1736265364906,631.537703348572));
#268326=CARTESIAN_POINT('Ctrl Pts',(144.516898051454,68.7998999948417,629.537703348572));
#268327=CARTESIAN_POINT('Ctrl Pts',(149.931567610411,57.4261734531929,627.537703348572));
#268328=CARTESIAN_POINT('Ctrl Pts',(153.500330774912,45.3454354230638,625.537703348572));
#268329=CARTESIAN_POINT('Ctrl Pts',(157.069093939413,33.2646973929347,623.537703348572));
#268330=CARTESIAN_POINT('Ctrl Pts',(158.704075916301,20.774415738298,621.537703348572));
#268331=CARTESIAN_POINT('Ctrl Pts',(160.339057893189,8.28413408366131,619.537703348572));
#268332=CARTESIAN_POINT('Ctrl Pts',(160.,-4.30813900827765,617.537703348572));
#268333=CARTESIAN_POINT('Ctrl Pts',(159.660942106811,-16.9004121002166,
615.537703348572));
#268334=CARTESIAN_POINT('Ctrl Pts',(157.356193074143,-29.2846130745759,
613.537703348572));
#268335=CARTESIAN_POINT('Ctrl Pts',(155.051444041476,-41.6688140489352,
611.537703348572));
#268336=CARTESIAN_POINT('Ctrl Pts',(150.837754439537,-53.5400027769194,
609.537703348572));
#268337=CARTESIAN_POINT('Ctrl Pts',(146.624064837599,-65.4111915049036,
607.537703348572));
#268338=CARTESIAN_POINT('Ctrl Pts',(140.605189688823,-76.4770599218133,
605.537703348572));
#268339=CARTESIAN_POINT('Ctrl Pts',(134.586314540048,-87.5429283387229,
603.537703348572));
#268340=CARTESIAN_POINT('Ctrl Pts',(126.9104585261,-97.530998038622,601.537703348572));
#268341=CARTESIAN_POINT('Ctrl Pts',(119.234602512152,-107.519067738521,
599.537703348572));
#268342=CARTESIAN_POINT('Ctrl Pts',(110.0907706828,-116.183399296895,597.537703348572));
#268343=CARTESIAN_POINT('Ctrl Pts',(100.946938853448,-124.847730855269,
595.537703348572));
#268344=CARTESIAN_POINT('Ctrl Pts',(90.5602826949695,-131.974979673883,
593.537703348572));
#268345=CARTESIAN_POINT('Ctrl Pts',(80.1736265364905,-139.102228492497,
591.537703348572));
#268346=CARTESIAN_POINT('Ctrl Pts',(68.7998999948417,-144.516898051454,
589.537703348572));
#268347=CARTESIAN_POINT('Ctrl Pts',(57.426173453193,-149.931567610411,587.537703348572));
#268348=CARTESIAN_POINT('Ctrl Pts',(45.3454354230638,-153.500330774912,
585.537703348572));
#268349=CARTESIAN_POINT('Ctrl Pts',(33.2646973929347,-157.069093939413,
583.537703348572));
#268350=CARTESIAN_POINT('Ctrl Pts',(20.774415738298,-158.704075916301,581.537703348572));
#268351=CARTESIAN_POINT('Ctrl Pts',(8.28413408366139,-160.339057893189,
579.537703348572));
#268352=CARTESIAN_POINT('Ctrl Pts',(-4.30813900827764,-160.,577.537703348572));
#268353=CARTESIAN_POINT('Ctrl Pts',(-16.9004121002167,-159.660942106811,
575.537703348572));
#268354=CARTESIAN_POINT('Ctrl Pts',(-29.2846130745759,-157.356193074143,
573.537703348572));
#268355=CARTESIAN_POINT('Ctrl Pts',(-41.6688140489351,-155.051444041476,
571.537703348572));
#268356=CARTESIAN_POINT('Ctrl Pts',(-53.5400027769194,-150.837754439537,
569.537703348572));
#268357=CARTESIAN_POINT('Ctrl Pts',(-65.4111915049037,-146.624064837599,
567.537703348572));
#268358=CARTESIAN_POINT('Ctrl Pts',(-76.4770599218133,-140.605189688823,
565.537703348572));
#268359=CARTESIAN_POINT('Ctrl Pts',(-87.5429283387229,-134.586314540048,
563.537703348572));
#268360=CARTESIAN_POINT('Ctrl Pts',(-97.530998038622,-126.9104585261,561.537703348572));
#268361=CARTESIAN_POINT('Ctrl Pts',(-107.519067738521,-119.234602512152,
559.537703348572));
#268362=CARTESIAN_POINT('Ctrl Pts',(-116.183399296895,-110.0907706828,557.537703348572));
#268363=CARTESIAN_POINT('Ctrl Pts',(-124.847730855269,-100.946938853448,
555.537703348572));
#268364=CARTESIAN_POINT('Ctrl Pts',(-131.974979673883,-90.5602826949695,
553.537703348572));
#268365=CARTESIAN_POINT('Ctrl Pts',(-139.102228492497,-80.1736265364905,
551.537703348572));
#268366=CARTESIAN_POINT('Ctrl Pts',(-144.516898051454,-68.7998999948417,
549.537703348572));
#268367=CARTESIAN_POINT('Ctrl Pts',(-149.931567610411,-57.426173453193,
547.537703348572));
#268368=CARTESIAN_POINT('Ctrl Pts',(-153.500330774912,-45.3454354230638,
545.537703348572));
#268369=CARTESIAN_POINT('Ctrl Pts',(-157.069093939413,-33.2646973929347,
543.537703348572));
#268370=CARTESIAN_POINT('Ctrl Pts',(-158.704075916301,-20.774415738298,
541.537703348572));
#268371=CARTESIAN_POINT('Ctrl Pts',(-160.339057893189,-8.2841340836614,
539.537703348572));
#268372=CARTESIAN_POINT('Ctrl Pts',(-160.,4.30813900827767,537.537703348572));
#268373=CARTESIAN_POINT('Ctrl Pts',(-130.,4.30813900827773,697.537703348572));
#268374=CARTESIAN_POINT('Ctrl Pts',(-129.660942106811,14.5393608954781,
695.537703348572));
#268375=CARTESIAN_POINT('Ctrl Pts',(-127.725542856289,24.591579123369,693.537703348572));
#268376=CARTESIAN_POINT('Ctrl Pts',(-125.790143605767,34.6437973512599,
691.537703348572));
#268377=CARTESIAN_POINT('Ctrl Pts',(-122.306058950683,44.269492945671,689.537703348572));
#268378=CARTESIAN_POINT('Ctrl Pts',(-118.821974295598,53.8951885400822,
687.537703348572));
#268379=CARTESIAN_POINT('Ctrl Pts',(-113.874993963172,62.8573449296269,
685.537703348572));
#268380=CARTESIAN_POINT('Ctrl Pts',(-108.928013630747,71.8195013191717,
683.537703348572));
#268381=CARTESIAN_POINT('Ctrl Pts',(-102.639948694852,79.8974404698478,
681.537703348572));
#268382=CARTESIAN_POINT('Ctrl Pts',(-96.3518837589562,87.9753796205239,
679.537703348572));
#268383=CARTESIAN_POINT('Ctrl Pts',(-88.8775672472037,94.9701958612987,
677.537703348572));
#268384=CARTESIAN_POINT('Ctrl Pts',(-81.4032507354512,101.965012102073,
675.537703348572));
#268385=CARTESIAN_POINT('Ctrl Pts',(-72.9267251261952,107.704469842635,
673.537703348572));
#268386=CARTESIAN_POINT('Ctrl Pts',(-64.4501995169392,113.443927583196,
671.537703348572));
#268387=CARTESIAN_POINT('Ctrl Pts',(-55.1801850026552,117.786702325803,
669.537703348572));
#268388=CARTESIAN_POINT('Ctrl Pts',(-45.9101704883713,122.12947706841,667.537703348572));
#268389=CARTESIAN_POINT('Ctrl Pts',(-36.0749255918153,124.968635286057,
665.537703348572));
#268390=CARTESIAN_POINT('Ctrl Pts',(-26.2396806952593,127.807793503704,
663.537703348572));
#268391=CARTESIAN_POINT('Ctrl Pts',(-16.081381787091,129.073425698447,661.537703348572));
#268392=CARTESIAN_POINT('Ctrl Pts',(-5.92308287892268,130.339057893189,
659.537703348572));
#268393=CARTESIAN_POINT('Ctrl Pts',(4.30813900827772,130.,657.537703348572));
#268394=CARTESIAN_POINT('Ctrl Pts',(14.5393608954781,129.660942106811,655.537703348572));
#268395=CARTESIAN_POINT('Ctrl Pts',(24.591579123369,127.725542856289,653.537703348572));
#268396=CARTESIAN_POINT('Ctrl Pts',(34.6437973512599,125.790143605767,651.537703348572));
#268397=CARTESIAN_POINT('Ctrl Pts',(44.269492945671,122.306058950683,649.537703348572));
#268398=CARTESIAN_POINT('Ctrl Pts',(53.8951885400822,118.821974295598,647.537703348572));
#268399=CARTESIAN_POINT('Ctrl Pts',(62.8573449296269,113.874993963172,645.537703348572));
#268400=CARTESIAN_POINT('Ctrl Pts',(71.8195013191717,108.928013630747,643.537703348572));
#268401=CARTESIAN_POINT('Ctrl Pts',(79.8974404698478,102.639948694852,641.537703348572));
#268402=CARTESIAN_POINT('Ctrl Pts',(87.9753796205239,96.3518837589562,639.537703348572));
#268403=CARTESIAN_POINT('Ctrl Pts',(94.9701958612986,88.8775672472037,637.537703348572));
#268404=CARTESIAN_POINT('Ctrl Pts',(101.965012102073,81.4032507354512,635.537703348572));
#268405=CARTESIAN_POINT('Ctrl Pts',(107.704469842635,72.9267251261952,633.537703348572));
#268406=CARTESIAN_POINT('Ctrl Pts',(113.443927583196,64.4501995169392,631.537703348572));
#268407=CARTESIAN_POINT('Ctrl Pts',(117.786702325803,55.1801850026552,629.537703348572));
#268408=CARTESIAN_POINT('Ctrl Pts',(122.12947706841,45.9101704883713,627.537703348572));
#268409=CARTESIAN_POINT('Ctrl Pts',(124.968635286057,36.0749255918153,625.537703348572));
#268410=CARTESIAN_POINT('Ctrl Pts',(127.807793503704,26.2396806952593,623.537703348572));
#268411=CARTESIAN_POINT('Ctrl Pts',(129.073425698447,16.081381787091,621.537703348572));
#268412=CARTESIAN_POINT('Ctrl Pts',(130.339057893189,5.92308287892268,619.537703348572));
#268413=CARTESIAN_POINT('Ctrl Pts',(130.,-4.30813900827772,617.537703348572));
#268414=CARTESIAN_POINT('Ctrl Pts',(129.660942106811,-14.5393608954781,
615.537703348572));
#268415=CARTESIAN_POINT('Ctrl Pts',(127.725542856289,-24.591579123369,613.537703348572));
#268416=CARTESIAN_POINT('Ctrl Pts',(125.790143605767,-34.6437973512599,
611.537703348572));
#268417=CARTESIAN_POINT('Ctrl Pts',(122.306058950683,-44.269492945671,609.537703348572));
#268418=CARTESIAN_POINT('Ctrl Pts',(118.821974295598,-53.8951885400822,
607.537703348572));
#268419=CARTESIAN_POINT('Ctrl Pts',(113.874993963172,-62.8573449296269,
605.537703348572));
#268420=CARTESIAN_POINT('Ctrl Pts',(108.928013630747,-71.8195013191717,
603.537703348572));
#268421=CARTESIAN_POINT('Ctrl Pts',(102.639948694852,-79.8974404698478,
601.537703348572));
#268422=CARTESIAN_POINT('Ctrl Pts',(96.3518837589563,-87.9753796205239,
599.537703348572));
#268423=CARTESIAN_POINT('Ctrl Pts',(88.8775672472037,-94.9701958612986,
597.537703348572));
#268424=CARTESIAN_POINT('Ctrl Pts',(81.4032507354513,-101.965012102073,
595.537703348572));
#268425=CARTESIAN_POINT('Ctrl Pts',(72.9267251261952,-107.704469842635,
593.537703348572));
#268426=CARTESIAN_POINT('Ctrl Pts',(64.4501995169392,-113.443927583196,
591.537703348572));
#268427=CARTESIAN_POINT('Ctrl Pts',(55.1801850026552,-117.786702325803,
589.537703348572));
#268428=CARTESIAN_POINT('Ctrl Pts',(45.9101704883713,-122.12947706841,587.537703348572));
#268429=CARTESIAN_POINT('Ctrl Pts',(36.0749255918153,-124.968635286057,
585.537703348572));
#268430=CARTESIAN_POINT('Ctrl Pts',(26.2396806952593,-127.807793503704,
583.537703348572));
#268431=CARTESIAN_POINT('Ctrl Pts',(16.081381787091,-129.073425698447,581.537703348572));
#268432=CARTESIAN_POINT('Ctrl Pts',(5.92308287892275,-130.339057893189,
579.537703348572));
#268433=CARTESIAN_POINT('Ctrl Pts',(-4.30813900827771,-130.,577.537703348572));
#268434=CARTESIAN_POINT('Ctrl Pts',(-14.5393608954782,-129.660942106811,
575.537703348572));
#268435=CARTESIAN_POINT('Ctrl Pts',(-24.591579123369,-127.725542856289,
573.537703348572));
#268436=CARTESIAN_POINT('Ctrl Pts',(-34.6437973512598,-125.790143605767,
571.537703348572));
#268437=CARTESIAN_POINT('Ctrl Pts',(-44.269492945671,-122.306058950683,
569.537703348572));
#268438=CARTESIAN_POINT('Ctrl Pts',(-53.8951885400822,-118.821974295598,
567.537703348572));
#268439=CARTESIAN_POINT('Ctrl Pts',(-62.8573449296269,-113.874993963172,
565.537703348572));
#268440=CARTESIAN_POINT('Ctrl Pts',(-71.8195013191717,-108.928013630747,
563.537703348572));
#268441=CARTESIAN_POINT('Ctrl Pts',(-79.8974404698478,-102.639948694852,
561.537703348572));
#268442=CARTESIAN_POINT('Ctrl Pts',(-87.975379620524,-96.3518837589562,
559.537703348572));
#268443=CARTESIAN_POINT('Ctrl Pts',(-94.9701958612986,-88.8775672472037,
557.537703348572));
#268444=CARTESIAN_POINT('Ctrl Pts',(-101.965012102073,-81.4032507354513,
555.537703348572));
#268445=CARTESIAN_POINT('Ctrl Pts',(-107.704469842635,-72.9267251261952,
553.537703348572));
#268446=CARTESIAN_POINT('Ctrl Pts',(-113.443927583196,-64.4501995169392,
551.537703348572));
#268447=CARTESIAN_POINT('Ctrl Pts',(-117.786702325803,-55.1801850026553,
549.537703348572));
#268448=CARTESIAN_POINT('Ctrl Pts',(-122.12947706841,-45.9101704883713,
547.537703348572));
#268449=CARTESIAN_POINT('Ctrl Pts',(-124.968635286057,-36.0749255918153,
545.537703348572));
#268450=CARTESIAN_POINT('Ctrl Pts',(-127.807793503704,-26.2396806952593,
543.537703348572));
#268451=CARTESIAN_POINT('Ctrl Pts',(-129.073425698447,-16.081381787091,
541.537703348572));
#268452=CARTESIAN_POINT('Ctrl Pts',(-130.339057893189,-5.92308287892275,
539.537703348572));
#268453=CARTESIAN_POINT('Ctrl Pts',(-130.,4.30813900827773,537.537703348572));
#268454=CARTESIAN_POINT('Ctrl Pts',(-130.,-4.30813900827845,532.462296651428));
#268455=CARTESIAN_POINT('Ctrl Pts',(-130.339057893189,5.92308287892195,
530.462296651429));
#268456=CARTESIAN_POINT('Ctrl Pts',(-129.073425698447,16.0813817870903,
528.462296651428));
#268457=CARTESIAN_POINT('Ctrl Pts',(-127.807793503705,26.2396806952586,
526.462296651429));
#268458=CARTESIAN_POINT('Ctrl Pts',(-124.968635286058,36.0749255918146,
524.462296651428));
#268459=CARTESIAN_POINT('Ctrl Pts',(-122.129477068411,45.9101704883706,
522.462296651428));
#268460=CARTESIAN_POINT('Ctrl Pts',(-117.786702325804,55.1801850026546,
520.462296651428));
#268461=CARTESIAN_POINT('Ctrl Pts',(-113.443927583196,64.4501995169386,
518.462296651428));
#268462=CARTESIAN_POINT('Ctrl Pts',(-107.704469842635,72.9267251261946,
516.462296651428));
#268463=CARTESIAN_POINT('Ctrl Pts',(-101.965012102074,81.4032507354507,
514.462296651428));
#268464=CARTESIAN_POINT('Ctrl Pts',(-94.9701958612992,88.8775672472032,
512.462296651428));
#268465=CARTESIAN_POINT('Ctrl Pts',(-87.9753796205245,96.3518837589558,
510.462296651429));
#268466=CARTESIAN_POINT('Ctrl Pts',(-79.8974404698484,102.639948694851,
508.462296651428));
#268467=CARTESIAN_POINT('Ctrl Pts',(-71.8195013191724,108.928013630747,
506.462296651428));
#268468=CARTESIAN_POINT('Ctrl Pts',(-62.8573449296276,113.874993963172,
504.462296651428));
#268469=CARTESIAN_POINT('Ctrl Pts',(-53.8951885400828,118.821974295598,
502.462296651428));
#268470=CARTESIAN_POINT('Ctrl Pts',(-44.2694929456717,122.306058950682,
500.462296651428));
#268471=CARTESIAN_POINT('Ctrl Pts',(-34.6437973512606,125.790143605767,
498.462296651429));
#268472=CARTESIAN_POINT('Ctrl Pts',(-24.5915791233697,127.725542856289,
496.462296651428));
#268473=CARTESIAN_POINT('Ctrl Pts',(-14.5393608954789,129.660942106811,
494.462296651428));
#268474=CARTESIAN_POINT('Ctrl Pts',(-4.30813900827846,130.,492.462296651428));
#268475=CARTESIAN_POINT('Ctrl Pts',(5.92308287892194,130.339057893189,490.462296651429));
#268476=CARTESIAN_POINT('Ctrl Pts',(16.0813817870903,129.073425698447,488.462296651428));
#268477=CARTESIAN_POINT('Ctrl Pts',(26.2396806952586,127.807793503705,486.462296651428));
#268478=CARTESIAN_POINT('Ctrl Pts',(36.0749255918146,124.968635286058,484.462296651428));
#268479=CARTESIAN_POINT('Ctrl Pts',(45.9101704883706,122.129477068411,482.462296651428));
#268480=CARTESIAN_POINT('Ctrl Pts',(55.1801850026546,117.786702325804,480.462296651428));
#268481=CARTESIAN_POINT('Ctrl Pts',(64.4501995169386,113.443927583196,478.462296651429));
#268482=CARTESIAN_POINT('Ctrl Pts',(72.9267251261946,107.704469842635,476.462296651428));
#268483=CARTESIAN_POINT('Ctrl Pts',(81.4032507354506,101.965012102074,474.462296651428));
#268484=CARTESIAN_POINT('Ctrl Pts',(88.8775672472032,94.9701958612992,472.462296651428));
#268485=CARTESIAN_POINT('Ctrl Pts',(96.3518837589558,87.9753796205245,470.462296651428));
#268486=CARTESIAN_POINT('Ctrl Pts',(102.639948694851,79.8974404698484,468.462296651428));
#268487=CARTESIAN_POINT('Ctrl Pts',(108.928013630747,71.8195013191724,466.462296651428));
#268488=CARTESIAN_POINT('Ctrl Pts',(113.874993963172,62.8573449296276,464.462296651428));
#268489=CARTESIAN_POINT('Ctrl Pts',(118.821974295598,53.8951885400829,462.462296651428));
#268490=CARTESIAN_POINT('Ctrl Pts',(122.306058950682,44.2694929456717,460.462296651428));
#268491=CARTESIAN_POINT('Ctrl Pts',(125.790143605767,34.6437973512606,458.462296651429));
#268492=CARTESIAN_POINT('Ctrl Pts',(127.725542856289,24.5915791233698,456.462296651428));
#268493=CARTESIAN_POINT('Ctrl Pts',(129.660942106811,14.5393608954789,454.462296651429));
#268494=CARTESIAN_POINT('Ctrl Pts',(130.,4.30813900827846,452.462296651428));
#268495=CARTESIAN_POINT('Ctrl Pts',(130.339057893189,-5.92308287892194,
450.462296651428));
#268496=CARTESIAN_POINT('Ctrl Pts',(129.073425698447,-16.0813817870903,
448.462296651429));
#268497=CARTESIAN_POINT('Ctrl Pts',(127.807793503705,-26.2396806952586,
446.462296651429));
#268498=CARTESIAN_POINT('Ctrl Pts',(124.968635286058,-36.0749255918146,
444.462296651429));
#268499=CARTESIAN_POINT('Ctrl Pts',(122.129477068411,-45.9101704883706,
442.462296651429));
#268500=CARTESIAN_POINT('Ctrl Pts',(117.786702325804,-55.1801850026546,
440.462296651428));
#268501=CARTESIAN_POINT('Ctrl Pts',(113.443927583196,-64.4501995169386,
438.462296651429));
#268502=CARTESIAN_POINT('Ctrl Pts',(107.704469842635,-72.9267251261946,
436.462296651428));
#268503=CARTESIAN_POINT('Ctrl Pts',(101.965012102074,-81.4032507354506,
434.462296651429));
#268504=CARTESIAN_POINT('Ctrl Pts',(94.9701958612992,-88.8775672472032,
432.462296651428));
#268505=CARTESIAN_POINT('Ctrl Pts',(87.9753796205246,-96.3518837589557,
430.462296651429));
#268506=CARTESIAN_POINT('Ctrl Pts',(79.8974404698484,-102.639948694851,
428.462296651429));
#268507=CARTESIAN_POINT('Ctrl Pts',(71.8195013191723,-108.928013630747,
426.462296651428));
#268508=CARTESIAN_POINT('Ctrl Pts',(62.8573449296276,-113.874993963172,
424.462296651428));
#268509=CARTESIAN_POINT('Ctrl Pts',(53.8951885400829,-118.821974295598,
422.462296651428));
#268510=CARTESIAN_POINT('Ctrl Pts',(44.2694929456717,-122.306058950682,
420.462296651428));
#268511=CARTESIAN_POINT('Ctrl Pts',(34.6437973512606,-125.790143605767,
418.462296651429));
#268512=CARTESIAN_POINT('Ctrl Pts',(24.5915791233698,-127.725542856289,
416.462296651428));
#268513=CARTESIAN_POINT('Ctrl Pts',(14.5393608954789,-129.660942106811,
414.462296651429));
#268514=CARTESIAN_POINT('Ctrl Pts',(4.30813900827847,-130.,412.462296651428));
#268515=CARTESIAN_POINT('Ctrl Pts',(-5.92308287892199,-130.339057893189,
410.462296651428));
#268516=CARTESIAN_POINT('Ctrl Pts',(-16.0813817870903,-129.073425698447,
408.462296651428));
#268517=CARTESIAN_POINT('Ctrl Pts',(-26.2396806952585,-127.807793503705,
406.462296651429));
#268518=CARTESIAN_POINT('Ctrl Pts',(-36.0749255918146,-124.968635286058,
404.462296651428));
#268519=CARTESIAN_POINT('Ctrl Pts',(-45.9101704883706,-122.129477068411,
402.462296651429));
#268520=CARTESIAN_POINT('Ctrl Pts',(-55.1801850026546,-117.786702325804,
400.462296651428));
#268521=CARTESIAN_POINT('Ctrl Pts',(-64.4501995169385,-113.443927583197,
398.462296651429));
#268522=CARTESIAN_POINT('Ctrl Pts',(-72.9267251261946,-107.704469842635,
396.462296651428));
#268523=CARTESIAN_POINT('Ctrl Pts',(-81.4032507354507,-101.965012102074,
394.462296651429));
#268524=CARTESIAN_POINT('Ctrl Pts',(-88.8775672472032,-94.9701958612992,
392.462296651428));
#268525=CARTESIAN_POINT('Ctrl Pts',(-96.3518837589557,-87.9753796205246,
390.462296651428));
#268526=CARTESIAN_POINT('Ctrl Pts',(-102.639948694851,-79.8974404698484,
388.462296651428));
#268527=CARTESIAN_POINT('Ctrl Pts',(-108.928013630747,-71.8195013191723,
386.462296651428));
#268528=CARTESIAN_POINT('Ctrl Pts',(-113.874993963172,-62.8573449296276,
384.462296651428));
#268529=CARTESIAN_POINT('Ctrl Pts',(-118.821974295598,-53.8951885400829,
382.462296651429));
#268530=CARTESIAN_POINT('Ctrl Pts',(-122.306058950682,-44.2694929456718,
380.462296651428));
#268531=CARTESIAN_POINT('Ctrl Pts',(-125.790143605767,-34.6437973512606,
378.462296651429));
#268532=CARTESIAN_POINT('Ctrl Pts',(-127.725542856289,-24.5915791233698,
376.462296651428));
#268533=CARTESIAN_POINT('Ctrl Pts',(-129.660942106811,-14.5393608954789,
374.462296651428));
#268534=CARTESIAN_POINT('Ctrl Pts',(-130.,-4.30813900827845,372.462296651428));
#268535=CARTESIAN_POINT('Ctrl Pts',(-160.,-4.30813900827851,532.462296651429));
#268536=CARTESIAN_POINT('Ctrl Pts',(-160.339057893189,8.28413408366045,
530.462296651429));
#268537=CARTESIAN_POINT('Ctrl Pts',(-158.704075916301,20.7744157382972,
528.462296651429));
#268538=CARTESIAN_POINT('Ctrl Pts',(-157.069093939413,33.2646973929339,
526.462296651429));
#268539=CARTESIAN_POINT('Ctrl Pts',(-153.500330774912,45.345435423063,524.462296651428));
#268540=CARTESIAN_POINT('Ctrl Pts',(-149.931567610412,57.4261734531921,
522.462296651429));
#268541=CARTESIAN_POINT('Ctrl Pts',(-144.516898051455,68.7998999948409,
520.462296651428));
#268542=CARTESIAN_POINT('Ctrl Pts',(-139.102228492498,80.1736265364898,
518.462296651428));
#268543=CARTESIAN_POINT('Ctrl Pts',(-131.974979673884,90.5602826949688,
516.462296651428));
#268544=CARTESIAN_POINT('Ctrl Pts',(-124.84773085527,100.946938853448,514.462296651429));
#268545=CARTESIAN_POINT('Ctrl Pts',(-116.183399296896,110.0907706828,512.462296651428));
#268546=CARTESIAN_POINT('Ctrl Pts',(-107.519067738522,119.234602512151,
510.462296651429));
#268547=CARTESIAN_POINT('Ctrl Pts',(-97.5309980386227,126.9104585261,508.462296651429));
#268548=CARTESIAN_POINT('Ctrl Pts',(-87.5429283387237,134.586314540048,
506.462296651428));
#268549=CARTESIAN_POINT('Ctrl Pts',(-76.4770599218141,140.605189688823,
504.462296651429));
#268550=CARTESIAN_POINT('Ctrl Pts',(-65.4111915049045,146.624064837598,
502.462296651429));
#268551=CARTESIAN_POINT('Ctrl Pts',(-53.5400027769202,150.837754439537,
500.462296651429));
#268552=CARTESIAN_POINT('Ctrl Pts',(-41.668814048936,155.051444041475,498.462296651429));
#268553=CARTESIAN_POINT('Ctrl Pts',(-29.2846130745767,157.356193074143,
496.462296651429));
#268554=CARTESIAN_POINT('Ctrl Pts',(-16.9004121002175,159.660942106811,
494.462296651429));
#268555=CARTESIAN_POINT('Ctrl Pts',(-4.30813900827852,160.,492.462296651428));
#268556=CARTESIAN_POINT('Ctrl Pts',(8.28413408366043,160.339057893189,490.462296651429));
#268557=CARTESIAN_POINT('Ctrl Pts',(20.7744157382972,158.704075916301,488.462296651429));
#268558=CARTESIAN_POINT('Ctrl Pts',(33.2646973929339,157.069093939413,486.462296651429));
#268559=CARTESIAN_POINT('Ctrl Pts',(45.345435423063,153.500330774912,484.462296651429));
#268560=CARTESIAN_POINT('Ctrl Pts',(57.4261734531921,149.931567610412,482.462296651429));
#268561=CARTESIAN_POINT('Ctrl Pts',(68.7998999948409,144.516898051455,480.462296651428));
#268562=CARTESIAN_POINT('Ctrl Pts',(80.1736265364898,139.102228492498,478.462296651429));
#268563=CARTESIAN_POINT('Ctrl Pts',(90.5602826949688,131.974979673884,476.462296651428));
#268564=CARTESIAN_POINT('Ctrl Pts',(100.946938853448,124.84773085527,474.462296651429));
#268565=CARTESIAN_POINT('Ctrl Pts',(110.0907706828,116.183399296896,472.462296651429));
#268566=CARTESIAN_POINT('Ctrl Pts',(119.234602512151,107.519067738522,470.462296651429));
#268567=CARTESIAN_POINT('Ctrl Pts',(126.9104585261,97.5309980386227,468.462296651429));
#268568=CARTESIAN_POINT('Ctrl Pts',(134.586314540048,87.5429283387237,466.462296651429));
#268569=CARTESIAN_POINT('Ctrl Pts',(140.605189688823,76.4770599218141,464.462296651429));
#268570=CARTESIAN_POINT('Ctrl Pts',(146.624064837598,65.4111915049045,462.462296651429));
#268571=CARTESIAN_POINT('Ctrl Pts',(150.837754439537,53.5400027769202,460.462296651429));
#268572=CARTESIAN_POINT('Ctrl Pts',(155.051444041475,41.668814048936,458.462296651429));
#268573=CARTESIAN_POINT('Ctrl Pts',(157.356193074143,29.2846130745767,456.462296651429));
#268574=CARTESIAN_POINT('Ctrl Pts',(159.660942106811,16.9004121002175,454.462296651429));
#268575=CARTESIAN_POINT('Ctrl Pts',(160.,4.30813900827853,452.462296651429));
#268576=CARTESIAN_POINT('Ctrl Pts',(160.339057893189,-8.28413408366043,
450.462296651429));
#268577=CARTESIAN_POINT('Ctrl Pts',(158.704075916301,-20.7744157382971,
448.462296651429));
#268578=CARTESIAN_POINT('Ctrl Pts',(157.069093939413,-33.2646973929339,
446.462296651429));
#268579=CARTESIAN_POINT('Ctrl Pts',(153.500330774912,-45.345435423063,444.462296651429));
#268580=CARTESIAN_POINT('Ctrl Pts',(149.931567610412,-57.4261734531921,
442.462296651429));
#268581=CARTESIAN_POINT('Ctrl Pts',(144.516898051455,-68.7998999948409,
440.462296651429));
#268582=CARTESIAN_POINT('Ctrl Pts',(139.102228492498,-80.1736265364898,
438.462296651429));
#268583=CARTESIAN_POINT('Ctrl Pts',(131.974979673884,-90.5602826949688,
436.462296651429));
#268584=CARTESIAN_POINT('Ctrl Pts',(124.84773085527,-100.946938853448,434.462296651429));
#268585=CARTESIAN_POINT('Ctrl Pts',(116.183399296896,-110.0907706828,432.462296651429));
#268586=CARTESIAN_POINT('Ctrl Pts',(107.519067738522,-119.234602512151,
430.462296651429));
#268587=CARTESIAN_POINT('Ctrl Pts',(97.5309980386227,-126.9104585261,428.462296651429));
#268588=CARTESIAN_POINT('Ctrl Pts',(87.5429283387236,-134.586314540048,
426.462296651429));
#268589=CARTESIAN_POINT('Ctrl Pts',(76.4770599218141,-140.605189688823,
424.462296651429));
#268590=CARTESIAN_POINT('Ctrl Pts',(65.4111915049046,-146.624064837598,
422.462296651429));
#268591=CARTESIAN_POINT('Ctrl Pts',(53.5400027769202,-150.837754439537,
420.462296651429));
#268592=CARTESIAN_POINT('Ctrl Pts',(41.6688140489359,-155.051444041475,
418.462296651429));
#268593=CARTESIAN_POINT('Ctrl Pts',(29.2846130745768,-157.356193074143,
416.462296651429));
#268594=CARTESIAN_POINT('Ctrl Pts',(16.9004121002176,-159.660942106811,
414.462296651429));
#268595=CARTESIAN_POINT('Ctrl Pts',(4.30813900827854,-160.,412.462296651429));
#268596=CARTESIAN_POINT('Ctrl Pts',(-8.28413408366049,-160.339057893189,
410.462296651429));
#268597=CARTESIAN_POINT('Ctrl Pts',(-20.7744157382971,-158.704075916301,
408.462296651429));
#268598=CARTESIAN_POINT('Ctrl Pts',(-33.2646973929338,-157.069093939413,
406.462296651429));
#268599=CARTESIAN_POINT('Ctrl Pts',(-45.345435423063,-153.500330774912,
404.462296651429));
#268600=CARTESIAN_POINT('Ctrl Pts',(-57.4261734531921,-149.931567610412,
402.462296651429));
#268601=CARTESIAN_POINT('Ctrl Pts',(-68.7998999948409,-144.516898051455,
400.462296651429));
#268602=CARTESIAN_POINT('Ctrl Pts',(-80.1736265364897,-139.102228492498,
398.462296651429));
#268603=CARTESIAN_POINT('Ctrl Pts',(-90.5602826949688,-131.974979673884,
396.462296651429));
#268604=CARTESIAN_POINT('Ctrl Pts',(-100.946938853448,-124.84773085527,
394.462296651429));
#268605=CARTESIAN_POINT('Ctrl Pts',(-110.0907706828,-116.183399296896,392.462296651429));
#268606=CARTESIAN_POINT('Ctrl Pts',(-119.234602512151,-107.519067738522,
390.462296651429));
#268607=CARTESIAN_POINT('Ctrl Pts',(-126.9104585261,-97.5309980386227,388.462296651429));
#268608=CARTESIAN_POINT('Ctrl Pts',(-134.586314540048,-87.5429283387236,
386.462296651429));
#268609=CARTESIAN_POINT('Ctrl Pts',(-140.605189688823,-76.4770599218141,
384.462296651429));
#268610=CARTESIAN_POINT('Ctrl Pts',(-146.624064837598,-65.4111915049046,
382.462296651429));
#268611=CARTESIAN_POINT('Ctrl Pts',(-150.837754439537,-53.5400027769203,
380.462296651429));
#268612=CARTESIAN_POINT('Ctrl Pts',(-155.051444041475,-41.668814048936,
378.462296651429));
#268613=CARTESIAN_POINT('Ctrl Pts',(-157.356193074143,-29.2846130745768,
376.462296651429));
#268614=CARTESIAN_POINT('Ctrl Pts',(-159.660942106811,-16.9004121002176,
374.462296651429));
#268615=CARTESIAN_POINT('Ctrl Pts',(-160.,-4.30813900827851,372.462296651429));
#268616=CARTESIAN_POINT('Origin',(4.03737035483175,-0.209103843988196,530.46237739249));
#268617=CARTESIAN_POINT('Ctrl Pts',(-160.,-4.30813900827851,532.462296651429));
#268618=CARTESIAN_POINT('Ctrl Pts',(-160.339057893189,8.28413408366045,
530.462296651429));
#268619=CARTESIAN_POINT('Ctrl Pts',(-158.704075916301,20.7744157382972,
528.462296651429));
#268620=CARTESIAN_POINT('Ctrl Pts',(-157.069093939413,33.2646973929339,
526.462296651429));
#268621=CARTESIAN_POINT('Ctrl Pts',(-153.500330774912,45.345435423063,524.462296651428));
#268622=CARTESIAN_POINT('Ctrl Pts',(-149.931567610412,57.4261734531921,
522.462296651429));
#268623=CARTESIAN_POINT('Ctrl Pts',(-144.516898051455,68.7998999948409,
520.462296651428));
#268624=CARTESIAN_POINT('Ctrl Pts',(-139.102228492498,80.1736265364898,
518.462296651428));
#268625=CARTESIAN_POINT('Ctrl Pts',(-131.974979673884,90.5602826949688,
516.462296651428));
#268626=CARTESIAN_POINT('Ctrl Pts',(-124.84773085527,100.946938853448,514.462296651429));
#268627=CARTESIAN_POINT('Ctrl Pts',(-116.183399296896,110.0907706828,512.462296651428));
#268628=CARTESIAN_POINT('Ctrl Pts',(-107.519067738522,119.234602512151,
510.462296651429));
#268629=CARTESIAN_POINT('Ctrl Pts',(-97.5309980386227,126.9104585261,508.462296651429));
#268630=CARTESIAN_POINT('Ctrl Pts',(-87.5429283387237,134.586314540048,
506.462296651428));
#268631=CARTESIAN_POINT('Ctrl Pts',(-76.4770599218141,140.605189688823,
504.462296651429));
#268632=CARTESIAN_POINT('Ctrl Pts',(-65.4111915049045,146.624064837598,
502.462296651429));
#268633=CARTESIAN_POINT('Ctrl Pts',(-53.5400027769202,150.837754439537,
500.462296651429));
#268634=CARTESIAN_POINT('Ctrl Pts',(-41.668814048936,155.051444041475,498.462296651429));
#268635=CARTESIAN_POINT('Ctrl Pts',(-29.2846130745767,157.356193074143,
496.462296651429));
#268636=CARTESIAN_POINT('Ctrl Pts',(-16.9004121002175,159.660942106811,
494.462296651429));
#268637=CARTESIAN_POINT('Ctrl Pts',(-4.30813900827852,160.,492.462296651428));
#268638=CARTESIAN_POINT('Ctrl Pts',(8.28413408366043,160.339057893189,490.462296651429));
#268639=CARTESIAN_POINT('Ctrl Pts',(20.7744157382972,158.704075916301,488.462296651429));
#268640=CARTESIAN_POINT('Ctrl Pts',(33.2646973929339,157.069093939413,486.462296651429));
#268641=CARTESIAN_POINT('Ctrl Pts',(45.345435423063,153.500330774912,484.462296651429));
#268642=CARTESIAN_POINT('Ctrl Pts',(57.4261734531921,149.931567610412,482.462296651429));
#268643=CARTESIAN_POINT('Ctrl Pts',(68.7998999948409,144.516898051455,480.462296651428));
#268644=CARTESIAN_POINT('Ctrl Pts',(80.1736265364898,139.102228492498,478.462296651429));
#268645=CARTESIAN_POINT('Ctrl Pts',(90.5602826949688,131.974979673884,476.462296651428));
#268646=CARTESIAN_POINT('Ctrl Pts',(100.946938853448,124.84773085527,474.462296651429));
#268647=CARTESIAN_POINT('Ctrl Pts',(110.0907706828,116.183399296896,472.462296651429));
#268648=CARTESIAN_POINT('Ctrl Pts',(119.234602512151,107.519067738522,470.462296651429));
#268649=CARTESIAN_POINT('Ctrl Pts',(126.9104585261,97.5309980386227,468.462296651429));
#268650=CARTESIAN_POINT('Ctrl Pts',(134.586314540048,87.5429283387237,466.462296651429));
#268651=CARTESIAN_POINT('Ctrl Pts',(140.605189688823,76.4770599218141,464.462296651429));
#268652=CARTESIAN_POINT('Ctrl Pts',(146.624064837598,65.4111915049045,462.462296651429));
#268653=CARTESIAN_POINT('Ctrl Pts',(150.837754439537,53.5400027769202,460.462296651429));
#268654=CARTESIAN_POINT('Ctrl Pts',(155.051444041475,41.668814048936,458.462296651429));
#268655=CARTESIAN_POINT('Ctrl Pts',(157.356193074143,29.2846130745767,456.462296651429));
#268656=CARTESIAN_POINT('Ctrl Pts',(159.660942106811,16.9004121002175,454.462296651429));
#268657=CARTESIAN_POINT('Ctrl Pts',(160.,4.30813900827853,452.462296651429));
#268658=CARTESIAN_POINT('Ctrl Pts',(160.339057893189,-8.28413408366043,
450.462296651429));
#268659=CARTESIAN_POINT('Ctrl Pts',(158.704075916301,-20.7744157382971,
448.462296651429));
#268660=CARTESIAN_POINT('Ctrl Pts',(157.069093939413,-33.2646973929339,
446.462296651429));
#268661=CARTESIAN_POINT('Ctrl Pts',(153.500330774912,-45.345435423063,444.462296651429));
#268662=CARTESIAN_POINT('Ctrl Pts',(149.931567610412,-57.4261734531921,
442.462296651429));
#268663=CARTESIAN_POINT('Ctrl Pts',(144.516898051455,-68.7998999948409,
440.462296651429));
#268664=CARTESIAN_POINT('Ctrl Pts',(139.102228492498,-80.1736265364898,
438.462296651429));
#268665=CARTESIAN_POINT('Ctrl Pts',(131.974979673884,-90.5602826949688,
436.462296651429));
#268666=CARTESIAN_POINT('Ctrl Pts',(124.84773085527,-100.946938853448,434.462296651429));
#268667=CARTESIAN_POINT('Ctrl Pts',(116.183399296896,-110.0907706828,432.462296651429));
#268668=CARTESIAN_POINT('Ctrl Pts',(107.519067738522,-119.234602512151,
430.462296651429));
#268669=CARTESIAN_POINT('Ctrl Pts',(97.5309980386227,-126.9104585261,428.462296651429));
#268670=CARTESIAN_POINT('Ctrl Pts',(87.5429283387236,-134.586314540048,
426.462296651429));
#268671=CARTESIAN_POINT('Ctrl Pts',(76.4770599218141,-140.605189688823,
424.462296651429));
#268672=CARTESIAN_POINT('Ctrl Pts',(65.4111915049046,-146.624064837598,
422.462296651429));
#268673=CARTESIAN_POINT('Ctrl Pts',(53.5400027769202,-150.837754439537,
420.462296651429));
#268674=CARTESIAN_POINT('Ctrl Pts',(41.6688140489359,-155.051444041475,
418.462296651429));
#268675=CARTESIAN_POINT('Ctrl Pts',(29.2846130745768,-157.356193074143,
416.462296651429));
#268676=CARTESIAN_POINT('Ctrl Pts',(16.9004121002176,-159.660942106811,
414.462296651429));
#268677=CARTESIAN_POINT('Ctrl Pts',(4.30813900827854,-160.,412.462296651429));
#268678=CARTESIAN_POINT('Ctrl Pts',(-8.28413408366049,-160.339057893189,
410.462296651429));
#268679=CARTESIAN_POINT('Ctrl Pts',(-20.7744157382971,-158.704075916301,
408.462296651429));
#268680=CARTESIAN_POINT('Ctrl Pts',(-33.2646973929338,-157.069093939413,
406.462296651429));
#268681=CARTESIAN_POINT('Ctrl Pts',(-45.345435423063,-153.500330774912,
404.462296651429));
#268682=CARTESIAN_POINT('Ctrl Pts',(-57.4261734531921,-149.931567610412,
402.462296651429));
#268683=CARTESIAN_POINT('Ctrl Pts',(-68.7998999948409,-144.516898051455,
400.462296651429));
#268684=CARTESIAN_POINT('Ctrl Pts',(-80.1736265364897,-139.102228492498,
398.462296651429));
#268685=CARTESIAN_POINT('Ctrl Pts',(-90.5602826949688,-131.974979673884,
396.462296651429));
#268686=CARTESIAN_POINT('Ctrl Pts',(-100.946938853448,-124.84773085527,
394.462296651429));
#268687=CARTESIAN_POINT('Ctrl Pts',(-110.0907706828,-116.183399296896,392.462296651429));
#268688=CARTESIAN_POINT('Ctrl Pts',(-119.234602512151,-107.519067738522,
390.462296651429));
#268689=CARTESIAN_POINT('Ctrl Pts',(-126.9104585261,-97.5309980386227,388.462296651429));
#268690=CARTESIAN_POINT('Ctrl Pts',(-134.586314540048,-87.5429283387236,
386.462296651429));
#268691=CARTESIAN_POINT('Ctrl Pts',(-140.605189688823,-76.4770599218141,
384.462296651429));
#268692=CARTESIAN_POINT('Ctrl Pts',(-146.624064837598,-65.4111915049046,
382.462296651429));
#268693=CARTESIAN_POINT('Ctrl Pts',(-150.837754439537,-53.5400027769203,
380.462296651429));
#268694=CARTESIAN_POINT('Ctrl Pts',(-155.051444041475,-41.668814048936,
378.462296651429));
#268695=CARTESIAN_POINT('Ctrl Pts',(-157.356193074143,-29.2846130745768,
376.462296651429));
#268696=CARTESIAN_POINT('Ctrl Pts',(-159.660942106811,-16.9004121002176,
374.462296651429));
#268697=CARTESIAN_POINT('Ctrl Pts',(-160.,-4.30813900827851,372.462296651429));
#268698=CARTESIAN_POINT('Ctrl Pts',(-160.,4.30813900827767,537.537703348572));
#268699=CARTESIAN_POINT('Ctrl Pts',(-159.660942106811,16.9004121002166,
535.537703348572));
#268700=CARTESIAN_POINT('Ctrl Pts',(-157.356193074143,29.2846130745759,
533.537703348572));
#268701=CARTESIAN_POINT('Ctrl Pts',(-155.051444041476,41.6688140489352,
531.537703348572));
#268702=CARTESIAN_POINT('Ctrl Pts',(-150.837754439537,53.5400027769194,
529.537703348572));
#268703=CARTESIAN_POINT('Ctrl Pts',(-146.624064837599,65.4111915049037,
527.537703348572));
#268704=CARTESIAN_POINT('Ctrl Pts',(-140.605189688823,76.4770599218133,
525.537703348572));
#268705=CARTESIAN_POINT('Ctrl Pts',(-134.586314540048,87.542928338723,523.537703348572));
#268706=CARTESIAN_POINT('Ctrl Pts',(-126.9104585261,97.530998038622,521.537703348572));
#268707=CARTESIAN_POINT('Ctrl Pts',(-119.234602512152,107.519067738521,
519.537703348572));
#268708=CARTESIAN_POINT('Ctrl Pts',(-110.0907706828,116.183399296895,517.537703348572));
#268709=CARTESIAN_POINT('Ctrl Pts',(-100.946938853448,124.847730855269,
515.537703348572));
#268710=CARTESIAN_POINT('Ctrl Pts',(-90.5602826949695,131.974979673883,
513.537703348572));
#268711=CARTESIAN_POINT('Ctrl Pts',(-80.1736265364906,139.102228492497,
511.537703348572));
#268712=CARTESIAN_POINT('Ctrl Pts',(-68.7998999948417,144.516898051454,
509.537703348572));
#268713=CARTESIAN_POINT('Ctrl Pts',(-57.4261734531929,149.931567610411,
507.537703348572));
#268714=CARTESIAN_POINT('Ctrl Pts',(-45.3454354230638,153.500330774912,
505.537703348572));
#268715=CARTESIAN_POINT('Ctrl Pts',(-33.2646973929347,157.069093939413,
503.537703348572));
#268716=CARTESIAN_POINT('Ctrl Pts',(-20.774415738298,158.704075916301,501.537703348572));
#268717=CARTESIAN_POINT('Ctrl Pts',(-8.28413408366129,160.339057893189,
499.537703348572));
#268718=CARTESIAN_POINT('Ctrl Pts',(4.30813900827766,160.,497.537703348572));
#268719=CARTESIAN_POINT('Ctrl Pts',(16.9004121002166,159.660942106811,495.537703348572));
#268720=CARTESIAN_POINT('Ctrl Pts',(29.2846130745759,157.356193074143,493.537703348572));
#268721=CARTESIAN_POINT('Ctrl Pts',(41.6688140489352,155.051444041476,491.537703348572));
#268722=CARTESIAN_POINT('Ctrl Pts',(53.5400027769194,150.837754439537,489.537703348572));
#268723=CARTESIAN_POINT('Ctrl Pts',(65.4111915049037,146.624064837599,487.537703348572));
#268724=CARTESIAN_POINT('Ctrl Pts',(76.4770599218133,140.605189688823,485.537703348572));
#268725=CARTESIAN_POINT('Ctrl Pts',(87.542928338723,134.586314540048,483.537703348572));
#268726=CARTESIAN_POINT('Ctrl Pts',(97.530998038622,126.9104585261,481.537703348572));
#268727=CARTESIAN_POINT('Ctrl Pts',(107.519067738521,119.234602512152,479.537703348572));
#268728=CARTESIAN_POINT('Ctrl Pts',(116.183399296895,110.0907706828,477.537703348572));
#268729=CARTESIAN_POINT('Ctrl Pts',(124.847730855269,100.946938853448,475.537703348572));
#268730=CARTESIAN_POINT('Ctrl Pts',(131.974979673883,90.5602826949695,473.537703348572));
#268731=CARTESIAN_POINT('Ctrl Pts',(139.102228492497,80.1736265364906,471.537703348572));
#268732=CARTESIAN_POINT('Ctrl Pts',(144.516898051454,68.7998999948417,469.537703348572));
#268733=CARTESIAN_POINT('Ctrl Pts',(149.931567610411,57.4261734531929,467.537703348572));
#268734=CARTESIAN_POINT('Ctrl Pts',(153.500330774912,45.3454354230638,465.537703348572));
#268735=CARTESIAN_POINT('Ctrl Pts',(157.069093939413,33.2646973929347,463.537703348572));
#268736=CARTESIAN_POINT('Ctrl Pts',(158.704075916301,20.774415738298,461.537703348572));
#268737=CARTESIAN_POINT('Ctrl Pts',(160.339057893189,8.28413408366131,459.537703348572));
#268738=CARTESIAN_POINT('Ctrl Pts',(160.,-4.30813900827765,457.537703348572));
#268739=CARTESIAN_POINT('Ctrl Pts',(159.660942106811,-16.9004121002166,
455.537703348572));
#268740=CARTESIAN_POINT('Ctrl Pts',(157.356193074143,-29.2846130745759,
453.537703348572));
#268741=CARTESIAN_POINT('Ctrl Pts',(155.051444041476,-41.6688140489352,
451.537703348572));
#268742=CARTESIAN_POINT('Ctrl Pts',(150.837754439537,-53.5400027769194,
449.537703348572));
#268743=CARTESIAN_POINT('Ctrl Pts',(146.624064837599,-65.4111915049036,
447.537703348572));
#268744=CARTESIAN_POINT('Ctrl Pts',(140.605189688823,-76.4770599218133,
445.537703348572));
#268745=CARTESIAN_POINT('Ctrl Pts',(134.586314540048,-87.5429283387229,
443.537703348572));
#268746=CARTESIAN_POINT('Ctrl Pts',(126.9104585261,-97.530998038622,441.537703348572));
#268747=CARTESIAN_POINT('Ctrl Pts',(119.234602512152,-107.519067738521,
439.537703348572));
#268748=CARTESIAN_POINT('Ctrl Pts',(110.0907706828,-116.183399296895,437.537703348572));
#268749=CARTESIAN_POINT('Ctrl Pts',(100.946938853448,-124.847730855269,
435.537703348572));
#268750=CARTESIAN_POINT('Ctrl Pts',(90.5602826949695,-131.974979673883,
433.537703348572));
#268751=CARTESIAN_POINT('Ctrl Pts',(80.1736265364905,-139.102228492497,
431.537703348572));
#268752=CARTESIAN_POINT('Ctrl Pts',(68.7998999948417,-144.516898051454,
429.537703348572));
#268753=CARTESIAN_POINT('Ctrl Pts',(57.426173453193,-149.931567610411,427.537703348572));
#268754=CARTESIAN_POINT('Ctrl Pts',(45.3454354230638,-153.500330774912,
425.537703348572));
#268755=CARTESIAN_POINT('Ctrl Pts',(33.2646973929347,-157.069093939413,
423.537703348572));
#268756=CARTESIAN_POINT('Ctrl Pts',(20.774415738298,-158.704075916301,421.537703348572));
#268757=CARTESIAN_POINT('Ctrl Pts',(8.28413408366139,-160.339057893189,
419.537703348572));
#268758=CARTESIAN_POINT('Ctrl Pts',(-4.30813900827764,-160.,417.537703348572));
#268759=CARTESIAN_POINT('Ctrl Pts',(-16.9004121002167,-159.660942106811,
415.537703348572));
#268760=CARTESIAN_POINT('Ctrl Pts',(-29.2846130745759,-157.356193074143,
413.537703348572));
#268761=CARTESIAN_POINT('Ctrl Pts',(-41.6688140489351,-155.051444041476,
411.537703348572));
#268762=CARTESIAN_POINT('Ctrl Pts',(-53.5400027769194,-150.837754439537,
409.537703348572));
#268763=CARTESIAN_POINT('Ctrl Pts',(-65.4111915049037,-146.624064837599,
407.537703348572));
#268764=CARTESIAN_POINT('Ctrl Pts',(-76.4770599218133,-140.605189688823,
405.537703348572));
#268765=CARTESIAN_POINT('Ctrl Pts',(-87.5429283387229,-134.586314540048,
403.537703348572));
#268766=CARTESIAN_POINT('Ctrl Pts',(-97.530998038622,-126.9104585261,401.537703348572));
#268767=CARTESIAN_POINT('Ctrl Pts',(-107.519067738521,-119.234602512152,
399.537703348572));
#268768=CARTESIAN_POINT('Ctrl Pts',(-116.183399296895,-110.0907706828,397.537703348572));
#268769=CARTESIAN_POINT('Ctrl Pts',(-124.847730855269,-100.946938853448,
395.537703348572));
#268770=CARTESIAN_POINT('Ctrl Pts',(-131.974979673883,-90.5602826949695,
393.537703348572));
#268771=CARTESIAN_POINT('Ctrl Pts',(-139.102228492497,-80.1736265364905,
391.537703348572));
#268772=CARTESIAN_POINT('Ctrl Pts',(-144.516898051454,-68.7998999948417,
389.537703348572));
#268773=CARTESIAN_POINT('Ctrl Pts',(-149.931567610411,-57.426173453193,
387.537703348572));
#268774=CARTESIAN_POINT('Ctrl Pts',(-153.500330774912,-45.3454354230638,
385.537703348572));
#268775=CARTESIAN_POINT('Ctrl Pts',(-157.069093939413,-33.2646973929347,
383.537703348572));
#268776=CARTESIAN_POINT('Ctrl Pts',(-158.704075916301,-20.774415738298,
381.537703348572));
#268777=CARTESIAN_POINT('Ctrl Pts',(-160.339057893189,-8.2841340836614,
379.537703348572));
#268778=CARTESIAN_POINT('Ctrl Pts',(-160.,4.30813900827767,377.537703348572));
#268779=CARTESIAN_POINT('Ctrl Pts',(-130.,4.30813900827773,537.537703348572));
#268780=CARTESIAN_POINT('Ctrl Pts',(-129.660942106811,14.5393608954781,
535.537703348572));
#268781=CARTESIAN_POINT('Ctrl Pts',(-127.725542856289,24.591579123369,533.537703348572));
#268782=CARTESIAN_POINT('Ctrl Pts',(-125.790143605767,34.6437973512599,
531.537703348572));
#268783=CARTESIAN_POINT('Ctrl Pts',(-122.306058950683,44.269492945671,529.537703348572));
#268784=CARTESIAN_POINT('Ctrl Pts',(-118.821974295598,53.8951885400822,
527.537703348572));
#268785=CARTESIAN_POINT('Ctrl Pts',(-113.874993963172,62.8573449296269,
525.537703348572));
#268786=CARTESIAN_POINT('Ctrl Pts',(-108.928013630747,71.8195013191717,
523.537703348572));
#268787=CARTESIAN_POINT('Ctrl Pts',(-102.639948694852,79.8974404698478,
521.537703348572));
#268788=CARTESIAN_POINT('Ctrl Pts',(-96.3518837589562,87.9753796205239,
519.537703348572));
#268789=CARTESIAN_POINT('Ctrl Pts',(-88.8775672472037,94.9701958612987,
517.537703348572));
#268790=CARTESIAN_POINT('Ctrl Pts',(-81.4032507354512,101.965012102073,
515.537703348572));
#268791=CARTESIAN_POINT('Ctrl Pts',(-72.9267251261952,107.704469842635,
513.537703348572));
#268792=CARTESIAN_POINT('Ctrl Pts',(-64.4501995169392,113.443927583196,
511.537703348572));
#268793=CARTESIAN_POINT('Ctrl Pts',(-55.1801850026552,117.786702325803,
509.537703348572));
#268794=CARTESIAN_POINT('Ctrl Pts',(-45.9101704883713,122.12947706841,507.537703348572));
#268795=CARTESIAN_POINT('Ctrl Pts',(-36.0749255918153,124.968635286057,
505.537703348572));
#268796=CARTESIAN_POINT('Ctrl Pts',(-26.2396806952593,127.807793503704,
503.537703348572));
#268797=CARTESIAN_POINT('Ctrl Pts',(-16.081381787091,129.073425698447,501.537703348572));
#268798=CARTESIAN_POINT('Ctrl Pts',(-5.92308287892268,130.339057893189,
499.537703348572));
#268799=CARTESIAN_POINT('Ctrl Pts',(4.30813900827772,130.,497.537703348572));
#268800=CARTESIAN_POINT('Ctrl Pts',(14.5393608954781,129.660942106811,495.537703348572));
#268801=CARTESIAN_POINT('Ctrl Pts',(24.591579123369,127.725542856289,493.537703348572));
#268802=CARTESIAN_POINT('Ctrl Pts',(34.6437973512599,125.790143605767,491.537703348572));
#268803=CARTESIAN_POINT('Ctrl Pts',(44.269492945671,122.306058950683,489.537703348572));
#268804=CARTESIAN_POINT('Ctrl Pts',(53.8951885400822,118.821974295598,487.537703348572));
#268805=CARTESIAN_POINT('Ctrl Pts',(62.8573449296269,113.874993963172,485.537703348572));
#268806=CARTESIAN_POINT('Ctrl Pts',(71.8195013191717,108.928013630747,483.537703348572));
#268807=CARTESIAN_POINT('Ctrl Pts',(79.8974404698478,102.639948694852,481.537703348572));
#268808=CARTESIAN_POINT('Ctrl Pts',(87.9753796205239,96.3518837589562,479.537703348572));
#268809=CARTESIAN_POINT('Ctrl Pts',(94.9701958612986,88.8775672472037,477.537703348572));
#268810=CARTESIAN_POINT('Ctrl Pts',(101.965012102073,81.4032507354512,475.537703348572));
#268811=CARTESIAN_POINT('Ctrl Pts',(107.704469842635,72.9267251261952,473.537703348572));
#268812=CARTESIAN_POINT('Ctrl Pts',(113.443927583196,64.4501995169392,471.537703348572));
#268813=CARTESIAN_POINT('Ctrl Pts',(117.786702325803,55.1801850026552,469.537703348572));
#268814=CARTESIAN_POINT('Ctrl Pts',(122.12947706841,45.9101704883713,467.537703348572));
#268815=CARTESIAN_POINT('Ctrl Pts',(124.968635286057,36.0749255918153,465.537703348572));
#268816=CARTESIAN_POINT('Ctrl Pts',(127.807793503704,26.2396806952593,463.537703348572));
#268817=CARTESIAN_POINT('Ctrl Pts',(129.073425698447,16.081381787091,461.537703348572));
#268818=CARTESIAN_POINT('Ctrl Pts',(130.339057893189,5.92308287892268,459.537703348572));
#268819=CARTESIAN_POINT('Ctrl Pts',(130.,-4.30813900827772,457.537703348572));
#268820=CARTESIAN_POINT('Ctrl Pts',(129.660942106811,-14.5393608954781,
455.537703348572));
#268821=CARTESIAN_POINT('Ctrl Pts',(127.725542856289,-24.591579123369,453.537703348572));
#268822=CARTESIAN_POINT('Ctrl Pts',(125.790143605767,-34.6437973512599,
451.537703348572));
#268823=CARTESIAN_POINT('Ctrl Pts',(122.306058950683,-44.269492945671,449.537703348572));
#268824=CARTESIAN_POINT('Ctrl Pts',(118.821974295598,-53.8951885400822,
447.537703348572));
#268825=CARTESIAN_POINT('Ctrl Pts',(113.874993963172,-62.8573449296269,
445.537703348572));
#268826=CARTESIAN_POINT('Ctrl Pts',(108.928013630747,-71.8195013191717,
443.537703348572));
#268827=CARTESIAN_POINT('Ctrl Pts',(102.639948694852,-79.8974404698478,
441.537703348572));
#268828=CARTESIAN_POINT('Ctrl Pts',(96.3518837589563,-87.9753796205239,
439.537703348572));
#268829=CARTESIAN_POINT('Ctrl Pts',(88.8775672472037,-94.9701958612986,
437.537703348572));
#268830=CARTESIAN_POINT('Ctrl Pts',(81.4032507354513,-101.965012102073,
435.537703348572));
#268831=CARTESIAN_POINT('Ctrl Pts',(72.9267251261952,-107.704469842635,
433.537703348572));
#268832=CARTESIAN_POINT('Ctrl Pts',(64.4501995169392,-113.443927583196,
431.537703348572));
#268833=CARTESIAN_POINT('Ctrl Pts',(55.1801850026552,-117.786702325803,
429.537703348572));
#268834=CARTESIAN_POINT('Ctrl Pts',(45.9101704883713,-122.12947706841,427.537703348572));
#268835=CARTESIAN_POINT('Ctrl Pts',(36.0749255918153,-124.968635286057,
425.537703348572));
#268836=CARTESIAN_POINT('Ctrl Pts',(26.2396806952593,-127.807793503704,
423.537703348572));
#268837=CARTESIAN_POINT('Ctrl Pts',(16.081381787091,-129.073425698447,421.537703348572));
#268838=CARTESIAN_POINT('Ctrl Pts',(5.92308287892275,-130.339057893189,
419.537703348572));
#268839=CARTESIAN_POINT('Ctrl Pts',(-4.30813900827771,-130.,417.537703348572));
#268840=CARTESIAN_POINT('Ctrl Pts',(-14.5393608954782,-129.660942106811,
415.537703348572));
#268841=CARTESIAN_POINT('Ctrl Pts',(-24.591579123369,-127.725542856289,
413.537703348572));
#268842=CARTESIAN_POINT('Ctrl Pts',(-34.6437973512598,-125.790143605767,
411.537703348572));
#268843=CARTESIAN_POINT('Ctrl Pts',(-44.269492945671,-122.306058950683,
409.537703348572));
#268844=CARTESIAN_POINT('Ctrl Pts',(-53.8951885400822,-118.821974295598,
407.537703348572));
#268845=CARTESIAN_POINT('Ctrl Pts',(-62.8573449296269,-113.874993963172,
405.537703348572));
#268846=CARTESIAN_POINT('Ctrl Pts',(-71.8195013191717,-108.928013630747,
403.537703348572));
#268847=CARTESIAN_POINT('Ctrl Pts',(-79.8974404698478,-102.639948694852,
401.537703348572));
#268848=CARTESIAN_POINT('Ctrl Pts',(-87.975379620524,-96.3518837589562,
399.537703348572));
#268849=CARTESIAN_POINT('Ctrl Pts',(-94.9701958612986,-88.8775672472037,
397.537703348572));
#268850=CARTESIAN_POINT('Ctrl Pts',(-101.965012102073,-81.4032507354513,
395.537703348572));
#268851=CARTESIAN_POINT('Ctrl Pts',(-107.704469842635,-72.9267251261952,
393.537703348572));
#268852=CARTESIAN_POINT('Ctrl Pts',(-113.443927583196,-64.4501995169392,
391.537703348572));
#268853=CARTESIAN_POINT('Ctrl Pts',(-117.786702325803,-55.1801850026553,
389.537703348572));
#268854=CARTESIAN_POINT('Ctrl Pts',(-122.12947706841,-45.9101704883713,
387.537703348572));
#268855=CARTESIAN_POINT('Ctrl Pts',(-124.968635286057,-36.0749255918153,
385.537703348572));
#268856=CARTESIAN_POINT('Ctrl Pts',(-127.807793503704,-26.2396806952593,
383.537703348572));
#268857=CARTESIAN_POINT('Ctrl Pts',(-129.073425698447,-16.081381787091,
381.537703348572));
#268858=CARTESIAN_POINT('Ctrl Pts',(-130.339057893189,-5.92308287892275,
379.537703348572));
#268859=CARTESIAN_POINT('Ctrl Pts',(-130.,4.30813900827773,377.537703348572));
#268860=CARTESIAN_POINT('Ctrl Pts',(-130.,-4.30813900827845,532.462296651428));
#268861=CARTESIAN_POINT('Ctrl Pts',(-130.339057893189,5.92308287892195,
530.462296651429));
#268862=CARTESIAN_POINT('Ctrl Pts',(-129.073425698447,16.0813817870903,
528.462296651428));
#268863=CARTESIAN_POINT('Ctrl Pts',(-127.807793503705,26.2396806952586,
526.462296651429));
#268864=CARTESIAN_POINT('Ctrl Pts',(-124.968635286058,36.0749255918146,
524.462296651428));
#268865=CARTESIAN_POINT('Ctrl Pts',(-122.129477068411,45.9101704883706,
522.462296651428));
#268866=CARTESIAN_POINT('Ctrl Pts',(-117.786702325804,55.1801850026546,
520.462296651428));
#268867=CARTESIAN_POINT('Ctrl Pts',(-113.443927583196,64.4501995169386,
518.462296651428));
#268868=CARTESIAN_POINT('Ctrl Pts',(-107.704469842635,72.9267251261946,
516.462296651428));
#268869=CARTESIAN_POINT('Ctrl Pts',(-101.965012102074,81.4032507354507,
514.462296651428));
#268870=CARTESIAN_POINT('Ctrl Pts',(-94.9701958612992,88.8775672472032,
512.462296651428));
#268871=CARTESIAN_POINT('Ctrl Pts',(-87.9753796205245,96.3518837589558,
510.462296651429));
#268872=CARTESIAN_POINT('Ctrl Pts',(-79.8974404698484,102.639948694851,
508.462296651428));
#268873=CARTESIAN_POINT('Ctrl Pts',(-71.8195013191724,108.928013630747,
506.462296651428));
#268874=CARTESIAN_POINT('Ctrl Pts',(-62.8573449296276,113.874993963172,
504.462296651428));
#268875=CARTESIAN_POINT('Ctrl Pts',(-53.8951885400828,118.821974295598,
502.462296651428));
#268876=CARTESIAN_POINT('Ctrl Pts',(-44.2694929456717,122.306058950682,
500.462296651428));
#268877=CARTESIAN_POINT('Ctrl Pts',(-34.6437973512606,125.790143605767,
498.462296651429));
#268878=CARTESIAN_POINT('Ctrl Pts',(-24.5915791233697,127.725542856289,
496.462296651428));
#268879=CARTESIAN_POINT('Ctrl Pts',(-14.5393608954789,129.660942106811,
494.462296651428));
#268880=CARTESIAN_POINT('Ctrl Pts',(-4.30813900827846,130.,492.462296651428));
#268881=CARTESIAN_POINT('Ctrl Pts',(5.92308287892194,130.339057893189,490.462296651429));
#268882=CARTESIAN_POINT('Ctrl Pts',(16.0813817870903,129.073425698447,488.462296651428));
#268883=CARTESIAN_POINT('Ctrl Pts',(26.2396806952586,127.807793503705,486.462296651428));
#268884=CARTESIAN_POINT('Ctrl Pts',(36.0749255918146,124.968635286058,484.462296651428));
#268885=CARTESIAN_POINT('Ctrl Pts',(45.9101704883706,122.129477068411,482.462296651428));
#268886=CARTESIAN_POINT('Ctrl Pts',(55.1801850026546,117.786702325804,480.462296651428));
#268887=CARTESIAN_POINT('Ctrl Pts',(64.4501995169386,113.443927583196,478.462296651429));
#268888=CARTESIAN_POINT('Ctrl Pts',(72.9267251261946,107.704469842635,476.462296651428));
#268889=CARTESIAN_POINT('Ctrl Pts',(81.4032507354506,101.965012102074,474.462296651428));
#268890=CARTESIAN_POINT('Ctrl Pts',(88.8775672472032,94.9701958612992,472.462296651428));
#268891=CARTESIAN_POINT('Ctrl Pts',(96.3518837589558,87.9753796205245,470.462296651428));
#268892=CARTESIAN_POINT('Ctrl Pts',(102.639948694851,79.8974404698484,468.462296651428));
#268893=CARTESIAN_POINT('Ctrl Pts',(108.928013630747,71.8195013191724,466.462296651428));
#268894=CARTESIAN_POINT('Ctrl Pts',(113.874993963172,62.8573449296276,464.462296651428));
#268895=CARTESIAN_POINT('Ctrl Pts',(118.821974295598,53.8951885400829,462.462296651428));
#268896=CARTESIAN_POINT('Ctrl Pts',(122.306058950682,44.2694929456717,460.462296651428));
#268897=CARTESIAN_POINT('Ctrl Pts',(125.790143605767,34.6437973512606,458.462296651429));
#268898=CARTESIAN_POINT('Ctrl Pts',(127.725542856289,24.5915791233698,456.462296651428));
#268899=CARTESIAN_POINT('Ctrl Pts',(129.660942106811,14.5393608954789,454.462296651429));
#268900=CARTESIAN_POINT('Ctrl Pts',(130.,4.30813900827846,452.462296651428));
#268901=CARTESIAN_POINT('Ctrl Pts',(130.339057893189,-5.92308287892194,
450.462296651428));
#268902=CARTESIAN_POINT('Ctrl Pts',(129.073425698447,-16.0813817870903,
448.462296651429));
#268903=CARTESIAN_POINT('Ctrl Pts',(127.807793503705,-26.2396806952586,
446.462296651429));
#268904=CARTESIAN_POINT('Ctrl Pts',(124.968635286058,-36.0749255918146,
444.462296651429));
#268905=CARTESIAN_POINT('Ctrl Pts',(122.129477068411,-45.9101704883706,
442.462296651429));
#268906=CARTESIAN_POINT('Ctrl Pts',(117.786702325804,-55.1801850026546,
440.462296651428));
#268907=CARTESIAN_POINT('Ctrl Pts',(113.443927583196,-64.4501995169386,
438.462296651429));
#268908=CARTESIAN_POINT('Ctrl Pts',(107.704469842635,-72.9267251261946,
436.462296651428));
#268909=CARTESIAN_POINT('Ctrl Pts',(101.965012102074,-81.4032507354506,
434.462296651429));
#268910=CARTESIAN_POINT('Ctrl Pts',(94.9701958612992,-88.8775672472032,
432.462296651428));
#268911=CARTESIAN_POINT('Ctrl Pts',(87.9753796205246,-96.3518837589557,
430.462296651429));
#268912=CARTESIAN_POINT('Ctrl Pts',(79.8974404698484,-102.639948694851,
428.462296651429));
#268913=CARTESIAN_POINT('Ctrl Pts',(71.8195013191723,-108.928013630747,
426.462296651428));
#268914=CARTESIAN_POINT('Ctrl Pts',(62.8573449296276,-113.874993963172,
424.462296651428));
#268915=CARTESIAN_POINT('Ctrl Pts',(53.8951885400829,-118.821974295598,
422.462296651428));
#268916=CARTESIAN_POINT('Ctrl Pts',(44.2694929456717,-122.306058950682,
420.462296651428));
#268917=CARTESIAN_POINT('Ctrl Pts',(34.6437973512606,-125.790143605767,
418.462296651429));
#268918=CARTESIAN_POINT('Ctrl Pts',(24.5915791233698,-127.725542856289,
416.462296651428));
#268919=CARTESIAN_POINT('Ctrl Pts',(14.5393608954789,-129.660942106811,
414.462296651429));
#268920=CARTESIAN_POINT('Ctrl Pts',(4.30813900827847,-130.,412.462296651428));
#268921=CARTESIAN_POINT('Ctrl Pts',(-5.92308287892199,-130.339057893189,
410.462296651428));
#268922=CARTESIAN_POINT('Ctrl Pts',(-16.0813817870903,-129.073425698447,
408.462296651428));
#268923=CARTESIAN_POINT('Ctrl Pts',(-26.2396806952585,-127.807793503705,
406.462296651429));
#268924=CARTESIAN_POINT('Ctrl Pts',(-36.0749255918146,-124.968635286058,
404.462296651428));
#268925=CARTESIAN_POINT('Ctrl Pts',(-45.9101704883706,-122.129477068411,
402.462296651429));
#268926=CARTESIAN_POINT('Ctrl Pts',(-55.1801850026546,-117.786702325804,
400.462296651428));
#268927=CARTESIAN_POINT('Ctrl Pts',(-64.4501995169385,-113.443927583197,
398.462296651429));
#268928=CARTESIAN_POINT('Ctrl Pts',(-72.9267251261946,-107.704469842635,
396.462296651428));
#268929=CARTESIAN_POINT('Ctrl Pts',(-81.4032507354507,-101.965012102074,
394.462296651429));
#268930=CARTESIAN_POINT('Ctrl Pts',(-88.8775672472032,-94.9701958612992,
392.462296651428));
#268931=CARTESIAN_POINT('Ctrl Pts',(-96.3518837589557,-87.9753796205246,
390.462296651428));
#268932=CARTESIAN_POINT('Ctrl Pts',(-102.639948694851,-79.8974404698484,
388.462296651428));
#268933=CARTESIAN_POINT('Ctrl Pts',(-108.928013630747,-71.8195013191723,
386.462296651428));
#268934=CARTESIAN_POINT('Ctrl Pts',(-113.874993963172,-62.8573449296276,
384.462296651428));
#268935=CARTESIAN_POINT('Ctrl Pts',(-118.821974295598,-53.8951885400829,
382.462296651429));
#268936=CARTESIAN_POINT('Ctrl Pts',(-122.306058950682,-44.2694929456718,
380.462296651428));
#268937=CARTESIAN_POINT('Ctrl Pts',(-125.790143605767,-34.6437973512606,
378.462296651429));
#268938=CARTESIAN_POINT('Ctrl Pts',(-127.725542856289,-24.5915791233698,
376.462296651428));
#268939=CARTESIAN_POINT('Ctrl Pts',(-129.660942106811,-14.5393608954789,
374.462296651428));
#268940=CARTESIAN_POINT('Ctrl Pts',(-130.,-4.30813900827845,372.462296651428));
#268941=CARTESIAN_POINT('Ctrl Pts',(-129.869812400585,7.23822414350004,
536.964207537012));
#268942=CARTESIAN_POINT('Ctrl Pts',(-129.382196958681,15.9871278397991,
535.249654101829));
#268943=CARTESIAN_POINT('Ctrl Pts',(-127.725542856289,24.591579123369,533.537703348572));
#268944=CARTESIAN_POINT('Ctrl Pts',(-125.790143605767,34.6437973512599,
531.537703348572));
#268945=CARTESIAN_POINT('Ctrl Pts',(-122.306058950683,44.269492945671,529.537703348572));
#268946=CARTESIAN_POINT('Ctrl Pts',(-118.821974295598,53.8951885400822,
527.537703348572));
#268947=CARTESIAN_POINT('Ctrl Pts',(-113.874993963172,62.8573449296269,
525.537703348572));
#268948=CARTESIAN_POINT('Ctrl Pts',(-108.928013630747,71.8195013191717,
523.537703348572));
#268949=CARTESIAN_POINT('Ctrl Pts',(-102.639948694852,79.8974404698478,
521.537703348572));
#268950=CARTESIAN_POINT('Ctrl Pts',(-96.3518837589562,87.9753796205239,
519.537703348572));
#268951=CARTESIAN_POINT('Ctrl Pts',(-88.8775672472037,94.9701958612987,
517.537703348572));
#268952=CARTESIAN_POINT('Ctrl Pts',(-81.4032507354512,101.965012102073,
515.537703348572));
#268953=CARTESIAN_POINT('Ctrl Pts',(-72.9267251261952,107.704469842635,
513.537703348572));
#268954=CARTESIAN_POINT('Ctrl Pts',(-64.4501995169392,113.443927583196,
511.537703348572));
#268955=CARTESIAN_POINT('Ctrl Pts',(-55.1801850026552,117.786702325803,
509.537703348572));
#268956=CARTESIAN_POINT('Ctrl Pts',(-45.9101704883713,122.12947706841,507.537703348572));
#268957=CARTESIAN_POINT('Ctrl Pts',(-36.0749255918153,124.968635286057,
505.537703348572));
#268958=CARTESIAN_POINT('Ctrl Pts',(-26.2396806952593,127.807793503704,
503.537703348572));
#268959=CARTESIAN_POINT('Ctrl Pts',(-16.081381787091,129.073425698447,501.537703348572));
#268960=CARTESIAN_POINT('Ctrl Pts',(-5.92308287892268,130.339057893189,
499.537703348572));
#268961=CARTESIAN_POINT('Ctrl Pts',(4.30813900827772,130.,497.537703348572));
#268962=CARTESIAN_POINT('Ctrl Pts',(14.5393608954781,129.660942106811,495.537703348572));
#268963=CARTESIAN_POINT('Ctrl Pts',(24.591579123369,127.725542856289,493.537703348572));
#268964=CARTESIAN_POINT('Ctrl Pts',(34.6437973512599,125.790143605767,491.537703348572));
#268965=CARTESIAN_POINT('Ctrl Pts',(44.269492945671,122.306058950683,489.537703348572));
#268966=CARTESIAN_POINT('Ctrl Pts',(53.8951885400822,118.821974295598,487.537703348572));
#268967=CARTESIAN_POINT('Ctrl Pts',(62.8573449296269,113.874993963172,485.537703348572));
#268968=CARTESIAN_POINT('Ctrl Pts',(71.8195013191717,108.928013630747,483.537703348572));
#268969=CARTESIAN_POINT('Ctrl Pts',(79.8974404698478,102.639948694852,481.537703348572));
#268970=CARTESIAN_POINT('Ctrl Pts',(87.9753796205239,96.3518837589562,479.537703348572));
#268971=CARTESIAN_POINT('Ctrl Pts',(94.9701958612986,88.8775672472037,477.537703348572));
#268972=CARTESIAN_POINT('Ctrl Pts',(101.965012102073,81.4032507354512,475.537703348572));
#268973=CARTESIAN_POINT('Ctrl Pts',(107.704469842635,72.9267251261952,473.537703348572));
#268974=CARTESIAN_POINT('Ctrl Pts',(113.443927583196,64.4501995169392,471.537703348572));
#268975=CARTESIAN_POINT('Ctrl Pts',(117.786702325803,55.1801850026552,469.537703348572));
#268976=CARTESIAN_POINT('Ctrl Pts',(122.12947706841,45.9101704883713,467.537703348572));
#268977=CARTESIAN_POINT('Ctrl Pts',(124.968635286057,36.0749255918153,465.537703348572));
#268978=CARTESIAN_POINT('Ctrl Pts',(127.807793503704,26.2396806952593,463.537703348572));
#268979=CARTESIAN_POINT('Ctrl Pts',(129.073425698447,16.081381787091,461.537703348572));
#268980=CARTESIAN_POINT('Ctrl Pts',(130.339057893189,5.92308287892268,459.537703348572));
#268981=CARTESIAN_POINT('Ctrl Pts',(130.,-4.30813900827772,457.537703348572));
#268982=CARTESIAN_POINT('Ctrl Pts',(129.660942106811,-14.5393608954781,
455.537703348572));
#268983=CARTESIAN_POINT('Ctrl Pts',(127.725542856289,-24.591579123369,453.537703348572));
#268984=CARTESIAN_POINT('Ctrl Pts',(125.790143605767,-34.6437973512599,
451.537703348572));
#268985=CARTESIAN_POINT('Ctrl Pts',(122.306058950683,-44.269492945671,449.537703348572));
#268986=CARTESIAN_POINT('Ctrl Pts',(118.821974295598,-53.8951885400822,
447.537703348572));
#268987=CARTESIAN_POINT('Ctrl Pts',(113.874993963172,-62.8573449296269,
445.537703348572));
#268988=CARTESIAN_POINT('Ctrl Pts',(108.928013630747,-71.8195013191717,
443.537703348572));
#268989=CARTESIAN_POINT('Ctrl Pts',(102.639948694852,-79.8974404698478,
441.537703348572));
#268990=CARTESIAN_POINT('Ctrl Pts',(96.3518837589563,-87.9753796205239,
439.537703348572));
#268991=CARTESIAN_POINT('Ctrl Pts',(88.8775672472037,-94.9701958612986,
437.537703348572));
#268992=CARTESIAN_POINT('Ctrl Pts',(81.4032507354513,-101.965012102073,
435.537703348572));
#268993=CARTESIAN_POINT('Ctrl Pts',(72.9267251261952,-107.704469842635,
433.537703348572));
#268994=CARTESIAN_POINT('Ctrl Pts',(64.4501995169392,-113.443927583196,
431.537703348572));
#268995=CARTESIAN_POINT('Ctrl Pts',(55.1801850026552,-117.786702325803,
429.537703348572));
#268996=CARTESIAN_POINT('Ctrl Pts',(45.9101704883713,-122.12947706841,427.537703348572));
#268997=CARTESIAN_POINT('Ctrl Pts',(36.0749255918153,-124.968635286057,
425.537703348572));
#268998=CARTESIAN_POINT('Ctrl Pts',(26.2396806952593,-127.807793503704,
423.537703348572));
#268999=CARTESIAN_POINT('Ctrl Pts',(16.081381787091,-129.073425698447,421.537703348572));
#269000=CARTESIAN_POINT('Ctrl Pts',(5.92308287892275,-130.339057893189,
419.537703348572));
#269001=CARTESIAN_POINT('Ctrl Pts',(-4.30813900827771,-130.,417.537703348572));
#269002=CARTESIAN_POINT('Ctrl Pts',(-14.5393608954782,-129.660942106811,
415.537703348572));
#269003=CARTESIAN_POINT('Ctrl Pts',(-24.591579123369,-127.725542856289,
413.537703348572));
#269004=CARTESIAN_POINT('Ctrl Pts',(-34.6437973512598,-125.790143605767,
411.537703348572));
#269005=CARTESIAN_POINT('Ctrl Pts',(-44.269492945671,-122.306058950683,
409.537703348572));
#269006=CARTESIAN_POINT('Ctrl Pts',(-53.8951885400822,-118.821974295598,
407.537703348572));
#269007=CARTESIAN_POINT('Ctrl Pts',(-62.8573449296269,-113.874993963172,
405.537703348572));
#269008=CARTESIAN_POINT('Ctrl Pts',(-71.8195013191717,-108.928013630747,
403.537703348572));
#269009=CARTESIAN_POINT('Ctrl Pts',(-79.8974404698478,-102.639948694852,
401.537703348572));
#269010=CARTESIAN_POINT('Ctrl Pts',(-87.975379620524,-96.3518837589562,
399.537703348572));
#269011=CARTESIAN_POINT('Ctrl Pts',(-94.9701958612986,-88.8775672472037,
397.537703348572));
#269012=CARTESIAN_POINT('Ctrl Pts',(-101.965012102073,-81.4032507354513,
395.537703348572));
#269013=CARTESIAN_POINT('Ctrl Pts',(-107.704469842635,-72.9267251261952,
393.537703348572));
#269014=CARTESIAN_POINT('Ctrl Pts',(-113.443927583196,-64.4501995169392,
391.537703348572));
#269015=CARTESIAN_POINT('Ctrl Pts',(-117.786702325803,-55.1801850026553,
389.537703348572));
#269016=CARTESIAN_POINT('Ctrl Pts',(-122.12947706841,-45.9101704883713,
387.537703348572));
#269017=CARTESIAN_POINT('Ctrl Pts',(-124.968635286057,-36.0749255918153,
385.537703348572));
#269018=CARTESIAN_POINT('Ctrl Pts',(-127.807793503704,-26.2396806952593,
383.537703348572));
#269019=CARTESIAN_POINT('Ctrl Pts',(-129.073425698447,-16.081381787091,
381.537703348572));
#269020=CARTESIAN_POINT('Ctrl Pts',(-129.701667605591,-11.038945994199,
380.54493165747));
#269021=CARTESIAN_POINT('Ctrl Pts',(-129.934615416877,-5.962866607847,379.549090218607));
#269022=CARTESIAN_POINT('Ctrl Pts',(-129.934615416877,5.96286660784693,
530.450909781394));
#269023=CARTESIAN_POINT('Ctrl Pts',(-129.701667605591,11.0389459941986,
529.455068342531));
#269024=CARTESIAN_POINT('Ctrl Pts',(-129.073425698447,16.0813817870903,
528.462296651428));
#269025=CARTESIAN_POINT('Ctrl Pts',(-127.807793503705,26.2396806952586,
526.462296651429));
#269026=CARTESIAN_POINT('Ctrl Pts',(-124.968635286058,36.0749255918146,
524.462296651428));
#269027=CARTESIAN_POINT('Ctrl Pts',(-122.129477068411,45.9101704883706,
522.462296651428));
#269028=CARTESIAN_POINT('Ctrl Pts',(-117.786702325804,55.1801850026546,
520.462296651428));
#269029=CARTESIAN_POINT('Ctrl Pts',(-113.443927583196,64.4501995169386,
518.462296651428));
#269030=CARTESIAN_POINT('Ctrl Pts',(-107.704469842635,72.9267251261946,
516.462296651428));
#269031=CARTESIAN_POINT('Ctrl Pts',(-101.965012102074,81.4032507354507,
514.462296651428));
#269032=CARTESIAN_POINT('Ctrl Pts',(-94.9701958612992,88.8775672472032,
512.462296651428));
#269033=CARTESIAN_POINT('Ctrl Pts',(-87.9753796205245,96.3518837589558,
510.462296651429));
#269034=CARTESIAN_POINT('Ctrl Pts',(-79.8974404698484,102.639948694851,
508.462296651428));
#269035=CARTESIAN_POINT('Ctrl Pts',(-71.8195013191724,108.928013630747,
506.462296651428));
#269036=CARTESIAN_POINT('Ctrl Pts',(-62.8573449296276,113.874993963172,
504.462296651428));
#269037=CARTESIAN_POINT('Ctrl Pts',(-53.8951885400828,118.821974295598,
502.462296651429));
#269038=CARTESIAN_POINT('Ctrl Pts',(-44.2694929456717,122.306058950682,
500.462296651428));
#269039=CARTESIAN_POINT('Ctrl Pts',(-34.6437973512606,125.790143605767,
498.462296651429));
#269040=CARTESIAN_POINT('Ctrl Pts',(-24.5915791233697,127.725542856289,
496.462296651428));
#269041=CARTESIAN_POINT('Ctrl Pts',(-14.5393608954789,129.660942106811,
494.462296651429));
#269042=CARTESIAN_POINT('Ctrl Pts',(-4.30813900827846,130.,492.462296651428));
#269043=CARTESIAN_POINT('Ctrl Pts',(5.92308287892194,130.339057893189,490.462296651428));
#269044=CARTESIAN_POINT('Ctrl Pts',(16.0813817870903,129.073425698447,488.462296651428));
#269045=CARTESIAN_POINT('Ctrl Pts',(26.2396806952586,127.807793503705,486.462296651428));
#269046=CARTESIAN_POINT('Ctrl Pts',(36.0749255918146,124.968635286058,484.462296651428));
#269047=CARTESIAN_POINT('Ctrl Pts',(45.9101704883706,122.129477068411,482.462296651428));
#269048=CARTESIAN_POINT('Ctrl Pts',(55.1801850026546,117.786702325804,480.462296651428));
#269049=CARTESIAN_POINT('Ctrl Pts',(64.4501995169386,113.443927583196,478.462296651429));
#269050=CARTESIAN_POINT('Ctrl Pts',(72.9267251261946,107.704469842635,476.462296651428));
#269051=CARTESIAN_POINT('Ctrl Pts',(81.4032507354506,101.965012102074,474.462296651428));
#269052=CARTESIAN_POINT('Ctrl Pts',(88.8775672472032,94.9701958612992,472.462296651428));
#269053=CARTESIAN_POINT('Ctrl Pts',(96.3518837589558,87.9753796205245,470.462296651428));
#269054=CARTESIAN_POINT('Ctrl Pts',(102.639948694851,79.8974404698484,468.462296651428));
#269055=CARTESIAN_POINT('Ctrl Pts',(108.928013630747,71.8195013191724,466.462296651428));
#269056=CARTESIAN_POINT('Ctrl Pts',(113.874993963172,62.8573449296276,464.462296651428));
#269057=CARTESIAN_POINT('Ctrl Pts',(118.821974295598,53.8951885400829,462.462296651428));
#269058=CARTESIAN_POINT('Ctrl Pts',(122.306058950682,44.2694929456717,460.462296651428));
#269059=CARTESIAN_POINT('Ctrl Pts',(125.790143605767,34.6437973512606,458.462296651429));
#269060=CARTESIAN_POINT('Ctrl Pts',(127.725542856289,24.5915791233698,456.462296651428));
#269061=CARTESIAN_POINT('Ctrl Pts',(129.660942106811,14.5393608954789,454.462296651429));
#269062=CARTESIAN_POINT('Ctrl Pts',(130.,4.30813900827846,452.462296651428));
#269063=CARTESIAN_POINT('Ctrl Pts',(130.339057893189,-5.92308287892194,
450.462296651429));
#269064=CARTESIAN_POINT('Ctrl Pts',(129.073425698447,-16.0813817870903,
448.462296651429));
#269065=CARTESIAN_POINT('Ctrl Pts',(127.807793503705,-26.2396806952586,
446.462296651429));
#269066=CARTESIAN_POINT('Ctrl Pts',(124.968635286058,-36.0749255918146,
444.462296651429));
#269067=CARTESIAN_POINT('Ctrl Pts',(122.129477068411,-45.9101704883706,
442.462296651429));
#269068=CARTESIAN_POINT('Ctrl Pts',(117.786702325804,-55.1801850026546,
440.462296651428));
#269069=CARTESIAN_POINT('Ctrl Pts',(113.443927583196,-64.4501995169386,
438.462296651429));
#269070=CARTESIAN_POINT('Ctrl Pts',(107.704469842635,-72.9267251261946,
436.462296651428));
#269071=CARTESIAN_POINT('Ctrl Pts',(101.965012102074,-81.4032507354506,
434.462296651429));
#269072=CARTESIAN_POINT('Ctrl Pts',(94.9701958612992,-88.8775672472032,
432.462296651428));
#269073=CARTESIAN_POINT('Ctrl Pts',(87.9753796205245,-96.3518837589557,
430.462296651429));
#269074=CARTESIAN_POINT('Ctrl Pts',(79.8974404698484,-102.639948694851,
428.462296651429));
#269075=CARTESIAN_POINT('Ctrl Pts',(71.8195013191723,-108.928013630747,
426.462296651428));
#269076=CARTESIAN_POINT('Ctrl Pts',(62.8573449296276,-113.874993963172,
424.462296651428));
#269077=CARTESIAN_POINT('Ctrl Pts',(53.8951885400829,-118.821974295598,
422.462296651428));
#269078=CARTESIAN_POINT('Ctrl Pts',(44.2694929456717,-122.306058950682,
420.462296651428));
#269079=CARTESIAN_POINT('Ctrl Pts',(34.6437973512606,-125.790143605767,
418.462296651429));
#269080=CARTESIAN_POINT('Ctrl Pts',(24.5915791233698,-127.725542856289,
416.462296651428));
#269081=CARTESIAN_POINT('Ctrl Pts',(14.5393608954789,-129.660942106811,
414.462296651429));
#269082=CARTESIAN_POINT('Ctrl Pts',(4.30813900827847,-130.,412.462296651428));
#269083=CARTESIAN_POINT('Ctrl Pts',(-5.92308287892199,-130.339057893189,
410.462296651428));
#269084=CARTESIAN_POINT('Ctrl Pts',(-16.0813817870903,-129.073425698447,
408.462296651428));
#269085=CARTESIAN_POINT('Ctrl Pts',(-26.2396806952585,-127.807793503705,
406.462296651429));
#269086=CARTESIAN_POINT('Ctrl Pts',(-36.0749255918146,-124.968635286058,
404.462296651428));
#269087=CARTESIAN_POINT('Ctrl Pts',(-45.9101704883706,-122.129477068411,
402.462296651428));
#269088=CARTESIAN_POINT('Ctrl Pts',(-55.1801850026546,-117.786702325804,
400.462296651428));
#269089=CARTESIAN_POINT('Ctrl Pts',(-64.4501995169385,-113.443927583197,
398.462296651429));
#269090=CARTESIAN_POINT('Ctrl Pts',(-72.9267251261946,-107.704469842635,
396.462296651428));
#269091=CARTESIAN_POINT('Ctrl Pts',(-81.4032507354507,-101.965012102074,
394.462296651429));
#269092=CARTESIAN_POINT('Ctrl Pts',(-88.8775672472032,-94.9701958612992,
392.462296651428));
#269093=CARTESIAN_POINT('Ctrl Pts',(-96.3518837589557,-87.9753796205245,
390.462296651428));
#269094=CARTESIAN_POINT('Ctrl Pts',(-102.639948694851,-79.8974404698484,
388.462296651428));
#269095=CARTESIAN_POINT('Ctrl Pts',(-108.928013630747,-71.8195013191723,
386.462296651429));
#269096=CARTESIAN_POINT('Ctrl Pts',(-113.874993963172,-62.8573449296276,
384.462296651428));
#269097=CARTESIAN_POINT('Ctrl Pts',(-118.821974295598,-53.8951885400829,
382.462296651429));
#269098=CARTESIAN_POINT('Ctrl Pts',(-122.306058950682,-44.2694929456718,
380.462296651428));
#269099=CARTESIAN_POINT('Ctrl Pts',(-125.790143605767,-34.6437973512606,
378.462296651429));
#269100=CARTESIAN_POINT('Ctrl Pts',(-127.725542856289,-24.5915791233698,
376.462296651428));
#269101=CARTESIAN_POINT('Ctrl Pts',(-129.382196958681,-15.9871278397995,
374.750345898172));
#269102=CARTESIAN_POINT('Ctrl Pts',(-129.869812400585,-7.23822414349998,
373.035792462989));
#269103=CARTESIAN_POINT('Ctrl Pts',(-160.,4.30813900827767,537.537703348572));
#269104=CARTESIAN_POINT('Ctrl Pts',(-159.660942106811,16.9004121002166,
535.537703348572));
#269105=CARTESIAN_POINT('Ctrl Pts',(-157.356193074143,29.2846130745759,
533.537703348572));
#269106=CARTESIAN_POINT('Ctrl Pts',(-155.051444041476,41.6688140489352,
531.537703348572));
#269107=CARTESIAN_POINT('Ctrl Pts',(-150.837754439537,53.5400027769194,
529.537703348572));
#269108=CARTESIAN_POINT('Ctrl Pts',(-146.624064837599,65.4111915049037,
527.537703348572));
#269109=CARTESIAN_POINT('Ctrl Pts',(-140.605189688823,76.4770599218133,
525.537703348572));
#269110=CARTESIAN_POINT('Ctrl Pts',(-134.586314540048,87.542928338723,523.537703348572));
#269111=CARTESIAN_POINT('Ctrl Pts',(-126.9104585261,97.530998038622,521.537703348572));
#269112=CARTESIAN_POINT('Ctrl Pts',(-119.234602512152,107.519067738521,
519.537703348572));
#269113=CARTESIAN_POINT('Ctrl Pts',(-110.0907706828,116.183399296895,517.537703348572));
#269114=CARTESIAN_POINT('Ctrl Pts',(-100.946938853448,124.847730855269,
515.537703348572));
#269115=CARTESIAN_POINT('Ctrl Pts',(-90.5602826949695,131.974979673883,
513.537703348572));
#269116=CARTESIAN_POINT('Ctrl Pts',(-80.1736265364906,139.102228492497,
511.537703348572));
#269117=CARTESIAN_POINT('Ctrl Pts',(-68.7998999948417,144.516898051454,
509.537703348572));
#269118=CARTESIAN_POINT('Ctrl Pts',(-57.4261734531929,149.931567610411,
507.537703348572));
#269119=CARTESIAN_POINT('Ctrl Pts',(-45.3454354230638,153.500330774912,
505.537703348572));
#269120=CARTESIAN_POINT('Ctrl Pts',(-33.2646973929347,157.069093939413,
503.537703348572));
#269121=CARTESIAN_POINT('Ctrl Pts',(-20.774415738298,158.704075916301,501.537703348572));
#269122=CARTESIAN_POINT('Ctrl Pts',(-8.28413408366129,160.339057893189,
499.537703348572));
#269123=CARTESIAN_POINT('Ctrl Pts',(4.30813900827766,160.,497.537703348572));
#269124=CARTESIAN_POINT('Ctrl Pts',(16.9004121002166,159.660942106811,495.537703348572));
#269125=CARTESIAN_POINT('Ctrl Pts',(29.2846130745759,157.356193074143,493.537703348572));
#269126=CARTESIAN_POINT('Ctrl Pts',(41.6688140489352,155.051444041476,491.537703348572));
#269127=CARTESIAN_POINT('Ctrl Pts',(53.5400027769194,150.837754439537,489.537703348572));
#269128=CARTESIAN_POINT('Ctrl Pts',(65.4111915049037,146.624064837599,487.537703348572));
#269129=CARTESIAN_POINT('Ctrl Pts',(76.4770599218133,140.605189688823,485.537703348572));
#269130=CARTESIAN_POINT('Ctrl Pts',(87.542928338723,134.586314540048,483.537703348572));
#269131=CARTESIAN_POINT('Ctrl Pts',(97.530998038622,126.9104585261,481.537703348572));
#269132=CARTESIAN_POINT('Ctrl Pts',(107.519067738521,119.234602512152,479.537703348572));
#269133=CARTESIAN_POINT('Ctrl Pts',(116.183399296895,110.0907706828,477.537703348572));
#269134=CARTESIAN_POINT('Ctrl Pts',(124.847730855269,100.946938853448,475.537703348572));
#269135=CARTESIAN_POINT('Ctrl Pts',(131.974979673883,90.5602826949695,473.537703348572));
#269136=CARTESIAN_POINT('Ctrl Pts',(139.102228492497,80.1736265364906,471.537703348572));
#269137=CARTESIAN_POINT('Ctrl Pts',(144.516898051454,68.7998999948417,469.537703348572));
#269138=CARTESIAN_POINT('Ctrl Pts',(149.931567610411,57.4261734531929,467.537703348572));
#269139=CARTESIAN_POINT('Ctrl Pts',(153.500330774912,45.3454354230638,465.537703348572));
#269140=CARTESIAN_POINT('Ctrl Pts',(157.069093939413,33.2646973929347,463.537703348572));
#269141=CARTESIAN_POINT('Ctrl Pts',(158.704075916301,20.774415738298,461.537703348572));
#269142=CARTESIAN_POINT('Ctrl Pts',(160.339057893189,8.28413408366131,459.537703348572));
#269143=CARTESIAN_POINT('Ctrl Pts',(160.,-4.30813900827765,457.537703348572));
#269144=CARTESIAN_POINT('Ctrl Pts',(159.660942106811,-16.9004121002166,
455.537703348572));
#269145=CARTESIAN_POINT('Ctrl Pts',(157.356193074143,-29.2846130745759,
453.537703348572));
#269146=CARTESIAN_POINT('Ctrl Pts',(155.051444041476,-41.6688140489352,
451.537703348572));
#269147=CARTESIAN_POINT('Ctrl Pts',(150.837754439537,-53.5400027769194,
449.537703348572));
#269148=CARTESIAN_POINT('Ctrl Pts',(146.624064837599,-65.4111915049036,
447.537703348572));
#269149=CARTESIAN_POINT('Ctrl Pts',(140.605189688823,-76.4770599218133,
445.537703348572));
#269150=CARTESIAN_POINT('Ctrl Pts',(134.586314540048,-87.5429283387229,
443.537703348572));
#269151=CARTESIAN_POINT('Ctrl Pts',(126.9104585261,-97.530998038622,441.537703348572));
#269152=CARTESIAN_POINT('Ctrl Pts',(119.234602512152,-107.519067738521,
439.537703348572));
#269153=CARTESIAN_POINT('Ctrl Pts',(110.0907706828,-116.183399296895,437.537703348572));
#269154=CARTESIAN_POINT('Ctrl Pts',(100.946938853448,-124.847730855269,
435.537703348572));
#269155=CARTESIAN_POINT('Ctrl Pts',(90.5602826949695,-131.974979673883,
433.537703348572));
#269156=CARTESIAN_POINT('Ctrl Pts',(80.1736265364905,-139.102228492497,
431.537703348572));
#269157=CARTESIAN_POINT('Ctrl Pts',(68.7998999948417,-144.516898051454,
429.537703348572));
#269158=CARTESIAN_POINT('Ctrl Pts',(57.426173453193,-149.931567610411,427.537703348572));
#269159=CARTESIAN_POINT('Ctrl Pts',(45.3454354230638,-153.500330774912,
425.537703348572));
#269160=CARTESIAN_POINT('Ctrl Pts',(33.2646973929347,-157.069093939413,
423.537703348572));
#269161=CARTESIAN_POINT('Ctrl Pts',(20.774415738298,-158.704075916301,421.537703348572));
#269162=CARTESIAN_POINT('Ctrl Pts',(8.28413408366139,-160.339057893189,
419.537703348572));
#269163=CARTESIAN_POINT('Ctrl Pts',(-4.30813900827764,-160.,417.537703348572));
#269164=CARTESIAN_POINT('Ctrl Pts',(-16.9004121002167,-159.660942106811,
415.537703348572));
#269165=CARTESIAN_POINT('Ctrl Pts',(-29.2846130745759,-157.356193074143,
413.537703348572));
#269166=CARTESIAN_POINT('Ctrl Pts',(-41.6688140489351,-155.051444041476,
411.537703348572));
#269167=CARTESIAN_POINT('Ctrl Pts',(-53.5400027769194,-150.837754439537,
409.537703348572));
#269168=CARTESIAN_POINT('Ctrl Pts',(-65.4111915049037,-146.624064837599,
407.537703348572));
#269169=CARTESIAN_POINT('Ctrl Pts',(-76.4770599218133,-140.605189688823,
405.537703348572));
#269170=CARTESIAN_POINT('Ctrl Pts',(-87.5429283387229,-134.586314540048,
403.537703348572));
#269171=CARTESIAN_POINT('Ctrl Pts',(-97.530998038622,-126.9104585261,401.537703348572));
#269172=CARTESIAN_POINT('Ctrl Pts',(-107.519067738521,-119.234602512152,
399.537703348572));
#269173=CARTESIAN_POINT('Ctrl Pts',(-116.183399296895,-110.0907706828,397.537703348572));
#269174=CARTESIAN_POINT('Ctrl Pts',(-124.847730855269,-100.946938853448,
395.537703348572));
#269175=CARTESIAN_POINT('Ctrl Pts',(-131.974979673883,-90.5602826949695,
393.537703348572));
#269176=CARTESIAN_POINT('Ctrl Pts',(-139.102228492497,-80.1736265364905,
391.537703348572));
#269177=CARTESIAN_POINT('Ctrl Pts',(-144.516898051454,-68.7998999948417,
389.537703348572));
#269178=CARTESIAN_POINT('Ctrl Pts',(-149.931567610411,-57.426173453193,
387.537703348572));
#269179=CARTESIAN_POINT('Ctrl Pts',(-153.500330774912,-45.3454354230638,
385.537703348572));
#269180=CARTESIAN_POINT('Ctrl Pts',(-157.069093939413,-33.2646973929347,
383.537703348572));
#269181=CARTESIAN_POINT('Ctrl Pts',(-158.704075916301,-20.774415738298,
381.537703348572));
#269182=CARTESIAN_POINT('Ctrl Pts',(-160.339057893189,-8.2841340836614,
379.537703348572));
#269183=CARTESIAN_POINT('Ctrl Pts',(-160.,4.30813900827767,377.537703348572));
#269184=CARTESIAN_POINT('Ctrl Pts',(-130.,4.30813900827773,537.537703348572));
#269185=CARTESIAN_POINT('Ctrl Pts',(-129.660942106811,14.5393608954781,
535.537703348572));
#269186=CARTESIAN_POINT('Ctrl Pts',(-127.725542856289,24.591579123369,533.537703348572));
#269187=CARTESIAN_POINT('Ctrl Pts',(-125.790143605767,34.6437973512599,
531.537703348572));
#269188=CARTESIAN_POINT('Ctrl Pts',(-122.306058950683,44.269492945671,529.537703348572));
#269189=CARTESIAN_POINT('Ctrl Pts',(-118.821974295598,53.8951885400822,
527.537703348572));
#269190=CARTESIAN_POINT('Ctrl Pts',(-113.874993963172,62.8573449296269,
525.537703348572));
#269191=CARTESIAN_POINT('Ctrl Pts',(-108.928013630747,71.8195013191717,
523.537703348572));
#269192=CARTESIAN_POINT('Ctrl Pts',(-102.639948694852,79.8974404698478,
521.537703348572));
#269193=CARTESIAN_POINT('Ctrl Pts',(-96.3518837589562,87.9753796205239,
519.537703348572));
#269194=CARTESIAN_POINT('Ctrl Pts',(-88.8775672472037,94.9701958612987,
517.537703348572));
#269195=CARTESIAN_POINT('Ctrl Pts',(-81.4032507354512,101.965012102073,
515.537703348572));
#269196=CARTESIAN_POINT('Ctrl Pts',(-72.9267251261952,107.704469842635,
513.537703348572));
#269197=CARTESIAN_POINT('Ctrl Pts',(-64.4501995169392,113.443927583196,
511.537703348572));
#269198=CARTESIAN_POINT('Ctrl Pts',(-55.1801850026552,117.786702325803,
509.537703348572));
#269199=CARTESIAN_POINT('Ctrl Pts',(-45.9101704883713,122.12947706841,507.537703348572));
#269200=CARTESIAN_POINT('Ctrl Pts',(-36.0749255918153,124.968635286057,
505.537703348572));
#269201=CARTESIAN_POINT('Ctrl Pts',(-26.2396806952593,127.807793503704,
503.537703348572));
#269202=CARTESIAN_POINT('Ctrl Pts',(-16.081381787091,129.073425698447,501.537703348572));
#269203=CARTESIAN_POINT('Ctrl Pts',(-5.92308287892268,130.339057893189,
499.537703348572));
#269204=CARTESIAN_POINT('Ctrl Pts',(4.30813900827772,130.,497.537703348572));
#269205=CARTESIAN_POINT('Ctrl Pts',(14.5393608954781,129.660942106811,495.537703348572));
#269206=CARTESIAN_POINT('Ctrl Pts',(24.591579123369,127.725542856289,493.537703348572));
#269207=CARTESIAN_POINT('Ctrl Pts',(34.6437973512599,125.790143605767,491.537703348572));
#269208=CARTESIAN_POINT('Ctrl Pts',(44.269492945671,122.306058950683,489.537703348572));
#269209=CARTESIAN_POINT('Ctrl Pts',(53.8951885400822,118.821974295598,487.537703348572));
#269210=CARTESIAN_POINT('Ctrl Pts',(62.8573449296269,113.874993963172,485.537703348572));
#269211=CARTESIAN_POINT('Ctrl Pts',(71.8195013191717,108.928013630747,483.537703348572));
#269212=CARTESIAN_POINT('Ctrl Pts',(79.8974404698478,102.639948694852,481.537703348572));
#269213=CARTESIAN_POINT('Ctrl Pts',(87.9753796205239,96.3518837589562,479.537703348572));
#269214=CARTESIAN_POINT('Ctrl Pts',(94.9701958612986,88.8775672472037,477.537703348572));
#269215=CARTESIAN_POINT('Ctrl Pts',(101.965012102073,81.4032507354512,475.537703348572));
#269216=CARTESIAN_POINT('Ctrl Pts',(107.704469842635,72.9267251261952,473.537703348572));
#269217=CARTESIAN_POINT('Ctrl Pts',(113.443927583196,64.4501995169392,471.537703348572));
#269218=CARTESIAN_POINT('Ctrl Pts',(117.786702325803,55.1801850026552,469.537703348572));
#269219=CARTESIAN_POINT('Ctrl Pts',(122.12947706841,45.9101704883713,467.537703348572));
#269220=CARTESIAN_POINT('Ctrl Pts',(124.968635286057,36.0749255918153,465.537703348572));
#269221=CARTESIAN_POINT('Ctrl Pts',(127.807793503704,26.2396806952593,463.537703348572));
#269222=CARTESIAN_POINT('Ctrl Pts',(129.073425698447,16.081381787091,461.537703348572));
#269223=CARTESIAN_POINT('Ctrl Pts',(130.339057893189,5.92308287892268,459.537703348572));
#269224=CARTESIAN_POINT('Ctrl Pts',(130.,-4.30813900827772,457.537703348572));
#269225=CARTESIAN_POINT('Ctrl Pts',(129.660942106811,-14.5393608954781,
455.537703348572));
#269226=CARTESIAN_POINT('Ctrl Pts',(127.725542856289,-24.591579123369,453.537703348572));
#269227=CARTESIAN_POINT('Ctrl Pts',(125.790143605767,-34.6437973512599,
451.537703348572));
#269228=CARTESIAN_POINT('Ctrl Pts',(122.306058950683,-44.269492945671,449.537703348572));
#269229=CARTESIAN_POINT('Ctrl Pts',(118.821974295598,-53.8951885400822,
447.537703348572));
#269230=CARTESIAN_POINT('Ctrl Pts',(113.874993963172,-62.8573449296269,
445.537703348572));
#269231=CARTESIAN_POINT('Ctrl Pts',(108.928013630747,-71.8195013191717,
443.537703348572));
#269232=CARTESIAN_POINT('Ctrl Pts',(102.639948694852,-79.8974404698478,
441.537703348572));
#269233=CARTESIAN_POINT('Ctrl Pts',(96.3518837589563,-87.9753796205239,
439.537703348572));
#269234=CARTESIAN_POINT('Ctrl Pts',(88.8775672472037,-94.9701958612986,
437.537703348572));
#269235=CARTESIAN_POINT('Ctrl Pts',(81.4032507354513,-101.965012102073,
435.537703348572));
#269236=CARTESIAN_POINT('Ctrl Pts',(72.9267251261952,-107.704469842635,
433.537703348572));
#269237=CARTESIAN_POINT('Ctrl Pts',(64.4501995169392,-113.443927583196,
431.537703348572));
#269238=CARTESIAN_POINT('Ctrl Pts',(55.1801850026552,-117.786702325803,
429.537703348572));
#269239=CARTESIAN_POINT('Ctrl Pts',(45.9101704883713,-122.12947706841,427.537703348572));
#269240=CARTESIAN_POINT('Ctrl Pts',(36.0749255918153,-124.968635286057,
425.537703348572));
#269241=CARTESIAN_POINT('Ctrl Pts',(26.2396806952593,-127.807793503704,
423.537703348572));
#269242=CARTESIAN_POINT('Ctrl Pts',(16.081381787091,-129.073425698447,421.537703348572));
#269243=CARTESIAN_POINT('Ctrl Pts',(5.92308287892275,-130.339057893189,
419.537703348572));
#269244=CARTESIAN_POINT('Ctrl Pts',(-4.30813900827771,-130.,417.537703348572));
#269245=CARTESIAN_POINT('Ctrl Pts',(-14.5393608954782,-129.660942106811,
415.537703348572));
#269246=CARTESIAN_POINT('Ctrl Pts',(-24.591579123369,-127.725542856289,
413.537703348572));
#269247=CARTESIAN_POINT('Ctrl Pts',(-34.6437973512598,-125.790143605767,
411.537703348572));
#269248=CARTESIAN_POINT('Ctrl Pts',(-44.269492945671,-122.306058950683,
409.537703348572));
#269249=CARTESIAN_POINT('Ctrl Pts',(-53.8951885400822,-118.821974295598,
407.537703348572));
#269250=CARTESIAN_POINT('Ctrl Pts',(-62.8573449296269,-113.874993963172,
405.537703348572));
#269251=CARTESIAN_POINT('Ctrl Pts',(-71.8195013191717,-108.928013630747,
403.537703348572));
#269252=CARTESIAN_POINT('Ctrl Pts',(-79.8974404698478,-102.639948694852,
401.537703348572));
#269253=CARTESIAN_POINT('Ctrl Pts',(-87.975379620524,-96.3518837589562,
399.537703348572));
#269254=CARTESIAN_POINT('Ctrl Pts',(-94.9701958612986,-88.8775672472037,
397.537703348572));
#269255=CARTESIAN_POINT('Ctrl Pts',(-101.965012102073,-81.4032507354513,
395.537703348572));
#269256=CARTESIAN_POINT('Ctrl Pts',(-107.704469842635,-72.9267251261952,
393.537703348572));
#269257=CARTESIAN_POINT('Ctrl Pts',(-113.443927583196,-64.4501995169392,
391.537703348572));
#269258=CARTESIAN_POINT('Ctrl Pts',(-117.786702325803,-55.1801850026553,
389.537703348572));
#269259=CARTESIAN_POINT('Ctrl Pts',(-122.12947706841,-45.9101704883713,
387.537703348572));
#269260=CARTESIAN_POINT('Ctrl Pts',(-124.968635286057,-36.0749255918153,
385.537703348572));
#269261=CARTESIAN_POINT('Ctrl Pts',(-127.807793503704,-26.2396806952593,
383.537703348572));
#269262=CARTESIAN_POINT('Ctrl Pts',(-129.073425698447,-16.081381787091,
381.537703348572));
#269263=CARTESIAN_POINT('Ctrl Pts',(-130.339057893189,-5.92308287892275,
379.537703348572));
#269264=CARTESIAN_POINT('Ctrl Pts',(-130.,4.30813900827773,377.537703348572));
#269265=CARTESIAN_POINT('Ctrl Pts',(-159.895664541343,7.20669984090294,
537.076891283416));
#269266=CARTESIAN_POINT('Ctrl Pts',(-159.394142202012,18.3340187941078,
535.306181476978));
#269267=CARTESIAN_POINT('Ctrl Pts',(-157.356193074143,29.2846130745759,
533.537703348572));
#269268=CARTESIAN_POINT('Ctrl Pts',(-155.051444041476,41.6688140489352,
531.537703348572));
#269269=CARTESIAN_POINT('Ctrl Pts',(-150.837754439537,53.5400027769194,
529.537703348572));
#269270=CARTESIAN_POINT('Ctrl Pts',(-146.624064837599,65.4111915049037,
527.537703348572));
#269271=CARTESIAN_POINT('Ctrl Pts',(-140.605189688823,76.4770599218133,
525.537703348572));
#269272=CARTESIAN_POINT('Ctrl Pts',(-134.586314540048,87.542928338723,523.537703348572));
#269273=CARTESIAN_POINT('Ctrl Pts',(-126.9104585261,97.530998038622,521.537703348572));
#269274=CARTESIAN_POINT('Ctrl Pts',(-119.234602512152,107.519067738521,
519.537703348572));
#269275=CARTESIAN_POINT('Ctrl Pts',(-110.0907706828,116.183399296895,517.537703348572));
#269276=CARTESIAN_POINT('Ctrl Pts',(-100.946938853448,124.847730855269,
515.537703348572));
#269277=CARTESIAN_POINT('Ctrl Pts',(-90.5602826949695,131.974979673883,
513.537703348572));
#269278=CARTESIAN_POINT('Ctrl Pts',(-80.1736265364906,139.102228492497,
511.537703348572));
#269279=CARTESIAN_POINT('Ctrl Pts',(-68.7998999948417,144.516898051454,
509.537703348572));
#269280=CARTESIAN_POINT('Ctrl Pts',(-57.4261734531929,149.931567610411,
507.537703348572));
#269281=CARTESIAN_POINT('Ctrl Pts',(-45.3454354230638,153.500330774912,
505.537703348572));
#269282=CARTESIAN_POINT('Ctrl Pts',(-33.2646973929347,157.069093939413,
503.537703348572));
#269283=CARTESIAN_POINT('Ctrl Pts',(-20.774415738298,158.704075916301,501.537703348572));
#269284=CARTESIAN_POINT('Ctrl Pts',(-8.28413408366129,160.339057893189,
499.537703348572));
#269285=CARTESIAN_POINT('Ctrl Pts',(4.30813900827766,160.,497.537703348572));
#269286=CARTESIAN_POINT('Ctrl Pts',(16.9004121002166,159.660942106811,495.537703348572));
#269287=CARTESIAN_POINT('Ctrl Pts',(29.2846130745759,157.356193074143,493.537703348572));
#269288=CARTESIAN_POINT('Ctrl Pts',(41.6688140489352,155.051444041476,491.537703348572));
#269289=CARTESIAN_POINT('Ctrl Pts',(53.5400027769194,150.837754439537,489.537703348572));
#269290=CARTESIAN_POINT('Ctrl Pts',(65.4111915049037,146.624064837599,487.537703348572));
#269291=CARTESIAN_POINT('Ctrl Pts',(76.4770599218133,140.605189688823,485.537703348572));
#269292=CARTESIAN_POINT('Ctrl Pts',(87.542928338723,134.586314540048,483.537703348572));
#269293=CARTESIAN_POINT('Ctrl Pts',(97.530998038622,126.9104585261,481.537703348572));
#269294=CARTESIAN_POINT('Ctrl Pts',(107.519067738521,119.234602512152,479.537703348572));
#269295=CARTESIAN_POINT('Ctrl Pts',(116.183399296895,110.0907706828,477.537703348572));
#269296=CARTESIAN_POINT('Ctrl Pts',(124.847730855269,100.946938853448,475.537703348572));
#269297=CARTESIAN_POINT('Ctrl Pts',(131.974979673883,90.5602826949695,473.537703348572));
#269298=CARTESIAN_POINT('Ctrl Pts',(139.102228492497,80.1736265364906,471.537703348572));
#269299=CARTESIAN_POINT('Ctrl Pts',(144.516898051454,68.7998999948417,469.537703348572));
#269300=CARTESIAN_POINT('Ctrl Pts',(149.931567610411,57.4261734531929,467.537703348572));
#269301=CARTESIAN_POINT('Ctrl Pts',(153.500330774912,45.3454354230638,465.537703348572));
#269302=CARTESIAN_POINT('Ctrl Pts',(157.069093939413,33.2646973929347,463.537703348572));
#269303=CARTESIAN_POINT('Ctrl Pts',(158.704075916301,20.774415738298,461.537703348572));
#269304=CARTESIAN_POINT('Ctrl Pts',(160.339057893189,8.28413408366131,459.537703348572));
#269305=CARTESIAN_POINT('Ctrl Pts',(160.,-4.30813900827765,457.537703348572));
#269306=CARTESIAN_POINT('Ctrl Pts',(159.660942106811,-16.9004121002166,
455.537703348572));
#269307=CARTESIAN_POINT('Ctrl Pts',(157.356193074143,-29.2846130745759,
453.537703348572));
#269308=CARTESIAN_POINT('Ctrl Pts',(155.051444041476,-41.6688140489352,
451.537703348572));
#269309=CARTESIAN_POINT('Ctrl Pts',(150.837754439537,-53.5400027769194,
449.537703348572));
#269310=CARTESIAN_POINT('Ctrl Pts',(146.624064837599,-65.4111915049036,
447.537703348572));
#269311=CARTESIAN_POINT('Ctrl Pts',(140.605189688823,-76.4770599218133,
445.537703348572));
#269312=CARTESIAN_POINT('Ctrl Pts',(134.586314540048,-87.5429283387229,
443.537703348572));
#269313=CARTESIAN_POINT('Ctrl Pts',(126.9104585261,-97.530998038622,441.537703348572));
#269314=CARTESIAN_POINT('Ctrl Pts',(119.234602512152,-107.519067738521,
439.537703348572));
#269315=CARTESIAN_POINT('Ctrl Pts',(110.0907706828,-116.183399296895,437.537703348572));
#269316=CARTESIAN_POINT('Ctrl Pts',(100.946938853448,-124.847730855269,
435.537703348572));
#269317=CARTESIAN_POINT('Ctrl Pts',(90.5602826949695,-131.974979673883,
433.537703348572));
#269318=CARTESIAN_POINT('Ctrl Pts',(80.1736265364905,-139.102228492497,
431.537703348572));
#269319=CARTESIAN_POINT('Ctrl Pts',(68.7998999948417,-144.516898051454,
429.537703348572));
#269320=CARTESIAN_POINT('Ctrl Pts',(57.426173453193,-149.931567610411,427.537703348572));
#269321=CARTESIAN_POINT('Ctrl Pts',(45.3454354230638,-153.500330774912,
425.537703348572));
#269322=CARTESIAN_POINT('Ctrl Pts',(33.2646973929347,-157.069093939413,
423.537703348572));
#269323=CARTESIAN_POINT('Ctrl Pts',(20.774415738298,-158.704075916301,421.537703348572));
#269324=CARTESIAN_POINT('Ctrl Pts',(8.28413408366139,-160.339057893189,
419.537703348572));
#269325=CARTESIAN_POINT('Ctrl Pts',(-4.30813900827764,-160.,417.537703348572));
#269326=CARTESIAN_POINT('Ctrl Pts',(-16.9004121002167,-159.660942106811,
415.537703348572));
#269327=CARTESIAN_POINT('Ctrl Pts',(-29.2846130745759,-157.356193074143,
413.537703348572));
#269328=CARTESIAN_POINT('Ctrl Pts',(-41.6688140489351,-155.051444041476,
411.537703348572));
#269329=CARTESIAN_POINT('Ctrl Pts',(-53.5400027769194,-150.837754439537,
409.537703348572));
#269330=CARTESIAN_POINT('Ctrl Pts',(-65.4111915049037,-146.624064837599,
407.537703348572));
#269331=CARTESIAN_POINT('Ctrl Pts',(-76.4770599218133,-140.605189688823,
405.537703348572));
#269332=CARTESIAN_POINT('Ctrl Pts',(-87.5429283387229,-134.586314540048,
403.537703348572));
#269333=CARTESIAN_POINT('Ctrl Pts',(-97.530998038622,-126.9104585261,401.537703348572));
#269334=CARTESIAN_POINT('Ctrl Pts',(-107.519067738521,-119.234602512152,
399.537703348572));
#269335=CARTESIAN_POINT('Ctrl Pts',(-116.183399296895,-110.0907706828,397.537703348572));
#269336=CARTESIAN_POINT('Ctrl Pts',(-124.847730855269,-100.946938853448,
395.537703348572));
#269337=CARTESIAN_POINT('Ctrl Pts',(-131.974979673883,-90.5602826949695,
393.537703348572));
#269338=CARTESIAN_POINT('Ctrl Pts',(-139.102228492497,-80.1736265364905,
391.537703348572));
#269339=CARTESIAN_POINT('Ctrl Pts',(-144.516898051454,-68.7998999948417,
389.537703348572));
#269340=CARTESIAN_POINT('Ctrl Pts',(-149.931567610411,-57.426173453193,
387.537703348572));
#269341=CARTESIAN_POINT('Ctrl Pts',(-153.500330774912,-45.3454354230638,
385.537703348572));
#269342=CARTESIAN_POINT('Ctrl Pts',(-157.069093939413,-33.2646973929347,
383.537703348572));
#269343=CARTESIAN_POINT('Ctrl Pts',(-158.704075916301,-20.774415738298,
381.537703348572));
#269344=CARTESIAN_POINT('Ctrl Pts',(-159.653854600275,-13.5186762622036,
380.375881753716));
#269345=CARTESIAN_POINT('Ctrl Pts',(-159.937609420477,-6.20654127333065,
379.210563551645));
#269346=CARTESIAN_POINT('Ctrl Pts',(-160.,-4.30813900827851,532.462296651429));
#269347=CARTESIAN_POINT('Ctrl Pts',(-160.339057893189,8.28413408366045,
530.462296651429));
#269348=CARTESIAN_POINT('Ctrl Pts',(-158.704075916301,20.7744157382972,
528.462296651429));
#269349=CARTESIAN_POINT('Ctrl Pts',(-157.069093939413,33.2646973929339,
526.462296651429));
#269350=CARTESIAN_POINT('Ctrl Pts',(-153.500330774912,45.345435423063,524.462296651428));
#269351=CARTESIAN_POINT('Ctrl Pts',(-149.931567610412,57.4261734531921,
522.462296651429));
#269352=CARTESIAN_POINT('Ctrl Pts',(-144.516898051455,68.7998999948409,
520.462296651428));
#269353=CARTESIAN_POINT('Ctrl Pts',(-139.102228492498,80.1736265364898,
518.462296651428));
#269354=CARTESIAN_POINT('Ctrl Pts',(-131.974979673884,90.5602826949688,
516.462296651428));
#269355=CARTESIAN_POINT('Ctrl Pts',(-124.84773085527,100.946938853448,514.462296651429));
#269356=CARTESIAN_POINT('Ctrl Pts',(-116.183399296896,110.0907706828,512.462296651428));
#269357=CARTESIAN_POINT('Ctrl Pts',(-107.519067738522,119.234602512151,
510.462296651429));
#269358=CARTESIAN_POINT('Ctrl Pts',(-97.5309980386227,126.9104585261,508.462296651429));
#269359=CARTESIAN_POINT('Ctrl Pts',(-87.5429283387237,134.586314540048,
506.462296651428));
#269360=CARTESIAN_POINT('Ctrl Pts',(-76.4770599218141,140.605189688823,
504.462296651429));
#269361=CARTESIAN_POINT('Ctrl Pts',(-65.4111915049045,146.624064837598,
502.462296651429));
#269362=CARTESIAN_POINT('Ctrl Pts',(-53.5400027769202,150.837754439537,
500.462296651429));
#269363=CARTESIAN_POINT('Ctrl Pts',(-41.668814048936,155.051444041475,498.462296651429));
#269364=CARTESIAN_POINT('Ctrl Pts',(-29.2846130745767,157.356193074143,
496.462296651429));
#269365=CARTESIAN_POINT('Ctrl Pts',(-16.9004121002175,159.660942106811,
494.462296651429));
#269366=CARTESIAN_POINT('Ctrl Pts',(-4.30813900827852,160.,492.462296651428));
#269367=CARTESIAN_POINT('Ctrl Pts',(8.28413408366043,160.339057893189,490.462296651429));
#269368=CARTESIAN_POINT('Ctrl Pts',(20.7744157382972,158.704075916301,488.462296651429));
#269369=CARTESIAN_POINT('Ctrl Pts',(33.2646973929339,157.069093939413,486.462296651429));
#269370=CARTESIAN_POINT('Ctrl Pts',(45.345435423063,153.500330774912,484.462296651429));
#269371=CARTESIAN_POINT('Ctrl Pts',(57.4261734531921,149.931567610412,482.462296651429));
#269372=CARTESIAN_POINT('Ctrl Pts',(68.7998999948409,144.516898051455,480.462296651428));
#269373=CARTESIAN_POINT('Ctrl Pts',(80.1736265364898,139.102228492498,478.462296651429));
#269374=CARTESIAN_POINT('Ctrl Pts',(90.5602826949688,131.974979673884,476.462296651428));
#269375=CARTESIAN_POINT('Ctrl Pts',(100.946938853448,124.84773085527,474.462296651429));
#269376=CARTESIAN_POINT('Ctrl Pts',(110.0907706828,116.183399296896,472.462296651429));
#269377=CARTESIAN_POINT('Ctrl Pts',(119.234602512151,107.519067738522,470.462296651429));
#269378=CARTESIAN_POINT('Ctrl Pts',(126.9104585261,97.5309980386227,468.462296651429));
#269379=CARTESIAN_POINT('Ctrl Pts',(134.586314540048,87.5429283387237,466.462296651429));
#269380=CARTESIAN_POINT('Ctrl Pts',(140.605189688823,76.4770599218141,464.462296651429));
#269381=CARTESIAN_POINT('Ctrl Pts',(146.624064837598,65.4111915049045,462.462296651429));
#269382=CARTESIAN_POINT('Ctrl Pts',(150.837754439537,53.5400027769202,460.462296651429));
#269383=CARTESIAN_POINT('Ctrl Pts',(155.051444041475,41.668814048936,458.462296651429));
#269384=CARTESIAN_POINT('Ctrl Pts',(157.356193074143,29.2846130745767,456.462296651429));
#269385=CARTESIAN_POINT('Ctrl Pts',(159.660942106811,16.9004121002175,454.462296651429));
#269386=CARTESIAN_POINT('Ctrl Pts',(160.,4.30813900827853,452.462296651429));
#269387=CARTESIAN_POINT('Ctrl Pts',(160.339057893189,-8.28413408366043,
450.462296651429));
#269388=CARTESIAN_POINT('Ctrl Pts',(158.704075916301,-20.7744157382971,
448.462296651429));
#269389=CARTESIAN_POINT('Ctrl Pts',(157.069093939413,-33.2646973929339,
446.462296651429));
#269390=CARTESIAN_POINT('Ctrl Pts',(153.500330774912,-45.345435423063,444.462296651429));
#269391=CARTESIAN_POINT('Ctrl Pts',(149.931567610412,-57.4261734531921,
442.462296651429));
#269392=CARTESIAN_POINT('Ctrl Pts',(144.516898051455,-68.7998999948409,
440.462296651429));
#269393=CARTESIAN_POINT('Ctrl Pts',(139.102228492498,-80.1736265364898,
438.462296651429));
#269394=CARTESIAN_POINT('Ctrl Pts',(131.974979673884,-90.5602826949688,
436.462296651429));
#269395=CARTESIAN_POINT('Ctrl Pts',(124.84773085527,-100.946938853448,434.462296651429));
#269396=CARTESIAN_POINT('Ctrl Pts',(116.183399296896,-110.0907706828,432.462296651429));
#269397=CARTESIAN_POINT('Ctrl Pts',(107.519067738522,-119.234602512151,
430.462296651429));
#269398=CARTESIAN_POINT('Ctrl Pts',(97.5309980386227,-126.9104585261,428.462296651429));
#269399=CARTESIAN_POINT('Ctrl Pts',(87.5429283387236,-134.586314540048,
426.462296651429));
#269400=CARTESIAN_POINT('Ctrl Pts',(76.4770599218141,-140.605189688823,
424.462296651429));
#269401=CARTESIAN_POINT('Ctrl Pts',(65.4111915049046,-146.624064837598,
422.462296651429));
#269402=CARTESIAN_POINT('Ctrl Pts',(53.5400027769202,-150.837754439537,
420.462296651429));
#269403=CARTESIAN_POINT('Ctrl Pts',(41.6688140489359,-155.051444041475,
418.462296651429));
#269404=CARTESIAN_POINT('Ctrl Pts',(29.2846130745768,-157.356193074143,
416.462296651429));
#269405=CARTESIAN_POINT('Ctrl Pts',(16.9004121002176,-159.660942106811,
414.462296651429));
#269406=CARTESIAN_POINT('Ctrl Pts',(4.30813900827854,-160.,412.462296651429));
#269407=CARTESIAN_POINT('Ctrl Pts',(-8.28413408366049,-160.339057893189,
410.462296651429));
#269408=CARTESIAN_POINT('Ctrl Pts',(-20.7744157382971,-158.704075916301,
408.462296651429));
#269409=CARTESIAN_POINT('Ctrl Pts',(-33.2646973929338,-157.069093939413,
406.462296651429));
#269410=CARTESIAN_POINT('Ctrl Pts',(-45.345435423063,-153.500330774912,
404.462296651429));
#269411=CARTESIAN_POINT('Ctrl Pts',(-57.4261734531921,-149.931567610412,
402.462296651429));
#269412=CARTESIAN_POINT('Ctrl Pts',(-68.7998999948409,-144.516898051455,
400.462296651429));
#269413=CARTESIAN_POINT('Ctrl Pts',(-80.1736265364897,-139.102228492498,
398.462296651429));
#269414=CARTESIAN_POINT('Ctrl Pts',(-90.5602826949688,-131.974979673884,
396.462296651429));
#269415=CARTESIAN_POINT('Ctrl Pts',(-100.946938853448,-124.84773085527,
394.462296651429));
#269416=CARTESIAN_POINT('Ctrl Pts',(-110.0907706828,-116.183399296896,392.462296651429));
#269417=CARTESIAN_POINT('Ctrl Pts',(-119.234602512151,-107.519067738522,
390.462296651429));
#269418=CARTESIAN_POINT('Ctrl Pts',(-126.9104585261,-97.5309980386227,388.462296651429));
#269419=CARTESIAN_POINT('Ctrl Pts',(-134.586314540048,-87.5429283387236,
386.462296651429));
#269420=CARTESIAN_POINT('Ctrl Pts',(-140.605189688823,-76.4770599218141,
384.462296651429));
#269421=CARTESIAN_POINT('Ctrl Pts',(-146.624064837598,-65.4111915049046,
382.462296651429));
#269422=CARTESIAN_POINT('Ctrl Pts',(-150.837754439537,-53.5400027769203,
380.462296651429));
#269423=CARTESIAN_POINT('Ctrl Pts',(-155.051444041475,-41.668814048936,
378.462296651429));
#269424=CARTESIAN_POINT('Ctrl Pts',(-157.356193074143,-29.2846130745768,
376.462296651429));
#269425=CARTESIAN_POINT('Ctrl Pts',(-159.660942106811,-16.9004121002176,
374.462296651429));
#269426=CARTESIAN_POINT('Ctrl Pts',(-160.,-4.30813900827851,372.462296651429));
#269427=CARTESIAN_POINT('Ctrl Pts',(-160.,4.30813900827767,537.537703348572));
#269428=CARTESIAN_POINT('Ctrl Pts',(-159.660942106811,16.9004121002166,
535.537703348572));
#269429=CARTESIAN_POINT('Ctrl Pts',(-157.356193074143,29.2846130745759,
533.537703348572));
#269430=CARTESIAN_POINT('Ctrl Pts',(-155.051444041476,41.6688140489352,
531.537703348572));
#269431=CARTESIAN_POINT('Ctrl Pts',(-150.837754439537,53.5400027769194,
529.537703348572));
#269432=CARTESIAN_POINT('Ctrl Pts',(-146.624064837599,65.4111915049037,
527.537703348572));
#269433=CARTESIAN_POINT('Ctrl Pts',(-140.605189688823,76.4770599218133,
525.537703348572));
#269434=CARTESIAN_POINT('Ctrl Pts',(-134.586314540048,87.542928338723,523.537703348572));
#269435=CARTESIAN_POINT('Ctrl Pts',(-126.9104585261,97.530998038622,521.537703348572));
#269436=CARTESIAN_POINT('Ctrl Pts',(-119.234602512152,107.519067738521,
519.537703348572));
#269437=CARTESIAN_POINT('Ctrl Pts',(-110.0907706828,116.183399296895,517.537703348572));
#269438=CARTESIAN_POINT('Ctrl Pts',(-100.946938853448,124.847730855269,
515.537703348572));
#269439=CARTESIAN_POINT('Ctrl Pts',(-90.5602826949695,131.974979673883,
513.537703348572));
#269440=CARTESIAN_POINT('Ctrl Pts',(-80.1736265364906,139.102228492497,
511.537703348572));
#269441=CARTESIAN_POINT('Ctrl Pts',(-68.7998999948417,144.516898051454,
509.537703348572));
#269442=CARTESIAN_POINT('Ctrl Pts',(-57.4261734531929,149.931567610411,
507.537703348572));
#269443=CARTESIAN_POINT('Ctrl Pts',(-45.3454354230638,153.500330774912,
505.537703348572));
#269444=CARTESIAN_POINT('Ctrl Pts',(-33.2646973929347,157.069093939413,
503.537703348572));
#269445=CARTESIAN_POINT('Ctrl Pts',(-20.774415738298,158.704075916301,501.537703348572));
#269446=CARTESIAN_POINT('Ctrl Pts',(-8.28413408366129,160.339057893189,
499.537703348572));
#269447=CARTESIAN_POINT('Ctrl Pts',(4.30813900827766,160.,497.537703348572));
#269448=CARTESIAN_POINT('Ctrl Pts',(16.9004121002166,159.660942106811,495.537703348572));
#269449=CARTESIAN_POINT('Ctrl Pts',(29.2846130745759,157.356193074143,493.537703348572));
#269450=CARTESIAN_POINT('Ctrl Pts',(41.6688140489352,155.051444041476,491.537703348572));
#269451=CARTESIAN_POINT('Ctrl Pts',(53.5400027769194,150.837754439537,489.537703348572));
#269452=CARTESIAN_POINT('Ctrl Pts',(65.4111915049037,146.624064837599,487.537703348572));
#269453=CARTESIAN_POINT('Ctrl Pts',(76.4770599218133,140.605189688823,485.537703348572));
#269454=CARTESIAN_POINT('Ctrl Pts',(87.542928338723,134.586314540048,483.537703348572));
#269455=CARTESIAN_POINT('Ctrl Pts',(97.530998038622,126.9104585261,481.537703348572));
#269456=CARTESIAN_POINT('Ctrl Pts',(107.519067738521,119.234602512152,479.537703348572));
#269457=CARTESIAN_POINT('Ctrl Pts',(116.183399296895,110.0907706828,477.537703348572));
#269458=CARTESIAN_POINT('Ctrl Pts',(124.847730855269,100.946938853448,475.537703348572));
#269459=CARTESIAN_POINT('Ctrl Pts',(131.974979673883,90.5602826949695,473.537703348572));
#269460=CARTESIAN_POINT('Ctrl Pts',(139.102228492497,80.1736265364906,471.537703348572));
#269461=CARTESIAN_POINT('Ctrl Pts',(144.516898051454,68.7998999948417,469.537703348572));
#269462=CARTESIAN_POINT('Ctrl Pts',(149.931567610411,57.4261734531929,467.537703348572));
#269463=CARTESIAN_POINT('Ctrl Pts',(153.500330774912,45.3454354230638,465.537703348572));
#269464=CARTESIAN_POINT('Ctrl Pts',(157.069093939413,33.2646973929347,463.537703348572));
#269465=CARTESIAN_POINT('Ctrl Pts',(158.704075916301,20.774415738298,461.537703348572));
#269466=CARTESIAN_POINT('Ctrl Pts',(160.339057893189,8.28413408366131,459.537703348572));
#269467=CARTESIAN_POINT('Ctrl Pts',(160.,-4.30813900827765,457.537703348572));
#269468=CARTESIAN_POINT('Ctrl Pts',(159.660942106811,-16.9004121002166,
455.537703348572));
#269469=CARTESIAN_POINT('Ctrl Pts',(157.356193074143,-29.2846130745759,
453.537703348572));
#269470=CARTESIAN_POINT('Ctrl Pts',(155.051444041476,-41.6688140489352,
451.537703348572));
#269471=CARTESIAN_POINT('Ctrl Pts',(150.837754439537,-53.5400027769194,
449.537703348572));
#269472=CARTESIAN_POINT('Ctrl Pts',(146.624064837599,-65.4111915049036,
447.537703348572));
#269473=CARTESIAN_POINT('Ctrl Pts',(140.605189688823,-76.4770599218133,
445.537703348572));
#269474=CARTESIAN_POINT('Ctrl Pts',(134.586314540048,-87.5429283387229,
443.537703348572));
#269475=CARTESIAN_POINT('Ctrl Pts',(126.9104585261,-97.530998038622,441.537703348572));
#269476=CARTESIAN_POINT('Ctrl Pts',(119.234602512152,-107.519067738521,
439.537703348572));
#269477=CARTESIAN_POINT('Ctrl Pts',(110.0907706828,-116.183399296895,437.537703348572));
#269478=CARTESIAN_POINT('Ctrl Pts',(100.946938853448,-124.847730855269,
435.537703348572));
#269479=CARTESIAN_POINT('Ctrl Pts',(90.5602826949695,-131.974979673883,
433.537703348572));
#269480=CARTESIAN_POINT('Ctrl Pts',(80.1736265364905,-139.102228492497,
431.537703348572));
#269481=CARTESIAN_POINT('Ctrl Pts',(68.7998999948417,-144.516898051454,
429.537703348572));
#269482=CARTESIAN_POINT('Ctrl Pts',(57.426173453193,-149.931567610411,427.537703348572));
#269483=CARTESIAN_POINT('Ctrl Pts',(45.3454354230638,-153.500330774912,
425.537703348572));
#269484=CARTESIAN_POINT('Ctrl Pts',(33.2646973929347,-157.069093939413,
423.537703348572));
#269485=CARTESIAN_POINT('Ctrl Pts',(20.774415738298,-158.704075916301,421.537703348572));
#269486=CARTESIAN_POINT('Ctrl Pts',(8.28413408366139,-160.339057893189,
419.537703348572));
#269487=CARTESIAN_POINT('Ctrl Pts',(-4.30813900827764,-160.,417.537703348572));
#269488=CARTESIAN_POINT('Ctrl Pts',(-16.9004121002167,-159.660942106811,
415.537703348572));
#269489=CARTESIAN_POINT('Ctrl Pts',(-29.2846130745759,-157.356193074143,
413.537703348572));
#269490=CARTESIAN_POINT('Ctrl Pts',(-41.6688140489351,-155.051444041476,
411.537703348572));
#269491=CARTESIAN_POINT('Ctrl Pts',(-53.5400027769194,-150.837754439537,
409.537703348572));
#269492=CARTESIAN_POINT('Ctrl Pts',(-65.4111915049037,-146.624064837599,
407.537703348572));
#269493=CARTESIAN_POINT('Ctrl Pts',(-76.4770599218133,-140.605189688823,
405.537703348572));
#269494=CARTESIAN_POINT('Ctrl Pts',(-87.5429283387229,-134.586314540048,
403.537703348572));
#269495=CARTESIAN_POINT('Ctrl Pts',(-97.530998038622,-126.9104585261,401.537703348572));
#269496=CARTESIAN_POINT('Ctrl Pts',(-107.519067738521,-119.234602512152,
399.537703348572));
#269497=CARTESIAN_POINT('Ctrl Pts',(-116.183399296895,-110.0907706828,397.537703348572));
#269498=CARTESIAN_POINT('Ctrl Pts',(-124.847730855269,-100.946938853448,
395.537703348572));
#269499=CARTESIAN_POINT('Ctrl Pts',(-131.974979673883,-90.5602826949695,
393.537703348572));
#269500=CARTESIAN_POINT('Ctrl Pts',(-139.102228492497,-80.1736265364905,
391.537703348572));
#269501=CARTESIAN_POINT('Ctrl Pts',(-144.516898051454,-68.7998999948417,
389.537703348572));
#269502=CARTESIAN_POINT('Ctrl Pts',(-149.931567610411,-57.426173453193,
387.537703348572));
#269503=CARTESIAN_POINT('Ctrl Pts',(-153.500330774912,-45.3454354230638,
385.537703348572));
#269504=CARTESIAN_POINT('Ctrl Pts',(-157.069093939413,-33.2646973929347,
383.537703348572));
#269505=CARTESIAN_POINT('Ctrl Pts',(-158.704075916301,-20.774415738298,
381.537703348572));
#269506=CARTESIAN_POINT('Ctrl Pts',(-160.339057893189,-8.2841340836614,
379.537703348572));
#269507=CARTESIAN_POINT('Ctrl Pts',(-160.,4.30813900827767,377.537703348572));
#269508=CARTESIAN_POINT('Ctrl Pts',(-159.937609420477,6.2065412733309,530.789436448355));
#269509=CARTESIAN_POINT('Ctrl Pts',(-159.653854600275,13.5186762622033,
529.624118246284));
#269510=CARTESIAN_POINT('Ctrl Pts',(-158.704075916301,20.7744157382972,
528.462296651429));
#269511=CARTESIAN_POINT('Ctrl Pts',(-157.069093939413,33.2646973929339,
526.462296651429));
#269512=CARTESIAN_POINT('Ctrl Pts',(-153.500330774912,45.345435423063,524.462296651428));
#269513=CARTESIAN_POINT('Ctrl Pts',(-149.931567610412,57.4261734531921,
522.462296651429));
#269514=CARTESIAN_POINT('Ctrl Pts',(-144.516898051455,68.7998999948409,
520.462296651428));
#269515=CARTESIAN_POINT('Ctrl Pts',(-139.102228492498,80.1736265364898,
518.462296651428));
#269516=CARTESIAN_POINT('Ctrl Pts',(-131.974979673884,90.5602826949688,
516.462296651428));
#269517=CARTESIAN_POINT('Ctrl Pts',(-124.84773085527,100.946938853448,514.462296651429));
#269518=CARTESIAN_POINT('Ctrl Pts',(-116.183399296896,110.0907706828,512.462296651428));
#269519=CARTESIAN_POINT('Ctrl Pts',(-107.519067738522,119.234602512151,
510.462296651429));
#269520=CARTESIAN_POINT('Ctrl Pts',(-97.5309980386227,126.9104585261,508.462296651429));
#269521=CARTESIAN_POINT('Ctrl Pts',(-87.5429283387237,134.586314540048,
506.462296651429));
#269522=CARTESIAN_POINT('Ctrl Pts',(-76.4770599218141,140.605189688823,
504.462296651429));
#269523=CARTESIAN_POINT('Ctrl Pts',(-65.4111915049045,146.624064837598,
502.462296651429));
#269524=CARTESIAN_POINT('Ctrl Pts',(-53.5400027769202,150.837754439537,
500.462296651429));
#269525=CARTESIAN_POINT('Ctrl Pts',(-41.668814048936,155.051444041475,498.462296651429));
#269526=CARTESIAN_POINT('Ctrl Pts',(-29.2846130745767,157.356193074143,
496.462296651429));
#269527=CARTESIAN_POINT('Ctrl Pts',(-16.9004121002175,159.660942106811,
494.462296651429));
#269528=CARTESIAN_POINT('Ctrl Pts',(-4.30813900827852,160.,492.462296651428));
#269529=CARTESIAN_POINT('Ctrl Pts',(8.28413408366043,160.339057893189,490.462296651429));
#269530=CARTESIAN_POINT('Ctrl Pts',(20.7744157382972,158.704075916301,488.462296651429));
#269531=CARTESIAN_POINT('Ctrl Pts',(33.2646973929339,157.069093939413,486.462296651429));
#269532=CARTESIAN_POINT('Ctrl Pts',(45.345435423063,153.500330774912,484.462296651429));
#269533=CARTESIAN_POINT('Ctrl Pts',(57.4261734531921,149.931567610412,482.462296651429));
#269534=CARTESIAN_POINT('Ctrl Pts',(68.7998999948409,144.516898051455,480.462296651428));
#269535=CARTESIAN_POINT('Ctrl Pts',(80.1736265364898,139.102228492498,478.462296651429));
#269536=CARTESIAN_POINT('Ctrl Pts',(90.5602826949688,131.974979673884,476.462296651428));
#269537=CARTESIAN_POINT('Ctrl Pts',(100.946938853448,124.84773085527,474.462296651429));
#269538=CARTESIAN_POINT('Ctrl Pts',(110.0907706828,116.183399296896,472.462296651429));
#269539=CARTESIAN_POINT('Ctrl Pts',(119.234602512151,107.519067738522,470.462296651429));
#269540=CARTESIAN_POINT('Ctrl Pts',(126.9104585261,97.5309980386227,468.462296651429));
#269541=CARTESIAN_POINT('Ctrl Pts',(134.586314540048,87.5429283387237,466.462296651429));
#269542=CARTESIAN_POINT('Ctrl Pts',(140.605189688823,76.4770599218141,464.462296651429));
#269543=CARTESIAN_POINT('Ctrl Pts',(146.624064837598,65.4111915049045,462.462296651429));
#269544=CARTESIAN_POINT('Ctrl Pts',(150.837754439537,53.5400027769202,460.462296651429));
#269545=CARTESIAN_POINT('Ctrl Pts',(155.051444041475,41.668814048936,458.462296651429));
#269546=CARTESIAN_POINT('Ctrl Pts',(157.356193074143,29.2846130745767,456.462296651429));
#269547=CARTESIAN_POINT('Ctrl Pts',(159.660942106811,16.9004121002175,454.462296651429));
#269548=CARTESIAN_POINT('Ctrl Pts',(160.,4.30813900827853,452.462296651429));
#269549=CARTESIAN_POINT('Ctrl Pts',(160.339057893189,-8.28413408366043,
450.462296651429));
#269550=CARTESIAN_POINT('Ctrl Pts',(158.704075916301,-20.7744157382971,
448.462296651429));
#269551=CARTESIAN_POINT('Ctrl Pts',(157.069093939413,-33.2646973929339,
446.462296651429));
#269552=CARTESIAN_POINT('Ctrl Pts',(153.500330774912,-45.345435423063,444.462296651429));
#269553=CARTESIAN_POINT('Ctrl Pts',(149.931567610412,-57.4261734531921,
442.462296651429));
#269554=CARTESIAN_POINT('Ctrl Pts',(144.516898051455,-68.7998999948409,
440.462296651429));
#269555=CARTESIAN_POINT('Ctrl Pts',(139.102228492498,-80.1736265364898,
438.462296651429));
#269556=CARTESIAN_POINT('Ctrl Pts',(131.974979673884,-90.5602826949688,
436.462296651429));
#269557=CARTESIAN_POINT('Ctrl Pts',(124.84773085527,-100.946938853448,434.462296651429));
#269558=CARTESIAN_POINT('Ctrl Pts',(116.183399296896,-110.0907706828,432.462296651429));
#269559=CARTESIAN_POINT('Ctrl Pts',(107.519067738522,-119.234602512151,
430.462296651429));
#269560=CARTESIAN_POINT('Ctrl Pts',(97.5309980386227,-126.9104585261,428.462296651429));
#269561=CARTESIAN_POINT('Ctrl Pts',(87.5429283387236,-134.586314540048,
426.462296651429));
#269562=CARTESIAN_POINT('Ctrl Pts',(76.4770599218141,-140.605189688823,
424.462296651429));
#269563=CARTESIAN_POINT('Ctrl Pts',(65.4111915049045,-146.624064837598,
422.462296651429));
#269564=CARTESIAN_POINT('Ctrl Pts',(53.5400027769202,-150.837754439537,
420.462296651429));
#269565=CARTESIAN_POINT('Ctrl Pts',(41.6688140489359,-155.051444041475,
418.462296651429));
#269566=CARTESIAN_POINT('Ctrl Pts',(29.2846130745768,-157.356193074143,
416.462296651429));
#269567=CARTESIAN_POINT('Ctrl Pts',(16.9004121002176,-159.660942106811,
414.462296651429));
#269568=CARTESIAN_POINT('Ctrl Pts',(4.30813900827854,-160.,412.462296651429));
#269569=CARTESIAN_POINT('Ctrl Pts',(-8.28413408366049,-160.339057893189,
410.462296651429));
#269570=CARTESIAN_POINT('Ctrl Pts',(-20.7744157382971,-158.704075916301,
408.462296651429));
#269571=CARTESIAN_POINT('Ctrl Pts',(-33.2646973929338,-157.069093939413,
406.462296651429));
#269572=CARTESIAN_POINT('Ctrl Pts',(-45.345435423063,-153.500330774912,
404.462296651429));
#269573=CARTESIAN_POINT('Ctrl Pts',(-57.4261734531921,-149.931567610412,
402.462296651429));
#269574=CARTESIAN_POINT('Ctrl Pts',(-68.7998999948409,-144.516898051455,
400.462296651429));
#269575=CARTESIAN_POINT('Ctrl Pts',(-80.1736265364897,-139.102228492498,
398.462296651429));
#269576=CARTESIAN_POINT('Ctrl Pts',(-90.5602826949688,-131.974979673884,
396.462296651429));
#269577=CARTESIAN_POINT('Ctrl Pts',(-100.946938853448,-124.84773085527,
394.462296651429));
#269578=CARTESIAN_POINT('Ctrl Pts',(-110.0907706828,-116.183399296896,392.462296651429));
#269579=CARTESIAN_POINT('Ctrl Pts',(-119.234602512151,-107.519067738522,
390.462296651429));
#269580=CARTESIAN_POINT('Ctrl Pts',(-126.9104585261,-97.5309980386227,388.462296651429));
#269581=CARTESIAN_POINT('Ctrl Pts',(-134.586314540048,-87.5429283387237,
386.462296651429));
#269582=CARTESIAN_POINT('Ctrl Pts',(-140.605189688823,-76.4770599218141,
384.462296651429));
#269583=CARTESIAN_POINT('Ctrl Pts',(-146.624064837598,-65.4111915049046,
382.462296651429));
#269584=CARTESIAN_POINT('Ctrl Pts',(-150.837754439537,-53.5400027769203,
380.462296651429));
#269585=CARTESIAN_POINT('Ctrl Pts',(-155.051444041475,-41.668814048936,
378.462296651429));
#269586=CARTESIAN_POINT('Ctrl Pts',(-157.356193074143,-29.2846130745768,
376.462296651429));
#269587=CARTESIAN_POINT('Ctrl Pts',(-159.394142202012,-18.3340187941083,
374.693818523023));
#269588=CARTESIAN_POINT('Ctrl Pts',(-159.895664541343,-7.20669984090295,
372.923108716584));
#269589=CARTESIAN_POINT('Ctrl Pts',(-130.,-4.30813900827845,532.462296651428));
#269590=CARTESIAN_POINT('Ctrl Pts',(-130.339057893189,5.92308287892195,
530.462296651429));
#269591=CARTESIAN_POINT('Ctrl Pts',(-129.073425698447,16.0813817870903,
528.462296651428));
#269592=CARTESIAN_POINT('Ctrl Pts',(-127.807793503705,26.2396806952586,
526.462296651429));
#269593=CARTESIAN_POINT('Ctrl Pts',(-124.968635286058,36.0749255918146,
524.462296651428));
#269594=CARTESIAN_POINT('Ctrl Pts',(-122.129477068411,45.9101704883706,
522.462296651428));
#269595=CARTESIAN_POINT('Ctrl Pts',(-117.786702325804,55.1801850026546,
520.462296651428));
#269596=CARTESIAN_POINT('Ctrl Pts',(-113.443927583196,64.4501995169386,
518.462296651428));
#269597=CARTESIAN_POINT('Ctrl Pts',(-107.704469842635,72.9267251261946,
516.462296651428));
#269598=CARTESIAN_POINT('Ctrl Pts',(-101.965012102074,81.4032507354507,
514.462296651428));
#269599=CARTESIAN_POINT('Ctrl Pts',(-94.9701958612992,88.8775672472032,
512.462296651428));
#269600=CARTESIAN_POINT('Ctrl Pts',(-87.9753796205245,96.3518837589558,
510.462296651429));
#269601=CARTESIAN_POINT('Ctrl Pts',(-79.8974404698484,102.639948694851,
508.462296651428));
#269602=CARTESIAN_POINT('Ctrl Pts',(-71.8195013191724,108.928013630747,
506.462296651428));
#269603=CARTESIAN_POINT('Ctrl Pts',(-62.8573449296276,113.874993963172,
504.462296651428));
#269604=CARTESIAN_POINT('Ctrl Pts',(-53.8951885400828,118.821974295598,
502.462296651428));
#269605=CARTESIAN_POINT('Ctrl Pts',(-44.2694929456717,122.306058950682,
500.462296651428));
#269606=CARTESIAN_POINT('Ctrl Pts',(-34.6437973512606,125.790143605767,
498.462296651429));
#269607=CARTESIAN_POINT('Ctrl Pts',(-24.5915791233697,127.725542856289,
496.462296651428));
#269608=CARTESIAN_POINT('Ctrl Pts',(-14.5393608954789,129.660942106811,
494.462296651428));
#269609=CARTESIAN_POINT('Ctrl Pts',(-4.30813900827846,130.,492.462296651428));
#269610=CARTESIAN_POINT('Ctrl Pts',(5.92308287892194,130.339057893189,490.462296651429));
#269611=CARTESIAN_POINT('Ctrl Pts',(16.0813817870903,129.073425698447,488.462296651428));
#269612=CARTESIAN_POINT('Ctrl Pts',(26.2396806952586,127.807793503705,486.462296651428));
#269613=CARTESIAN_POINT('Ctrl Pts',(36.0749255918146,124.968635286058,484.462296651428));
#269614=CARTESIAN_POINT('Ctrl Pts',(45.9101704883706,122.129477068411,482.462296651428));
#269615=CARTESIAN_POINT('Ctrl Pts',(55.1801850026546,117.786702325804,480.462296651428));
#269616=CARTESIAN_POINT('Ctrl Pts',(64.4501995169386,113.443927583196,478.462296651429));
#269617=CARTESIAN_POINT('Ctrl Pts',(72.9267251261946,107.704469842635,476.462296651428));
#269618=CARTESIAN_POINT('Ctrl Pts',(81.4032507354506,101.965012102074,474.462296651428));
#269619=CARTESIAN_POINT('Ctrl Pts',(88.8775672472032,94.9701958612992,472.462296651428));
#269620=CARTESIAN_POINT('Ctrl Pts',(96.3518837589558,87.9753796205245,470.462296651428));
#269621=CARTESIAN_POINT('Ctrl Pts',(102.639948694851,79.8974404698484,468.462296651428));
#269622=CARTESIAN_POINT('Ctrl Pts',(108.928013630747,71.8195013191724,466.462296651428));
#269623=CARTESIAN_POINT('Ctrl Pts',(113.874993963172,62.8573449296276,464.462296651428));
#269624=CARTESIAN_POINT('Ctrl Pts',(118.821974295598,53.8951885400829,462.462296651428));
#269625=CARTESIAN_POINT('Ctrl Pts',(122.306058950682,44.2694929456717,460.462296651428));
#269626=CARTESIAN_POINT('Ctrl Pts',(125.790143605767,34.6437973512606,458.462296651429));
#269627=CARTESIAN_POINT('Ctrl Pts',(127.725542856289,24.5915791233698,456.462296651428));
#269628=CARTESIAN_POINT('Ctrl Pts',(129.660942106811,14.5393608954789,454.462296651429));
#269629=CARTESIAN_POINT('Ctrl Pts',(130.,4.30813900827846,452.462296651428));
#269630=CARTESIAN_POINT('Ctrl Pts',(130.339057893189,-5.92308287892194,
450.462296651428));
#269631=CARTESIAN_POINT('Ctrl Pts',(129.073425698447,-16.0813817870903,
448.462296651429));
#269632=CARTESIAN_POINT('Ctrl Pts',(127.807793503705,-26.2396806952586,
446.462296651429));
#269633=CARTESIAN_POINT('Ctrl Pts',(124.968635286058,-36.0749255918146,
444.462296651429));
#269634=CARTESIAN_POINT('Ctrl Pts',(122.129477068411,-45.9101704883706,
442.462296651429));
#269635=CARTESIAN_POINT('Ctrl Pts',(117.786702325804,-55.1801850026546,
440.462296651428));
#269636=CARTESIAN_POINT('Ctrl Pts',(113.443927583196,-64.4501995169386,
438.462296651429));
#269637=CARTESIAN_POINT('Ctrl Pts',(107.704469842635,-72.9267251261946,
436.462296651428));
#269638=CARTESIAN_POINT('Ctrl Pts',(101.965012102074,-81.4032507354506,
434.462296651429));
#269639=CARTESIAN_POINT('Ctrl Pts',(94.9701958612992,-88.8775672472032,
432.462296651428));
#269640=CARTESIAN_POINT('Ctrl Pts',(87.9753796205246,-96.3518837589557,
430.462296651429));
#269641=CARTESIAN_POINT('Ctrl Pts',(79.8974404698484,-102.639948694851,
428.462296651429));
#269642=CARTESIAN_POINT('Ctrl Pts',(71.8195013191723,-108.928013630747,
426.462296651428));
#269643=CARTESIAN_POINT('Ctrl Pts',(62.8573449296276,-113.874993963172,
424.462296651428));
#269644=CARTESIAN_POINT('Ctrl Pts',(53.8951885400829,-118.821974295598,
422.462296651428));
#269645=CARTESIAN_POINT('Ctrl Pts',(44.2694929456717,-122.306058950682,
420.462296651428));
#269646=CARTESIAN_POINT('Ctrl Pts',(34.6437973512606,-125.790143605767,
418.462296651429));
#269647=CARTESIAN_POINT('Ctrl Pts',(24.5915791233698,-127.725542856289,
416.462296651428));
#269648=CARTESIAN_POINT('Ctrl Pts',(14.5393608954789,-129.660942106811,
414.462296651429));
#269649=CARTESIAN_POINT('Ctrl Pts',(4.30813900827847,-130.,412.462296651428));
#269650=CARTESIAN_POINT('Ctrl Pts',(-5.92308287892199,-130.339057893189,
410.462296651428));
#269651=CARTESIAN_POINT('Ctrl Pts',(-16.0813817870903,-129.073425698447,
408.462296651428));
#269652=CARTESIAN_POINT('Ctrl Pts',(-26.2396806952585,-127.807793503705,
406.462296651429));
#269653=CARTESIAN_POINT('Ctrl Pts',(-36.0749255918146,-124.968635286058,
404.462296651428));
#269654=CARTESIAN_POINT('Ctrl Pts',(-45.9101704883706,-122.129477068411,
402.462296651429));
#269655=CARTESIAN_POINT('Ctrl Pts',(-55.1801850026546,-117.786702325804,
400.462296651428));
#269656=CARTESIAN_POINT('Ctrl Pts',(-64.4501995169385,-113.443927583197,
398.462296651429));
#269657=CARTESIAN_POINT('Ctrl Pts',(-72.9267251261946,-107.704469842635,
396.462296651428));
#269658=CARTESIAN_POINT('Ctrl Pts',(-81.4032507354507,-101.965012102074,
394.462296651429));
#269659=CARTESIAN_POINT('Ctrl Pts',(-88.8775672472032,-94.9701958612992,
392.462296651428));
#269660=CARTESIAN_POINT('Ctrl Pts',(-96.3518837589557,-87.9753796205246,
390.462296651428));
#269661=CARTESIAN_POINT('Ctrl Pts',(-102.639948694851,-79.8974404698484,
388.462296651428));
#269662=CARTESIAN_POINT('Ctrl Pts',(-108.928013630747,-71.8195013191723,
386.462296651428));
#269663=CARTESIAN_POINT('Ctrl Pts',(-113.874993963172,-62.8573449296276,
384.462296651428));
#269664=CARTESIAN_POINT('Ctrl Pts',(-118.821974295598,-53.8951885400829,
382.462296651429));
#269665=CARTESIAN_POINT('Ctrl Pts',(-122.306058950682,-44.2694929456718,
380.462296651428));
#269666=CARTESIAN_POINT('Ctrl Pts',(-125.790143605767,-34.6437973512606,
378.462296651429));
#269667=CARTESIAN_POINT('Ctrl Pts',(-127.725542856289,-24.5915791233698,
376.462296651428));
#269668=CARTESIAN_POINT('Ctrl Pts',(-129.660942106811,-14.5393608954789,
374.462296651428));
#269669=CARTESIAN_POINT('Ctrl Pts',(-130.,-4.30813900827845,372.462296651428));
#269670=CARTESIAN_POINT('Ctrl Pts',(-160.,-4.30813900827851,532.462296651429));
#269671=CARTESIAN_POINT('Ctrl Pts',(-160.339057893189,8.28413408366045,
530.462296651429));
#269672=CARTESIAN_POINT('Ctrl Pts',(-158.704075916301,20.7744157382972,
528.462296651429));
#269673=CARTESIAN_POINT('Ctrl Pts',(-157.069093939413,33.2646973929339,
526.462296651429));
#269674=CARTESIAN_POINT('Ctrl Pts',(-153.500330774912,45.345435423063,524.462296651428));
#269675=CARTESIAN_POINT('Ctrl Pts',(-149.931567610412,57.4261734531921,
522.462296651429));
#269676=CARTESIAN_POINT('Ctrl Pts',(-144.516898051455,68.7998999948409,
520.462296651428));
#269677=CARTESIAN_POINT('Ctrl Pts',(-139.102228492498,80.1736265364898,
518.462296651428));
#269678=CARTESIAN_POINT('Ctrl Pts',(-131.974979673884,90.5602826949688,
516.462296651428));
#269679=CARTESIAN_POINT('Ctrl Pts',(-124.84773085527,100.946938853448,514.462296651429));
#269680=CARTESIAN_POINT('Ctrl Pts',(-116.183399296896,110.0907706828,512.462296651428));
#269681=CARTESIAN_POINT('Ctrl Pts',(-107.519067738522,119.234602512151,
510.462296651429));
#269682=CARTESIAN_POINT('Ctrl Pts',(-97.5309980386227,126.9104585261,508.462296651429));
#269683=CARTESIAN_POINT('Ctrl Pts',(-87.5429283387237,134.586314540048,
506.462296651428));
#269684=CARTESIAN_POINT('Ctrl Pts',(-76.4770599218141,140.605189688823,
504.462296651429));
#269685=CARTESIAN_POINT('Ctrl Pts',(-65.4111915049045,146.624064837598,
502.462296651429));
#269686=CARTESIAN_POINT('Ctrl Pts',(-53.5400027769202,150.837754439537,
500.462296651429));
#269687=CARTESIAN_POINT('Ctrl Pts',(-41.668814048936,155.051444041475,498.462296651429));
#269688=CARTESIAN_POINT('Ctrl Pts',(-29.2846130745767,157.356193074143,
496.462296651429));
#269689=CARTESIAN_POINT('Ctrl Pts',(-16.9004121002175,159.660942106811,
494.462296651429));
#269690=CARTESIAN_POINT('Ctrl Pts',(-4.30813900827852,160.,492.462296651428));
#269691=CARTESIAN_POINT('Ctrl Pts',(8.28413408366043,160.339057893189,490.462296651429));
#269692=CARTESIAN_POINT('Ctrl Pts',(20.7744157382972,158.704075916301,488.462296651429));
#269693=CARTESIAN_POINT('Ctrl Pts',(33.2646973929339,157.069093939413,486.462296651429));
#269694=CARTESIAN_POINT('Ctrl Pts',(45.345435423063,153.500330774912,484.462296651429));
#269695=CARTESIAN_POINT('Ctrl Pts',(57.4261734531921,149.931567610412,482.462296651429));
#269696=CARTESIAN_POINT('Ctrl Pts',(68.7998999948409,144.516898051455,480.462296651428));
#269697=CARTESIAN_POINT('Ctrl Pts',(80.1736265364898,139.102228492498,478.462296651429));
#269698=CARTESIAN_POINT('Ctrl Pts',(90.5602826949688,131.974979673884,476.462296651428));
#269699=CARTESIAN_POINT('Ctrl Pts',(100.946938853448,124.84773085527,474.462296651429));
#269700=CARTESIAN_POINT('Ctrl Pts',(110.0907706828,116.183399296896,472.462296651429));
#269701=CARTESIAN_POINT('Ctrl Pts',(119.234602512151,107.519067738522,470.462296651429));
#269702=CARTESIAN_POINT('Ctrl Pts',(126.9104585261,97.5309980386227,468.462296651429));
#269703=CARTESIAN_POINT('Ctrl Pts',(134.586314540048,87.5429283387237,466.462296651429));
#269704=CARTESIAN_POINT('Ctrl Pts',(140.605189688823,76.4770599218141,464.462296651429));
#269705=CARTESIAN_POINT('Ctrl Pts',(146.624064837598,65.4111915049045,462.462296651429));
#269706=CARTESIAN_POINT('Ctrl Pts',(150.837754439537,53.5400027769202,460.462296651429));
#269707=CARTESIAN_POINT('Ctrl Pts',(155.051444041475,41.668814048936,458.462296651429));
#269708=CARTESIAN_POINT('Ctrl Pts',(157.356193074143,29.2846130745767,456.462296651429));
#269709=CARTESIAN_POINT('Ctrl Pts',(159.660942106811,16.9004121002175,454.462296651429));
#269710=CARTESIAN_POINT('Ctrl Pts',(160.,4.30813900827853,452.462296651429));
#269711=CARTESIAN_POINT('Ctrl Pts',(160.339057893189,-8.28413408366043,
450.462296651429));
#269712=CARTESIAN_POINT('Ctrl Pts',(158.704075916301,-20.7744157382971,
448.462296651429));
#269713=CARTESIAN_POINT('Ctrl Pts',(157.069093939413,-33.2646973929339,
446.462296651429));
#269714=CARTESIAN_POINT('Ctrl Pts',(153.500330774912,-45.345435423063,444.462296651429));
#269715=CARTESIAN_POINT('Ctrl Pts',(149.931567610412,-57.4261734531921,
442.462296651429));
#269716=CARTESIAN_POINT('Ctrl Pts',(144.516898051455,-68.7998999948409,
440.462296651429));
#269717=CARTESIAN_POINT('Ctrl Pts',(139.102228492498,-80.1736265364898,
438.462296651429));
#269718=CARTESIAN_POINT('Ctrl Pts',(131.974979673884,-90.5602826949688,
436.462296651429));
#269719=CARTESIAN_POINT('Ctrl Pts',(124.84773085527,-100.946938853448,434.462296651429));
#269720=CARTESIAN_POINT('Ctrl Pts',(116.183399296896,-110.0907706828,432.462296651429));
#269721=CARTESIAN_POINT('Ctrl Pts',(107.519067738522,-119.234602512151,
430.462296651429));
#269722=CARTESIAN_POINT('Ctrl Pts',(97.5309980386227,-126.9104585261,428.462296651429));
#269723=CARTESIAN_POINT('Ctrl Pts',(87.5429283387236,-134.586314540048,
426.462296651429));
#269724=CARTESIAN_POINT('Ctrl Pts',(76.4770599218141,-140.605189688823,
424.462296651429));
#269725=CARTESIAN_POINT('Ctrl Pts',(65.4111915049046,-146.624064837598,
422.462296651429));
#269726=CARTESIAN_POINT('Ctrl Pts',(53.5400027769202,-150.837754439537,
420.462296651429));
#269727=CARTESIAN_POINT('Ctrl Pts',(41.6688140489359,-155.051444041475,
418.462296651429));
#269728=CARTESIAN_POINT('Ctrl Pts',(29.2846130745768,-157.356193074143,
416.462296651429));
#269729=CARTESIAN_POINT('Ctrl Pts',(16.9004121002176,-159.660942106811,
414.462296651429));
#269730=CARTESIAN_POINT('Ctrl Pts',(4.30813900827854,-160.,412.462296651429));
#269731=CARTESIAN_POINT('Ctrl Pts',(-8.28413408366049,-160.339057893189,
410.462296651429));
#269732=CARTESIAN_POINT('Ctrl Pts',(-20.7744157382971,-158.704075916301,
408.462296651429));
#269733=CARTESIAN_POINT('Ctrl Pts',(-33.2646973929338,-157.069093939413,
406.462296651429));
#269734=CARTESIAN_POINT('Ctrl Pts',(-45.345435423063,-153.500330774912,
404.462296651429));
#269735=CARTESIAN_POINT('Ctrl Pts',(-57.4261734531921,-149.931567610412,
402.462296651429));
#269736=CARTESIAN_POINT('Ctrl Pts',(-68.7998999948409,-144.516898051455,
400.462296651429));
#269737=CARTESIAN_POINT('Ctrl Pts',(-80.1736265364897,-139.102228492498,
398.462296651429));
#269738=CARTESIAN_POINT('Ctrl Pts',(-90.5602826949688,-131.974979673884,
396.462296651429));
#269739=CARTESIAN_POINT('Ctrl Pts',(-100.946938853448,-124.84773085527,
394.462296651429));
#269740=CARTESIAN_POINT('Ctrl Pts',(-110.0907706828,-116.183399296896,392.462296651429));
#269741=CARTESIAN_POINT('Ctrl Pts',(-119.234602512151,-107.519067738522,
390.462296651429));
#269742=CARTESIAN_POINT('Ctrl Pts',(-126.9104585261,-97.5309980386227,388.462296651429));
#269743=CARTESIAN_POINT('Ctrl Pts',(-134.586314540048,-87.5429283387236,
386.462296651429));
#269744=CARTESIAN_POINT('Ctrl Pts',(-140.605189688823,-76.4770599218141,
384.462296651429));
#269745=CARTESIAN_POINT('Ctrl Pts',(-146.624064837598,-65.4111915049046,
382.462296651429));
#269746=CARTESIAN_POINT('Ctrl Pts',(-150.837754439537,-53.5400027769203,
380.462296651429));
#269747=CARTESIAN_POINT('Ctrl Pts',(-155.051444041475,-41.668814048936,
378.462296651429));
#269748=CARTESIAN_POINT('Ctrl Pts',(-157.356193074143,-29.2846130745768,
376.462296651429));
#269749=CARTESIAN_POINT('Ctrl Pts',(-159.660942106811,-16.9004121002176,
374.462296651429));
#269750=CARTESIAN_POINT('Ctrl Pts',(-160.,-4.30813900827851,372.462296651429));
#269751=CARTESIAN_POINT('Ctrl Pts',(160.,4.30813900827813,692.462296651428));
#269752=CARTESIAN_POINT('Ctrl Pts',(160.339057893189,-8.28413408366083,
690.462296651428));
#269753=CARTESIAN_POINT('Ctrl Pts',(158.704075916301,-20.7744157382975,
688.462296651428));
#269754=CARTESIAN_POINT('Ctrl Pts',(157.069093939413,-33.2646973929343,
686.462296651429));
#269755=CARTESIAN_POINT('Ctrl Pts',(153.500330774912,-45.3454354230633,
684.462296651428));
#269756=CARTESIAN_POINT('Ctrl Pts',(149.931567610412,-57.4261734531924,
682.462296651428));
#269757=CARTESIAN_POINT('Ctrl Pts',(144.516898051455,-68.7998999948413,
680.462296651428));
#269758=CARTESIAN_POINT('Ctrl Pts',(139.102228492497,-80.1736265364901,
678.462296651428));
#269759=CARTESIAN_POINT('Ctrl Pts',(131.974979673883,-90.5602826949691,
676.462296651428));
#269760=CARTESIAN_POINT('Ctrl Pts',(124.847730855269,-100.946938853448,
674.462296651428));
#269761=CARTESIAN_POINT('Ctrl Pts',(116.183399296895,-110.0907706828,672.462296651428));
#269762=CARTESIAN_POINT('Ctrl Pts',(107.519067738521,-119.234602512152,
670.462296651428));
#269763=CARTESIAN_POINT('Ctrl Pts',(97.5309980386224,-126.9104585261,668.462296651428));
#269764=CARTESIAN_POINT('Ctrl Pts',(87.5429283387234,-134.586314540048,
666.462296651428));
#269765=CARTESIAN_POINT('Ctrl Pts',(76.4770599218137,-140.605189688823,
664.462296651428));
#269766=CARTESIAN_POINT('Ctrl Pts',(65.4111915049041,-146.624064837599,
662.462296651428));
#269767=CARTESIAN_POINT('Ctrl Pts',(53.5400027769198,-150.837754439537,
660.462296651428));
#269768=CARTESIAN_POINT('Ctrl Pts',(41.6688140489356,-155.051444041475,
658.462296651428));
#269769=CARTESIAN_POINT('Ctrl Pts',(29.2846130745764,-157.356193074143,
656.462296651428));
#269770=CARTESIAN_POINT('Ctrl Pts',(16.9004121002171,-159.660942106811,
654.462296651428));
#269771=CARTESIAN_POINT('Ctrl Pts',(4.30813900827814,-160.,652.462296651428));
#269772=CARTESIAN_POINT('Ctrl Pts',(-8.28413408366082,-160.339057893189,
650.462296651428));
#269773=CARTESIAN_POINT('Ctrl Pts',(-20.7744157382975,-158.704075916301,
648.462296651428));
#269774=CARTESIAN_POINT('Ctrl Pts',(-33.2646973929342,-157.069093939413,
646.462296651428));
#269775=CARTESIAN_POINT('Ctrl Pts',(-45.3454354230633,-153.500330774912,
644.462296651428));
#269776=CARTESIAN_POINT('Ctrl Pts',(-57.4261734531924,-149.931567610412,
642.462296651428));
#269777=CARTESIAN_POINT('Ctrl Pts',(-68.7998999948413,-144.516898051455,
640.462296651428));
#269778=CARTESIAN_POINT('Ctrl Pts',(-80.1736265364901,-139.102228492497,
638.462296651428));
#269779=CARTESIAN_POINT('Ctrl Pts',(-90.5602826949691,-131.974979673883,
636.462296651428));
#269780=CARTESIAN_POINT('Ctrl Pts',(-100.946938853448,-124.847730855269,
634.462296651428));
#269781=CARTESIAN_POINT('Ctrl Pts',(-110.0907706828,-116.183399296895,632.462296651428));
#269782=CARTESIAN_POINT('Ctrl Pts',(-119.234602512152,-107.519067738521,
630.462296651428));
#269783=CARTESIAN_POINT('Ctrl Pts',(-126.9104585261,-97.5309980386224,628.462296651428));
#269784=CARTESIAN_POINT('Ctrl Pts',(-134.586314540048,-87.5429283387234,
626.462296651429));
#269785=CARTESIAN_POINT('Ctrl Pts',(-140.605189688823,-76.4770599218137,
624.462296651428));
#269786=CARTESIAN_POINT('Ctrl Pts',(-146.624064837599,-65.4111915049041,
622.462296651428));
#269787=CARTESIAN_POINT('Ctrl Pts',(-150.837754439537,-53.5400027769199,
620.462296651428));
#269788=CARTESIAN_POINT('Ctrl Pts',(-155.051444041475,-41.6688140489356,
618.462296651428));
#269789=CARTESIAN_POINT('Ctrl Pts',(-157.356193074143,-29.2846130745764,
616.462296651428));
#269790=CARTESIAN_POINT('Ctrl Pts',(-159.660942106811,-16.9004121002171,
614.462296651429));
#269791=CARTESIAN_POINT('Ctrl Pts',(-160.,-4.30813900827815,612.462296651428));
#269792=CARTESIAN_POINT('Ctrl Pts',(-160.339057893189,8.28413408366081,
610.462296651428));
#269793=CARTESIAN_POINT('Ctrl Pts',(-158.704075916301,20.7744157382975,
608.462296651428));
#269794=CARTESIAN_POINT('Ctrl Pts',(-157.069093939413,33.2646973929342,
606.462296651428));
#269795=CARTESIAN_POINT('Ctrl Pts',(-153.500330774912,45.3454354230633,
604.462296651428));
#269796=CARTESIAN_POINT('Ctrl Pts',(-149.931567610412,57.4261734531924,
602.462296651429));
#269797=CARTESIAN_POINT('Ctrl Pts',(-144.516898051455,68.7998999948413,
600.462296651428));
#269798=CARTESIAN_POINT('Ctrl Pts',(-139.102228492497,80.1736265364901,
598.462296651428));
#269799=CARTESIAN_POINT('Ctrl Pts',(-131.974979673883,90.5602826949691,
596.462296651428));
#269800=CARTESIAN_POINT('Ctrl Pts',(-124.847730855269,100.946938853448,
594.462296651428));
#269801=CARTESIAN_POINT('Ctrl Pts',(-116.183399296895,110.0907706828,592.462296651428));
#269802=CARTESIAN_POINT('Ctrl Pts',(-107.519067738521,119.234602512152,
590.462296651428));
#269803=CARTESIAN_POINT('Ctrl Pts',(-97.5309980386224,126.9104585261,588.462296651428));
#269804=CARTESIAN_POINT('Ctrl Pts',(-87.5429283387233,134.586314540048,
586.462296651428));
#269805=CARTESIAN_POINT('Ctrl Pts',(-76.4770599218137,140.605189688823,
584.462296651428));
#269806=CARTESIAN_POINT('Ctrl Pts',(-65.4111915049042,146.624064837599,
582.462296651428));
#269807=CARTESIAN_POINT('Ctrl Pts',(-53.5400027769199,150.837754439537,
580.462296651428));
#269808=CARTESIAN_POINT('Ctrl Pts',(-41.6688140489356,155.051444041475,
578.462296651428));
#269809=CARTESIAN_POINT('Ctrl Pts',(-29.2846130745764,157.356193074143,
576.462296651428));
#269810=CARTESIAN_POINT('Ctrl Pts',(-16.9004121002172,159.660942106811,
574.462296651428));
#269811=CARTESIAN_POINT('Ctrl Pts',(-4.30813900827816,160.,572.462296651428));
#269812=CARTESIAN_POINT('Ctrl Pts',(8.28413408366087,160.339057893189,570.462296651428));
#269813=CARTESIAN_POINT('Ctrl Pts',(20.7744157382975,158.704075916301,568.462296651428));
#269814=CARTESIAN_POINT('Ctrl Pts',(33.2646973929342,157.069093939413,566.462296651428));
#269815=CARTESIAN_POINT('Ctrl Pts',(45.3454354230633,153.500330774912,564.462296651428));
#269816=CARTESIAN_POINT('Ctrl Pts',(57.4261734531925,149.931567610412,562.462296651428));
#269817=CARTESIAN_POINT('Ctrl Pts',(68.7998999948413,144.516898051455,560.462296651428));
#269818=CARTESIAN_POINT('Ctrl Pts',(80.1736265364901,139.102228492498,558.462296651428));
#269819=CARTESIAN_POINT('Ctrl Pts',(90.560282694969,131.974979673883,556.462296651428));
#269820=CARTESIAN_POINT('Ctrl Pts',(100.946938853448,124.847730855269,554.462296651428));
#269821=CARTESIAN_POINT('Ctrl Pts',(110.0907706828,116.183399296895,552.462296651428));
#269822=CARTESIAN_POINT('Ctrl Pts',(119.234602512152,107.519067738521,550.462296651428));
#269823=CARTESIAN_POINT('Ctrl Pts',(126.9104585261,97.5309980386224,548.462296651428));
#269824=CARTESIAN_POINT('Ctrl Pts',(134.586314540048,87.5429283387233,546.462296651428));
#269825=CARTESIAN_POINT('Ctrl Pts',(140.605189688823,76.4770599218137,544.462296651428));
#269826=CARTESIAN_POINT('Ctrl Pts',(146.624064837599,65.4111915049042,542.462296651428));
#269827=CARTESIAN_POINT('Ctrl Pts',(150.837754439537,53.5400027769199,540.462296651428));
#269828=CARTESIAN_POINT('Ctrl Pts',(155.051444041475,41.6688140489356,538.462296651428));
#269829=CARTESIAN_POINT('Ctrl Pts',(157.356193074143,29.2846130745764,536.462296651428));
#269830=CARTESIAN_POINT('Ctrl Pts',(159.660942106811,16.9004121002172,534.462296651428));
#269831=CARTESIAN_POINT('Ctrl Pts',(160.,4.30813900827813,532.462296651428));
#269832=CARTESIAN_POINT('Ctrl Pts',(160.,-4.30813900827805,697.537703348572));
#269833=CARTESIAN_POINT('Ctrl Pts',(159.660942106811,-16.900412100217,695.537703348572));
#269834=CARTESIAN_POINT('Ctrl Pts',(157.356193074143,-29.2846130745763,
693.537703348572));
#269835=CARTESIAN_POINT('Ctrl Pts',(155.051444041475,-41.6688140489355,
691.537703348572));
#269836=CARTESIAN_POINT('Ctrl Pts',(150.837754439537,-53.5400027769198,
689.537703348572));
#269837=CARTESIAN_POINT('Ctrl Pts',(146.624064837599,-65.411191504904,687.537703348572));
#269838=CARTESIAN_POINT('Ctrl Pts',(140.605189688823,-76.4770599218136,
685.537703348572));
#269839=CARTESIAN_POINT('Ctrl Pts',(134.586314540048,-87.5429283387233,
683.537703348572));
#269840=CARTESIAN_POINT('Ctrl Pts',(126.9104585261,-97.5309980386223,681.537703348572));
#269841=CARTESIAN_POINT('Ctrl Pts',(119.234602512152,-107.519067738521,
679.537703348572));
#269842=CARTESIAN_POINT('Ctrl Pts',(110.0907706828,-116.183399296895,677.537703348572));
#269843=CARTESIAN_POINT('Ctrl Pts',(100.946938853448,-124.847730855269,
675.537703348572));
#269844=CARTESIAN_POINT('Ctrl Pts',(90.5602826949691,-131.974979673883,
673.537703348572));
#269845=CARTESIAN_POINT('Ctrl Pts',(80.1736265364902,-139.102228492497,
671.537703348572));
#269846=CARTESIAN_POINT('Ctrl Pts',(68.7998999948414,-144.516898051454,
669.537703348572));
#269847=CARTESIAN_POINT('Ctrl Pts',(57.4261734531925,-149.931567610412,
667.537703348572));
#269848=CARTESIAN_POINT('Ctrl Pts',(45.3454354230634,-153.500330774912,
665.537703348572));
#269849=CARTESIAN_POINT('Ctrl Pts',(33.2646973929343,-157.069093939413,
663.537703348572));
#269850=CARTESIAN_POINT('Ctrl Pts',(20.7744157382976,-158.704075916301,
661.537703348572));
#269851=CARTESIAN_POINT('Ctrl Pts',(8.28413408366091,-160.339057893189,
659.537703348572));
#269852=CARTESIAN_POINT('Ctrl Pts',(-4.30813900827804,-160.,657.537703348572));
#269853=CARTESIAN_POINT('Ctrl Pts',(-16.900412100217,-159.660942106811,
655.537703348572));
#269854=CARTESIAN_POINT('Ctrl Pts',(-29.2846130745763,-157.356193074143,
653.537703348572));
#269855=CARTESIAN_POINT('Ctrl Pts',(-41.6688140489355,-155.051444041475,
651.537703348572));
#269856=CARTESIAN_POINT('Ctrl Pts',(-53.5400027769198,-150.837754439537,
649.537703348572));
#269857=CARTESIAN_POINT('Ctrl Pts',(-65.411191504904,-146.624064837599,
647.537703348572));
#269858=CARTESIAN_POINT('Ctrl Pts',(-76.4770599218136,-140.605189688823,
645.537703348572));
#269859=CARTESIAN_POINT('Ctrl Pts',(-87.5429283387233,-134.586314540048,
643.537703348572));
#269860=CARTESIAN_POINT('Ctrl Pts',(-97.5309980386223,-126.9104585261,641.537703348572));
#269861=CARTESIAN_POINT('Ctrl Pts',(-107.519067738521,-119.234602512152,
639.537703348572));
#269862=CARTESIAN_POINT('Ctrl Pts',(-116.183399296895,-110.0907706828,637.537703348572));
#269863=CARTESIAN_POINT('Ctrl Pts',(-124.847730855269,-100.946938853448,
635.537703348572));
#269864=CARTESIAN_POINT('Ctrl Pts',(-131.974979673883,-90.5602826949692,
633.537703348572));
#269865=CARTESIAN_POINT('Ctrl Pts',(-139.102228492497,-80.1736265364902,
631.537703348572));
#269866=CARTESIAN_POINT('Ctrl Pts',(-144.516898051454,-68.7998999948414,
629.537703348572));
#269867=CARTESIAN_POINT('Ctrl Pts',(-149.931567610412,-57.4261734531925,
627.537703348572));
#269868=CARTESIAN_POINT('Ctrl Pts',(-153.500330774912,-45.3454354230634,
625.537703348572));
#269869=CARTESIAN_POINT('Ctrl Pts',(-157.069093939413,-33.2646973929344,
623.537703348572));
#269870=CARTESIAN_POINT('Ctrl Pts',(-158.704075916301,-20.7744157382976,
621.537703348572));
#269871=CARTESIAN_POINT('Ctrl Pts',(-160.339057893189,-8.28413408366092,
619.537703348572));
#269872=CARTESIAN_POINT('Ctrl Pts',(-160.,4.30813900827803,617.537703348572));
#269873=CARTESIAN_POINT('Ctrl Pts',(-159.660942106811,16.900412100217,615.537703348572));
#269874=CARTESIAN_POINT('Ctrl Pts',(-157.356193074143,29.2846130745763,
613.537703348572));
#269875=CARTESIAN_POINT('Ctrl Pts',(-155.051444041475,41.6688140489355,
611.537703348572));
#269876=CARTESIAN_POINT('Ctrl Pts',(-150.837754439537,53.5400027769198,
609.537703348572));
#269877=CARTESIAN_POINT('Ctrl Pts',(-146.624064837599,65.411191504904,607.537703348572));
#269878=CARTESIAN_POINT('Ctrl Pts',(-140.605189688823,76.4770599218136,
605.537703348572));
#269879=CARTESIAN_POINT('Ctrl Pts',(-134.586314540048,87.5429283387233,
603.537703348572));
#269880=CARTESIAN_POINT('Ctrl Pts',(-126.9104585261,97.5309980386223,601.537703348572));
#269881=CARTESIAN_POINT('Ctrl Pts',(-119.234602512152,107.519067738521,
599.537703348572));
#269882=CARTESIAN_POINT('Ctrl Pts',(-110.0907706828,116.183399296895,597.537703348572));
#269883=CARTESIAN_POINT('Ctrl Pts',(-100.946938853448,124.847730855269,
595.537703348572));
#269884=CARTESIAN_POINT('Ctrl Pts',(-90.5602826949692,131.974979673883,
593.537703348572));
#269885=CARTESIAN_POINT('Ctrl Pts',(-80.1736265364901,139.102228492497,
591.537703348572));
#269886=CARTESIAN_POINT('Ctrl Pts',(-68.7998999948414,144.516898051454,
589.537703348572));
#269887=CARTESIAN_POINT('Ctrl Pts',(-57.4261734531926,149.931567610412,
587.537703348572));
#269888=CARTESIAN_POINT('Ctrl Pts',(-45.3454354230634,153.500330774912,
585.537703348572));
#269889=CARTESIAN_POINT('Ctrl Pts',(-33.2646973929343,157.069093939413,
583.537703348572));
#269890=CARTESIAN_POINT('Ctrl Pts',(-20.7744157382976,158.704075916301,
581.537703348572));
#269891=CARTESIAN_POINT('Ctrl Pts',(-8.284134083661,160.339057893189,579.537703348572));
#269892=CARTESIAN_POINT('Ctrl Pts',(4.30813900827803,160.,577.537703348572));
#269893=CARTESIAN_POINT('Ctrl Pts',(16.9004121002171,159.660942106811,575.537703348572));
#269894=CARTESIAN_POINT('Ctrl Pts',(29.2846130745762,157.356193074143,573.537703348572));
#269895=CARTESIAN_POINT('Ctrl Pts',(41.6688140489354,155.051444041476,571.537703348572));
#269896=CARTESIAN_POINT('Ctrl Pts',(53.5400027769198,150.837754439537,569.537703348572));
#269897=CARTESIAN_POINT('Ctrl Pts',(65.4111915049041,146.624064837599,567.537703348572));
#269898=CARTESIAN_POINT('Ctrl Pts',(76.4770599218136,140.605189688823,565.537703348572));
#269899=CARTESIAN_POINT('Ctrl Pts',(87.5429283387232,134.586314540048,563.537703348572));
#269900=CARTESIAN_POINT('Ctrl Pts',(97.5309980386223,126.9104585261,561.537703348572));
#269901=CARTESIAN_POINT('Ctrl Pts',(107.519067738521,119.234602512152,559.537703348572));
#269902=CARTESIAN_POINT('Ctrl Pts',(116.183399296895,110.0907706828,557.537703348572));
#269903=CARTESIAN_POINT('Ctrl Pts',(124.847730855269,100.946938853448,555.537703348572));
#269904=CARTESIAN_POINT('Ctrl Pts',(131.974979673883,90.5602826949692,553.537703348572));
#269905=CARTESIAN_POINT('Ctrl Pts',(139.102228492497,80.1736265364902,551.537703348572));
#269906=CARTESIAN_POINT('Ctrl Pts',(144.516898051454,68.7998999948414,549.537703348572));
#269907=CARTESIAN_POINT('Ctrl Pts',(149.931567610412,57.4261734531926,547.537703348572));
#269908=CARTESIAN_POINT('Ctrl Pts',(153.500330774912,45.3454354230634,545.537703348572));
#269909=CARTESIAN_POINT('Ctrl Pts',(157.069093939413,33.2646973929343,543.537703348572));
#269910=CARTESIAN_POINT('Ctrl Pts',(158.704075916301,20.7744157382976,541.537703348572));
#269911=CARTESIAN_POINT('Ctrl Pts',(160.339057893189,8.28413408366101,539.537703348572));
#269912=CARTESIAN_POINT('Ctrl Pts',(160.,-4.30813900827805,537.537703348572));
#269913=CARTESIAN_POINT('Ctrl Pts',(159.937609420477,-6.20654127333164,
690.789436448355));
#269914=CARTESIAN_POINT('Ctrl Pts',(159.653854600275,-13.5186762622038,
689.624118246284));
#269915=CARTESIAN_POINT('Ctrl Pts',(158.704075916301,-20.7744157382975,
688.462296651428));
#269916=CARTESIAN_POINT('Ctrl Pts',(157.069093939413,-33.2646973929343,
686.462296651429));
#269917=CARTESIAN_POINT('Ctrl Pts',(153.500330774912,-45.3454354230633,
684.462296651428));
#269918=CARTESIAN_POINT('Ctrl Pts',(149.931567610412,-57.4261734531925,
682.462296651428));
#269919=CARTESIAN_POINT('Ctrl Pts',(144.516898051455,-68.7998999948413,
680.462296651428));
#269920=CARTESIAN_POINT('Ctrl Pts',(139.102228492497,-80.1736265364901,
678.462296651428));
#269921=CARTESIAN_POINT('Ctrl Pts',(131.974979673883,-90.5602826949691,
676.462296651428));
#269922=CARTESIAN_POINT('Ctrl Pts',(124.847730855269,-100.946938853448,
674.462296651428));
#269923=CARTESIAN_POINT('Ctrl Pts',(116.183399296895,-110.0907706828,672.462296651428));
#269924=CARTESIAN_POINT('Ctrl Pts',(107.519067738521,-119.234602512152,
670.462296651428));
#269925=CARTESIAN_POINT('Ctrl Pts',(97.5309980386224,-126.9104585261,668.462296651428));
#269926=CARTESIAN_POINT('Ctrl Pts',(87.5429283387234,-134.586314540048,
666.462296651428));
#269927=CARTESIAN_POINT('Ctrl Pts',(76.4770599218137,-140.605189688823,
664.462296651428));
#269928=CARTESIAN_POINT('Ctrl Pts',(65.4111915049041,-146.624064837599,
662.462296651428));
#269929=CARTESIAN_POINT('Ctrl Pts',(53.5400027769198,-150.837754439537,
660.462296651428));
#269930=CARTESIAN_POINT('Ctrl Pts',(41.6688140489356,-155.051444041475,
658.462296651428));
#269931=CARTESIAN_POINT('Ctrl Pts',(29.2846130745764,-157.356193074143,
656.462296651428));
#269932=CARTESIAN_POINT('Ctrl Pts',(16.9004121002171,-159.660942106811,
654.462296651428));
#269933=CARTESIAN_POINT('Ctrl Pts',(4.30813900827814,-160.,652.462296651428));
#269934=CARTESIAN_POINT('Ctrl Pts',(-8.28413408366082,-160.339057893189,
650.462296651428));
#269935=CARTESIAN_POINT('Ctrl Pts',(-20.7744157382975,-158.704075916301,
648.462296651428));
#269936=CARTESIAN_POINT('Ctrl Pts',(-33.2646973929342,-157.069093939413,
646.462296651428));
#269937=CARTESIAN_POINT('Ctrl Pts',(-45.3454354230633,-153.500330774912,
644.462296651428));
#269938=CARTESIAN_POINT('Ctrl Pts',(-57.4261734531924,-149.931567610412,
642.462296651428));
#269939=CARTESIAN_POINT('Ctrl Pts',(-68.7998999948413,-144.516898051455,
640.462296651428));
#269940=CARTESIAN_POINT('Ctrl Pts',(-80.1736265364901,-139.102228492497,
638.462296651428));
#269941=CARTESIAN_POINT('Ctrl Pts',(-90.5602826949691,-131.974979673883,
636.462296651428));
#269942=CARTESIAN_POINT('Ctrl Pts',(-100.946938853448,-124.847730855269,
634.462296651428));
#269943=CARTESIAN_POINT('Ctrl Pts',(-110.0907706828,-116.183399296895,632.462296651428));
#269944=CARTESIAN_POINT('Ctrl Pts',(-119.234602512152,-107.519067738521,
630.462296651428));
#269945=CARTESIAN_POINT('Ctrl Pts',(-126.9104585261,-97.5309980386224,628.462296651428));
#269946=CARTESIAN_POINT('Ctrl Pts',(-134.586314540048,-87.5429283387234,
626.462296651428));
#269947=CARTESIAN_POINT('Ctrl Pts',(-140.605189688823,-76.4770599218137,
624.462296651428));
#269948=CARTESIAN_POINT('Ctrl Pts',(-146.624064837599,-65.4111915049041,
622.462296651428));
#269949=CARTESIAN_POINT('Ctrl Pts',(-150.837754439537,-53.5400027769199,
620.462296651428));
#269950=CARTESIAN_POINT('Ctrl Pts',(-155.051444041475,-41.6688140489356,
618.462296651428));
#269951=CARTESIAN_POINT('Ctrl Pts',(-157.356193074143,-29.2846130745764,
616.462296651428));
#269952=CARTESIAN_POINT('Ctrl Pts',(-159.660942106811,-16.9004121002171,
614.462296651428));
#269953=CARTESIAN_POINT('Ctrl Pts',(-160.,-4.30813900827815,612.462296651428));
#269954=CARTESIAN_POINT('Ctrl Pts',(-160.339057893189,8.28413408366081,
610.462296651428));
#269955=CARTESIAN_POINT('Ctrl Pts',(-158.704075916301,20.7744157382975,
608.462296651428));
#269956=CARTESIAN_POINT('Ctrl Pts',(-157.069093939413,33.2646973929342,
606.462296651428));
#269957=CARTESIAN_POINT('Ctrl Pts',(-153.500330774912,45.3454354230633,
604.462296651428));
#269958=CARTESIAN_POINT('Ctrl Pts',(-149.931567610412,57.4261734531924,
602.462296651428));
#269959=CARTESIAN_POINT('Ctrl Pts',(-144.516898051455,68.7998999948413,
600.462296651428));
#269960=CARTESIAN_POINT('Ctrl Pts',(-139.102228492497,80.1736265364901,
598.462296651428));
#269961=CARTESIAN_POINT('Ctrl Pts',(-131.974979673883,90.5602826949691,
596.462296651428));
#269962=CARTESIAN_POINT('Ctrl Pts',(-124.847730855269,100.946938853448,
594.462296651428));
#269963=CARTESIAN_POINT('Ctrl Pts',(-116.183399296895,110.0907706828,592.462296651428));
#269964=CARTESIAN_POINT('Ctrl Pts',(-107.519067738521,119.234602512152,
590.462296651428));
#269965=CARTESIAN_POINT('Ctrl Pts',(-97.5309980386224,126.9104585261,588.462296651428));
#269966=CARTESIAN_POINT('Ctrl Pts',(-87.5429283387233,134.586314540048,
586.462296651428));
#269967=CARTESIAN_POINT('Ctrl Pts',(-76.4770599218137,140.605189688823,
584.462296651428));
#269968=CARTESIAN_POINT('Ctrl Pts',(-65.4111915049042,146.624064837599,
582.462296651428));
#269969=CARTESIAN_POINT('Ctrl Pts',(-53.5400027769199,150.837754439537,
580.462296651428));
#269970=CARTESIAN_POINT('Ctrl Pts',(-41.6688140489356,155.051444041475,
578.462296651428));
#269971=CARTESIAN_POINT('Ctrl Pts',(-29.2846130745764,157.356193074143,
576.462296651428));
#269972=CARTESIAN_POINT('Ctrl Pts',(-16.9004121002172,159.660942106811,
574.462296651428));
#269973=CARTESIAN_POINT('Ctrl Pts',(-4.30813900827816,160.,572.462296651428));
#269974=CARTESIAN_POINT('Ctrl Pts',(8.28413408366087,160.339057893189,570.462296651428));
#269975=CARTESIAN_POINT('Ctrl Pts',(20.7744157382975,158.704075916301,568.462296651428));
#269976=CARTESIAN_POINT('Ctrl Pts',(33.2646973929342,157.069093939413,566.462296651428));
#269977=CARTESIAN_POINT('Ctrl Pts',(45.3454354230633,153.500330774912,564.462296651428));
#269978=CARTESIAN_POINT('Ctrl Pts',(57.4261734531925,149.931567610412,562.462296651428));
#269979=CARTESIAN_POINT('Ctrl Pts',(68.7998999948413,144.516898051455,560.462296651428));
#269980=CARTESIAN_POINT('Ctrl Pts',(80.1736265364901,139.102228492498,558.462296651428));
#269981=CARTESIAN_POINT('Ctrl Pts',(90.560282694969,131.974979673883,556.462296651428));
#269982=CARTESIAN_POINT('Ctrl Pts',(100.946938853448,124.847730855269,554.462296651428));
#269983=CARTESIAN_POINT('Ctrl Pts',(110.0907706828,116.183399296895,552.462296651428));
#269984=CARTESIAN_POINT('Ctrl Pts',(119.234602512152,107.519067738521,550.462296651428));
#269985=CARTESIAN_POINT('Ctrl Pts',(126.9104585261,97.5309980386224,548.462296651428));
#269986=CARTESIAN_POINT('Ctrl Pts',(134.586314540048,87.5429283387233,546.462296651428));
#269987=CARTESIAN_POINT('Ctrl Pts',(140.605189688823,76.4770599218137,544.462296651428));
#269988=CARTESIAN_POINT('Ctrl Pts',(146.624064837599,65.4111915049042,542.462296651428));
#269989=CARTESIAN_POINT('Ctrl Pts',(150.837754439537,53.5400027769199,540.462296651428));
#269990=CARTESIAN_POINT('Ctrl Pts',(155.051444041475,41.6688140489356,538.462296651428));
#269991=CARTESIAN_POINT('Ctrl Pts',(157.356193074143,29.2846130745764,536.462296651428));
#269992=CARTESIAN_POINT('Ctrl Pts',(159.394142202012,18.3340187941081,534.693818523022));
#269993=CARTESIAN_POINT('Ctrl Pts',(159.895664541343,7.20669984090287,532.923108716584));
#269994=CARTESIAN_POINT('Ctrl Pts',(159.895664541343,-7.20669984090406,
697.076891283416));
#269995=CARTESIAN_POINT('Ctrl Pts',(159.394142202012,-18.3340187941086,
695.306181476978));
#269996=CARTESIAN_POINT('Ctrl Pts',(157.356193074143,-29.2846130745763,
693.537703348572));
#269997=CARTESIAN_POINT('Ctrl Pts',(155.051444041475,-41.6688140489355,
691.537703348572));
#269998=CARTESIAN_POINT('Ctrl Pts',(150.837754439537,-53.5400027769198,
689.537703348572));
#269999=CARTESIAN_POINT('Ctrl Pts',(146.624064837599,-65.411191504904,687.537703348572));
#270000=CARTESIAN_POINT('Ctrl Pts',(140.605189688823,-76.4770599218136,
685.537703348572));
#270001=CARTESIAN_POINT('Ctrl Pts',(134.586314540048,-87.5429283387233,
683.537703348572));
#270002=CARTESIAN_POINT('Ctrl Pts',(126.9104585261,-97.5309980386223,681.537703348572));
#270003=CARTESIAN_POINT('Ctrl Pts',(119.234602512152,-107.519067738521,
679.537703348572));
#270004=CARTESIAN_POINT('Ctrl Pts',(110.0907706828,-116.183399296895,677.537703348572));
#270005=CARTESIAN_POINT('Ctrl Pts',(100.946938853448,-124.847730855269,
675.537703348572));
#270006=CARTESIAN_POINT('Ctrl Pts',(90.5602826949691,-131.974979673883,
673.537703348572));
#270007=CARTESIAN_POINT('Ctrl Pts',(80.1736265364902,-139.102228492497,
671.537703348572));
#270008=CARTESIAN_POINT('Ctrl Pts',(68.7998999948414,-144.516898051454,
669.537703348572));
#270009=CARTESIAN_POINT('Ctrl Pts',(57.4261734531925,-149.931567610412,
667.537703348572));
#270010=CARTESIAN_POINT('Ctrl Pts',(45.3454354230634,-153.500330774912,
665.537703348572));
#270011=CARTESIAN_POINT('Ctrl Pts',(33.2646973929343,-157.069093939413,
663.537703348572));
#270012=CARTESIAN_POINT('Ctrl Pts',(20.7744157382976,-158.704075916301,
661.537703348572));
#270013=CARTESIAN_POINT('Ctrl Pts',(8.28413408366091,-160.339057893189,
659.537703348572));
#270014=CARTESIAN_POINT('Ctrl Pts',(-4.30813900827804,-160.,657.537703348572));
#270015=CARTESIAN_POINT('Ctrl Pts',(-16.900412100217,-159.660942106811,
655.537703348572));
#270016=CARTESIAN_POINT('Ctrl Pts',(-29.2846130745763,-157.356193074143,
653.537703348572));
#270017=CARTESIAN_POINT('Ctrl Pts',(-41.6688140489355,-155.051444041475,
651.537703348572));
#270018=CARTESIAN_POINT('Ctrl Pts',(-53.5400027769198,-150.837754439537,
649.537703348572));
#270019=CARTESIAN_POINT('Ctrl Pts',(-65.411191504904,-146.624064837599,
647.537703348572));
#270020=CARTESIAN_POINT('Ctrl Pts',(-76.4770599218136,-140.605189688823,
645.537703348572));
#270021=CARTESIAN_POINT('Ctrl Pts',(-87.5429283387233,-134.586314540048,
643.537703348572));
#270022=CARTESIAN_POINT('Ctrl Pts',(-97.5309980386223,-126.9104585261,641.537703348572));
#270023=CARTESIAN_POINT('Ctrl Pts',(-107.519067738521,-119.234602512152,
639.537703348572));
#270024=CARTESIAN_POINT('Ctrl Pts',(-116.183399296895,-110.0907706828,637.537703348572));
#270025=CARTESIAN_POINT('Ctrl Pts',(-124.847730855269,-100.946938853448,
635.537703348572));
#270026=CARTESIAN_POINT('Ctrl Pts',(-131.974979673883,-90.5602826949692,
633.537703348572));
#270027=CARTESIAN_POINT('Ctrl Pts',(-139.102228492497,-80.1736265364902,
631.537703348572));
#270028=CARTESIAN_POINT('Ctrl Pts',(-144.516898051454,-68.7998999948414,
629.537703348572));
#270029=CARTESIAN_POINT('Ctrl Pts',(-149.931567610412,-57.4261734531925,
627.537703348572));
#270030=CARTESIAN_POINT('Ctrl Pts',(-153.500330774912,-45.3454354230634,
625.537703348572));
#270031=CARTESIAN_POINT('Ctrl Pts',(-157.069093939413,-33.2646973929344,
623.537703348572));
#270032=CARTESIAN_POINT('Ctrl Pts',(-158.704075916301,-20.7744157382976,
621.537703348572));
#270033=CARTESIAN_POINT('Ctrl Pts',(-160.339057893189,-8.28413408366092,
619.537703348572));
#270034=CARTESIAN_POINT('Ctrl Pts',(-160.,4.30813900827803,617.537703348572));
#270035=CARTESIAN_POINT('Ctrl Pts',(-159.660942106811,16.900412100217,615.537703348572));
#270036=CARTESIAN_POINT('Ctrl Pts',(-157.356193074143,29.2846130745763,
613.537703348572));
#270037=CARTESIAN_POINT('Ctrl Pts',(-155.051444041475,41.6688140489355,
611.537703348572));
#270038=CARTESIAN_POINT('Ctrl Pts',(-150.837754439537,53.5400027769198,
609.537703348572));
#270039=CARTESIAN_POINT('Ctrl Pts',(-146.624064837599,65.411191504904,607.537703348572));
#270040=CARTESIAN_POINT('Ctrl Pts',(-140.605189688823,76.4770599218136,
605.537703348572));
#270041=CARTESIAN_POINT('Ctrl Pts',(-134.586314540048,87.5429283387233,
603.537703348572));
#270042=CARTESIAN_POINT('Ctrl Pts',(-126.9104585261,97.5309980386223,601.537703348572));
#270043=CARTESIAN_POINT('Ctrl Pts',(-119.234602512152,107.519067738521,
599.537703348572));
#270044=CARTESIAN_POINT('Ctrl Pts',(-110.0907706828,116.183399296895,597.537703348572));
#270045=CARTESIAN_POINT('Ctrl Pts',(-100.946938853448,124.847730855269,
595.537703348572));
#270046=CARTESIAN_POINT('Ctrl Pts',(-90.5602826949692,131.974979673883,
593.537703348572));
#270047=CARTESIAN_POINT('Ctrl Pts',(-80.1736265364902,139.102228492497,
591.537703348572));
#270048=CARTESIAN_POINT('Ctrl Pts',(-68.7998999948414,144.516898051454,
589.537703348572));
#270049=CARTESIAN_POINT('Ctrl Pts',(-57.4261734531926,149.931567610412,
587.537703348572));
#270050=CARTESIAN_POINT('Ctrl Pts',(-45.3454354230634,153.500330774912,
585.537703348572));
#270051=CARTESIAN_POINT('Ctrl Pts',(-33.2646973929343,157.069093939413,
583.537703348572));
#270052=CARTESIAN_POINT('Ctrl Pts',(-20.7744157382976,158.704075916301,
581.537703348572));
#270053=CARTESIAN_POINT('Ctrl Pts',(-8.284134083661,160.339057893189,579.537703348572));
#270054=CARTESIAN_POINT('Ctrl Pts',(4.30813900827803,160.,577.537703348572));
#270055=CARTESIAN_POINT('Ctrl Pts',(16.9004121002171,159.660942106811,575.537703348572));
#270056=CARTESIAN_POINT('Ctrl Pts',(29.2846130745762,157.356193074143,573.537703348572));
#270057=CARTESIAN_POINT('Ctrl Pts',(41.6688140489354,155.051444041476,571.537703348572));
#270058=CARTESIAN_POINT('Ctrl Pts',(53.5400027769198,150.837754439537,569.537703348572));
#270059=CARTESIAN_POINT('Ctrl Pts',(65.4111915049041,146.624064837599,567.537703348572));
#270060=CARTESIAN_POINT('Ctrl Pts',(76.4770599218136,140.605189688823,565.537703348572));
#270061=CARTESIAN_POINT('Ctrl Pts',(87.5429283387232,134.586314540048,563.537703348572));
#270062=CARTESIAN_POINT('Ctrl Pts',(97.5309980386223,126.9104585261,561.537703348572));
#270063=CARTESIAN_POINT('Ctrl Pts',(107.519067738521,119.234602512152,559.537703348572));
#270064=CARTESIAN_POINT('Ctrl Pts',(116.183399296895,110.0907706828,557.537703348572));
#270065=CARTESIAN_POINT('Ctrl Pts',(124.847730855269,100.946938853448,555.537703348572));
#270066=CARTESIAN_POINT('Ctrl Pts',(131.974979673883,90.5602826949692,553.537703348572));
#270067=CARTESIAN_POINT('Ctrl Pts',(139.102228492497,80.1736265364902,551.537703348572));
#270068=CARTESIAN_POINT('Ctrl Pts',(144.516898051454,68.7998999948414,549.537703348572));
#270069=CARTESIAN_POINT('Ctrl Pts',(149.931567610412,57.4261734531926,547.537703348572));
#270070=CARTESIAN_POINT('Ctrl Pts',(153.500330774912,45.3454354230634,545.537703348572));
#270071=CARTESIAN_POINT('Ctrl Pts',(157.069093939413,33.2646973929343,543.537703348572));
#270072=CARTESIAN_POINT('Ctrl Pts',(158.704075916301,20.7744157382976,541.537703348572));
#270073=CARTESIAN_POINT('Ctrl Pts',(159.653854600275,13.5186762622035,540.375881753716));
#270074=CARTESIAN_POINT('Ctrl Pts',(159.937609420477,6.20654127333082,539.210563551645));
#270075=CARTESIAN_POINT('Ctrl Pts',(130.,4.30813900827812,692.462296651428));
#270076=CARTESIAN_POINT('Ctrl Pts',(130.339057893189,-5.92308287892228,
690.462296651428));
#270077=CARTESIAN_POINT('Ctrl Pts',(129.073425698447,-16.0813817870906,
688.462296651428));
#270078=CARTESIAN_POINT('Ctrl Pts',(127.807793503704,-26.2396806952589,
686.462296651429));
#270079=CARTESIAN_POINT('Ctrl Pts',(124.968635286058,-36.0749255918149,
684.462296651428));
#270080=CARTESIAN_POINT('Ctrl Pts',(122.129477068411,-45.9101704883709,
682.462296651428));
#270081=CARTESIAN_POINT('Ctrl Pts',(117.786702325803,-55.1801850026549,
680.462296651428));
#270082=CARTESIAN_POINT('Ctrl Pts',(113.443927583196,-64.4501995169389,
678.462296651428));
#270083=CARTESIAN_POINT('Ctrl Pts',(107.704469842635,-72.9267251261949,
676.462296651428));
#270084=CARTESIAN_POINT('Ctrl Pts',(101.965012102074,-81.4032507354509,
674.462296651428));
#270085=CARTESIAN_POINT('Ctrl Pts',(94.9701958612989,-88.8775672472035,
672.462296651428));
#270086=CARTESIAN_POINT('Ctrl Pts',(87.9753796205242,-96.351883758956,670.462296651428));
#270087=CARTESIAN_POINT('Ctrl Pts',(79.8974404698481,-102.639948694851,
668.462296651428));
#270088=CARTESIAN_POINT('Ctrl Pts',(71.8195013191721,-108.928013630747,
666.462296651428));
#270089=CARTESIAN_POINT('Ctrl Pts',(62.8573449296273,-113.874993963172,
664.462296651428));
#270090=CARTESIAN_POINT('Ctrl Pts',(53.8951885400825,-118.821974295598,
662.462296651428));
#270091=CARTESIAN_POINT('Ctrl Pts',(44.2694929456714,-122.306058950682,
660.462296651428));
#270092=CARTESIAN_POINT('Ctrl Pts',(34.6437973512603,-125.790143605767,
658.462296651428));
#270093=CARTESIAN_POINT('Ctrl Pts',(24.5915791233694,-127.725542856289,
656.462296651428));
#270094=CARTESIAN_POINT('Ctrl Pts',(14.5393608954785,-129.660942106811,
654.462296651428));
#270095=CARTESIAN_POINT('Ctrl Pts',(4.30813900827813,-130.,652.462296651428));
#270096=CARTESIAN_POINT('Ctrl Pts',(-5.92308287892227,-130.339057893189,
650.462296651428));
#270097=CARTESIAN_POINT('Ctrl Pts',(-16.0813817870906,-129.073425698447,
648.462296651428));
#270098=CARTESIAN_POINT('Ctrl Pts',(-26.2396806952589,-127.807793503705,
646.462296651428));
#270099=CARTESIAN_POINT('Ctrl Pts',(-36.0749255918149,-124.968635286058,
644.462296651428));
#270100=CARTESIAN_POINT('Ctrl Pts',(-45.9101704883709,-122.129477068411,
642.462296651428));
#270101=CARTESIAN_POINT('Ctrl Pts',(-55.1801850026549,-117.786702325803,
640.462296651428));
#270102=CARTESIAN_POINT('Ctrl Pts',(-64.4501995169389,-113.443927583196,
638.462296651428));
#270103=CARTESIAN_POINT('Ctrl Pts',(-72.9267251261949,-107.704469842635,
636.462296651428));
#270104=CARTESIAN_POINT('Ctrl Pts',(-81.4032507354509,-101.965012102074,
634.462296651428));
#270105=CARTESIAN_POINT('Ctrl Pts',(-88.8775672472034,-94.9701958612989,
632.462296651428));
#270106=CARTESIAN_POINT('Ctrl Pts',(-96.351883758956,-87.9753796205242,
630.462296651428));
#270107=CARTESIAN_POINT('Ctrl Pts',(-102.639948694851,-79.8974404698482,
628.462296651428));
#270108=CARTESIAN_POINT('Ctrl Pts',(-108.928013630747,-71.8195013191721,
626.462296651429));
#270109=CARTESIAN_POINT('Ctrl Pts',(-113.874993963172,-62.8573449296273,
624.462296651428));
#270110=CARTESIAN_POINT('Ctrl Pts',(-118.821974295598,-53.8951885400825,
622.462296651428));
#270111=CARTESIAN_POINT('Ctrl Pts',(-122.306058950682,-44.2694929456714,
620.462296651428));
#270112=CARTESIAN_POINT('Ctrl Pts',(-125.790143605767,-34.6437973512603,
618.462296651428));
#270113=CARTESIAN_POINT('Ctrl Pts',(-127.725542856289,-24.5915791233694,
616.462296651428));
#270114=CARTESIAN_POINT('Ctrl Pts',(-129.660942106811,-14.5393608954785,
614.462296651429));
#270115=CARTESIAN_POINT('Ctrl Pts',(-130.,-4.30813900827813,612.462296651428));
#270116=CARTESIAN_POINT('Ctrl Pts',(-130.339057893189,5.92308287892227,
610.462296651428));
#270117=CARTESIAN_POINT('Ctrl Pts',(-129.073425698447,16.0813817870906,
608.462296651428));
#270118=CARTESIAN_POINT('Ctrl Pts',(-127.807793503705,26.2396806952589,
606.462296651428));
#270119=CARTESIAN_POINT('Ctrl Pts',(-124.968635286058,36.0749255918149,
604.462296651428));
#270120=CARTESIAN_POINT('Ctrl Pts',(-122.129477068411,45.9101704883709,
602.462296651429));
#270121=CARTESIAN_POINT('Ctrl Pts',(-117.786702325803,55.1801850026549,
600.462296651428));
#270122=CARTESIAN_POINT('Ctrl Pts',(-113.443927583196,64.4501995169388,
598.462296651428));
#270123=CARTESIAN_POINT('Ctrl Pts',(-107.704469842635,72.9267251261949,
596.462296651428));
#270124=CARTESIAN_POINT('Ctrl Pts',(-101.965012102074,81.4032507354509,
594.462296651428));
#270125=CARTESIAN_POINT('Ctrl Pts',(-94.9701958612989,88.8775672472034,
592.462296651428));
#270126=CARTESIAN_POINT('Ctrl Pts',(-87.9753796205243,96.3518837589559,
590.462296651428));
#270127=CARTESIAN_POINT('Ctrl Pts',(-79.8974404698482,102.639948694851,
588.462296651428));
#270128=CARTESIAN_POINT('Ctrl Pts',(-71.819501319172,108.928013630747,586.462296651428));
#270129=CARTESIAN_POINT('Ctrl Pts',(-62.8573449296273,113.874993963172,
584.462296651428));
#270130=CARTESIAN_POINT('Ctrl Pts',(-53.8951885400826,118.821974295598,
582.462296651428));
#270131=CARTESIAN_POINT('Ctrl Pts',(-44.2694929456714,122.306058950682,
580.462296651428));
#270132=CARTESIAN_POINT('Ctrl Pts',(-34.6437973512603,125.790143605767,
578.462296651428));
#270133=CARTESIAN_POINT('Ctrl Pts',(-24.5915791233694,127.725542856289,
576.462296651428));
#270134=CARTESIAN_POINT('Ctrl Pts',(-14.5393608954786,129.660942106811,
574.462296651428));
#270135=CARTESIAN_POINT('Ctrl Pts',(-4.30813900827814,130.,572.462296651428));
#270136=CARTESIAN_POINT('Ctrl Pts',(5.92308287892232,130.339057893189,570.462296651428));
#270137=CARTESIAN_POINT('Ctrl Pts',(16.0813817870906,129.073425698447,568.462296651428));
#270138=CARTESIAN_POINT('Ctrl Pts',(26.2396806952589,127.807793503705,566.462296651428));
#270139=CARTESIAN_POINT('Ctrl Pts',(36.0749255918149,124.968635286058,564.462296651428));
#270140=CARTESIAN_POINT('Ctrl Pts',(45.9101704883709,122.129477068411,562.462296651428));
#270141=CARTESIAN_POINT('Ctrl Pts',(55.1801850026549,117.786702325803,560.462296651428));
#270142=CARTESIAN_POINT('Ctrl Pts',(64.4501995169388,113.443927583196,558.462296651428));
#270143=CARTESIAN_POINT('Ctrl Pts',(72.9267251261949,107.704469842635,556.462296651428));
#270144=CARTESIAN_POINT('Ctrl Pts',(81.4032507354509,101.965012102074,554.462296651428));
#270145=CARTESIAN_POINT('Ctrl Pts',(88.8775672472034,94.9701958612989,552.462296651428));
#270146=CARTESIAN_POINT('Ctrl Pts',(96.3518837589559,87.9753796205243,550.462296651428));
#270147=CARTESIAN_POINT('Ctrl Pts',(102.639948694851,79.8974404698482,548.462296651428));
#270148=CARTESIAN_POINT('Ctrl Pts',(108.928013630747,71.819501319172,546.462296651428));
#270149=CARTESIAN_POINT('Ctrl Pts',(113.874993963172,62.8573449296273,544.462296651428));
#270150=CARTESIAN_POINT('Ctrl Pts',(118.821974295598,53.8951885400826,542.462296651428));
#270151=CARTESIAN_POINT('Ctrl Pts',(122.306058950682,44.2694929456714,540.462296651428));
#270152=CARTESIAN_POINT('Ctrl Pts',(125.790143605767,34.6437973512603,538.462296651428));
#270153=CARTESIAN_POINT('Ctrl Pts',(127.725542856289,24.5915791233694,536.462296651428));
#270154=CARTESIAN_POINT('Ctrl Pts',(129.660942106811,14.5393608954786,534.462296651428));
#270155=CARTESIAN_POINT('Ctrl Pts',(130.,4.30813900827812,532.462296651428));
#270156=CARTESIAN_POINT('Ctrl Pts',(160.,4.30813900827813,692.462296651428));
#270157=CARTESIAN_POINT('Ctrl Pts',(160.339057893189,-8.28413408366083,
690.462296651428));
#270158=CARTESIAN_POINT('Ctrl Pts',(158.704075916301,-20.7744157382975,
688.462296651428));
#270159=CARTESIAN_POINT('Ctrl Pts',(157.069093939413,-33.2646973929343,
686.462296651429));
#270160=CARTESIAN_POINT('Ctrl Pts',(153.500330774912,-45.3454354230633,
684.462296651428));
#270161=CARTESIAN_POINT('Ctrl Pts',(149.931567610412,-57.4261734531924,
682.462296651428));
#270162=CARTESIAN_POINT('Ctrl Pts',(144.516898051455,-68.7998999948413,
680.462296651428));
#270163=CARTESIAN_POINT('Ctrl Pts',(139.102228492497,-80.1736265364901,
678.462296651428));
#270164=CARTESIAN_POINT('Ctrl Pts',(131.974979673883,-90.5602826949691,
676.462296651428));
#270165=CARTESIAN_POINT('Ctrl Pts',(124.847730855269,-100.946938853448,
674.462296651428));
#270166=CARTESIAN_POINT('Ctrl Pts',(116.183399296895,-110.0907706828,672.462296651428));
#270167=CARTESIAN_POINT('Ctrl Pts',(107.519067738521,-119.234602512152,
670.462296651428));
#270168=CARTESIAN_POINT('Ctrl Pts',(97.5309980386224,-126.9104585261,668.462296651428));
#270169=CARTESIAN_POINT('Ctrl Pts',(87.5429283387234,-134.586314540048,
666.462296651428));
#270170=CARTESIAN_POINT('Ctrl Pts',(76.4770599218137,-140.605189688823,
664.462296651428));
#270171=CARTESIAN_POINT('Ctrl Pts',(65.4111915049041,-146.624064837599,
662.462296651428));
#270172=CARTESIAN_POINT('Ctrl Pts',(53.5400027769198,-150.837754439537,
660.462296651428));
#270173=CARTESIAN_POINT('Ctrl Pts',(41.6688140489356,-155.051444041475,
658.462296651428));
#270174=CARTESIAN_POINT('Ctrl Pts',(29.2846130745764,-157.356193074143,
656.462296651428));
#270175=CARTESIAN_POINT('Ctrl Pts',(16.9004121002171,-159.660942106811,
654.462296651428));
#270176=CARTESIAN_POINT('Ctrl Pts',(4.30813900827814,-160.,652.462296651428));
#270177=CARTESIAN_POINT('Ctrl Pts',(-8.28413408366082,-160.339057893189,
650.462296651428));
#270178=CARTESIAN_POINT('Ctrl Pts',(-20.7744157382975,-158.704075916301,
648.462296651428));
#270179=CARTESIAN_POINT('Ctrl Pts',(-33.2646973929342,-157.069093939413,
646.462296651428));
#270180=CARTESIAN_POINT('Ctrl Pts',(-45.3454354230633,-153.500330774912,
644.462296651428));
#270181=CARTESIAN_POINT('Ctrl Pts',(-57.4261734531924,-149.931567610412,
642.462296651428));
#270182=CARTESIAN_POINT('Ctrl Pts',(-68.7998999948413,-144.516898051455,
640.462296651428));
#270183=CARTESIAN_POINT('Ctrl Pts',(-80.1736265364901,-139.102228492497,
638.462296651428));
#270184=CARTESIAN_POINT('Ctrl Pts',(-90.5602826949691,-131.974979673883,
636.462296651428));
#270185=CARTESIAN_POINT('Ctrl Pts',(-100.946938853448,-124.847730855269,
634.462296651428));
#270186=CARTESIAN_POINT('Ctrl Pts',(-110.0907706828,-116.183399296895,632.462296651428));
#270187=CARTESIAN_POINT('Ctrl Pts',(-119.234602512152,-107.519067738521,
630.462296651428));
#270188=CARTESIAN_POINT('Ctrl Pts',(-126.9104585261,-97.5309980386224,628.462296651428));
#270189=CARTESIAN_POINT('Ctrl Pts',(-134.586314540048,-87.5429283387234,
626.462296651429));
#270190=CARTESIAN_POINT('Ctrl Pts',(-140.605189688823,-76.4770599218137,
624.462296651428));
#270191=CARTESIAN_POINT('Ctrl Pts',(-146.624064837599,-65.4111915049041,
622.462296651428));
#270192=CARTESIAN_POINT('Ctrl Pts',(-150.837754439537,-53.5400027769199,
620.462296651428));
#270193=CARTESIAN_POINT('Ctrl Pts',(-155.051444041475,-41.6688140489356,
618.462296651428));
#270194=CARTESIAN_POINT('Ctrl Pts',(-157.356193074143,-29.2846130745764,
616.462296651428));
#270195=CARTESIAN_POINT('Ctrl Pts',(-159.660942106811,-16.9004121002171,
614.462296651429));
#270196=CARTESIAN_POINT('Ctrl Pts',(-160.,-4.30813900827815,612.462296651428));
#270197=CARTESIAN_POINT('Ctrl Pts',(-160.339057893189,8.28413408366081,
610.462296651428));
#270198=CARTESIAN_POINT('Ctrl Pts',(-158.704075916301,20.7744157382975,
608.462296651428));
#270199=CARTESIAN_POINT('Ctrl Pts',(-157.069093939413,33.2646973929342,
606.462296651428));
#270200=CARTESIAN_POINT('Ctrl Pts',(-153.500330774912,45.3454354230633,
604.462296651428));
#270201=CARTESIAN_POINT('Ctrl Pts',(-149.931567610412,57.4261734531924,
602.462296651429));
#270202=CARTESIAN_POINT('Ctrl Pts',(-144.516898051455,68.7998999948413,
600.462296651428));
#270203=CARTESIAN_POINT('Ctrl Pts',(-139.102228492497,80.1736265364901,
598.462296651428));
#270204=CARTESIAN_POINT('Ctrl Pts',(-131.974979673883,90.5602826949691,
596.462296651428));
#270205=CARTESIAN_POINT('Ctrl Pts',(-124.847730855269,100.946938853448,
594.462296651428));
#270206=CARTESIAN_POINT('Ctrl Pts',(-116.183399296895,110.0907706828,592.462296651428));
#270207=CARTESIAN_POINT('Ctrl Pts',(-107.519067738521,119.234602512152,
590.462296651428));
#270208=CARTESIAN_POINT('Ctrl Pts',(-97.5309980386224,126.9104585261,588.462296651428));
#270209=CARTESIAN_POINT('Ctrl Pts',(-87.5429283387233,134.586314540048,
586.462296651428));
#270210=CARTESIAN_POINT('Ctrl Pts',(-76.4770599218137,140.605189688823,
584.462296651428));
#270211=CARTESIAN_POINT('Ctrl Pts',(-65.4111915049042,146.624064837599,
582.462296651428));
#270212=CARTESIAN_POINT('Ctrl Pts',(-53.5400027769199,150.837754439537,
580.462296651428));
#270213=CARTESIAN_POINT('Ctrl Pts',(-41.6688140489356,155.051444041475,
578.462296651428));
#270214=CARTESIAN_POINT('Ctrl Pts',(-29.2846130745764,157.356193074143,
576.462296651428));
#270215=CARTESIAN_POINT('Ctrl Pts',(-16.9004121002172,159.660942106811,
574.462296651428));
#270216=CARTESIAN_POINT('Ctrl Pts',(-4.30813900827816,160.,572.462296651428));
#270217=CARTESIAN_POINT('Ctrl Pts',(8.28413408366087,160.339057893189,570.462296651428));
#270218=CARTESIAN_POINT('Ctrl Pts',(20.7744157382975,158.704075916301,568.462296651428));
#270219=CARTESIAN_POINT('Ctrl Pts',(33.2646973929342,157.069093939413,566.462296651428));
#270220=CARTESIAN_POINT('Ctrl Pts',(45.3454354230633,153.500330774912,564.462296651428));
#270221=CARTESIAN_POINT('Ctrl Pts',(57.4261734531925,149.931567610412,562.462296651428));
#270222=CARTESIAN_POINT('Ctrl Pts',(68.7998999948413,144.516898051455,560.462296651428));
#270223=CARTESIAN_POINT('Ctrl Pts',(80.1736265364901,139.102228492498,558.462296651428));
#270224=CARTESIAN_POINT('Ctrl Pts',(90.560282694969,131.974979673883,556.462296651428));
#270225=CARTESIAN_POINT('Ctrl Pts',(100.946938853448,124.847730855269,554.462296651428));
#270226=CARTESIAN_POINT('Ctrl Pts',(110.0907706828,116.183399296895,552.462296651428));
#270227=CARTESIAN_POINT('Ctrl Pts',(119.234602512152,107.519067738521,550.462296651428));
#270228=CARTESIAN_POINT('Ctrl Pts',(126.9104585261,97.5309980386224,548.462296651428));
#270229=CARTESIAN_POINT('Ctrl Pts',(134.586314540048,87.5429283387233,546.462296651428));
#270230=CARTESIAN_POINT('Ctrl Pts',(140.605189688823,76.4770599218137,544.462296651428));
#270231=CARTESIAN_POINT('Ctrl Pts',(146.624064837599,65.4111915049042,542.462296651428));
#270232=CARTESIAN_POINT('Ctrl Pts',(150.837754439537,53.5400027769199,540.462296651428));
#270233=CARTESIAN_POINT('Ctrl Pts',(155.051444041475,41.6688140489356,538.462296651428));
#270234=CARTESIAN_POINT('Ctrl Pts',(157.356193074143,29.2846130745764,536.462296651428));
#270235=CARTESIAN_POINT('Ctrl Pts',(159.660942106811,16.9004121002172,534.462296651428));
#270236=CARTESIAN_POINT('Ctrl Pts',(160.,4.30813900827813,532.462296651428));
#270237=CARTESIAN_POINT('Ctrl Pts',(129.934615416877,-5.96286660784778,
690.450909781393));
#270238=CARTESIAN_POINT('Ctrl Pts',(129.701667605591,-11.0389459941992,
689.45506834253));
#270239=CARTESIAN_POINT('Ctrl Pts',(129.073425698447,-16.0813817870906,
688.462296651428));
#270240=CARTESIAN_POINT('Ctrl Pts',(127.807793503704,-26.2396806952589,
686.462296651429));
#270241=CARTESIAN_POINT('Ctrl Pts',(124.968635286058,-36.0749255918149,
684.462296651428));
#270242=CARTESIAN_POINT('Ctrl Pts',(122.129477068411,-45.9101704883709,
682.462296651428));
#270243=CARTESIAN_POINT('Ctrl Pts',(117.786702325803,-55.1801850026549,
680.462296651428));
#270244=CARTESIAN_POINT('Ctrl Pts',(113.443927583196,-64.4501995169389,
678.462296651428));
#270245=CARTESIAN_POINT('Ctrl Pts',(107.704469842635,-72.9267251261949,
676.462296651428));
#270246=CARTESIAN_POINT('Ctrl Pts',(101.965012102074,-81.4032507354509,
674.462296651428));
#270247=CARTESIAN_POINT('Ctrl Pts',(94.9701958612989,-88.8775672472035,
672.462296651428));
#270248=CARTESIAN_POINT('Ctrl Pts',(87.9753796205242,-96.351883758956,670.462296651428));
#270249=CARTESIAN_POINT('Ctrl Pts',(79.8974404698481,-102.639948694851,
668.462296651428));
#270250=CARTESIAN_POINT('Ctrl Pts',(71.8195013191721,-108.928013630747,
666.462296651428));
#270251=CARTESIAN_POINT('Ctrl Pts',(62.8573449296273,-113.874993963172,
664.462296651428));
#270252=CARTESIAN_POINT('Ctrl Pts',(53.8951885400825,-118.821974295598,
662.462296651428));
#270253=CARTESIAN_POINT('Ctrl Pts',(44.2694929456714,-122.306058950682,
660.462296651428));
#270254=CARTESIAN_POINT('Ctrl Pts',(34.6437973512603,-125.790143605767,
658.462296651428));
#270255=CARTESIAN_POINT('Ctrl Pts',(24.5915791233694,-127.725542856289,
656.462296651428));
#270256=CARTESIAN_POINT('Ctrl Pts',(14.5393608954785,-129.660942106811,
654.462296651428));
#270257=CARTESIAN_POINT('Ctrl Pts',(4.30813900827813,-130.,652.462296651428));
#270258=CARTESIAN_POINT('Ctrl Pts',(-5.92308287892227,-130.339057893189,
650.462296651428));
#270259=CARTESIAN_POINT('Ctrl Pts',(-16.0813817870906,-129.073425698447,
648.462296651428));
#270260=CARTESIAN_POINT('Ctrl Pts',(-26.2396806952589,-127.807793503705,
646.462296651428));
#270261=CARTESIAN_POINT('Ctrl Pts',(-36.0749255918149,-124.968635286058,
644.462296651428));
#270262=CARTESIAN_POINT('Ctrl Pts',(-45.9101704883709,-122.129477068411,
642.462296651428));
#270263=CARTESIAN_POINT('Ctrl Pts',(-55.1801850026549,-117.786702325803,
640.462296651428));
#270264=CARTESIAN_POINT('Ctrl Pts',(-64.4501995169389,-113.443927583196,
638.462296651428));
#270265=CARTESIAN_POINT('Ctrl Pts',(-72.9267251261949,-107.704469842635,
636.462296651428));
#270266=CARTESIAN_POINT('Ctrl Pts',(-81.4032507354509,-101.965012102074,
634.462296651428));
#270267=CARTESIAN_POINT('Ctrl Pts',(-88.8775672472034,-94.9701958612989,
632.462296651428));
#270268=CARTESIAN_POINT('Ctrl Pts',(-96.351883758956,-87.9753796205242,
630.462296651428));
#270269=CARTESIAN_POINT('Ctrl Pts',(-102.639948694851,-79.8974404698482,
628.462296651428));
#270270=CARTESIAN_POINT('Ctrl Pts',(-108.928013630747,-71.8195013191721,
626.462296651428));
#270271=CARTESIAN_POINT('Ctrl Pts',(-113.874993963172,-62.8573449296273,
624.462296651428));
#270272=CARTESIAN_POINT('Ctrl Pts',(-118.821974295598,-53.8951885400825,
622.462296651428));
#270273=CARTESIAN_POINT('Ctrl Pts',(-122.306058950682,-44.2694929456714,
620.462296651428));
#270274=CARTESIAN_POINT('Ctrl Pts',(-125.790143605767,-34.6437973512603,
618.462296651428));
#270275=CARTESIAN_POINT('Ctrl Pts',(-127.725542856289,-24.5915791233694,
616.462296651428));
#270276=CARTESIAN_POINT('Ctrl Pts',(-129.660942106811,-14.5393608954785,
614.462296651428));
#270277=CARTESIAN_POINT('Ctrl Pts',(-130.,-4.30813900827813,612.462296651428));
#270278=CARTESIAN_POINT('Ctrl Pts',(-130.339057893189,5.92308287892227,
610.462296651428));
#270279=CARTESIAN_POINT('Ctrl Pts',(-129.073425698447,16.0813817870906,
608.462296651428));
#270280=CARTESIAN_POINT('Ctrl Pts',(-127.807793503705,26.2396806952589,
606.462296651428));
#270281=CARTESIAN_POINT('Ctrl Pts',(-124.968635286058,36.0749255918149,
604.462296651428));
#270282=CARTESIAN_POINT('Ctrl Pts',(-122.129477068411,45.9101704883709,
602.462296651428));
#270283=CARTESIAN_POINT('Ctrl Pts',(-117.786702325803,55.1801850026549,
600.462296651428));
#270284=CARTESIAN_POINT('Ctrl Pts',(-113.443927583196,64.4501995169388,
598.462296651428));
#270285=CARTESIAN_POINT('Ctrl Pts',(-107.704469842635,72.9267251261949,
596.462296651428));
#270286=CARTESIAN_POINT('Ctrl Pts',(-101.965012102074,81.4032507354509,
594.462296651428));
#270287=CARTESIAN_POINT('Ctrl Pts',(-94.9701958612989,88.8775672472034,
592.462296651428));
#270288=CARTESIAN_POINT('Ctrl Pts',(-87.9753796205243,96.3518837589559,
590.462296651428));
#270289=CARTESIAN_POINT('Ctrl Pts',(-79.8974404698482,102.639948694851,
588.462296651428));
#270290=CARTESIAN_POINT('Ctrl Pts',(-71.819501319172,108.928013630747,586.462296651428));
#270291=CARTESIAN_POINT('Ctrl Pts',(-62.8573449296273,113.874993963172,
584.462296651428));
#270292=CARTESIAN_POINT('Ctrl Pts',(-53.8951885400826,118.821974295598,
582.462296651428));
#270293=CARTESIAN_POINT('Ctrl Pts',(-44.2694929456714,122.306058950682,
580.462296651428));
#270294=CARTESIAN_POINT('Ctrl Pts',(-34.6437973512603,125.790143605767,
578.462296651428));
#270295=CARTESIAN_POINT('Ctrl Pts',(-24.5915791233694,127.725542856289,
576.462296651428));
#270296=CARTESIAN_POINT('Ctrl Pts',(-14.5393608954786,129.660942106811,
574.462296651428));
#270297=CARTESIAN_POINT('Ctrl Pts',(-4.30813900827814,130.,572.462296651428));
#270298=CARTESIAN_POINT('Ctrl Pts',(5.92308287892232,130.339057893189,570.462296651428));
#270299=CARTESIAN_POINT('Ctrl Pts',(16.0813817870906,129.073425698447,568.462296651428));
#270300=CARTESIAN_POINT('Ctrl Pts',(26.2396806952589,127.807793503705,566.462296651428));
#270301=CARTESIAN_POINT('Ctrl Pts',(36.0749255918149,124.968635286058,564.462296651428));
#270302=CARTESIAN_POINT('Ctrl Pts',(45.9101704883709,122.129477068411,562.462296651428));
#270303=CARTESIAN_POINT('Ctrl Pts',(55.1801850026549,117.786702325803,560.462296651428));
#270304=CARTESIAN_POINT('Ctrl Pts',(64.4501995169388,113.443927583196,558.462296651428));
#270305=CARTESIAN_POINT('Ctrl Pts',(72.9267251261949,107.704469842635,556.462296651428));
#270306=CARTESIAN_POINT('Ctrl Pts',(81.403250735451,101.965012102074,554.462296651428));
#270307=CARTESIAN_POINT('Ctrl Pts',(88.8775672472034,94.9701958612989,552.462296651428));
#270308=CARTESIAN_POINT('Ctrl Pts',(96.3518837589559,87.9753796205243,550.462296651428));
#270309=CARTESIAN_POINT('Ctrl Pts',(102.639948694851,79.8974404698482,548.462296651428));
#270310=CARTESIAN_POINT('Ctrl Pts',(108.928013630747,71.8195013191721,546.462296651428));
#270311=CARTESIAN_POINT('Ctrl Pts',(113.874993963172,62.8573449296273,544.462296651428));
#270312=CARTESIAN_POINT('Ctrl Pts',(118.821974295598,53.8951885400826,542.462296651428));
#270313=CARTESIAN_POINT('Ctrl Pts',(122.306058950682,44.2694929456714,540.462296651428));
#270314=CARTESIAN_POINT('Ctrl Pts',(125.790143605767,34.6437973512603,538.462296651428));
#270315=CARTESIAN_POINT('Ctrl Pts',(127.725542856289,24.5915791233694,536.462296651428));
#270316=CARTESIAN_POINT('Ctrl Pts',(129.382196958681,15.9871278397994,534.750345898172));
#270317=CARTESIAN_POINT('Ctrl Pts',(129.869812400585,7.23822414350004,533.035792462989));
#270318=CARTESIAN_POINT('Ctrl Pts',(130.,-4.30813900827807,697.537703348572));
#270319=CARTESIAN_POINT('Ctrl Pts',(129.660942106811,-14.5393608954785,
695.537703348572));
#270320=CARTESIAN_POINT('Ctrl Pts',(127.725542856289,-24.5915791233694,
693.537703348572));
#270321=CARTESIAN_POINT('Ctrl Pts',(125.790143605767,-34.6437973512603,
691.537703348572));
#270322=CARTESIAN_POINT('Ctrl Pts',(122.306058950682,-44.2694929456714,
689.537703348572));
#270323=CARTESIAN_POINT('Ctrl Pts',(118.821974295598,-53.8951885400825,
687.537703348572));
#270324=CARTESIAN_POINT('Ctrl Pts',(113.874993963172,-62.8573449296272,
685.537703348572));
#270325=CARTESIAN_POINT('Ctrl Pts',(108.928013630747,-71.819501319172,683.537703348572));
#270326=CARTESIAN_POINT('Ctrl Pts',(102.639948694851,-79.8974404698481,
681.537703348572));
#270327=CARTESIAN_POINT('Ctrl Pts',(96.351883758956,-87.9753796205242,679.537703348572));
#270328=CARTESIAN_POINT('Ctrl Pts',(88.8775672472035,-94.9701958612989,
677.537703348572));
#270329=CARTESIAN_POINT('Ctrl Pts',(81.403250735451,-101.965012102074,675.537703348572));
#270330=CARTESIAN_POINT('Ctrl Pts',(72.9267251261949,-107.704469842635,
673.537703348572));
#270331=CARTESIAN_POINT('Ctrl Pts',(64.4501995169389,-113.443927583196,
671.537703348572));
#270332=CARTESIAN_POINT('Ctrl Pts',(55.1801850026549,-117.786702325803,
669.537703348572));
#270333=CARTESIAN_POINT('Ctrl Pts',(45.910170488371,-122.129477068411,667.537703348572));
#270334=CARTESIAN_POINT('Ctrl Pts',(36.074925591815,-124.968635286058,665.537703348572));
#270335=CARTESIAN_POINT('Ctrl Pts',(26.239680695259,-127.807793503704,663.537703348572));
#270336=CARTESIAN_POINT('Ctrl Pts',(16.0813817870907,-129.073425698447,
661.537703348572));
#270337=CARTESIAN_POINT('Ctrl Pts',(5.92308287892234,-130.339057893189,
659.537703348572));
#270338=CARTESIAN_POINT('Ctrl Pts',(-4.30813900827806,-130.,657.537703348572));
#270339=CARTESIAN_POINT('Ctrl Pts',(-14.5393608954785,-129.660942106811,
655.537703348572));
#270340=CARTESIAN_POINT('Ctrl Pts',(-24.5915791233694,-127.725542856289,
653.537703348572));
#270341=CARTESIAN_POINT('Ctrl Pts',(-34.6437973512603,-125.790143605767,
651.537703348572));
#270342=CARTESIAN_POINT('Ctrl Pts',(-44.2694929456713,-122.306058950682,
649.537703348572));
#270343=CARTESIAN_POINT('Ctrl Pts',(-53.8951885400825,-118.821974295598,
647.537703348572));
#270344=CARTESIAN_POINT('Ctrl Pts',(-62.8573449296272,-113.874993963172,
645.537703348572));
#270345=CARTESIAN_POINT('Ctrl Pts',(-71.819501319172,-108.928013630747,
643.537703348572));
#270346=CARTESIAN_POINT('Ctrl Pts',(-79.8974404698481,-102.639948694851,
641.537703348572));
#270347=CARTESIAN_POINT('Ctrl Pts',(-87.9753796205242,-96.351883758956,
639.537703348572));
#270348=CARTESIAN_POINT('Ctrl Pts',(-94.9701958612989,-88.8775672472035,
637.537703348572));
#270349=CARTESIAN_POINT('Ctrl Pts',(-101.965012102074,-81.403250735451,
635.537703348572));
#270350=CARTESIAN_POINT('Ctrl Pts',(-107.704469842635,-72.9267251261949,
633.537703348572));
#270351=CARTESIAN_POINT('Ctrl Pts',(-113.443927583196,-64.4501995169389,
631.537703348572));
#270352=CARTESIAN_POINT('Ctrl Pts',(-117.786702325803,-55.1801850026549,
629.537703348572));
#270353=CARTESIAN_POINT('Ctrl Pts',(-122.129477068411,-45.910170488371,
627.537703348572));
#270354=CARTESIAN_POINT('Ctrl Pts',(-124.968635286058,-36.074925591815,
625.537703348572));
#270355=CARTESIAN_POINT('Ctrl Pts',(-127.807793503704,-26.239680695259,
623.537703348572));
#270356=CARTESIAN_POINT('Ctrl Pts',(-129.073425698447,-16.0813817870907,
621.537703348572));
#270357=CARTESIAN_POINT('Ctrl Pts',(-130.339057893189,-5.92308287892235,
619.537703348572));
#270358=CARTESIAN_POINT('Ctrl Pts',(-130.,4.30813900827805,617.537703348572));
#270359=CARTESIAN_POINT('Ctrl Pts',(-129.660942106811,14.5393608954784,
615.537703348572));
#270360=CARTESIAN_POINT('Ctrl Pts',(-127.725542856289,24.5915791233693,
613.537703348572));
#270361=CARTESIAN_POINT('Ctrl Pts',(-125.790143605767,34.6437973512602,
611.537703348572));
#270362=CARTESIAN_POINT('Ctrl Pts',(-122.306058950682,44.2694929456713,
609.537703348572));
#270363=CARTESIAN_POINT('Ctrl Pts',(-118.821974295598,53.8951885400825,
607.537703348572));
#270364=CARTESIAN_POINT('Ctrl Pts',(-113.874993963172,62.8573449296272,
605.537703348572));
#270365=CARTESIAN_POINT('Ctrl Pts',(-108.928013630747,71.819501319172,603.537703348572));
#270366=CARTESIAN_POINT('Ctrl Pts',(-102.639948694851,79.8974404698481,
601.537703348572));
#270367=CARTESIAN_POINT('Ctrl Pts',(-96.3518837589561,87.9753796205242,
599.537703348572));
#270368=CARTESIAN_POINT('Ctrl Pts',(-88.8775672472035,94.9701958612989,
597.537703348572));
#270369=CARTESIAN_POINT('Ctrl Pts',(-81.403250735451,101.965012102074,595.537703348572));
#270370=CARTESIAN_POINT('Ctrl Pts',(-72.9267251261949,107.704469842635,
593.537703348572));
#270371=CARTESIAN_POINT('Ctrl Pts',(-64.4501995169389,113.443927583196,
591.537703348572));
#270372=CARTESIAN_POINT('Ctrl Pts',(-55.1801850026549,117.786702325803,
589.537703348572));
#270373=CARTESIAN_POINT('Ctrl Pts',(-45.910170488371,122.129477068411,587.537703348572));
#270374=CARTESIAN_POINT('Ctrl Pts',(-36.074925591815,124.968635286058,585.537703348572));
#270375=CARTESIAN_POINT('Ctrl Pts',(-26.239680695259,127.807793503704,583.537703348572));
#270376=CARTESIAN_POINT('Ctrl Pts',(-16.0813817870907,129.073425698447,
581.537703348572));
#270377=CARTESIAN_POINT('Ctrl Pts',(-5.92308287892242,130.339057893189,
579.537703348572));
#270378=CARTESIAN_POINT('Ctrl Pts',(4.30813900827804,130.,577.537703348572));
#270379=CARTESIAN_POINT('Ctrl Pts',(14.5393608954785,129.660942106811,575.537703348572));
#270380=CARTESIAN_POINT('Ctrl Pts',(24.5915791233693,127.725542856289,573.537703348572));
#270381=CARTESIAN_POINT('Ctrl Pts',(34.6437973512602,125.790143605767,571.537703348572));
#270382=CARTESIAN_POINT('Ctrl Pts',(44.2694929456713,122.306058950682,569.537703348572));
#270383=CARTESIAN_POINT('Ctrl Pts',(53.8951885400825,118.821974295598,567.537703348572));
#270384=CARTESIAN_POINT('Ctrl Pts',(62.8573449296272,113.874993963172,565.537703348572));
#270385=CARTESIAN_POINT('Ctrl Pts',(71.819501319172,108.928013630747,563.537703348572));
#270386=CARTESIAN_POINT('Ctrl Pts',(79.8974404698481,102.639948694851,561.537703348572));
#270387=CARTESIAN_POINT('Ctrl Pts',(87.9753796205242,96.351883758956,559.537703348572));
#270388=CARTESIAN_POINT('Ctrl Pts',(94.9701958612989,88.8775672472035,557.537703348572));
#270389=CARTESIAN_POINT('Ctrl Pts',(101.965012102074,81.403250735451,555.537703348572));
#270390=CARTESIAN_POINT('Ctrl Pts',(107.704469842635,72.926725126195,553.537703348572));
#270391=CARTESIAN_POINT('Ctrl Pts',(113.443927583196,64.4501995169389,551.537703348572));
#270392=CARTESIAN_POINT('Ctrl Pts',(117.786702325803,55.1801850026549,549.537703348572));
#270393=CARTESIAN_POINT('Ctrl Pts',(122.129477068411,45.910170488371,547.537703348572));
#270394=CARTESIAN_POINT('Ctrl Pts',(124.968635286058,36.074925591815,545.537703348572));
#270395=CARTESIAN_POINT('Ctrl Pts',(127.807793503704,26.239680695259,543.537703348572));
#270396=CARTESIAN_POINT('Ctrl Pts',(129.073425698447,16.0813817870907,541.537703348572));
#270397=CARTESIAN_POINT('Ctrl Pts',(130.339057893189,5.92308287892242,539.537703348572));
#270398=CARTESIAN_POINT('Ctrl Pts',(130.,-4.30813900827807,537.537703348572));
#270399=CARTESIAN_POINT('Ctrl Pts',(130.,4.30813900827812,692.462296651428));
#270400=CARTESIAN_POINT('Ctrl Pts',(130.339057893189,-5.92308287892228,
690.462296651428));
#270401=CARTESIAN_POINT('Ctrl Pts',(129.073425698447,-16.0813817870906,
688.462296651428));
#270402=CARTESIAN_POINT('Ctrl Pts',(127.807793503704,-26.2396806952589,
686.462296651429));
#270403=CARTESIAN_POINT('Ctrl Pts',(124.968635286058,-36.0749255918149,
684.462296651428));
#270404=CARTESIAN_POINT('Ctrl Pts',(122.129477068411,-45.9101704883709,
682.462296651428));
#270405=CARTESIAN_POINT('Ctrl Pts',(117.786702325803,-55.1801850026549,
680.462296651428));
#270406=CARTESIAN_POINT('Ctrl Pts',(113.443927583196,-64.4501995169389,
678.462296651428));
#270407=CARTESIAN_POINT('Ctrl Pts',(107.704469842635,-72.9267251261949,
676.462296651428));
#270408=CARTESIAN_POINT('Ctrl Pts',(101.965012102074,-81.4032507354509,
674.462296651428));
#270409=CARTESIAN_POINT('Ctrl Pts',(94.9701958612989,-88.8775672472035,
672.462296651428));
#270410=CARTESIAN_POINT('Ctrl Pts',(87.9753796205242,-96.351883758956,670.462296651428));
#270411=CARTESIAN_POINT('Ctrl Pts',(79.8974404698481,-102.639948694851,
668.462296651428));
#270412=CARTESIAN_POINT('Ctrl Pts',(71.8195013191721,-108.928013630747,
666.462296651428));
#270413=CARTESIAN_POINT('Ctrl Pts',(62.8573449296273,-113.874993963172,
664.462296651428));
#270414=CARTESIAN_POINT('Ctrl Pts',(53.8951885400825,-118.821974295598,
662.462296651428));
#270415=CARTESIAN_POINT('Ctrl Pts',(44.2694929456714,-122.306058950682,
660.462296651428));
#270416=CARTESIAN_POINT('Ctrl Pts',(34.6437973512603,-125.790143605767,
658.462296651428));
#270417=CARTESIAN_POINT('Ctrl Pts',(24.5915791233694,-127.725542856289,
656.462296651428));
#270418=CARTESIAN_POINT('Ctrl Pts',(14.5393608954785,-129.660942106811,
654.462296651428));
#270419=CARTESIAN_POINT('Ctrl Pts',(4.30813900827813,-130.,652.462296651428));
#270420=CARTESIAN_POINT('Ctrl Pts',(-5.92308287892227,-130.339057893189,
650.462296651428));
#270421=CARTESIAN_POINT('Ctrl Pts',(-16.0813817870906,-129.073425698447,
648.462296651428));
#270422=CARTESIAN_POINT('Ctrl Pts',(-26.2396806952589,-127.807793503705,
646.462296651428));
#270423=CARTESIAN_POINT('Ctrl Pts',(-36.0749255918149,-124.968635286058,
644.462296651428));
#270424=CARTESIAN_POINT('Ctrl Pts',(-45.9101704883709,-122.129477068411,
642.462296651428));
#270425=CARTESIAN_POINT('Ctrl Pts',(-55.1801850026549,-117.786702325803,
640.462296651428));
#270426=CARTESIAN_POINT('Ctrl Pts',(-64.4501995169389,-113.443927583196,
638.462296651428));
#270427=CARTESIAN_POINT('Ctrl Pts',(-72.9267251261949,-107.704469842635,
636.462296651428));
#270428=CARTESIAN_POINT('Ctrl Pts',(-81.4032507354509,-101.965012102074,
634.462296651428));
#270429=CARTESIAN_POINT('Ctrl Pts',(-88.8775672472034,-94.9701958612989,
632.462296651428));
#270430=CARTESIAN_POINT('Ctrl Pts',(-96.351883758956,-87.9753796205242,
630.462296651428));
#270431=CARTESIAN_POINT('Ctrl Pts',(-102.639948694851,-79.8974404698482,
628.462296651428));
#270432=CARTESIAN_POINT('Ctrl Pts',(-108.928013630747,-71.8195013191721,
626.462296651429));
#270433=CARTESIAN_POINT('Ctrl Pts',(-113.874993963172,-62.8573449296273,
624.462296651428));
#270434=CARTESIAN_POINT('Ctrl Pts',(-118.821974295598,-53.8951885400825,
622.462296651428));
#270435=CARTESIAN_POINT('Ctrl Pts',(-122.306058950682,-44.2694929456714,
620.462296651428));
#270436=CARTESIAN_POINT('Ctrl Pts',(-125.790143605767,-34.6437973512603,
618.462296651428));
#270437=CARTESIAN_POINT('Ctrl Pts',(-127.725542856289,-24.5915791233694,
616.462296651428));
#270438=CARTESIAN_POINT('Ctrl Pts',(-129.660942106811,-14.5393608954785,
614.462296651429));
#270439=CARTESIAN_POINT('Ctrl Pts',(-130.,-4.30813900827813,612.462296651428));
#270440=CARTESIAN_POINT('Ctrl Pts',(-130.339057893189,5.92308287892227,
610.462296651428));
#270441=CARTESIAN_POINT('Ctrl Pts',(-129.073425698447,16.0813817870906,
608.462296651428));
#270442=CARTESIAN_POINT('Ctrl Pts',(-127.807793503705,26.2396806952589,
606.462296651428));
#270443=CARTESIAN_POINT('Ctrl Pts',(-124.968635286058,36.0749255918149,
604.462296651428));
#270444=CARTESIAN_POINT('Ctrl Pts',(-122.129477068411,45.9101704883709,
602.462296651429));
#270445=CARTESIAN_POINT('Ctrl Pts',(-117.786702325803,55.1801850026549,
600.462296651428));
#270446=CARTESIAN_POINT('Ctrl Pts',(-113.443927583196,64.4501995169388,
598.462296651428));
#270447=CARTESIAN_POINT('Ctrl Pts',(-107.704469842635,72.9267251261949,
596.462296651428));
#270448=CARTESIAN_POINT('Ctrl Pts',(-101.965012102074,81.4032507354509,
594.462296651428));
#270449=CARTESIAN_POINT('Ctrl Pts',(-94.9701958612989,88.8775672472034,
592.462296651428));
#270450=CARTESIAN_POINT('Ctrl Pts',(-87.9753796205243,96.3518837589559,
590.462296651428));
#270451=CARTESIAN_POINT('Ctrl Pts',(-79.8974404698482,102.639948694851,
588.462296651428));
#270452=CARTESIAN_POINT('Ctrl Pts',(-71.819501319172,108.928013630747,586.462296651428));
#270453=CARTESIAN_POINT('Ctrl Pts',(-62.8573449296273,113.874993963172,
584.462296651428));
#270454=CARTESIAN_POINT('Ctrl Pts',(-53.8951885400826,118.821974295598,
582.462296651428));
#270455=CARTESIAN_POINT('Ctrl Pts',(-44.2694929456714,122.306058950682,
580.462296651428));
#270456=CARTESIAN_POINT('Ctrl Pts',(-34.6437973512603,125.790143605767,
578.462296651428));
#270457=CARTESIAN_POINT('Ctrl Pts',(-24.5915791233694,127.725542856289,
576.462296651428));
#270458=CARTESIAN_POINT('Ctrl Pts',(-14.5393608954786,129.660942106811,
574.462296651428));
#270459=CARTESIAN_POINT('Ctrl Pts',(-4.30813900827814,130.,572.462296651428));
#270460=CARTESIAN_POINT('Ctrl Pts',(5.92308287892232,130.339057893189,570.462296651428));
#270461=CARTESIAN_POINT('Ctrl Pts',(16.0813817870906,129.073425698447,568.462296651428));
#270462=CARTESIAN_POINT('Ctrl Pts',(26.2396806952589,127.807793503705,566.462296651428));
#270463=CARTESIAN_POINT('Ctrl Pts',(36.0749255918149,124.968635286058,564.462296651428));
#270464=CARTESIAN_POINT('Ctrl Pts',(45.9101704883709,122.129477068411,562.462296651428));
#270465=CARTESIAN_POINT('Ctrl Pts',(55.1801850026549,117.786702325803,560.462296651428));
#270466=CARTESIAN_POINT('Ctrl Pts',(64.4501995169388,113.443927583196,558.462296651428));
#270467=CARTESIAN_POINT('Ctrl Pts',(72.9267251261949,107.704469842635,556.462296651428));
#270468=CARTESIAN_POINT('Ctrl Pts',(81.4032507354509,101.965012102074,554.462296651428));
#270469=CARTESIAN_POINT('Ctrl Pts',(88.8775672472034,94.9701958612989,552.462296651428));
#270470=CARTESIAN_POINT('Ctrl Pts',(96.3518837589559,87.9753796205243,550.462296651428));
#270471=CARTESIAN_POINT('Ctrl Pts',(102.639948694851,79.8974404698482,548.462296651428));
#270472=CARTESIAN_POINT('Ctrl Pts',(108.928013630747,71.819501319172,546.462296651428));
#270473=CARTESIAN_POINT('Ctrl Pts',(113.874993963172,62.8573449296273,544.462296651428));
#270474=CARTESIAN_POINT('Ctrl Pts',(118.821974295598,53.8951885400826,542.462296651428));
#270475=CARTESIAN_POINT('Ctrl Pts',(122.306058950682,44.2694929456714,540.462296651428));
#270476=CARTESIAN_POINT('Ctrl Pts',(125.790143605767,34.6437973512603,538.462296651428));
#270477=CARTESIAN_POINT('Ctrl Pts',(127.725542856289,24.5915791233694,536.462296651428));
#270478=CARTESIAN_POINT('Ctrl Pts',(129.660942106811,14.5393608954786,534.462296651428));
#270479=CARTESIAN_POINT('Ctrl Pts',(130.,4.30813900827812,532.462296651428));
#270480=CARTESIAN_POINT('Ctrl Pts',(129.869812400585,-7.23822414350117,
696.964207537011));
#270481=CARTESIAN_POINT('Ctrl Pts',(129.382196958681,-15.9871278397999,
695.249654101829));
#270482=CARTESIAN_POINT('Ctrl Pts',(127.725542856289,-24.5915791233694,
693.537703348572));
#270483=CARTESIAN_POINT('Ctrl Pts',(125.790143605767,-34.6437973512603,
691.537703348572));
#270484=CARTESIAN_POINT('Ctrl Pts',(122.306058950682,-44.2694929456714,
689.537703348572));
#270485=CARTESIAN_POINT('Ctrl Pts',(118.821974295598,-53.8951885400825,
687.537703348572));
#270486=CARTESIAN_POINT('Ctrl Pts',(113.874993963172,-62.8573449296272,
685.537703348572));
#270487=CARTESIAN_POINT('Ctrl Pts',(108.928013630747,-71.819501319172,683.537703348572));
#270488=CARTESIAN_POINT('Ctrl Pts',(102.639948694851,-79.8974404698481,
681.537703348572));
#270489=CARTESIAN_POINT('Ctrl Pts',(96.351883758956,-87.9753796205242,679.537703348572));
#270490=CARTESIAN_POINT('Ctrl Pts',(88.8775672472035,-94.9701958612989,
677.537703348572));
#270491=CARTESIAN_POINT('Ctrl Pts',(81.403250735451,-101.965012102074,675.537703348572));
#270492=CARTESIAN_POINT('Ctrl Pts',(72.9267251261949,-107.704469842635,
673.537703348572));
#270493=CARTESIAN_POINT('Ctrl Pts',(64.4501995169389,-113.443927583196,
671.537703348572));
#270494=CARTESIAN_POINT('Ctrl Pts',(55.1801850026549,-117.786702325803,
669.537703348572));
#270495=CARTESIAN_POINT('Ctrl Pts',(45.910170488371,-122.129477068411,667.537703348572));
#270496=CARTESIAN_POINT('Ctrl Pts',(36.074925591815,-124.968635286058,665.537703348572));
#270497=CARTESIAN_POINT('Ctrl Pts',(26.239680695259,-127.807793503704,663.537703348572));
#270498=CARTESIAN_POINT('Ctrl Pts',(16.0813817870907,-129.073425698447,
661.537703348572));
#270499=CARTESIAN_POINT('Ctrl Pts',(5.92308287892234,-130.339057893189,
659.537703348572));
#270500=CARTESIAN_POINT('Ctrl Pts',(-4.30813900827806,-130.,657.537703348572));
#270501=CARTESIAN_POINT('Ctrl Pts',(-14.5393608954785,-129.660942106811,
655.537703348572));
#270502=CARTESIAN_POINT('Ctrl Pts',(-24.5915791233694,-127.725542856289,
653.537703348572));
#270503=CARTESIAN_POINT('Ctrl Pts',(-34.6437973512602,-125.790143605767,
651.537703348572));
#270504=CARTESIAN_POINT('Ctrl Pts',(-44.2694929456713,-122.306058950682,
649.537703348572));
#270505=CARTESIAN_POINT('Ctrl Pts',(-53.8951885400825,-118.821974295598,
647.537703348572));
#270506=CARTESIAN_POINT('Ctrl Pts',(-62.8573449296272,-113.874993963172,
645.537703348572));
#270507=CARTESIAN_POINT('Ctrl Pts',(-71.819501319172,-108.928013630747,
643.537703348572));
#270508=CARTESIAN_POINT('Ctrl Pts',(-79.8974404698481,-102.639948694851,
641.537703348572));
#270509=CARTESIAN_POINT('Ctrl Pts',(-87.9753796205242,-96.351883758956,
639.537703348572));
#270510=CARTESIAN_POINT('Ctrl Pts',(-94.9701958612989,-88.8775672472035,
637.537703348572));
#270511=CARTESIAN_POINT('Ctrl Pts',(-101.965012102074,-81.403250735451,
635.537703348572));
#270512=CARTESIAN_POINT('Ctrl Pts',(-107.704469842635,-72.9267251261949,
633.537703348572));
#270513=CARTESIAN_POINT('Ctrl Pts',(-113.443927583196,-64.4501995169389,
631.537703348572));
#270514=CARTESIAN_POINT('Ctrl Pts',(-117.786702325803,-55.1801850026549,
629.537703348572));
#270515=CARTESIAN_POINT('Ctrl Pts',(-122.129477068411,-45.910170488371,
627.537703348572));
#270516=CARTESIAN_POINT('Ctrl Pts',(-124.968635286058,-36.074925591815,
625.537703348572));
#270517=CARTESIAN_POINT('Ctrl Pts',(-127.807793503704,-26.239680695259,
623.537703348572));
#270518=CARTESIAN_POINT('Ctrl Pts',(-129.073425698447,-16.0813817870907,
621.537703348572));
#270519=CARTESIAN_POINT('Ctrl Pts',(-130.339057893189,-5.92308287892235,
619.537703348572));
#270520=CARTESIAN_POINT('Ctrl Pts',(-130.,4.30813900827805,617.537703348572));
#270521=CARTESIAN_POINT('Ctrl Pts',(-129.660942106811,14.5393608954784,
615.537703348572));
#270522=CARTESIAN_POINT('Ctrl Pts',(-127.725542856289,24.5915791233693,
613.537703348572));
#270523=CARTESIAN_POINT('Ctrl Pts',(-125.790143605767,34.6437973512602,
611.537703348572));
#270524=CARTESIAN_POINT('Ctrl Pts',(-122.306058950682,44.2694929456713,
609.537703348572));
#270525=CARTESIAN_POINT('Ctrl Pts',(-118.821974295598,53.8951885400825,
607.537703348572));
#270526=CARTESIAN_POINT('Ctrl Pts',(-113.874993963172,62.8573449296272,
605.537703348572));
#270527=CARTESIAN_POINT('Ctrl Pts',(-108.928013630747,71.819501319172,603.537703348572));
#270528=CARTESIAN_POINT('Ctrl Pts',(-102.639948694851,79.8974404698481,
601.537703348572));
#270529=CARTESIAN_POINT('Ctrl Pts',(-96.3518837589561,87.9753796205242,
599.537703348572));
#270530=CARTESIAN_POINT('Ctrl Pts',(-88.8775672472035,94.9701958612989,
597.537703348572));
#270531=CARTESIAN_POINT('Ctrl Pts',(-81.403250735451,101.965012102074,595.537703348572));
#270532=CARTESIAN_POINT('Ctrl Pts',(-72.9267251261949,107.704469842635,
593.537703348572));
#270533=CARTESIAN_POINT('Ctrl Pts',(-64.4501995169389,113.443927583196,
591.537703348572));
#270534=CARTESIAN_POINT('Ctrl Pts',(-55.1801850026549,117.786702325803,
589.537703348572));
#270535=CARTESIAN_POINT('Ctrl Pts',(-45.910170488371,122.129477068411,587.537703348572));
#270536=CARTESIAN_POINT('Ctrl Pts',(-36.074925591815,124.968635286058,585.537703348572));
#270537=CARTESIAN_POINT('Ctrl Pts',(-26.239680695259,127.807793503704,583.537703348572));
#270538=CARTESIAN_POINT('Ctrl Pts',(-16.0813817870907,129.073425698447,
581.537703348572));
#270539=CARTESIAN_POINT('Ctrl Pts',(-5.92308287892242,130.339057893189,
579.537703348572));
#270540=CARTESIAN_POINT('Ctrl Pts',(4.30813900827804,130.,577.537703348572));
#270541=CARTESIAN_POINT('Ctrl Pts',(14.5393608954785,129.660942106811,575.537703348572));
#270542=CARTESIAN_POINT('Ctrl Pts',(24.5915791233693,127.725542856289,573.537703348572));
#270543=CARTESIAN_POINT('Ctrl Pts',(34.6437973512602,125.790143605767,571.537703348572));
#270544=CARTESIAN_POINT('Ctrl Pts',(44.2694929456713,122.306058950682,569.537703348572));
#270545=CARTESIAN_POINT('Ctrl Pts',(53.8951885400825,118.821974295598,567.537703348572));
#270546=CARTESIAN_POINT('Ctrl Pts',(62.8573449296272,113.874993963172,565.537703348572));
#270547=CARTESIAN_POINT('Ctrl Pts',(71.819501319172,108.928013630747,563.537703348572));
#270548=CARTESIAN_POINT('Ctrl Pts',(79.8974404698481,102.639948694851,561.537703348572));
#270549=CARTESIAN_POINT('Ctrl Pts',(87.9753796205242,96.351883758956,559.537703348572));
#270550=CARTESIAN_POINT('Ctrl Pts',(94.9701958612989,88.8775672472035,557.537703348572));
#270551=CARTESIAN_POINT('Ctrl Pts',(101.965012102074,81.403250735451,555.537703348572));
#270552=CARTESIAN_POINT('Ctrl Pts',(107.704469842635,72.926725126195,553.537703348572));
#270553=CARTESIAN_POINT('Ctrl Pts',(113.443927583196,64.4501995169389,551.537703348572));
#270554=CARTESIAN_POINT('Ctrl Pts',(117.786702325803,55.1801850026549,549.537703348572));
#270555=CARTESIAN_POINT('Ctrl Pts',(122.129477068411,45.910170488371,547.537703348572));
#270556=CARTESIAN_POINT('Ctrl Pts',(124.968635286058,36.074925591815,545.537703348572));
#270557=CARTESIAN_POINT('Ctrl Pts',(127.807793503704,26.239680695259,543.537703348572));
#270558=CARTESIAN_POINT('Ctrl Pts',(129.073425698447,16.0813817870907,541.537703348572));
#270559=CARTESIAN_POINT('Ctrl Pts',(129.701667605591,11.0389459941988,540.54493165747));
#270560=CARTESIAN_POINT('Ctrl Pts',(129.934615416877,5.96286660784701,539.549090218607));
#270561=CARTESIAN_POINT('Ctrl Pts',(160.,-4.30813900827805,697.537703348572));
#270562=CARTESIAN_POINT('Ctrl Pts',(159.660942106811,-16.900412100217,695.537703348572));
#270563=CARTESIAN_POINT('Ctrl Pts',(157.356193074143,-29.2846130745763,
693.537703348572));
#270564=CARTESIAN_POINT('Ctrl Pts',(155.051444041475,-41.6688140489355,
691.537703348572));
#270565=CARTESIAN_POINT('Ctrl Pts',(150.837754439537,-53.5400027769198,
689.537703348572));
#270566=CARTESIAN_POINT('Ctrl Pts',(146.624064837599,-65.411191504904,687.537703348572));
#270567=CARTESIAN_POINT('Ctrl Pts',(140.605189688823,-76.4770599218136,
685.537703348572));
#270568=CARTESIAN_POINT('Ctrl Pts',(134.586314540048,-87.5429283387233,
683.537703348572));
#270569=CARTESIAN_POINT('Ctrl Pts',(126.9104585261,-97.5309980386223,681.537703348572));
#270570=CARTESIAN_POINT('Ctrl Pts',(119.234602512152,-107.519067738521,
679.537703348572));
#270571=CARTESIAN_POINT('Ctrl Pts',(110.0907706828,-116.183399296895,677.537703348572));
#270572=CARTESIAN_POINT('Ctrl Pts',(100.946938853448,-124.847730855269,
675.537703348572));
#270573=CARTESIAN_POINT('Ctrl Pts',(90.5602826949691,-131.974979673883,
673.537703348572));
#270574=CARTESIAN_POINT('Ctrl Pts',(80.1736265364902,-139.102228492497,
671.537703348572));
#270575=CARTESIAN_POINT('Ctrl Pts',(68.7998999948414,-144.516898051454,
669.537703348572));
#270576=CARTESIAN_POINT('Ctrl Pts',(57.4261734531925,-149.931567610412,
667.537703348572));
#270577=CARTESIAN_POINT('Ctrl Pts',(45.3454354230634,-153.500330774912,
665.537703348572));
#270578=CARTESIAN_POINT('Ctrl Pts',(33.2646973929343,-157.069093939413,
663.537703348572));
#270579=CARTESIAN_POINT('Ctrl Pts',(20.7744157382976,-158.704075916301,
661.537703348572));
#270580=CARTESIAN_POINT('Ctrl Pts',(8.28413408366091,-160.339057893189,
659.537703348572));
#270581=CARTESIAN_POINT('Ctrl Pts',(-4.30813900827804,-160.,657.537703348572));
#270582=CARTESIAN_POINT('Ctrl Pts',(-16.900412100217,-159.660942106811,
655.537703348572));
#270583=CARTESIAN_POINT('Ctrl Pts',(-29.2846130745763,-157.356193074143,
653.537703348572));
#270584=CARTESIAN_POINT('Ctrl Pts',(-41.6688140489355,-155.051444041475,
651.537703348572));
#270585=CARTESIAN_POINT('Ctrl Pts',(-53.5400027769198,-150.837754439537,
649.537703348572));
#270586=CARTESIAN_POINT('Ctrl Pts',(-65.411191504904,-146.624064837599,
647.537703348572));
#270587=CARTESIAN_POINT('Ctrl Pts',(-76.4770599218136,-140.605189688823,
645.537703348572));
#270588=CARTESIAN_POINT('Ctrl Pts',(-87.5429283387233,-134.586314540048,
643.537703348572));
#270589=CARTESIAN_POINT('Ctrl Pts',(-97.5309980386223,-126.9104585261,641.537703348572));
#270590=CARTESIAN_POINT('Ctrl Pts',(-107.519067738521,-119.234602512152,
639.537703348572));
#270591=CARTESIAN_POINT('Ctrl Pts',(-116.183399296895,-110.0907706828,637.537703348572));
#270592=CARTESIAN_POINT('Ctrl Pts',(-124.847730855269,-100.946938853448,
635.537703348572));
#270593=CARTESIAN_POINT('Ctrl Pts',(-131.974979673883,-90.5602826949692,
633.537703348572));
#270594=CARTESIAN_POINT('Ctrl Pts',(-139.102228492497,-80.1736265364902,
631.537703348572));
#270595=CARTESIAN_POINT('Ctrl Pts',(-144.516898051454,-68.7998999948414,
629.537703348572));
#270596=CARTESIAN_POINT('Ctrl Pts',(-149.931567610412,-57.4261734531925,
627.537703348572));
#270597=CARTESIAN_POINT('Ctrl Pts',(-153.500330774912,-45.3454354230634,
625.537703348572));
#270598=CARTESIAN_POINT('Ctrl Pts',(-157.069093939413,-33.2646973929344,
623.537703348572));
#270599=CARTESIAN_POINT('Ctrl Pts',(-158.704075916301,-20.7744157382976,
621.537703348572));
#270600=CARTESIAN_POINT('Ctrl Pts',(-160.339057893189,-8.28413408366092,
619.537703348572));
#270601=CARTESIAN_POINT('Ctrl Pts',(-160.,4.30813900827803,617.537703348572));
#270602=CARTESIAN_POINT('Ctrl Pts',(-159.660942106811,16.900412100217,615.537703348572));
#270603=CARTESIAN_POINT('Ctrl Pts',(-157.356193074143,29.2846130745763,
613.537703348572));
#270604=CARTESIAN_POINT('Ctrl Pts',(-155.051444041475,41.6688140489355,
611.537703348572));
#270605=CARTESIAN_POINT('Ctrl Pts',(-150.837754439537,53.5400027769198,
609.537703348572));
#270606=CARTESIAN_POINT('Ctrl Pts',(-146.624064837599,65.411191504904,607.537703348572));
#270607=CARTESIAN_POINT('Ctrl Pts',(-140.605189688823,76.4770599218136,
605.537703348572));
#270608=CARTESIAN_POINT('Ctrl Pts',(-134.586314540048,87.5429283387233,
603.537703348572));
#270609=CARTESIAN_POINT('Ctrl Pts',(-126.9104585261,97.5309980386223,601.537703348572));
#270610=CARTESIAN_POINT('Ctrl Pts',(-119.234602512152,107.519067738521,
599.537703348572));
#270611=CARTESIAN_POINT('Ctrl Pts',(-110.0907706828,116.183399296895,597.537703348572));
#270612=CARTESIAN_POINT('Ctrl Pts',(-100.946938853448,124.847730855269,
595.537703348572));
#270613=CARTESIAN_POINT('Ctrl Pts',(-90.5602826949692,131.974979673883,
593.537703348572));
#270614=CARTESIAN_POINT('Ctrl Pts',(-80.1736265364901,139.102228492497,
591.537703348572));
#270615=CARTESIAN_POINT('Ctrl Pts',(-68.7998999948414,144.516898051454,
589.537703348572));
#270616=CARTESIAN_POINT('Ctrl Pts',(-57.4261734531926,149.931567610412,
587.537703348572));
#270617=CARTESIAN_POINT('Ctrl Pts',(-45.3454354230634,153.500330774912,
585.537703348572));
#270618=CARTESIAN_POINT('Ctrl Pts',(-33.2646973929343,157.069093939413,
583.537703348572));
#270619=CARTESIAN_POINT('Ctrl Pts',(-20.7744157382976,158.704075916301,
581.537703348572));
#270620=CARTESIAN_POINT('Ctrl Pts',(-8.284134083661,160.339057893189,579.537703348572));
#270621=CARTESIAN_POINT('Ctrl Pts',(4.30813900827803,160.,577.537703348572));
#270622=CARTESIAN_POINT('Ctrl Pts',(16.9004121002171,159.660942106811,575.537703348572));
#270623=CARTESIAN_POINT('Ctrl Pts',(29.2846130745762,157.356193074143,573.537703348572));
#270624=CARTESIAN_POINT('Ctrl Pts',(41.6688140489354,155.051444041476,571.537703348572));
#270625=CARTESIAN_POINT('Ctrl Pts',(53.5400027769198,150.837754439537,569.537703348572));
#270626=CARTESIAN_POINT('Ctrl Pts',(65.4111915049041,146.624064837599,567.537703348572));
#270627=CARTESIAN_POINT('Ctrl Pts',(76.4770599218136,140.605189688823,565.537703348572));
#270628=CARTESIAN_POINT('Ctrl Pts',(87.5429283387232,134.586314540048,563.537703348572));
#270629=CARTESIAN_POINT('Ctrl Pts',(97.5309980386223,126.9104585261,561.537703348572));
#270630=CARTESIAN_POINT('Ctrl Pts',(107.519067738521,119.234602512152,559.537703348572));
#270631=CARTESIAN_POINT('Ctrl Pts',(116.183399296895,110.0907706828,557.537703348572));
#270632=CARTESIAN_POINT('Ctrl Pts',(124.847730855269,100.946938853448,555.537703348572));
#270633=CARTESIAN_POINT('Ctrl Pts',(131.974979673883,90.5602826949692,553.537703348572));
#270634=CARTESIAN_POINT('Ctrl Pts',(139.102228492497,80.1736265364902,551.537703348572));
#270635=CARTESIAN_POINT('Ctrl Pts',(144.516898051454,68.7998999948414,549.537703348572));
#270636=CARTESIAN_POINT('Ctrl Pts',(149.931567610412,57.4261734531926,547.537703348572));
#270637=CARTESIAN_POINT('Ctrl Pts',(153.500330774912,45.3454354230634,545.537703348572));
#270638=CARTESIAN_POINT('Ctrl Pts',(157.069093939413,33.2646973929343,543.537703348572));
#270639=CARTESIAN_POINT('Ctrl Pts',(158.704075916301,20.7744157382976,541.537703348572));
#270640=CARTESIAN_POINT('Ctrl Pts',(160.339057893189,8.28413408366101,539.537703348572));
#270641=CARTESIAN_POINT('Ctrl Pts',(160.,-4.30813900827805,537.537703348572));
#270642=CARTESIAN_POINT('Ctrl Pts',(130.,-4.30813900827807,697.537703348572));
#270643=CARTESIAN_POINT('Ctrl Pts',(129.660942106811,-14.5393608954785,
695.537703348572));
#270644=CARTESIAN_POINT('Ctrl Pts',(127.725542856289,-24.5915791233694,
693.537703348572));
#270645=CARTESIAN_POINT('Ctrl Pts',(125.790143605767,-34.6437973512603,
691.537703348572));
#270646=CARTESIAN_POINT('Ctrl Pts',(122.306058950682,-44.2694929456714,
689.537703348572));
#270647=CARTESIAN_POINT('Ctrl Pts',(118.821974295598,-53.8951885400825,
687.537703348572));
#270648=CARTESIAN_POINT('Ctrl Pts',(113.874993963172,-62.8573449296272,
685.537703348572));
#270649=CARTESIAN_POINT('Ctrl Pts',(108.928013630747,-71.819501319172,683.537703348572));
#270650=CARTESIAN_POINT('Ctrl Pts',(102.639948694851,-79.8974404698481,
681.537703348572));
#270651=CARTESIAN_POINT('Ctrl Pts',(96.351883758956,-87.9753796205242,679.537703348572));
#270652=CARTESIAN_POINT('Ctrl Pts',(88.8775672472035,-94.9701958612989,
677.537703348572));
#270653=CARTESIAN_POINT('Ctrl Pts',(81.403250735451,-101.965012102074,675.537703348572));
#270654=CARTESIAN_POINT('Ctrl Pts',(72.9267251261949,-107.704469842635,
673.537703348572));
#270655=CARTESIAN_POINT('Ctrl Pts',(64.4501995169389,-113.443927583196,
671.537703348572));
#270656=CARTESIAN_POINT('Ctrl Pts',(55.1801850026549,-117.786702325803,
669.537703348572));
#270657=CARTESIAN_POINT('Ctrl Pts',(45.910170488371,-122.129477068411,667.537703348572));
#270658=CARTESIAN_POINT('Ctrl Pts',(36.074925591815,-124.968635286058,665.537703348572));
#270659=CARTESIAN_POINT('Ctrl Pts',(26.239680695259,-127.807793503704,663.537703348572));
#270660=CARTESIAN_POINT('Ctrl Pts',(16.0813817870907,-129.073425698447,
661.537703348572));
#270661=CARTESIAN_POINT('Ctrl Pts',(5.92308287892234,-130.339057893189,
659.537703348572));
#270662=CARTESIAN_POINT('Ctrl Pts',(-4.30813900827806,-130.,657.537703348572));
#270663=CARTESIAN_POINT('Ctrl Pts',(-14.5393608954785,-129.660942106811,
655.537703348572));
#270664=CARTESIAN_POINT('Ctrl Pts',(-24.5915791233694,-127.725542856289,
653.537703348572));
#270665=CARTESIAN_POINT('Ctrl Pts',(-34.6437973512603,-125.790143605767,
651.537703348572));
#270666=CARTESIAN_POINT('Ctrl Pts',(-44.2694929456713,-122.306058950682,
649.537703348572));
#270667=CARTESIAN_POINT('Ctrl Pts',(-53.8951885400825,-118.821974295598,
647.537703348572));
#270668=CARTESIAN_POINT('Ctrl Pts',(-62.8573449296272,-113.874993963172,
645.537703348572));
#270669=CARTESIAN_POINT('Ctrl Pts',(-71.819501319172,-108.928013630747,
643.537703348572));
#270670=CARTESIAN_POINT('Ctrl Pts',(-79.8974404698481,-102.639948694851,
641.537703348572));
#270671=CARTESIAN_POINT('Ctrl Pts',(-87.9753796205242,-96.351883758956,
639.537703348572));
#270672=CARTESIAN_POINT('Ctrl Pts',(-94.9701958612989,-88.8775672472035,
637.537703348572));
#270673=CARTESIAN_POINT('Ctrl Pts',(-101.965012102074,-81.403250735451,
635.537703348572));
#270674=CARTESIAN_POINT('Ctrl Pts',(-107.704469842635,-72.9267251261949,
633.537703348572));
#270675=CARTESIAN_POINT('Ctrl Pts',(-113.443927583196,-64.4501995169389,
631.537703348572));
#270676=CARTESIAN_POINT('Ctrl Pts',(-117.786702325803,-55.1801850026549,
629.537703348572));
#270677=CARTESIAN_POINT('Ctrl Pts',(-122.129477068411,-45.910170488371,
627.537703348572));
#270678=CARTESIAN_POINT('Ctrl Pts',(-124.968635286058,-36.074925591815,
625.537703348572));
#270679=CARTESIAN_POINT('Ctrl Pts',(-127.807793503704,-26.239680695259,
623.537703348572));
#270680=CARTESIAN_POINT('Ctrl Pts',(-129.073425698447,-16.0813817870907,
621.537703348572));
#270681=CARTESIAN_POINT('Ctrl Pts',(-130.339057893189,-5.92308287892235,
619.537703348572));
#270682=CARTESIAN_POINT('Ctrl Pts',(-130.,4.30813900827805,617.537703348572));
#270683=CARTESIAN_POINT('Ctrl Pts',(-129.660942106811,14.5393608954784,
615.537703348572));
#270684=CARTESIAN_POINT('Ctrl Pts',(-127.725542856289,24.5915791233693,
613.537703348572));
#270685=CARTESIAN_POINT('Ctrl Pts',(-125.790143605767,34.6437973512602,
611.537703348572));
#270686=CARTESIAN_POINT('Ctrl Pts',(-122.306058950682,44.2694929456713,
609.537703348572));
#270687=CARTESIAN_POINT('Ctrl Pts',(-118.821974295598,53.8951885400825,
607.537703348572));
#270688=CARTESIAN_POINT('Ctrl Pts',(-113.874993963172,62.8573449296272,
605.537703348572));
#270689=CARTESIAN_POINT('Ctrl Pts',(-108.928013630747,71.819501319172,603.537703348572));
#270690=CARTESIAN_POINT('Ctrl Pts',(-102.639948694851,79.8974404698481,
601.537703348572));
#270691=CARTESIAN_POINT('Ctrl Pts',(-96.3518837589561,87.9753796205242,
599.537703348572));
#270692=CARTESIAN_POINT('Ctrl Pts',(-88.8775672472035,94.9701958612989,
597.537703348572));
#270693=CARTESIAN_POINT('Ctrl Pts',(-81.403250735451,101.965012102074,595.537703348572));
#270694=CARTESIAN_POINT('Ctrl Pts',(-72.9267251261949,107.704469842635,
593.537703348572));
#270695=CARTESIAN_POINT('Ctrl Pts',(-64.4501995169389,113.443927583196,
591.537703348572));
#270696=CARTESIAN_POINT('Ctrl Pts',(-55.1801850026549,117.786702325803,
589.537703348572));
#270697=CARTESIAN_POINT('Ctrl Pts',(-45.910170488371,122.129477068411,587.537703348572));
#270698=CARTESIAN_POINT('Ctrl Pts',(-36.074925591815,124.968635286058,585.537703348572));
#270699=CARTESIAN_POINT('Ctrl Pts',(-26.239680695259,127.807793503704,583.537703348572));
#270700=CARTESIAN_POINT('Ctrl Pts',(-16.0813817870907,129.073425698447,
581.537703348572));
#270701=CARTESIAN_POINT('Ctrl Pts',(-5.92308287892242,130.339057893189,
579.537703348572));
#270702=CARTESIAN_POINT('Ctrl Pts',(4.30813900827804,130.,577.537703348572));
#270703=CARTESIAN_POINT('Ctrl Pts',(14.5393608954785,129.660942106811,575.537703348572));
#270704=CARTESIAN_POINT('Ctrl Pts',(24.5915791233693,127.725542856289,573.537703348572));
#270705=CARTESIAN_POINT('Ctrl Pts',(34.6437973512602,125.790143605767,571.537703348572));
#270706=CARTESIAN_POINT('Ctrl Pts',(44.2694929456713,122.306058950682,569.537703348572));
#270707=CARTESIAN_POINT('Ctrl Pts',(53.8951885400825,118.821974295598,567.537703348572));
#270708=CARTESIAN_POINT('Ctrl Pts',(62.8573449296272,113.874993963172,565.537703348572));
#270709=CARTESIAN_POINT('Ctrl Pts',(71.819501319172,108.928013630747,563.537703348572));
#270710=CARTESIAN_POINT('Ctrl Pts',(79.8974404698481,102.639948694851,561.537703348572));
#270711=CARTESIAN_POINT('Ctrl Pts',(87.9753796205242,96.351883758956,559.537703348572));
#270712=CARTESIAN_POINT('Ctrl Pts',(94.9701958612989,88.8775672472035,557.537703348572));
#270713=CARTESIAN_POINT('Ctrl Pts',(101.965012102074,81.403250735451,555.537703348572));
#270714=CARTESIAN_POINT('Ctrl Pts',(107.704469842635,72.926725126195,553.537703348572));
#270715=CARTESIAN_POINT('Ctrl Pts',(113.443927583196,64.4501995169389,551.537703348572));
#270716=CARTESIAN_POINT('Ctrl Pts',(117.786702325803,55.1801850026549,549.537703348572));
#270717=CARTESIAN_POINT('Ctrl Pts',(122.129477068411,45.910170488371,547.537703348572));
#270718=CARTESIAN_POINT('Ctrl Pts',(124.968635286058,36.074925591815,545.537703348572));
#270719=CARTESIAN_POINT('Ctrl Pts',(127.807793503704,26.239680695259,543.537703348572));
#270720=CARTESIAN_POINT('Ctrl Pts',(129.073425698447,16.0813817870907,541.537703348572));
#270721=CARTESIAN_POINT('Ctrl Pts',(130.339057893189,5.92308287892242,539.537703348572));
#270722=CARTESIAN_POINT('Ctrl Pts',(130.,-4.30813900827807,537.537703348572));
#270723=CARTESIAN_POINT('Ctrl Pts',(130.,-4.30813900827807,537.537703348572));
#270724=CARTESIAN_POINT('Ctrl Pts',(129.660942106811,-14.5393608954785,
535.537703348572));
#270725=CARTESIAN_POINT('Ctrl Pts',(127.725542856289,-24.5915791233694,
533.537703348572));
#270726=CARTESIAN_POINT('Ctrl Pts',(125.790143605767,-34.6437973512603,
531.537703348572));
#270727=CARTESIAN_POINT('Ctrl Pts',(122.306058950682,-44.2694929456714,
529.537703348572));
#270728=CARTESIAN_POINT('Ctrl Pts',(118.821974295598,-53.8951885400825,
527.537703348572));
#270729=CARTESIAN_POINT('Ctrl Pts',(113.874993963172,-62.8573449296272,
525.537703348572));
#270730=CARTESIAN_POINT('Ctrl Pts',(108.928013630747,-71.819501319172,523.537703348572));
#270731=CARTESIAN_POINT('Ctrl Pts',(102.639948694851,-79.8974404698481,
521.537703348572));
#270732=CARTESIAN_POINT('Ctrl Pts',(96.351883758956,-87.9753796205242,519.537703348572));
#270733=CARTESIAN_POINT('Ctrl Pts',(88.8775672472035,-94.9701958612989,
517.537703348572));
#270734=CARTESIAN_POINT('Ctrl Pts',(81.403250735451,-101.965012102074,515.537703348572));
#270735=CARTESIAN_POINT('Ctrl Pts',(72.9267251261949,-107.704469842635,
513.537703348572));
#270736=CARTESIAN_POINT('Ctrl Pts',(64.4501995169389,-113.443927583196,
511.537703348572));
#270737=CARTESIAN_POINT('Ctrl Pts',(55.1801850026549,-117.786702325803,
509.537703348572));
#270738=CARTESIAN_POINT('Ctrl Pts',(45.910170488371,-122.129477068411,507.537703348572));
#270739=CARTESIAN_POINT('Ctrl Pts',(36.074925591815,-124.968635286058,505.537703348572));
#270740=CARTESIAN_POINT('Ctrl Pts',(26.239680695259,-127.807793503704,503.537703348572));
#270741=CARTESIAN_POINT('Ctrl Pts',(16.0813817870907,-129.073425698447,
501.537703348572));
#270742=CARTESIAN_POINT('Ctrl Pts',(5.92308287892234,-130.339057893189,
499.537703348572));
#270743=CARTESIAN_POINT('Ctrl Pts',(-4.30813900827806,-130.,497.537703348572));
#270744=CARTESIAN_POINT('Ctrl Pts',(-14.5393608954785,-129.660942106811,
495.537703348572));
#270745=CARTESIAN_POINT('Ctrl Pts',(-24.5915791233694,-127.725542856289,
493.537703348572));
#270746=CARTESIAN_POINT('Ctrl Pts',(-34.6437973512603,-125.790143605767,
491.537703348572));
#270747=CARTESIAN_POINT('Ctrl Pts',(-44.2694929456713,-122.306058950682,
489.537703348572));
#270748=CARTESIAN_POINT('Ctrl Pts',(-53.8951885400825,-118.821974295598,
487.537703348572));
#270749=CARTESIAN_POINT('Ctrl Pts',(-62.8573449296272,-113.874993963172,
485.537703348572));
#270750=CARTESIAN_POINT('Ctrl Pts',(-71.819501319172,-108.928013630747,
483.537703348572));
#270751=CARTESIAN_POINT('Ctrl Pts',(-79.8974404698481,-102.639948694851,
481.537703348572));
#270752=CARTESIAN_POINT('Ctrl Pts',(-87.9753796205242,-96.351883758956,
479.537703348572));
#270753=CARTESIAN_POINT('Ctrl Pts',(-94.9701958612989,-88.8775672472035,
477.537703348572));
#270754=CARTESIAN_POINT('Ctrl Pts',(-101.965012102074,-81.403250735451,
475.537703348572));
#270755=CARTESIAN_POINT('Ctrl Pts',(-107.704469842635,-72.9267251261949,
473.537703348572));
#270756=CARTESIAN_POINT('Ctrl Pts',(-113.443927583196,-64.4501995169389,
471.537703348572));
#270757=CARTESIAN_POINT('Ctrl Pts',(-117.786702325803,-55.1801850026549,
469.537703348572));
#270758=CARTESIAN_POINT('Ctrl Pts',(-122.129477068411,-45.910170488371,
467.537703348572));
#270759=CARTESIAN_POINT('Ctrl Pts',(-124.968635286058,-36.074925591815,
465.537703348572));
#270760=CARTESIAN_POINT('Ctrl Pts',(-127.807793503704,-26.239680695259,
463.537703348572));
#270761=CARTESIAN_POINT('Ctrl Pts',(-129.073425698447,-16.0813817870907,
461.537703348572));
#270762=CARTESIAN_POINT('Ctrl Pts',(-130.339057893189,-5.92308287892235,
459.537703348572));
#270763=CARTESIAN_POINT('Ctrl Pts',(-130.,4.30813900827805,457.537703348572));
#270764=CARTESIAN_POINT('Ctrl Pts',(-129.660942106811,14.5393608954784,
455.537703348572));
#270765=CARTESIAN_POINT('Ctrl Pts',(-127.725542856289,24.5915791233693,
453.537703348572));
#270766=CARTESIAN_POINT('Ctrl Pts',(-125.790143605767,34.6437973512602,
451.537703348572));
#270767=CARTESIAN_POINT('Ctrl Pts',(-122.306058950682,44.2694929456713,
449.537703348572));
#270768=CARTESIAN_POINT('Ctrl Pts',(-118.821974295598,53.8951885400825,
447.537703348572));
#270769=CARTESIAN_POINT('Ctrl Pts',(-113.874993963172,62.8573449296272,
445.537703348572));
#270770=CARTESIAN_POINT('Ctrl Pts',(-108.928013630747,71.819501319172,443.537703348572));
#270771=CARTESIAN_POINT('Ctrl Pts',(-102.639948694851,79.8974404698481,
441.537703348572));
#270772=CARTESIAN_POINT('Ctrl Pts',(-96.3518837589561,87.9753796205242,
439.537703348572));
#270773=CARTESIAN_POINT('Ctrl Pts',(-88.8775672472035,94.9701958612989,
437.537703348572));
#270774=CARTESIAN_POINT('Ctrl Pts',(-81.403250735451,101.965012102074,435.537703348572));
#270775=CARTESIAN_POINT('Ctrl Pts',(-72.9267251261949,107.704469842635,
433.537703348572));
#270776=CARTESIAN_POINT('Ctrl Pts',(-64.4501995169389,113.443927583196,
431.537703348572));
#270777=CARTESIAN_POINT('Ctrl Pts',(-55.1801850026549,117.786702325803,
429.537703348572));
#270778=CARTESIAN_POINT('Ctrl Pts',(-45.910170488371,122.129477068411,427.537703348572));
#270779=CARTESIAN_POINT('Ctrl Pts',(-36.074925591815,124.968635286058,425.537703348572));
#270780=CARTESIAN_POINT('Ctrl Pts',(-26.239680695259,127.807793503704,423.537703348572));
#270781=CARTESIAN_POINT('Ctrl Pts',(-16.0813817870907,129.073425698447,
421.537703348572));
#270782=CARTESIAN_POINT('Ctrl Pts',(-5.92308287892242,130.339057893189,
419.537703348572));
#270783=CARTESIAN_POINT('Ctrl Pts',(4.30813900827804,130.,417.537703348572));
#270784=CARTESIAN_POINT('Ctrl Pts',(14.5393608954785,129.660942106811,415.537703348572));
#270785=CARTESIAN_POINT('Ctrl Pts',(24.5915791233693,127.725542856289,413.537703348572));
#270786=CARTESIAN_POINT('Ctrl Pts',(34.6437973512602,125.790143605767,411.537703348572));
#270787=CARTESIAN_POINT('Ctrl Pts',(44.2694929456713,122.306058950682,409.537703348572));
#270788=CARTESIAN_POINT('Ctrl Pts',(53.8951885400825,118.821974295598,407.537703348572));
#270789=CARTESIAN_POINT('Ctrl Pts',(62.8573449296272,113.874993963172,405.537703348572));
#270790=CARTESIAN_POINT('Ctrl Pts',(71.819501319172,108.928013630747,403.537703348572));
#270791=CARTESIAN_POINT('Ctrl Pts',(79.8974404698481,102.639948694851,401.537703348572));
#270792=CARTESIAN_POINT('Ctrl Pts',(87.9753796205242,96.351883758956,399.537703348572));
#270793=CARTESIAN_POINT('Ctrl Pts',(94.9701958612989,88.8775672472035,397.537703348572));
#270794=CARTESIAN_POINT('Ctrl Pts',(101.965012102074,81.403250735451,395.537703348572));
#270795=CARTESIAN_POINT('Ctrl Pts',(107.704469842635,72.926725126195,393.537703348572));
#270796=CARTESIAN_POINT('Ctrl Pts',(113.443927583196,64.4501995169389,391.537703348572));
#270797=CARTESIAN_POINT('Ctrl Pts',(117.786702325803,55.1801850026549,389.537703348572));
#270798=CARTESIAN_POINT('Ctrl Pts',(122.129477068411,45.910170488371,387.537703348572));
#270799=CARTESIAN_POINT('Ctrl Pts',(124.968635286058,36.074925591815,385.537703348572));
#270800=CARTESIAN_POINT('Ctrl Pts',(127.807793503704,26.239680695259,383.537703348572));
#270801=CARTESIAN_POINT('Ctrl Pts',(129.073425698447,16.0813817870907,381.537703348572));
#270802=CARTESIAN_POINT('Ctrl Pts',(130.339057893189,5.92308287892242,379.537703348572));
#270803=CARTESIAN_POINT('Ctrl Pts',(130.,-4.30813900827807,377.537703348572));
#270804=CARTESIAN_POINT('Ctrl Pts',(130.,4.30813900827812,532.462296651428));
#270805=CARTESIAN_POINT('Ctrl Pts',(130.339057893189,-5.92308287892228,
530.462296651428));
#270806=CARTESIAN_POINT('Ctrl Pts',(129.073425698447,-16.0813817870906,
528.462296651428));
#270807=CARTESIAN_POINT('Ctrl Pts',(127.807793503704,-26.2396806952589,
526.462296651428));
#270808=CARTESIAN_POINT('Ctrl Pts',(124.968635286058,-36.0749255918149,
524.462296651428));
#270809=CARTESIAN_POINT('Ctrl Pts',(122.129477068411,-45.9101704883709,
522.462296651428));
#270810=CARTESIAN_POINT('Ctrl Pts',(117.786702325803,-55.1801850026549,
520.462296651428));
#270811=CARTESIAN_POINT('Ctrl Pts',(113.443927583196,-64.4501995169389,
518.462296651428));
#270812=CARTESIAN_POINT('Ctrl Pts',(107.704469842635,-72.9267251261949,
516.462296651428));
#270813=CARTESIAN_POINT('Ctrl Pts',(101.965012102074,-81.4032507354509,
514.462296651428));
#270814=CARTESIAN_POINT('Ctrl Pts',(94.9701958612989,-88.8775672472035,
512.462296651428));
#270815=CARTESIAN_POINT('Ctrl Pts',(87.9753796205242,-96.351883758956,510.462296651428));
#270816=CARTESIAN_POINT('Ctrl Pts',(79.8974404698481,-102.639948694851,
508.462296651428));
#270817=CARTESIAN_POINT('Ctrl Pts',(71.8195013191721,-108.928013630747,
506.462296651428));
#270818=CARTESIAN_POINT('Ctrl Pts',(62.8573449296273,-113.874993963172,
504.462296651428));
#270819=CARTESIAN_POINT('Ctrl Pts',(53.8951885400825,-118.821974295598,
502.462296651428));
#270820=CARTESIAN_POINT('Ctrl Pts',(44.2694929456714,-122.306058950682,
500.462296651428));
#270821=CARTESIAN_POINT('Ctrl Pts',(34.6437973512603,-125.790143605767,
498.462296651428));
#270822=CARTESIAN_POINT('Ctrl Pts',(24.5915791233694,-127.725542856289,
496.462296651428));
#270823=CARTESIAN_POINT('Ctrl Pts',(14.5393608954785,-129.660942106811,
494.462296651428));
#270824=CARTESIAN_POINT('Ctrl Pts',(4.30813900827813,-130.,492.462296651428));
#270825=CARTESIAN_POINT('Ctrl Pts',(-5.92308287892227,-130.339057893189,
490.462296651428));
#270826=CARTESIAN_POINT('Ctrl Pts',(-16.0813817870906,-129.073425698447,
488.462296651428));
#270827=CARTESIAN_POINT('Ctrl Pts',(-26.2396806952589,-127.807793503705,
486.462296651428));
#270828=CARTESIAN_POINT('Ctrl Pts',(-36.0749255918149,-124.968635286058,
484.462296651428));
#270829=CARTESIAN_POINT('Ctrl Pts',(-45.9101704883709,-122.129477068411,
482.462296651428));
#270830=CARTESIAN_POINT('Ctrl Pts',(-55.1801850026549,-117.786702325803,
480.462296651428));
#270831=CARTESIAN_POINT('Ctrl Pts',(-64.4501995169389,-113.443927583196,
478.462296651428));
#270832=CARTESIAN_POINT('Ctrl Pts',(-72.9267251261949,-107.704469842635,
476.462296651428));
#270833=CARTESIAN_POINT('Ctrl Pts',(-81.4032507354509,-101.965012102074,
474.462296651428));
#270834=CARTESIAN_POINT('Ctrl Pts',(-88.8775672472034,-94.9701958612989,
472.462296651428));
#270835=CARTESIAN_POINT('Ctrl Pts',(-96.351883758956,-87.9753796205242,
470.462296651428));
#270836=CARTESIAN_POINT('Ctrl Pts',(-102.639948694851,-79.8974404698482,
468.462296651428));
#270837=CARTESIAN_POINT('Ctrl Pts',(-108.928013630747,-71.8195013191721,
466.462296651428));
#270838=CARTESIAN_POINT('Ctrl Pts',(-113.874993963172,-62.8573449296273,
464.462296651428));
#270839=CARTESIAN_POINT('Ctrl Pts',(-118.821974295598,-53.8951885400825,
462.462296651428));
#270840=CARTESIAN_POINT('Ctrl Pts',(-122.306058950682,-44.2694929456714,
460.462296651428));
#270841=CARTESIAN_POINT('Ctrl Pts',(-125.790143605767,-34.6437973512603,
458.462296651428));
#270842=CARTESIAN_POINT('Ctrl Pts',(-127.725542856289,-24.5915791233694,
456.462296651428));
#270843=CARTESIAN_POINT('Ctrl Pts',(-129.660942106811,-14.5393608954785,
454.462296651429));
#270844=CARTESIAN_POINT('Ctrl Pts',(-130.,-4.30813900827813,452.462296651428));
#270845=CARTESIAN_POINT('Ctrl Pts',(-130.339057893189,5.92308287892227,
450.462296651428));
#270846=CARTESIAN_POINT('Ctrl Pts',(-129.073425698447,16.0813817870906,
448.462296651428));
#270847=CARTESIAN_POINT('Ctrl Pts',(-127.807793503705,26.2396806952589,
446.462296651428));
#270848=CARTESIAN_POINT('Ctrl Pts',(-124.968635286058,36.0749255918149,
444.462296651428));
#270849=CARTESIAN_POINT('Ctrl Pts',(-122.129477068411,45.9101704883709,
442.462296651428));
#270850=CARTESIAN_POINT('Ctrl Pts',(-117.786702325803,55.1801850026549,
440.462296651428));
#270851=CARTESIAN_POINT('Ctrl Pts',(-113.443927583196,64.4501995169388,
438.462296651428));
#270852=CARTESIAN_POINT('Ctrl Pts',(-107.704469842635,72.9267251261949,
436.462296651428));
#270853=CARTESIAN_POINT('Ctrl Pts',(-101.965012102074,81.4032507354509,
434.462296651428));
#270854=CARTESIAN_POINT('Ctrl Pts',(-94.9701958612989,88.8775672472034,
432.462296651428));
#270855=CARTESIAN_POINT('Ctrl Pts',(-87.9753796205243,96.3518837589559,
430.462296651428));
#270856=CARTESIAN_POINT('Ctrl Pts',(-79.8974404698482,102.639948694851,
428.462296651428));
#270857=CARTESIAN_POINT('Ctrl Pts',(-71.819501319172,108.928013630747,426.462296651428));
#270858=CARTESIAN_POINT('Ctrl Pts',(-62.8573449296273,113.874993963172,
424.462296651428));
#270859=CARTESIAN_POINT('Ctrl Pts',(-53.8951885400826,118.821974295598,
422.462296651428));
#270860=CARTESIAN_POINT('Ctrl Pts',(-44.2694929456714,122.306058950682,
420.462296651428));
#270861=CARTESIAN_POINT('Ctrl Pts',(-34.6437973512603,125.790143605767,
418.462296651428));
#270862=CARTESIAN_POINT('Ctrl Pts',(-24.5915791233694,127.725542856289,
416.462296651428));
#270863=CARTESIAN_POINT('Ctrl Pts',(-14.5393608954786,129.660942106811,
414.462296651428));
#270864=CARTESIAN_POINT('Ctrl Pts',(-4.30813900827814,130.,412.462296651428));
#270865=CARTESIAN_POINT('Ctrl Pts',(5.92308287892232,130.339057893189,410.462296651428));
#270866=CARTESIAN_POINT('Ctrl Pts',(16.0813817870906,129.073425698447,408.462296651428));
#270867=CARTESIAN_POINT('Ctrl Pts',(26.2396806952589,127.807793503705,406.462296651428));
#270868=CARTESIAN_POINT('Ctrl Pts',(36.0749255918149,124.968635286058,404.462296651428));
#270869=CARTESIAN_POINT('Ctrl Pts',(45.9101704883709,122.129477068411,402.462296651428));
#270870=CARTESIAN_POINT('Ctrl Pts',(55.1801850026549,117.786702325803,400.462296651428));
#270871=CARTESIAN_POINT('Ctrl Pts',(64.4501995169388,113.443927583196,398.462296651428));
#270872=CARTESIAN_POINT('Ctrl Pts',(72.9267251261949,107.704469842635,396.462296651428));
#270873=CARTESIAN_POINT('Ctrl Pts',(81.4032507354509,101.965012102074,394.462296651428));
#270874=CARTESIAN_POINT('Ctrl Pts',(88.8775672472034,94.9701958612989,392.462296651428));
#270875=CARTESIAN_POINT('Ctrl Pts',(96.3518837589559,87.9753796205243,390.462296651428));
#270876=CARTESIAN_POINT('Ctrl Pts',(102.639948694851,79.8974404698482,388.462296651428));
#270877=CARTESIAN_POINT('Ctrl Pts',(108.928013630747,71.819501319172,386.462296651428));
#270878=CARTESIAN_POINT('Ctrl Pts',(113.874993963172,62.8573449296273,384.462296651428));
#270879=CARTESIAN_POINT('Ctrl Pts',(118.821974295598,53.8951885400826,382.462296651428));
#270880=CARTESIAN_POINT('Ctrl Pts',(122.306058950682,44.2694929456714,380.462296651428));
#270881=CARTESIAN_POINT('Ctrl Pts',(125.790143605767,34.6437973512603,378.462296651428));
#270882=CARTESIAN_POINT('Ctrl Pts',(127.725542856289,24.5915791233694,376.462296651428));
#270883=CARTESIAN_POINT('Ctrl Pts',(129.660942106811,14.5393608954786,374.462296651428));
#270884=CARTESIAN_POINT('Ctrl Pts',(130.,4.30813900827812,372.462296651428));
#270885=CARTESIAN_POINT('Ctrl Pts',(129.934615416877,-5.96286660784692,
530.450909781393));
#270886=CARTESIAN_POINT('Ctrl Pts',(129.701667605591,-11.0389459941987,
529.455068342531));
#270887=CARTESIAN_POINT('Ctrl Pts',(129.073425698447,-16.0813817870906,
528.462296651428));
#270888=CARTESIAN_POINT('Ctrl Pts',(127.807793503704,-26.2396806952589,
526.462296651428));
#270889=CARTESIAN_POINT('Ctrl Pts',(124.968635286058,-36.0749255918149,
524.462296651428));
#270890=CARTESIAN_POINT('Ctrl Pts',(122.129477068411,-45.9101704883709,
522.462296651428));
#270891=CARTESIAN_POINT('Ctrl Pts',(117.786702325803,-55.1801850026549,
520.462296651428));
#270892=CARTESIAN_POINT('Ctrl Pts',(113.443927583196,-64.4501995169389,
518.462296651428));
#270893=CARTESIAN_POINT('Ctrl Pts',(107.704469842635,-72.9267251261949,
516.462296651428));
#270894=CARTESIAN_POINT('Ctrl Pts',(101.965012102074,-81.4032507354509,
514.462296651428));
#270895=CARTESIAN_POINT('Ctrl Pts',(94.9701958612989,-88.8775672472035,
512.462296651428));
#270896=CARTESIAN_POINT('Ctrl Pts',(87.9753796205242,-96.351883758956,510.462296651428));
#270897=CARTESIAN_POINT('Ctrl Pts',(79.8974404698481,-102.639948694851,
508.462296651428));
#270898=CARTESIAN_POINT('Ctrl Pts',(71.8195013191721,-108.928013630747,
506.462296651428));
#270899=CARTESIAN_POINT('Ctrl Pts',(62.8573449296273,-113.874993963172,
504.462296651428));
#270900=CARTESIAN_POINT('Ctrl Pts',(53.8951885400825,-118.821974295598,
502.462296651428));
#270901=CARTESIAN_POINT('Ctrl Pts',(44.2694929456714,-122.306058950682,
500.462296651428));
#270902=CARTESIAN_POINT('Ctrl Pts',(34.6437973512603,-125.790143605767,
498.462296651428));
#270903=CARTESIAN_POINT('Ctrl Pts',(24.5915791233694,-127.725542856289,
496.462296651428));
#270904=CARTESIAN_POINT('Ctrl Pts',(14.5393608954785,-129.660942106811,
494.462296651428));
#270905=CARTESIAN_POINT('Ctrl Pts',(4.30813900827813,-130.,492.462296651428));
#270906=CARTESIAN_POINT('Ctrl Pts',(-5.92308287892227,-130.339057893189,
490.462296651428));
#270907=CARTESIAN_POINT('Ctrl Pts',(-16.0813817870906,-129.073425698447,
488.462296651428));
#270908=CARTESIAN_POINT('Ctrl Pts',(-26.2396806952589,-127.807793503705,
486.462296651428));
#270909=CARTESIAN_POINT('Ctrl Pts',(-36.0749255918149,-124.968635286058,
484.462296651428));
#270910=CARTESIAN_POINT('Ctrl Pts',(-45.9101704883709,-122.129477068411,
482.462296651428));
#270911=CARTESIAN_POINT('Ctrl Pts',(-55.1801850026549,-117.786702325803,
480.462296651428));
#270912=CARTESIAN_POINT('Ctrl Pts',(-64.4501995169389,-113.443927583196,
478.462296651428));
#270913=CARTESIAN_POINT('Ctrl Pts',(-72.9267251261949,-107.704469842635,
476.462296651428));
#270914=CARTESIAN_POINT('Ctrl Pts',(-81.4032507354509,-101.965012102074,
474.462296651428));
#270915=CARTESIAN_POINT('Ctrl Pts',(-88.8775672472034,-94.9701958612989,
472.462296651428));
#270916=CARTESIAN_POINT('Ctrl Pts',(-96.351883758956,-87.9753796205242,
470.462296651428));
#270917=CARTESIAN_POINT('Ctrl Pts',(-102.639948694851,-79.8974404698482,
468.462296651428));
#270918=CARTESIAN_POINT('Ctrl Pts',(-108.928013630747,-71.8195013191721,
466.462296651428));
#270919=CARTESIAN_POINT('Ctrl Pts',(-113.874993963172,-62.8573449296273,
464.462296651428));
#270920=CARTESIAN_POINT('Ctrl Pts',(-118.821974295598,-53.8951885400825,
462.462296651428));
#270921=CARTESIAN_POINT('Ctrl Pts',(-122.306058950682,-44.2694929456714,
460.462296651428));
#270922=CARTESIAN_POINT('Ctrl Pts',(-125.790143605767,-34.6437973512603,
458.462296651428));
#270923=CARTESIAN_POINT('Ctrl Pts',(-127.725542856289,-24.5915791233694,
456.462296651428));
#270924=CARTESIAN_POINT('Ctrl Pts',(-129.660942106811,-14.5393608954785,
454.462296651429));
#270925=CARTESIAN_POINT('Ctrl Pts',(-130.,-4.30813900827813,452.462296651428));
#270926=CARTESIAN_POINT('Ctrl Pts',(-130.339057893189,5.92308287892227,
450.462296651428));
#270927=CARTESIAN_POINT('Ctrl Pts',(-129.073425698447,16.0813817870906,
448.462296651428));
#270928=CARTESIAN_POINT('Ctrl Pts',(-127.807793503705,26.2396806952589,
446.462296651428));
#270929=CARTESIAN_POINT('Ctrl Pts',(-124.968635286058,36.0749255918149,
444.462296651428));
#270930=CARTESIAN_POINT('Ctrl Pts',(-122.129477068411,45.9101704883709,
442.462296651428));
#270931=CARTESIAN_POINT('Ctrl Pts',(-117.786702325803,55.1801850026549,
440.462296651428));
#270932=CARTESIAN_POINT('Ctrl Pts',(-113.443927583196,64.4501995169388,
438.462296651428));
#270933=CARTESIAN_POINT('Ctrl Pts',(-107.704469842635,72.9267251261949,
436.462296651428));
#270934=CARTESIAN_POINT('Ctrl Pts',(-101.965012102074,81.4032507354509,
434.462296651428));
#270935=CARTESIAN_POINT('Ctrl Pts',(-94.9701958612989,88.8775672472034,
432.462296651428));
#270936=CARTESIAN_POINT('Ctrl Pts',(-87.9753796205243,96.3518837589559,
430.462296651428));
#270937=CARTESIAN_POINT('Ctrl Pts',(-79.8974404698482,102.639948694851,
428.462296651428));
#270938=CARTESIAN_POINT('Ctrl Pts',(-71.819501319172,108.928013630747,426.462296651428));
#270939=CARTESIAN_POINT('Ctrl Pts',(-62.8573449296273,113.874993963172,
424.462296651428));
#270940=CARTESIAN_POINT('Ctrl Pts',(-53.8951885400826,118.821974295598,
422.462296651428));
#270941=CARTESIAN_POINT('Ctrl Pts',(-44.2694929456714,122.306058950682,
420.462296651428));
#270942=CARTESIAN_POINT('Ctrl Pts',(-34.6437973512603,125.790143605767,
418.462296651428));
#270943=CARTESIAN_POINT('Ctrl Pts',(-24.5915791233694,127.725542856289,
416.462296651428));
#270944=CARTESIAN_POINT('Ctrl Pts',(-14.5393608954786,129.660942106811,
414.462296651428));
#270945=CARTESIAN_POINT('Ctrl Pts',(-4.30813900827814,130.,412.462296651428));
#270946=CARTESIAN_POINT('Ctrl Pts',(5.92308287892232,130.339057893189,410.462296651428));
#270947=CARTESIAN_POINT('Ctrl Pts',(16.0813817870906,129.073425698447,408.462296651428));
#270948=CARTESIAN_POINT('Ctrl Pts',(26.2396806952589,127.807793503705,406.462296651428));
#270949=CARTESIAN_POINT('Ctrl Pts',(36.0749255918149,124.968635286058,404.462296651428));
#270950=CARTESIAN_POINT('Ctrl Pts',(45.9101704883709,122.129477068411,402.462296651428));
#270951=CARTESIAN_POINT('Ctrl Pts',(55.1801850026549,117.786702325803,400.462296651428));
#270952=CARTESIAN_POINT('Ctrl Pts',(64.4501995169388,113.443927583196,398.462296651428));
#270953=CARTESIAN_POINT('Ctrl Pts',(72.9267251261949,107.704469842635,396.462296651428));
#270954=CARTESIAN_POINT('Ctrl Pts',(81.403250735451,101.965012102074,394.462296651428));
#270955=CARTESIAN_POINT('Ctrl Pts',(88.8775672472034,94.9701958612989,392.462296651428));
#270956=CARTESIAN_POINT('Ctrl Pts',(96.3518837589559,87.9753796205243,390.462296651428));
#270957=CARTESIAN_POINT('Ctrl Pts',(102.639948694851,79.8974404698482,388.462296651428));
#270958=CARTESIAN_POINT('Ctrl Pts',(108.928013630747,71.8195013191721,386.462296651428));
#270959=CARTESIAN_POINT('Ctrl Pts',(113.874993963172,62.8573449296273,384.462296651428));
#270960=CARTESIAN_POINT('Ctrl Pts',(118.821974295598,53.8951885400826,382.462296651428));
#270961=CARTESIAN_POINT('Ctrl Pts',(122.306058950682,44.2694929456714,380.462296651428));
#270962=CARTESIAN_POINT('Ctrl Pts',(125.790143605767,34.6437973512603,378.462296651428));
#270963=CARTESIAN_POINT('Ctrl Pts',(127.725542856289,24.5915791233694,376.462296651428));
#270964=CARTESIAN_POINT('Ctrl Pts',(129.382196958681,15.9871278397994,374.750345898171));
#270965=CARTESIAN_POINT('Ctrl Pts',(129.869812400585,7.23822414350007,373.035792462989));
#270966=CARTESIAN_POINT('Ctrl Pts',(129.869812400585,-7.23822414349995,
536.964207537012));
#270967=CARTESIAN_POINT('Ctrl Pts',(129.382196958681,-15.9871278397992,
535.249654101829));
#270968=CARTESIAN_POINT('Ctrl Pts',(127.725542856289,-24.5915791233694,
533.537703348572));
#270969=CARTESIAN_POINT('Ctrl Pts',(125.790143605767,-34.6437973512603,
531.537703348572));
#270970=CARTESIAN_POINT('Ctrl Pts',(122.306058950682,-44.2694929456714,
529.537703348572));
#270971=CARTESIAN_POINT('Ctrl Pts',(118.821974295598,-53.8951885400825,
527.537703348572));
#270972=CARTESIAN_POINT('Ctrl Pts',(113.874993963172,-62.8573449296272,
525.537703348572));
#270973=CARTESIAN_POINT('Ctrl Pts',(108.928013630747,-71.819501319172,523.537703348572));
#270974=CARTESIAN_POINT('Ctrl Pts',(102.639948694851,-79.8974404698481,
521.537703348572));
#270975=CARTESIAN_POINT('Ctrl Pts',(96.351883758956,-87.9753796205242,519.537703348572));
#270976=CARTESIAN_POINT('Ctrl Pts',(88.8775672472035,-94.9701958612989,
517.537703348572));
#270977=CARTESIAN_POINT('Ctrl Pts',(81.403250735451,-101.965012102074,515.537703348572));
#270978=CARTESIAN_POINT('Ctrl Pts',(72.9267251261949,-107.704469842635,
513.537703348572));
#270979=CARTESIAN_POINT('Ctrl Pts',(64.4501995169389,-113.443927583196,
511.537703348572));
#270980=CARTESIAN_POINT('Ctrl Pts',(55.1801850026549,-117.786702325803,
509.537703348572));
#270981=CARTESIAN_POINT('Ctrl Pts',(45.910170488371,-122.129477068411,507.537703348572));
#270982=CARTESIAN_POINT('Ctrl Pts',(36.074925591815,-124.968635286058,505.537703348572));
#270983=CARTESIAN_POINT('Ctrl Pts',(26.239680695259,-127.807793503704,503.537703348572));
#270984=CARTESIAN_POINT('Ctrl Pts',(16.0813817870907,-129.073425698447,
501.537703348572));
#270985=CARTESIAN_POINT('Ctrl Pts',(5.92308287892234,-130.339057893189,
499.537703348572));
#270986=CARTESIAN_POINT('Ctrl Pts',(-4.30813900827806,-130.,497.537703348572));
#270987=CARTESIAN_POINT('Ctrl Pts',(-14.5393608954785,-129.660942106811,
495.537703348572));
#270988=CARTESIAN_POINT('Ctrl Pts',(-24.5915791233694,-127.725542856289,
493.537703348572));
#270989=CARTESIAN_POINT('Ctrl Pts',(-34.6437973512602,-125.790143605767,
491.537703348572));
#270990=CARTESIAN_POINT('Ctrl Pts',(-44.2694929456713,-122.306058950682,
489.537703348572));
#270991=CARTESIAN_POINT('Ctrl Pts',(-53.8951885400825,-118.821974295598,
487.537703348572));
#270992=CARTESIAN_POINT('Ctrl Pts',(-62.8573449296272,-113.874993963172,
485.537703348572));
#270993=CARTESIAN_POINT('Ctrl Pts',(-71.819501319172,-108.928013630747,
483.537703348572));
#270994=CARTESIAN_POINT('Ctrl Pts',(-79.8974404698481,-102.639948694851,
481.537703348572));
#270995=CARTESIAN_POINT('Ctrl Pts',(-87.9753796205242,-96.351883758956,
479.537703348572));
#270996=CARTESIAN_POINT('Ctrl Pts',(-94.9701958612989,-88.8775672472035,
477.537703348572));
#270997=CARTESIAN_POINT('Ctrl Pts',(-101.965012102074,-81.403250735451,
475.537703348572));
#270998=CARTESIAN_POINT('Ctrl Pts',(-107.704469842635,-72.9267251261949,
473.537703348572));
#270999=CARTESIAN_POINT('Ctrl Pts',(-113.443927583196,-64.4501995169389,
471.537703348572));
#271000=CARTESIAN_POINT('Ctrl Pts',(-117.786702325803,-55.1801850026549,
469.537703348572));
#271001=CARTESIAN_POINT('Ctrl Pts',(-122.129477068411,-45.910170488371,
467.537703348572));
#271002=CARTESIAN_POINT('Ctrl Pts',(-124.968635286058,-36.074925591815,
465.537703348572));
#271003=CARTESIAN_POINT('Ctrl Pts',(-127.807793503704,-26.239680695259,
463.537703348572));
#271004=CARTESIAN_POINT('Ctrl Pts',(-129.073425698447,-16.0813817870907,
461.537703348572));
#271005=CARTESIAN_POINT('Ctrl Pts',(-130.339057893189,-5.92308287892235,
459.537703348572));
#271006=CARTESIAN_POINT('Ctrl Pts',(-130.,4.30813900827805,457.537703348572));
#271007=CARTESIAN_POINT('Ctrl Pts',(-129.660942106811,14.5393608954784,
455.537703348572));
#271008=CARTESIAN_POINT('Ctrl Pts',(-127.725542856289,24.5915791233693,
453.537703348572));
#271009=CARTESIAN_POINT('Ctrl Pts',(-125.790143605767,34.6437973512602,
451.537703348572));
#271010=CARTESIAN_POINT('Ctrl Pts',(-122.306058950682,44.2694929456713,
449.537703348572));
#271011=CARTESIAN_POINT('Ctrl Pts',(-118.821974295598,53.8951885400825,
447.537703348572));
#271012=CARTESIAN_POINT('Ctrl Pts',(-113.874993963172,62.8573449296272,
445.537703348572));
#271013=CARTESIAN_POINT('Ctrl Pts',(-108.928013630747,71.819501319172,443.537703348572));
#271014=CARTESIAN_POINT('Ctrl Pts',(-102.639948694851,79.8974404698481,
441.537703348572));
#271015=CARTESIAN_POINT('Ctrl Pts',(-96.3518837589561,87.9753796205242,
439.537703348572));
#271016=CARTESIAN_POINT('Ctrl Pts',(-88.8775672472035,94.9701958612989,
437.537703348572));
#271017=CARTESIAN_POINT('Ctrl Pts',(-81.403250735451,101.965012102074,435.537703348572));
#271018=CARTESIAN_POINT('Ctrl Pts',(-72.9267251261949,107.704469842635,
433.537703348572));
#271019=CARTESIAN_POINT('Ctrl Pts',(-64.4501995169389,113.443927583196,
431.537703348572));
#271020=CARTESIAN_POINT('Ctrl Pts',(-55.1801850026549,117.786702325803,
429.537703348572));
#271021=CARTESIAN_POINT('Ctrl Pts',(-45.910170488371,122.129477068411,427.537703348572));
#271022=CARTESIAN_POINT('Ctrl Pts',(-36.074925591815,124.968635286058,425.537703348572));
#271023=CARTESIAN_POINT('Ctrl Pts',(-26.239680695259,127.807793503704,423.537703348572));
#271024=CARTESIAN_POINT('Ctrl Pts',(-16.0813817870907,129.073425698447,
421.537703348572));
#271025=CARTESIAN_POINT('Ctrl Pts',(-5.92308287892242,130.339057893189,
419.537703348572));
#271026=CARTESIAN_POINT('Ctrl Pts',(4.30813900827804,130.,417.537703348572));
#271027=CARTESIAN_POINT('Ctrl Pts',(14.5393608954785,129.660942106811,415.537703348572));
#271028=CARTESIAN_POINT('Ctrl Pts',(24.5915791233693,127.725542856289,413.537703348572));
#271029=CARTESIAN_POINT('Ctrl Pts',(34.6437973512602,125.790143605767,411.537703348572));
#271030=CARTESIAN_POINT('Ctrl Pts',(44.2694929456713,122.306058950682,409.537703348572));
#271031=CARTESIAN_POINT('Ctrl Pts',(53.8951885400825,118.821974295598,407.537703348572));
#271032=CARTESIAN_POINT('Ctrl Pts',(62.8573449296272,113.874993963172,405.537703348572));
#271033=CARTESIAN_POINT('Ctrl Pts',(71.819501319172,108.928013630747,403.537703348572));
#271034=CARTESIAN_POINT('Ctrl Pts',(79.8974404698481,102.639948694851,401.537703348572));
#271035=CARTESIAN_POINT('Ctrl Pts',(87.9753796205242,96.351883758956,399.537703348572));
#271036=CARTESIAN_POINT('Ctrl Pts',(94.9701958612989,88.8775672472035,397.537703348572));
#271037=CARTESIAN_POINT('Ctrl Pts',(101.965012102074,81.403250735451,395.537703348572));
#271038=CARTESIAN_POINT('Ctrl Pts',(107.704469842635,72.926725126195,393.537703348572));
#271039=CARTESIAN_POINT('Ctrl Pts',(113.443927583196,64.4501995169389,391.537703348572));
#271040=CARTESIAN_POINT('Ctrl Pts',(117.786702325803,55.1801850026549,389.537703348572));
#271041=CARTESIAN_POINT('Ctrl Pts',(122.129477068411,45.910170488371,387.537703348572));
#271042=CARTESIAN_POINT('Ctrl Pts',(124.968635286058,36.074925591815,385.537703348572));
#271043=CARTESIAN_POINT('Ctrl Pts',(127.807793503704,26.239680695259,383.537703348572));
#271044=CARTESIAN_POINT('Ctrl Pts',(129.073425698447,16.0813817870907,381.537703348572));
#271045=CARTESIAN_POINT('Ctrl Pts',(129.701667605591,11.0389459941988,380.54493165747));
#271046=CARTESIAN_POINT('Ctrl Pts',(129.934615416877,5.96286660784696,379.549090218607));
#271047=CARTESIAN_POINT('Ctrl Pts',(130.,4.30813900827812,532.462296651428));
#271048=CARTESIAN_POINT('Ctrl Pts',(130.339057893189,-5.92308287892228,
530.462296651428));
#271049=CARTESIAN_POINT('Ctrl Pts',(129.073425698447,-16.0813817870906,
528.462296651428));
#271050=CARTESIAN_POINT('Ctrl Pts',(127.807793503704,-26.2396806952589,
526.462296651428));
#271051=CARTESIAN_POINT('Ctrl Pts',(124.968635286058,-36.0749255918149,
524.462296651428));
#271052=CARTESIAN_POINT('Ctrl Pts',(122.129477068411,-45.9101704883709,
522.462296651428));
#271053=CARTESIAN_POINT('Ctrl Pts',(117.786702325803,-55.1801850026549,
520.462296651428));
#271054=CARTESIAN_POINT('Ctrl Pts',(113.443927583196,-64.4501995169389,
518.462296651428));
#271055=CARTESIAN_POINT('Ctrl Pts',(107.704469842635,-72.9267251261949,
516.462296651428));
#271056=CARTESIAN_POINT('Ctrl Pts',(101.965012102074,-81.4032507354509,
514.462296651428));
#271057=CARTESIAN_POINT('Ctrl Pts',(94.9701958612989,-88.8775672472035,
512.462296651428));
#271058=CARTESIAN_POINT('Ctrl Pts',(87.9753796205242,-96.351883758956,510.462296651428));
#271059=CARTESIAN_POINT('Ctrl Pts',(79.8974404698481,-102.639948694851,
508.462296651428));
#271060=CARTESIAN_POINT('Ctrl Pts',(71.8195013191721,-108.928013630747,
506.462296651428));
#271061=CARTESIAN_POINT('Ctrl Pts',(62.8573449296273,-113.874993963172,
504.462296651428));
#271062=CARTESIAN_POINT('Ctrl Pts',(53.8951885400825,-118.821974295598,
502.462296651428));
#271063=CARTESIAN_POINT('Ctrl Pts',(44.2694929456714,-122.306058950682,
500.462296651428));
#271064=CARTESIAN_POINT('Ctrl Pts',(34.6437973512603,-125.790143605767,
498.462296651428));
#271065=CARTESIAN_POINT('Ctrl Pts',(24.5915791233694,-127.725542856289,
496.462296651428));
#271066=CARTESIAN_POINT('Ctrl Pts',(14.5393608954785,-129.660942106811,
494.462296651428));
#271067=CARTESIAN_POINT('Ctrl Pts',(4.30813900827813,-130.,492.462296651428));
#271068=CARTESIAN_POINT('Ctrl Pts',(-5.92308287892227,-130.339057893189,
490.462296651428));
#271069=CARTESIAN_POINT('Ctrl Pts',(-16.0813817870906,-129.073425698447,
488.462296651428));
#271070=CARTESIAN_POINT('Ctrl Pts',(-26.2396806952589,-127.807793503705,
486.462296651428));
#271071=CARTESIAN_POINT('Ctrl Pts',(-36.0749255918149,-124.968635286058,
484.462296651428));
#271072=CARTESIAN_POINT('Ctrl Pts',(-45.9101704883709,-122.129477068411,
482.462296651428));
#271073=CARTESIAN_POINT('Ctrl Pts',(-55.1801850026549,-117.786702325803,
480.462296651428));
#271074=CARTESIAN_POINT('Ctrl Pts',(-64.4501995169389,-113.443927583196,
478.462296651428));
#271075=CARTESIAN_POINT('Ctrl Pts',(-72.9267251261949,-107.704469842635,
476.462296651428));
#271076=CARTESIAN_POINT('Ctrl Pts',(-81.4032507354509,-101.965012102074,
474.462296651428));
#271077=CARTESIAN_POINT('Ctrl Pts',(-88.8775672472034,-94.9701958612989,
472.462296651428));
#271078=CARTESIAN_POINT('Ctrl Pts',(-96.351883758956,-87.9753796205242,
470.462296651428));
#271079=CARTESIAN_POINT('Ctrl Pts',(-102.639948694851,-79.8974404698482,
468.462296651428));
#271080=CARTESIAN_POINT('Ctrl Pts',(-108.928013630747,-71.8195013191721,
466.462296651428));
#271081=CARTESIAN_POINT('Ctrl Pts',(-113.874993963172,-62.8573449296273,
464.462296651428));
#271082=CARTESIAN_POINT('Ctrl Pts',(-118.821974295598,-53.8951885400825,
462.462296651428));
#271083=CARTESIAN_POINT('Ctrl Pts',(-122.306058950682,-44.2694929456714,
460.462296651428));
#271084=CARTESIAN_POINT('Ctrl Pts',(-125.790143605767,-34.6437973512603,
458.462296651428));
#271085=CARTESIAN_POINT('Ctrl Pts',(-127.725542856289,-24.5915791233694,
456.462296651428));
#271086=CARTESIAN_POINT('Ctrl Pts',(-129.660942106811,-14.5393608954785,
454.462296651429));
#271087=CARTESIAN_POINT('Ctrl Pts',(-130.,-4.30813900827813,452.462296651428));
#271088=CARTESIAN_POINT('Ctrl Pts',(-130.339057893189,5.92308287892227,
450.462296651428));
#271089=CARTESIAN_POINT('Ctrl Pts',(-129.073425698447,16.0813817870906,
448.462296651428));
#271090=CARTESIAN_POINT('Ctrl Pts',(-127.807793503705,26.2396806952589,
446.462296651428));
#271091=CARTESIAN_POINT('Ctrl Pts',(-124.968635286058,36.0749255918149,
444.462296651428));
#271092=CARTESIAN_POINT('Ctrl Pts',(-122.129477068411,45.9101704883709,
442.462296651428));
#271093=CARTESIAN_POINT('Ctrl Pts',(-117.786702325803,55.1801850026549,
440.462296651428));
#271094=CARTESIAN_POINT('Ctrl Pts',(-113.443927583196,64.4501995169388,
438.462296651428));
#271095=CARTESIAN_POINT('Ctrl Pts',(-107.704469842635,72.9267251261949,
436.462296651428));
#271096=CARTESIAN_POINT('Ctrl Pts',(-101.965012102074,81.4032507354509,
434.462296651428));
#271097=CARTESIAN_POINT('Ctrl Pts',(-94.9701958612989,88.8775672472034,
432.462296651428));
#271098=CARTESIAN_POINT('Ctrl Pts',(-87.9753796205243,96.3518837589559,
430.462296651428));
#271099=CARTESIAN_POINT('Ctrl Pts',(-79.8974404698482,102.639948694851,
428.462296651428));
#271100=CARTESIAN_POINT('Ctrl Pts',(-71.819501319172,108.928013630747,426.462296651428));
#271101=CARTESIAN_POINT('Ctrl Pts',(-62.8573449296273,113.874993963172,
424.462296651428));
#271102=CARTESIAN_POINT('Ctrl Pts',(-53.8951885400826,118.821974295598,
422.462296651428));
#271103=CARTESIAN_POINT('Ctrl Pts',(-44.2694929456714,122.306058950682,
420.462296651428));
#271104=CARTESIAN_POINT('Ctrl Pts',(-34.6437973512603,125.790143605767,
418.462296651428));
#271105=CARTESIAN_POINT('Ctrl Pts',(-24.5915791233694,127.725542856289,
416.462296651428));
#271106=CARTESIAN_POINT('Ctrl Pts',(-14.5393608954786,129.660942106811,
414.462296651428));
#271107=CARTESIAN_POINT('Ctrl Pts',(-4.30813900827814,130.,412.462296651428));
#271108=CARTESIAN_POINT('Ctrl Pts',(5.92308287892232,130.339057893189,410.462296651428));
#271109=CARTESIAN_POINT('Ctrl Pts',(16.0813817870906,129.073425698447,408.462296651428));
#271110=CARTESIAN_POINT('Ctrl Pts',(26.2396806952589,127.807793503705,406.462296651428));
#271111=CARTESIAN_POINT('Ctrl Pts',(36.0749255918149,124.968635286058,404.462296651428));
#271112=CARTESIAN_POINT('Ctrl Pts',(45.9101704883709,122.129477068411,402.462296651428));
#271113=CARTESIAN_POINT('Ctrl Pts',(55.1801850026549,117.786702325803,400.462296651428));
#271114=CARTESIAN_POINT('Ctrl Pts',(64.4501995169388,113.443927583196,398.462296651428));
#271115=CARTESIAN_POINT('Ctrl Pts',(72.9267251261949,107.704469842635,396.462296651428));
#271116=CARTESIAN_POINT('Ctrl Pts',(81.4032507354509,101.965012102074,394.462296651428));
#271117=CARTESIAN_POINT('Ctrl Pts',(88.8775672472034,94.9701958612989,392.462296651428));
#271118=CARTESIAN_POINT('Ctrl Pts',(96.3518837589559,87.9753796205243,390.462296651428));
#271119=CARTESIAN_POINT('Ctrl Pts',(102.639948694851,79.8974404698482,388.462296651428));
#271120=CARTESIAN_POINT('Ctrl Pts',(108.928013630747,71.819501319172,386.462296651428));
#271121=CARTESIAN_POINT('Ctrl Pts',(113.874993963172,62.8573449296273,384.462296651428));
#271122=CARTESIAN_POINT('Ctrl Pts',(118.821974295598,53.8951885400826,382.462296651428));
#271123=CARTESIAN_POINT('Ctrl Pts',(122.306058950682,44.2694929456714,380.462296651428));
#271124=CARTESIAN_POINT('Ctrl Pts',(125.790143605767,34.6437973512603,378.462296651428));
#271125=CARTESIAN_POINT('Ctrl Pts',(127.725542856289,24.5915791233694,376.462296651428));
#271126=CARTESIAN_POINT('Ctrl Pts',(129.660942106811,14.5393608954786,374.462296651428));
#271127=CARTESIAN_POINT('Ctrl Pts',(130.,4.30813900827812,372.462296651428));
#271128=CARTESIAN_POINT('Ctrl Pts',(160.,4.30813900827813,532.462296651428));
#271129=CARTESIAN_POINT('Ctrl Pts',(160.339057893189,-8.28413408366083,
530.462296651428));
#271130=CARTESIAN_POINT('Ctrl Pts',(158.704075916301,-20.7744157382975,
528.462296651428));
#271131=CARTESIAN_POINT('Ctrl Pts',(157.069093939413,-33.2646973929343,
526.462296651428));
#271132=CARTESIAN_POINT('Ctrl Pts',(153.500330774912,-45.3454354230633,
524.462296651428));
#271133=CARTESIAN_POINT('Ctrl Pts',(149.931567610412,-57.4261734531924,
522.462296651428));
#271134=CARTESIAN_POINT('Ctrl Pts',(144.516898051455,-68.7998999948413,
520.462296651428));
#271135=CARTESIAN_POINT('Ctrl Pts',(139.102228492497,-80.1736265364901,
518.462296651428));
#271136=CARTESIAN_POINT('Ctrl Pts',(131.974979673883,-90.5602826949691,
516.462296651428));
#271137=CARTESIAN_POINT('Ctrl Pts',(124.847730855269,-100.946938853448,
514.462296651428));
#271138=CARTESIAN_POINT('Ctrl Pts',(116.183399296895,-110.0907706828,512.462296651428));
#271139=CARTESIAN_POINT('Ctrl Pts',(107.519067738521,-119.234602512152,
510.462296651428));
#271140=CARTESIAN_POINT('Ctrl Pts',(97.5309980386224,-126.9104585261,508.462296651428));
#271141=CARTESIAN_POINT('Ctrl Pts',(87.5429283387234,-134.586314540048,
506.462296651428));
#271142=CARTESIAN_POINT('Ctrl Pts',(76.4770599218137,-140.605189688823,
504.462296651428));
#271143=CARTESIAN_POINT('Ctrl Pts',(65.4111915049041,-146.624064837599,
502.462296651428));
#271144=CARTESIAN_POINT('Ctrl Pts',(53.5400027769198,-150.837754439537,
500.462296651428));
#271145=CARTESIAN_POINT('Ctrl Pts',(41.6688140489356,-155.051444041475,
498.462296651428));
#271146=CARTESIAN_POINT('Ctrl Pts',(29.2846130745764,-157.356193074143,
496.462296651428));
#271147=CARTESIAN_POINT('Ctrl Pts',(16.9004121002171,-159.660942106811,
494.462296651428));
#271148=CARTESIAN_POINT('Ctrl Pts',(4.30813900827814,-160.,492.462296651428));
#271149=CARTESIAN_POINT('Ctrl Pts',(-8.28413408366082,-160.339057893189,
490.462296651428));
#271150=CARTESIAN_POINT('Ctrl Pts',(-20.7744157382975,-158.704075916301,
488.462296651428));
#271151=CARTESIAN_POINT('Ctrl Pts',(-33.2646973929342,-157.069093939413,
486.462296651428));
#271152=CARTESIAN_POINT('Ctrl Pts',(-45.3454354230633,-153.500330774912,
484.462296651428));
#271153=CARTESIAN_POINT('Ctrl Pts',(-57.4261734531924,-149.931567610412,
482.462296651428));
#271154=CARTESIAN_POINT('Ctrl Pts',(-68.7998999948413,-144.516898051455,
480.462296651428));
#271155=CARTESIAN_POINT('Ctrl Pts',(-80.1736265364901,-139.102228492497,
478.462296651428));
#271156=CARTESIAN_POINT('Ctrl Pts',(-90.5602826949691,-131.974979673883,
476.462296651428));
#271157=CARTESIAN_POINT('Ctrl Pts',(-100.946938853448,-124.847730855269,
474.462296651428));
#271158=CARTESIAN_POINT('Ctrl Pts',(-110.0907706828,-116.183399296895,472.462296651428));
#271159=CARTESIAN_POINT('Ctrl Pts',(-119.234602512152,-107.519067738521,
470.462296651428));
#271160=CARTESIAN_POINT('Ctrl Pts',(-126.9104585261,-97.5309980386224,468.462296651428));
#271161=CARTESIAN_POINT('Ctrl Pts',(-134.586314540048,-87.5429283387234,
466.462296651428));
#271162=CARTESIAN_POINT('Ctrl Pts',(-140.605189688823,-76.4770599218137,
464.462296651428));
#271163=CARTESIAN_POINT('Ctrl Pts',(-146.624064837599,-65.4111915049041,
462.462296651428));
#271164=CARTESIAN_POINT('Ctrl Pts',(-150.837754439537,-53.5400027769199,
460.462296651428));
#271165=CARTESIAN_POINT('Ctrl Pts',(-155.051444041475,-41.6688140489356,
458.462296651428));
#271166=CARTESIAN_POINT('Ctrl Pts',(-157.356193074143,-29.2846130745764,
456.462296651428));
#271167=CARTESIAN_POINT('Ctrl Pts',(-159.660942106811,-16.9004121002171,
454.462296651429));
#271168=CARTESIAN_POINT('Ctrl Pts',(-160.,-4.30813900827815,452.462296651428));
#271169=CARTESIAN_POINT('Ctrl Pts',(-160.339057893189,8.28413408366081,
450.462296651428));
#271170=CARTESIAN_POINT('Ctrl Pts',(-158.704075916301,20.7744157382975,
448.462296651428));
#271171=CARTESIAN_POINT('Ctrl Pts',(-157.069093939413,33.2646973929342,
446.462296651428));
#271172=CARTESIAN_POINT('Ctrl Pts',(-153.500330774912,45.3454354230633,
444.462296651428));
#271173=CARTESIAN_POINT('Ctrl Pts',(-149.931567610412,57.4261734531924,
442.462296651428));
#271174=CARTESIAN_POINT('Ctrl Pts',(-144.516898051455,68.7998999948413,
440.462296651428));
#271175=CARTESIAN_POINT('Ctrl Pts',(-139.102228492497,80.1736265364901,
438.462296651428));
#271176=CARTESIAN_POINT('Ctrl Pts',(-131.974979673883,90.5602826949691,
436.462296651428));
#271177=CARTESIAN_POINT('Ctrl Pts',(-124.847730855269,100.946938853448,
434.462296651428));
#271178=CARTESIAN_POINT('Ctrl Pts',(-116.183399296895,110.0907706828,432.462296651428));
#271179=CARTESIAN_POINT('Ctrl Pts',(-107.519067738521,119.234602512152,
430.462296651428));
#271180=CARTESIAN_POINT('Ctrl Pts',(-97.5309980386224,126.9104585261,428.462296651428));
#271181=CARTESIAN_POINT('Ctrl Pts',(-87.5429283387233,134.586314540048,
426.462296651428));
#271182=CARTESIAN_POINT('Ctrl Pts',(-76.4770599218137,140.605189688823,
424.462296651428));
#271183=CARTESIAN_POINT('Ctrl Pts',(-65.4111915049042,146.624064837599,
422.462296651428));
#271184=CARTESIAN_POINT('Ctrl Pts',(-53.5400027769199,150.837754439537,
420.462296651428));
#271185=CARTESIAN_POINT('Ctrl Pts',(-41.6688140489356,155.051444041475,
418.462296651428));
#271186=CARTESIAN_POINT('Ctrl Pts',(-29.2846130745764,157.356193074143,
416.462296651428));
#271187=CARTESIAN_POINT('Ctrl Pts',(-16.9004121002172,159.660942106811,
414.462296651428));
#271188=CARTESIAN_POINT('Ctrl Pts',(-4.30813900827816,160.,412.462296651428));
#271189=CARTESIAN_POINT('Ctrl Pts',(8.28413408366087,160.339057893189,410.462296651428));
#271190=CARTESIAN_POINT('Ctrl Pts',(20.7744157382975,158.704075916301,408.462296651428));
#271191=CARTESIAN_POINT('Ctrl Pts',(33.2646973929342,157.069093939413,406.462296651428));
#271192=CARTESIAN_POINT('Ctrl Pts',(45.3454354230633,153.500330774912,404.462296651428));
#271193=CARTESIAN_POINT('Ctrl Pts',(57.4261734531925,149.931567610412,402.462296651428));
#271194=CARTESIAN_POINT('Ctrl Pts',(68.7998999948413,144.516898051455,400.462296651428));
#271195=CARTESIAN_POINT('Ctrl Pts',(80.1736265364901,139.102228492498,398.462296651428));
#271196=CARTESIAN_POINT('Ctrl Pts',(90.560282694969,131.974979673883,396.462296651428));
#271197=CARTESIAN_POINT('Ctrl Pts',(100.946938853448,124.847730855269,394.462296651428));
#271198=CARTESIAN_POINT('Ctrl Pts',(110.0907706828,116.183399296895,392.462296651428));
#271199=CARTESIAN_POINT('Ctrl Pts',(119.234602512152,107.519067738521,390.462296651428));
#271200=CARTESIAN_POINT('Ctrl Pts',(126.9104585261,97.5309980386224,388.462296651428));
#271201=CARTESIAN_POINT('Ctrl Pts',(134.586314540048,87.5429283387233,386.462296651428));
#271202=CARTESIAN_POINT('Ctrl Pts',(140.605189688823,76.4770599218137,384.462296651428));
#271203=CARTESIAN_POINT('Ctrl Pts',(146.624064837599,65.4111915049042,382.462296651428));
#271204=CARTESIAN_POINT('Ctrl Pts',(150.837754439537,53.5400027769199,380.462296651428));
#271205=CARTESIAN_POINT('Ctrl Pts',(155.051444041475,41.6688140489356,378.462296651428));
#271206=CARTESIAN_POINT('Ctrl Pts',(157.356193074143,29.2846130745764,376.462296651428));
#271207=CARTESIAN_POINT('Ctrl Pts',(159.660942106811,16.9004121002172,374.462296651428));
#271208=CARTESIAN_POINT('Ctrl Pts',(160.,4.30813900827813,372.462296651428));
#271209=CARTESIAN_POINT('Ctrl Pts',(159.937609420477,-6.20654127333069,
530.789436448355));
#271210=CARTESIAN_POINT('Ctrl Pts',(159.653854600275,-13.5186762622034,
529.624118246284));
#271211=CARTESIAN_POINT('Ctrl Pts',(158.704075916301,-20.7744157382975,
528.462296651428));
#271212=CARTESIAN_POINT('Ctrl Pts',(157.069093939413,-33.2646973929343,
526.462296651428));
#271213=CARTESIAN_POINT('Ctrl Pts',(153.500330774912,-45.3454354230633,
524.462296651428));
#271214=CARTESIAN_POINT('Ctrl Pts',(149.931567610412,-57.4261734531925,
522.462296651428));
#271215=CARTESIAN_POINT('Ctrl Pts',(144.516898051455,-68.7998999948413,
520.462296651428));
#271216=CARTESIAN_POINT('Ctrl Pts',(139.102228492497,-80.1736265364901,
518.462296651428));
#271217=CARTESIAN_POINT('Ctrl Pts',(131.974979673883,-90.5602826949691,
516.462296651428));
#271218=CARTESIAN_POINT('Ctrl Pts',(124.847730855269,-100.946938853448,
514.462296651428));
#271219=CARTESIAN_POINT('Ctrl Pts',(116.183399296895,-110.0907706828,512.462296651428));
#271220=CARTESIAN_POINT('Ctrl Pts',(107.519067738521,-119.234602512152,
510.462296651428));
#271221=CARTESIAN_POINT('Ctrl Pts',(97.5309980386224,-126.9104585261,508.462296651428));
#271222=CARTESIAN_POINT('Ctrl Pts',(87.5429283387234,-134.586314540048,
506.462296651428));
#271223=CARTESIAN_POINT('Ctrl Pts',(76.4770599218137,-140.605189688823,
504.462296651428));
#271224=CARTESIAN_POINT('Ctrl Pts',(65.4111915049041,-146.624064837599,
502.462296651428));
#271225=CARTESIAN_POINT('Ctrl Pts',(53.5400027769198,-150.837754439537,
500.462296651428));
#271226=CARTESIAN_POINT('Ctrl Pts',(41.6688140489356,-155.051444041475,
498.462296651428));
#271227=CARTESIAN_POINT('Ctrl Pts',(29.2846130745764,-157.356193074143,
496.462296651428));
#271228=CARTESIAN_POINT('Ctrl Pts',(16.9004121002171,-159.660942106811,
494.462296651428));
#271229=CARTESIAN_POINT('Ctrl Pts',(4.30813900827814,-160.,492.462296651428));
#271230=CARTESIAN_POINT('Ctrl Pts',(-8.28413408366082,-160.339057893189,
490.462296651428));
#271231=CARTESIAN_POINT('Ctrl Pts',(-20.7744157382975,-158.704075916301,
488.462296651428));
#271232=CARTESIAN_POINT('Ctrl Pts',(-33.2646973929342,-157.069093939413,
486.462296651428));
#271233=CARTESIAN_POINT('Ctrl Pts',(-45.3454354230633,-153.500330774912,
484.462296651428));
#271234=CARTESIAN_POINT('Ctrl Pts',(-57.4261734531924,-149.931567610412,
482.462296651428));
#271235=CARTESIAN_POINT('Ctrl Pts',(-68.7998999948413,-144.516898051455,
480.462296651428));
#271236=CARTESIAN_POINT('Ctrl Pts',(-80.1736265364901,-139.102228492497,
478.462296651428));
#271237=CARTESIAN_POINT('Ctrl Pts',(-90.5602826949691,-131.974979673883,
476.462296651428));
#271238=CARTESIAN_POINT('Ctrl Pts',(-100.946938853448,-124.847730855269,
474.462296651428));
#271239=CARTESIAN_POINT('Ctrl Pts',(-110.0907706828,-116.183399296895,472.462296651428));
#271240=CARTESIAN_POINT('Ctrl Pts',(-119.234602512152,-107.519067738521,
470.462296651428));
#271241=CARTESIAN_POINT('Ctrl Pts',(-126.9104585261,-97.5309980386224,468.462296651428));
#271242=CARTESIAN_POINT('Ctrl Pts',(-134.586314540048,-87.5429283387234,
466.462296651428));
#271243=CARTESIAN_POINT('Ctrl Pts',(-140.605189688823,-76.4770599218137,
464.462296651428));
#271244=CARTESIAN_POINT('Ctrl Pts',(-146.624064837599,-65.4111915049041,
462.462296651428));
#271245=CARTESIAN_POINT('Ctrl Pts',(-150.837754439537,-53.5400027769199,
460.462296651428));
#271246=CARTESIAN_POINT('Ctrl Pts',(-155.051444041475,-41.6688140489356,
458.462296651428));
#271247=CARTESIAN_POINT('Ctrl Pts',(-157.356193074143,-29.2846130745764,
456.462296651428));
#271248=CARTESIAN_POINT('Ctrl Pts',(-159.660942106811,-16.9004121002171,
454.462296651429));
#271249=CARTESIAN_POINT('Ctrl Pts',(-160.,-4.30813900827815,452.462296651428));
#271250=CARTESIAN_POINT('Ctrl Pts',(-160.339057893189,8.28413408366081,
450.462296651428));
#271251=CARTESIAN_POINT('Ctrl Pts',(-158.704075916301,20.7744157382975,
448.462296651428));
#271252=CARTESIAN_POINT('Ctrl Pts',(-157.069093939413,33.2646973929342,
446.462296651428));
#271253=CARTESIAN_POINT('Ctrl Pts',(-153.500330774912,45.3454354230633,
444.462296651428));
#271254=CARTESIAN_POINT('Ctrl Pts',(-149.931567610412,57.4261734531924,
442.462296651428));
#271255=CARTESIAN_POINT('Ctrl Pts',(-144.516898051455,68.7998999948413,
440.462296651428));
#271256=CARTESIAN_POINT('Ctrl Pts',(-139.102228492497,80.1736265364901,
438.462296651428));
#271257=CARTESIAN_POINT('Ctrl Pts',(-131.974979673883,90.5602826949691,
436.462296651428));
#271258=CARTESIAN_POINT('Ctrl Pts',(-124.847730855269,100.946938853448,
434.462296651428));
#271259=CARTESIAN_POINT('Ctrl Pts',(-116.183399296895,110.0907706828,432.462296651428));
#271260=CARTESIAN_POINT('Ctrl Pts',(-107.519067738521,119.234602512152,
430.462296651428));
#271261=CARTESIAN_POINT('Ctrl Pts',(-97.5309980386224,126.9104585261,428.462296651428));
#271262=CARTESIAN_POINT('Ctrl Pts',(-87.5429283387233,134.586314540048,
426.462296651428));
#271263=CARTESIAN_POINT('Ctrl Pts',(-76.4770599218137,140.605189688823,
424.462296651428));
#271264=CARTESIAN_POINT('Ctrl Pts',(-65.4111915049042,146.624064837599,
422.462296651428));
#271265=CARTESIAN_POINT('Ctrl Pts',(-53.5400027769199,150.837754439537,
420.462296651428));
#271266=CARTESIAN_POINT('Ctrl Pts',(-41.6688140489356,155.051444041475,
418.462296651428));
#271267=CARTESIAN_POINT('Ctrl Pts',(-29.2846130745764,157.356193074143,
416.462296651428));
#271268=CARTESIAN_POINT('Ctrl Pts',(-16.9004121002172,159.660942106811,
414.462296651428));
#271269=CARTESIAN_POINT('Ctrl Pts',(-4.30813900827816,160.,412.462296651428));
#271270=CARTESIAN_POINT('Ctrl Pts',(8.28413408366087,160.339057893189,410.462296651428));
#271271=CARTESIAN_POINT('Ctrl Pts',(20.7744157382975,158.704075916301,408.462296651428));
#271272=CARTESIAN_POINT('Ctrl Pts',(33.2646973929342,157.069093939413,406.462296651428));
#271273=CARTESIAN_POINT('Ctrl Pts',(45.3454354230633,153.500330774912,404.462296651428));
#271274=CARTESIAN_POINT('Ctrl Pts',(57.4261734531925,149.931567610412,402.462296651428));
#271275=CARTESIAN_POINT('Ctrl Pts',(68.7998999948413,144.516898051455,400.462296651428));
#271276=CARTESIAN_POINT('Ctrl Pts',(80.1736265364901,139.102228492498,398.462296651428));
#271277=CARTESIAN_POINT('Ctrl Pts',(90.560282694969,131.974979673883,396.462296651428));
#271278=CARTESIAN_POINT('Ctrl Pts',(100.946938853448,124.847730855269,394.462296651428));
#271279=CARTESIAN_POINT('Ctrl Pts',(110.0907706828,116.183399296895,392.462296651428));
#271280=CARTESIAN_POINT('Ctrl Pts',(119.234602512152,107.519067738521,390.462296651428));
#271281=CARTESIAN_POINT('Ctrl Pts',(126.9104585261,97.5309980386224,388.462296651428));
#271282=CARTESIAN_POINT('Ctrl Pts',(134.586314540048,87.5429283387233,386.462296651428));
#271283=CARTESIAN_POINT('Ctrl Pts',(140.605189688823,76.4770599218137,384.462296651428));
#271284=CARTESIAN_POINT('Ctrl Pts',(146.624064837599,65.4111915049042,382.462296651428));
#271285=CARTESIAN_POINT('Ctrl Pts',(150.837754439537,53.5400027769199,380.462296651428));
#271286=CARTESIAN_POINT('Ctrl Pts',(155.051444041475,41.6688140489356,378.462296651428));
#271287=CARTESIAN_POINT('Ctrl Pts',(157.356193074143,29.2846130745764,376.462296651428));
#271288=CARTESIAN_POINT('Ctrl Pts',(159.394142202012,18.3340187941081,374.693818523023));
#271289=CARTESIAN_POINT('Ctrl Pts',(159.895664541343,7.20669984090294,372.923108716584));
#271290=CARTESIAN_POINT('Ctrl Pts',(160.,-4.30813900827805,537.537703348572));
#271291=CARTESIAN_POINT('Ctrl Pts',(159.660942106811,-16.900412100217,535.537703348572));
#271292=CARTESIAN_POINT('Ctrl Pts',(157.356193074143,-29.2846130745763,
533.537703348572));
#271293=CARTESIAN_POINT('Ctrl Pts',(155.051444041475,-41.6688140489355,
531.537703348572));
#271294=CARTESIAN_POINT('Ctrl Pts',(150.837754439537,-53.5400027769198,
529.537703348572));
#271295=CARTESIAN_POINT('Ctrl Pts',(146.624064837599,-65.411191504904,527.537703348572));
#271296=CARTESIAN_POINT('Ctrl Pts',(140.605189688823,-76.4770599218136,
525.537703348572));
#271297=CARTESIAN_POINT('Ctrl Pts',(134.586314540048,-87.5429283387233,
523.537703348572));
#271298=CARTESIAN_POINT('Ctrl Pts',(126.9104585261,-97.5309980386223,521.537703348572));
#271299=CARTESIAN_POINT('Ctrl Pts',(119.234602512152,-107.519067738521,
519.537703348572));
#271300=CARTESIAN_POINT('Ctrl Pts',(110.0907706828,-116.183399296895,517.537703348572));
#271301=CARTESIAN_POINT('Ctrl Pts',(100.946938853448,-124.847730855269,
515.537703348572));
#271302=CARTESIAN_POINT('Ctrl Pts',(90.5602826949691,-131.974979673883,
513.537703348572));
#271303=CARTESIAN_POINT('Ctrl Pts',(80.1736265364902,-139.102228492497,
511.537703348572));
#271304=CARTESIAN_POINT('Ctrl Pts',(68.7998999948414,-144.516898051454,
509.537703348572));
#271305=CARTESIAN_POINT('Ctrl Pts',(57.4261734531925,-149.931567610412,
507.537703348572));
#271306=CARTESIAN_POINT('Ctrl Pts',(45.3454354230634,-153.500330774912,
505.537703348572));
#271307=CARTESIAN_POINT('Ctrl Pts',(33.2646973929343,-157.069093939413,
503.537703348572));
#271308=CARTESIAN_POINT('Ctrl Pts',(20.7744157382976,-158.704075916301,
501.537703348572));
#271309=CARTESIAN_POINT('Ctrl Pts',(8.28413408366091,-160.339057893189,
499.537703348572));
#271310=CARTESIAN_POINT('Ctrl Pts',(-4.30813900827804,-160.,497.537703348572));
#271311=CARTESIAN_POINT('Ctrl Pts',(-16.900412100217,-159.660942106811,
495.537703348572));
#271312=CARTESIAN_POINT('Ctrl Pts',(-29.2846130745763,-157.356193074143,
493.537703348572));
#271313=CARTESIAN_POINT('Ctrl Pts',(-41.6688140489355,-155.051444041475,
491.537703348572));
#271314=CARTESIAN_POINT('Ctrl Pts',(-53.5400027769198,-150.837754439537,
489.537703348572));
#271315=CARTESIAN_POINT('Ctrl Pts',(-65.411191504904,-146.624064837599,
487.537703348572));
#271316=CARTESIAN_POINT('Ctrl Pts',(-76.4770599218136,-140.605189688823,
485.537703348572));
#271317=CARTESIAN_POINT('Ctrl Pts',(-87.5429283387233,-134.586314540048,
483.537703348572));
#271318=CARTESIAN_POINT('Ctrl Pts',(-97.5309980386223,-126.9104585261,481.537703348572));
#271319=CARTESIAN_POINT('Ctrl Pts',(-107.519067738521,-119.234602512152,
479.537703348572));
#271320=CARTESIAN_POINT('Ctrl Pts',(-116.183399296895,-110.0907706828,477.537703348572));
#271321=CARTESIAN_POINT('Ctrl Pts',(-124.847730855269,-100.946938853448,
475.537703348572));
#271322=CARTESIAN_POINT('Ctrl Pts',(-131.974979673883,-90.5602826949692,
473.537703348572));
#271323=CARTESIAN_POINT('Ctrl Pts',(-139.102228492497,-80.1736265364902,
471.537703348572));
#271324=CARTESIAN_POINT('Ctrl Pts',(-144.516898051454,-68.7998999948414,
469.537703348572));
#271325=CARTESIAN_POINT('Ctrl Pts',(-149.931567610412,-57.4261734531925,
467.537703348572));
#271326=CARTESIAN_POINT('Ctrl Pts',(-153.500330774912,-45.3454354230634,
465.537703348572));
#271327=CARTESIAN_POINT('Ctrl Pts',(-157.069093939413,-33.2646973929344,
463.537703348572));
#271328=CARTESIAN_POINT('Ctrl Pts',(-158.704075916301,-20.7744157382976,
461.537703348572));
#271329=CARTESIAN_POINT('Ctrl Pts',(-160.339057893189,-8.28413408366092,
459.537703348572));
#271330=CARTESIAN_POINT('Ctrl Pts',(-160.,4.30813900827803,457.537703348572));
#271331=CARTESIAN_POINT('Ctrl Pts',(-159.660942106811,16.900412100217,455.537703348572));
#271332=CARTESIAN_POINT('Ctrl Pts',(-157.356193074143,29.2846130745763,
453.537703348572));
#271333=CARTESIAN_POINT('Ctrl Pts',(-155.051444041475,41.6688140489355,
451.537703348572));
#271334=CARTESIAN_POINT('Ctrl Pts',(-150.837754439537,53.5400027769198,
449.537703348572));
#271335=CARTESIAN_POINT('Ctrl Pts',(-146.624064837599,65.411191504904,447.537703348572));
#271336=CARTESIAN_POINT('Ctrl Pts',(-140.605189688823,76.4770599218136,
445.537703348572));
#271337=CARTESIAN_POINT('Ctrl Pts',(-134.586314540048,87.5429283387233,
443.537703348572));
#271338=CARTESIAN_POINT('Ctrl Pts',(-126.9104585261,97.5309980386223,441.537703348572));
#271339=CARTESIAN_POINT('Ctrl Pts',(-119.234602512152,107.519067738521,
439.537703348572));
#271340=CARTESIAN_POINT('Ctrl Pts',(-110.0907706828,116.183399296895,437.537703348572));
#271341=CARTESIAN_POINT('Ctrl Pts',(-100.946938853448,124.847730855269,
435.537703348572));
#271342=CARTESIAN_POINT('Ctrl Pts',(-90.5602826949692,131.974979673883,
433.537703348572));
#271343=CARTESIAN_POINT('Ctrl Pts',(-80.1736265364901,139.102228492497,
431.537703348572));
#271344=CARTESIAN_POINT('Ctrl Pts',(-68.7998999948414,144.516898051454,
429.537703348572));
#271345=CARTESIAN_POINT('Ctrl Pts',(-57.4261734531926,149.931567610412,
427.537703348572));
#271346=CARTESIAN_POINT('Ctrl Pts',(-45.3454354230634,153.500330774912,
425.537703348572));
#271347=CARTESIAN_POINT('Ctrl Pts',(-33.2646973929343,157.069093939413,
423.537703348572));
#271348=CARTESIAN_POINT('Ctrl Pts',(-20.7744157382976,158.704075916301,
421.537703348572));
#271349=CARTESIAN_POINT('Ctrl Pts',(-8.284134083661,160.339057893189,419.537703348572));
#271350=CARTESIAN_POINT('Ctrl Pts',(4.30813900827803,160.,417.537703348572));
#271351=CARTESIAN_POINT('Ctrl Pts',(16.9004121002171,159.660942106811,415.537703348572));
#271352=CARTESIAN_POINT('Ctrl Pts',(29.2846130745762,157.356193074143,413.537703348572));
#271353=CARTESIAN_POINT('Ctrl Pts',(41.6688140489354,155.051444041476,411.537703348572));
#271354=CARTESIAN_POINT('Ctrl Pts',(53.5400027769198,150.837754439537,409.537703348572));
#271355=CARTESIAN_POINT('Ctrl Pts',(65.4111915049041,146.624064837599,407.537703348572));
#271356=CARTESIAN_POINT('Ctrl Pts',(76.4770599218136,140.605189688823,405.537703348572));
#271357=CARTESIAN_POINT('Ctrl Pts',(87.5429283387232,134.586314540048,403.537703348572));
#271358=CARTESIAN_POINT('Ctrl Pts',(97.5309980386223,126.9104585261,401.537703348572));
#271359=CARTESIAN_POINT('Ctrl Pts',(107.519067738521,119.234602512152,399.537703348572));
#271360=CARTESIAN_POINT('Ctrl Pts',(116.183399296895,110.0907706828,397.537703348572));
#271361=CARTESIAN_POINT('Ctrl Pts',(124.847730855269,100.946938853448,395.537703348572));
#271362=CARTESIAN_POINT('Ctrl Pts',(131.974979673883,90.5602826949692,393.537703348572));
#271363=CARTESIAN_POINT('Ctrl Pts',(139.102228492497,80.1736265364902,391.537703348572));
#271364=CARTESIAN_POINT('Ctrl Pts',(144.516898051454,68.7998999948414,389.537703348572));
#271365=CARTESIAN_POINT('Ctrl Pts',(149.931567610412,57.4261734531926,387.537703348572));
#271366=CARTESIAN_POINT('Ctrl Pts',(153.500330774912,45.3454354230634,385.537703348572));
#271367=CARTESIAN_POINT('Ctrl Pts',(157.069093939413,33.2646973929343,383.537703348572));
#271368=CARTESIAN_POINT('Ctrl Pts',(158.704075916301,20.7744157382976,381.537703348572));
#271369=CARTESIAN_POINT('Ctrl Pts',(160.339057893189,8.28413408366101,379.537703348572));
#271370=CARTESIAN_POINT('Ctrl Pts',(160.,-4.30813900827805,377.537703348572));
#271371=CARTESIAN_POINT('Ctrl Pts',(130.,-4.30813900827807,537.537703348572));
#271372=CARTESIAN_POINT('Ctrl Pts',(129.660942106811,-14.5393608954785,
535.537703348572));
#271373=CARTESIAN_POINT('Ctrl Pts',(127.725542856289,-24.5915791233694,
533.537703348572));
#271374=CARTESIAN_POINT('Ctrl Pts',(125.790143605767,-34.6437973512603,
531.537703348572));
#271375=CARTESIAN_POINT('Ctrl Pts',(122.306058950682,-44.2694929456714,
529.537703348572));
#271376=CARTESIAN_POINT('Ctrl Pts',(118.821974295598,-53.8951885400825,
527.537703348572));
#271377=CARTESIAN_POINT('Ctrl Pts',(113.874993963172,-62.8573449296272,
525.537703348572));
#271378=CARTESIAN_POINT('Ctrl Pts',(108.928013630747,-71.819501319172,523.537703348572));
#271379=CARTESIAN_POINT('Ctrl Pts',(102.639948694851,-79.8974404698481,
521.537703348572));
#271380=CARTESIAN_POINT('Ctrl Pts',(96.351883758956,-87.9753796205242,519.537703348572));
#271381=CARTESIAN_POINT('Ctrl Pts',(88.8775672472035,-94.9701958612989,
517.537703348572));
#271382=CARTESIAN_POINT('Ctrl Pts',(81.403250735451,-101.965012102074,515.537703348572));
#271383=CARTESIAN_POINT('Ctrl Pts',(72.9267251261949,-107.704469842635,
513.537703348572));
#271384=CARTESIAN_POINT('Ctrl Pts',(64.4501995169389,-113.443927583196,
511.537703348572));
#271385=CARTESIAN_POINT('Ctrl Pts',(55.1801850026549,-117.786702325803,
509.537703348572));
#271386=CARTESIAN_POINT('Ctrl Pts',(45.910170488371,-122.129477068411,507.537703348572));
#271387=CARTESIAN_POINT('Ctrl Pts',(36.074925591815,-124.968635286058,505.537703348572));
#271388=CARTESIAN_POINT('Ctrl Pts',(26.239680695259,-127.807793503704,503.537703348572));
#271389=CARTESIAN_POINT('Ctrl Pts',(16.0813817870907,-129.073425698447,
501.537703348572));
#271390=CARTESIAN_POINT('Ctrl Pts',(5.92308287892234,-130.339057893189,
499.537703348572));
#271391=CARTESIAN_POINT('Ctrl Pts',(-4.30813900827806,-130.,497.537703348572));
#271392=CARTESIAN_POINT('Ctrl Pts',(-14.5393608954785,-129.660942106811,
495.537703348572));
#271393=CARTESIAN_POINT('Ctrl Pts',(-24.5915791233694,-127.725542856289,
493.537703348572));
#271394=CARTESIAN_POINT('Ctrl Pts',(-34.6437973512603,-125.790143605767,
491.537703348572));
#271395=CARTESIAN_POINT('Ctrl Pts',(-44.2694929456713,-122.306058950682,
489.537703348572));
#271396=CARTESIAN_POINT('Ctrl Pts',(-53.8951885400825,-118.821974295598,
487.537703348572));
#271397=CARTESIAN_POINT('Ctrl Pts',(-62.8573449296272,-113.874993963172,
485.537703348572));
#271398=CARTESIAN_POINT('Ctrl Pts',(-71.819501319172,-108.928013630747,
483.537703348572));
#271399=CARTESIAN_POINT('Ctrl Pts',(-79.8974404698481,-102.639948694851,
481.537703348572));
#271400=CARTESIAN_POINT('Ctrl Pts',(-87.9753796205242,-96.351883758956,
479.537703348572));
#271401=CARTESIAN_POINT('Ctrl Pts',(-94.9701958612989,-88.8775672472035,
477.537703348572));
#271402=CARTESIAN_POINT('Ctrl Pts',(-101.965012102074,-81.403250735451,
475.537703348572));
#271403=CARTESIAN_POINT('Ctrl Pts',(-107.704469842635,-72.9267251261949,
473.537703348572));
#271404=CARTESIAN_POINT('Ctrl Pts',(-113.443927583196,-64.4501995169389,
471.537703348572));
#271405=CARTESIAN_POINT('Ctrl Pts',(-117.786702325803,-55.1801850026549,
469.537703348572));
#271406=CARTESIAN_POINT('Ctrl Pts',(-122.129477068411,-45.910170488371,
467.537703348572));
#271407=CARTESIAN_POINT('Ctrl Pts',(-124.968635286058,-36.074925591815,
465.537703348572));
#271408=CARTESIAN_POINT('Ctrl Pts',(-127.807793503704,-26.239680695259,
463.537703348572));
#271409=CARTESIAN_POINT('Ctrl Pts',(-129.073425698447,-16.0813817870907,
461.537703348572));
#271410=CARTESIAN_POINT('Ctrl Pts',(-130.339057893189,-5.92308287892235,
459.537703348572));
#271411=CARTESIAN_POINT('Ctrl Pts',(-130.,4.30813900827805,457.537703348572));
#271412=CARTESIAN_POINT('Ctrl Pts',(-129.660942106811,14.5393608954784,
455.537703348572));
#271413=CARTESIAN_POINT('Ctrl Pts',(-127.725542856289,24.5915791233693,
453.537703348572));
#271414=CARTESIAN_POINT('Ctrl Pts',(-125.790143605767,34.6437973512602,
451.537703348572));
#271415=CARTESIAN_POINT('Ctrl Pts',(-122.306058950682,44.2694929456713,
449.537703348572));
#271416=CARTESIAN_POINT('Ctrl Pts',(-118.821974295598,53.8951885400825,
447.537703348572));
#271417=CARTESIAN_POINT('Ctrl Pts',(-113.874993963172,62.8573449296272,
445.537703348572));
#271418=CARTESIAN_POINT('Ctrl Pts',(-108.928013630747,71.819501319172,443.537703348572));
#271419=CARTESIAN_POINT('Ctrl Pts',(-102.639948694851,79.8974404698481,
441.537703348572));
#271420=CARTESIAN_POINT('Ctrl Pts',(-96.3518837589561,87.9753796205242,
439.537703348572));
#271421=CARTESIAN_POINT('Ctrl Pts',(-88.8775672472035,94.9701958612989,
437.537703348572));
#271422=CARTESIAN_POINT('Ctrl Pts',(-81.403250735451,101.965012102074,435.537703348572));
#271423=CARTESIAN_POINT('Ctrl Pts',(-72.9267251261949,107.704469842635,
433.537703348572));
#271424=CARTESIAN_POINT('Ctrl Pts',(-64.4501995169389,113.443927583196,
431.537703348572));
#271425=CARTESIAN_POINT('Ctrl Pts',(-55.1801850026549,117.786702325803,
429.537703348572));
#271426=CARTESIAN_POINT('Ctrl Pts',(-45.910170488371,122.129477068411,427.537703348572));
#271427=CARTESIAN_POINT('Ctrl Pts',(-36.074925591815,124.968635286058,425.537703348572));
#271428=CARTESIAN_POINT('Ctrl Pts',(-26.239680695259,127.807793503704,423.537703348572));
#271429=CARTESIAN_POINT('Ctrl Pts',(-16.0813817870907,129.073425698447,
421.537703348572));
#271430=CARTESIAN_POINT('Ctrl Pts',(-5.92308287892242,130.339057893189,
419.537703348572));
#271431=CARTESIAN_POINT('Ctrl Pts',(4.30813900827804,130.,417.537703348572));
#271432=CARTESIAN_POINT('Ctrl Pts',(14.5393608954785,129.660942106811,415.537703348572));
#271433=CARTESIAN_POINT('Ctrl Pts',(24.5915791233693,127.725542856289,413.537703348572));
#271434=CARTESIAN_POINT('Ctrl Pts',(34.6437973512602,125.790143605767,411.537703348572));
#271435=CARTESIAN_POINT('Ctrl Pts',(44.2694929456713,122.306058950682,409.537703348572));
#271436=CARTESIAN_POINT('Ctrl Pts',(53.8951885400825,118.821974295598,407.537703348572));
#271437=CARTESIAN_POINT('Ctrl Pts',(62.8573449296272,113.874993963172,405.537703348572));
#271438=CARTESIAN_POINT('Ctrl Pts',(71.819501319172,108.928013630747,403.537703348572));
#271439=CARTESIAN_POINT('Ctrl Pts',(79.8974404698481,102.639948694851,401.537703348572));
#271440=CARTESIAN_POINT('Ctrl Pts',(87.9753796205242,96.351883758956,399.537703348572));
#271441=CARTESIAN_POINT('Ctrl Pts',(94.9701958612989,88.8775672472035,397.537703348572));
#271442=CARTESIAN_POINT('Ctrl Pts',(101.965012102074,81.403250735451,395.537703348572));
#271443=CARTESIAN_POINT('Ctrl Pts',(107.704469842635,72.926725126195,393.537703348572));
#271444=CARTESIAN_POINT('Ctrl Pts',(113.443927583196,64.4501995169389,391.537703348572));
#271445=CARTESIAN_POINT('Ctrl Pts',(117.786702325803,55.1801850026549,389.537703348572));
#271446=CARTESIAN_POINT('Ctrl Pts',(122.129477068411,45.910170488371,387.537703348572));
#271447=CARTESIAN_POINT('Ctrl Pts',(124.968635286058,36.074925591815,385.537703348572));
#271448=CARTESIAN_POINT('Ctrl Pts',(127.807793503704,26.239680695259,383.537703348572));
#271449=CARTESIAN_POINT('Ctrl Pts',(129.073425698447,16.0813817870907,381.537703348572));
#271450=CARTESIAN_POINT('Ctrl Pts',(130.339057893189,5.92308287892242,379.537703348572));
#271451=CARTESIAN_POINT('Ctrl Pts',(130.,-4.30813900827807,377.537703348572));
#271452=CARTESIAN_POINT('Ctrl Pts',(159.895664541343,-7.20669984090288,
537.076891283416));
#271453=CARTESIAN_POINT('Ctrl Pts',(159.394142202012,-18.334018794108,535.306181476978));
#271454=CARTESIAN_POINT('Ctrl Pts',(157.356193074143,-29.2846130745763,
533.537703348572));
#271455=CARTESIAN_POINT('Ctrl Pts',(155.051444041475,-41.6688140489355,
531.537703348572));
#271456=CARTESIAN_POINT('Ctrl Pts',(150.837754439537,-53.5400027769198,
529.537703348572));
#271457=CARTESIAN_POINT('Ctrl Pts',(146.624064837599,-65.411191504904,527.537703348572));
#271458=CARTESIAN_POINT('Ctrl Pts',(140.605189688823,-76.4770599218136,
525.537703348572));
#271459=CARTESIAN_POINT('Ctrl Pts',(134.586314540048,-87.5429283387233,
523.537703348572));
#271460=CARTESIAN_POINT('Ctrl Pts',(126.9104585261,-97.5309980386223,521.537703348572));
#271461=CARTESIAN_POINT('Ctrl Pts',(119.234602512152,-107.519067738521,
519.537703348572));
#271462=CARTESIAN_POINT('Ctrl Pts',(110.0907706828,-116.183399296895,517.537703348572));
#271463=CARTESIAN_POINT('Ctrl Pts',(100.946938853448,-124.847730855269,
515.537703348572));
#271464=CARTESIAN_POINT('Ctrl Pts',(90.5602826949691,-131.974979673883,
513.537703348572));
#271465=CARTESIAN_POINT('Ctrl Pts',(80.1736265364902,-139.102228492497,
511.537703348572));
#271466=CARTESIAN_POINT('Ctrl Pts',(68.7998999948414,-144.516898051454,
509.537703348572));
#271467=CARTESIAN_POINT('Ctrl Pts',(57.4261734531925,-149.931567610412,
507.537703348572));
#271468=CARTESIAN_POINT('Ctrl Pts',(45.3454354230634,-153.500330774912,
505.537703348572));
#271469=CARTESIAN_POINT('Ctrl Pts',(33.2646973929343,-157.069093939413,
503.537703348572));
#271470=CARTESIAN_POINT('Ctrl Pts',(20.7744157382976,-158.704075916301,
501.537703348572));
#271471=CARTESIAN_POINT('Ctrl Pts',(8.28413408366091,-160.339057893189,
499.537703348572));
#271472=CARTESIAN_POINT('Ctrl Pts',(-4.30813900827804,-160.,497.537703348572));
#271473=CARTESIAN_POINT('Ctrl Pts',(-16.900412100217,-159.660942106811,
495.537703348572));
#271474=CARTESIAN_POINT('Ctrl Pts',(-29.2846130745763,-157.356193074143,
493.537703348572));
#271475=CARTESIAN_POINT('Ctrl Pts',(-41.6688140489355,-155.051444041475,
491.537703348572));
#271476=CARTESIAN_POINT('Ctrl Pts',(-53.5400027769198,-150.837754439537,
489.537703348572));
#271477=CARTESIAN_POINT('Ctrl Pts',(-65.411191504904,-146.624064837599,
487.537703348572));
#271478=CARTESIAN_POINT('Ctrl Pts',(-76.4770599218136,-140.605189688823,
485.537703348572));
#271479=CARTESIAN_POINT('Ctrl Pts',(-87.5429283387233,-134.586314540048,
483.537703348572));
#271480=CARTESIAN_POINT('Ctrl Pts',(-97.5309980386223,-126.9104585261,481.537703348572));
#271481=CARTESIAN_POINT('Ctrl Pts',(-107.519067738521,-119.234602512152,
479.537703348572));
#271482=CARTESIAN_POINT('Ctrl Pts',(-116.183399296895,-110.0907706828,477.537703348572));
#271483=CARTESIAN_POINT('Ctrl Pts',(-124.847730855269,-100.946938853448,
475.537703348572));
#271484=CARTESIAN_POINT('Ctrl Pts',(-131.974979673883,-90.5602826949692,
473.537703348572));
#271485=CARTESIAN_POINT('Ctrl Pts',(-139.102228492497,-80.1736265364902,
471.537703348572));
#271486=CARTESIAN_POINT('Ctrl Pts',(-144.516898051454,-68.7998999948414,
469.537703348572));
#271487=CARTESIAN_POINT('Ctrl Pts',(-149.931567610412,-57.4261734531925,
467.537703348572));
#271488=CARTESIAN_POINT('Ctrl Pts',(-153.500330774912,-45.3454354230634,
465.537703348572));
#271489=CARTESIAN_POINT('Ctrl Pts',(-157.069093939413,-33.2646973929344,
463.537703348572));
#271490=CARTESIAN_POINT('Ctrl Pts',(-158.704075916301,-20.7744157382976,
461.537703348572));
#271491=CARTESIAN_POINT('Ctrl Pts',(-160.339057893189,-8.28413408366092,
459.537703348572));
#271492=CARTESIAN_POINT('Ctrl Pts',(-160.,4.30813900827803,457.537703348572));
#271493=CARTESIAN_POINT('Ctrl Pts',(-159.660942106811,16.900412100217,455.537703348572));
#271494=CARTESIAN_POINT('Ctrl Pts',(-157.356193074143,29.2846130745763,
453.537703348572));
#271495=CARTESIAN_POINT('Ctrl Pts',(-155.051444041475,41.6688140489355,
451.537703348572));
#271496=CARTESIAN_POINT('Ctrl Pts',(-150.837754439537,53.5400027769198,
449.537703348572));
#271497=CARTESIAN_POINT('Ctrl Pts',(-146.624064837599,65.411191504904,447.537703348572));
#271498=CARTESIAN_POINT('Ctrl Pts',(-140.605189688823,76.4770599218136,
445.537703348572));
#271499=CARTESIAN_POINT('Ctrl Pts',(-134.586314540048,87.5429283387233,
443.537703348572));
#271500=CARTESIAN_POINT('Ctrl Pts',(-126.9104585261,97.5309980386223,441.537703348572));
#271501=CARTESIAN_POINT('Ctrl Pts',(-119.234602512152,107.519067738521,
439.537703348572));
#271502=CARTESIAN_POINT('Ctrl Pts',(-110.0907706828,116.183399296895,437.537703348572));
#271503=CARTESIAN_POINT('Ctrl Pts',(-100.946938853448,124.847730855269,
435.537703348572));
#271504=CARTESIAN_POINT('Ctrl Pts',(-90.5602826949692,131.974979673883,
433.537703348572));
#271505=CARTESIAN_POINT('Ctrl Pts',(-80.1736265364902,139.102228492497,
431.537703348572));
#271506=CARTESIAN_POINT('Ctrl Pts',(-68.7998999948414,144.516898051454,
429.537703348572));
#271507=CARTESIAN_POINT('Ctrl Pts',(-57.4261734531926,149.931567610412,
427.537703348572));
#271508=CARTESIAN_POINT('Ctrl Pts',(-45.3454354230634,153.500330774912,
425.537703348572));
#271509=CARTESIAN_POINT('Ctrl Pts',(-33.2646973929343,157.069093939413,
423.537703348572));
#271510=CARTESIAN_POINT('Ctrl Pts',(-20.7744157382976,158.704075916301,
421.537703348572));
#271511=CARTESIAN_POINT('Ctrl Pts',(-8.284134083661,160.339057893189,419.537703348572));
#271512=CARTESIAN_POINT('Ctrl Pts',(4.30813900827803,160.,417.537703348572));
#271513=CARTESIAN_POINT('Ctrl Pts',(16.9004121002171,159.660942106811,415.537703348572));
#271514=CARTESIAN_POINT('Ctrl Pts',(29.2846130745762,157.356193074143,413.537703348572));
#271515=CARTESIAN_POINT('Ctrl Pts',(41.6688140489354,155.051444041476,411.537703348572));
#271516=CARTESIAN_POINT('Ctrl Pts',(53.5400027769198,150.837754439537,409.537703348572));
#271517=CARTESIAN_POINT('Ctrl Pts',(65.4111915049041,146.624064837599,407.537703348572));
#271518=CARTESIAN_POINT('Ctrl Pts',(76.4770599218136,140.605189688823,405.537703348572));
#271519=CARTESIAN_POINT('Ctrl Pts',(87.5429283387232,134.586314540048,403.537703348572));
#271520=CARTESIAN_POINT('Ctrl Pts',(97.5309980386223,126.9104585261,401.537703348572));
#271521=CARTESIAN_POINT('Ctrl Pts',(107.519067738521,119.234602512152,399.537703348572));
#271522=CARTESIAN_POINT('Ctrl Pts',(116.183399296895,110.0907706828,397.537703348572));
#271523=CARTESIAN_POINT('Ctrl Pts',(124.847730855269,100.946938853448,395.537703348572));
#271524=CARTESIAN_POINT('Ctrl Pts',(131.974979673883,90.5602826949692,393.537703348572));
#271525=CARTESIAN_POINT('Ctrl Pts',(139.102228492497,80.1736265364902,391.537703348572));
#271526=CARTESIAN_POINT('Ctrl Pts',(144.516898051454,68.7998999948414,389.537703348572));
#271527=CARTESIAN_POINT('Ctrl Pts',(149.931567610412,57.4261734531926,387.537703348572));
#271528=CARTESIAN_POINT('Ctrl Pts',(153.500330774912,45.3454354230634,385.537703348572));
#271529=CARTESIAN_POINT('Ctrl Pts',(157.069093939413,33.2646973929343,383.537703348572));
#271530=CARTESIAN_POINT('Ctrl Pts',(158.704075916301,20.7744157382976,381.537703348572));
#271531=CARTESIAN_POINT('Ctrl Pts',(159.653854600275,13.5186762622035,380.375881753716));
#271532=CARTESIAN_POINT('Ctrl Pts',(159.937609420477,6.20654127333073,379.210563551645));
#271533=CARTESIAN_POINT('Ctrl Pts',(160.,4.30813900827813,532.462296651428));
#271534=CARTESIAN_POINT('Ctrl Pts',(160.339057893189,-8.28413408366083,
530.462296651428));
#271535=CARTESIAN_POINT('Ctrl Pts',(158.704075916301,-20.7744157382975,
528.462296651428));
#271536=CARTESIAN_POINT('Ctrl Pts',(157.069093939413,-33.2646973929343,
526.462296651428));
#271537=CARTESIAN_POINT('Ctrl Pts',(153.500330774912,-45.3454354230633,
524.462296651428));
#271538=CARTESIAN_POINT('Ctrl Pts',(149.931567610412,-57.4261734531924,
522.462296651428));
#271539=CARTESIAN_POINT('Ctrl Pts',(144.516898051455,-68.7998999948413,
520.462296651428));
#271540=CARTESIAN_POINT('Ctrl Pts',(139.102228492497,-80.1736265364901,
518.462296651428));
#271541=CARTESIAN_POINT('Ctrl Pts',(131.974979673883,-90.5602826949691,
516.462296651428));
#271542=CARTESIAN_POINT('Ctrl Pts',(124.847730855269,-100.946938853448,
514.462296651428));
#271543=CARTESIAN_POINT('Ctrl Pts',(116.183399296895,-110.0907706828,512.462296651428));
#271544=CARTESIAN_POINT('Ctrl Pts',(107.519067738521,-119.234602512152,
510.462296651428));
#271545=CARTESIAN_POINT('Ctrl Pts',(97.5309980386224,-126.9104585261,508.462296651428));
#271546=CARTESIAN_POINT('Ctrl Pts',(87.5429283387234,-134.586314540048,
506.462296651428));
#271547=CARTESIAN_POINT('Ctrl Pts',(76.4770599218137,-140.605189688823,
504.462296651428));
#271548=CARTESIAN_POINT('Ctrl Pts',(65.4111915049041,-146.624064837599,
502.462296651428));
#271549=CARTESIAN_POINT('Ctrl Pts',(53.5400027769198,-150.837754439537,
500.462296651428));
#271550=CARTESIAN_POINT('Ctrl Pts',(41.6688140489356,-155.051444041475,
498.462296651428));
#271551=CARTESIAN_POINT('Ctrl Pts',(29.2846130745764,-157.356193074143,
496.462296651428));
#271552=CARTESIAN_POINT('Ctrl Pts',(16.9004121002171,-159.660942106811,
494.462296651428));
#271553=CARTESIAN_POINT('Ctrl Pts',(4.30813900827814,-160.,492.462296651428));
#271554=CARTESIAN_POINT('Ctrl Pts',(-8.28413408366082,-160.339057893189,
490.462296651428));
#271555=CARTESIAN_POINT('Ctrl Pts',(-20.7744157382975,-158.704075916301,
488.462296651428));
#271556=CARTESIAN_POINT('Ctrl Pts',(-33.2646973929342,-157.069093939413,
486.462296651428));
#271557=CARTESIAN_POINT('Ctrl Pts',(-45.3454354230633,-153.500330774912,
484.462296651428));
#271558=CARTESIAN_POINT('Ctrl Pts',(-57.4261734531924,-149.931567610412,
482.462296651428));
#271559=CARTESIAN_POINT('Ctrl Pts',(-68.7998999948413,-144.516898051455,
480.462296651428));
#271560=CARTESIAN_POINT('Ctrl Pts',(-80.1736265364901,-139.102228492497,
478.462296651428));
#271561=CARTESIAN_POINT('Ctrl Pts',(-90.5602826949691,-131.974979673883,
476.462296651428));
#271562=CARTESIAN_POINT('Ctrl Pts',(-100.946938853448,-124.847730855269,
474.462296651428));
#271563=CARTESIAN_POINT('Ctrl Pts',(-110.0907706828,-116.183399296895,472.462296651428));
#271564=CARTESIAN_POINT('Ctrl Pts',(-119.234602512152,-107.519067738521,
470.462296651428));
#271565=CARTESIAN_POINT('Ctrl Pts',(-126.9104585261,-97.5309980386224,468.462296651428));
#271566=CARTESIAN_POINT('Ctrl Pts',(-134.586314540048,-87.5429283387234,
466.462296651428));
#271567=CARTESIAN_POINT('Ctrl Pts',(-140.605189688823,-76.4770599218137,
464.462296651428));
#271568=CARTESIAN_POINT('Ctrl Pts',(-146.624064837599,-65.4111915049041,
462.462296651428));
#271569=CARTESIAN_POINT('Ctrl Pts',(-150.837754439537,-53.5400027769199,
460.462296651428));
#271570=CARTESIAN_POINT('Ctrl Pts',(-155.051444041475,-41.6688140489356,
458.462296651428));
#271571=CARTESIAN_POINT('Ctrl Pts',(-157.356193074143,-29.2846130745764,
456.462296651428));
#271572=CARTESIAN_POINT('Ctrl Pts',(-159.660942106811,-16.9004121002171,
454.462296651429));
#271573=CARTESIAN_POINT('Ctrl Pts',(-160.,-4.30813900827815,452.462296651428));
#271574=CARTESIAN_POINT('Ctrl Pts',(-160.339057893189,8.28413408366081,
450.462296651428));
#271575=CARTESIAN_POINT('Ctrl Pts',(-158.704075916301,20.7744157382975,
448.462296651428));
#271576=CARTESIAN_POINT('Ctrl Pts',(-157.069093939413,33.2646973929342,
446.462296651428));
#271577=CARTESIAN_POINT('Ctrl Pts',(-153.500330774912,45.3454354230633,
444.462296651428));
#271578=CARTESIAN_POINT('Ctrl Pts',(-149.931567610412,57.4261734531924,
442.462296651428));
#271579=CARTESIAN_POINT('Ctrl Pts',(-144.516898051455,68.7998999948413,
440.462296651428));
#271580=CARTESIAN_POINT('Ctrl Pts',(-139.102228492497,80.1736265364901,
438.462296651428));
#271581=CARTESIAN_POINT('Ctrl Pts',(-131.974979673883,90.5602826949691,
436.462296651428));
#271582=CARTESIAN_POINT('Ctrl Pts',(-124.847730855269,100.946938853448,
434.462296651428));
#271583=CARTESIAN_POINT('Ctrl Pts',(-116.183399296895,110.0907706828,432.462296651428));
#271584=CARTESIAN_POINT('Ctrl Pts',(-107.519067738521,119.234602512152,
430.462296651428));
#271585=CARTESIAN_POINT('Ctrl Pts',(-97.5309980386224,126.9104585261,428.462296651428));
#271586=CARTESIAN_POINT('Ctrl Pts',(-87.5429283387233,134.586314540048,
426.462296651428));
#271587=CARTESIAN_POINT('Ctrl Pts',(-76.4770599218137,140.605189688823,
424.462296651428));
#271588=CARTESIAN_POINT('Ctrl Pts',(-65.4111915049042,146.624064837599,
422.462296651428));
#271589=CARTESIAN_POINT('Ctrl Pts',(-53.5400027769199,150.837754439537,
420.462296651428));
#271590=CARTESIAN_POINT('Ctrl Pts',(-41.6688140489356,155.051444041475,
418.462296651428));
#271591=CARTESIAN_POINT('Ctrl Pts',(-29.2846130745764,157.356193074143,
416.462296651428));
#271592=CARTESIAN_POINT('Ctrl Pts',(-16.9004121002172,159.660942106811,
414.462296651428));
#271593=CARTESIAN_POINT('Ctrl Pts',(-4.30813900827816,160.,412.462296651428));
#271594=CARTESIAN_POINT('Ctrl Pts',(8.28413408366087,160.339057893189,410.462296651428));
#271595=CARTESIAN_POINT('Ctrl Pts',(20.7744157382975,158.704075916301,408.462296651428));
#271596=CARTESIAN_POINT('Ctrl Pts',(33.2646973929342,157.069093939413,406.462296651428));
#271597=CARTESIAN_POINT('Ctrl Pts',(45.3454354230633,153.500330774912,404.462296651428));
#271598=CARTESIAN_POINT('Ctrl Pts',(57.4261734531925,149.931567610412,402.462296651428));
#271599=CARTESIAN_POINT('Ctrl Pts',(68.7998999948413,144.516898051455,400.462296651428));
#271600=CARTESIAN_POINT('Ctrl Pts',(80.1736265364901,139.102228492498,398.462296651428));
#271601=CARTESIAN_POINT('Ctrl Pts',(90.560282694969,131.974979673883,396.462296651428));
#271602=CARTESIAN_POINT('Ctrl Pts',(100.946938853448,124.847730855269,394.462296651428));
#271603=CARTESIAN_POINT('Ctrl Pts',(110.0907706828,116.183399296895,392.462296651428));
#271604=CARTESIAN_POINT('Ctrl Pts',(119.234602512152,107.519067738521,390.462296651428));
#271605=CARTESIAN_POINT('Ctrl Pts',(126.9104585261,97.5309980386224,388.462296651428));
#271606=CARTESIAN_POINT('Ctrl Pts',(134.586314540048,87.5429283387233,386.462296651428));
#271607=CARTESIAN_POINT('Ctrl Pts',(140.605189688823,76.4770599218137,384.462296651428));
#271608=CARTESIAN_POINT('Ctrl Pts',(146.624064837599,65.4111915049042,382.462296651428));
#271609=CARTESIAN_POINT('Ctrl Pts',(150.837754439537,53.5400027769199,380.462296651428));
#271610=CARTESIAN_POINT('Ctrl Pts',(155.051444041475,41.6688140489356,378.462296651428));
#271611=CARTESIAN_POINT('Ctrl Pts',(157.356193074143,29.2846130745764,376.462296651428));
#271612=CARTESIAN_POINT('Ctrl Pts',(159.660942106811,16.9004121002172,374.462296651428));
#271613=CARTESIAN_POINT('Ctrl Pts',(160.,4.30813900827813,372.462296651428));
#271614=CARTESIAN_POINT('Ctrl Pts',(160.,-4.30813900827805,537.537703348572));
#271615=CARTESIAN_POINT('Ctrl Pts',(159.660942106811,-16.900412100217,535.537703348572));
#271616=CARTESIAN_POINT('Ctrl Pts',(157.356193074143,-29.2846130745763,
533.537703348572));
#271617=CARTESIAN_POINT('Ctrl Pts',(155.051444041475,-41.6688140489355,
531.537703348572));
#271618=CARTESIAN_POINT('Ctrl Pts',(150.837754439537,-53.5400027769198,
529.537703348572));
#271619=CARTESIAN_POINT('Ctrl Pts',(146.624064837599,-65.411191504904,527.537703348572));
#271620=CARTESIAN_POINT('Ctrl Pts',(140.605189688823,-76.4770599218136,
525.537703348572));
#271621=CARTESIAN_POINT('Ctrl Pts',(134.586314540048,-87.5429283387233,
523.537703348572));
#271622=CARTESIAN_POINT('Ctrl Pts',(126.9104585261,-97.5309980386223,521.537703348572));
#271623=CARTESIAN_POINT('Ctrl Pts',(119.234602512152,-107.519067738521,
519.537703348572));
#271624=CARTESIAN_POINT('Ctrl Pts',(110.0907706828,-116.183399296895,517.537703348572));
#271625=CARTESIAN_POINT('Ctrl Pts',(100.946938853448,-124.847730855269,
515.537703348572));
#271626=CARTESIAN_POINT('Ctrl Pts',(90.5602826949691,-131.974979673883,
513.537703348572));
#271627=CARTESIAN_POINT('Ctrl Pts',(80.1736265364902,-139.102228492497,
511.537703348572));
#271628=CARTESIAN_POINT('Ctrl Pts',(68.7998999948414,-144.516898051454,
509.537703348572));
#271629=CARTESIAN_POINT('Ctrl Pts',(57.4261734531925,-149.931567610412,
507.537703348572));
#271630=CARTESIAN_POINT('Ctrl Pts',(45.3454354230634,-153.500330774912,
505.537703348572));
#271631=CARTESIAN_POINT('Ctrl Pts',(33.2646973929343,-157.069093939413,
503.537703348572));
#271632=CARTESIAN_POINT('Ctrl Pts',(20.7744157382976,-158.704075916301,
501.537703348572));
#271633=CARTESIAN_POINT('Ctrl Pts',(8.28413408366091,-160.339057893189,
499.537703348572));
#271634=CARTESIAN_POINT('Ctrl Pts',(-4.30813900827804,-160.,497.537703348572));
#271635=CARTESIAN_POINT('Ctrl Pts',(-16.900412100217,-159.660942106811,
495.537703348572));
#271636=CARTESIAN_POINT('Ctrl Pts',(-29.2846130745763,-157.356193074143,
493.537703348572));
#271637=CARTESIAN_POINT('Ctrl Pts',(-41.6688140489355,-155.051444041475,
491.537703348572));
#271638=CARTESIAN_POINT('Ctrl Pts',(-53.5400027769198,-150.837754439537,
489.537703348572));
#271639=CARTESIAN_POINT('Ctrl Pts',(-65.411191504904,-146.624064837599,
487.537703348572));
#271640=CARTESIAN_POINT('Ctrl Pts',(-76.4770599218136,-140.605189688823,
485.537703348572));
#271641=CARTESIAN_POINT('Ctrl Pts',(-87.5429283387233,-134.586314540048,
483.537703348572));
#271642=CARTESIAN_POINT('Ctrl Pts',(-97.5309980386223,-126.9104585261,481.537703348572));
#271643=CARTESIAN_POINT('Ctrl Pts',(-107.519067738521,-119.234602512152,
479.537703348572));
#271644=CARTESIAN_POINT('Ctrl Pts',(-116.183399296895,-110.0907706828,477.537703348572));
#271645=CARTESIAN_POINT('Ctrl Pts',(-124.847730855269,-100.946938853448,
475.537703348572));
#271646=CARTESIAN_POINT('Ctrl Pts',(-131.974979673883,-90.5602826949692,
473.537703348572));
#271647=CARTESIAN_POINT('Ctrl Pts',(-139.102228492497,-80.1736265364902,
471.537703348572));
#271648=CARTESIAN_POINT('Ctrl Pts',(-144.516898051454,-68.7998999948414,
469.537703348572));
#271649=CARTESIAN_POINT('Ctrl Pts',(-149.931567610412,-57.4261734531925,
467.537703348572));
#271650=CARTESIAN_POINT('Ctrl Pts',(-153.500330774912,-45.3454354230634,
465.537703348572));
#271651=CARTESIAN_POINT('Ctrl Pts',(-157.069093939413,-33.2646973929344,
463.537703348572));
#271652=CARTESIAN_POINT('Ctrl Pts',(-158.704075916301,-20.7744157382976,
461.537703348572));
#271653=CARTESIAN_POINT('Ctrl Pts',(-160.339057893189,-8.28413408366092,
459.537703348572));
#271654=CARTESIAN_POINT('Ctrl Pts',(-160.,4.30813900827803,457.537703348572));
#271655=CARTESIAN_POINT('Ctrl Pts',(-159.660942106811,16.900412100217,455.537703348572));
#271656=CARTESIAN_POINT('Ctrl Pts',(-157.356193074143,29.2846130745763,
453.537703348572));
#271657=CARTESIAN_POINT('Ctrl Pts',(-155.051444041475,41.6688140489355,
451.537703348572));
#271658=CARTESIAN_POINT('Ctrl Pts',(-150.837754439537,53.5400027769198,
449.537703348572));
#271659=CARTESIAN_POINT('Ctrl Pts',(-146.624064837599,65.411191504904,447.537703348572));
#271660=CARTESIAN_POINT('Ctrl Pts',(-140.605189688823,76.4770599218136,
445.537703348572));
#271661=CARTESIAN_POINT('Ctrl Pts',(-134.586314540048,87.5429283387233,
443.537703348572));
#271662=CARTESIAN_POINT('Ctrl Pts',(-126.9104585261,97.5309980386223,441.537703348572));
#271663=CARTESIAN_POINT('Ctrl Pts',(-119.234602512152,107.519067738521,
439.537703348572));
#271664=CARTESIAN_POINT('Ctrl Pts',(-110.0907706828,116.183399296895,437.537703348572));
#271665=CARTESIAN_POINT('Ctrl Pts',(-100.946938853448,124.847730855269,
435.537703348572));
#271666=CARTESIAN_POINT('Ctrl Pts',(-90.5602826949692,131.974979673883,
433.537703348572));
#271667=CARTESIAN_POINT('Ctrl Pts',(-80.1736265364901,139.102228492497,
431.537703348572));
#271668=CARTESIAN_POINT('Ctrl Pts',(-68.7998999948414,144.516898051454,
429.537703348572));
#271669=CARTESIAN_POINT('Ctrl Pts',(-57.4261734531926,149.931567610412,
427.537703348572));
#271670=CARTESIAN_POINT('Ctrl Pts',(-45.3454354230634,153.500330774912,
425.537703348572));
#271671=CARTESIAN_POINT('Ctrl Pts',(-33.2646973929343,157.069093939413,
423.537703348572));
#271672=CARTESIAN_POINT('Ctrl Pts',(-20.7744157382976,158.704075916301,
421.537703348572));
#271673=CARTESIAN_POINT('Ctrl Pts',(-8.284134083661,160.339057893189,419.537703348572));
#271674=CARTESIAN_POINT('Ctrl Pts',(4.30813900827803,160.,417.537703348572));
#271675=CARTESIAN_POINT('Ctrl Pts',(16.9004121002171,159.660942106811,415.537703348572));
#271676=CARTESIAN_POINT('Ctrl Pts',(29.2846130745762,157.356193074143,413.537703348572));
#271677=CARTESIAN_POINT('Ctrl Pts',(41.6688140489354,155.051444041476,411.537703348572));
#271678=CARTESIAN_POINT('Ctrl Pts',(53.5400027769198,150.837754439537,409.537703348572));
#271679=CARTESIAN_POINT('Ctrl Pts',(65.4111915049041,146.624064837599,407.537703348572));
#271680=CARTESIAN_POINT('Ctrl Pts',(76.4770599218136,140.605189688823,405.537703348572));
#271681=CARTESIAN_POINT('Ctrl Pts',(87.5429283387232,134.586314540048,403.537703348572));
#271682=CARTESIAN_POINT('Ctrl Pts',(97.5309980386223,126.9104585261,401.537703348572));
#271683=CARTESIAN_POINT('Ctrl Pts',(107.519067738521,119.234602512152,399.537703348572));
#271684=CARTESIAN_POINT('Ctrl Pts',(116.183399296895,110.0907706828,397.537703348572));
#271685=CARTESIAN_POINT('Ctrl Pts',(124.847730855269,100.946938853448,395.537703348572));
#271686=CARTESIAN_POINT('Ctrl Pts',(131.974979673883,90.5602826949692,393.537703348572));
#271687=CARTESIAN_POINT('Ctrl Pts',(139.102228492497,80.1736265364902,391.537703348572));
#271688=CARTESIAN_POINT('Ctrl Pts',(144.516898051454,68.7998999948414,389.537703348572));
#271689=CARTESIAN_POINT('Ctrl Pts',(149.931567610412,57.4261734531926,387.537703348572));
#271690=CARTESIAN_POINT('Ctrl Pts',(153.500330774912,45.3454354230634,385.537703348572));
#271691=CARTESIAN_POINT('Ctrl Pts',(157.069093939413,33.2646973929343,383.537703348572));
#271692=CARTESIAN_POINT('Ctrl Pts',(158.704075916301,20.7744157382976,381.537703348572));
#271693=CARTESIAN_POINT('Ctrl Pts',(160.339057893189,8.28413408366101,379.537703348572));
#271694=CARTESIAN_POINT('Ctrl Pts',(160.,-4.30813900827805,377.537703348572));
#271695=CARTESIAN_POINT('Origin',(160.,3.64291929955129E-14,535.));
#271696=CARTESIAN_POINT('',(160.,4.30813900827813,532.462296651428));
#271697=CARTESIAN_POINT('',(160.,-2.95752061042501E-13,535.));
#271698=CARTESIAN_POINT('',(160.,3.64291929955129E-14,535.));
#271699=CARTESIAN_POINT('',(160.,-4.30813900827846,531.09188778474));
#271700=CARTESIAN_POINT('Ctrl Pts',(160.,-4.30813900827846,531.09188778474));
#271701=CARTESIAN_POINT('Ctrl Pts',(160.,-1.43604209808346,531.54866409354));
#271702=CARTESIAN_POINT('Ctrl Pts',(160.,1.43594781991679,532.006113535419));
#271703=CARTESIAN_POINT('Ctrl Pts',(160.,4.30813900827813,532.462296651428));
#271704=CARTESIAN_POINT('Ctrl Pts',(160.,-2.96429547574917E-13,535.));
#271705=CARTESIAN_POINT('Ctrl Pts',(160.,-0.0199151703857166,534.98194265546));
#271706=CARTESIAN_POINT('Ctrl Pts',(160.,-0.039830432386428,534.96388541196));
#271707=CARTESIAN_POINT('Ctrl Pts',(160.,-0.0597455111566523,534.94582796638));
#271708=CARTESIAN_POINT('Ctrl Pts',(160.,-1.47617978783616,533.66151545298));
#271709=CARTESIAN_POINT('Ctrl Pts',(160.,-2.89215276710073,532.376694251498));
#271710=CARTESIAN_POINT('Ctrl Pts',(160.,-4.30813900827846,531.09188778474));
#271711=CARTESIAN_POINT('',(160.,-4.30813900827805,537.537703348572));
#271712=CARTESIAN_POINT('',(160.,3.64291929955129E-14,535.));
#271713=CARTESIAN_POINT('',(160.,4.30813900825421,538.908112215256));
#271714=CARTESIAN_POINT('Ctrl Pts',(160.,-4.30813900827805,537.537703348572));
#271715=CARTESIAN_POINT('Ctrl Pts',(160.,-1.43594781992483,537.99388646458));
#271716=CARTESIAN_POINT('Ctrl Pts',(160.,1.4360420980673,538.451335906457));
#271717=CARTESIAN_POINT('Ctrl Pts',(160.,4.30813900825421,538.908112215256));
#271718=CARTESIAN_POINT('Ctrl Pts',(160.000000000001,4.30813900825419,538.908112215256));
#271719=CARTESIAN_POINT('Ctrl Pts',(160.,2.89215276709868,537.623305748502));
#271720=CARTESIAN_POINT('Ctrl Pts',(160.,1.47617978787219,536.338484546979));
#271721=CARTESIAN_POINT('Ctrl Pts',(160.,0.0597455111551169,535.054172033622));
#271722=CARTESIAN_POINT('Ctrl Pts',(160.,0.0398304323843582,535.036114588042));
#271723=CARTESIAN_POINT('Ctrl Pts',(160.,0.0199151703848928,535.018057344541));
#271724=CARTESIAN_POINT('Ctrl Pts',(160.,-3.06976666308856E-13,535.));
#271725=CARTESIAN_POINT('Ctrl Pts',(160.,-4.30813900827805,697.537703348572));
#271726=CARTESIAN_POINT('Ctrl Pts',(159.660942106811,-16.900412100217,695.537703348572));
#271727=CARTESIAN_POINT('Ctrl Pts',(157.356193074143,-29.2846130745763,
693.537703348572));
#271728=CARTESIAN_POINT('Ctrl Pts',(155.051444041475,-41.6688140489355,
691.537703348572));
#271729=CARTESIAN_POINT('Ctrl Pts',(150.837754439537,-53.5400027769198,
689.537703348572));
#271730=CARTESIAN_POINT('Ctrl Pts',(146.624064837599,-65.411191504904,687.537703348572));
#271731=CARTESIAN_POINT('Ctrl Pts',(140.605189688823,-76.4770599218136,
685.537703348572));
#271732=CARTESIAN_POINT('Ctrl Pts',(134.586314540048,-87.5429283387233,
683.537703348572));
#271733=CARTESIAN_POINT('Ctrl Pts',(126.9104585261,-97.5309980386223,681.537703348572));
#271734=CARTESIAN_POINT('Ctrl Pts',(119.234602512152,-107.519067738521,
679.537703348572));
#271735=CARTESIAN_POINT('Ctrl Pts',(110.0907706828,-116.183399296895,677.537703348572));
#271736=CARTESIAN_POINT('Ctrl Pts',(100.946938853448,-124.847730855269,
675.537703348572));
#271737=CARTESIAN_POINT('Ctrl Pts',(90.5602826949691,-131.974979673883,
673.537703348572));
#271738=CARTESIAN_POINT('Ctrl Pts',(80.1736265364902,-139.102228492497,
671.537703348572));
#271739=CARTESIAN_POINT('Ctrl Pts',(68.7998999948414,-144.516898051454,
669.537703348572));
#271740=CARTESIAN_POINT('Ctrl Pts',(57.4261734531925,-149.931567610412,
667.537703348572));
#271741=CARTESIAN_POINT('Ctrl Pts',(45.3454354230634,-153.500330774912,
665.537703348572));
#271742=CARTESIAN_POINT('Ctrl Pts',(33.2646973929343,-157.069093939413,
663.537703348572));
#271743=CARTESIAN_POINT('Ctrl Pts',(20.7744157382976,-158.704075916301,
661.537703348572));
#271744=CARTESIAN_POINT('Ctrl Pts',(8.28413408366091,-160.339057893189,
659.537703348572));
#271745=CARTESIAN_POINT('Ctrl Pts',(-4.30813900827804,-160.,657.537703348572));
#271746=CARTESIAN_POINT('Ctrl Pts',(-16.900412100217,-159.660942106811,
655.537703348572));
#271747=CARTESIAN_POINT('Ctrl Pts',(-29.2846130745763,-157.356193074143,
653.537703348572));
#271748=CARTESIAN_POINT('Ctrl Pts',(-41.6688140489355,-155.051444041475,
651.537703348572));
#271749=CARTESIAN_POINT('Ctrl Pts',(-53.5400027769198,-150.837754439537,
649.537703348572));
#271750=CARTESIAN_POINT('Ctrl Pts',(-65.411191504904,-146.624064837599,
647.537703348572));
#271751=CARTESIAN_POINT('Ctrl Pts',(-76.4770599218136,-140.605189688823,
645.537703348572));
#271752=CARTESIAN_POINT('Ctrl Pts',(-87.5429283387233,-134.586314540048,
643.537703348572));
#271753=CARTESIAN_POINT('Ctrl Pts',(-97.5309980386223,-126.9104585261,641.537703348572));
#271754=CARTESIAN_POINT('Ctrl Pts',(-107.519067738521,-119.234602512152,
639.537703348572));
#271755=CARTESIAN_POINT('Ctrl Pts',(-116.183399296895,-110.0907706828,637.537703348572));
#271756=CARTESIAN_POINT('Ctrl Pts',(-124.847730855269,-100.946938853448,
635.537703348572));
#271757=CARTESIAN_POINT('Ctrl Pts',(-131.974979673883,-90.5602826949692,
633.537703348572));
#271758=CARTESIAN_POINT('Ctrl Pts',(-139.102228492497,-80.1736265364902,
631.537703348572));
#271759=CARTESIAN_POINT('Ctrl Pts',(-144.516898051454,-68.7998999948414,
629.537703348572));
#271760=CARTESIAN_POINT('Ctrl Pts',(-149.931567610412,-57.4261734531925,
627.537703348572));
#271761=CARTESIAN_POINT('Ctrl Pts',(-153.500330774912,-45.3454354230634,
625.537703348572));
#271762=CARTESIAN_POINT('Ctrl Pts',(-157.069093939413,-33.2646973929344,
623.537703348572));
#271763=CARTESIAN_POINT('Ctrl Pts',(-158.704075916301,-20.7744157382976,
621.537703348572));
#271764=CARTESIAN_POINT('Ctrl Pts',(-160.339057893189,-8.28413408366092,
619.537703348572));
#271765=CARTESIAN_POINT('Ctrl Pts',(-160.,4.30813900827803,617.537703348572));
#271766=CARTESIAN_POINT('Ctrl Pts',(-159.660942106811,16.900412100217,615.537703348572));
#271767=CARTESIAN_POINT('Ctrl Pts',(-157.356193074143,29.2846130745763,
613.537703348572));
#271768=CARTESIAN_POINT('Ctrl Pts',(-155.051444041475,41.6688140489355,
611.537703348572));
#271769=CARTESIAN_POINT('Ctrl Pts',(-150.837754439537,53.5400027769198,
609.537703348572));
#271770=CARTESIAN_POINT('Ctrl Pts',(-146.624064837599,65.411191504904,607.537703348572));
#271771=CARTESIAN_POINT('Ctrl Pts',(-140.605189688823,76.4770599218136,
605.537703348572));
#271772=CARTESIAN_POINT('Ctrl Pts',(-134.586314540048,87.5429283387233,
603.537703348572));
#271773=CARTESIAN_POINT('Ctrl Pts',(-126.9104585261,97.5309980386223,601.537703348572));
#271774=CARTESIAN_POINT('Ctrl Pts',(-119.234602512152,107.519067738521,
599.537703348572));
#271775=CARTESIAN_POINT('Ctrl Pts',(-110.0907706828,116.183399296895,597.537703348572));
#271776=CARTESIAN_POINT('Ctrl Pts',(-100.946938853448,124.847730855269,
595.537703348572));
#271777=CARTESIAN_POINT('Ctrl Pts',(-90.5602826949692,131.974979673883,
593.537703348572));
#271778=CARTESIAN_POINT('Ctrl Pts',(-80.1736265364901,139.102228492497,
591.537703348572));
#271779=CARTESIAN_POINT('Ctrl Pts',(-68.7998999948414,144.516898051454,
589.537703348572));
#271780=CARTESIAN_POINT('Ctrl Pts',(-57.4261734531926,149.931567610412,
587.537703348572));
#271781=CARTESIAN_POINT('Ctrl Pts',(-45.3454354230634,153.500330774912,
585.537703348572));
#271782=CARTESIAN_POINT('Ctrl Pts',(-33.2646973929343,157.069093939413,
583.537703348572));
#271783=CARTESIAN_POINT('Ctrl Pts',(-20.7744157382976,158.704075916301,
581.537703348572));
#271784=CARTESIAN_POINT('Ctrl Pts',(-8.284134083661,160.339057893189,579.537703348572));
#271785=CARTESIAN_POINT('Ctrl Pts',(4.30813900827803,160.,577.537703348572));
#271786=CARTESIAN_POINT('Ctrl Pts',(16.9004121002171,159.660942106811,575.537703348572));
#271787=CARTESIAN_POINT('Ctrl Pts',(29.2846130745762,157.356193074143,573.537703348572));
#271788=CARTESIAN_POINT('Ctrl Pts',(41.6688140489354,155.051444041476,571.537703348572));
#271789=CARTESIAN_POINT('Ctrl Pts',(53.5400027769198,150.837754439537,569.537703348572));
#271790=CARTESIAN_POINT('Ctrl Pts',(65.4111915049041,146.624064837599,567.537703348572));
#271791=CARTESIAN_POINT('Ctrl Pts',(76.4770599218136,140.605189688823,565.537703348572));
#271792=CARTESIAN_POINT('Ctrl Pts',(87.5429283387232,134.586314540048,563.537703348572));
#271793=CARTESIAN_POINT('Ctrl Pts',(97.5309980386223,126.9104585261,561.537703348572));
#271794=CARTESIAN_POINT('Ctrl Pts',(107.519067738521,119.234602512152,559.537703348572));
#271795=CARTESIAN_POINT('Ctrl Pts',(116.183399296895,110.0907706828,557.537703348572));
#271796=CARTESIAN_POINT('Ctrl Pts',(124.847730855269,100.946938853448,555.537703348572));
#271797=CARTESIAN_POINT('Ctrl Pts',(131.974979673883,90.5602826949692,553.537703348572));
#271798=CARTESIAN_POINT('Ctrl Pts',(139.102228492497,80.1736265364902,551.537703348572));
#271799=CARTESIAN_POINT('Ctrl Pts',(144.516898051454,68.7998999948414,549.537703348572));
#271800=CARTESIAN_POINT('Ctrl Pts',(149.931567610412,57.4261734531926,547.537703348572));
#271801=CARTESIAN_POINT('Ctrl Pts',(153.500330774912,45.3454354230634,545.537703348572));
#271802=CARTESIAN_POINT('Ctrl Pts',(157.069093939413,33.2646973929343,543.537703348572));
#271803=CARTESIAN_POINT('Ctrl Pts',(158.704075916301,20.7744157382976,541.537703348572));
#271804=CARTESIAN_POINT('Ctrl Pts',(160.339057893189,8.28413408366101,539.537703348572));
#271805=CARTESIAN_POINT('Ctrl Pts',(160.,-4.30813900827805,537.537703348572));
#271806=CARTESIAN_POINT('Ctrl Pts',(130.,-4.30813900827807,697.537703348572));
#271807=CARTESIAN_POINT('Ctrl Pts',(129.660942106811,-14.5393608954785,
695.537703348572));
#271808=CARTESIAN_POINT('Ctrl Pts',(127.725542856289,-24.5915791233694,
693.537703348572));
#271809=CARTESIAN_POINT('Ctrl Pts',(125.790143605767,-34.6437973512603,
691.537703348572));
#271810=CARTESIAN_POINT('Ctrl Pts',(122.306058950682,-44.2694929456714,
689.537703348572));
#271811=CARTESIAN_POINT('Ctrl Pts',(118.821974295598,-53.8951885400825,
687.537703348572));
#271812=CARTESIAN_POINT('Ctrl Pts',(113.874993963172,-62.8573449296272,
685.537703348572));
#271813=CARTESIAN_POINT('Ctrl Pts',(108.928013630747,-71.819501319172,683.537703348572));
#271814=CARTESIAN_POINT('Ctrl Pts',(102.639948694851,-79.8974404698481,
681.537703348572));
#271815=CARTESIAN_POINT('Ctrl Pts',(96.351883758956,-87.9753796205242,679.537703348572));
#271816=CARTESIAN_POINT('Ctrl Pts',(88.8775672472035,-94.9701958612989,
677.537703348572));
#271817=CARTESIAN_POINT('Ctrl Pts',(81.403250735451,-101.965012102074,675.537703348572));
#271818=CARTESIAN_POINT('Ctrl Pts',(72.9267251261949,-107.704469842635,
673.537703348572));
#271819=CARTESIAN_POINT('Ctrl Pts',(64.4501995169389,-113.443927583196,
671.537703348572));
#271820=CARTESIAN_POINT('Ctrl Pts',(55.1801850026549,-117.786702325803,
669.537703348572));
#271821=CARTESIAN_POINT('Ctrl Pts',(45.910170488371,-122.129477068411,667.537703348572));
#271822=CARTESIAN_POINT('Ctrl Pts',(36.074925591815,-124.968635286058,665.537703348572));
#271823=CARTESIAN_POINT('Ctrl Pts',(26.239680695259,-127.807793503704,663.537703348572));
#271824=CARTESIAN_POINT('Ctrl Pts',(16.0813817870907,-129.073425698447,
661.537703348572));
#271825=CARTESIAN_POINT('Ctrl Pts',(5.92308287892234,-130.339057893189,
659.537703348572));
#271826=CARTESIAN_POINT('Ctrl Pts',(-4.30813900827806,-130.,657.537703348572));
#271827=CARTESIAN_POINT('Ctrl Pts',(-14.5393608954785,-129.660942106811,
655.537703348572));
#271828=CARTESIAN_POINT('Ctrl Pts',(-24.5915791233694,-127.725542856289,
653.537703348572));
#271829=CARTESIAN_POINT('Ctrl Pts',(-34.6437973512603,-125.790143605767,
651.537703348572));
#271830=CARTESIAN_POINT('Ctrl Pts',(-44.2694929456713,-122.306058950682,
649.537703348572));
#271831=CARTESIAN_POINT('Ctrl Pts',(-53.8951885400825,-118.821974295598,
647.537703348572));
#271832=CARTESIAN_POINT('Ctrl Pts',(-62.8573449296272,-113.874993963172,
645.537703348572));
#271833=CARTESIAN_POINT('Ctrl Pts',(-71.819501319172,-108.928013630747,
643.537703348572));
#271834=CARTESIAN_POINT('Ctrl Pts',(-79.8974404698481,-102.639948694851,
641.537703348572));
#271835=CARTESIAN_POINT('Ctrl Pts',(-87.9753796205242,-96.351883758956,
639.537703348572));
#271836=CARTESIAN_POINT('Ctrl Pts',(-94.9701958612989,-88.8775672472035,
637.537703348572));
#271837=CARTESIAN_POINT('Ctrl Pts',(-101.965012102074,-81.403250735451,
635.537703348572));
#271838=CARTESIAN_POINT('Ctrl Pts',(-107.704469842635,-72.9267251261949,
633.537703348572));
#271839=CARTESIAN_POINT('Ctrl Pts',(-113.443927583196,-64.4501995169389,
631.537703348572));
#271840=CARTESIAN_POINT('Ctrl Pts',(-117.786702325803,-55.1801850026549,
629.537703348572));
#271841=CARTESIAN_POINT('Ctrl Pts',(-122.129477068411,-45.910170488371,
627.537703348572));
#271842=CARTESIAN_POINT('Ctrl Pts',(-124.968635286058,-36.074925591815,
625.537703348572));
#271843=CARTESIAN_POINT('Ctrl Pts',(-127.807793503704,-26.239680695259,
623.537703348572));
#271844=CARTESIAN_POINT('Ctrl Pts',(-129.073425698447,-16.0813817870907,
621.537703348572));
#271845=CARTESIAN_POINT('Ctrl Pts',(-130.339057893189,-5.92308287892235,
619.537703348572));
#271846=CARTESIAN_POINT('Ctrl Pts',(-130.,4.30813900827805,617.537703348572));
#271847=CARTESIAN_POINT('Ctrl Pts',(-129.660942106811,14.5393608954784,
615.537703348572));
#271848=CARTESIAN_POINT('Ctrl Pts',(-127.725542856289,24.5915791233693,
613.537703348572));
#271849=CARTESIAN_POINT('Ctrl Pts',(-125.790143605767,34.6437973512602,
611.537703348572));
#271850=CARTESIAN_POINT('Ctrl Pts',(-122.306058950682,44.2694929456713,
609.537703348572));
#271851=CARTESIAN_POINT('Ctrl Pts',(-118.821974295598,53.8951885400825,
607.537703348572));
#271852=CARTESIAN_POINT('Ctrl Pts',(-113.874993963172,62.8573449296272,
605.537703348572));
#271853=CARTESIAN_POINT('Ctrl Pts',(-108.928013630747,71.819501319172,603.537703348572));
#271854=CARTESIAN_POINT('Ctrl Pts',(-102.639948694851,79.8974404698481,
601.537703348572));
#271855=CARTESIAN_POINT('Ctrl Pts',(-96.3518837589561,87.9753796205242,
599.537703348572));
#271856=CARTESIAN_POINT('Ctrl Pts',(-88.8775672472035,94.9701958612989,
597.537703348572));
#271857=CARTESIAN_POINT('Ctrl Pts',(-81.403250735451,101.965012102074,595.537703348572));
#271858=CARTESIAN_POINT('Ctrl Pts',(-72.9267251261949,107.704469842635,
593.537703348572));
#271859=CARTESIAN_POINT('Ctrl Pts',(-64.4501995169389,113.443927583196,
591.537703348572));
#271860=CARTESIAN_POINT('Ctrl Pts',(-55.1801850026549,117.786702325803,
589.537703348572));
#271861=CARTESIAN_POINT('Ctrl Pts',(-45.910170488371,122.129477068411,587.537703348572));
#271862=CARTESIAN_POINT('Ctrl Pts',(-36.074925591815,124.968635286058,585.537703348572));
#271863=CARTESIAN_POINT('Ctrl Pts',(-26.239680695259,127.807793503704,583.537703348572));
#271864=CARTESIAN_POINT('Ctrl Pts',(-16.0813817870907,129.073425698447,
581.537703348572));
#271865=CARTESIAN_POINT('Ctrl Pts',(-5.92308287892242,130.339057893189,
579.537703348572));
#271866=CARTESIAN_POINT('Ctrl Pts',(4.30813900827804,130.,577.537703348572));
#271867=CARTESIAN_POINT('Ctrl Pts',(14.5393608954785,129.660942106811,575.537703348572));
#271868=CARTESIAN_POINT('Ctrl Pts',(24.5915791233693,127.725542856289,573.537703348572));
#271869=CARTESIAN_POINT('Ctrl Pts',(34.6437973512602,125.790143605767,571.537703348572));
#271870=CARTESIAN_POINT('Ctrl Pts',(44.2694929456713,122.306058950682,569.537703348572));
#271871=CARTESIAN_POINT('Ctrl Pts',(53.8951885400825,118.821974295598,567.537703348572));
#271872=CARTESIAN_POINT('Ctrl Pts',(62.8573449296272,113.874993963172,565.537703348572));
#271873=CARTESIAN_POINT('Ctrl Pts',(71.819501319172,108.928013630747,563.537703348572));
#271874=CARTESIAN_POINT('Ctrl Pts',(79.8974404698481,102.639948694851,561.537703348572));
#271875=CARTESIAN_POINT('Ctrl Pts',(87.9753796205242,96.351883758956,559.537703348572));
#271876=CARTESIAN_POINT('Ctrl Pts',(94.9701958612989,88.8775672472035,557.537703348572));
#271877=CARTESIAN_POINT('Ctrl Pts',(101.965012102074,81.403250735451,555.537703348572));
#271878=CARTESIAN_POINT('Ctrl Pts',(107.704469842635,72.926725126195,553.537703348572));
#271879=CARTESIAN_POINT('Ctrl Pts',(113.443927583196,64.4501995169389,551.537703348572));
#271880=CARTESIAN_POINT('Ctrl Pts',(117.786702325803,55.1801850026549,549.537703348572));
#271881=CARTESIAN_POINT('Ctrl Pts',(122.129477068411,45.910170488371,547.537703348572));
#271882=CARTESIAN_POINT('Ctrl Pts',(124.968635286058,36.074925591815,545.537703348572));
#271883=CARTESIAN_POINT('Ctrl Pts',(127.807793503704,26.239680695259,543.537703348572));
#271884=CARTESIAN_POINT('Ctrl Pts',(129.073425698447,16.0813817870907,541.537703348572));
#271885=CARTESIAN_POINT('Ctrl Pts',(130.339057893189,5.92308287892242,539.537703348572));
#271886=CARTESIAN_POINT('Ctrl Pts',(130.,-4.30813900827807,537.537703348572));
#271887=CARTESIAN_POINT('Origin',(-4.03737035466399,-0.209103844047687,
539.537622607813));
#271888=CARTESIAN_POINT('Ctrl Pts',(160.,4.30813900827813,692.462296651428));
#271889=CARTESIAN_POINT('Ctrl Pts',(160.339057893189,-8.28413408366083,
690.462296651428));
#271890=CARTESIAN_POINT('Ctrl Pts',(158.704075916301,-20.7744157382975,
688.462296651428));
#271891=CARTESIAN_POINT('Ctrl Pts',(157.069093939413,-33.2646973929343,
686.462296651429));
#271892=CARTESIAN_POINT('Ctrl Pts',(153.500330774912,-45.3454354230633,
684.462296651428));
#271893=CARTESIAN_POINT('Ctrl Pts',(149.931567610412,-57.4261734531924,
682.462296651428));
#271894=CARTESIAN_POINT('Ctrl Pts',(144.516898051455,-68.7998999948413,
680.462296651428));
#271895=CARTESIAN_POINT('Ctrl Pts',(139.102228492497,-80.1736265364901,
678.462296651428));
#271896=CARTESIAN_POINT('Ctrl Pts',(131.974979673883,-90.5602826949691,
676.462296651428));
#271897=CARTESIAN_POINT('Ctrl Pts',(124.847730855269,-100.946938853448,
674.462296651428));
#271898=CARTESIAN_POINT('Ctrl Pts',(116.183399296895,-110.0907706828,672.462296651428));
#271899=CARTESIAN_POINT('Ctrl Pts',(107.519067738521,-119.234602512152,
670.462296651428));
#271900=CARTESIAN_POINT('Ctrl Pts',(97.5309980386224,-126.9104585261,668.462296651428));
#271901=CARTESIAN_POINT('Ctrl Pts',(87.5429283387234,-134.586314540048,
666.462296651428));
#271902=CARTESIAN_POINT('Ctrl Pts',(76.4770599218137,-140.605189688823,
664.462296651428));
#271903=CARTESIAN_POINT('Ctrl Pts',(65.4111915049041,-146.624064837599,
662.462296651428));
#271904=CARTESIAN_POINT('Ctrl Pts',(53.5400027769198,-150.837754439537,
660.462296651428));
#271905=CARTESIAN_POINT('Ctrl Pts',(41.6688140489356,-155.051444041475,
658.462296651428));
#271906=CARTESIAN_POINT('Ctrl Pts',(29.2846130745764,-157.356193074143,
656.462296651428));
#271907=CARTESIAN_POINT('Ctrl Pts',(16.9004121002171,-159.660942106811,
654.462296651428));
#271908=CARTESIAN_POINT('Ctrl Pts',(4.30813900827814,-160.,652.462296651428));
#271909=CARTESIAN_POINT('Ctrl Pts',(-8.28413408366082,-160.339057893189,
650.462296651428));
#271910=CARTESIAN_POINT('Ctrl Pts',(-20.7744157382975,-158.704075916301,
648.462296651428));
#271911=CARTESIAN_POINT('Ctrl Pts',(-33.2646973929342,-157.069093939413,
646.462296651428));
#271912=CARTESIAN_POINT('Ctrl Pts',(-45.3454354230633,-153.500330774912,
644.462296651428));
#271913=CARTESIAN_POINT('Ctrl Pts',(-57.4261734531924,-149.931567610412,
642.462296651428));
#271914=CARTESIAN_POINT('Ctrl Pts',(-68.7998999948413,-144.516898051455,
640.462296651428));
#271915=CARTESIAN_POINT('Ctrl Pts',(-80.1736265364901,-139.102228492497,
638.462296651428));
#271916=CARTESIAN_POINT('Ctrl Pts',(-90.5602826949691,-131.974979673883,
636.462296651428));
#271917=CARTESIAN_POINT('Ctrl Pts',(-100.946938853448,-124.847730855269,
634.462296651428));
#271918=CARTESIAN_POINT('Ctrl Pts',(-110.0907706828,-116.183399296895,632.462296651428));
#271919=CARTESIAN_POINT('Ctrl Pts',(-119.234602512152,-107.519067738521,
630.462296651428));
#271920=CARTESIAN_POINT('Ctrl Pts',(-126.9104585261,-97.5309980386224,628.462296651428));
#271921=CARTESIAN_POINT('Ctrl Pts',(-134.586314540048,-87.5429283387234,
626.462296651429));
#271922=CARTESIAN_POINT('Ctrl Pts',(-140.605189688823,-76.4770599218137,
624.462296651428));
#271923=CARTESIAN_POINT('Ctrl Pts',(-146.624064837599,-65.4111915049041,
622.462296651428));
#271924=CARTESIAN_POINT('Ctrl Pts',(-150.837754439537,-53.5400027769199,
620.462296651428));
#271925=CARTESIAN_POINT('Ctrl Pts',(-155.051444041475,-41.6688140489356,
618.462296651428));
#271926=CARTESIAN_POINT('Ctrl Pts',(-157.356193074143,-29.2846130745764,
616.462296651428));
#271927=CARTESIAN_POINT('Ctrl Pts',(-159.660942106811,-16.9004121002171,
614.462296651429));
#271928=CARTESIAN_POINT('Ctrl Pts',(-160.,-4.30813900827815,612.462296651428));
#271929=CARTESIAN_POINT('Ctrl Pts',(-160.339057893189,8.28413408366081,
610.462296651428));
#271930=CARTESIAN_POINT('Ctrl Pts',(-158.704075916301,20.7744157382975,
608.462296651428));
#271931=CARTESIAN_POINT('Ctrl Pts',(-157.069093939413,33.2646973929342,
606.462296651428));
#271932=CARTESIAN_POINT('Ctrl Pts',(-153.500330774912,45.3454354230633,
604.462296651428));
#271933=CARTESIAN_POINT('Ctrl Pts',(-149.931567610412,57.4261734531924,
602.462296651429));
#271934=CARTESIAN_POINT('Ctrl Pts',(-144.516898051455,68.7998999948413,
600.462296651428));
#271935=CARTESIAN_POINT('Ctrl Pts',(-139.102228492497,80.1736265364901,
598.462296651428));
#271936=CARTESIAN_POINT('Ctrl Pts',(-131.974979673883,90.5602826949691,
596.462296651428));
#271937=CARTESIAN_POINT('Ctrl Pts',(-124.847730855269,100.946938853448,
594.462296651428));
#271938=CARTESIAN_POINT('Ctrl Pts',(-116.183399296895,110.0907706828,592.462296651428));
#271939=CARTESIAN_POINT('Ctrl Pts',(-107.519067738521,119.234602512152,
590.462296651428));
#271940=CARTESIAN_POINT('Ctrl Pts',(-97.5309980386224,126.9104585261,588.462296651428));
#271941=CARTESIAN_POINT('Ctrl Pts',(-87.5429283387233,134.586314540048,
586.462296651428));
#271942=CARTESIAN_POINT('Ctrl Pts',(-76.4770599218137,140.605189688823,
584.462296651428));
#271943=CARTESIAN_POINT('Ctrl Pts',(-65.4111915049042,146.624064837599,
582.462296651428));
#271944=CARTESIAN_POINT('Ctrl Pts',(-53.5400027769199,150.837754439537,
580.462296651428));
#271945=CARTESIAN_POINT('Ctrl Pts',(-41.6688140489356,155.051444041475,
578.462296651428));
#271946=CARTESIAN_POINT('Ctrl Pts',(-29.2846130745764,157.356193074143,
576.462296651428));
#271947=CARTESIAN_POINT('Ctrl Pts',(-16.9004121002172,159.660942106811,
574.462296651428));
#271948=CARTESIAN_POINT('Ctrl Pts',(-4.30813900827816,160.,572.462296651428));
#271949=CARTESIAN_POINT('Ctrl Pts',(8.28413408366087,160.339057893189,570.462296651428));
#271950=CARTESIAN_POINT('Ctrl Pts',(20.7744157382975,158.704075916301,568.462296651428));
#271951=CARTESIAN_POINT('Ctrl Pts',(33.2646973929342,157.069093939413,566.462296651428));
#271952=CARTESIAN_POINT('Ctrl Pts',(45.3454354230633,153.500330774912,564.462296651428));
#271953=CARTESIAN_POINT('Ctrl Pts',(57.4261734531925,149.931567610412,562.462296651428));
#271954=CARTESIAN_POINT('Ctrl Pts',(68.7998999948413,144.516898051455,560.462296651428));
#271955=CARTESIAN_POINT('Ctrl Pts',(80.1736265364901,139.102228492498,558.462296651428));
#271956=CARTESIAN_POINT('Ctrl Pts',(90.560282694969,131.974979673883,556.462296651428));
#271957=CARTESIAN_POINT('Ctrl Pts',(100.946938853448,124.847730855269,554.462296651428));
#271958=CARTESIAN_POINT('Ctrl Pts',(110.0907706828,116.183399296895,552.462296651428));
#271959=CARTESIAN_POINT('Ctrl Pts',(119.234602512152,107.519067738521,550.462296651428));
#271960=CARTESIAN_POINT('Ctrl Pts',(126.9104585261,97.5309980386224,548.462296651428));
#271961=CARTESIAN_POINT('Ctrl Pts',(134.586314540048,87.5429283387233,546.462296651428));
#271962=CARTESIAN_POINT('Ctrl Pts',(140.605189688823,76.4770599218137,544.462296651428));
#271963=CARTESIAN_POINT('Ctrl Pts',(146.624064837599,65.4111915049042,542.462296651428));
#271964=CARTESIAN_POINT('Ctrl Pts',(150.837754439537,53.5400027769199,540.462296651428));
#271965=CARTESIAN_POINT('Ctrl Pts',(155.051444041475,41.6688140489356,538.462296651428));
#271966=CARTESIAN_POINT('Ctrl Pts',(157.356193074143,29.2846130745764,536.462296651428));
#271967=CARTESIAN_POINT('Ctrl Pts',(159.660942106811,16.9004121002172,534.462296651428));
#271968=CARTESIAN_POINT('Ctrl Pts',(160.,4.30813900827813,532.462296651428));
#271969=CARTESIAN_POINT('Ctrl Pts',(160.,-4.30813900827805,697.537703348572));
#271970=CARTESIAN_POINT('Ctrl Pts',(159.660942106811,-16.900412100217,695.537703348572));
#271971=CARTESIAN_POINT('Ctrl Pts',(157.356193074143,-29.2846130745763,
693.537703348572));
#271972=CARTESIAN_POINT('Ctrl Pts',(155.051444041475,-41.6688140489355,
691.537703348572));
#271973=CARTESIAN_POINT('Ctrl Pts',(150.837754439537,-53.5400027769198,
689.537703348572));
#271974=CARTESIAN_POINT('Ctrl Pts',(146.624064837599,-65.411191504904,687.537703348572));
#271975=CARTESIAN_POINT('Ctrl Pts',(140.605189688823,-76.4770599218136,
685.537703348572));
#271976=CARTESIAN_POINT('Ctrl Pts',(134.586314540048,-87.5429283387233,
683.537703348572));
#271977=CARTESIAN_POINT('Ctrl Pts',(126.9104585261,-97.5309980386223,681.537703348572));
#271978=CARTESIAN_POINT('Ctrl Pts',(119.234602512152,-107.519067738521,
679.537703348572));
#271979=CARTESIAN_POINT('Ctrl Pts',(110.0907706828,-116.183399296895,677.537703348572));
#271980=CARTESIAN_POINT('Ctrl Pts',(100.946938853448,-124.847730855269,
675.537703348572));
#271981=CARTESIAN_POINT('Ctrl Pts',(90.5602826949691,-131.974979673883,
673.537703348572));
#271982=CARTESIAN_POINT('Ctrl Pts',(80.1736265364902,-139.102228492497,
671.537703348572));
#271983=CARTESIAN_POINT('Ctrl Pts',(68.7998999948414,-144.516898051454,
669.537703348572));
#271984=CARTESIAN_POINT('Ctrl Pts',(57.4261734531925,-149.931567610412,
667.537703348572));
#271985=CARTESIAN_POINT('Ctrl Pts',(45.3454354230634,-153.500330774912,
665.537703348572));
#271986=CARTESIAN_POINT('Ctrl Pts',(33.2646973929343,-157.069093939413,
663.537703348572));
#271987=CARTESIAN_POINT('Ctrl Pts',(20.7744157382976,-158.704075916301,
661.537703348572));
#271988=CARTESIAN_POINT('Ctrl Pts',(8.28413408366091,-160.339057893189,
659.537703348572));
#271989=CARTESIAN_POINT('Ctrl Pts',(-4.30813900827804,-160.,657.537703348572));
#271990=CARTESIAN_POINT('Ctrl Pts',(-16.900412100217,-159.660942106811,
655.537703348572));
#271991=CARTESIAN_POINT('Ctrl Pts',(-29.2846130745763,-157.356193074143,
653.537703348572));
#271992=CARTESIAN_POINT('Ctrl Pts',(-41.6688140489355,-155.051444041475,
651.537703348572));
#271993=CARTESIAN_POINT('Ctrl Pts',(-53.5400027769198,-150.837754439537,
649.537703348572));
#271994=CARTESIAN_POINT('Ctrl Pts',(-65.411191504904,-146.624064837599,
647.537703348572));
#271995=CARTESIAN_POINT('Ctrl Pts',(-76.4770599218136,-140.605189688823,
645.537703348572));
#271996=CARTESIAN_POINT('Ctrl Pts',(-87.5429283387233,-134.586314540048,
643.537703348572));
#271997=CARTESIAN_POINT('Ctrl Pts',(-97.5309980386223,-126.9104585261,641.537703348572));
#271998=CARTESIAN_POINT('Ctrl Pts',(-107.519067738521,-119.234602512152,
639.537703348572));
#271999=CARTESIAN_POINT('Ctrl Pts',(-116.183399296895,-110.0907706828,637.537703348572));
#272000=CARTESIAN_POINT('Ctrl Pts',(-124.847730855269,-100.946938853448,
635.537703348572));
#272001=CARTESIAN_POINT('Ctrl Pts',(-131.974979673883,-90.5602826949692,
633.537703348572));
#272002=CARTESIAN_POINT('Ctrl Pts',(-139.102228492497,-80.1736265364902,
631.537703348572));
#272003=CARTESIAN_POINT('Ctrl Pts',(-144.516898051454,-68.7998999948414,
629.537703348572));
#272004=CARTESIAN_POINT('Ctrl Pts',(-149.931567610412,-57.4261734531925,
627.537703348572));
#272005=CARTESIAN_POINT('Ctrl Pts',(-153.500330774912,-45.3454354230634,
625.537703348572));
#272006=CARTESIAN_POINT('Ctrl Pts',(-157.069093939413,-33.2646973929344,
623.537703348572));
#272007=CARTESIAN_POINT('Ctrl Pts',(-158.704075916301,-20.7744157382976,
621.537703348572));
#272008=CARTESIAN_POINT('Ctrl Pts',(-160.339057893189,-8.28413408366092,
619.537703348572));
#272009=CARTESIAN_POINT('Ctrl Pts',(-160.,4.30813900827803,617.537703348572));
#272010=CARTESIAN_POINT('Ctrl Pts',(-159.660942106811,16.900412100217,615.537703348572));
#272011=CARTESIAN_POINT('Ctrl Pts',(-157.356193074143,29.2846130745763,
613.537703348572));
#272012=CARTESIAN_POINT('Ctrl Pts',(-155.051444041475,41.6688140489355,
611.537703348572));
#272013=CARTESIAN_POINT('Ctrl Pts',(-150.837754439537,53.5400027769198,
609.537703348572));
#272014=CARTESIAN_POINT('Ctrl Pts',(-146.624064837599,65.411191504904,607.537703348572));
#272015=CARTESIAN_POINT('Ctrl Pts',(-140.605189688823,76.4770599218136,
605.537703348572));
#272016=CARTESIAN_POINT('Ctrl Pts',(-134.586314540048,87.5429283387233,
603.537703348572));
#272017=CARTESIAN_POINT('Ctrl Pts',(-126.9104585261,97.5309980386223,601.537703348572));
#272018=CARTESIAN_POINT('Ctrl Pts',(-119.234602512152,107.519067738521,
599.537703348572));
#272019=CARTESIAN_POINT('Ctrl Pts',(-110.0907706828,116.183399296895,597.537703348572));
#272020=CARTESIAN_POINT('Ctrl Pts',(-100.946938853448,124.847730855269,
595.537703348572));
#272021=CARTESIAN_POINT('Ctrl Pts',(-90.5602826949692,131.974979673883,
593.537703348572));
#272022=CARTESIAN_POINT('Ctrl Pts',(-80.1736265364901,139.102228492497,
591.537703348572));
#272023=CARTESIAN_POINT('Ctrl Pts',(-68.7998999948414,144.516898051454,
589.537703348572));
#272024=CARTESIAN_POINT('Ctrl Pts',(-57.4261734531926,149.931567610412,
587.537703348572));
#272025=CARTESIAN_POINT('Ctrl Pts',(-45.3454354230634,153.500330774912,
585.537703348572));
#272026=CARTESIAN_POINT('Ctrl Pts',(-33.2646973929343,157.069093939413,
583.537703348572));
#272027=CARTESIAN_POINT('Ctrl Pts',(-20.7744157382976,158.704075916301,
581.537703348572));
#272028=CARTESIAN_POINT('Ctrl Pts',(-8.284134083661,160.339057893189,579.537703348572));
#272029=CARTESIAN_POINT('Ctrl Pts',(4.30813900827803,160.,577.537703348572));
#272030=CARTESIAN_POINT('Ctrl Pts',(16.9004121002171,159.660942106811,575.537703348572));
#272031=CARTESIAN_POINT('Ctrl Pts',(29.2846130745762,157.356193074143,573.537703348572));
#272032=CARTESIAN_POINT('Ctrl Pts',(41.6688140489354,155.051444041476,571.537703348572));
#272033=CARTESIAN_POINT('Ctrl Pts',(53.5400027769198,150.837754439537,569.537703348572));
#272034=CARTESIAN_POINT('Ctrl Pts',(65.4111915049041,146.624064837599,567.537703348572));
#272035=CARTESIAN_POINT('Ctrl Pts',(76.4770599218136,140.605189688823,565.537703348572));
#272036=CARTESIAN_POINT('Ctrl Pts',(87.5429283387232,134.586314540048,563.537703348572));
#272037=CARTESIAN_POINT('Ctrl Pts',(97.5309980386223,126.9104585261,561.537703348572));
#272038=CARTESIAN_POINT('Ctrl Pts',(107.519067738521,119.234602512152,559.537703348572));
#272039=CARTESIAN_POINT('Ctrl Pts',(116.183399296895,110.0907706828,557.537703348572));
#272040=CARTESIAN_POINT('Ctrl Pts',(124.847730855269,100.946938853448,555.537703348572));
#272041=CARTESIAN_POINT('Ctrl Pts',(131.974979673883,90.5602826949692,553.537703348572));
#272042=CARTESIAN_POINT('Ctrl Pts',(139.102228492497,80.1736265364902,551.537703348572));
#272043=CARTESIAN_POINT('Ctrl Pts',(144.516898051454,68.7998999948414,549.537703348572));
#272044=CARTESIAN_POINT('Ctrl Pts',(149.931567610412,57.4261734531926,547.537703348572));
#272045=CARTESIAN_POINT('Ctrl Pts',(153.500330774912,45.3454354230634,545.537703348572));
#272046=CARTESIAN_POINT('Ctrl Pts',(157.069093939413,33.2646973929343,543.537703348572));
#272047=CARTESIAN_POINT('Ctrl Pts',(158.704075916301,20.7744157382976,541.537703348572));
#272048=CARTESIAN_POINT('Ctrl Pts',(160.339057893189,8.28413408366101,539.537703348572));
#272049=CARTESIAN_POINT('Ctrl Pts',(160.,-4.30813900827805,537.537703348572));
#272050=CARTESIAN_POINT('Ctrl Pts',(130.,4.30813900827812,532.462296651428));
#272051=CARTESIAN_POINT('Ctrl Pts',(130.339057893189,-5.92308287892228,
530.462296651428));
#272052=CARTESIAN_POINT('Ctrl Pts',(129.073425698447,-16.0813817870906,
528.462296651428));
#272053=CARTESIAN_POINT('Ctrl Pts',(127.807793503704,-26.2396806952589,
526.462296651428));
#272054=CARTESIAN_POINT('Ctrl Pts',(124.968635286058,-36.0749255918149,
524.462296651428));
#272055=CARTESIAN_POINT('Ctrl Pts',(122.129477068411,-45.9101704883709,
522.462296651428));
#272056=CARTESIAN_POINT('Ctrl Pts',(117.786702325803,-55.1801850026549,
520.462296651428));
#272057=CARTESIAN_POINT('Ctrl Pts',(113.443927583196,-64.4501995169389,
518.462296651428));
#272058=CARTESIAN_POINT('Ctrl Pts',(107.704469842635,-72.9267251261949,
516.462296651428));
#272059=CARTESIAN_POINT('Ctrl Pts',(101.965012102074,-81.4032507354509,
514.462296651428));
#272060=CARTESIAN_POINT('Ctrl Pts',(94.9701958612989,-88.8775672472035,
512.462296651428));
#272061=CARTESIAN_POINT('Ctrl Pts',(87.9753796205242,-96.351883758956,510.462296651428));
#272062=CARTESIAN_POINT('Ctrl Pts',(79.8974404698481,-102.639948694851,
508.462296651428));
#272063=CARTESIAN_POINT('Ctrl Pts',(71.8195013191721,-108.928013630747,
506.462296651428));
#272064=CARTESIAN_POINT('Ctrl Pts',(62.8573449296273,-113.874993963172,
504.462296651428));
#272065=CARTESIAN_POINT('Ctrl Pts',(53.8951885400825,-118.821974295598,
502.462296651428));
#272066=CARTESIAN_POINT('Ctrl Pts',(44.2694929456714,-122.306058950682,
500.462296651428));
#272067=CARTESIAN_POINT('Ctrl Pts',(34.6437973512603,-125.790143605767,
498.462296651428));
#272068=CARTESIAN_POINT('Ctrl Pts',(24.5915791233694,-127.725542856289,
496.462296651428));
#272069=CARTESIAN_POINT('Ctrl Pts',(14.5393608954785,-129.660942106811,
494.462296651428));
#272070=CARTESIAN_POINT('Ctrl Pts',(4.30813900827813,-130.,492.462296651428));
#272071=CARTESIAN_POINT('Ctrl Pts',(-5.92308287892227,-130.339057893189,
490.462296651428));
#272072=CARTESIAN_POINT('Ctrl Pts',(-16.0813817870906,-129.073425698447,
488.462296651428));
#272073=CARTESIAN_POINT('Ctrl Pts',(-26.2396806952589,-127.807793503705,
486.462296651428));
#272074=CARTESIAN_POINT('Ctrl Pts',(-36.0749255918149,-124.968635286058,
484.462296651428));
#272075=CARTESIAN_POINT('Ctrl Pts',(-45.9101704883709,-122.129477068411,
482.462296651428));
#272076=CARTESIAN_POINT('Ctrl Pts',(-55.1801850026549,-117.786702325803,
480.462296651428));
#272077=CARTESIAN_POINT('Ctrl Pts',(-64.4501995169389,-113.443927583196,
478.462296651428));
#272078=CARTESIAN_POINT('Ctrl Pts',(-72.9267251261949,-107.704469842635,
476.462296651428));
#272079=CARTESIAN_POINT('Ctrl Pts',(-81.4032507354509,-101.965012102074,
474.462296651428));
#272080=CARTESIAN_POINT('Ctrl Pts',(-88.8775672472034,-94.9701958612989,
472.462296651428));
#272081=CARTESIAN_POINT('Ctrl Pts',(-96.351883758956,-87.9753796205242,
470.462296651428));
#272082=CARTESIAN_POINT('Ctrl Pts',(-102.639948694851,-79.8974404698482,
468.462296651428));
#272083=CARTESIAN_POINT('Ctrl Pts',(-108.928013630747,-71.8195013191721,
466.462296651428));
#272084=CARTESIAN_POINT('Ctrl Pts',(-113.874993963172,-62.8573449296273,
464.462296651428));
#272085=CARTESIAN_POINT('Ctrl Pts',(-118.821974295598,-53.8951885400825,
462.462296651428));
#272086=CARTESIAN_POINT('Ctrl Pts',(-122.306058950682,-44.2694929456714,
460.462296651428));
#272087=CARTESIAN_POINT('Ctrl Pts',(-125.790143605767,-34.6437973512603,
458.462296651428));
#272088=CARTESIAN_POINT('Ctrl Pts',(-127.725542856289,-24.5915791233694,
456.462296651428));
#272089=CARTESIAN_POINT('Ctrl Pts',(-129.660942106811,-14.5393608954785,
454.462296651429));
#272090=CARTESIAN_POINT('Ctrl Pts',(-130.,-4.30813900827813,452.462296651428));
#272091=CARTESIAN_POINT('Ctrl Pts',(-130.339057893189,5.92308287892227,
450.462296651428));
#272092=CARTESIAN_POINT('Ctrl Pts',(-129.073425698447,16.0813817870906,
448.462296651428));
#272093=CARTESIAN_POINT('Ctrl Pts',(-127.807793503705,26.2396806952589,
446.462296651428));
#272094=CARTESIAN_POINT('Ctrl Pts',(-124.968635286058,36.0749255918149,
444.462296651428));
#272095=CARTESIAN_POINT('Ctrl Pts',(-122.129477068411,45.9101704883709,
442.462296651428));
#272096=CARTESIAN_POINT('Ctrl Pts',(-117.786702325803,55.1801850026549,
440.462296651428));
#272097=CARTESIAN_POINT('Ctrl Pts',(-113.443927583196,64.4501995169388,
438.462296651428));
#272098=CARTESIAN_POINT('Ctrl Pts',(-107.704469842635,72.9267251261949,
436.462296651428));
#272099=CARTESIAN_POINT('Ctrl Pts',(-101.965012102074,81.4032507354509,
434.462296651428));
#272100=CARTESIAN_POINT('Ctrl Pts',(-94.9701958612989,88.8775672472034,
432.462296651428));
#272101=CARTESIAN_POINT('Ctrl Pts',(-87.9753796205243,96.3518837589559,
430.462296651428));
#272102=CARTESIAN_POINT('Ctrl Pts',(-79.8974404698482,102.639948694851,
428.462296651428));
#272103=CARTESIAN_POINT('Ctrl Pts',(-71.819501319172,108.928013630747,426.462296651428));
#272104=CARTESIAN_POINT('Ctrl Pts',(-62.8573449296273,113.874993963172,
424.462296651428));
#272105=CARTESIAN_POINT('Ctrl Pts',(-53.8951885400826,118.821974295598,
422.462296651428));
#272106=CARTESIAN_POINT('Ctrl Pts',(-44.2694929456714,122.306058950682,
420.462296651428));
#272107=CARTESIAN_POINT('Ctrl Pts',(-34.6437973512603,125.790143605767,
418.462296651428));
#272108=CARTESIAN_POINT('Ctrl Pts',(-24.5915791233694,127.725542856289,
416.462296651428));
#272109=CARTESIAN_POINT('Ctrl Pts',(-14.5393608954786,129.660942106811,
414.462296651428));
#272110=CARTESIAN_POINT('Ctrl Pts',(-4.30813900827814,130.,412.462296651428));
#272111=CARTESIAN_POINT('Ctrl Pts',(5.92308287892232,130.339057893189,410.462296651428));
#272112=CARTESIAN_POINT('Ctrl Pts',(16.0813817870906,129.073425698447,408.462296651428));
#272113=CARTESIAN_POINT('Ctrl Pts',(26.2396806952589,127.807793503705,406.462296651428));
#272114=CARTESIAN_POINT('Ctrl Pts',(36.0749255918149,124.968635286058,404.462296651428));
#272115=CARTESIAN_POINT('Ctrl Pts',(45.9101704883709,122.129477068411,402.462296651428));
#272116=CARTESIAN_POINT('Ctrl Pts',(55.1801850026549,117.786702325803,400.462296651428));
#272117=CARTESIAN_POINT('Ctrl Pts',(64.4501995169388,113.443927583196,398.462296651428));
#272118=CARTESIAN_POINT('Ctrl Pts',(72.9267251261949,107.704469842635,396.462296651428));
#272119=CARTESIAN_POINT('Ctrl Pts',(81.4032507354509,101.965012102074,394.462296651428));
#272120=CARTESIAN_POINT('Ctrl Pts',(88.8775672472034,94.9701958612989,392.462296651428));
#272121=CARTESIAN_POINT('Ctrl Pts',(96.3518837589559,87.9753796205243,390.462296651428));
#272122=CARTESIAN_POINT('Ctrl Pts',(102.639948694851,79.8974404698482,388.462296651428));
#272123=CARTESIAN_POINT('Ctrl Pts',(108.928013630747,71.819501319172,386.462296651428));
#272124=CARTESIAN_POINT('Ctrl Pts',(113.874993963172,62.8573449296273,384.462296651428));
#272125=CARTESIAN_POINT('Ctrl Pts',(118.821974295598,53.8951885400826,382.462296651428));
#272126=CARTESIAN_POINT('Ctrl Pts',(122.306058950682,44.2694929456714,380.462296651428));
#272127=CARTESIAN_POINT('Ctrl Pts',(125.790143605767,34.6437973512603,378.462296651428));
#272128=CARTESIAN_POINT('Ctrl Pts',(127.725542856289,24.5915791233694,376.462296651428));
#272129=CARTESIAN_POINT('Ctrl Pts',(129.660942106811,14.5393608954786,374.462296651428));
#272130=CARTESIAN_POINT('Ctrl Pts',(130.,4.30813900827812,372.462296651428));
#272131=CARTESIAN_POINT('Ctrl Pts',(160.,4.30813900827813,532.462296651428));
#272132=CARTESIAN_POINT('Ctrl Pts',(160.339057893189,-8.28413408366083,
530.462296651428));
#272133=CARTESIAN_POINT('Ctrl Pts',(158.704075916301,-20.7744157382975,
528.462296651428));
#272134=CARTESIAN_POINT('Ctrl Pts',(157.069093939413,-33.2646973929343,
526.462296651428));
#272135=CARTESIAN_POINT('Ctrl Pts',(153.500330774912,-45.3454354230633,
524.462296651428));
#272136=CARTESIAN_POINT('Ctrl Pts',(149.931567610412,-57.4261734531924,
522.462296651428));
#272137=CARTESIAN_POINT('Ctrl Pts',(144.516898051455,-68.7998999948413,
520.462296651428));
#272138=CARTESIAN_POINT('Ctrl Pts',(139.102228492497,-80.1736265364901,
518.462296651428));
#272139=CARTESIAN_POINT('Ctrl Pts',(131.974979673883,-90.5602826949691,
516.462296651428));
#272140=CARTESIAN_POINT('Ctrl Pts',(124.847730855269,-100.946938853448,
514.462296651428));
#272141=CARTESIAN_POINT('Ctrl Pts',(116.183399296895,-110.0907706828,512.462296651428));
#272142=CARTESIAN_POINT('Ctrl Pts',(107.519067738521,-119.234602512152,
510.462296651428));
#272143=CARTESIAN_POINT('Ctrl Pts',(97.5309980386224,-126.9104585261,508.462296651428));
#272144=CARTESIAN_POINT('Ctrl Pts',(87.5429283387234,-134.586314540048,
506.462296651428));
#272145=CARTESIAN_POINT('Ctrl Pts',(76.4770599218137,-140.605189688823,
504.462296651428));
#272146=CARTESIAN_POINT('Ctrl Pts',(65.4111915049041,-146.624064837599,
502.462296651428));
#272147=CARTESIAN_POINT('Ctrl Pts',(53.5400027769198,-150.837754439537,
500.462296651428));
#272148=CARTESIAN_POINT('Ctrl Pts',(41.6688140489356,-155.051444041475,
498.462296651428));
#272149=CARTESIAN_POINT('Ctrl Pts',(29.2846130745764,-157.356193074143,
496.462296651428));
#272150=CARTESIAN_POINT('Ctrl Pts',(16.9004121002171,-159.660942106811,
494.462296651428));
#272151=CARTESIAN_POINT('Ctrl Pts',(4.30813900827814,-160.,492.462296651428));
#272152=CARTESIAN_POINT('Ctrl Pts',(-8.28413408366082,-160.339057893189,
490.462296651428));
#272153=CARTESIAN_POINT('Ctrl Pts',(-20.7744157382975,-158.704075916301,
488.462296651428));
#272154=CARTESIAN_POINT('Ctrl Pts',(-33.2646973929342,-157.069093939413,
486.462296651428));
#272155=CARTESIAN_POINT('Ctrl Pts',(-45.3454354230633,-153.500330774912,
484.462296651428));
#272156=CARTESIAN_POINT('Ctrl Pts',(-57.4261734531924,-149.931567610412,
482.462296651428));
#272157=CARTESIAN_POINT('Ctrl Pts',(-68.7998999948413,-144.516898051455,
480.462296651428));
#272158=CARTESIAN_POINT('Ctrl Pts',(-80.1736265364901,-139.102228492497,
478.462296651428));
#272159=CARTESIAN_POINT('Ctrl Pts',(-90.5602826949691,-131.974979673883,
476.462296651428));
#272160=CARTESIAN_POINT('Ctrl Pts',(-100.946938853448,-124.847730855269,
474.462296651428));
#272161=CARTESIAN_POINT('Ctrl Pts',(-110.0907706828,-116.183399296895,472.462296651428));
#272162=CARTESIAN_POINT('Ctrl Pts',(-119.234602512152,-107.519067738521,
470.462296651428));
#272163=CARTESIAN_POINT('Ctrl Pts',(-126.9104585261,-97.5309980386224,468.462296651428));
#272164=CARTESIAN_POINT('Ctrl Pts',(-134.586314540048,-87.5429283387234,
466.462296651428));
#272165=CARTESIAN_POINT('Ctrl Pts',(-140.605189688823,-76.4770599218137,
464.462296651428));
#272166=CARTESIAN_POINT('Ctrl Pts',(-146.624064837599,-65.4111915049041,
462.462296651428));
#272167=CARTESIAN_POINT('Ctrl Pts',(-150.837754439537,-53.5400027769199,
460.462296651428));
#272168=CARTESIAN_POINT('Ctrl Pts',(-155.051444041475,-41.6688140489356,
458.462296651428));
#272169=CARTESIAN_POINT('Ctrl Pts',(-157.356193074143,-29.2846130745764,
456.462296651428));
#272170=CARTESIAN_POINT('Ctrl Pts',(-159.660942106811,-16.9004121002171,
454.462296651429));
#272171=CARTESIAN_POINT('Ctrl Pts',(-160.,-4.30813900827815,452.462296651428));
#272172=CARTESIAN_POINT('Ctrl Pts',(-160.339057893189,8.28413408366081,
450.462296651428));
#272173=CARTESIAN_POINT('Ctrl Pts',(-158.704075916301,20.7744157382975,
448.462296651428));
#272174=CARTESIAN_POINT('Ctrl Pts',(-157.069093939413,33.2646973929342,
446.462296651428));
#272175=CARTESIAN_POINT('Ctrl Pts',(-153.500330774912,45.3454354230633,
444.462296651428));
#272176=CARTESIAN_POINT('Ctrl Pts',(-149.931567610412,57.4261734531924,
442.462296651428));
#272177=CARTESIAN_POINT('Ctrl Pts',(-144.516898051455,68.7998999948413,
440.462296651428));
#272178=CARTESIAN_POINT('Ctrl Pts',(-139.102228492497,80.1736265364901,
438.462296651428));
#272179=CARTESIAN_POINT('Ctrl Pts',(-131.974979673883,90.5602826949691,
436.462296651428));
#272180=CARTESIAN_POINT('Ctrl Pts',(-124.847730855269,100.946938853448,
434.462296651428));
#272181=CARTESIAN_POINT('Ctrl Pts',(-116.183399296895,110.0907706828,432.462296651428));
#272182=CARTESIAN_POINT('Ctrl Pts',(-107.519067738521,119.234602512152,
430.462296651428));
#272183=CARTESIAN_POINT('Ctrl Pts',(-97.5309980386224,126.9104585261,428.462296651428));
#272184=CARTESIAN_POINT('Ctrl Pts',(-87.5429283387233,134.586314540048,
426.462296651428));
#272185=CARTESIAN_POINT('Ctrl Pts',(-76.4770599218137,140.605189688823,
424.462296651428));
#272186=CARTESIAN_POINT('Ctrl Pts',(-65.4111915049042,146.624064837599,
422.462296651428));
#272187=CARTESIAN_POINT('Ctrl Pts',(-53.5400027769199,150.837754439537,
420.462296651428));
#272188=CARTESIAN_POINT('Ctrl Pts',(-41.6688140489356,155.051444041475,
418.462296651428));
#272189=CARTESIAN_POINT('Ctrl Pts',(-29.2846130745764,157.356193074143,
416.462296651428));
#272190=CARTESIAN_POINT('Ctrl Pts',(-16.9004121002172,159.660942106811,
414.462296651428));
#272191=CARTESIAN_POINT('Ctrl Pts',(-4.30813900827816,160.,412.462296651428));
#272192=CARTESIAN_POINT('Ctrl Pts',(8.28413408366087,160.339057893189,410.462296651428));
#272193=CARTESIAN_POINT('Ctrl Pts',(20.7744157382975,158.704075916301,408.462296651428));
#272194=CARTESIAN_POINT('Ctrl Pts',(33.2646973929342,157.069093939413,406.462296651428));
#272195=CARTESIAN_POINT('Ctrl Pts',(45.3454354230633,153.500330774912,404.462296651428));
#272196=CARTESIAN_POINT('Ctrl Pts',(57.4261734531925,149.931567610412,402.462296651428));
#272197=CARTESIAN_POINT('Ctrl Pts',(68.7998999948413,144.516898051455,400.462296651428));
#272198=CARTESIAN_POINT('Ctrl Pts',(80.1736265364901,139.102228492498,398.462296651428));
#272199=CARTESIAN_POINT('Ctrl Pts',(90.560282694969,131.974979673883,396.462296651428));
#272200=CARTESIAN_POINT('Ctrl Pts',(100.946938853448,124.847730855269,394.462296651428));
#272201=CARTESIAN_POINT('Ctrl Pts',(110.0907706828,116.183399296895,392.462296651428));
#272202=CARTESIAN_POINT('Ctrl Pts',(119.234602512152,107.519067738521,390.462296651428));
#272203=CARTESIAN_POINT('Ctrl Pts',(126.9104585261,97.5309980386224,388.462296651428));
#272204=CARTESIAN_POINT('Ctrl Pts',(134.586314540048,87.5429283387233,386.462296651428));
#272205=CARTESIAN_POINT('Ctrl Pts',(140.605189688823,76.4770599218137,384.462296651428));
#272206=CARTESIAN_POINT('Ctrl Pts',(146.624064837599,65.4111915049042,382.462296651428));
#272207=CARTESIAN_POINT('Ctrl Pts',(150.837754439537,53.5400027769199,380.462296651428));
#272208=CARTESIAN_POINT('Ctrl Pts',(155.051444041475,41.6688140489356,378.462296651428));
#272209=CARTESIAN_POINT('Ctrl Pts',(157.356193074143,29.2846130745764,376.462296651428));
#272210=CARTESIAN_POINT('Ctrl Pts',(159.660942106811,16.9004121002172,374.462296651428));
#272211=CARTESIAN_POINT('Ctrl Pts',(160.,4.30813900827813,372.462296651428));
#272212=CARTESIAN_POINT('Origin',(-4.03737035478777,0.209103844014949,530.462377392398));
#272213=CARTESIAN_POINT('Ctrl Pts',(160.,4.30813900827813,532.462296651428));
#272214=CARTESIAN_POINT('Ctrl Pts',(160.339057893189,-8.28413408366083,
530.462296651428));
#272215=CARTESIAN_POINT('Ctrl Pts',(158.704075916301,-20.7744157382975,
528.462296651428));
#272216=CARTESIAN_POINT('Ctrl Pts',(157.069093939413,-33.2646973929343,
526.462296651428));
#272217=CARTESIAN_POINT('Ctrl Pts',(153.500330774912,-45.3454354230633,
524.462296651428));
#272218=CARTESIAN_POINT('Ctrl Pts',(149.931567610412,-57.4261734531924,
522.462296651428));
#272219=CARTESIAN_POINT('Ctrl Pts',(144.516898051455,-68.7998999948413,
520.462296651428));
#272220=CARTESIAN_POINT('Ctrl Pts',(139.102228492497,-80.1736265364901,
518.462296651428));
#272221=CARTESIAN_POINT('Ctrl Pts',(131.974979673883,-90.5602826949691,
516.462296651428));
#272222=CARTESIAN_POINT('Ctrl Pts',(124.847730855269,-100.946938853448,
514.462296651428));
#272223=CARTESIAN_POINT('Ctrl Pts',(116.183399296895,-110.0907706828,512.462296651428));
#272224=CARTESIAN_POINT('Ctrl Pts',(107.519067738521,-119.234602512152,
510.462296651428));
#272225=CARTESIAN_POINT('Ctrl Pts',(97.5309980386224,-126.9104585261,508.462296651428));
#272226=CARTESIAN_POINT('Ctrl Pts',(87.5429283387234,-134.586314540048,
506.462296651428));
#272227=CARTESIAN_POINT('Ctrl Pts',(76.4770599218137,-140.605189688823,
504.462296651428));
#272228=CARTESIAN_POINT('Ctrl Pts',(65.4111915049041,-146.624064837599,
502.462296651428));
#272229=CARTESIAN_POINT('Ctrl Pts',(53.5400027769198,-150.837754439537,
500.462296651428));
#272230=CARTESIAN_POINT('Ctrl Pts',(41.6688140489356,-155.051444041475,
498.462296651428));
#272231=CARTESIAN_POINT('Ctrl Pts',(29.2846130745764,-157.356193074143,
496.462296651428));
#272232=CARTESIAN_POINT('Ctrl Pts',(16.9004121002171,-159.660942106811,
494.462296651428));
#272233=CARTESIAN_POINT('Ctrl Pts',(4.30813900827814,-160.,492.462296651428));
#272234=CARTESIAN_POINT('Ctrl Pts',(-8.28413408366082,-160.339057893189,
490.462296651428));
#272235=CARTESIAN_POINT('Ctrl Pts',(-20.7744157382975,-158.704075916301,
488.462296651428));
#272236=CARTESIAN_POINT('Ctrl Pts',(-33.2646973929342,-157.069093939413,
486.462296651428));
#272237=CARTESIAN_POINT('Ctrl Pts',(-45.3454354230633,-153.500330774912,
484.462296651428));
#272238=CARTESIAN_POINT('Ctrl Pts',(-57.4261734531924,-149.931567610412,
482.462296651428));
#272239=CARTESIAN_POINT('Ctrl Pts',(-68.7998999948413,-144.516898051455,
480.462296651428));
#272240=CARTESIAN_POINT('Ctrl Pts',(-80.1736265364901,-139.102228492497,
478.462296651428));
#272241=CARTESIAN_POINT('Ctrl Pts',(-90.5602826949691,-131.974979673883,
476.462296651428));
#272242=CARTESIAN_POINT('Ctrl Pts',(-100.946938853448,-124.847730855269,
474.462296651428));
#272243=CARTESIAN_POINT('Ctrl Pts',(-110.0907706828,-116.183399296895,472.462296651428));
#272244=CARTESIAN_POINT('Ctrl Pts',(-119.234602512152,-107.519067738521,
470.462296651428));
#272245=CARTESIAN_POINT('Ctrl Pts',(-126.9104585261,-97.5309980386224,468.462296651428));
#272246=CARTESIAN_POINT('Ctrl Pts',(-134.586314540048,-87.5429283387234,
466.462296651428));
#272247=CARTESIAN_POINT('Ctrl Pts',(-140.605189688823,-76.4770599218137,
464.462296651428));
#272248=CARTESIAN_POINT('Ctrl Pts',(-146.624064837599,-65.4111915049041,
462.462296651428));
#272249=CARTESIAN_POINT('Ctrl Pts',(-150.837754439537,-53.5400027769199,
460.462296651428));
#272250=CARTESIAN_POINT('Ctrl Pts',(-155.051444041475,-41.6688140489356,
458.462296651428));
#272251=CARTESIAN_POINT('Ctrl Pts',(-157.356193074143,-29.2846130745764,
456.462296651428));
#272252=CARTESIAN_POINT('Ctrl Pts',(-159.660942106811,-16.9004121002171,
454.462296651429));
#272253=CARTESIAN_POINT('Ctrl Pts',(-160.,-4.30813900827815,452.462296651428));
#272254=CARTESIAN_POINT('Ctrl Pts',(-160.339057893189,8.28413408366081,
450.462296651428));
#272255=CARTESIAN_POINT('Ctrl Pts',(-158.704075916301,20.7744157382975,
448.462296651428));
#272256=CARTESIAN_POINT('Ctrl Pts',(-157.069093939413,33.2646973929342,
446.462296651428));
#272257=CARTESIAN_POINT('Ctrl Pts',(-153.500330774912,45.3454354230633,
444.462296651428));
#272258=CARTESIAN_POINT('Ctrl Pts',(-149.931567610412,57.4261734531924,
442.462296651428));
#272259=CARTESIAN_POINT('Ctrl Pts',(-144.516898051455,68.7998999948413,
440.462296651428));
#272260=CARTESIAN_POINT('Ctrl Pts',(-139.102228492497,80.1736265364901,
438.462296651428));
#272261=CARTESIAN_POINT('Ctrl Pts',(-131.974979673883,90.5602826949691,
436.462296651428));
#272262=CARTESIAN_POINT('Ctrl Pts',(-124.847730855269,100.946938853448,
434.462296651428));
#272263=CARTESIAN_POINT('Ctrl Pts',(-116.183399296895,110.0907706828,432.462296651428));
#272264=CARTESIAN_POINT('Ctrl Pts',(-107.519067738521,119.234602512152,
430.462296651428));
#272265=CARTESIAN_POINT('Ctrl Pts',(-97.5309980386224,126.9104585261,428.462296651428));
#272266=CARTESIAN_POINT('Ctrl Pts',(-87.5429283387233,134.586314540048,
426.462296651428));
#272267=CARTESIAN_POINT('Ctrl Pts',(-76.4770599218137,140.605189688823,
424.462296651428));
#272268=CARTESIAN_POINT('Ctrl Pts',(-65.4111915049042,146.624064837599,
422.462296651428));
#272269=CARTESIAN_POINT('Ctrl Pts',(-53.5400027769199,150.837754439537,
420.462296651428));
#272270=CARTESIAN_POINT('Ctrl Pts',(-41.6688140489356,155.051444041475,
418.462296651428));
#272271=CARTESIAN_POINT('Ctrl Pts',(-29.2846130745764,157.356193074143,
416.462296651428));
#272272=CARTESIAN_POINT('Ctrl Pts',(-16.9004121002172,159.660942106811,
414.462296651428));
#272273=CARTESIAN_POINT('Ctrl Pts',(-4.30813900827816,160.,412.462296651428));
#272274=CARTESIAN_POINT('Ctrl Pts',(8.28413408366087,160.339057893189,410.462296651428));
#272275=CARTESIAN_POINT('Ctrl Pts',(20.7744157382975,158.704075916301,408.462296651428));
#272276=CARTESIAN_POINT('Ctrl Pts',(33.2646973929342,157.069093939413,406.462296651428));
#272277=CARTESIAN_POINT('Ctrl Pts',(45.3454354230633,153.500330774912,404.462296651428));
#272278=CARTESIAN_POINT('Ctrl Pts',(57.4261734531925,149.931567610412,402.462296651428));
#272279=CARTESIAN_POINT('Ctrl Pts',(68.7998999948413,144.516898051455,400.462296651428));
#272280=CARTESIAN_POINT('Ctrl Pts',(80.1736265364901,139.102228492498,398.462296651428));
#272281=CARTESIAN_POINT('Ctrl Pts',(90.560282694969,131.974979673883,396.462296651428));
#272282=CARTESIAN_POINT('Ctrl Pts',(100.946938853448,124.847730855269,394.462296651428));
#272283=CARTESIAN_POINT('Ctrl Pts',(110.0907706828,116.183399296895,392.462296651428));
#272284=CARTESIAN_POINT('Ctrl Pts',(119.234602512152,107.519067738521,390.462296651428));
#272285=CARTESIAN_POINT('Ctrl Pts',(126.9104585261,97.5309980386224,388.462296651428));
#272286=CARTESIAN_POINT('Ctrl Pts',(134.586314540048,87.5429283387233,386.462296651428));
#272287=CARTESIAN_POINT('Ctrl Pts',(140.605189688823,76.4770599218137,384.462296651428));
#272288=CARTESIAN_POINT('Ctrl Pts',(146.624064837599,65.4111915049042,382.462296651428));
#272289=CARTESIAN_POINT('Ctrl Pts',(150.837754439537,53.5400027769199,380.462296651428));
#272290=CARTESIAN_POINT('Ctrl Pts',(155.051444041475,41.6688140489356,378.462296651428));
#272291=CARTESIAN_POINT('Ctrl Pts',(157.356193074143,29.2846130745764,376.462296651428));
#272292=CARTESIAN_POINT('Ctrl Pts',(159.660942106811,16.9004121002172,374.462296651428));
#272293=CARTESIAN_POINT('Ctrl Pts',(160.,4.30813900827813,372.462296651428));
#272294=CARTESIAN_POINT('Ctrl Pts',(160.,-4.30813900827805,537.537703348572));
#272295=CARTESIAN_POINT('Ctrl Pts',(159.660942106811,-16.900412100217,535.537703348572));
#272296=CARTESIAN_POINT('Ctrl Pts',(157.356193074143,-29.2846130745763,
533.537703348572));
#272297=CARTESIAN_POINT('Ctrl Pts',(155.051444041475,-41.6688140489355,
531.537703348572));
#272298=CARTESIAN_POINT('Ctrl Pts',(150.837754439537,-53.5400027769198,
529.537703348572));
#272299=CARTESIAN_POINT('Ctrl Pts',(146.624064837599,-65.411191504904,527.537703348572));
#272300=CARTESIAN_POINT('Ctrl Pts',(140.605189688823,-76.4770599218136,
525.537703348572));
#272301=CARTESIAN_POINT('Ctrl Pts',(134.586314540048,-87.5429283387233,
523.537703348572));
#272302=CARTESIAN_POINT('Ctrl Pts',(126.9104585261,-97.5309980386223,521.537703348572));
#272303=CARTESIAN_POINT('Ctrl Pts',(119.234602512152,-107.519067738521,
519.537703348572));
#272304=CARTESIAN_POINT('Ctrl Pts',(110.0907706828,-116.183399296895,517.537703348572));
#272305=CARTESIAN_POINT('Ctrl Pts',(100.946938853448,-124.847730855269,
515.537703348572));
#272306=CARTESIAN_POINT('Ctrl Pts',(90.5602826949691,-131.974979673883,
513.537703348572));
#272307=CARTESIAN_POINT('Ctrl Pts',(80.1736265364902,-139.102228492497,
511.537703348572));
#272308=CARTESIAN_POINT('Ctrl Pts',(68.7998999948414,-144.516898051454,
509.537703348572));
#272309=CARTESIAN_POINT('Ctrl Pts',(57.4261734531925,-149.931567610412,
507.537703348572));
#272310=CARTESIAN_POINT('Ctrl Pts',(45.3454354230634,-153.500330774912,
505.537703348572));
#272311=CARTESIAN_POINT('Ctrl Pts',(33.2646973929343,-157.069093939413,
503.537703348572));
#272312=CARTESIAN_POINT('Ctrl Pts',(20.7744157382976,-158.704075916301,
501.537703348572));
#272313=CARTESIAN_POINT('Ctrl Pts',(8.28413408366091,-160.339057893189,
499.537703348572));
#272314=CARTESIAN_POINT('Ctrl Pts',(-4.30813900827804,-160.,497.537703348572));
#272315=CARTESIAN_POINT('Ctrl Pts',(-16.900412100217,-159.660942106811,
495.537703348572));
#272316=CARTESIAN_POINT('Ctrl Pts',(-29.2846130745763,-157.356193074143,
493.537703348572));
#272317=CARTESIAN_POINT('Ctrl Pts',(-41.6688140489355,-155.051444041475,
491.537703348572));
#272318=CARTESIAN_POINT('Ctrl Pts',(-53.5400027769198,-150.837754439537,
489.537703348572));
#272319=CARTESIAN_POINT('Ctrl Pts',(-65.411191504904,-146.624064837599,
487.537703348572));
#272320=CARTESIAN_POINT('Ctrl Pts',(-76.4770599218136,-140.605189688823,
485.537703348572));
#272321=CARTESIAN_POINT('Ctrl Pts',(-87.5429283387233,-134.586314540048,
483.537703348572));
#272322=CARTESIAN_POINT('Ctrl Pts',(-97.5309980386223,-126.9104585261,481.537703348572));
#272323=CARTESIAN_POINT('Ctrl Pts',(-107.519067738521,-119.234602512152,
479.537703348572));
#272324=CARTESIAN_POINT('Ctrl Pts',(-116.183399296895,-110.0907706828,477.537703348572));
#272325=CARTESIAN_POINT('Ctrl Pts',(-124.847730855269,-100.946938853448,
475.537703348572));
#272326=CARTESIAN_POINT('Ctrl Pts',(-131.974979673883,-90.5602826949692,
473.537703348572));
#272327=CARTESIAN_POINT('Ctrl Pts',(-139.102228492497,-80.1736265364902,
471.537703348572));
#272328=CARTESIAN_POINT('Ctrl Pts',(-144.516898051454,-68.7998999948414,
469.537703348572));
#272329=CARTESIAN_POINT('Ctrl Pts',(-149.931567610412,-57.4261734531925,
467.537703348572));
#272330=CARTESIAN_POINT('Ctrl Pts',(-153.500330774912,-45.3454354230634,
465.537703348572));
#272331=CARTESIAN_POINT('Ctrl Pts',(-157.069093939413,-33.2646973929344,
463.537703348572));
#272332=CARTESIAN_POINT('Ctrl Pts',(-158.704075916301,-20.7744157382976,
461.537703348572));
#272333=CARTESIAN_POINT('Ctrl Pts',(-160.339057893189,-8.28413408366092,
459.537703348572));
#272334=CARTESIAN_POINT('Ctrl Pts',(-160.,4.30813900827803,457.537703348572));
#272335=CARTESIAN_POINT('Ctrl Pts',(-159.660942106811,16.900412100217,455.537703348572));
#272336=CARTESIAN_POINT('Ctrl Pts',(-157.356193074143,29.2846130745763,
453.537703348572));
#272337=CARTESIAN_POINT('Ctrl Pts',(-155.051444041475,41.6688140489355,
451.537703348572));
#272338=CARTESIAN_POINT('Ctrl Pts',(-150.837754439537,53.5400027769198,
449.537703348572));
#272339=CARTESIAN_POINT('Ctrl Pts',(-146.624064837599,65.411191504904,447.537703348572));
#272340=CARTESIAN_POINT('Ctrl Pts',(-140.605189688823,76.4770599218136,
445.537703348572));
#272341=CARTESIAN_POINT('Ctrl Pts',(-134.586314540048,87.5429283387233,
443.537703348572));
#272342=CARTESIAN_POINT('Ctrl Pts',(-126.9104585261,97.5309980386223,441.537703348572));
#272343=CARTESIAN_POINT('Ctrl Pts',(-119.234602512152,107.519067738521,
439.537703348572));
#272344=CARTESIAN_POINT('Ctrl Pts',(-110.0907706828,116.183399296895,437.537703348572));
#272345=CARTESIAN_POINT('Ctrl Pts',(-100.946938853448,124.847730855269,
435.537703348572));
#272346=CARTESIAN_POINT('Ctrl Pts',(-90.5602826949692,131.974979673883,
433.537703348572));
#272347=CARTESIAN_POINT('Ctrl Pts',(-80.1736265364901,139.102228492497,
431.537703348572));
#272348=CARTESIAN_POINT('Ctrl Pts',(-68.7998999948414,144.516898051454,
429.537703348572));
#272349=CARTESIAN_POINT('Ctrl Pts',(-57.4261734531926,149.931567610412,
427.537703348572));
#272350=CARTESIAN_POINT('Ctrl Pts',(-45.3454354230634,153.500330774912,
425.537703348572));
#272351=CARTESIAN_POINT('Ctrl Pts',(-33.2646973929343,157.069093939413,
423.537703348572));
#272352=CARTESIAN_POINT('Ctrl Pts',(-20.7744157382976,158.704075916301,
421.537703348572));
#272353=CARTESIAN_POINT('Ctrl Pts',(-8.284134083661,160.339057893189,419.537703348572));
#272354=CARTESIAN_POINT('Ctrl Pts',(4.30813900827803,160.,417.537703348572));
#272355=CARTESIAN_POINT('Ctrl Pts',(16.9004121002171,159.660942106811,415.537703348572));
#272356=CARTESIAN_POINT('Ctrl Pts',(29.2846130745762,157.356193074143,413.537703348572));
#272357=CARTESIAN_POINT('Ctrl Pts',(41.6688140489354,155.051444041476,411.537703348572));
#272358=CARTESIAN_POINT('Ctrl Pts',(53.5400027769198,150.837754439537,409.537703348572));
#272359=CARTESIAN_POINT('Ctrl Pts',(65.4111915049041,146.624064837599,407.537703348572));
#272360=CARTESIAN_POINT('Ctrl Pts',(76.4770599218136,140.605189688823,405.537703348572));
#272361=CARTESIAN_POINT('Ctrl Pts',(87.5429283387232,134.586314540048,403.537703348572));
#272362=CARTESIAN_POINT('Ctrl Pts',(97.5309980386223,126.9104585261,401.537703348572));
#272363=CARTESIAN_POINT('Ctrl Pts',(107.519067738521,119.234602512152,399.537703348572));
#272364=CARTESIAN_POINT('Ctrl Pts',(116.183399296895,110.0907706828,397.537703348572));
#272365=CARTESIAN_POINT('Ctrl Pts',(124.847730855269,100.946938853448,395.537703348572));
#272366=CARTESIAN_POINT('Ctrl Pts',(131.974979673883,90.5602826949692,393.537703348572));
#272367=CARTESIAN_POINT('Ctrl Pts',(139.102228492497,80.1736265364902,391.537703348572));
#272368=CARTESIAN_POINT('Ctrl Pts',(144.516898051454,68.7998999948414,389.537703348572));
#272369=CARTESIAN_POINT('Ctrl Pts',(149.931567610412,57.4261734531926,387.537703348572));
#272370=CARTESIAN_POINT('Ctrl Pts',(153.500330774912,45.3454354230634,385.537703348572));
#272371=CARTESIAN_POINT('Ctrl Pts',(157.069093939413,33.2646973929343,383.537703348572));
#272372=CARTESIAN_POINT('Ctrl Pts',(158.704075916301,20.7744157382976,381.537703348572));
#272373=CARTESIAN_POINT('Ctrl Pts',(160.339057893189,8.28413408366101,379.537703348572));
#272374=CARTESIAN_POINT('Ctrl Pts',(160.,-4.30813900827805,377.537703348572));
#272375=CARTESIAN_POINT('Origin',(160.,3.64291929955129E-14,375.));
#272376=CARTESIAN_POINT('',(160.,-4.30813900827807,377.537703348572));
#272377=CARTESIAN_POINT('',(160.,1.10715726269171E-13,375.));
#272378=CARTESIAN_POINT('',(160.,3.64291929955129E-14,375.));
#272379=CARTESIAN_POINT('',(160.,4.30813900827833,378.90811221526));
#272380=CARTESIAN_POINT('Ctrl Pts',(160.,-4.30813900827807,377.537703348572));
#272381=CARTESIAN_POINT('Ctrl Pts',(160.,-1.43594781992484,377.99388646458));
#272382=CARTESIAN_POINT('Ctrl Pts',(160.,1.43604209806729,378.451335906457));
#272383=CARTESIAN_POINT('Ctrl Pts',(160.,4.30813900827833,378.90811221526));
#272384=CARTESIAN_POINT('Ctrl Pts',(160.,4.30813900827833,378.90811221526));
#272385=CARTESIAN_POINT('Ctrl Pts',(160.,2.8921527671012,377.623305748502));
#272386=CARTESIAN_POINT('Ctrl Pts',(160.,1.4761797878303,376.338484547026));
#272387=CARTESIAN_POINT('Ctrl Pts',(160.,0.0597455111575994,375.05417203362));
#272388=CARTESIAN_POINT('Ctrl Pts',(160.,0.039830432387403,375.036114588039));
#272389=CARTESIAN_POINT('Ctrl Pts',(160.,0.0199151703859646,375.01805734454));
#272390=CARTESIAN_POINT('Ctrl Pts',(160.,1.64868119156836E-13,375.));
#272391=CARTESIAN_POINT('Ctrl Pts',(160.,4.30813900827813,532.462296651428));
#272392=CARTESIAN_POINT('Ctrl Pts',(160.339057893189,-8.28413408366083,
530.462296651428));
#272393=CARTESIAN_POINT('Ctrl Pts',(158.704075916301,-20.7744157382975,
528.462296651428));
#272394=CARTESIAN_POINT('Ctrl Pts',(157.069093939413,-33.2646973929343,
526.462296651428));
#272395=CARTESIAN_POINT('Ctrl Pts',(153.500330774912,-45.3454354230633,
524.462296651428));
#272396=CARTESIAN_POINT('Ctrl Pts',(149.931567610412,-57.4261734531924,
522.462296651428));
#272397=CARTESIAN_POINT('Ctrl Pts',(144.516898051455,-68.7998999948413,
520.462296651428));
#272398=CARTESIAN_POINT('Ctrl Pts',(139.102228492497,-80.1736265364901,
518.462296651428));
#272399=CARTESIAN_POINT('Ctrl Pts',(131.974979673883,-90.5602826949691,
516.462296651428));
#272400=CARTESIAN_POINT('Ctrl Pts',(124.847730855269,-100.946938853448,
514.462296651428));
#272401=CARTESIAN_POINT('Ctrl Pts',(116.183399296895,-110.0907706828,512.462296651428));
#272402=CARTESIAN_POINT('Ctrl Pts',(107.519067738521,-119.234602512152,
510.462296651428));
#272403=CARTESIAN_POINT('Ctrl Pts',(97.5309980386224,-126.9104585261,508.462296651428));
#272404=CARTESIAN_POINT('Ctrl Pts',(87.5429283387234,-134.586314540048,
506.462296651428));
#272405=CARTESIAN_POINT('Ctrl Pts',(76.4770599218137,-140.605189688823,
504.462296651428));
#272406=CARTESIAN_POINT('Ctrl Pts',(65.4111915049041,-146.624064837599,
502.462296651428));
#272407=CARTESIAN_POINT('Ctrl Pts',(53.5400027769198,-150.837754439537,
500.462296651428));
#272408=CARTESIAN_POINT('Ctrl Pts',(41.6688140489356,-155.051444041475,
498.462296651428));
#272409=CARTESIAN_POINT('Ctrl Pts',(29.2846130745764,-157.356193074143,
496.462296651428));
#272410=CARTESIAN_POINT('Ctrl Pts',(16.9004121002171,-159.660942106811,
494.462296651428));
#272411=CARTESIAN_POINT('Ctrl Pts',(4.30813900827814,-160.,492.462296651428));
#272412=CARTESIAN_POINT('Ctrl Pts',(-8.28413408366082,-160.339057893189,
490.462296651428));
#272413=CARTESIAN_POINT('Ctrl Pts',(-20.7744157382975,-158.704075916301,
488.462296651428));
#272414=CARTESIAN_POINT('Ctrl Pts',(-33.2646973929342,-157.069093939413,
486.462296651428));
#272415=CARTESIAN_POINT('Ctrl Pts',(-45.3454354230633,-153.500330774912,
484.462296651428));
#272416=CARTESIAN_POINT('Ctrl Pts',(-57.4261734531924,-149.931567610412,
482.462296651428));
#272417=CARTESIAN_POINT('Ctrl Pts',(-68.7998999948413,-144.516898051455,
480.462296651428));
#272418=CARTESIAN_POINT('Ctrl Pts',(-80.1736265364901,-139.102228492497,
478.462296651428));
#272419=CARTESIAN_POINT('Ctrl Pts',(-90.5602826949691,-131.974979673883,
476.462296651428));
#272420=CARTESIAN_POINT('Ctrl Pts',(-100.946938853448,-124.847730855269,
474.462296651428));
#272421=CARTESIAN_POINT('Ctrl Pts',(-110.0907706828,-116.183399296895,472.462296651428));
#272422=CARTESIAN_POINT('Ctrl Pts',(-119.234602512152,-107.519067738521,
470.462296651428));
#272423=CARTESIAN_POINT('Ctrl Pts',(-126.9104585261,-97.5309980386224,468.462296651428));
#272424=CARTESIAN_POINT('Ctrl Pts',(-134.586314540048,-87.5429283387234,
466.462296651428));
#272425=CARTESIAN_POINT('Ctrl Pts',(-140.605189688823,-76.4770599218137,
464.462296651428));
#272426=CARTESIAN_POINT('Ctrl Pts',(-146.624064837599,-65.4111915049041,
462.462296651428));
#272427=CARTESIAN_POINT('Ctrl Pts',(-150.837754439537,-53.5400027769199,
460.462296651428));
#272428=CARTESIAN_POINT('Ctrl Pts',(-155.051444041475,-41.6688140489356,
458.462296651428));
#272429=CARTESIAN_POINT('Ctrl Pts',(-157.356193074143,-29.2846130745764,
456.462296651428));
#272430=CARTESIAN_POINT('Ctrl Pts',(-159.660942106811,-16.9004121002171,
454.462296651429));
#272431=CARTESIAN_POINT('Ctrl Pts',(-160.,-4.30813900827815,452.462296651428));
#272432=CARTESIAN_POINT('Ctrl Pts',(-160.339057893189,8.28413408366081,
450.462296651428));
#272433=CARTESIAN_POINT('Ctrl Pts',(-158.704075916301,20.7744157382975,
448.462296651428));
#272434=CARTESIAN_POINT('Ctrl Pts',(-157.069093939413,33.2646973929342,
446.462296651428));
#272435=CARTESIAN_POINT('Ctrl Pts',(-153.500330774912,45.3454354230633,
444.462296651428));
#272436=CARTESIAN_POINT('Ctrl Pts',(-149.931567610412,57.4261734531924,
442.462296651428));
#272437=CARTESIAN_POINT('Ctrl Pts',(-144.516898051455,68.7998999948413,
440.462296651428));
#272438=CARTESIAN_POINT('Ctrl Pts',(-139.102228492497,80.1736265364901,
438.462296651428));
#272439=CARTESIAN_POINT('Ctrl Pts',(-131.974979673883,90.5602826949691,
436.462296651428));
#272440=CARTESIAN_POINT('Ctrl Pts',(-124.847730855269,100.946938853448,
434.462296651428));
#272441=CARTESIAN_POINT('Ctrl Pts',(-116.183399296895,110.0907706828,432.462296651428));
#272442=CARTESIAN_POINT('Ctrl Pts',(-107.519067738521,119.234602512152,
430.462296651428));
#272443=CARTESIAN_POINT('Ctrl Pts',(-97.5309980386224,126.9104585261,428.462296651428));
#272444=CARTESIAN_POINT('Ctrl Pts',(-87.5429283387233,134.586314540048,
426.462296651428));
#272445=CARTESIAN_POINT('Ctrl Pts',(-76.4770599218137,140.605189688823,
424.462296651428));
#272446=CARTESIAN_POINT('Ctrl Pts',(-65.4111915049042,146.624064837599,
422.462296651428));
#272447=CARTESIAN_POINT('Ctrl Pts',(-53.5400027769199,150.837754439537,
420.462296651428));
#272448=CARTESIAN_POINT('Ctrl Pts',(-41.6688140489356,155.051444041475,
418.462296651428));
#272449=CARTESIAN_POINT('Ctrl Pts',(-29.2846130745764,157.356193074143,
416.462296651428));
#272450=CARTESIAN_POINT('Ctrl Pts',(-16.9004121002172,159.660942106811,
414.462296651428));
#272451=CARTESIAN_POINT('Ctrl Pts',(-4.30813900827816,160.,412.462296651428));
#272452=CARTESIAN_POINT('Ctrl Pts',(8.28413408366087,160.339057893189,410.462296651428));
#272453=CARTESIAN_POINT('Ctrl Pts',(20.7744157382975,158.704075916301,408.462296651428));
#272454=CARTESIAN_POINT('Ctrl Pts',(33.2646973929342,157.069093939413,406.462296651428));
#272455=CARTESIAN_POINT('Ctrl Pts',(45.3454354230633,153.500330774912,404.462296651428));
#272456=CARTESIAN_POINT('Ctrl Pts',(57.4261734531925,149.931567610412,402.462296651428));
#272457=CARTESIAN_POINT('Ctrl Pts',(68.7998999948413,144.516898051455,400.462296651428));
#272458=CARTESIAN_POINT('Ctrl Pts',(80.1736265364901,139.102228492498,398.462296651428));
#272459=CARTESIAN_POINT('Ctrl Pts',(90.560282694969,131.974979673883,396.462296651428));
#272460=CARTESIAN_POINT('Ctrl Pts',(100.946938853448,124.847730855269,394.462296651428));
#272461=CARTESIAN_POINT('Ctrl Pts',(110.0907706828,116.183399296895,392.462296651428));
#272462=CARTESIAN_POINT('Ctrl Pts',(119.234602512152,107.519067738521,390.462296651428));
#272463=CARTESIAN_POINT('Ctrl Pts',(126.9104585261,97.5309980386224,388.462296651428));
#272464=CARTESIAN_POINT('Ctrl Pts',(134.586314540048,87.5429283387233,386.462296651428));
#272465=CARTESIAN_POINT('Ctrl Pts',(140.605189688823,76.4770599218137,384.462296651428));
#272466=CARTESIAN_POINT('Ctrl Pts',(146.624064837599,65.4111915049042,382.462296651428));
#272467=CARTESIAN_POINT('Ctrl Pts',(150.837754439537,53.5400027769199,380.462296651428));
#272468=CARTESIAN_POINT('Ctrl Pts',(155.051444041475,41.6688140489356,378.462296651428));
#272469=CARTESIAN_POINT('Ctrl Pts',(157.356193074143,29.2846130745764,376.462296651428));
#272470=CARTESIAN_POINT('Ctrl Pts',(159.660942106811,16.9004121002172,374.462296651428));
#272471=CARTESIAN_POINT('Ctrl Pts',(160.,4.30813900827813,372.462296651428));
#272472=CARTESIAN_POINT('Ctrl Pts',(160.,-4.30813900827805,537.537703348572));
#272473=CARTESIAN_POINT('Ctrl Pts',(159.660942106811,-16.900412100217,535.537703348572));
#272474=CARTESIAN_POINT('Ctrl Pts',(157.356193074143,-29.2846130745763,
533.537703348572));
#272475=CARTESIAN_POINT('Ctrl Pts',(155.051444041475,-41.6688140489355,
531.537703348572));
#272476=CARTESIAN_POINT('Ctrl Pts',(150.837754439537,-53.5400027769198,
529.537703348572));
#272477=CARTESIAN_POINT('Ctrl Pts',(146.624064837599,-65.411191504904,527.537703348572));
#272478=CARTESIAN_POINT('Ctrl Pts',(140.605189688823,-76.4770599218136,
525.537703348572));
#272479=CARTESIAN_POINT('Ctrl Pts',(134.586314540048,-87.5429283387233,
523.537703348572));
#272480=CARTESIAN_POINT('Ctrl Pts',(126.9104585261,-97.5309980386223,521.537703348572));
#272481=CARTESIAN_POINT('Ctrl Pts',(119.234602512152,-107.519067738521,
519.537703348572));
#272482=CARTESIAN_POINT('Ctrl Pts',(110.0907706828,-116.183399296895,517.537703348572));
#272483=CARTESIAN_POINT('Ctrl Pts',(100.946938853448,-124.847730855269,
515.537703348572));
#272484=CARTESIAN_POINT('Ctrl Pts',(90.5602826949691,-131.974979673883,
513.537703348572));
#272485=CARTESIAN_POINT('Ctrl Pts',(80.1736265364902,-139.102228492497,
511.537703348572));
#272486=CARTESIAN_POINT('Ctrl Pts',(68.7998999948414,-144.516898051454,
509.537703348572));
#272487=CARTESIAN_POINT('Ctrl Pts',(57.4261734531925,-149.931567610412,
507.537703348572));
#272488=CARTESIAN_POINT('Ctrl Pts',(45.3454354230634,-153.500330774912,
505.537703348572));
#272489=CARTESIAN_POINT('Ctrl Pts',(33.2646973929343,-157.069093939413,
503.537703348572));
#272490=CARTESIAN_POINT('Ctrl Pts',(20.7744157382976,-158.704075916301,
501.537703348572));
#272491=CARTESIAN_POINT('Ctrl Pts',(8.28413408366091,-160.339057893189,
499.537703348572));
#272492=CARTESIAN_POINT('Ctrl Pts',(-4.30813900827804,-160.,497.537703348572));
#272493=CARTESIAN_POINT('Ctrl Pts',(-16.900412100217,-159.660942106811,
495.537703348572));
#272494=CARTESIAN_POINT('Ctrl Pts',(-29.2846130745763,-157.356193074143,
493.537703348572));
#272495=CARTESIAN_POINT('Ctrl Pts',(-41.6688140489355,-155.051444041475,
491.537703348572));
#272496=CARTESIAN_POINT('Ctrl Pts',(-53.5400027769198,-150.837754439537,
489.537703348572));
#272497=CARTESIAN_POINT('Ctrl Pts',(-65.411191504904,-146.624064837599,
487.537703348572));
#272498=CARTESIAN_POINT('Ctrl Pts',(-76.4770599218136,-140.605189688823,
485.537703348572));
#272499=CARTESIAN_POINT('Ctrl Pts',(-87.5429283387233,-134.586314540048,
483.537703348572));
#272500=CARTESIAN_POINT('Ctrl Pts',(-97.5309980386223,-126.9104585261,481.537703348572));
#272501=CARTESIAN_POINT('Ctrl Pts',(-107.519067738521,-119.234602512152,
479.537703348572));
#272502=CARTESIAN_POINT('Ctrl Pts',(-116.183399296895,-110.0907706828,477.537703348572));
#272503=CARTESIAN_POINT('Ctrl Pts',(-124.847730855269,-100.946938853448,
475.537703348572));
#272504=CARTESIAN_POINT('Ctrl Pts',(-131.974979673883,-90.5602826949692,
473.537703348572));
#272505=CARTESIAN_POINT('Ctrl Pts',(-139.102228492497,-80.1736265364902,
471.537703348572));
#272506=CARTESIAN_POINT('Ctrl Pts',(-144.516898051454,-68.7998999948414,
469.537703348572));
#272507=CARTESIAN_POINT('Ctrl Pts',(-149.931567610412,-57.4261734531925,
467.537703348572));
#272508=CARTESIAN_POINT('Ctrl Pts',(-153.500330774912,-45.3454354230634,
465.537703348572));
#272509=CARTESIAN_POINT('Ctrl Pts',(-157.069093939413,-33.2646973929344,
463.537703348572));
#272510=CARTESIAN_POINT('Ctrl Pts',(-158.704075916301,-20.7744157382976,
461.537703348572));
#272511=CARTESIAN_POINT('Ctrl Pts',(-160.339057893189,-8.28413408366092,
459.537703348572));
#272512=CARTESIAN_POINT('Ctrl Pts',(-160.,4.30813900827803,457.537703348572));
#272513=CARTESIAN_POINT('Ctrl Pts',(-159.660942106811,16.900412100217,455.537703348572));
#272514=CARTESIAN_POINT('Ctrl Pts',(-157.356193074143,29.2846130745763,
453.537703348572));
#272515=CARTESIAN_POINT('Ctrl Pts',(-155.051444041475,41.6688140489355,
451.537703348572));
#272516=CARTESIAN_POINT('Ctrl Pts',(-150.837754439537,53.5400027769198,
449.537703348572));
#272517=CARTESIAN_POINT('Ctrl Pts',(-146.624064837599,65.411191504904,447.537703348572));
#272518=CARTESIAN_POINT('Ctrl Pts',(-140.605189688823,76.4770599218136,
445.537703348572));
#272519=CARTESIAN_POINT('Ctrl Pts',(-134.586314540048,87.5429283387233,
443.537703348572));
#272520=CARTESIAN_POINT('Ctrl Pts',(-126.9104585261,97.5309980386223,441.537703348572));
#272521=CARTESIAN_POINT('Ctrl Pts',(-119.234602512152,107.519067738521,
439.537703348572));
#272522=CARTESIAN_POINT('Ctrl Pts',(-110.0907706828,116.183399296895,437.537703348572));
#272523=CARTESIAN_POINT('Ctrl Pts',(-100.946938853448,124.847730855269,
435.537703348572));
#272524=CARTESIAN_POINT('Ctrl Pts',(-90.5602826949692,131.974979673883,
433.537703348572));
#272525=CARTESIAN_POINT('Ctrl Pts',(-80.1736265364901,139.102228492497,
431.537703348572));
#272526=CARTESIAN_POINT('Ctrl Pts',(-68.7998999948414,144.516898051454,
429.537703348572));
#272527=CARTESIAN_POINT('Ctrl Pts',(-57.4261734531926,149.931567610412,
427.537703348572));
#272528=CARTESIAN_POINT('Ctrl Pts',(-45.3454354230634,153.500330774912,
425.537703348572));
#272529=CARTESIAN_POINT('Ctrl Pts',(-33.2646973929343,157.069093939413,
423.537703348572));
#272530=CARTESIAN_POINT('Ctrl Pts',(-20.7744157382976,158.704075916301,
421.537703348572));
#272531=CARTESIAN_POINT('Ctrl Pts',(-8.284134083661,160.339057893189,419.537703348572));
#272532=CARTESIAN_POINT('Ctrl Pts',(4.30813900827803,160.,417.537703348572));
#272533=CARTESIAN_POINT('Ctrl Pts',(16.9004121002171,159.660942106811,415.537703348572));
#272534=CARTESIAN_POINT('Ctrl Pts',(29.2846130745762,157.356193074143,413.537703348572));
#272535=CARTESIAN_POINT('Ctrl Pts',(41.6688140489354,155.051444041476,411.537703348572));
#272536=CARTESIAN_POINT('Ctrl Pts',(53.5400027769198,150.837754439537,409.537703348572));
#272537=CARTESIAN_POINT('Ctrl Pts',(65.4111915049041,146.624064837599,407.537703348572));
#272538=CARTESIAN_POINT('Ctrl Pts',(76.4770599218136,140.605189688823,405.537703348572));
#272539=CARTESIAN_POINT('Ctrl Pts',(87.5429283387232,134.586314540048,403.537703348572));
#272540=CARTESIAN_POINT('Ctrl Pts',(97.5309980386223,126.9104585261,401.537703348572));
#272541=CARTESIAN_POINT('Ctrl Pts',(107.519067738521,119.234602512152,399.537703348572));
#272542=CARTESIAN_POINT('Ctrl Pts',(116.183399296895,110.0907706828,397.537703348572));
#272543=CARTESIAN_POINT('Ctrl Pts',(124.847730855269,100.946938853448,395.537703348572));
#272544=CARTESIAN_POINT('Ctrl Pts',(131.974979673883,90.5602826949692,393.537703348572));
#272545=CARTESIAN_POINT('Ctrl Pts',(139.102228492497,80.1736265364902,391.537703348572));
#272546=CARTESIAN_POINT('Ctrl Pts',(144.516898051454,68.7998999948414,389.537703348572));
#272547=CARTESIAN_POINT('Ctrl Pts',(149.931567610412,57.4261734531926,387.537703348572));
#272548=CARTESIAN_POINT('Ctrl Pts',(153.500330774912,45.3454354230634,385.537703348572));
#272549=CARTESIAN_POINT('Ctrl Pts',(157.069093939413,33.2646973929343,383.537703348572));
#272550=CARTESIAN_POINT('Ctrl Pts',(158.704075916301,20.7744157382976,381.537703348572));
#272551=CARTESIAN_POINT('Ctrl Pts',(160.339057893189,8.28413408366101,379.537703348572));
#272552=CARTESIAN_POINT('Ctrl Pts',(160.,-4.30813900827805,377.537703348572));
#272553=CARTESIAN_POINT('Origin',(-4.03737035478301,-0.209103844006933,
379.537622607614));
#272554=CARTESIAN_POINT('Ctrl Pts',(160.,-4.30813900827805,537.537703348572));
#272555=CARTESIAN_POINT('Ctrl Pts',(159.660942106811,-16.900412100217,535.537703348572));
#272556=CARTESIAN_POINT('Ctrl Pts',(157.356193074143,-29.2846130745763,
533.537703348572));
#272557=CARTESIAN_POINT('Ctrl Pts',(155.051444041475,-41.6688140489355,
531.537703348572));
#272558=CARTESIAN_POINT('Ctrl Pts',(150.837754439537,-53.5400027769198,
529.537703348572));
#272559=CARTESIAN_POINT('Ctrl Pts',(146.624064837599,-65.411191504904,527.537703348572));
#272560=CARTESIAN_POINT('Ctrl Pts',(140.605189688823,-76.4770599218136,
525.537703348572));
#272561=CARTESIAN_POINT('Ctrl Pts',(134.586314540048,-87.5429283387233,
523.537703348572));
#272562=CARTESIAN_POINT('Ctrl Pts',(126.9104585261,-97.5309980386223,521.537703348572));
#272563=CARTESIAN_POINT('Ctrl Pts',(119.234602512152,-107.519067738521,
519.537703348572));
#272564=CARTESIAN_POINT('Ctrl Pts',(110.0907706828,-116.183399296895,517.537703348572));
#272565=CARTESIAN_POINT('Ctrl Pts',(100.946938853448,-124.847730855269,
515.537703348572));
#272566=CARTESIAN_POINT('Ctrl Pts',(90.5602826949691,-131.974979673883,
513.537703348572));
#272567=CARTESIAN_POINT('Ctrl Pts',(80.1736265364902,-139.102228492497,
511.537703348572));
#272568=CARTESIAN_POINT('Ctrl Pts',(68.7998999948414,-144.516898051454,
509.537703348572));
#272569=CARTESIAN_POINT('Ctrl Pts',(57.4261734531925,-149.931567610412,
507.537703348572));
#272570=CARTESIAN_POINT('Ctrl Pts',(45.3454354230634,-153.500330774912,
505.537703348572));
#272571=CARTESIAN_POINT('Ctrl Pts',(33.2646973929343,-157.069093939413,
503.537703348572));
#272572=CARTESIAN_POINT('Ctrl Pts',(20.7744157382976,-158.704075916301,
501.537703348572));
#272573=CARTESIAN_POINT('Ctrl Pts',(8.28413408366091,-160.339057893189,
499.537703348572));
#272574=CARTESIAN_POINT('Ctrl Pts',(-4.30813900827804,-160.,497.537703348572));
#272575=CARTESIAN_POINT('Ctrl Pts',(-16.900412100217,-159.660942106811,
495.537703348572));
#272576=CARTESIAN_POINT('Ctrl Pts',(-29.2846130745763,-157.356193074143,
493.537703348572));
#272577=CARTESIAN_POINT('Ctrl Pts',(-41.6688140489355,-155.051444041475,
491.537703348572));
#272578=CARTESIAN_POINT('Ctrl Pts',(-53.5400027769198,-150.837754439537,
489.537703348572));
#272579=CARTESIAN_POINT('Ctrl Pts',(-65.411191504904,-146.624064837599,
487.537703348572));
#272580=CARTESIAN_POINT('Ctrl Pts',(-76.4770599218136,-140.605189688823,
485.537703348572));
#272581=CARTESIAN_POINT('Ctrl Pts',(-87.5429283387233,-134.586314540048,
483.537703348572));
#272582=CARTESIAN_POINT('Ctrl Pts',(-97.5309980386223,-126.9104585261,481.537703348572));
#272583=CARTESIAN_POINT('Ctrl Pts',(-107.519067738521,-119.234602512152,
479.537703348572));
#272584=CARTESIAN_POINT('Ctrl Pts',(-116.183399296895,-110.0907706828,477.537703348572));
#272585=CARTESIAN_POINT('Ctrl Pts',(-124.847730855269,-100.946938853448,
475.537703348572));
#272586=CARTESIAN_POINT('Ctrl Pts',(-131.974979673883,-90.5602826949692,
473.537703348572));
#272587=CARTESIAN_POINT('Ctrl Pts',(-139.102228492497,-80.1736265364902,
471.537703348572));
#272588=CARTESIAN_POINT('Ctrl Pts',(-144.516898051454,-68.7998999948414,
469.537703348572));
#272589=CARTESIAN_POINT('Ctrl Pts',(-149.931567610412,-57.4261734531925,
467.537703348572));
#272590=CARTESIAN_POINT('Ctrl Pts',(-153.500330774912,-45.3454354230634,
465.537703348572));
#272591=CARTESIAN_POINT('Ctrl Pts',(-157.069093939413,-33.2646973929344,
463.537703348572));
#272592=CARTESIAN_POINT('Ctrl Pts',(-158.704075916301,-20.7744157382976,
461.537703348572));
#272593=CARTESIAN_POINT('Ctrl Pts',(-160.339057893189,-8.28413408366092,
459.537703348572));
#272594=CARTESIAN_POINT('Ctrl Pts',(-160.,4.30813900827803,457.537703348572));
#272595=CARTESIAN_POINT('Ctrl Pts',(-159.660942106811,16.900412100217,455.537703348572));
#272596=CARTESIAN_POINT('Ctrl Pts',(-157.356193074143,29.2846130745763,
453.537703348572));
#272597=CARTESIAN_POINT('Ctrl Pts',(-155.051444041475,41.6688140489355,
451.537703348572));
#272598=CARTESIAN_POINT('Ctrl Pts',(-150.837754439537,53.5400027769198,
449.537703348572));
#272599=CARTESIAN_POINT('Ctrl Pts',(-146.624064837599,65.411191504904,447.537703348572));
#272600=CARTESIAN_POINT('Ctrl Pts',(-140.605189688823,76.4770599218136,
445.537703348572));
#272601=CARTESIAN_POINT('Ctrl Pts',(-134.586314540048,87.5429283387233,
443.537703348572));
#272602=CARTESIAN_POINT('Ctrl Pts',(-126.9104585261,97.5309980386223,441.537703348572));
#272603=CARTESIAN_POINT('Ctrl Pts',(-119.234602512152,107.519067738521,
439.537703348572));
#272604=CARTESIAN_POINT('Ctrl Pts',(-110.0907706828,116.183399296895,437.537703348572));
#272605=CARTESIAN_POINT('Ctrl Pts',(-100.946938853448,124.847730855269,
435.537703348572));
#272606=CARTESIAN_POINT('Ctrl Pts',(-90.5602826949692,131.974979673883,
433.537703348572));
#272607=CARTESIAN_POINT('Ctrl Pts',(-80.1736265364901,139.102228492497,
431.537703348572));
#272608=CARTESIAN_POINT('Ctrl Pts',(-68.7998999948414,144.516898051454,
429.537703348572));
#272609=CARTESIAN_POINT('Ctrl Pts',(-57.4261734531926,149.931567610412,
427.537703348572));
#272610=CARTESIAN_POINT('Ctrl Pts',(-45.3454354230634,153.500330774912,
425.537703348572));
#272611=CARTESIAN_POINT('Ctrl Pts',(-33.2646973929343,157.069093939413,
423.537703348572));
#272612=CARTESIAN_POINT('Ctrl Pts',(-20.7744157382976,158.704075916301,
421.537703348572));
#272613=CARTESIAN_POINT('Ctrl Pts',(-8.284134083661,160.339057893189,419.537703348572));
#272614=CARTESIAN_POINT('Ctrl Pts',(4.30813900827803,160.,417.537703348572));
#272615=CARTESIAN_POINT('Ctrl Pts',(16.9004121002171,159.660942106811,415.537703348572));
#272616=CARTESIAN_POINT('Ctrl Pts',(29.2846130745762,157.356193074143,413.537703348572));
#272617=CARTESIAN_POINT('Ctrl Pts',(41.6688140489354,155.051444041476,411.537703348572));
#272618=CARTESIAN_POINT('Ctrl Pts',(53.5400027769198,150.837754439537,409.537703348572));
#272619=CARTESIAN_POINT('Ctrl Pts',(65.4111915049041,146.624064837599,407.537703348572));
#272620=CARTESIAN_POINT('Ctrl Pts',(76.4770599218136,140.605189688823,405.537703348572));
#272621=CARTESIAN_POINT('Ctrl Pts',(87.5429283387232,134.586314540048,403.537703348572));
#272622=CARTESIAN_POINT('Ctrl Pts',(97.5309980386223,126.9104585261,401.537703348572));
#272623=CARTESIAN_POINT('Ctrl Pts',(107.519067738521,119.234602512152,399.537703348572));
#272624=CARTESIAN_POINT('Ctrl Pts',(116.183399296895,110.0907706828,397.537703348572));
#272625=CARTESIAN_POINT('Ctrl Pts',(124.847730855269,100.946938853448,395.537703348572));
#272626=CARTESIAN_POINT('Ctrl Pts',(131.974979673883,90.5602826949692,393.537703348572));
#272627=CARTESIAN_POINT('Ctrl Pts',(139.102228492497,80.1736265364902,391.537703348572));
#272628=CARTESIAN_POINT('Ctrl Pts',(144.516898051454,68.7998999948414,389.537703348572));
#272629=CARTESIAN_POINT('Ctrl Pts',(149.931567610412,57.4261734531926,387.537703348572));
#272630=CARTESIAN_POINT('Ctrl Pts',(153.500330774912,45.3454354230634,385.537703348572));
#272631=CARTESIAN_POINT('Ctrl Pts',(157.069093939413,33.2646973929343,383.537703348572));
#272632=CARTESIAN_POINT('Ctrl Pts',(158.704075916301,20.7744157382976,381.537703348572));
#272633=CARTESIAN_POINT('Ctrl Pts',(160.339057893189,8.28413408366101,379.537703348572));
#272634=CARTESIAN_POINT('Ctrl Pts',(160.,-4.30813900827805,377.537703348572));
#272635=CARTESIAN_POINT('Ctrl Pts',(130.,-4.30813900827807,537.537703348572));
#272636=CARTESIAN_POINT('Ctrl Pts',(129.660942106811,-14.5393608954785,
535.537703348572));
#272637=CARTESIAN_POINT('Ctrl Pts',(127.725542856289,-24.5915791233694,
533.537703348572));
#272638=CARTESIAN_POINT('Ctrl Pts',(125.790143605767,-34.6437973512603,
531.537703348572));
#272639=CARTESIAN_POINT('Ctrl Pts',(122.306058950682,-44.2694929456714,
529.537703348572));
#272640=CARTESIAN_POINT('Ctrl Pts',(118.821974295598,-53.8951885400825,
527.537703348572));
#272641=CARTESIAN_POINT('Ctrl Pts',(113.874993963172,-62.8573449296272,
525.537703348572));
#272642=CARTESIAN_POINT('Ctrl Pts',(108.928013630747,-71.819501319172,523.537703348572));
#272643=CARTESIAN_POINT('Ctrl Pts',(102.639948694851,-79.8974404698481,
521.537703348572));
#272644=CARTESIAN_POINT('Ctrl Pts',(96.351883758956,-87.9753796205242,519.537703348572));
#272645=CARTESIAN_POINT('Ctrl Pts',(88.8775672472035,-94.9701958612989,
517.537703348572));
#272646=CARTESIAN_POINT('Ctrl Pts',(81.403250735451,-101.965012102074,515.537703348572));
#272647=CARTESIAN_POINT('Ctrl Pts',(72.9267251261949,-107.704469842635,
513.537703348572));
#272648=CARTESIAN_POINT('Ctrl Pts',(64.4501995169389,-113.443927583196,
511.537703348572));
#272649=CARTESIAN_POINT('Ctrl Pts',(55.1801850026549,-117.786702325803,
509.537703348572));
#272650=CARTESIAN_POINT('Ctrl Pts',(45.910170488371,-122.129477068411,507.537703348572));
#272651=CARTESIAN_POINT('Ctrl Pts',(36.074925591815,-124.968635286058,505.537703348572));
#272652=CARTESIAN_POINT('Ctrl Pts',(26.239680695259,-127.807793503704,503.537703348572));
#272653=CARTESIAN_POINT('Ctrl Pts',(16.0813817870907,-129.073425698447,
501.537703348572));
#272654=CARTESIAN_POINT('Ctrl Pts',(5.92308287892234,-130.339057893189,
499.537703348572));
#272655=CARTESIAN_POINT('Ctrl Pts',(-4.30813900827806,-130.,497.537703348572));
#272656=CARTESIAN_POINT('Ctrl Pts',(-14.5393608954785,-129.660942106811,
495.537703348572));
#272657=CARTESIAN_POINT('Ctrl Pts',(-24.5915791233694,-127.725542856289,
493.537703348572));
#272658=CARTESIAN_POINT('Ctrl Pts',(-34.6437973512603,-125.790143605767,
491.537703348572));
#272659=CARTESIAN_POINT('Ctrl Pts',(-44.2694929456713,-122.306058950682,
489.537703348572));
#272660=CARTESIAN_POINT('Ctrl Pts',(-53.8951885400825,-118.821974295598,
487.537703348572));
#272661=CARTESIAN_POINT('Ctrl Pts',(-62.8573449296272,-113.874993963172,
485.537703348572));
#272662=CARTESIAN_POINT('Ctrl Pts',(-71.819501319172,-108.928013630747,
483.537703348572));
#272663=CARTESIAN_POINT('Ctrl Pts',(-79.8974404698481,-102.639948694851,
481.537703348572));
#272664=CARTESIAN_POINT('Ctrl Pts',(-87.9753796205242,-96.351883758956,
479.537703348572));
#272665=CARTESIAN_POINT('Ctrl Pts',(-94.9701958612989,-88.8775672472035,
477.537703348572));
#272666=CARTESIAN_POINT('Ctrl Pts',(-101.965012102074,-81.403250735451,
475.537703348572));
#272667=CARTESIAN_POINT('Ctrl Pts',(-107.704469842635,-72.9267251261949,
473.537703348572));
#272668=CARTESIAN_POINT('Ctrl Pts',(-113.443927583196,-64.4501995169389,
471.537703348572));
#272669=CARTESIAN_POINT('Ctrl Pts',(-117.786702325803,-55.1801850026549,
469.537703348572));
#272670=CARTESIAN_POINT('Ctrl Pts',(-122.129477068411,-45.910170488371,
467.537703348572));
#272671=CARTESIAN_POINT('Ctrl Pts',(-124.968635286058,-36.074925591815,
465.537703348572));
#272672=CARTESIAN_POINT('Ctrl Pts',(-127.807793503704,-26.239680695259,
463.537703348572));
#272673=CARTESIAN_POINT('Ctrl Pts',(-129.073425698447,-16.0813817870907,
461.537703348572));
#272674=CARTESIAN_POINT('Ctrl Pts',(-130.339057893189,-5.92308287892235,
459.537703348572));
#272675=CARTESIAN_POINT('Ctrl Pts',(-130.,4.30813900827805,457.537703348572));
#272676=CARTESIAN_POINT('Ctrl Pts',(-129.660942106811,14.5393608954784,
455.537703348572));
#272677=CARTESIAN_POINT('Ctrl Pts',(-127.725542856289,24.5915791233693,
453.537703348572));
#272678=CARTESIAN_POINT('Ctrl Pts',(-125.790143605767,34.6437973512602,
451.537703348572));
#272679=CARTESIAN_POINT('Ctrl Pts',(-122.306058950682,44.2694929456713,
449.537703348572));
#272680=CARTESIAN_POINT('Ctrl Pts',(-118.821974295598,53.8951885400825,
447.537703348572));
#272681=CARTESIAN_POINT('Ctrl Pts',(-113.874993963172,62.8573449296272,
445.537703348572));
#272682=CARTESIAN_POINT('Ctrl Pts',(-108.928013630747,71.819501319172,443.537703348572));
#272683=CARTESIAN_POINT('Ctrl Pts',(-102.639948694851,79.8974404698481,
441.537703348572));
#272684=CARTESIAN_POINT('Ctrl Pts',(-96.3518837589561,87.9753796205242,
439.537703348572));
#272685=CARTESIAN_POINT('Ctrl Pts',(-88.8775672472035,94.9701958612989,
437.537703348572));
#272686=CARTESIAN_POINT('Ctrl Pts',(-81.403250735451,101.965012102074,435.537703348572));
#272687=CARTESIAN_POINT('Ctrl Pts',(-72.9267251261949,107.704469842635,
433.537703348572));
#272688=CARTESIAN_POINT('Ctrl Pts',(-64.4501995169389,113.443927583196,
431.537703348572));
#272689=CARTESIAN_POINT('Ctrl Pts',(-55.1801850026549,117.786702325803,
429.537703348572));
#272690=CARTESIAN_POINT('Ctrl Pts',(-45.910170488371,122.129477068411,427.537703348572));
#272691=CARTESIAN_POINT('Ctrl Pts',(-36.074925591815,124.968635286058,425.537703348572));
#272692=CARTESIAN_POINT('Ctrl Pts',(-26.239680695259,127.807793503704,423.537703348572));
#272693=CARTESIAN_POINT('Ctrl Pts',(-16.0813817870907,129.073425698447,
421.537703348572));
#272694=CARTESIAN_POINT('Ctrl Pts',(-5.92308287892242,130.339057893189,
419.537703348572));
#272695=CARTESIAN_POINT('Ctrl Pts',(4.30813900827804,130.,417.537703348572));
#272696=CARTESIAN_POINT('Ctrl Pts',(14.5393608954785,129.660942106811,415.537703348572));
#272697=CARTESIAN_POINT('Ctrl Pts',(24.5915791233693,127.725542856289,413.537703348572));
#272698=CARTESIAN_POINT('Ctrl Pts',(34.6437973512602,125.790143605767,411.537703348572));
#272699=CARTESIAN_POINT('Ctrl Pts',(44.2694929456713,122.306058950682,409.537703348572));
#272700=CARTESIAN_POINT('Ctrl Pts',(53.8951885400825,118.821974295598,407.537703348572));
#272701=CARTESIAN_POINT('Ctrl Pts',(62.8573449296272,113.874993963172,405.537703348572));
#272702=CARTESIAN_POINT('Ctrl Pts',(71.819501319172,108.928013630747,403.537703348572));
#272703=CARTESIAN_POINT('Ctrl Pts',(79.8974404698481,102.639948694851,401.537703348572));
#272704=CARTESIAN_POINT('Ctrl Pts',(87.9753796205242,96.351883758956,399.537703348572));
#272705=CARTESIAN_POINT('Ctrl Pts',(94.9701958612989,88.8775672472035,397.537703348572));
#272706=CARTESIAN_POINT('Ctrl Pts',(101.965012102074,81.403250735451,395.537703348572));
#272707=CARTESIAN_POINT('Ctrl Pts',(107.704469842635,72.926725126195,393.537703348572));
#272708=CARTESIAN_POINT('Ctrl Pts',(113.443927583196,64.4501995169389,391.537703348572));
#272709=CARTESIAN_POINT('Ctrl Pts',(117.786702325803,55.1801850026549,389.537703348572));
#272710=CARTESIAN_POINT('Ctrl Pts',(122.129477068411,45.910170488371,387.537703348572));
#272711=CARTESIAN_POINT('Ctrl Pts',(124.968635286058,36.074925591815,385.537703348572));
#272712=CARTESIAN_POINT('Ctrl Pts',(127.807793503704,26.239680695259,383.537703348572));
#272713=CARTESIAN_POINT('Ctrl Pts',(129.073425698447,16.0813817870907,381.537703348572));
#272714=CARTESIAN_POINT('Ctrl Pts',(130.339057893189,5.92308287892242,379.537703348572));
#272715=CARTESIAN_POINT('Ctrl Pts',(130.,-4.30813900827807,377.537703348572));
#272716=CARTESIAN_POINT('Origin',(160.,-1.08084483543429E-12,695.));
#272717=CARTESIAN_POINT('',(160.,4.30813900827813,692.462296651428));
#272718=CARTESIAN_POINT('',(160.,-4.3081390082785,691.09188778474));
#272719=CARTESIAN_POINT('Ctrl Pts',(160.,4.30813900827813,692.462296651428));
#272720=CARTESIAN_POINT('Ctrl Pts',(160.,1.43594781991678,692.006113535419));
#272721=CARTESIAN_POINT('Ctrl Pts',(160.,-1.43604209808348,691.54866409354));
#272722=CARTESIAN_POINT('Ctrl Pts',(160.,-4.3081390082785,691.09188778474));
#272723=CARTESIAN_POINT('',(160.,-2.89658996530608E-13,695.));
#272724=CARTESIAN_POINT('Ctrl Pts',(160.,-4.3081390082785,691.09188778474));
#272725=CARTESIAN_POINT('Ctrl Pts',(160.,-2.89215276710194,692.376694251499));
#272726=CARTESIAN_POINT('Ctrl Pts',(160.,-1.47617978718644,693.661515452264));
#272727=CARTESIAN_POINT('Ctrl Pts',(160.,-0.0597455111855364,694.945827966412));
#272728=CARTESIAN_POINT('Ctrl Pts',(160.,-0.0398304324249309,694.963885412003));
#272729=CARTESIAN_POINT('Ctrl Pts',(160.,-0.0199151703953438,694.981942655471));
#272730=CARTESIAN_POINT('Ctrl Pts',(160.,-3.33066907387547E-13,695.));
#272731=CARTESIAN_POINT('',(160.,3.64291929955129E-14,695.));
#272732=CARTESIAN_POINT('Ctrl Pts',(160.,4.30813900827813,692.462296651428));
#272733=CARTESIAN_POINT('Ctrl Pts',(160.339057893189,-8.28413408366083,
690.462296651428));
#272734=CARTESIAN_POINT('Ctrl Pts',(158.704075916301,-20.7744157382975,
688.462296651428));
#272735=CARTESIAN_POINT('Ctrl Pts',(157.069093939413,-33.2646973929343,
686.462296651429));
#272736=CARTESIAN_POINT('Ctrl Pts',(153.500330774912,-45.3454354230633,
684.462296651428));
#272737=CARTESIAN_POINT('Ctrl Pts',(149.931567610412,-57.4261734531924,
682.462296651428));
#272738=CARTESIAN_POINT('Ctrl Pts',(144.516898051455,-68.7998999948413,
680.462296651428));
#272739=CARTESIAN_POINT('Ctrl Pts',(139.102228492497,-80.1736265364901,
678.462296651428));
#272740=CARTESIAN_POINT('Ctrl Pts',(131.974979673883,-90.5602826949691,
676.462296651428));
#272741=CARTESIAN_POINT('Ctrl Pts',(124.847730855269,-100.946938853448,
674.462296651428));
#272742=CARTESIAN_POINT('Ctrl Pts',(116.183399296895,-110.0907706828,672.462296651428));
#272743=CARTESIAN_POINT('Ctrl Pts',(107.519067738521,-119.234602512152,
670.462296651428));
#272744=CARTESIAN_POINT('Ctrl Pts',(97.5309980386224,-126.9104585261,668.462296651428));
#272745=CARTESIAN_POINT('Ctrl Pts',(87.5429283387234,-134.586314540048,
666.462296651428));
#272746=CARTESIAN_POINT('Ctrl Pts',(76.4770599218137,-140.605189688823,
664.462296651428));
#272747=CARTESIAN_POINT('Ctrl Pts',(65.4111915049041,-146.624064837599,
662.462296651428));
#272748=CARTESIAN_POINT('Ctrl Pts',(53.5400027769198,-150.837754439537,
660.462296651428));
#272749=CARTESIAN_POINT('Ctrl Pts',(41.6688140489356,-155.051444041475,
658.462296651428));
#272750=CARTESIAN_POINT('Ctrl Pts',(29.2846130745764,-157.356193074143,
656.462296651428));
#272751=CARTESIAN_POINT('Ctrl Pts',(16.9004121002171,-159.660942106811,
654.462296651428));
#272752=CARTESIAN_POINT('Ctrl Pts',(4.30813900827814,-160.,652.462296651428));
#272753=CARTESIAN_POINT('Ctrl Pts',(-8.28413408366082,-160.339057893189,
650.462296651428));
#272754=CARTESIAN_POINT('Ctrl Pts',(-20.7744157382975,-158.704075916301,
648.462296651428));
#272755=CARTESIAN_POINT('Ctrl Pts',(-33.2646973929342,-157.069093939413,
646.462296651428));
#272756=CARTESIAN_POINT('Ctrl Pts',(-45.3454354230633,-153.500330774912,
644.462296651428));
#272757=CARTESIAN_POINT('Ctrl Pts',(-57.4261734531924,-149.931567610412,
642.462296651428));
#272758=CARTESIAN_POINT('Ctrl Pts',(-68.7998999948413,-144.516898051455,
640.462296651428));
#272759=CARTESIAN_POINT('Ctrl Pts',(-80.1736265364901,-139.102228492497,
638.462296651428));
#272760=CARTESIAN_POINT('Ctrl Pts',(-90.5602826949691,-131.974979673883,
636.462296651428));
#272761=CARTESIAN_POINT('Ctrl Pts',(-100.946938853448,-124.847730855269,
634.462296651428));
#272762=CARTESIAN_POINT('Ctrl Pts',(-110.0907706828,-116.183399296895,632.462296651428));
#272763=CARTESIAN_POINT('Ctrl Pts',(-119.234602512152,-107.519067738521,
630.462296651428));
#272764=CARTESIAN_POINT('Ctrl Pts',(-126.9104585261,-97.5309980386224,628.462296651428));
#272765=CARTESIAN_POINT('Ctrl Pts',(-134.586314540048,-87.5429283387234,
626.462296651429));
#272766=CARTESIAN_POINT('Ctrl Pts',(-140.605189688823,-76.4770599218137,
624.462296651428));
#272767=CARTESIAN_POINT('Ctrl Pts',(-146.624064837599,-65.4111915049041,
622.462296651428));
#272768=CARTESIAN_POINT('Ctrl Pts',(-150.837754439537,-53.5400027769199,
620.462296651428));
#272769=CARTESIAN_POINT('Ctrl Pts',(-155.051444041475,-41.6688140489356,
618.462296651428));
#272770=CARTESIAN_POINT('Ctrl Pts',(-157.356193074143,-29.2846130745764,
616.462296651428));
#272771=CARTESIAN_POINT('Ctrl Pts',(-159.660942106811,-16.9004121002171,
614.462296651429));
#272772=CARTESIAN_POINT('Ctrl Pts',(-160.,-4.30813900827815,612.462296651428));
#272773=CARTESIAN_POINT('Ctrl Pts',(-160.339057893189,8.28413408366081,
610.462296651428));
#272774=CARTESIAN_POINT('Ctrl Pts',(-158.704075916301,20.7744157382975,
608.462296651428));
#272775=CARTESIAN_POINT('Ctrl Pts',(-157.069093939413,33.2646973929342,
606.462296651428));
#272776=CARTESIAN_POINT('Ctrl Pts',(-153.500330774912,45.3454354230633,
604.462296651428));
#272777=CARTESIAN_POINT('Ctrl Pts',(-149.931567610412,57.4261734531924,
602.462296651429));
#272778=CARTESIAN_POINT('Ctrl Pts',(-144.516898051455,68.7998999948413,
600.462296651428));
#272779=CARTESIAN_POINT('Ctrl Pts',(-139.102228492497,80.1736265364901,
598.462296651428));
#272780=CARTESIAN_POINT('Ctrl Pts',(-131.974979673883,90.5602826949691,
596.462296651428));
#272781=CARTESIAN_POINT('Ctrl Pts',(-124.847730855269,100.946938853448,
594.462296651428));
#272782=CARTESIAN_POINT('Ctrl Pts',(-116.183399296895,110.0907706828,592.462296651428));
#272783=CARTESIAN_POINT('Ctrl Pts',(-107.519067738521,119.234602512152,
590.462296651428));
#272784=CARTESIAN_POINT('Ctrl Pts',(-97.5309980386224,126.9104585261,588.462296651428));
#272785=CARTESIAN_POINT('Ctrl Pts',(-87.5429283387233,134.586314540048,
586.462296651428));
#272786=CARTESIAN_POINT('Ctrl Pts',(-76.4770599218137,140.605189688823,
584.462296651428));
#272787=CARTESIAN_POINT('Ctrl Pts',(-65.4111915049042,146.624064837599,
582.462296651428));
#272788=CARTESIAN_POINT('Ctrl Pts',(-53.5400027769199,150.837754439537,
580.462296651428));
#272789=CARTESIAN_POINT('Ctrl Pts',(-41.6688140489356,155.051444041475,
578.462296651428));
#272790=CARTESIAN_POINT('Ctrl Pts',(-29.2846130745764,157.356193074143,
576.462296651428));
#272791=CARTESIAN_POINT('Ctrl Pts',(-16.9004121002172,159.660942106811,
574.462296651428));
#272792=CARTESIAN_POINT('Ctrl Pts',(-4.30813900827816,160.,572.462296651428));
#272793=CARTESIAN_POINT('Ctrl Pts',(8.28413408366087,160.339057893189,570.462296651428));
#272794=CARTESIAN_POINT('Ctrl Pts',(20.7744157382975,158.704075916301,568.462296651428));
#272795=CARTESIAN_POINT('Ctrl Pts',(33.2646973929342,157.069093939413,566.462296651428));
#272796=CARTESIAN_POINT('Ctrl Pts',(45.3454354230633,153.500330774912,564.462296651428));
#272797=CARTESIAN_POINT('Ctrl Pts',(57.4261734531925,149.931567610412,562.462296651428));
#272798=CARTESIAN_POINT('Ctrl Pts',(68.7998999948413,144.516898051455,560.462296651428));
#272799=CARTESIAN_POINT('Ctrl Pts',(80.1736265364901,139.102228492498,558.462296651428));
#272800=CARTESIAN_POINT('Ctrl Pts',(90.560282694969,131.974979673883,556.462296651428));
#272801=CARTESIAN_POINT('Ctrl Pts',(100.946938853448,124.847730855269,554.462296651428));
#272802=CARTESIAN_POINT('Ctrl Pts',(110.0907706828,116.183399296895,552.462296651428));
#272803=CARTESIAN_POINT('Ctrl Pts',(119.234602512152,107.519067738521,550.462296651428));
#272804=CARTESIAN_POINT('Ctrl Pts',(126.9104585261,97.5309980386224,548.462296651428));
#272805=CARTESIAN_POINT('Ctrl Pts',(134.586314540048,87.5429283387233,546.462296651428));
#272806=CARTESIAN_POINT('Ctrl Pts',(140.605189688823,76.4770599218137,544.462296651428));
#272807=CARTESIAN_POINT('Ctrl Pts',(146.624064837599,65.4111915049042,542.462296651428));
#272808=CARTESIAN_POINT('Ctrl Pts',(150.837754439537,53.5400027769199,540.462296651428));
#272809=CARTESIAN_POINT('Ctrl Pts',(155.051444041475,41.6688140489356,538.462296651428));
#272810=CARTESIAN_POINT('Ctrl Pts',(157.356193074143,29.2846130745764,536.462296651428));
#272811=CARTESIAN_POINT('Ctrl Pts',(159.660942106811,16.9004121002172,534.462296651428));
#272812=CARTESIAN_POINT('Ctrl Pts',(160.,4.30813900827813,532.462296651428));
#272813=CARTESIAN_POINT('Ctrl Pts',(160.,-4.30813900827805,697.537703348572));
#272814=CARTESIAN_POINT('Ctrl Pts',(159.660942106811,-16.900412100217,695.537703348572));
#272815=CARTESIAN_POINT('Ctrl Pts',(157.356193074143,-29.2846130745763,
693.537703348572));
#272816=CARTESIAN_POINT('Ctrl Pts',(155.051444041475,-41.6688140489355,
691.537703348572));
#272817=CARTESIAN_POINT('Ctrl Pts',(150.837754439537,-53.5400027769198,
689.537703348572));
#272818=CARTESIAN_POINT('Ctrl Pts',(146.624064837599,-65.411191504904,687.537703348572));
#272819=CARTESIAN_POINT('Ctrl Pts',(140.605189688823,-76.4770599218136,
685.537703348572));
#272820=CARTESIAN_POINT('Ctrl Pts',(134.586314540048,-87.5429283387233,
683.537703348572));
#272821=CARTESIAN_POINT('Ctrl Pts',(126.9104585261,-97.5309980386223,681.537703348572));
#272822=CARTESIAN_POINT('Ctrl Pts',(119.234602512152,-107.519067738521,
679.537703348572));
#272823=CARTESIAN_POINT('Ctrl Pts',(110.0907706828,-116.183399296895,677.537703348572));
#272824=CARTESIAN_POINT('Ctrl Pts',(100.946938853448,-124.847730855269,
675.537703348572));
#272825=CARTESIAN_POINT('Ctrl Pts',(90.5602826949691,-131.974979673883,
673.537703348572));
#272826=CARTESIAN_POINT('Ctrl Pts',(80.1736265364902,-139.102228492497,
671.537703348572));
#272827=CARTESIAN_POINT('Ctrl Pts',(68.7998999948414,-144.516898051454,
669.537703348572));
#272828=CARTESIAN_POINT('Ctrl Pts',(57.4261734531925,-149.931567610412,
667.537703348572));
#272829=CARTESIAN_POINT('Ctrl Pts',(45.3454354230634,-153.500330774912,
665.537703348572));
#272830=CARTESIAN_POINT('Ctrl Pts',(33.2646973929343,-157.069093939413,
663.537703348572));
#272831=CARTESIAN_POINT('Ctrl Pts',(20.7744157382976,-158.704075916301,
661.537703348572));
#272832=CARTESIAN_POINT('Ctrl Pts',(8.28413408366091,-160.339057893189,
659.537703348572));
#272833=CARTESIAN_POINT('Ctrl Pts',(-4.30813900827804,-160.,657.537703348572));
#272834=CARTESIAN_POINT('Ctrl Pts',(-16.900412100217,-159.660942106811,
655.537703348572));
#272835=CARTESIAN_POINT('Ctrl Pts',(-29.2846130745763,-157.356193074143,
653.537703348572));
#272836=CARTESIAN_POINT('Ctrl Pts',(-41.6688140489355,-155.051444041475,
651.537703348572));
#272837=CARTESIAN_POINT('Ctrl Pts',(-53.5400027769198,-150.837754439537,
649.537703348572));
#272838=CARTESIAN_POINT('Ctrl Pts',(-65.411191504904,-146.624064837599,
647.537703348572));
#272839=CARTESIAN_POINT('Ctrl Pts',(-76.4770599218136,-140.605189688823,
645.537703348572));
#272840=CARTESIAN_POINT('Ctrl Pts',(-87.5429283387233,-134.586314540048,
643.537703348572));
#272841=CARTESIAN_POINT('Ctrl Pts',(-97.5309980386223,-126.9104585261,641.537703348572));
#272842=CARTESIAN_POINT('Ctrl Pts',(-107.519067738521,-119.234602512152,
639.537703348572));
#272843=CARTESIAN_POINT('Ctrl Pts',(-116.183399296895,-110.0907706828,637.537703348572));
#272844=CARTESIAN_POINT('Ctrl Pts',(-124.847730855269,-100.946938853448,
635.537703348572));
#272845=CARTESIAN_POINT('Ctrl Pts',(-131.974979673883,-90.5602826949692,
633.537703348572));
#272846=CARTESIAN_POINT('Ctrl Pts',(-139.102228492497,-80.1736265364902,
631.537703348572));
#272847=CARTESIAN_POINT('Ctrl Pts',(-144.516898051454,-68.7998999948414,
629.537703348572));
#272848=CARTESIAN_POINT('Ctrl Pts',(-149.931567610412,-57.4261734531925,
627.537703348572));
#272849=CARTESIAN_POINT('Ctrl Pts',(-153.500330774912,-45.3454354230634,
625.537703348572));
#272850=CARTESIAN_POINT('Ctrl Pts',(-157.069093939413,-33.2646973929344,
623.537703348572));
#272851=CARTESIAN_POINT('Ctrl Pts',(-158.704075916301,-20.7744157382976,
621.537703348572));
#272852=CARTESIAN_POINT('Ctrl Pts',(-160.339057893189,-8.28413408366092,
619.537703348572));
#272853=CARTESIAN_POINT('Ctrl Pts',(-160.,4.30813900827803,617.537703348572));
#272854=CARTESIAN_POINT('Ctrl Pts',(-159.660942106811,16.900412100217,615.537703348572));
#272855=CARTESIAN_POINT('Ctrl Pts',(-157.356193074143,29.2846130745763,
613.537703348572));
#272856=CARTESIAN_POINT('Ctrl Pts',(-155.051444041475,41.6688140489355,
611.537703348572));
#272857=CARTESIAN_POINT('Ctrl Pts',(-150.837754439537,53.5400027769198,
609.537703348572));
#272858=CARTESIAN_POINT('Ctrl Pts',(-146.624064837599,65.411191504904,607.537703348572));
#272859=CARTESIAN_POINT('Ctrl Pts',(-140.605189688823,76.4770599218136,
605.537703348572));
#272860=CARTESIAN_POINT('Ctrl Pts',(-134.586314540048,87.5429283387233,
603.537703348572));
#272861=CARTESIAN_POINT('Ctrl Pts',(-126.9104585261,97.5309980386223,601.537703348572));
#272862=CARTESIAN_POINT('Ctrl Pts',(-119.234602512152,107.519067738521,
599.537703348572));
#272863=CARTESIAN_POINT('Ctrl Pts',(-110.0907706828,116.183399296895,597.537703348572));
#272864=CARTESIAN_POINT('Ctrl Pts',(-100.946938853448,124.847730855269,
595.537703348572));
#272865=CARTESIAN_POINT('Ctrl Pts',(-90.5602826949692,131.974979673883,
593.537703348572));
#272866=CARTESIAN_POINT('Ctrl Pts',(-80.1736265364901,139.102228492497,
591.537703348572));
#272867=CARTESIAN_POINT('Ctrl Pts',(-68.7998999948414,144.516898051454,
589.537703348572));
#272868=CARTESIAN_POINT('Ctrl Pts',(-57.4261734531926,149.931567610412,
587.537703348572));
#272869=CARTESIAN_POINT('Ctrl Pts',(-45.3454354230634,153.500330774912,
585.537703348572));
#272870=CARTESIAN_POINT('Ctrl Pts',(-33.2646973929343,157.069093939413,
583.537703348572));
#272871=CARTESIAN_POINT('Ctrl Pts',(-20.7744157382976,158.704075916301,
581.537703348572));
#272872=CARTESIAN_POINT('Ctrl Pts',(-8.284134083661,160.339057893189,579.537703348572));
#272873=CARTESIAN_POINT('Ctrl Pts',(4.30813900827803,160.,577.537703348572));
#272874=CARTESIAN_POINT('Ctrl Pts',(16.9004121002171,159.660942106811,575.537703348572));
#272875=CARTESIAN_POINT('Ctrl Pts',(29.2846130745762,157.356193074143,573.537703348572));
#272876=CARTESIAN_POINT('Ctrl Pts',(41.6688140489354,155.051444041476,571.537703348572));
#272877=CARTESIAN_POINT('Ctrl Pts',(53.5400027769198,150.837754439537,569.537703348572));
#272878=CARTESIAN_POINT('Ctrl Pts',(65.4111915049041,146.624064837599,567.537703348572));
#272879=CARTESIAN_POINT('Ctrl Pts',(76.4770599218136,140.605189688823,565.537703348572));
#272880=CARTESIAN_POINT('Ctrl Pts',(87.5429283387232,134.586314540048,563.537703348572));
#272881=CARTESIAN_POINT('Ctrl Pts',(97.5309980386223,126.9104585261,561.537703348572));
#272882=CARTESIAN_POINT('Ctrl Pts',(107.519067738521,119.234602512152,559.537703348572));
#272883=CARTESIAN_POINT('Ctrl Pts',(116.183399296895,110.0907706828,557.537703348572));
#272884=CARTESIAN_POINT('Ctrl Pts',(124.847730855269,100.946938853448,555.537703348572));
#272885=CARTESIAN_POINT('Ctrl Pts',(131.974979673883,90.5602826949692,553.537703348572));
#272886=CARTESIAN_POINT('Ctrl Pts',(139.102228492497,80.1736265364902,551.537703348572));
#272887=CARTESIAN_POINT('Ctrl Pts',(144.516898051454,68.7998999948414,549.537703348572));
#272888=CARTESIAN_POINT('Ctrl Pts',(149.931567610412,57.4261734531926,547.537703348572));
#272889=CARTESIAN_POINT('Ctrl Pts',(153.500330774912,45.3454354230634,545.537703348572));
#272890=CARTESIAN_POINT('Ctrl Pts',(157.069093939413,33.2646973929343,543.537703348572));
#272891=CARTESIAN_POINT('Ctrl Pts',(158.704075916301,20.7744157382976,541.537703348572));
#272892=CARTESIAN_POINT('Ctrl Pts',(160.339057893189,8.28413408366101,539.537703348572));
#272893=CARTESIAN_POINT('Ctrl Pts',(160.,-4.30813900827805,537.537703348572));
#272894=CARTESIAN_POINT('Origin',(-4.03737035479217,0.209103843994654,690.46237739249));
#272895=CARTESIAN_POINT('Ctrl Pts',(130.,4.30813900827812,692.462296651428));
#272896=CARTESIAN_POINT('Ctrl Pts',(130.339057893189,-5.92308287892228,
690.462296651428));
#272897=CARTESIAN_POINT('Ctrl Pts',(129.073425698447,-16.0813817870906,
688.462296651428));
#272898=CARTESIAN_POINT('Ctrl Pts',(127.807793503704,-26.2396806952589,
686.462296651429));
#272899=CARTESIAN_POINT('Ctrl Pts',(124.968635286058,-36.0749255918149,
684.462296651428));
#272900=CARTESIAN_POINT('Ctrl Pts',(122.129477068411,-45.9101704883709,
682.462296651428));
#272901=CARTESIAN_POINT('Ctrl Pts',(117.786702325803,-55.1801850026549,
680.462296651428));
#272902=CARTESIAN_POINT('Ctrl Pts',(113.443927583196,-64.4501995169389,
678.462296651428));
#272903=CARTESIAN_POINT('Ctrl Pts',(107.704469842635,-72.9267251261949,
676.462296651428));
#272904=CARTESIAN_POINT('Ctrl Pts',(101.965012102074,-81.4032507354509,
674.462296651428));
#272905=CARTESIAN_POINT('Ctrl Pts',(94.9701958612989,-88.8775672472035,
672.462296651428));
#272906=CARTESIAN_POINT('Ctrl Pts',(87.9753796205242,-96.351883758956,670.462296651428));
#272907=CARTESIAN_POINT('Ctrl Pts',(79.8974404698481,-102.639948694851,
668.462296651428));
#272908=CARTESIAN_POINT('Ctrl Pts',(71.8195013191721,-108.928013630747,
666.462296651428));
#272909=CARTESIAN_POINT('Ctrl Pts',(62.8573449296273,-113.874993963172,
664.462296651428));
#272910=CARTESIAN_POINT('Ctrl Pts',(53.8951885400825,-118.821974295598,
662.462296651428));
#272911=CARTESIAN_POINT('Ctrl Pts',(44.2694929456714,-122.306058950682,
660.462296651428));
#272912=CARTESIAN_POINT('Ctrl Pts',(34.6437973512603,-125.790143605767,
658.462296651428));
#272913=CARTESIAN_POINT('Ctrl Pts',(24.5915791233694,-127.725542856289,
656.462296651428));
#272914=CARTESIAN_POINT('Ctrl Pts',(14.5393608954785,-129.660942106811,
654.462296651428));
#272915=CARTESIAN_POINT('Ctrl Pts',(4.30813900827813,-130.,652.462296651428));
#272916=CARTESIAN_POINT('Ctrl Pts',(-5.92308287892227,-130.339057893189,
650.462296651428));
#272917=CARTESIAN_POINT('Ctrl Pts',(-16.0813817870906,-129.073425698447,
648.462296651428));
#272918=CARTESIAN_POINT('Ctrl Pts',(-26.2396806952589,-127.807793503705,
646.462296651428));
#272919=CARTESIAN_POINT('Ctrl Pts',(-36.0749255918149,-124.968635286058,
644.462296651428));
#272920=CARTESIAN_POINT('Ctrl Pts',(-45.9101704883709,-122.129477068411,
642.462296651428));
#272921=CARTESIAN_POINT('Ctrl Pts',(-55.1801850026549,-117.786702325803,
640.462296651428));
#272922=CARTESIAN_POINT('Ctrl Pts',(-64.4501995169389,-113.443927583196,
638.462296651428));
#272923=CARTESIAN_POINT('Ctrl Pts',(-72.9267251261949,-107.704469842635,
636.462296651428));
#272924=CARTESIAN_POINT('Ctrl Pts',(-81.4032507354509,-101.965012102074,
634.462296651428));
#272925=CARTESIAN_POINT('Ctrl Pts',(-88.8775672472034,-94.9701958612989,
632.462296651428));
#272926=CARTESIAN_POINT('Ctrl Pts',(-96.351883758956,-87.9753796205242,
630.462296651428));
#272927=CARTESIAN_POINT('Ctrl Pts',(-102.639948694851,-79.8974404698482,
628.462296651428));
#272928=CARTESIAN_POINT('Ctrl Pts',(-108.928013630747,-71.8195013191721,
626.462296651429));
#272929=CARTESIAN_POINT('Ctrl Pts',(-113.874993963172,-62.8573449296273,
624.462296651428));
#272930=CARTESIAN_POINT('Ctrl Pts',(-118.821974295598,-53.8951885400825,
622.462296651428));
#272931=CARTESIAN_POINT('Ctrl Pts',(-122.306058950682,-44.2694929456714,
620.462296651428));
#272932=CARTESIAN_POINT('Ctrl Pts',(-125.790143605767,-34.6437973512603,
618.462296651428));
#272933=CARTESIAN_POINT('Ctrl Pts',(-127.725542856289,-24.5915791233694,
616.462296651428));
#272934=CARTESIAN_POINT('Ctrl Pts',(-129.660942106811,-14.5393608954785,
614.462296651429));
#272935=CARTESIAN_POINT('Ctrl Pts',(-130.,-4.30813900827813,612.462296651428));
#272936=CARTESIAN_POINT('Ctrl Pts',(-130.339057893189,5.92308287892227,
610.462296651428));
#272937=CARTESIAN_POINT('Ctrl Pts',(-129.073425698447,16.0813817870906,
608.462296651428));
#272938=CARTESIAN_POINT('Ctrl Pts',(-127.807793503705,26.2396806952589,
606.462296651428));
#272939=CARTESIAN_POINT('Ctrl Pts',(-124.968635286058,36.0749255918149,
604.462296651428));
#272940=CARTESIAN_POINT('Ctrl Pts',(-122.129477068411,45.9101704883709,
602.462296651429));
#272941=CARTESIAN_POINT('Ctrl Pts',(-117.786702325803,55.1801850026549,
600.462296651428));
#272942=CARTESIAN_POINT('Ctrl Pts',(-113.443927583196,64.4501995169388,
598.462296651428));
#272943=CARTESIAN_POINT('Ctrl Pts',(-107.704469842635,72.9267251261949,
596.462296651428));
#272944=CARTESIAN_POINT('Ctrl Pts',(-101.965012102074,81.4032507354509,
594.462296651428));
#272945=CARTESIAN_POINT('Ctrl Pts',(-94.9701958612989,88.8775672472034,
592.462296651428));
#272946=CARTESIAN_POINT('Ctrl Pts',(-87.9753796205243,96.3518837589559,
590.462296651428));
#272947=CARTESIAN_POINT('Ctrl Pts',(-79.8974404698482,102.639948694851,
588.462296651428));
#272948=CARTESIAN_POINT('Ctrl Pts',(-71.819501319172,108.928013630747,586.462296651428));
#272949=CARTESIAN_POINT('Ctrl Pts',(-62.8573449296273,113.874993963172,
584.462296651428));
#272950=CARTESIAN_POINT('Ctrl Pts',(-53.8951885400826,118.821974295598,
582.462296651428));
#272951=CARTESIAN_POINT('Ctrl Pts',(-44.2694929456714,122.306058950682,
580.462296651428));
#272952=CARTESIAN_POINT('Ctrl Pts',(-34.6437973512603,125.790143605767,
578.462296651428));
#272953=CARTESIAN_POINT('Ctrl Pts',(-24.5915791233694,127.725542856289,
576.462296651428));
#272954=CARTESIAN_POINT('Ctrl Pts',(-14.5393608954786,129.660942106811,
574.462296651428));
#272955=CARTESIAN_POINT('Ctrl Pts',(-4.30813900827814,130.,572.462296651428));
#272956=CARTESIAN_POINT('Ctrl Pts',(5.92308287892232,130.339057893189,570.462296651428));
#272957=CARTESIAN_POINT('Ctrl Pts',(16.0813817870906,129.073425698447,568.462296651428));
#272958=CARTESIAN_POINT('Ctrl Pts',(26.2396806952589,127.807793503705,566.462296651428));
#272959=CARTESIAN_POINT('Ctrl Pts',(36.0749255918149,124.968635286058,564.462296651428));
#272960=CARTESIAN_POINT('Ctrl Pts',(45.9101704883709,122.129477068411,562.462296651428));
#272961=CARTESIAN_POINT('Ctrl Pts',(55.1801850026549,117.786702325803,560.462296651428));
#272962=CARTESIAN_POINT('Ctrl Pts',(64.4501995169388,113.443927583196,558.462296651428));
#272963=CARTESIAN_POINT('Ctrl Pts',(72.9267251261949,107.704469842635,556.462296651428));
#272964=CARTESIAN_POINT('Ctrl Pts',(81.4032507354509,101.965012102074,554.462296651428));
#272965=CARTESIAN_POINT('Ctrl Pts',(88.8775672472034,94.9701958612989,552.462296651428));
#272966=CARTESIAN_POINT('Ctrl Pts',(96.3518837589559,87.9753796205243,550.462296651428));
#272967=CARTESIAN_POINT('Ctrl Pts',(102.639948694851,79.8974404698482,548.462296651428));
#272968=CARTESIAN_POINT('Ctrl Pts',(108.928013630747,71.819501319172,546.462296651428));
#272969=CARTESIAN_POINT('Ctrl Pts',(113.874993963172,62.8573449296273,544.462296651428));
#272970=CARTESIAN_POINT('Ctrl Pts',(118.821974295598,53.8951885400826,542.462296651428));
#272971=CARTESIAN_POINT('Ctrl Pts',(122.306058950682,44.2694929456714,540.462296651428));
#272972=CARTESIAN_POINT('Ctrl Pts',(125.790143605767,34.6437973512603,538.462296651428));
#272973=CARTESIAN_POINT('Ctrl Pts',(127.725542856289,24.5915791233694,536.462296651428));
#272974=CARTESIAN_POINT('Ctrl Pts',(129.660942106811,14.5393608954786,534.462296651428));
#272975=CARTESIAN_POINT('Ctrl Pts',(130.,4.30813900827812,532.462296651428));
#272976=CARTESIAN_POINT('Ctrl Pts',(160.,4.30813900827813,692.462296651428));
#272977=CARTESIAN_POINT('Ctrl Pts',(160.339057893189,-8.28413408366083,
690.462296651428));
#272978=CARTESIAN_POINT('Ctrl Pts',(158.704075916301,-20.7744157382975,
688.462296651428));
#272979=CARTESIAN_POINT('Ctrl Pts',(157.069093939413,-33.2646973929343,
686.462296651429));
#272980=CARTESIAN_POINT('Ctrl Pts',(153.500330774912,-45.3454354230633,
684.462296651428));
#272981=CARTESIAN_POINT('Ctrl Pts',(149.931567610412,-57.4261734531924,
682.462296651428));
#272982=CARTESIAN_POINT('Ctrl Pts',(144.516898051455,-68.7998999948413,
680.462296651428));
#272983=CARTESIAN_POINT('Ctrl Pts',(139.102228492497,-80.1736265364901,
678.462296651428));
#272984=CARTESIAN_POINT('Ctrl Pts',(131.974979673883,-90.5602826949691,
676.462296651428));
#272985=CARTESIAN_POINT('Ctrl Pts',(124.847730855269,-100.946938853448,
674.462296651428));
#272986=CARTESIAN_POINT('Ctrl Pts',(116.183399296895,-110.0907706828,672.462296651428));
#272987=CARTESIAN_POINT('Ctrl Pts',(107.519067738521,-119.234602512152,
670.462296651428));
#272988=CARTESIAN_POINT('Ctrl Pts',(97.5309980386224,-126.9104585261,668.462296651428));
#272989=CARTESIAN_POINT('Ctrl Pts',(87.5429283387234,-134.586314540048,
666.462296651428));
#272990=CARTESIAN_POINT('Ctrl Pts',(76.4770599218137,-140.605189688823,
664.462296651428));
#272991=CARTESIAN_POINT('Ctrl Pts',(65.4111915049041,-146.624064837599,
662.462296651428));
#272992=CARTESIAN_POINT('Ctrl Pts',(53.5400027769198,-150.837754439537,
660.462296651428));
#272993=CARTESIAN_POINT('Ctrl Pts',(41.6688140489356,-155.051444041475,
658.462296651428));
#272994=CARTESIAN_POINT('Ctrl Pts',(29.2846130745764,-157.356193074143,
656.462296651428));
#272995=CARTESIAN_POINT('Ctrl Pts',(16.9004121002171,-159.660942106811,
654.462296651428));
#272996=CARTESIAN_POINT('Ctrl Pts',(4.30813900827814,-160.,652.462296651428));
#272997=CARTESIAN_POINT('Ctrl Pts',(-8.28413408366082,-160.339057893189,
650.462296651428));
#272998=CARTESIAN_POINT('Ctrl Pts',(-20.7744157382975,-158.704075916301,
648.462296651428));
#272999=CARTESIAN_POINT('Ctrl Pts',(-33.2646973929342,-157.069093939413,
646.462296651428));
#273000=CARTESIAN_POINT('Ctrl Pts',(-45.3454354230633,-153.500330774912,
644.462296651428));
#273001=CARTESIAN_POINT('Ctrl Pts',(-57.4261734531924,-149.931567610412,
642.462296651428));
#273002=CARTESIAN_POINT('Ctrl Pts',(-68.7998999948413,-144.516898051455,
640.462296651428));
#273003=CARTESIAN_POINT('Ctrl Pts',(-80.1736265364901,-139.102228492497,
638.462296651428));
#273004=CARTESIAN_POINT('Ctrl Pts',(-90.5602826949691,-131.974979673883,
636.462296651428));
#273005=CARTESIAN_POINT('Ctrl Pts',(-100.946938853448,-124.847730855269,
634.462296651428));
#273006=CARTESIAN_POINT('Ctrl Pts',(-110.0907706828,-116.183399296895,632.462296651428));
#273007=CARTESIAN_POINT('Ctrl Pts',(-119.234602512152,-107.519067738521,
630.462296651428));
#273008=CARTESIAN_POINT('Ctrl Pts',(-126.9104585261,-97.5309980386224,628.462296651428));
#273009=CARTESIAN_POINT('Ctrl Pts',(-134.586314540048,-87.5429283387234,
626.462296651429));
#273010=CARTESIAN_POINT('Ctrl Pts',(-140.605189688823,-76.4770599218137,
624.462296651428));
#273011=CARTESIAN_POINT('Ctrl Pts',(-146.624064837599,-65.4111915049041,
622.462296651428));
#273012=CARTESIAN_POINT('Ctrl Pts',(-150.837754439537,-53.5400027769199,
620.462296651428));
#273013=CARTESIAN_POINT('Ctrl Pts',(-155.051444041475,-41.6688140489356,
618.462296651428));
#273014=CARTESIAN_POINT('Ctrl Pts',(-157.356193074143,-29.2846130745764,
616.462296651428));
#273015=CARTESIAN_POINT('Ctrl Pts',(-159.660942106811,-16.9004121002171,
614.462296651429));
#273016=CARTESIAN_POINT('Ctrl Pts',(-160.,-4.30813900827815,612.462296651428));
#273017=CARTESIAN_POINT('Ctrl Pts',(-160.339057893189,8.28413408366081,
610.462296651428));
#273018=CARTESIAN_POINT('Ctrl Pts',(-158.704075916301,20.7744157382975,
608.462296651428));
#273019=CARTESIAN_POINT('Ctrl Pts',(-157.069093939413,33.2646973929342,
606.462296651428));
#273020=CARTESIAN_POINT('Ctrl Pts',(-153.500330774912,45.3454354230633,
604.462296651428));
#273021=CARTESIAN_POINT('Ctrl Pts',(-149.931567610412,57.4261734531924,
602.462296651429));
#273022=CARTESIAN_POINT('Ctrl Pts',(-144.516898051455,68.7998999948413,
600.462296651428));
#273023=CARTESIAN_POINT('Ctrl Pts',(-139.102228492497,80.1736265364901,
598.462296651428));
#273024=CARTESIAN_POINT('Ctrl Pts',(-131.974979673883,90.5602826949691,
596.462296651428));
#273025=CARTESIAN_POINT('Ctrl Pts',(-124.847730855269,100.946938853448,
594.462296651428));
#273026=CARTESIAN_POINT('Ctrl Pts',(-116.183399296895,110.0907706828,592.462296651428));
#273027=CARTESIAN_POINT('Ctrl Pts',(-107.519067738521,119.234602512152,
590.462296651428));
#273028=CARTESIAN_POINT('Ctrl Pts',(-97.5309980386224,126.9104585261,588.462296651428));
#273029=CARTESIAN_POINT('Ctrl Pts',(-87.5429283387233,134.586314540048,
586.462296651428));
#273030=CARTESIAN_POINT('Ctrl Pts',(-76.4770599218137,140.605189688823,
584.462296651428));
#273031=CARTESIAN_POINT('Ctrl Pts',(-65.4111915049042,146.624064837599,
582.462296651428));
#273032=CARTESIAN_POINT('Ctrl Pts',(-53.5400027769199,150.837754439537,
580.462296651428));
#273033=CARTESIAN_POINT('Ctrl Pts',(-41.6688140489356,155.051444041475,
578.462296651428));
#273034=CARTESIAN_POINT('Ctrl Pts',(-29.2846130745764,157.356193074143,
576.462296651428));
#273035=CARTESIAN_POINT('Ctrl Pts',(-16.9004121002172,159.660942106811,
574.462296651428));
#273036=CARTESIAN_POINT('Ctrl Pts',(-4.30813900827816,160.,572.462296651428));
#273037=CARTESIAN_POINT('Ctrl Pts',(8.28413408366087,160.339057893189,570.462296651428));
#273038=CARTESIAN_POINT('Ctrl Pts',(20.7744157382975,158.704075916301,568.462296651428));
#273039=CARTESIAN_POINT('Ctrl Pts',(33.2646973929342,157.069093939413,566.462296651428));
#273040=CARTESIAN_POINT('Ctrl Pts',(45.3454354230633,153.500330774912,564.462296651428));
#273041=CARTESIAN_POINT('Ctrl Pts',(57.4261734531925,149.931567610412,562.462296651428));
#273042=CARTESIAN_POINT('Ctrl Pts',(68.7998999948413,144.516898051455,560.462296651428));
#273043=CARTESIAN_POINT('Ctrl Pts',(80.1736265364901,139.102228492498,558.462296651428));
#273044=CARTESIAN_POINT('Ctrl Pts',(90.560282694969,131.974979673883,556.462296651428));
#273045=CARTESIAN_POINT('Ctrl Pts',(100.946938853448,124.847730855269,554.462296651428));
#273046=CARTESIAN_POINT('Ctrl Pts',(110.0907706828,116.183399296895,552.462296651428));
#273047=CARTESIAN_POINT('Ctrl Pts',(119.234602512152,107.519067738521,550.462296651428));
#273048=CARTESIAN_POINT('Ctrl Pts',(126.9104585261,97.5309980386224,548.462296651428));
#273049=CARTESIAN_POINT('Ctrl Pts',(134.586314540048,87.5429283387233,546.462296651428));
#273050=CARTESIAN_POINT('Ctrl Pts',(140.605189688823,76.4770599218137,544.462296651428));
#273051=CARTESIAN_POINT('Ctrl Pts',(146.624064837599,65.4111915049042,542.462296651428));
#273052=CARTESIAN_POINT('Ctrl Pts',(150.837754439537,53.5400027769199,540.462296651428));
#273053=CARTESIAN_POINT('Ctrl Pts',(155.051444041475,41.6688140489356,538.462296651428));
#273054=CARTESIAN_POINT('Ctrl Pts',(157.356193074143,29.2846130745764,536.462296651428));
#273055=CARTESIAN_POINT('Ctrl Pts',(159.660942106811,16.9004121002172,534.462296651428));
#273056=CARTESIAN_POINT('Ctrl Pts',(160.,4.30813900827813,532.462296651428));
#273057=CARTESIAN_POINT('Origin',(-160.,3.64291929955129E-14,375.));
#273058=CARTESIAN_POINT('',(-160.,1.3142072080973E-15,375.000000000001));
#273059=CARTESIAN_POINT('',(-160.,-4.30813900827827,378.90811221526));
#273060=CARTESIAN_POINT('Ctrl Pts',(-160.,-7.32747196252603E-14,375.000000000001));
#273061=CARTESIAN_POINT('Ctrl Pts',(-160.,-0.0199151703950658,375.01805734453));
#273062=CARTESIAN_POINT('Ctrl Pts',(-160.,-0.0398304324242802,375.036114587998));
#273063=CARTESIAN_POINT('Ctrl Pts',(-160.,-0.0597455111851762,375.05417203359));
#273064=CARTESIAN_POINT('Ctrl Pts',(-160.,-1.47617978719699,376.338484547725));
#273065=CARTESIAN_POINT('Ctrl Pts',(-160.,-2.89215276710122,377.623305748502));
#273066=CARTESIAN_POINT('Ctrl Pts',(-160.,-4.30813900827827,378.90811221526));
#273067=CARTESIAN_POINT('',(-160.,4.30813900827767,377.537703348572));
#273068=CARTESIAN_POINT('',(-160.,-4.21537804662364E-13,375.));
#273069=CARTESIAN_POINT('Ctrl Pts',(-160.,-4.30813900827827,378.90811221526));
#273070=CARTESIAN_POINT('Ctrl Pts',(-160.,-1.43604209806711,378.451335906458));
#273071=CARTESIAN_POINT('Ctrl Pts',(-160.,1.43594781992473,377.99388646458));
#273072=CARTESIAN_POINT('Ctrl Pts',(-160.,4.30813900827767,377.537703348572));
#273073=CARTESIAN_POINT('Ctrl Pts',(-160.,-4.30813900827851,532.462296651429));
#273074=CARTESIAN_POINT('Ctrl Pts',(-160.339057893189,8.28413408366045,
530.462296651429));
#273075=CARTESIAN_POINT('Ctrl Pts',(-158.704075916301,20.7744157382972,
528.462296651429));
#273076=CARTESIAN_POINT('Ctrl Pts',(-157.069093939413,33.2646973929339,
526.462296651429));
#273077=CARTESIAN_POINT('Ctrl Pts',(-153.500330774912,45.345435423063,524.462296651428));
#273078=CARTESIAN_POINT('Ctrl Pts',(-149.931567610412,57.4261734531921,
522.462296651429));
#273079=CARTESIAN_POINT('Ctrl Pts',(-144.516898051455,68.7998999948409,
520.462296651428));
#273080=CARTESIAN_POINT('Ctrl Pts',(-139.102228492498,80.1736265364898,
518.462296651428));
#273081=CARTESIAN_POINT('Ctrl Pts',(-131.974979673884,90.5602826949688,
516.462296651428));
#273082=CARTESIAN_POINT('Ctrl Pts',(-124.84773085527,100.946938853448,514.462296651429));
#273083=CARTESIAN_POINT('Ctrl Pts',(-116.183399296896,110.0907706828,512.462296651428));
#273084=CARTESIAN_POINT('Ctrl Pts',(-107.519067738522,119.234602512151,
510.462296651429));
#273085=CARTESIAN_POINT('Ctrl Pts',(-97.5309980386227,126.9104585261,508.462296651429));
#273086=CARTESIAN_POINT('Ctrl Pts',(-87.5429283387237,134.586314540048,
506.462296651428));
#273087=CARTESIAN_POINT('Ctrl Pts',(-76.4770599218141,140.605189688823,
504.462296651429));
#273088=CARTESIAN_POINT('Ctrl Pts',(-65.4111915049045,146.624064837598,
502.462296651429));
#273089=CARTESIAN_POINT('Ctrl Pts',(-53.5400027769202,150.837754439537,
500.462296651429));
#273090=CARTESIAN_POINT('Ctrl Pts',(-41.668814048936,155.051444041475,498.462296651429));
#273091=CARTESIAN_POINT('Ctrl Pts',(-29.2846130745767,157.356193074143,
496.462296651429));
#273092=CARTESIAN_POINT('Ctrl Pts',(-16.9004121002175,159.660942106811,
494.462296651429));
#273093=CARTESIAN_POINT('Ctrl Pts',(-4.30813900827852,160.,492.462296651428));
#273094=CARTESIAN_POINT('Ctrl Pts',(8.28413408366043,160.339057893189,490.462296651429));
#273095=CARTESIAN_POINT('Ctrl Pts',(20.7744157382972,158.704075916301,488.462296651429));
#273096=CARTESIAN_POINT('Ctrl Pts',(33.2646973929339,157.069093939413,486.462296651429));
#273097=CARTESIAN_POINT('Ctrl Pts',(45.345435423063,153.500330774912,484.462296651429));
#273098=CARTESIAN_POINT('Ctrl Pts',(57.4261734531921,149.931567610412,482.462296651429));
#273099=CARTESIAN_POINT('Ctrl Pts',(68.7998999948409,144.516898051455,480.462296651428));
#273100=CARTESIAN_POINT('Ctrl Pts',(80.1736265364898,139.102228492498,478.462296651429));
#273101=CARTESIAN_POINT('Ctrl Pts',(90.5602826949688,131.974979673884,476.462296651428));
#273102=CARTESIAN_POINT('Ctrl Pts',(100.946938853448,124.84773085527,474.462296651429));
#273103=CARTESIAN_POINT('Ctrl Pts',(110.0907706828,116.183399296896,472.462296651429));
#273104=CARTESIAN_POINT('Ctrl Pts',(119.234602512151,107.519067738522,470.462296651429));
#273105=CARTESIAN_POINT('Ctrl Pts',(126.9104585261,97.5309980386227,468.462296651429));
#273106=CARTESIAN_POINT('Ctrl Pts',(134.586314540048,87.5429283387237,466.462296651429));
#273107=CARTESIAN_POINT('Ctrl Pts',(140.605189688823,76.4770599218141,464.462296651429));
#273108=CARTESIAN_POINT('Ctrl Pts',(146.624064837598,65.4111915049045,462.462296651429));
#273109=CARTESIAN_POINT('Ctrl Pts',(150.837754439537,53.5400027769202,460.462296651429));
#273110=CARTESIAN_POINT('Ctrl Pts',(155.051444041475,41.668814048936,458.462296651429));
#273111=CARTESIAN_POINT('Ctrl Pts',(157.356193074143,29.2846130745767,456.462296651429));
#273112=CARTESIAN_POINT('Ctrl Pts',(159.660942106811,16.9004121002175,454.462296651429));
#273113=CARTESIAN_POINT('Ctrl Pts',(160.,4.30813900827853,452.462296651429));
#273114=CARTESIAN_POINT('Ctrl Pts',(160.339057893189,-8.28413408366043,
450.462296651429));
#273115=CARTESIAN_POINT('Ctrl Pts',(158.704075916301,-20.7744157382971,
448.462296651429));
#273116=CARTESIAN_POINT('Ctrl Pts',(157.069093939413,-33.2646973929339,
446.462296651429));
#273117=CARTESIAN_POINT('Ctrl Pts',(153.500330774912,-45.345435423063,444.462296651429));
#273118=CARTESIAN_POINT('Ctrl Pts',(149.931567610412,-57.4261734531921,
442.462296651429));
#273119=CARTESIAN_POINT('Ctrl Pts',(144.516898051455,-68.7998999948409,
440.462296651429));
#273120=CARTESIAN_POINT('Ctrl Pts',(139.102228492498,-80.1736265364898,
438.462296651429));
#273121=CARTESIAN_POINT('Ctrl Pts',(131.974979673884,-90.5602826949688,
436.462296651429));
#273122=CARTESIAN_POINT('Ctrl Pts',(124.84773085527,-100.946938853448,434.462296651429));
#273123=CARTESIAN_POINT('Ctrl Pts',(116.183399296896,-110.0907706828,432.462296651429));
#273124=CARTESIAN_POINT('Ctrl Pts',(107.519067738522,-119.234602512151,
430.462296651429));
#273125=CARTESIAN_POINT('Ctrl Pts',(97.5309980386227,-126.9104585261,428.462296651429));
#273126=CARTESIAN_POINT('Ctrl Pts',(87.5429283387236,-134.586314540048,
426.462296651429));
#273127=CARTESIAN_POINT('Ctrl Pts',(76.4770599218141,-140.605189688823,
424.462296651429));
#273128=CARTESIAN_POINT('Ctrl Pts',(65.4111915049046,-146.624064837598,
422.462296651429));
#273129=CARTESIAN_POINT('Ctrl Pts',(53.5400027769202,-150.837754439537,
420.462296651429));
#273130=CARTESIAN_POINT('Ctrl Pts',(41.6688140489359,-155.051444041475,
418.462296651429));
#273131=CARTESIAN_POINT('Ctrl Pts',(29.2846130745768,-157.356193074143,
416.462296651429));
#273132=CARTESIAN_POINT('Ctrl Pts',(16.9004121002176,-159.660942106811,
414.462296651429));
#273133=CARTESIAN_POINT('Ctrl Pts',(4.30813900827854,-160.,412.462296651429));
#273134=CARTESIAN_POINT('Ctrl Pts',(-8.28413408366049,-160.339057893189,
410.462296651429));
#273135=CARTESIAN_POINT('Ctrl Pts',(-20.7744157382971,-158.704075916301,
408.462296651429));
#273136=CARTESIAN_POINT('Ctrl Pts',(-33.2646973929338,-157.069093939413,
406.462296651429));
#273137=CARTESIAN_POINT('Ctrl Pts',(-45.345435423063,-153.500330774912,
404.462296651429));
#273138=CARTESIAN_POINT('Ctrl Pts',(-57.4261734531921,-149.931567610412,
402.462296651429));
#273139=CARTESIAN_POINT('Ctrl Pts',(-68.7998999948409,-144.516898051455,
400.462296651429));
#273140=CARTESIAN_POINT('Ctrl Pts',(-80.1736265364897,-139.102228492498,
398.462296651429));
#273141=CARTESIAN_POINT('Ctrl Pts',(-90.5602826949688,-131.974979673884,
396.462296651429));
#273142=CARTESIAN_POINT('Ctrl Pts',(-100.946938853448,-124.84773085527,
394.462296651429));
#273143=CARTESIAN_POINT('Ctrl Pts',(-110.0907706828,-116.183399296896,392.462296651429));
#273144=CARTESIAN_POINT('Ctrl Pts',(-119.234602512151,-107.519067738522,
390.462296651429));
#273145=CARTESIAN_POINT('Ctrl Pts',(-126.9104585261,-97.5309980386227,388.462296651429));
#273146=CARTESIAN_POINT('Ctrl Pts',(-134.586314540048,-87.5429283387236,
386.462296651429));
#273147=CARTESIAN_POINT('Ctrl Pts',(-140.605189688823,-76.4770599218141,
384.462296651429));
#273148=CARTESIAN_POINT('Ctrl Pts',(-146.624064837598,-65.4111915049046,
382.462296651429));
#273149=CARTESIAN_POINT('Ctrl Pts',(-150.837754439537,-53.5400027769203,
380.462296651429));
#273150=CARTESIAN_POINT('Ctrl Pts',(-155.051444041475,-41.668814048936,
378.462296651429));
#273151=CARTESIAN_POINT('Ctrl Pts',(-157.356193074143,-29.2846130745768,
376.462296651429));
#273152=CARTESIAN_POINT('Ctrl Pts',(-159.660942106811,-16.9004121002176,
374.462296651429));
#273153=CARTESIAN_POINT('Ctrl Pts',(-160.,-4.30813900827851,372.462296651429));
#273154=CARTESIAN_POINT('Ctrl Pts',(-160.,4.30813900827767,537.537703348572));
#273155=CARTESIAN_POINT('Ctrl Pts',(-159.660942106811,16.9004121002166,
535.537703348572));
#273156=CARTESIAN_POINT('Ctrl Pts',(-157.356193074143,29.2846130745759,
533.537703348572));
#273157=CARTESIAN_POINT('Ctrl Pts',(-155.051444041476,41.6688140489352,
531.537703348572));
#273158=CARTESIAN_POINT('Ctrl Pts',(-150.837754439537,53.5400027769194,
529.537703348572));
#273159=CARTESIAN_POINT('Ctrl Pts',(-146.624064837599,65.4111915049037,
527.537703348572));
#273160=CARTESIAN_POINT('Ctrl Pts',(-140.605189688823,76.4770599218133,
525.537703348572));
#273161=CARTESIAN_POINT('Ctrl Pts',(-134.586314540048,87.542928338723,523.537703348572));
#273162=CARTESIAN_POINT('Ctrl Pts',(-126.9104585261,97.530998038622,521.537703348572));
#273163=CARTESIAN_POINT('Ctrl Pts',(-119.234602512152,107.519067738521,
519.537703348572));
#273164=CARTESIAN_POINT('Ctrl Pts',(-110.0907706828,116.183399296895,517.537703348572));
#273165=CARTESIAN_POINT('Ctrl Pts',(-100.946938853448,124.847730855269,
515.537703348572));
#273166=CARTESIAN_POINT('Ctrl Pts',(-90.5602826949695,131.974979673883,
513.537703348572));
#273167=CARTESIAN_POINT('Ctrl Pts',(-80.1736265364906,139.102228492497,
511.537703348572));
#273168=CARTESIAN_POINT('Ctrl Pts',(-68.7998999948417,144.516898051454,
509.537703348572));
#273169=CARTESIAN_POINT('Ctrl Pts',(-57.4261734531929,149.931567610411,
507.537703348572));
#273170=CARTESIAN_POINT('Ctrl Pts',(-45.3454354230638,153.500330774912,
505.537703348572));
#273171=CARTESIAN_POINT('Ctrl Pts',(-33.2646973929347,157.069093939413,
503.537703348572));
#273172=CARTESIAN_POINT('Ctrl Pts',(-20.774415738298,158.704075916301,501.537703348572));
#273173=CARTESIAN_POINT('Ctrl Pts',(-8.28413408366129,160.339057893189,
499.537703348572));
#273174=CARTESIAN_POINT('Ctrl Pts',(4.30813900827766,160.,497.537703348572));
#273175=CARTESIAN_POINT('Ctrl Pts',(16.9004121002166,159.660942106811,495.537703348572));
#273176=CARTESIAN_POINT('Ctrl Pts',(29.2846130745759,157.356193074143,493.537703348572));
#273177=CARTESIAN_POINT('Ctrl Pts',(41.6688140489352,155.051444041476,491.537703348572));
#273178=CARTESIAN_POINT('Ctrl Pts',(53.5400027769194,150.837754439537,489.537703348572));
#273179=CARTESIAN_POINT('Ctrl Pts',(65.4111915049037,146.624064837599,487.537703348572));
#273180=CARTESIAN_POINT('Ctrl Pts',(76.4770599218133,140.605189688823,485.537703348572));
#273181=CARTESIAN_POINT('Ctrl Pts',(87.542928338723,134.586314540048,483.537703348572));
#273182=CARTESIAN_POINT('Ctrl Pts',(97.530998038622,126.9104585261,481.537703348572));
#273183=CARTESIAN_POINT('Ctrl Pts',(107.519067738521,119.234602512152,479.537703348572));
#273184=CARTESIAN_POINT('Ctrl Pts',(116.183399296895,110.0907706828,477.537703348572));
#273185=CARTESIAN_POINT('Ctrl Pts',(124.847730855269,100.946938853448,475.537703348572));
#273186=CARTESIAN_POINT('Ctrl Pts',(131.974979673883,90.5602826949695,473.537703348572));
#273187=CARTESIAN_POINT('Ctrl Pts',(139.102228492497,80.1736265364906,471.537703348572));
#273188=CARTESIAN_POINT('Ctrl Pts',(144.516898051454,68.7998999948417,469.537703348572));
#273189=CARTESIAN_POINT('Ctrl Pts',(149.931567610411,57.4261734531929,467.537703348572));
#273190=CARTESIAN_POINT('Ctrl Pts',(153.500330774912,45.3454354230638,465.537703348572));
#273191=CARTESIAN_POINT('Ctrl Pts',(157.069093939413,33.2646973929347,463.537703348572));
#273192=CARTESIAN_POINT('Ctrl Pts',(158.704075916301,20.774415738298,461.537703348572));
#273193=CARTESIAN_POINT('Ctrl Pts',(160.339057893189,8.28413408366131,459.537703348572));
#273194=CARTESIAN_POINT('Ctrl Pts',(160.,-4.30813900827765,457.537703348572));
#273195=CARTESIAN_POINT('Ctrl Pts',(159.660942106811,-16.9004121002166,
455.537703348572));
#273196=CARTESIAN_POINT('Ctrl Pts',(157.356193074143,-29.2846130745759,
453.537703348572));
#273197=CARTESIAN_POINT('Ctrl Pts',(155.051444041476,-41.6688140489352,
451.537703348572));
#273198=CARTESIAN_POINT('Ctrl Pts',(150.837754439537,-53.5400027769194,
449.537703348572));
#273199=CARTESIAN_POINT('Ctrl Pts',(146.624064837599,-65.4111915049036,
447.537703348572));
#273200=CARTESIAN_POINT('Ctrl Pts',(140.605189688823,-76.4770599218133,
445.537703348572));
#273201=CARTESIAN_POINT('Ctrl Pts',(134.586314540048,-87.5429283387229,
443.537703348572));
#273202=CARTESIAN_POINT('Ctrl Pts',(126.9104585261,-97.530998038622,441.537703348572));
#273203=CARTESIAN_POINT('Ctrl Pts',(119.234602512152,-107.519067738521,
439.537703348572));
#273204=CARTESIAN_POINT('Ctrl Pts',(110.0907706828,-116.183399296895,437.537703348572));
#273205=CARTESIAN_POINT('Ctrl Pts',(100.946938853448,-124.847730855269,
435.537703348572));
#273206=CARTESIAN_POINT('Ctrl Pts',(90.5602826949695,-131.974979673883,
433.537703348572));
#273207=CARTESIAN_POINT('Ctrl Pts',(80.1736265364905,-139.102228492497,
431.537703348572));
#273208=CARTESIAN_POINT('Ctrl Pts',(68.7998999948417,-144.516898051454,
429.537703348572));
#273209=CARTESIAN_POINT('Ctrl Pts',(57.426173453193,-149.931567610411,427.537703348572));
#273210=CARTESIAN_POINT('Ctrl Pts',(45.3454354230638,-153.500330774912,
425.537703348572));
#273211=CARTESIAN_POINT('Ctrl Pts',(33.2646973929347,-157.069093939413,
423.537703348572));
#273212=CARTESIAN_POINT('Ctrl Pts',(20.774415738298,-158.704075916301,421.537703348572));
#273213=CARTESIAN_POINT('Ctrl Pts',(8.28413408366139,-160.339057893189,
419.537703348572));
#273214=CARTESIAN_POINT('Ctrl Pts',(-4.30813900827764,-160.,417.537703348572));
#273215=CARTESIAN_POINT('Ctrl Pts',(-16.9004121002167,-159.660942106811,
415.537703348572));
#273216=CARTESIAN_POINT('Ctrl Pts',(-29.2846130745759,-157.356193074143,
413.537703348572));
#273217=CARTESIAN_POINT('Ctrl Pts',(-41.6688140489351,-155.051444041476,
411.537703348572));
#273218=CARTESIAN_POINT('Ctrl Pts',(-53.5400027769194,-150.837754439537,
409.537703348572));
#273219=CARTESIAN_POINT('Ctrl Pts',(-65.4111915049037,-146.624064837599,
407.537703348572));
#273220=CARTESIAN_POINT('Ctrl Pts',(-76.4770599218133,-140.605189688823,
405.537703348572));
#273221=CARTESIAN_POINT('Ctrl Pts',(-87.5429283387229,-134.586314540048,
403.537703348572));
#273222=CARTESIAN_POINT('Ctrl Pts',(-97.530998038622,-126.9104585261,401.537703348572));
#273223=CARTESIAN_POINT('Ctrl Pts',(-107.519067738521,-119.234602512152,
399.537703348572));
#273224=CARTESIAN_POINT('Ctrl Pts',(-116.183399296895,-110.0907706828,397.537703348572));
#273225=CARTESIAN_POINT('Ctrl Pts',(-124.847730855269,-100.946938853448,
395.537703348572));
#273226=CARTESIAN_POINT('Ctrl Pts',(-131.974979673883,-90.5602826949695,
393.537703348572));
#273227=CARTESIAN_POINT('Ctrl Pts',(-139.102228492497,-80.1736265364905,
391.537703348572));
#273228=CARTESIAN_POINT('Ctrl Pts',(-144.516898051454,-68.7998999948417,
389.537703348572));
#273229=CARTESIAN_POINT('Ctrl Pts',(-149.931567610411,-57.426173453193,
387.537703348572));
#273230=CARTESIAN_POINT('Ctrl Pts',(-153.500330774912,-45.3454354230638,
385.537703348572));
#273231=CARTESIAN_POINT('Ctrl Pts',(-157.069093939413,-33.2646973929347,
383.537703348572));
#273232=CARTESIAN_POINT('Ctrl Pts',(-158.704075916301,-20.774415738298,
381.537703348572));
#273233=CARTESIAN_POINT('Ctrl Pts',(-160.339057893189,-8.2841340836614,
379.537703348572));
#273234=CARTESIAN_POINT('Ctrl Pts',(-160.,4.30813900827767,377.537703348572));
#273235=CARTESIAN_POINT('Origin',(4.03737035481559,0.209103844003473,379.537622607612));
#273236=CARTESIAN_POINT('Ctrl Pts',(-160.,4.30813900827767,537.537703348572));
#273237=CARTESIAN_POINT('Ctrl Pts',(-159.660942106811,16.9004121002166,
535.537703348572));
#273238=CARTESIAN_POINT('Ctrl Pts',(-157.356193074143,29.2846130745759,
533.537703348572));
#273239=CARTESIAN_POINT('Ctrl Pts',(-155.051444041476,41.6688140489352,
531.537703348572));
#273240=CARTESIAN_POINT('Ctrl Pts',(-150.837754439537,53.5400027769194,
529.537703348572));
#273241=CARTESIAN_POINT('Ctrl Pts',(-146.624064837599,65.4111915049037,
527.537703348572));
#273242=CARTESIAN_POINT('Ctrl Pts',(-140.605189688823,76.4770599218133,
525.537703348572));
#273243=CARTESIAN_POINT('Ctrl Pts',(-134.586314540048,87.542928338723,523.537703348572));
#273244=CARTESIAN_POINT('Ctrl Pts',(-126.9104585261,97.530998038622,521.537703348572));
#273245=CARTESIAN_POINT('Ctrl Pts',(-119.234602512152,107.519067738521,
519.537703348572));
#273246=CARTESIAN_POINT('Ctrl Pts',(-110.0907706828,116.183399296895,517.537703348572));
#273247=CARTESIAN_POINT('Ctrl Pts',(-100.946938853448,124.847730855269,
515.537703348572));
#273248=CARTESIAN_POINT('Ctrl Pts',(-90.5602826949695,131.974979673883,
513.537703348572));
#273249=CARTESIAN_POINT('Ctrl Pts',(-80.1736265364906,139.102228492497,
511.537703348572));
#273250=CARTESIAN_POINT('Ctrl Pts',(-68.7998999948417,144.516898051454,
509.537703348572));
#273251=CARTESIAN_POINT('Ctrl Pts',(-57.4261734531929,149.931567610411,
507.537703348572));
#273252=CARTESIAN_POINT('Ctrl Pts',(-45.3454354230638,153.500330774912,
505.537703348572));
#273253=CARTESIAN_POINT('Ctrl Pts',(-33.2646973929347,157.069093939413,
503.537703348572));
#273254=CARTESIAN_POINT('Ctrl Pts',(-20.774415738298,158.704075916301,501.537703348572));
#273255=CARTESIAN_POINT('Ctrl Pts',(-8.28413408366129,160.339057893189,
499.537703348572));
#273256=CARTESIAN_POINT('Ctrl Pts',(4.30813900827766,160.,497.537703348572));
#273257=CARTESIAN_POINT('Ctrl Pts',(16.9004121002166,159.660942106811,495.537703348572));
#273258=CARTESIAN_POINT('Ctrl Pts',(29.2846130745759,157.356193074143,493.537703348572));
#273259=CARTESIAN_POINT('Ctrl Pts',(41.6688140489352,155.051444041476,491.537703348572));
#273260=CARTESIAN_POINT('Ctrl Pts',(53.5400027769194,150.837754439537,489.537703348572));
#273261=CARTESIAN_POINT('Ctrl Pts',(65.4111915049037,146.624064837599,487.537703348572));
#273262=CARTESIAN_POINT('Ctrl Pts',(76.4770599218133,140.605189688823,485.537703348572));
#273263=CARTESIAN_POINT('Ctrl Pts',(87.542928338723,134.586314540048,483.537703348572));
#273264=CARTESIAN_POINT('Ctrl Pts',(97.530998038622,126.9104585261,481.537703348572));
#273265=CARTESIAN_POINT('Ctrl Pts',(107.519067738521,119.234602512152,479.537703348572));
#273266=CARTESIAN_POINT('Ctrl Pts',(116.183399296895,110.0907706828,477.537703348572));
#273267=CARTESIAN_POINT('Ctrl Pts',(124.847730855269,100.946938853448,475.537703348572));
#273268=CARTESIAN_POINT('Ctrl Pts',(131.974979673883,90.5602826949695,473.537703348572));
#273269=CARTESIAN_POINT('Ctrl Pts',(139.102228492497,80.1736265364906,471.537703348572));
#273270=CARTESIAN_POINT('Ctrl Pts',(144.516898051454,68.7998999948417,469.537703348572));
#273271=CARTESIAN_POINT('Ctrl Pts',(149.931567610411,57.4261734531929,467.537703348572));
#273272=CARTESIAN_POINT('Ctrl Pts',(153.500330774912,45.3454354230638,465.537703348572));
#273273=CARTESIAN_POINT('Ctrl Pts',(157.069093939413,33.2646973929347,463.537703348572));
#273274=CARTESIAN_POINT('Ctrl Pts',(158.704075916301,20.774415738298,461.537703348572));
#273275=CARTESIAN_POINT('Ctrl Pts',(160.339057893189,8.28413408366131,459.537703348572));
#273276=CARTESIAN_POINT('Ctrl Pts',(160.,-4.30813900827765,457.537703348572));
#273277=CARTESIAN_POINT('Ctrl Pts',(159.660942106811,-16.9004121002166,
455.537703348572));
#273278=CARTESIAN_POINT('Ctrl Pts',(157.356193074143,-29.2846130745759,
453.537703348572));
#273279=CARTESIAN_POINT('Ctrl Pts',(155.051444041476,-41.6688140489352,
451.537703348572));
#273280=CARTESIAN_POINT('Ctrl Pts',(150.837754439537,-53.5400027769194,
449.537703348572));
#273281=CARTESIAN_POINT('Ctrl Pts',(146.624064837599,-65.4111915049036,
447.537703348572));
#273282=CARTESIAN_POINT('Ctrl Pts',(140.605189688823,-76.4770599218133,
445.537703348572));
#273283=CARTESIAN_POINT('Ctrl Pts',(134.586314540048,-87.5429283387229,
443.537703348572));
#273284=CARTESIAN_POINT('Ctrl Pts',(126.9104585261,-97.530998038622,441.537703348572));
#273285=CARTESIAN_POINT('Ctrl Pts',(119.234602512152,-107.519067738521,
439.537703348572));
#273286=CARTESIAN_POINT('Ctrl Pts',(110.0907706828,-116.183399296895,437.537703348572));
#273287=CARTESIAN_POINT('Ctrl Pts',(100.946938853448,-124.847730855269,
435.537703348572));
#273288=CARTESIAN_POINT('Ctrl Pts',(90.5602826949695,-131.974979673883,
433.537703348572));
#273289=CARTESIAN_POINT('Ctrl Pts',(80.1736265364905,-139.102228492497,
431.537703348572));
#273290=CARTESIAN_POINT('Ctrl Pts',(68.7998999948417,-144.516898051454,
429.537703348572));
#273291=CARTESIAN_POINT('Ctrl Pts',(57.426173453193,-149.931567610411,427.537703348572));
#273292=CARTESIAN_POINT('Ctrl Pts',(45.3454354230638,-153.500330774912,
425.537703348572));
#273293=CARTESIAN_POINT('Ctrl Pts',(33.2646973929347,-157.069093939413,
423.537703348572));
#273294=CARTESIAN_POINT('Ctrl Pts',(20.774415738298,-158.704075916301,421.537703348572));
#273295=CARTESIAN_POINT('Ctrl Pts',(8.28413408366139,-160.339057893189,
419.537703348572));
#273296=CARTESIAN_POINT('Ctrl Pts',(-4.30813900827764,-160.,417.537703348572));
#273297=CARTESIAN_POINT('Ctrl Pts',(-16.9004121002167,-159.660942106811,
415.537703348572));
#273298=CARTESIAN_POINT('Ctrl Pts',(-29.2846130745759,-157.356193074143,
413.537703348572));
#273299=CARTESIAN_POINT('Ctrl Pts',(-41.6688140489351,-155.051444041476,
411.537703348572));
#273300=CARTESIAN_POINT('Ctrl Pts',(-53.5400027769194,-150.837754439537,
409.537703348572));
#273301=CARTESIAN_POINT('Ctrl Pts',(-65.4111915049037,-146.624064837599,
407.537703348572));
#273302=CARTESIAN_POINT('Ctrl Pts',(-76.4770599218133,-140.605189688823,
405.537703348572));
#273303=CARTESIAN_POINT('Ctrl Pts',(-87.5429283387229,-134.586314540048,
403.537703348572));
#273304=CARTESIAN_POINT('Ctrl Pts',(-97.530998038622,-126.9104585261,401.537703348572));
#273305=CARTESIAN_POINT('Ctrl Pts',(-107.519067738521,-119.234602512152,
399.537703348572));
#273306=CARTESIAN_POINT('Ctrl Pts',(-116.183399296895,-110.0907706828,397.537703348572));
#273307=CARTESIAN_POINT('Ctrl Pts',(-124.847730855269,-100.946938853448,
395.537703348572));
#273308=CARTESIAN_POINT('Ctrl Pts',(-131.974979673883,-90.5602826949695,
393.537703348572));
#273309=CARTESIAN_POINT('Ctrl Pts',(-139.102228492497,-80.1736265364905,
391.537703348572));
#273310=CARTESIAN_POINT('Ctrl Pts',(-144.516898051454,-68.7998999948417,
389.537703348572));
#273311=CARTESIAN_POINT('Ctrl Pts',(-149.931567610411,-57.426173453193,
387.537703348572));
#273312=CARTESIAN_POINT('Ctrl Pts',(-153.500330774912,-45.3454354230638,
385.537703348572));
#273313=CARTESIAN_POINT('Ctrl Pts',(-157.069093939413,-33.2646973929347,
383.537703348572));
#273314=CARTESIAN_POINT('Ctrl Pts',(-158.704075916301,-20.774415738298,
381.537703348572));
#273315=CARTESIAN_POINT('Ctrl Pts',(-160.339057893189,-8.2841340836614,
379.537703348572));
#273316=CARTESIAN_POINT('Ctrl Pts',(-160.,4.30813900827767,377.537703348572));
#273317=CARTESIAN_POINT('Ctrl Pts',(-130.,4.30813900827773,537.537703348572));
#273318=CARTESIAN_POINT('Ctrl Pts',(-129.660942106811,14.5393608954781,
535.537703348572));
#273319=CARTESIAN_POINT('Ctrl Pts',(-127.725542856289,24.591579123369,533.537703348572));
#273320=CARTESIAN_POINT('Ctrl Pts',(-125.790143605767,34.6437973512599,
531.537703348572));
#273321=CARTESIAN_POINT('Ctrl Pts',(-122.306058950683,44.269492945671,529.537703348572));
#273322=CARTESIAN_POINT('Ctrl Pts',(-118.821974295598,53.8951885400822,
527.537703348572));
#273323=CARTESIAN_POINT('Ctrl Pts',(-113.874993963172,62.8573449296269,
525.537703348572));
#273324=CARTESIAN_POINT('Ctrl Pts',(-108.928013630747,71.8195013191717,
523.537703348572));
#273325=CARTESIAN_POINT('Ctrl Pts',(-102.639948694852,79.8974404698478,
521.537703348572));
#273326=CARTESIAN_POINT('Ctrl Pts',(-96.3518837589562,87.9753796205239,
519.537703348572));
#273327=CARTESIAN_POINT('Ctrl Pts',(-88.8775672472037,94.9701958612987,
517.537703348572));
#273328=CARTESIAN_POINT('Ctrl Pts',(-81.4032507354512,101.965012102073,
515.537703348572));
#273329=CARTESIAN_POINT('Ctrl Pts',(-72.9267251261952,107.704469842635,
513.537703348572));
#273330=CARTESIAN_POINT('Ctrl Pts',(-64.4501995169392,113.443927583196,
511.537703348572));
#273331=CARTESIAN_POINT('Ctrl Pts',(-55.1801850026552,117.786702325803,
509.537703348572));
#273332=CARTESIAN_POINT('Ctrl Pts',(-45.9101704883713,122.12947706841,507.537703348572));
#273333=CARTESIAN_POINT('Ctrl Pts',(-36.0749255918153,124.968635286057,
505.537703348572));
#273334=CARTESIAN_POINT('Ctrl Pts',(-26.2396806952593,127.807793503704,
503.537703348572));
#273335=CARTESIAN_POINT('Ctrl Pts',(-16.081381787091,129.073425698447,501.537703348572));
#273336=CARTESIAN_POINT('Ctrl Pts',(-5.92308287892268,130.339057893189,
499.537703348572));
#273337=CARTESIAN_POINT('Ctrl Pts',(4.30813900827772,130.,497.537703348572));
#273338=CARTESIAN_POINT('Ctrl Pts',(14.5393608954781,129.660942106811,495.537703348572));
#273339=CARTESIAN_POINT('Ctrl Pts',(24.591579123369,127.725542856289,493.537703348572));
#273340=CARTESIAN_POINT('Ctrl Pts',(34.6437973512599,125.790143605767,491.537703348572));
#273341=CARTESIAN_POINT('Ctrl Pts',(44.269492945671,122.306058950683,489.537703348572));
#273342=CARTESIAN_POINT('Ctrl Pts',(53.8951885400822,118.821974295598,487.537703348572));
#273343=CARTESIAN_POINT('Ctrl Pts',(62.8573449296269,113.874993963172,485.537703348572));
#273344=CARTESIAN_POINT('Ctrl Pts',(71.8195013191717,108.928013630747,483.537703348572));
#273345=CARTESIAN_POINT('Ctrl Pts',(79.8974404698478,102.639948694852,481.537703348572));
#273346=CARTESIAN_POINT('Ctrl Pts',(87.9753796205239,96.3518837589562,479.537703348572));
#273347=CARTESIAN_POINT('Ctrl Pts',(94.9701958612986,88.8775672472037,477.537703348572));
#273348=CARTESIAN_POINT('Ctrl Pts',(101.965012102073,81.4032507354512,475.537703348572));
#273349=CARTESIAN_POINT('Ctrl Pts',(107.704469842635,72.9267251261952,473.537703348572));
#273350=CARTESIAN_POINT('Ctrl Pts',(113.443927583196,64.4501995169392,471.537703348572));
#273351=CARTESIAN_POINT('Ctrl Pts',(117.786702325803,55.1801850026552,469.537703348572));
#273352=CARTESIAN_POINT('Ctrl Pts',(122.12947706841,45.9101704883713,467.537703348572));
#273353=CARTESIAN_POINT('Ctrl Pts',(124.968635286057,36.0749255918153,465.537703348572));
#273354=CARTESIAN_POINT('Ctrl Pts',(127.807793503704,26.2396806952593,463.537703348572));
#273355=CARTESIAN_POINT('Ctrl Pts',(129.073425698447,16.081381787091,461.537703348572));
#273356=CARTESIAN_POINT('Ctrl Pts',(130.339057893189,5.92308287892268,459.537703348572));
#273357=CARTESIAN_POINT('Ctrl Pts',(130.,-4.30813900827772,457.537703348572));
#273358=CARTESIAN_POINT('Ctrl Pts',(129.660942106811,-14.5393608954781,
455.537703348572));
#273359=CARTESIAN_POINT('Ctrl Pts',(127.725542856289,-24.591579123369,453.537703348572));
#273360=CARTESIAN_POINT('Ctrl Pts',(125.790143605767,-34.6437973512599,
451.537703348572));
#273361=CARTESIAN_POINT('Ctrl Pts',(122.306058950683,-44.269492945671,449.537703348572));
#273362=CARTESIAN_POINT('Ctrl Pts',(118.821974295598,-53.8951885400822,
447.537703348572));
#273363=CARTESIAN_POINT('Ctrl Pts',(113.874993963172,-62.8573449296269,
445.537703348572));
#273364=CARTESIAN_POINT('Ctrl Pts',(108.928013630747,-71.8195013191717,
443.537703348572));
#273365=CARTESIAN_POINT('Ctrl Pts',(102.639948694852,-79.8974404698478,
441.537703348572));
#273366=CARTESIAN_POINT('Ctrl Pts',(96.3518837589563,-87.9753796205239,
439.537703348572));
#273367=CARTESIAN_POINT('Ctrl Pts',(88.8775672472037,-94.9701958612986,
437.537703348572));
#273368=CARTESIAN_POINT('Ctrl Pts',(81.4032507354513,-101.965012102073,
435.537703348572));
#273369=CARTESIAN_POINT('Ctrl Pts',(72.9267251261952,-107.704469842635,
433.537703348572));
#273370=CARTESIAN_POINT('Ctrl Pts',(64.4501995169392,-113.443927583196,
431.537703348572));
#273371=CARTESIAN_POINT('Ctrl Pts',(55.1801850026552,-117.786702325803,
429.537703348572));
#273372=CARTESIAN_POINT('Ctrl Pts',(45.9101704883713,-122.12947706841,427.537703348572));
#273373=CARTESIAN_POINT('Ctrl Pts',(36.0749255918153,-124.968635286057,
425.537703348572));
#273374=CARTESIAN_POINT('Ctrl Pts',(26.2396806952593,-127.807793503704,
423.537703348572));
#273375=CARTESIAN_POINT('Ctrl Pts',(16.081381787091,-129.073425698447,421.537703348572));
#273376=CARTESIAN_POINT('Ctrl Pts',(5.92308287892275,-130.339057893189,
419.537703348572));
#273377=CARTESIAN_POINT('Ctrl Pts',(-4.30813900827771,-130.,417.537703348572));
#273378=CARTESIAN_POINT('Ctrl Pts',(-14.5393608954782,-129.660942106811,
415.537703348572));
#273379=CARTESIAN_POINT('Ctrl Pts',(-24.591579123369,-127.725542856289,
413.537703348572));
#273380=CARTESIAN_POINT('Ctrl Pts',(-34.6437973512598,-125.790143605767,
411.537703348572));
#273381=CARTESIAN_POINT('Ctrl Pts',(-44.269492945671,-122.306058950683,
409.537703348572));
#273382=CARTESIAN_POINT('Ctrl Pts',(-53.8951885400822,-118.821974295598,
407.537703348572));
#273383=CARTESIAN_POINT('Ctrl Pts',(-62.8573449296269,-113.874993963172,
405.537703348572));
#273384=CARTESIAN_POINT('Ctrl Pts',(-71.8195013191717,-108.928013630747,
403.537703348572));
#273385=CARTESIAN_POINT('Ctrl Pts',(-79.8974404698478,-102.639948694852,
401.537703348572));
#273386=CARTESIAN_POINT('Ctrl Pts',(-87.975379620524,-96.3518837589562,
399.537703348572));
#273387=CARTESIAN_POINT('Ctrl Pts',(-94.9701958612986,-88.8775672472037,
397.537703348572));
#273388=CARTESIAN_POINT('Ctrl Pts',(-101.965012102073,-81.4032507354513,
395.537703348572));
#273389=CARTESIAN_POINT('Ctrl Pts',(-107.704469842635,-72.9267251261952,
393.537703348572));
#273390=CARTESIAN_POINT('Ctrl Pts',(-113.443927583196,-64.4501995169392,
391.537703348572));
#273391=CARTESIAN_POINT('Ctrl Pts',(-117.786702325803,-55.1801850026553,
389.537703348572));
#273392=CARTESIAN_POINT('Ctrl Pts',(-122.12947706841,-45.9101704883713,
387.537703348572));
#273393=CARTESIAN_POINT('Ctrl Pts',(-124.968635286057,-36.0749255918153,
385.537703348572));
#273394=CARTESIAN_POINT('Ctrl Pts',(-127.807793503704,-26.2396806952593,
383.537703348572));
#273395=CARTESIAN_POINT('Ctrl Pts',(-129.073425698447,-16.081381787091,
381.537703348572));
#273396=CARTESIAN_POINT('Ctrl Pts',(-130.339057893189,-5.92308287892275,
379.537703348572));
#273397=CARTESIAN_POINT('Ctrl Pts',(-130.,4.30813900827773,377.537703348572));
#273398=CARTESIAN_POINT('Origin',(-160.,-1.08084483543429E-12,695.));
#273399=CARTESIAN_POINT('',(-160.,4.68174708145216E-13,695.000000000001));
#273400=CARTESIAN_POINT('',(-160.,4.3081390082779,691.09188778474));
#273401=CARTESIAN_POINT('Ctrl Pts',(-160.,4.68514116391816E-13,695.000000000001));
#273402=CARTESIAN_POINT('Ctrl Pts',(-160.,0.0199151703862232,694.981942655461));
#273403=CARTESIAN_POINT('Ctrl Pts',(-160.,0.0398304323877712,694.963885411962));
#273404=CARTESIAN_POINT('Ctrl Pts',(-160.,0.0597455111577332,694.945827966381));
#273405=CARTESIAN_POINT('Ctrl Pts',(-160.,1.47617978782475,693.661515452968));
#273406=CARTESIAN_POINT('Ctrl Pts',(-160.,2.89215276710192,692.376694251499));
#273407=CARTESIAN_POINT('Ctrl Pts',(-160.,4.30813900827806,691.091887784741));
#273408=CARTESIAN_POINT('',(-160.,-4.30813900827851,692.462296651429));
#273409=CARTESIAN_POINT('',(-160.,-4.21537804662364E-13,695.));
#273410=CARTESIAN_POINT('Ctrl Pts',(-160.,4.3081390082779,691.09188778474));
#273411=CARTESIAN_POINT('Ctrl Pts',(-160.,1.43604209808296,691.548664093541));
#273412=CARTESIAN_POINT('Ctrl Pts',(-160.,-1.43594781991723,692.006113535419));
#273413=CARTESIAN_POINT('Ctrl Pts',(-160.,-4.30813900827851,692.462296651429));
#273414=CARTESIAN_POINT('Ctrl Pts',(-130.,-4.30813900827845,692.462296651428));
#273415=CARTESIAN_POINT('Ctrl Pts',(-130.339057893189,5.92308287892195,
690.462296651428));
#273416=CARTESIAN_POINT('Ctrl Pts',(-129.073425698447,16.0813817870903,
688.462296651428));
#273417=CARTESIAN_POINT('Ctrl Pts',(-127.807793503705,26.2396806952586,
686.462296651429));
#273418=CARTESIAN_POINT('Ctrl Pts',(-124.968635286058,36.0749255918146,
684.462296651428));
#273419=CARTESIAN_POINT('Ctrl Pts',(-122.129477068411,45.9101704883706,
682.462296651429));
#273420=CARTESIAN_POINT('Ctrl Pts',(-117.786702325804,55.1801850026546,
680.462296651428));
#273421=CARTESIAN_POINT('Ctrl Pts',(-113.443927583196,64.4501995169386,
678.462296651428));
#273422=CARTESIAN_POINT('Ctrl Pts',(-107.704469842635,72.9267251261946,
676.462296651429));
#273423=CARTESIAN_POINT('Ctrl Pts',(-101.965012102074,81.4032507354507,
674.462296651429));
#273424=CARTESIAN_POINT('Ctrl Pts',(-94.9701958612992,88.8775672472032,
672.462296651428));
#273425=CARTESIAN_POINT('Ctrl Pts',(-87.9753796205245,96.3518837589558,
670.462296651429));
#273426=CARTESIAN_POINT('Ctrl Pts',(-79.8974404698484,102.639948694851,
668.462296651428));
#273427=CARTESIAN_POINT('Ctrl Pts',(-71.8195013191724,108.928013630747,
666.462296651428));
#273428=CARTESIAN_POINT('Ctrl Pts',(-62.8573449296276,113.874993963172,
664.462296651428));
#273429=CARTESIAN_POINT('Ctrl Pts',(-53.8951885400828,118.821974295598,
662.462296651429));
#273430=CARTESIAN_POINT('Ctrl Pts',(-44.2694929456717,122.306058950682,
660.462296651428));
#273431=CARTESIAN_POINT('Ctrl Pts',(-34.6437973512606,125.790143605767,
658.462296651428));
#273432=CARTESIAN_POINT('Ctrl Pts',(-24.5915791233697,127.725542856289,
656.462296651429));
#273433=CARTESIAN_POINT('Ctrl Pts',(-14.5393608954789,129.660942106811,
654.462296651428));
#273434=CARTESIAN_POINT('Ctrl Pts',(-4.30813900827846,130.,652.462296651428));
#273435=CARTESIAN_POINT('Ctrl Pts',(5.92308287892194,130.339057893189,650.462296651429));
#273436=CARTESIAN_POINT('Ctrl Pts',(16.0813817870903,129.073425698447,648.462296651428));
#273437=CARTESIAN_POINT('Ctrl Pts',(26.2396806952586,127.807793503705,646.462296651428));
#273438=CARTESIAN_POINT('Ctrl Pts',(36.0749255918146,124.968635286058,644.462296651428));
#273439=CARTESIAN_POINT('Ctrl Pts',(45.9101704883706,122.129477068411,642.462296651428));
#273440=CARTESIAN_POINT('Ctrl Pts',(55.1801850026546,117.786702325804,640.462296651428));
#273441=CARTESIAN_POINT('Ctrl Pts',(64.4501995169386,113.443927583196,638.462296651429));
#273442=CARTESIAN_POINT('Ctrl Pts',(72.9267251261946,107.704469842635,636.462296651428));
#273443=CARTESIAN_POINT('Ctrl Pts',(81.4032507354506,101.965012102074,634.462296651428));
#273444=CARTESIAN_POINT('Ctrl Pts',(88.8775672472032,94.9701958612992,632.462296651428));
#273445=CARTESIAN_POINT('Ctrl Pts',(96.3518837589558,87.9753796205245,630.462296651428));
#273446=CARTESIAN_POINT('Ctrl Pts',(102.639948694851,79.8974404698484,628.462296651428));
#273447=CARTESIAN_POINT('Ctrl Pts',(108.928013630747,71.8195013191724,626.462296651429));
#273448=CARTESIAN_POINT('Ctrl Pts',(113.874993963172,62.8573449296276,624.462296651428));
#273449=CARTESIAN_POINT('Ctrl Pts',(118.821974295598,53.8951885400829,622.462296651428));
#273450=CARTESIAN_POINT('Ctrl Pts',(122.306058950682,44.2694929456717,620.462296651428));
#273451=CARTESIAN_POINT('Ctrl Pts',(125.790143605767,34.6437973512606,618.462296651428));
#273452=CARTESIAN_POINT('Ctrl Pts',(127.725542856289,24.5915791233698,616.462296651428));
#273453=CARTESIAN_POINT('Ctrl Pts',(129.660942106811,14.5393608954789,614.462296651429));
#273454=CARTESIAN_POINT('Ctrl Pts',(130.,4.30813900827846,612.462296651428));
#273455=CARTESIAN_POINT('Ctrl Pts',(130.339057893189,-5.92308287892194,
610.462296651428));
#273456=CARTESIAN_POINT('Ctrl Pts',(129.073425698447,-16.0813817870903,
608.462296651428));
#273457=CARTESIAN_POINT('Ctrl Pts',(127.807793503705,-26.2396806952586,
606.462296651428));
#273458=CARTESIAN_POINT('Ctrl Pts',(124.968635286058,-36.0749255918146,
604.462296651428));
#273459=CARTESIAN_POINT('Ctrl Pts',(122.129477068411,-45.9101704883706,
602.462296651429));
#273460=CARTESIAN_POINT('Ctrl Pts',(117.786702325804,-55.1801850026546,
600.462296651428));
#273461=CARTESIAN_POINT('Ctrl Pts',(113.443927583196,-64.4501995169386,
598.462296651428));
#273462=CARTESIAN_POINT('Ctrl Pts',(107.704469842635,-72.9267251261946,
596.462296651428));
#273463=CARTESIAN_POINT('Ctrl Pts',(101.965012102074,-81.4032507354506,
594.462296651428));
#273464=CARTESIAN_POINT('Ctrl Pts',(94.9701958612992,-88.8775672472032,
592.462296651428));
#273465=CARTESIAN_POINT('Ctrl Pts',(87.9753796205246,-96.3518837589557,
590.462296651429));
#273466=CARTESIAN_POINT('Ctrl Pts',(79.8974404698484,-102.639948694851,
588.462296651428));
#273467=CARTESIAN_POINT('Ctrl Pts',(71.8195013191723,-108.928013630747,
586.462296651428));
#273468=CARTESIAN_POINT('Ctrl Pts',(62.8573449296276,-113.874993963172,
584.462296651428));
#273469=CARTESIAN_POINT('Ctrl Pts',(53.8951885400829,-118.821974295598,
582.462296651428));
#273470=CARTESIAN_POINT('Ctrl Pts',(44.2694929456717,-122.306058950682,
580.462296651428));
#273471=CARTESIAN_POINT('Ctrl Pts',(34.6437973512606,-125.790143605767,
578.462296651429));
#273472=CARTESIAN_POINT('Ctrl Pts',(24.5915791233698,-127.725542856289,
576.462296651428));
#273473=CARTESIAN_POINT('Ctrl Pts',(14.5393608954789,-129.660942106811,
574.462296651428));
#273474=CARTESIAN_POINT('Ctrl Pts',(4.30813900827847,-130.,572.462296651428));
#273475=CARTESIAN_POINT('Ctrl Pts',(-5.92308287892199,-130.339057893189,
570.462296651428));
#273476=CARTESIAN_POINT('Ctrl Pts',(-16.0813817870903,-129.073425698447,
568.462296651428));
#273477=CARTESIAN_POINT('Ctrl Pts',(-26.2396806952585,-127.807793503705,
566.462296651429));
#273478=CARTESIAN_POINT('Ctrl Pts',(-36.0749255918146,-124.968635286058,
564.462296651428));
#273479=CARTESIAN_POINT('Ctrl Pts',(-45.9101704883706,-122.129477068411,
562.462296651428));
#273480=CARTESIAN_POINT('Ctrl Pts',(-55.1801850026546,-117.786702325804,
560.462296651428));
#273481=CARTESIAN_POINT('Ctrl Pts',(-64.4501995169385,-113.443927583197,
558.462296651429));
#273482=CARTESIAN_POINT('Ctrl Pts',(-72.9267251261946,-107.704469842635,
556.462296651428));
#273483=CARTESIAN_POINT('Ctrl Pts',(-81.4032507354507,-101.965012102074,
554.462296651429));
#273484=CARTESIAN_POINT('Ctrl Pts',(-88.8775672472032,-94.9701958612992,
552.462296651428));
#273485=CARTESIAN_POINT('Ctrl Pts',(-96.3518837589557,-87.9753796205246,
550.462296651428));
#273486=CARTESIAN_POINT('Ctrl Pts',(-102.639948694851,-79.8974404698484,
548.462296651428));
#273487=CARTESIAN_POINT('Ctrl Pts',(-108.928013630747,-71.8195013191723,
546.462296651429));
#273488=CARTESIAN_POINT('Ctrl Pts',(-113.874993963172,-62.8573449296276,
544.462296651428));
#273489=CARTESIAN_POINT('Ctrl Pts',(-118.821974295598,-53.8951885400829,
542.462296651429));
#273490=CARTESIAN_POINT('Ctrl Pts',(-122.306058950682,-44.2694929456718,
540.462296651428));
#273491=CARTESIAN_POINT('Ctrl Pts',(-125.790143605767,-34.6437973512606,
538.462296651428));
#273492=CARTESIAN_POINT('Ctrl Pts',(-127.725542856289,-24.5915791233698,
536.462296651428));
#273493=CARTESIAN_POINT('Ctrl Pts',(-129.660942106811,-14.5393608954789,
534.462296651429));
#273494=CARTESIAN_POINT('Ctrl Pts',(-130.,-4.30813900827845,532.462296651428));
#273495=CARTESIAN_POINT('Ctrl Pts',(-160.,-4.30813900827851,692.462296651429));
#273496=CARTESIAN_POINT('Ctrl Pts',(-160.339057893189,8.28413408366045,
690.462296651429));
#273497=CARTESIAN_POINT('Ctrl Pts',(-158.704075916301,20.7744157382972,
688.462296651429));
#273498=CARTESIAN_POINT('Ctrl Pts',(-157.069093939413,33.2646973929339,
686.462296651429));
#273499=CARTESIAN_POINT('Ctrl Pts',(-153.500330774912,45.345435423063,684.462296651429));
#273500=CARTESIAN_POINT('Ctrl Pts',(-149.931567610412,57.4261734531921,
682.462296651429));
#273501=CARTESIAN_POINT('Ctrl Pts',(-144.516898051455,68.7998999948409,
680.462296651429));
#273502=CARTESIAN_POINT('Ctrl Pts',(-139.102228492498,80.1736265364898,
678.462296651429));
#273503=CARTESIAN_POINT('Ctrl Pts',(-131.974979673884,90.5602826949688,
676.462296651429));
#273504=CARTESIAN_POINT('Ctrl Pts',(-124.84773085527,100.946938853448,674.462296651429));
#273505=CARTESIAN_POINT('Ctrl Pts',(-116.183399296896,110.0907706828,672.462296651429));
#273506=CARTESIAN_POINT('Ctrl Pts',(-107.519067738522,119.234602512151,
670.462296651429));
#273507=CARTESIAN_POINT('Ctrl Pts',(-97.5309980386227,126.9104585261,668.462296651429));
#273508=CARTESIAN_POINT('Ctrl Pts',(-87.5429283387237,134.586314540048,
666.462296651429));
#273509=CARTESIAN_POINT('Ctrl Pts',(-76.4770599218141,140.605189688823,
664.462296651429));
#273510=CARTESIAN_POINT('Ctrl Pts',(-65.4111915049045,146.624064837598,
662.462296651429));
#273511=CARTESIAN_POINT('Ctrl Pts',(-53.5400027769202,150.837754439537,
660.462296651429));
#273512=CARTESIAN_POINT('Ctrl Pts',(-41.668814048936,155.051444041475,658.462296651429));
#273513=CARTESIAN_POINT('Ctrl Pts',(-29.2846130745767,157.356193074143,
656.462296651429));
#273514=CARTESIAN_POINT('Ctrl Pts',(-16.9004121002175,159.660942106811,
654.462296651428));
#273515=CARTESIAN_POINT('Ctrl Pts',(-4.30813900827852,160.,652.462296651429));
#273516=CARTESIAN_POINT('Ctrl Pts',(8.28413408366043,160.339057893189,650.462296651429));
#273517=CARTESIAN_POINT('Ctrl Pts',(20.7744157382972,158.704075916301,648.462296651428));
#273518=CARTESIAN_POINT('Ctrl Pts',(33.2646973929339,157.069093939413,646.462296651429));
#273519=CARTESIAN_POINT('Ctrl Pts',(45.345435423063,153.500330774912,644.462296651428));
#273520=CARTESIAN_POINT('Ctrl Pts',(57.4261734531921,149.931567610412,642.462296651428));
#273521=CARTESIAN_POINT('Ctrl Pts',(68.7998999948409,144.516898051455,640.462296651428));
#273522=CARTESIAN_POINT('Ctrl Pts',(80.1736265364898,139.102228492498,638.462296651429));
#273523=CARTESIAN_POINT('Ctrl Pts',(90.5602826949688,131.974979673884,636.462296651428));
#273524=CARTESIAN_POINT('Ctrl Pts',(100.946938853448,124.84773085527,634.462296651428));
#273525=CARTESIAN_POINT('Ctrl Pts',(110.0907706828,116.183399296896,632.462296651429));
#273526=CARTESIAN_POINT('Ctrl Pts',(119.234602512151,107.519067738522,630.462296651429));
#273527=CARTESIAN_POINT('Ctrl Pts',(126.9104585261,97.5309980386227,628.462296651429));
#273528=CARTESIAN_POINT('Ctrl Pts',(134.586314540048,87.5429283387237,626.462296651429));
#273529=CARTESIAN_POINT('Ctrl Pts',(140.605189688823,76.4770599218141,624.462296651429));
#273530=CARTESIAN_POINT('Ctrl Pts',(146.624064837598,65.4111915049045,622.462296651429));
#273531=CARTESIAN_POINT('Ctrl Pts',(150.837754439537,53.5400027769202,620.462296651429));
#273532=CARTESIAN_POINT('Ctrl Pts',(155.051444041475,41.668814048936,618.462296651429));
#273533=CARTESIAN_POINT('Ctrl Pts',(157.356193074143,29.2846130745767,616.462296651429));
#273534=CARTESIAN_POINT('Ctrl Pts',(159.660942106811,16.9004121002175,614.462296651429));
#273535=CARTESIAN_POINT('Ctrl Pts',(160.,4.30813900827853,612.462296651429));
#273536=CARTESIAN_POINT('Ctrl Pts',(160.339057893189,-8.28413408366043,
610.462296651429));
#273537=CARTESIAN_POINT('Ctrl Pts',(158.704075916301,-20.7744157382971,
608.462296651429));
#273538=CARTESIAN_POINT('Ctrl Pts',(157.069093939413,-33.2646973929339,
606.462296651429));
#273539=CARTESIAN_POINT('Ctrl Pts',(153.500330774912,-45.345435423063,604.462296651429));
#273540=CARTESIAN_POINT('Ctrl Pts',(149.931567610412,-57.4261734531921,
602.462296651429));
#273541=CARTESIAN_POINT('Ctrl Pts',(144.516898051455,-68.7998999948409,
600.462296651429));
#273542=CARTESIAN_POINT('Ctrl Pts',(139.102228492498,-80.1736265364898,
598.462296651429));
#273543=CARTESIAN_POINT('Ctrl Pts',(131.974979673884,-90.5602826949688,
596.462296651429));
#273544=CARTESIAN_POINT('Ctrl Pts',(124.84773085527,-100.946938853448,594.462296651428));
#273545=CARTESIAN_POINT('Ctrl Pts',(116.183399296896,-110.0907706828,592.462296651429));
#273546=CARTESIAN_POINT('Ctrl Pts',(107.519067738522,-119.234602512151,
590.462296651429));
#273547=CARTESIAN_POINT('Ctrl Pts',(97.5309980386227,-126.9104585261,588.462296651429));
#273548=CARTESIAN_POINT('Ctrl Pts',(87.5429283387236,-134.586314540048,
586.462296651429));
#273549=CARTESIAN_POINT('Ctrl Pts',(76.4770599218141,-140.605189688823,
584.462296651429));
#273550=CARTESIAN_POINT('Ctrl Pts',(65.4111915049046,-146.624064837598,
582.462296651428));
#273551=CARTESIAN_POINT('Ctrl Pts',(53.5400027769202,-150.837754439537,
580.462296651429));
#273552=CARTESIAN_POINT('Ctrl Pts',(41.6688140489359,-155.051444041475,
578.462296651429));
#273553=CARTESIAN_POINT('Ctrl Pts',(29.2846130745768,-157.356193074143,
576.462296651429));
#273554=CARTESIAN_POINT('Ctrl Pts',(16.9004121002176,-159.660942106811,
574.462296651429));
#273555=CARTESIAN_POINT('Ctrl Pts',(4.30813900827854,-160.,572.462296651429));
#273556=CARTESIAN_POINT('Ctrl Pts',(-8.28413408366049,-160.339057893189,
570.462296651428));
#273557=CARTESIAN_POINT('Ctrl Pts',(-20.7744157382971,-158.704075916301,
568.462296651429));
#273558=CARTESIAN_POINT('Ctrl Pts',(-33.2646973929338,-157.069093939413,
566.462296651429));
#273559=CARTESIAN_POINT('Ctrl Pts',(-45.345435423063,-153.500330774912,
564.462296651429));
#273560=CARTESIAN_POINT('Ctrl Pts',(-57.4261734531921,-149.931567610412,
562.462296651429));
#273561=CARTESIAN_POINT('Ctrl Pts',(-68.7998999948409,-144.516898051455,
560.462296651429));
#273562=CARTESIAN_POINT('Ctrl Pts',(-80.1736265364897,-139.102228492498,
558.462296651429));
#273563=CARTESIAN_POINT('Ctrl Pts',(-90.5602826949688,-131.974979673884,
556.462296651429));
#273564=CARTESIAN_POINT('Ctrl Pts',(-100.946938853448,-124.84773085527,
554.462296651429));
#273565=CARTESIAN_POINT('Ctrl Pts',(-110.0907706828,-116.183399296896,552.462296651429));
#273566=CARTESIAN_POINT('Ctrl Pts',(-119.234602512151,-107.519067738522,
550.462296651429));
#273567=CARTESIAN_POINT('Ctrl Pts',(-126.9104585261,-97.5309980386227,548.462296651429));
#273568=CARTESIAN_POINT('Ctrl Pts',(-134.586314540048,-87.5429283387236,
546.462296651429));
#273569=CARTESIAN_POINT('Ctrl Pts',(-140.605189688823,-76.4770599218141,
544.462296651429));
#273570=CARTESIAN_POINT('Ctrl Pts',(-146.624064837598,-65.4111915049046,
542.462296651429));
#273571=CARTESIAN_POINT('Ctrl Pts',(-150.837754439537,-53.5400027769203,
540.462296651429));
#273572=CARTESIAN_POINT('Ctrl Pts',(-155.051444041475,-41.668814048936,
538.462296651429));
#273573=CARTESIAN_POINT('Ctrl Pts',(-157.356193074143,-29.2846130745768,
536.462296651429));
#273574=CARTESIAN_POINT('Ctrl Pts',(-159.660942106811,-16.9004121002176,
534.462296651429));
#273575=CARTESIAN_POINT('Ctrl Pts',(-160.,-4.30813900827851,532.462296651429));
#273576=CARTESIAN_POINT('Origin',(4.03737035478159,-0.209103844020683,690.462377392296));
#273577=CARTESIAN_POINT('Ctrl Pts',(-160.,-4.30813900827851,692.462296651429));
#273578=CARTESIAN_POINT('Ctrl Pts',(-160.339057893189,8.28413408366045,
690.462296651429));
#273579=CARTESIAN_POINT('Ctrl Pts',(-158.704075916301,20.7744157382972,
688.462296651429));
#273580=CARTESIAN_POINT('Ctrl Pts',(-157.069093939413,33.2646973929339,
686.462296651429));
#273581=CARTESIAN_POINT('Ctrl Pts',(-153.500330774912,45.345435423063,684.462296651429));
#273582=CARTESIAN_POINT('Ctrl Pts',(-149.931567610412,57.4261734531921,
682.462296651429));
#273583=CARTESIAN_POINT('Ctrl Pts',(-144.516898051455,68.7998999948409,
680.462296651429));
#273584=CARTESIAN_POINT('Ctrl Pts',(-139.102228492498,80.1736265364898,
678.462296651429));
#273585=CARTESIAN_POINT('Ctrl Pts',(-131.974979673884,90.5602826949688,
676.462296651429));
#273586=CARTESIAN_POINT('Ctrl Pts',(-124.84773085527,100.946938853448,674.462296651429));
#273587=CARTESIAN_POINT('Ctrl Pts',(-116.183399296896,110.0907706828,672.462296651429));
#273588=CARTESIAN_POINT('Ctrl Pts',(-107.519067738522,119.234602512151,
670.462296651429));
#273589=CARTESIAN_POINT('Ctrl Pts',(-97.5309980386227,126.9104585261,668.462296651429));
#273590=CARTESIAN_POINT('Ctrl Pts',(-87.5429283387237,134.586314540048,
666.462296651429));
#273591=CARTESIAN_POINT('Ctrl Pts',(-76.4770599218141,140.605189688823,
664.462296651429));
#273592=CARTESIAN_POINT('Ctrl Pts',(-65.4111915049045,146.624064837598,
662.462296651429));
#273593=CARTESIAN_POINT('Ctrl Pts',(-53.5400027769202,150.837754439537,
660.462296651429));
#273594=CARTESIAN_POINT('Ctrl Pts',(-41.668814048936,155.051444041475,658.462296651429));
#273595=CARTESIAN_POINT('Ctrl Pts',(-29.2846130745767,157.356193074143,
656.462296651429));
#273596=CARTESIAN_POINT('Ctrl Pts',(-16.9004121002175,159.660942106811,
654.462296651428));
#273597=CARTESIAN_POINT('Ctrl Pts',(-4.30813900827852,160.,652.462296651429));
#273598=CARTESIAN_POINT('Ctrl Pts',(8.28413408366043,160.339057893189,650.462296651429));
#273599=CARTESIAN_POINT('Ctrl Pts',(20.7744157382972,158.704075916301,648.462296651428));
#273600=CARTESIAN_POINT('Ctrl Pts',(33.2646973929339,157.069093939413,646.462296651429));
#273601=CARTESIAN_POINT('Ctrl Pts',(45.345435423063,153.500330774912,644.462296651428));
#273602=CARTESIAN_POINT('Ctrl Pts',(57.4261734531921,149.931567610412,642.462296651428));
#273603=CARTESIAN_POINT('Ctrl Pts',(68.7998999948409,144.516898051455,640.462296651428));
#273604=CARTESIAN_POINT('Ctrl Pts',(80.1736265364898,139.102228492498,638.462296651429));
#273605=CARTESIAN_POINT('Ctrl Pts',(90.5602826949688,131.974979673884,636.462296651428));
#273606=CARTESIAN_POINT('Ctrl Pts',(100.946938853448,124.84773085527,634.462296651428));
#273607=CARTESIAN_POINT('Ctrl Pts',(110.0907706828,116.183399296896,632.462296651429));
#273608=CARTESIAN_POINT('Ctrl Pts',(119.234602512151,107.519067738522,630.462296651429));
#273609=CARTESIAN_POINT('Ctrl Pts',(126.9104585261,97.5309980386227,628.462296651429));
#273610=CARTESIAN_POINT('Ctrl Pts',(134.586314540048,87.5429283387237,626.462296651429));
#273611=CARTESIAN_POINT('Ctrl Pts',(140.605189688823,76.4770599218141,624.462296651429));
#273612=CARTESIAN_POINT('Ctrl Pts',(146.624064837598,65.4111915049045,622.462296651429));
#273613=CARTESIAN_POINT('Ctrl Pts',(150.837754439537,53.5400027769202,620.462296651429));
#273614=CARTESIAN_POINT('Ctrl Pts',(155.051444041475,41.668814048936,618.462296651429));
#273615=CARTESIAN_POINT('Ctrl Pts',(157.356193074143,29.2846130745767,616.462296651429));
#273616=CARTESIAN_POINT('Ctrl Pts',(159.660942106811,16.9004121002175,614.462296651429));
#273617=CARTESIAN_POINT('Ctrl Pts',(160.,4.30813900827853,612.462296651429));
#273618=CARTESIAN_POINT('Ctrl Pts',(160.339057893189,-8.28413408366043,
610.462296651429));
#273619=CARTESIAN_POINT('Ctrl Pts',(158.704075916301,-20.7744157382971,
608.462296651429));
#273620=CARTESIAN_POINT('Ctrl Pts',(157.069093939413,-33.2646973929339,
606.462296651429));
#273621=CARTESIAN_POINT('Ctrl Pts',(153.500330774912,-45.345435423063,604.462296651429));
#273622=CARTESIAN_POINT('Ctrl Pts',(149.931567610412,-57.4261734531921,
602.462296651429));
#273623=CARTESIAN_POINT('Ctrl Pts',(144.516898051455,-68.7998999948409,
600.462296651429));
#273624=CARTESIAN_POINT('Ctrl Pts',(139.102228492498,-80.1736265364898,
598.462296651429));
#273625=CARTESIAN_POINT('Ctrl Pts',(131.974979673884,-90.5602826949688,
596.462296651429));
#273626=CARTESIAN_POINT('Ctrl Pts',(124.84773085527,-100.946938853448,594.462296651428));
#273627=CARTESIAN_POINT('Ctrl Pts',(116.183399296896,-110.0907706828,592.462296651429));
#273628=CARTESIAN_POINT('Ctrl Pts',(107.519067738522,-119.234602512151,
590.462296651429));
#273629=CARTESIAN_POINT('Ctrl Pts',(97.5309980386227,-126.9104585261,588.462296651429));
#273630=CARTESIAN_POINT('Ctrl Pts',(87.5429283387236,-134.586314540048,
586.462296651429));
#273631=CARTESIAN_POINT('Ctrl Pts',(76.4770599218141,-140.605189688823,
584.462296651429));
#273632=CARTESIAN_POINT('Ctrl Pts',(65.4111915049046,-146.624064837598,
582.462296651428));
#273633=CARTESIAN_POINT('Ctrl Pts',(53.5400027769202,-150.837754439537,
580.462296651429));
#273634=CARTESIAN_POINT('Ctrl Pts',(41.6688140489359,-155.051444041475,
578.462296651429));
#273635=CARTESIAN_POINT('Ctrl Pts',(29.2846130745768,-157.356193074143,
576.462296651429));
#273636=CARTESIAN_POINT('Ctrl Pts',(16.9004121002176,-159.660942106811,
574.462296651429));
#273637=CARTESIAN_POINT('Ctrl Pts',(4.30813900827854,-160.,572.462296651429));
#273638=CARTESIAN_POINT('Ctrl Pts',(-8.28413408366049,-160.339057893189,
570.462296651428));
#273639=CARTESIAN_POINT('Ctrl Pts',(-20.7744157382971,-158.704075916301,
568.462296651429));
#273640=CARTESIAN_POINT('Ctrl Pts',(-33.2646973929338,-157.069093939413,
566.462296651429));
#273641=CARTESIAN_POINT('Ctrl Pts',(-45.345435423063,-153.500330774912,
564.462296651429));
#273642=CARTESIAN_POINT('Ctrl Pts',(-57.4261734531921,-149.931567610412,
562.462296651429));
#273643=CARTESIAN_POINT('Ctrl Pts',(-68.7998999948409,-144.516898051455,
560.462296651429));
#273644=CARTESIAN_POINT('Ctrl Pts',(-80.1736265364897,-139.102228492498,
558.462296651429));
#273645=CARTESIAN_POINT('Ctrl Pts',(-90.5602826949688,-131.974979673884,
556.462296651429));
#273646=CARTESIAN_POINT('Ctrl Pts',(-100.946938853448,-124.84773085527,
554.462296651429));
#273647=CARTESIAN_POINT('Ctrl Pts',(-110.0907706828,-116.183399296896,552.462296651429));
#273648=CARTESIAN_POINT('Ctrl Pts',(-119.234602512151,-107.519067738522,
550.462296651429));
#273649=CARTESIAN_POINT('Ctrl Pts',(-126.9104585261,-97.5309980386227,548.462296651429));
#273650=CARTESIAN_POINT('Ctrl Pts',(-134.586314540048,-87.5429283387236,
546.462296651429));
#273651=CARTESIAN_POINT('Ctrl Pts',(-140.605189688823,-76.4770599218141,
544.462296651429));
#273652=CARTESIAN_POINT('Ctrl Pts',(-146.624064837598,-65.4111915049046,
542.462296651429));
#273653=CARTESIAN_POINT('Ctrl Pts',(-150.837754439537,-53.5400027769203,
540.462296651429));
#273654=CARTESIAN_POINT('Ctrl Pts',(-155.051444041475,-41.668814048936,
538.462296651429));
#273655=CARTESIAN_POINT('Ctrl Pts',(-157.356193074143,-29.2846130745768,
536.462296651429));
#273656=CARTESIAN_POINT('Ctrl Pts',(-159.660942106811,-16.9004121002176,
534.462296651429));
#273657=CARTESIAN_POINT('Ctrl Pts',(-160.,-4.30813900827851,532.462296651429));
#273658=CARTESIAN_POINT('Ctrl Pts',(-160.,4.30813900827767,697.537703348572));
#273659=CARTESIAN_POINT('Ctrl Pts',(-159.660942106811,16.9004121002166,
695.537703348572));
#273660=CARTESIAN_POINT('Ctrl Pts',(-157.356193074143,29.2846130745759,
693.537703348572));
#273661=CARTESIAN_POINT('Ctrl Pts',(-155.051444041476,41.6688140489352,
691.537703348572));
#273662=CARTESIAN_POINT('Ctrl Pts',(-150.837754439537,53.5400027769194,
689.537703348572));
#273663=CARTESIAN_POINT('Ctrl Pts',(-146.624064837599,65.4111915049037,
687.537703348572));
#273664=CARTESIAN_POINT('Ctrl Pts',(-140.605189688823,76.4770599218133,
685.537703348572));
#273665=CARTESIAN_POINT('Ctrl Pts',(-134.586314540048,87.542928338723,683.537703348572));
#273666=CARTESIAN_POINT('Ctrl Pts',(-126.9104585261,97.530998038622,681.537703348572));
#273667=CARTESIAN_POINT('Ctrl Pts',(-119.234602512152,107.519067738521,
679.537703348572));
#273668=CARTESIAN_POINT('Ctrl Pts',(-110.0907706828,116.183399296895,677.537703348572));
#273669=CARTESIAN_POINT('Ctrl Pts',(-100.946938853448,124.847730855269,
675.537703348572));
#273670=CARTESIAN_POINT('Ctrl Pts',(-90.5602826949695,131.974979673883,
673.537703348572));
#273671=CARTESIAN_POINT('Ctrl Pts',(-80.1736265364906,139.102228492497,
671.537703348572));
#273672=CARTESIAN_POINT('Ctrl Pts',(-68.7998999948417,144.516898051454,
669.537703348572));
#273673=CARTESIAN_POINT('Ctrl Pts',(-57.4261734531929,149.931567610411,
667.537703348572));
#273674=CARTESIAN_POINT('Ctrl Pts',(-45.3454354230638,153.500330774912,
665.537703348572));
#273675=CARTESIAN_POINT('Ctrl Pts',(-33.2646973929347,157.069093939413,
663.537703348572));
#273676=CARTESIAN_POINT('Ctrl Pts',(-20.774415738298,158.704075916301,661.537703348572));
#273677=CARTESIAN_POINT('Ctrl Pts',(-8.28413408366129,160.339057893189,
659.537703348572));
#273678=CARTESIAN_POINT('Ctrl Pts',(4.30813900827766,160.,657.537703348572));
#273679=CARTESIAN_POINT('Ctrl Pts',(16.9004121002166,159.660942106811,655.537703348572));
#273680=CARTESIAN_POINT('Ctrl Pts',(29.2846130745759,157.356193074143,653.537703348572));
#273681=CARTESIAN_POINT('Ctrl Pts',(41.6688140489352,155.051444041476,651.537703348572));
#273682=CARTESIAN_POINT('Ctrl Pts',(53.5400027769194,150.837754439537,649.537703348572));
#273683=CARTESIAN_POINT('Ctrl Pts',(65.4111915049037,146.624064837599,647.537703348572));
#273684=CARTESIAN_POINT('Ctrl Pts',(76.4770599218133,140.605189688823,645.537703348572));
#273685=CARTESIAN_POINT('Ctrl Pts',(87.542928338723,134.586314540048,643.537703348572));
#273686=CARTESIAN_POINT('Ctrl Pts',(97.530998038622,126.9104585261,641.537703348572));
#273687=CARTESIAN_POINT('Ctrl Pts',(107.519067738521,119.234602512152,639.537703348572));
#273688=CARTESIAN_POINT('Ctrl Pts',(116.183399296895,110.0907706828,637.537703348572));
#273689=CARTESIAN_POINT('Ctrl Pts',(124.847730855269,100.946938853448,635.537703348572));
#273690=CARTESIAN_POINT('Ctrl Pts',(131.974979673883,90.5602826949695,633.537703348572));
#273691=CARTESIAN_POINT('Ctrl Pts',(139.102228492497,80.1736265364906,631.537703348572));
#273692=CARTESIAN_POINT('Ctrl Pts',(144.516898051454,68.7998999948417,629.537703348572));
#273693=CARTESIAN_POINT('Ctrl Pts',(149.931567610411,57.4261734531929,627.537703348572));
#273694=CARTESIAN_POINT('Ctrl Pts',(153.500330774912,45.3454354230638,625.537703348572));
#273695=CARTESIAN_POINT('Ctrl Pts',(157.069093939413,33.2646973929347,623.537703348572));
#273696=CARTESIAN_POINT('Ctrl Pts',(158.704075916301,20.774415738298,621.537703348572));
#273697=CARTESIAN_POINT('Ctrl Pts',(160.339057893189,8.28413408366131,619.537703348572));
#273698=CARTESIAN_POINT('Ctrl Pts',(160.,-4.30813900827765,617.537703348572));
#273699=CARTESIAN_POINT('Ctrl Pts',(159.660942106811,-16.9004121002166,
615.537703348572));
#273700=CARTESIAN_POINT('Ctrl Pts',(157.356193074143,-29.2846130745759,
613.537703348572));
#273701=CARTESIAN_POINT('Ctrl Pts',(155.051444041476,-41.6688140489352,
611.537703348572));
#273702=CARTESIAN_POINT('Ctrl Pts',(150.837754439537,-53.5400027769194,
609.537703348572));
#273703=CARTESIAN_POINT('Ctrl Pts',(146.624064837599,-65.4111915049036,
607.537703348572));
#273704=CARTESIAN_POINT('Ctrl Pts',(140.605189688823,-76.4770599218133,
605.537703348572));
#273705=CARTESIAN_POINT('Ctrl Pts',(134.586314540048,-87.5429283387229,
603.537703348572));
#273706=CARTESIAN_POINT('Ctrl Pts',(126.9104585261,-97.530998038622,601.537703348572));
#273707=CARTESIAN_POINT('Ctrl Pts',(119.234602512152,-107.519067738521,
599.537703348572));
#273708=CARTESIAN_POINT('Ctrl Pts',(110.0907706828,-116.183399296895,597.537703348572));
#273709=CARTESIAN_POINT('Ctrl Pts',(100.946938853448,-124.847730855269,
595.537703348572));
#273710=CARTESIAN_POINT('Ctrl Pts',(90.5602826949695,-131.974979673883,
593.537703348572));
#273711=CARTESIAN_POINT('Ctrl Pts',(80.1736265364905,-139.102228492497,
591.537703348572));
#273712=CARTESIAN_POINT('Ctrl Pts',(68.7998999948417,-144.516898051454,
589.537703348572));
#273713=CARTESIAN_POINT('Ctrl Pts',(57.426173453193,-149.931567610411,587.537703348572));
#273714=CARTESIAN_POINT('Ctrl Pts',(45.3454354230638,-153.500330774912,
585.537703348572));
#273715=CARTESIAN_POINT('Ctrl Pts',(33.2646973929347,-157.069093939413,
583.537703348572));
#273716=CARTESIAN_POINT('Ctrl Pts',(20.774415738298,-158.704075916301,581.537703348572));
#273717=CARTESIAN_POINT('Ctrl Pts',(8.28413408366139,-160.339057893189,
579.537703348572));
#273718=CARTESIAN_POINT('Ctrl Pts',(-4.30813900827764,-160.,577.537703348572));
#273719=CARTESIAN_POINT('Ctrl Pts',(-16.9004121002167,-159.660942106811,
575.537703348572));
#273720=CARTESIAN_POINT('Ctrl Pts',(-29.2846130745759,-157.356193074143,
573.537703348572));
#273721=CARTESIAN_POINT('Ctrl Pts',(-41.6688140489351,-155.051444041476,
571.537703348572));
#273722=CARTESIAN_POINT('Ctrl Pts',(-53.5400027769194,-150.837754439537,
569.537703348572));
#273723=CARTESIAN_POINT('Ctrl Pts',(-65.4111915049037,-146.624064837599,
567.537703348572));
#273724=CARTESIAN_POINT('Ctrl Pts',(-76.4770599218133,-140.605189688823,
565.537703348572));
#273725=CARTESIAN_POINT('Ctrl Pts',(-87.5429283387229,-134.586314540048,
563.537703348572));
#273726=CARTESIAN_POINT('Ctrl Pts',(-97.530998038622,-126.9104585261,561.537703348572));
#273727=CARTESIAN_POINT('Ctrl Pts',(-107.519067738521,-119.234602512152,
559.537703348572));
#273728=CARTESIAN_POINT('Ctrl Pts',(-116.183399296895,-110.0907706828,557.537703348572));
#273729=CARTESIAN_POINT('Ctrl Pts',(-124.847730855269,-100.946938853448,
555.537703348572));
#273730=CARTESIAN_POINT('Ctrl Pts',(-131.974979673883,-90.5602826949695,
553.537703348572));
#273731=CARTESIAN_POINT('Ctrl Pts',(-139.102228492497,-80.1736265364905,
551.537703348572));
#273732=CARTESIAN_POINT('Ctrl Pts',(-144.516898051454,-68.7998999948417,
549.537703348572));
#273733=CARTESIAN_POINT('Ctrl Pts',(-149.931567610411,-57.426173453193,
547.537703348572));
#273734=CARTESIAN_POINT('Ctrl Pts',(-153.500330774912,-45.3454354230638,
545.537703348572));
#273735=CARTESIAN_POINT('Ctrl Pts',(-157.069093939413,-33.2646973929347,
543.537703348572));
#273736=CARTESIAN_POINT('Ctrl Pts',(-158.704075916301,-20.774415738298,
541.537703348572));
#273737=CARTESIAN_POINT('Ctrl Pts',(-160.339057893189,-8.2841340836614,
539.537703348572));
#273738=CARTESIAN_POINT('Ctrl Pts',(-160.,4.30813900827767,537.537703348572));
#273739=CARTESIAN_POINT('Origin',(-160.339057893189,22.4999999999891,848.));
#273740=CARTESIAN_POINT('Origin',(-160.,-160.339057893189,367.5));
#273741=CARTESIAN_POINT('',(0.,0.,0.));
#273742=CARTESIAN_POINT('Origin',(0.,0.,0.));
#273743=CARTESIAN_POINT('',(-65.,-614.173929613455,0.));
#273744=CARTESIAN_POINT('',(65.169448912385,-614.173929613455,0.));
#273745=CARTESIAN_POINT('',(65.169448912385,-614.173929613455,0.));
#273746=CARTESIAN_POINT('',(-65.,-550.402639059603,0.));
#273747=CARTESIAN_POINT('',(-65.,-511.398533506753,0.));
#273748=CARTESIAN_POINT('',(65.169448912385,-550.402639059603,0.));
#273749=CARTESIAN_POINT('',(65.169448912385,-550.402639059603,0.));
#273750=CARTESIAN_POINT('',(65.169448912385,-511.398533506753,0.));
#273751=CARTESIAN_POINT('Origin',(0.,0.,304.));
#273752=CARTESIAN_POINT('',(49.830664447451,-620.152805159724,304.));
#273753=CARTESIAN_POINT('',(49.830664447451,-541.923394840277,304.));
#273754=CARTESIAN_POINT('',(49.830664447451,-541.923394840277,304.));
#273755=CARTESIAN_POINT('',(41.5056707885714,-532.064675158837,304.));
#273756=CARTESIAN_POINT('Origin',(39.830664447451,-541.923394840277,304.));
#273757=CARTESIAN_POINT('',(53.6812599743419,-532.064675158837,304.));
#273758=CARTESIAN_POINT('',(-53.681259974342,-532.064675158837,304.));
#273759=CARTESIAN_POINT('',(53.6812599743419,-630.011524841163,304.));
#273760=CARTESIAN_POINT('',(53.6812599743419,-532.064675158837,304.));
#273761=CARTESIAN_POINT('',(41.5056707885714,-630.011524841163,304.));
#273762=CARTESIAN_POINT('',(-53.681259974342,-630.011524841163,304.));
#273763=CARTESIAN_POINT('Origin',(39.830664447451,-620.152805159724,304.));
#273764=CARTESIAN_POINT('Origin',(-65.,-511.398533506753,25.));
#273765=CARTESIAN_POINT('',(-65.,-647.946325817004,-15.));
#273766=CARTESIAN_POINT('',(-65.,-647.946325817004,22.));
#273767=CARTESIAN_POINT('',(-65.,-647.946325817004,25.));
#273768=CARTESIAN_POINT('',(-65.,-516.398533506753,22.));
#273769=CARTESIAN_POINT('',(-65.,-516.398533506753,22.));
#273770=CARTESIAN_POINT('',(-65.,-516.398533506753,-15.));
#273771=CARTESIAN_POINT('',(-65.,-516.398533506753,25.));
#273772=CARTESIAN_POINT('',(-65.,-550.402639059603,-15.));
#273773=CARTESIAN_POINT('',(-65.,-550.402639059603,-15.));
#273774=CARTESIAN_POINT('',(-65.,-550.402639059603,-15.));
#273775=CARTESIAN_POINT('',(-65.,-614.173929613455,-15.));
#273776=CARTESIAN_POINT('',(-65.,-614.173929613455,-15.));
#273777=CARTESIAN_POINT('',(-65.,-647.946325817004,-15.));
#273778=CARTESIAN_POINT('Origin',(-65.,-652.946325817004,25.));
#273779=CARTESIAN_POINT('',(60.169448912385,-652.946325817004,-15.));
#273780=CARTESIAN_POINT('',(60.169448912385,-652.946325817004,22.));
#273781=CARTESIAN_POINT('',(60.169448912385,-652.946325817004,25.));
#273782=CARTESIAN_POINT('',(-60.,-652.946325817004,22.));
#273783=CARTESIAN_POINT('',(-60.,-652.946325817004,22.));
#273784=CARTESIAN_POINT('',(-60.,-652.946325817004,-15.));
#273785=CARTESIAN_POINT('',(-60.,-652.946325817004,25.));
#273786=CARTESIAN_POINT('',(60.169448912385,-652.946325817004,-15.));
#273787=CARTESIAN_POINT('Origin',(65.169448912385,-511.398533506753,25.));
#273788=CARTESIAN_POINT('',(65.169448912385,-516.398533506753,-15.));
#273789=CARTESIAN_POINT('',(65.169448912385,-516.398533506753,22.));
#273790=CARTESIAN_POINT('',(65.169448912385,-516.398533506753,25.));
#273791=CARTESIAN_POINT('',(65.169448912385,-647.946325817004,22.));
#273792=CARTESIAN_POINT('',(65.169448912385,-647.946325817004,22.));
#273793=CARTESIAN_POINT('',(65.169448912385,-647.946325817004,-15.));
#273794=CARTESIAN_POINT('',(65.169448912385,-647.946325817004,25.));
#273795=CARTESIAN_POINT('',(65.169448912385,-614.173929613455,-15.));
#273796=CARTESIAN_POINT('',(65.169448912385,-614.173929613455,-15.));
#273797=CARTESIAN_POINT('',(65.169448912385,-614.173929613455,-15.));
#273798=CARTESIAN_POINT('',(65.169448912385,-550.402639059603,-15.));
#273799=CARTESIAN_POINT('',(65.169448912385,-550.402639059603,-15.));
#273800=CARTESIAN_POINT('',(65.169448912385,-516.398533506753,-15.));
#273801=CARTESIAN_POINT('Origin',(-65.,-511.398533506753,25.));
#273802=CARTESIAN_POINT('',(-60.,-511.398533506753,-15.));
#273803=CARTESIAN_POINT('',(-60.,-511.398533506753,22.));
#273804=CARTESIAN_POINT('',(-60.,-511.398533506753,25.));
#273805=CARTESIAN_POINT('',(60.169448912385,-511.398533506753,22.));
#273806=CARTESIAN_POINT('',(60.169448912385,-511.398533506753,22.));
#273807=CARTESIAN_POINT('',(60.169448912385,-511.398533506753,-15.));
#273808=CARTESIAN_POINT('',(60.169448912385,-511.398533506753,25.));
#273809=CARTESIAN_POINT('',(-60.,-511.398533506753,-15.));
#273810=CARTESIAN_POINT('Origin',(0.,0.,25.));
#273811=CARTESIAN_POINT('',(62.169448912385,-647.946325817004,25.));
#273812=CARTESIAN_POINT('',(62.169448912385,-516.398533506753,25.));
#273813=CARTESIAN_POINT('',(62.169448912385,-516.398533506753,25.));
#273814=CARTESIAN_POINT('',(60.169448912385,-514.398533506753,25.));
#273815=CARTESIAN_POINT('Origin',(60.169448912385,-516.398533506753,25.));
#273816=CARTESIAN_POINT('',(-60.,-514.398533506753,25.));
#273817=CARTESIAN_POINT('',(-60.,-514.398533506753,25.));
#273818=CARTESIAN_POINT('',(-62.,-516.398533506753,25.));
#273819=CARTESIAN_POINT('Origin',(-60.,-516.398533506753,25.));
#273820=CARTESIAN_POINT('',(-62.,-647.946325817004,25.));
#273821=CARTESIAN_POINT('',(-62.,-647.946325817004,25.));
#273822=CARTESIAN_POINT('',(-60.,-649.946325817004,25.));
#273823=CARTESIAN_POINT('Origin',(-60.,-647.946325817004,25.));
#273824=CARTESIAN_POINT('',(60.169448912385,-649.946325817004,25.));
#273825=CARTESIAN_POINT('',(60.169448912385,-649.946325817004,25.));
#273826=CARTESIAN_POINT('Origin',(60.169448912385,-647.946325817004,25.));
#273827=CARTESIAN_POINT('',(-39.830664447451,-531.923394840277,25.));
#273828=CARTESIAN_POINT('',(39.830664447451,-531.923394840277,25.));
#273829=CARTESIAN_POINT('',(0.,-531.923394840277,25.));
#273830=CARTESIAN_POINT('',(49.830664447451,-541.923394840277,25.));
#273831=CARTESIAN_POINT('Origin',(39.830664447451,-541.923394840277,25.));
#273832=CARTESIAN_POINT('',(49.830664447451,-620.152805159724,25.));
#273833=CARTESIAN_POINT('',(49.830664447451,0.,25.));
#273834=CARTESIAN_POINT('',(39.830664447451,-630.152805159724,25.));
#273835=CARTESIAN_POINT('Origin',(39.830664447451,-620.152805159724,25.));
#273836=CARTESIAN_POINT('',(-39.830664447451,-630.152805159724,25.));
#273837=CARTESIAN_POINT('',(0.,-630.152805159724,25.));
#273838=CARTESIAN_POINT('',(-49.830664447451,-620.152805159724,25.));
#273839=CARTESIAN_POINT('Origin',(-39.830664447451,-620.152805159724,25.));
#273840=CARTESIAN_POINT('',(-49.830664447451,-541.923394840277,25.));
#273841=CARTESIAN_POINT('',(-49.830664447451,0.,25.));
#273842=CARTESIAN_POINT('Origin',(-39.830664447451,-541.923394840277,25.));
#273843=CARTESIAN_POINT('Origin',(44.830664447451,-536.923394840277,304.));
#273844=CARTESIAN_POINT('',(44.830664447451,-620.152805159724,299.));
#273845=CARTESIAN_POINT('',(44.830664447451,-620.152805159724,30.));
#273846=CARTESIAN_POINT('',(44.830664447451,-620.152805159724,304.));
#273847=CARTESIAN_POINT('',(44.830664447451,-541.923394840277,30.));
#273848=CARTESIAN_POINT('',(44.830664447451,-536.923394840277,30.));
#273849=CARTESIAN_POINT('',(44.830664447451,-541.923394840277,299.));
#273850=CARTESIAN_POINT('',(44.830664447451,-541.923394840277,304.));
#273851=CARTESIAN_POINT('',(44.830664447451,-620.152805159724,299.));
#273852=CARTESIAN_POINT('Origin',(-44.830664447451,-536.923394840277,304.));
#273853=CARTESIAN_POINT('',(-39.830664447451,-536.923394840277,30.));
#273854=CARTESIAN_POINT('',(-39.830664447451,-536.923394840277,299.001996411407));
#273855=CARTESIAN_POINT('',(-39.830664447451,-536.923394840277,304.));
#273856=CARTESIAN_POINT('',(39.830664447451,-536.923394840277,299.001996411407));
#273857=CARTESIAN_POINT('',(-44.830664447451,-536.923394840277,299.001996411407));
#273858=CARTESIAN_POINT('',(39.830664447451,-536.923394840277,30.));
#273859=CARTESIAN_POINT('',(39.830664447451,-536.923394840277,304.));
#273860=CARTESIAN_POINT('',(-44.830664447451,-536.923394840277,30.));
#273861=CARTESIAN_POINT('Origin',(-44.830664447451,-536.923394840277,304.));
#273862=CARTESIAN_POINT('',(-44.830664447451,-541.923394840277,299.));
#273863=CARTESIAN_POINT('',(-44.830664447451,-541.923394840277,30.));
#273864=CARTESIAN_POINT('',(-44.830664447451,-541.923394840277,304.));
#273865=CARTESIAN_POINT('',(-44.830664447451,-620.152805159724,30.));
#273866=CARTESIAN_POINT('',(-44.830664447451,-536.923394840277,30.));
#273867=CARTESIAN_POINT('',(-44.830664447451,-620.152805159724,299.));
#273868=CARTESIAN_POINT('',(-44.830664447451,-620.152805159724,304.));
#273869=CARTESIAN_POINT('',(-44.830664447451,-541.923394840277,299.));
#273870=CARTESIAN_POINT('Origin',(-44.830664447451,-625.152805159724,304.));
#273871=CARTESIAN_POINT('',(-39.830664447451,-625.152805159724,299.001996411407));
#273872=CARTESIAN_POINT('',(-39.830664447451,-625.152805159724,30.));
#273873=CARTESIAN_POINT('',(-39.830664447451,-625.152805159724,304.));
#273874=CARTESIAN_POINT('',(39.830664447451,-625.152805159724,30.));
#273875=CARTESIAN_POINT('',(-44.830664447451,-625.152805159724,30.));
#273876=CARTESIAN_POINT('',(39.830664447451,-625.152805159724,299.001996411407));
#273877=CARTESIAN_POINT('',(39.830664447451,-625.152805159724,304.));
#273878=CARTESIAN_POINT('',(-44.830664447451,-625.152805159724,299.001996411407));
#273879=CARTESIAN_POINT('Origin',(-60.,-516.398533506753,25.));
#273880=CARTESIAN_POINT('Origin',(-60.,-516.398533506753,22.));
#273881=CARTESIAN_POINT('Origin',(-60.,-516.398533506753,-15.));
#273882=CARTESIAN_POINT('Origin',(60.169448912385,-647.946325817004,25.));
#273883=CARTESIAN_POINT('Origin',(60.169448912385,-647.946325817004,22.));
#273884=CARTESIAN_POINT('Origin',(60.169448912385,-647.946325817004,-15.));
#273885=CARTESIAN_POINT('Origin',(-60.,-647.946325817004,25.));
#273886=CARTESIAN_POINT('Origin',(-60.,-647.946325817004,22.));
#273887=CARTESIAN_POINT('Origin',(-60.,-647.946325817004,-15.));
#273888=CARTESIAN_POINT('Origin',(60.169448912385,-516.398533506753,25.));
#273889=CARTESIAN_POINT('Origin',(60.169448912385,-516.398533506753,22.));
#273890=CARTESIAN_POINT('Origin',(60.169448912385,-516.398533506753,-15.));
#273891=CARTESIAN_POINT('Ctrl Pts',(-65.,-647.946325817004,22.));
#273892=CARTESIAN_POINT('Ctrl Pts',(-65.,-652.946325817004,22.));
#273893=CARTESIAN_POINT('Ctrl Pts',(-60.,-652.946325817004,22.));
#273894=CARTESIAN_POINT('Ctrl Pts',(-65.,-647.946325817004,25.));
#273895=CARTESIAN_POINT('Ctrl Pts',(-65.,-652.946325817004,25.));
#273896=CARTESIAN_POINT('Ctrl Pts',(-60.,-652.946325817004,25.));
#273897=CARTESIAN_POINT('Ctrl Pts',(-62.,-647.946325817004,25.));
#273898=CARTESIAN_POINT('Ctrl Pts',(-62.,-649.946325817004,25.));
#273899=CARTESIAN_POINT('Ctrl Pts',(-60.,-649.946325817004,25.));
#273900=CARTESIAN_POINT('Origin',(-62.,-647.946325817004,22.));
#273901=CARTESIAN_POINT('Origin',(-60.,-649.946325817004,22.));
#273902=CARTESIAN_POINT('Origin',(0.,-649.946325817004,22.));
#273903=CARTESIAN_POINT('Origin',(60.169448912385,-649.946325817004,22.));
#273904=CARTESIAN_POINT('Origin',(-62.,0.,22.));
#273905=CARTESIAN_POINT('Origin',(-62.,-516.398533506753,22.));
#273906=CARTESIAN_POINT('Ctrl Pts',(60.169448912385,-652.946325817004,22.));
#273907=CARTESIAN_POINT('Ctrl Pts',(65.169448912385,-652.946325817004,22.));
#273908=CARTESIAN_POINT('Ctrl Pts',(65.169448912385,-647.946325817004,22.));
#273909=CARTESIAN_POINT('Ctrl Pts',(60.169448912385,-652.946325817004,25.));
#273910=CARTESIAN_POINT('Ctrl Pts',(65.169448912385,-652.946325817004,25.));
#273911=CARTESIAN_POINT('Ctrl Pts',(65.169448912385,-647.946325817004,25.));
#273912=CARTESIAN_POINT('Ctrl Pts',(60.169448912385,-649.946325817004,25.));
#273913=CARTESIAN_POINT('Ctrl Pts',(62.169448912385,-649.946325817004,25.));
#273914=CARTESIAN_POINT('Ctrl Pts',(62.169448912385,-647.946325817004,25.));
#273915=CARTESIAN_POINT('Origin',(62.169448912385,-647.946325817004,22.));
#273916=CARTESIAN_POINT('Ctrl Pts',(-60.,-511.398533506753,22.));
#273917=CARTESIAN_POINT('Ctrl Pts',(-65.,-511.398533506753,22.));
#273918=CARTESIAN_POINT('Ctrl Pts',(-65.,-516.398533506753,22.));
#273919=CARTESIAN_POINT('Ctrl Pts',(-60.,-511.398533506753,25.));
#273920=CARTESIAN_POINT('Ctrl Pts',(-65.,-511.398533506753,25.));
#273921=CARTESIAN_POINT('Ctrl Pts',(-65.,-516.398533506753,25.));
#273922=CARTESIAN_POINT('Ctrl Pts',(-60.,-514.398533506753,25.));
#273923=CARTESIAN_POINT('Ctrl Pts',(-62.,-514.398533506753,25.));
#273924=CARTESIAN_POINT('Ctrl Pts',(-62.,-516.398533506753,25.));
#273925=CARTESIAN_POINT('Origin',(-60.,-514.398533506753,22.));
#273926=CARTESIAN_POINT('Origin',(62.169448912385,0.,22.));
#273927=CARTESIAN_POINT('Origin',(62.169448912385,-516.398533506753,22.));
#273928=CARTESIAN_POINT('Origin',(0.,-514.398533506753,22.));
#273929=CARTESIAN_POINT('Origin',(60.169448912385,-514.398533506753,22.));
#273930=CARTESIAN_POINT('Ctrl Pts',(65.169448912385,-516.398533506753,22.));
#273931=CARTESIAN_POINT('Ctrl Pts',(65.169448912385,-511.398533506753,22.));
#273932=CARTESIAN_POINT('Ctrl Pts',(60.169448912385,-511.398533506753,22.));
#273933=CARTESIAN_POINT('Ctrl Pts',(65.169448912385,-516.398533506753,25.));
#273934=CARTESIAN_POINT('Ctrl Pts',(65.169448912385,-511.398533506753,25.));
#273935=CARTESIAN_POINT('Ctrl Pts',(60.169448912385,-511.398533506753,25.));
#273936=CARTESIAN_POINT('Ctrl Pts',(62.169448912385,-516.398533506753,25.));
#273937=CARTESIAN_POINT('Ctrl Pts',(62.169448912385,-514.398533506753,25.));
#273938=CARTESIAN_POINT('Ctrl Pts',(60.169448912385,-514.398533506753,25.));
#273939=CARTESIAN_POINT('Origin',(39.830664447451,-620.152805159724,304.));
#273940=CARTESIAN_POINT('Origin',(39.830664447451,-620.152805159724,30.));
#273941=CARTESIAN_POINT('',(40.6681676180112,-625.082165000443,299.));
#273942=CARTESIAN_POINT('Origin',(39.830664447451,-620.152805159724,299.));
#273943=CARTESIAN_POINT('Ctrl Pts',(40.6681676180112,-625.082165000443,
299.));
#273944=CARTESIAN_POINT('Ctrl Pts',(40.5568123862982,-625.101084365763,
299.));
#273945=CARTESIAN_POINT('Ctrl Pts',(40.4451315445969,-625.116181235656,
299.000322224733));
#273946=CARTESIAN_POINT('Ctrl Pts',(40.3331319375785,-625.127493735038,
299.000707767503));
#273947=CARTESIAN_POINT('Ctrl Pts',(40.221073548286,-625.138812171713,299.001093512622));
#273948=CARTESIAN_POINT('Ctrl Pts',(40.1086953597897,-625.146342339687,
299.001542642259));
#273949=CARTESIAN_POINT('Ctrl Pts',(39.9959972959025,-625.150070917038,
299.001795841848));
#273950=CARTESIAN_POINT('Ctrl Pts',(39.9409626133207,-625.151891720908,
299.001919488684));
#273951=CARTESIAN_POINT('Ctrl Pts',(39.8858516096048,-625.152805159724,
299.001996411407));
#273952=CARTESIAN_POINT('Ctrl Pts',(39.830664447451,-625.152805159724,299.001996411407));
#273953=CARTESIAN_POINT('Origin',(-39.830664447451,-620.152805159724,304.));
#273954=CARTESIAN_POINT('Origin',(-39.830664447451,-620.152805159724,30.));
#273955=CARTESIAN_POINT('',(-40.6681676180112,-625.082165000443,299.));
#273956=CARTESIAN_POINT('Ctrl Pts',(-39.830664447451,-625.152805159724,
299.001996411407));
#273957=CARTESIAN_POINT('Ctrl Pts',(-39.9432259736778,-625.152805159724,
299.001996411407));
#273958=CARTESIAN_POINT('Ctrl Pts',(-40.055467122883,-625.149008478778,
299.001676420839));
#273959=CARTESIAN_POINT('Ctrl Pts',(-40.1673902027881,-625.141453851072,
299.001292658354));
#273960=CARTESIAN_POINT('Ctrl Pts',(-40.2793727095621,-625.133895212148,
299.000908692105));
#273961=CARTESIAN_POINT('Ctrl Pts',(-40.3910375070763,-625.122574592185,
299.000460886201));
#273962=CARTESIAN_POINT('Ctrl Pts',(-40.5023851435054,-625.107478842873,
299.000205867636));
#273963=CARTESIAN_POINT('Ctrl Pts',(-40.5577247055267,-625.09997628438,
299.000079123898));
#273964=CARTESIAN_POINT('Ctrl Pts',(-40.6129858337698,-625.091540440815,
299.));
#273965=CARTESIAN_POINT('Ctrl Pts',(-40.6681676180113,-625.082165000443,
299.));
#273966=CARTESIAN_POINT('Origin',(-39.830664447451,-620.152805159724,299.));
#273967=CARTESIAN_POINT('Origin',(39.830664447451,-541.923394840277,304.));
#273968=CARTESIAN_POINT('Origin',(39.830664447451,-541.923394840277,30.));
#273969=CARTESIAN_POINT('',(40.6681676180112,-536.994034999557,299.));
#273970=CARTESIAN_POINT('Ctrl Pts',(39.830664447451,-536.923394840277,299.001996411407));
#273971=CARTESIAN_POINT('Ctrl Pts',(39.9432259736786,-536.923394840277,
299.001996411407));
#273972=CARTESIAN_POINT('Ctrl Pts',(40.0554671228846,-536.927191521222,
299.001676420839));
#273973=CARTESIAN_POINT('Ctrl Pts',(40.1673902027906,-536.934746148928,
299.001292658354));
#273974=CARTESIAN_POINT('Ctrl Pts',(40.279372709565,-536.942304787853,299.000908692105));
#273975=CARTESIAN_POINT('Ctrl Pts',(40.3910375070795,-536.953625407815,
299.000460886201));
#273976=CARTESIAN_POINT('Ctrl Pts',(40.502385143509,-536.968721157128,299.000205867636));
#273977=CARTESIAN_POINT('Ctrl Pts',(40.557724705529,-536.97622371562,299.000079123898));
#273978=CARTESIAN_POINT('Ctrl Pts',(40.6129858337709,-536.984659559185,
299.));
#273979=CARTESIAN_POINT('Ctrl Pts',(40.6681676180112,-536.994034999557,
299.));
#273980=CARTESIAN_POINT('Origin',(39.830664447451,-541.923394840277,299.));
#273981=CARTESIAN_POINT('Origin',(-39.830664447451,-541.923394840277,304.));
#273982=CARTESIAN_POINT('Origin',(-39.830664447451,-541.923394840277,30.));
#273983=CARTESIAN_POINT('',(-40.6681676180112,-536.994034999557,299.));
#273984=CARTESIAN_POINT('Origin',(-39.830664447451,-541.923394840277,299.));
#273985=CARTESIAN_POINT('Ctrl Pts',(-40.6681676180112,-536.994034999557,
299.));
#273986=CARTESIAN_POINT('Ctrl Pts',(-40.5568123862973,-536.975115634237,
299.));
#273987=CARTESIAN_POINT('Ctrl Pts',(-40.4451315445951,-536.960018764344,
299.000322224733));
#273988=CARTESIAN_POINT('Ctrl Pts',(-40.3331319375757,-536.948706264962,
299.000707767503));
#273989=CARTESIAN_POINT('Ctrl Pts',(-40.221073548282,-536.937387828287,
299.001093512622));
#273990=CARTESIAN_POINT('Ctrl Pts',(-40.1086953597845,-536.929857660313,
299.001542642259));
#273991=CARTESIAN_POINT('Ctrl Pts',(-39.9959972958961,-536.926129082962,
299.001795841848));
#273992=CARTESIAN_POINT('Ctrl Pts',(-39.9409626133164,-536.924308279092,
299.001919488684));
#273993=CARTESIAN_POINT('Ctrl Pts',(-39.8858516096027,-536.923394840277,
299.001996411407));
#273994=CARTESIAN_POINT('Ctrl Pts',(-39.830664447451,-536.923394840277,
299.001996411407));
#273995=CARTESIAN_POINT('Origin',(53.6812599743419,-532.064675158837,346.));
#273996=CARTESIAN_POINT('',(53.6812599743419,-532.064675158837,346.));
#273997=CARTESIAN_POINT('',(53.6812599743419,-532.064675158837,346.));
#273998=CARTESIAN_POINT('',(53.6812599743419,-630.011524841163,346.));
#273999=CARTESIAN_POINT('',(53.6812599743419,-532.064675158837,346.));
#274000=CARTESIAN_POINT('',(53.6812599743419,-630.011524841163,346.));
#274001=CARTESIAN_POINT('Origin',(-53.681259974342,-532.064675158837,346.));
#274002=CARTESIAN_POINT('',(39.830664447451,-532.064675158837,304.));
#274003=CARTESIAN_POINT('',(-53.681259974342,-532.064675158837,304.));
#274004=CARTESIAN_POINT('',(-39.830664447451,-532.064675158837,304.));
#274005=CARTESIAN_POINT('',(-53.681259974342,-532.064675158837,304.));
#274006=CARTESIAN_POINT('',(-41.5056707885714,-532.064675158837,304.));
#274007=CARTESIAN_POINT('',(-53.681259974342,-532.064675158837,304.));
#274008=CARTESIAN_POINT('',(-53.681259974342,-532.064675158837,304.));
#274009=CARTESIAN_POINT('',(-53.681259974342,-532.064675158837,304.));
#274010=CARTESIAN_POINT('',(-53.681259974342,-532.064675158837,346.));
#274011=CARTESIAN_POINT('',(-53.681259974342,-532.064675158837,346.));
#274012=CARTESIAN_POINT('',(-53.681259974342,-532.064675158837,346.));
#274013=CARTESIAN_POINT('Origin',(-53.681259974342,-532.064675158837,346.));
#274014=CARTESIAN_POINT('',(-53.681259974342,-630.011524841163,304.));
#274015=CARTESIAN_POINT('',(-53.681259974342,-532.064675158837,304.));
#274016=CARTESIAN_POINT('',(-53.681259974342,-630.011524841163,346.));
#274017=CARTESIAN_POINT('',(-53.681259974342,-630.011524841163,346.));
#274018=CARTESIAN_POINT('',(-53.681259974342,-532.064675158837,346.));
#274019=CARTESIAN_POINT('Origin',(-53.681259974342,-630.011524841163,346.));
#274020=CARTESIAN_POINT('',(-41.5056707885714,-630.011524841163,304.));
#274021=CARTESIAN_POINT('',(-53.681259974342,-630.011524841163,304.));
#274022=CARTESIAN_POINT('',(-39.830664447451,-630.011524841163,304.));
#274023=CARTESIAN_POINT('',(-53.681259974342,-630.011524841163,304.));
#274024=CARTESIAN_POINT('',(39.830664447451,-630.011524841163,304.));
#274025=CARTESIAN_POINT('',(-53.681259974342,-630.011524841163,304.));
#274026=CARTESIAN_POINT('',(-53.681259974342,-630.011524841163,304.));
#274027=CARTESIAN_POINT('',(-53.681259974342,-630.011524841163,346.));
#274028=CARTESIAN_POINT('Origin',(0.,0.,304.));
#274029=CARTESIAN_POINT('',(-49.830664447451,-541.923394840277,304.));
#274030=CARTESIAN_POINT('',(-49.830664447451,-620.152805159724,304.));
#274031=CARTESIAN_POINT('',(-49.830664447451,-620.152805159724,304.));
#274032=CARTESIAN_POINT('Origin',(-39.830664447451,-620.152805159724,304.));
#274033=CARTESIAN_POINT('Origin',(-39.830664447451,-541.923394840277,304.));
#274034=CARTESIAN_POINT('Origin',(-39.830664447451,-620.152805159724,30.));
#274035=CARTESIAN_POINT('Origin',(-39.830664447451,-630.152805159724,30.));
#274036=CARTESIAN_POINT('Origin',(-49.830664447451,-620.152805159724,30.));
#274037=CARTESIAN_POINT('Origin',(-49.830664447451,-536.923394840277,30.));
#274038=CARTESIAN_POINT('Origin',(-49.830664447451,-541.923394840277,30.));
#274039=CARTESIAN_POINT('Origin',(-44.830664447451,-630.152805159724,30.));
#274040=CARTESIAN_POINT('Origin',(39.830664447451,-630.152805159724,30.));
#274041=CARTESIAN_POINT('Origin',(-39.830664447451,-541.923394840277,30.));
#274042=CARTESIAN_POINT('Origin',(-39.830664447451,-531.923394840277,30.));
#274043=CARTESIAN_POINT('Origin',(39.830664447451,-620.152805159724,30.));
#274044=CARTESIAN_POINT('Origin',(49.830664447451,-620.152805159724,30.));
#274045=CARTESIAN_POINT('Origin',(-44.830664447451,-531.923394840277,30.));
#274046=CARTESIAN_POINT('Origin',(39.830664447451,-531.923394840277,30.));
#274047=CARTESIAN_POINT('Origin',(49.830664447451,-536.923394840277,30.));
#274048=CARTESIAN_POINT('Origin',(49.830664447451,-541.923394840277,30.));
#274049=CARTESIAN_POINT('Origin',(39.830664447451,-541.923394840277,30.));
#274050=CARTESIAN_POINT('Origin',(-39.830664447451,-620.152805159724,299.));
#274051=CARTESIAN_POINT('Origin',(-49.830664447451,-620.152805159724,299.));
#274052=CARTESIAN_POINT('Origin',(-41.5056707885714,-630.011524841163,299.));
#274053=CARTESIAN_POINT('Ctrl Pts',(-39.830664447451,-625.152805159724,
299.001996411407));
#274054=CARTESIAN_POINT('Ctrl Pts',(-39.830664447451,-625.152805159724,
303.862656868443));
#274055=CARTESIAN_POINT('Ctrl Pts',(-39.830664447451,-630.011524841163,
304.));
#274056=CARTESIAN_POINT('Ctrl Pts',(-40.1099566802916,-625.152805159724,
299.001996411454));
#274057=CARTESIAN_POINT('Ctrl Pts',(-40.1174997460946,-625.152805159662,
303.862656868474));
#274058=CARTESIAN_POINT('Ctrl Pts',(-40.3892847158792,-630.011524841163,
304.));
#274059=CARTESIAN_POINT('Ctrl Pts',(-40.389168630662,-625.129567207634,
299.000000001807));
#274060=CARTESIAN_POINT('Ctrl Pts',(-40.4072487687408,-625.126495377405,
303.907395550511));
#274061=CARTESIAN_POINT('Ctrl Pts',(-40.9476251437622,-630.011524841163,
304.));
#274062=CARTESIAN_POINT('Ctrl Pts',(-40.6681676180112,-625.082165000443,
299.));
#274063=CARTESIAN_POINT('Ctrl Pts',(-40.6681676180112,-625.082165000443,
304.));
#274064=CARTESIAN_POINT('Ctrl Pts',(-41.5056707885714,-630.011524841163,
304.));
#274065=CARTESIAN_POINT('Origin',(-39.830664447451,-630.152805159724,299.001996411407));
#274066=CARTESIAN_POINT('Origin',(-49.830664447451,0.,299.));
#274067=CARTESIAN_POINT('Origin',(-49.830664447451,-541.923394840277,299.));
#274068=CARTESIAN_POINT('Origin',(0.,-630.152805159724,299.001996411407));
#274069=CARTESIAN_POINT('Origin',(39.830664447451,-630.152805159724,299.001996411407));
#274070=CARTESIAN_POINT('Origin',(-39.830664447451,-541.923394840277,299.));
#274071=CARTESIAN_POINT('Origin',(-41.5056707885714,-532.064675158837,299.));
#274072=CARTESIAN_POINT('Ctrl Pts',(39.830664447451,-630.011524841163,304.));
#274073=CARTESIAN_POINT('Ctrl Pts',(39.830664447451,-625.152805159724,303.862656868443));
#274074=CARTESIAN_POINT('Ctrl Pts',(39.830664447451,-625.152805159724,299.001996411407));
#274075=CARTESIAN_POINT('Ctrl Pts',(40.3892847158792,-630.011524841165,
304.));
#274076=CARTESIAN_POINT('Ctrl Pts',(40.1174997461169,-625.152805159662,
303.862656868536));
#274077=CARTESIAN_POINT('Ctrl Pts',(40.1099566802917,-625.152805159724,
299.001996411454));
#274078=CARTESIAN_POINT('Ctrl Pts',(40.9476251437621,-630.011524841163,
304.));
#274079=CARTESIAN_POINT('Ctrl Pts',(40.4072487687113,-625.126495377409,
303.907395550502));
#274080=CARTESIAN_POINT('Ctrl Pts',(40.3891686306619,-625.129567207634,
299.000000001807));
#274081=CARTESIAN_POINT('Ctrl Pts',(41.5056707885714,-630.011524841163,
304.));
#274082=CARTESIAN_POINT('Ctrl Pts',(40.6681676180112,-625.082165000443,
304.));
#274083=CARTESIAN_POINT('Ctrl Pts',(40.6681676180112,-625.082165000443,
299.));
#274084=CARTESIAN_POINT('Origin',(41.5056707885714,-630.011524841163,299.));
#274085=CARTESIAN_POINT('Ctrl Pts',(-39.830664447451,-532.064675158837,
304.));
#274086=CARTESIAN_POINT('Ctrl Pts',(-39.830664447451,-536.923394840277,
303.862656868443));
#274087=CARTESIAN_POINT('Ctrl Pts',(-39.830664447451,-536.923394840277,
299.001996411407));
#274088=CARTESIAN_POINT('Ctrl Pts',(-40.3892847158792,-532.064675158837,
304.));
#274089=CARTESIAN_POINT('Ctrl Pts',(-40.117499746096,-536.923394840339,
303.862656868474));
#274090=CARTESIAN_POINT('Ctrl Pts',(-40.1099566802916,-536.923394840277,
299.001996411454));
#274091=CARTESIAN_POINT('Ctrl Pts',(-40.9476251437622,-532.064675158837,
304.));
#274092=CARTESIAN_POINT('Ctrl Pts',(-40.4072487687389,-536.949704622596,
303.907395550513));
#274093=CARTESIAN_POINT('Ctrl Pts',(-40.389168630662,-536.946632792366,
299.000000001807));
#274094=CARTESIAN_POINT('Ctrl Pts',(-41.5056707885714,-532.064675158837,
304.));
#274095=CARTESIAN_POINT('Ctrl Pts',(-40.6681676180112,-536.994034999557,
304.));
#274096=CARTESIAN_POINT('Ctrl Pts',(-40.6681676180112,-536.994034999557,
299.));
#274097=CARTESIAN_POINT('Origin',(-39.830664447451,-531.923394840277,299.001996411407));
#274098=CARTESIAN_POINT('Origin',(39.830664447451,-620.152805159724,299.));
#274099=CARTESIAN_POINT('Origin',(49.830664447451,-620.152805159724,299.));
#274100=CARTESIAN_POINT('Origin',(0.,-531.923394840277,299.001996411407));
#274101=CARTESIAN_POINT('Origin',(39.830664447451,-531.923394840277,299.001996411407));
#274102=CARTESIAN_POINT('Origin',(49.830664447451,0.,299.));
#274103=CARTESIAN_POINT('Origin',(49.830664447451,-541.923394840277,299.));
#274104=CARTESIAN_POINT('Ctrl Pts',(39.830664447451,-536.923394840277,299.001996411407));
#274105=CARTESIAN_POINT('Ctrl Pts',(39.830664447451,-536.923394840277,303.862656868443));
#274106=CARTESIAN_POINT('Ctrl Pts',(39.830664447451,-532.064675158837,304.));
#274107=CARTESIAN_POINT('Ctrl Pts',(40.1099566802915,-536.923394840277,
299.001996411454));
#274108=CARTESIAN_POINT('Ctrl Pts',(40.117499746096,-536.923394840339,303.862656868474));
#274109=CARTESIAN_POINT('Ctrl Pts',(40.3892847158792,-532.064675158837,
304.));
#274110=CARTESIAN_POINT('Ctrl Pts',(40.389168630662,-536.946632792366,299.000000001807));
#274111=CARTESIAN_POINT('Ctrl Pts',(40.4072487687388,-536.949704622596,
303.907395550513));
#274112=CARTESIAN_POINT('Ctrl Pts',(40.9476251437621,-532.064675158837,
304.));
#274113=CARTESIAN_POINT('Ctrl Pts',(40.6681676180112,-536.994034999557,
299.));
#274114=CARTESIAN_POINT('Ctrl Pts',(40.6681676180112,-536.994034999557,
304.));
#274115=CARTESIAN_POINT('Ctrl Pts',(41.5056707885714,-532.064675158837,
304.));
#274116=CARTESIAN_POINT('Origin',(41.5056707885714,-532.064675158837,299.));
#274117=CARTESIAN_POINT('Origin',(39.830664447451,-541.923394840277,299.));
#274118=CARTESIAN_POINT('Origin',(0.,0.,346.));
#274119=CARTESIAN_POINT('',(60.9525837346152,-637.028433422628,346.));
#274120=CARTESIAN_POINT('',(60.9525837346152,-525.047766577373,346.));
#274121=CARTESIAN_POINT('',(60.9525837346152,-525.047766577373,346.));
#274122=CARTESIAN_POINT('',(-60.9525837346153,-637.028433422628,346.));
#274123=CARTESIAN_POINT('',(-60.9525837346153,-637.028433422628,346.));
#274124=CARTESIAN_POINT('',(-60.9525837346153,-525.047766577373,346.));
#274125=CARTESIAN_POINT('',(-60.9525837346153,-525.047766577373,346.));
#274126=CARTESIAN_POINT('',(-60.9525837346153,-525.047766577373,346.));
#274127=CARTESIAN_POINT('Origin',(60.9525837346152,-525.047766577373,356.));
#274128=CARTESIAN_POINT('',(60.9525837346152,-525.047766577373,356.));
#274129=CARTESIAN_POINT('',(60.9525837346152,-525.047766577373,356.));
#274130=CARTESIAN_POINT('',(60.9525837346152,-637.028433422628,356.));
#274131=CARTESIAN_POINT('',(60.9525837346152,-525.047766577373,356.));
#274132=CARTESIAN_POINT('',(60.9525837346152,-637.028433422628,356.));
#274133=CARTESIAN_POINT('Origin',(-60.9525837346153,-525.047766577373,356.));
#274134=CARTESIAN_POINT('',(-60.9525837346153,-525.047766577373,356.));
#274135=CARTESIAN_POINT('',(-60.9525837346153,-525.047766577373,356.));
#274136=CARTESIAN_POINT('',(-60.9525837346153,-525.047766577373,356.));
#274137=CARTESIAN_POINT('Origin',(-60.9525837346153,-525.047766577373,356.));
#274138=CARTESIAN_POINT('',(-60.9525837346153,-637.028433422628,356.));
#274139=CARTESIAN_POINT('',(-60.9525837346153,-637.028433422628,356.));
#274140=CARTESIAN_POINT('',(-60.9525837346153,-525.047766577373,356.));
#274141=CARTESIAN_POINT('Origin',(-60.9525837346153,-637.028433422628,356.));
#274142=CARTESIAN_POINT('',(-60.9525837346153,-637.028433422628,356.));
#274143=CARTESIAN_POINT('Origin',(0.,0.,356.));
#274144=CARTESIAN_POINT('Origin',(65.169448912385,-550.402639059603,-15.));
#274145=CARTESIAN_POINT('',(65.169448912385,-550.402639059603,-15.));
#274146=CARTESIAN_POINT('Origin',(-60.,-516.398533506753,-15.));
#274147=CARTESIAN_POINT('Origin',(65.169448912385,-614.173929613455,-15.));
#274148=CARTESIAN_POINT('',(65.169448912385,-614.173929613455,-15.));
#274149=CARTESIAN_POINT('Origin',(-60.,-647.946325817004,-15.));
#274150=CARTESIAN_POINT('',(0.,0.,0.));
#274151=CARTESIAN_POINT('Origin',(-27.0086446004716,-26.9913553995289,910.));
#274152=CARTESIAN_POINT('',(-32.6729361631489,-24.2334937110131,1282.35584962783));
#274153=CARTESIAN_POINT('',(-32.6729361631488,-29.7492170880442,1282.35584962783));
#274154=CARTESIAN_POINT('Origin',(-27.0086446004717,-26.991355399529,1282.35584962783));
#274155=CARTESIAN_POINT('',(-32.6729361631488,-29.7492170880442,-260.));
#274156=CARTESIAN_POINT('',(-32.672936163149,-29.7492170880444,910.));
#274157=CARTESIAN_POINT('',(-32.6729361631487,-24.233493711013,-260.));
#274158=CARTESIAN_POINT('Origin',(-27.0086446004714,-26.9913553995287,-260.));
#274159=CARTESIAN_POINT('',(-32.6729361631489,-24.2334937110132,910.));
#274160=CARTESIAN_POINT('Origin',(0.,0.,-260.));
#274161=CARTESIAN_POINT('',(-35.1310673206098,-32.6891089669783,-260.));
#274162=CARTESIAN_POINT('',(-32.706398167921,-35.1137781196668,-260.));
#274163=CARTESIAN_POINT('Origin',(-27.0086446004714,-26.9913553995287,-260.));
#274164=CARTESIAN_POINT('',(-29.7665062889871,-32.655646962206,-260.));
#274165=CARTESIAN_POINT('',(-32.706398167921,-35.1137781196668,-260.));
#274166=CARTESIAN_POINT('',(-24.2507829119558,-32.6556469622061,-260.));
#274167=CARTESIAN_POINT('Origin',(-27.0086446004714,-26.9913553995287,-260.));
#274168=CARTESIAN_POINT('',(-21.3108910330219,-35.1137781196669,-260.));
#274169=CARTESIAN_POINT('',(-21.3108910330219,-35.1137781196669,-260.));
#274170=CARTESIAN_POINT('',(-18.8862218803333,-32.6891089669783,-260.));
#274171=CARTESIAN_POINT('Origin',(-27.0086446004714,-26.9913553995287,-260.));
#274172=CARTESIAN_POINT('',(-21.3443530377941,-29.7492170880443,-260.));
#274173=CARTESIAN_POINT('',(-18.8862218803333,-32.6891089669783,-260.));
#274174=CARTESIAN_POINT('',(-21.344353037794,-24.2334937110131,-260.));
#274175=CARTESIAN_POINT('Origin',(-27.0086446004714,-26.9913553995287,-260.));
#274176=CARTESIAN_POINT('',(-18.8862218803333,-21.2936018320792,-260.));
#274177=CARTESIAN_POINT('',(-18.8862218803333,-21.2936018320792,-260.));
#274178=CARTESIAN_POINT('',(-21.3108910330219,-18.8689326793906,-260.));
#274179=CARTESIAN_POINT('Origin',(-27.0086446004714,-26.9913553995287,-260.));
#274180=CARTESIAN_POINT('',(-24.2507829119558,-21.3270638368514,-260.));
#274181=CARTESIAN_POINT('',(-21.3108910330219,-18.8689326793906,-260.));
#274182=CARTESIAN_POINT('',(-29.7665062889869,-21.3270638368513,-260.));
#274183=CARTESIAN_POINT('Origin',(-27.0086446004714,-26.9913553995287,-260.));
#274184=CARTESIAN_POINT('',(-32.7063981679207,-18.8689326793905,-260.));
#274185=CARTESIAN_POINT('',(-32.7063981679207,-18.8689326793905,-260.));
#274186=CARTESIAN_POINT('',(-35.1310673206094,-21.293601832079,-260.));
#274187=CARTESIAN_POINT('Origin',(-27.0086446004714,-26.9913553995287,-260.));
#274188=CARTESIAN_POINT('',(-35.1310673206094,-21.293601832079,-260.));
#274189=CARTESIAN_POINT('',(-35.1310673206096,-32.6891089669781,-260.));
#274190=CARTESIAN_POINT('Origin',(-35.1310673206098,-32.6891089669783,910.));
#274191=CARTESIAN_POINT('',(-35.1310673206099,-32.6891089669784,1282.35584962783));
#274192=CARTESIAN_POINT('',(-35.1310673206098,-32.6891089669783,1282.35584962783));
#274193=CARTESIAN_POINT('',(-35.1310673206098,-32.6891089669783,910.));
#274194=CARTESIAN_POINT('Origin',(-35.1310673206096,-21.2936018320792,910.));
#274195=CARTESIAN_POINT('',(-35.1310673206099,-21.293601832079,1282.35584962783));
#274196=CARTESIAN_POINT('',(-35.1310673206096,-21.2936018320792,910.));
#274197=CARTESIAN_POINT('',(-35.1310673206097,-21.2936018320793,1282.35584962783));
#274198=CARTESIAN_POINT('Origin',(-27.0086446004716,-26.9913553995289,910.));
#274199=CARTESIAN_POINT('',(-32.7063981679208,-18.8689326793906,1282.35584962783));
#274200=CARTESIAN_POINT('',(-32.7063981679209,-18.8689326793907,910.));
#274201=CARTESIAN_POINT('Origin',(-27.0086446004717,-26.991355399529,1282.35584962783));
#274202=CARTESIAN_POINT('Origin',(-32.7063981679209,-18.8689326793907,910.));
#274203=CARTESIAN_POINT('',(-29.7665062889869,-21.3270638368518,1282.35584962783));
#274204=CARTESIAN_POINT('',(-29.7665062889871,-21.3270638368515,910.));
#274205=CARTESIAN_POINT('',(-32.706398167921,-18.8689326793908,1282.35584962783));
#274206=CARTESIAN_POINT('Origin',(-27.0086446004716,-26.9913553995289,910.));
#274207=CARTESIAN_POINT('',(-24.250782911956,-21.3270638368517,1282.35584962783));
#274208=CARTESIAN_POINT('',(-24.250782911956,-21.3270638368516,910.));
#274209=CARTESIAN_POINT('Origin',(-27.0086446004717,-26.991355399529,1282.35584962783));
#274210=CARTESIAN_POINT('Origin',(-21.3108910330221,-18.8689326793908,910.));
#274211=CARTESIAN_POINT('',(-21.3108910330219,-18.8689326793906,1282.35584962783));
#274212=CARTESIAN_POINT('',(-21.3108910330221,-18.8689326793908,910.));
#274213=CARTESIAN_POINT('',(-21.3108910330221,-18.8689326793908,1282.35584962783));
#274214=CARTESIAN_POINT('Origin',(-27.0086446004716,-26.9913553995289,910.));
#274215=CARTESIAN_POINT('',(-18.8862218803336,-21.2936018320794,1282.35584962783));
#274216=CARTESIAN_POINT('',(-18.8862218803335,-21.2936018320794,910.));
#274217=CARTESIAN_POINT('Origin',(-27.0086446004717,-26.991355399529,1282.35584962783));
#274218=CARTESIAN_POINT('Origin',(-18.8862218803335,-21.2936018320794,910.));
#274219=CARTESIAN_POINT('',(-21.3443530377943,-24.2334937110133,1282.35584962783));
#274220=CARTESIAN_POINT('',(-21.3443530377943,-24.2334937110133,910.));
#274221=CARTESIAN_POINT('',(-18.8862218803335,-21.2936018320794,1282.35584962783));
#274222=CARTESIAN_POINT('Origin',(-27.0086446004716,-26.9913553995289,910.));
#274223=CARTESIAN_POINT('',(-21.3443530377942,-29.7492170880444,1282.35584962783));
#274224=CARTESIAN_POINT('',(-21.3443530377943,-29.7492170880446,910.));
#274225=CARTESIAN_POINT('Origin',(-27.0086446004717,-26.991355399529,1282.35584962783));
#274226=CARTESIAN_POINT('Origin',(-18.8862218803335,-32.6891089669785,910.));
#274227=CARTESIAN_POINT('',(-18.8862218803336,-32.6891089669785,1282.35584962783));
#274228=CARTESIAN_POINT('',(-18.8862218803335,-32.6891089669785,910.));
#274229=CARTESIAN_POINT('',(-18.8862218803336,-32.6891089669786,1282.35584962783));
#274230=CARTESIAN_POINT('Origin',(-27.0086446004716,-26.9913553995289,910.));
#274231=CARTESIAN_POINT('',(-21.310891033022,-35.113778119667,1282.35584962783));
#274232=CARTESIAN_POINT('',(-21.3108910330221,-35.1137781196671,910.));
#274233=CARTESIAN_POINT('Origin',(-27.0086446004717,-26.991355399529,1282.35584962783));
#274234=CARTESIAN_POINT('Origin',(-21.3108910330221,-35.1137781196671,910.));
#274235=CARTESIAN_POINT('',(-24.2507829119561,-32.6556469622064,1282.35584962783));
#274236=CARTESIAN_POINT('',(-24.2507829119561,-32.6556469622063,910.));
#274237=CARTESIAN_POINT('',(-21.3108910330222,-35.1137781196672,1282.35584962783));
#274238=CARTESIAN_POINT('Origin',(-27.0086446004716,-26.9913553995289,910.));
#274239=CARTESIAN_POINT('',(-29.7665062889873,-32.6556469622064,1282.35584962783));
#274240=CARTESIAN_POINT('',(-29.7665062889873,-32.6556469622062,910.));
#274241=CARTESIAN_POINT('Origin',(-27.0086446004717,-26.991355399529,1282.35584962783));
#274242=CARTESIAN_POINT('Origin',(-32.7063981679213,-35.113778119667,910.));
#274243=CARTESIAN_POINT('',(-32.7063981679213,-35.113778119667,1282.35584962783));
#274244=CARTESIAN_POINT('',(-32.7063981679213,-35.113778119667,910.));
#274245=CARTESIAN_POINT('',(-32.7063981679212,-35.113778119667,1282.35584962783));
#274246=CARTESIAN_POINT('Origin',(-27.0086446004716,-26.9913553995289,910.));
#274247=CARTESIAN_POINT('Origin',(-27.0086446004717,-26.991355399529,1282.35584962783));
#274248=CARTESIAN_POINT('Origin',(0.,0.,1282.35584962783));
#274249=CARTESIAN_POINT('Origin',(0.,0.,-260.));
#274250=CARTESIAN_POINT('',(-45.9014446004718,-51.6603553995284,-260.));
#274251=CARTESIAN_POINT('',(-44.1014446004718,-49.8603553995284,-260.));
#274252=CARTESIAN_POINT('Origin',(-45.9014446004718,-49.8603553995284,-260.));
#274253=CARTESIAN_POINT('',(-44.1014446004717,-45.8841553995285,-260.));
#274254=CARTESIAN_POINT('',(-44.1014446004718,-49.8603553995284,-260.));
#274255=CARTESIAN_POINT('',(-45.9014446004717,-44.0841553995285,-260.));
#274256=CARTESIAN_POINT('Origin',(-45.9014446004717,-45.8841553995285,-260.));
#274257=CARTESIAN_POINT('',(-49.8776446004716,-44.0841553995285,-260.));
#274258=CARTESIAN_POINT('',(-45.9014446004717,-44.0841553995285,-260.));
#274259=CARTESIAN_POINT('',(-51.6776446004716,-45.8841553995285,-260.));
#274260=CARTESIAN_POINT('Origin',(-49.8776446004716,-45.8841553995285,-260.));
#274261=CARTESIAN_POINT('',(-51.6776446004716,-49.8603553995283,-260.));
#274262=CARTESIAN_POINT('',(-51.6776446004716,-45.8841553995285,-260.));
#274263=CARTESIAN_POINT('',(-49.8776446004716,-51.6603553995283,-260.));
#274264=CARTESIAN_POINT('Origin',(-49.8776446004716,-49.8603553995283,-260.));
#274265=CARTESIAN_POINT('',(-49.8776446004716,-51.6603553995283,-260.));
#274266=CARTESIAN_POINT('Origin',(-49.8776446004719,-51.6603553995285,910.));
#274267=CARTESIAN_POINT('',(-49.8776446004719,-51.6603553995286,1282.35584962783));
#274268=CARTESIAN_POINT('',(-49.8776446004719,-51.6603553995285,910.));
#274269=CARTESIAN_POINT('',(-45.9014446004721,-51.6603553995287,1282.35584962783));
#274270=CARTESIAN_POINT('',(-49.8776446004719,-51.6603553995286,1282.35584962783));
#274271=CARTESIAN_POINT('',(-45.901444600472,-51.6603553995286,910.));
#274272=CARTESIAN_POINT('Origin',(-49.8776446004718,-49.8603553995285,910.));
#274273=CARTESIAN_POINT('',(-51.6776446004719,-49.8603553995284,1282.35584962783));
#274274=CARTESIAN_POINT('',(-51.6776446004718,-49.8603553995285,910.));
#274275=CARTESIAN_POINT('Origin',(-49.8776446004719,-49.8603553995286,1282.35584962783));
#274276=CARTESIAN_POINT('Origin',(-51.6776446004718,-45.8841553995287,910.));
#274277=CARTESIAN_POINT('',(-51.6776446004719,-45.8841553995285,1282.35584962783));
#274278=CARTESIAN_POINT('',(-51.6776446004718,-45.8841553995287,910.));
#274279=CARTESIAN_POINT('',(-51.6776446004719,-45.8841553995287,1282.35584962783));
#274280=CARTESIAN_POINT('Origin',(-49.8776446004718,-45.8841553995287,910.));
#274281=CARTESIAN_POINT('',(-49.8776446004717,-44.0841553995288,1282.35584962783));
#274282=CARTESIAN_POINT('',(-49.8776446004718,-44.0841553995287,910.));
#274283=CARTESIAN_POINT('Origin',(-49.8776446004719,-45.8841553995288,1282.35584962783));
#274284=CARTESIAN_POINT('Origin',(-45.9014446004719,-44.0841553995287,910.));
#274285=CARTESIAN_POINT('',(-45.9014446004717,-44.0841553995288,1282.35584962783));
#274286=CARTESIAN_POINT('',(-45.9014446004719,-44.0841553995287,910.));
#274287=CARTESIAN_POINT('',(-45.9014446004719,-44.0841553995288,1282.35584962783));
#274288=CARTESIAN_POINT('Origin',(-45.901444600472,-45.8841553995287,910.));
#274289=CARTESIAN_POINT('',(-44.101444600472,-45.8841553995288,1282.35584962783));
#274290=CARTESIAN_POINT('',(-44.101444600472,-45.8841553995288,910.));
#274291=CARTESIAN_POINT('Origin',(-45.901444600472,-45.8841553995288,1282.35584962783));
#274292=CARTESIAN_POINT('Origin',(-44.101444600472,-49.8603553995286,910.));
#274293=CARTESIAN_POINT('',(-44.1014446004721,-49.8603553995286,1282.35584962783));
#274294=CARTESIAN_POINT('',(-44.101444600472,-49.8603553995286,910.));
#274295=CARTESIAN_POINT('',(-44.1014446004721,-49.8603553995286,1282.35584962783));
#274296=CARTESIAN_POINT('Origin',(-45.901444600472,-49.8603553995286,910.));
#274297=CARTESIAN_POINT('Origin',(-45.9014446004721,-49.8603553995287,1282.35584962783));
#274298=CARTESIAN_POINT('Origin',(0.,0.,1282.35584962783));
#274299=CARTESIAN_POINT('Origin',(0.,0.,1282.35584962783));
#274300=CARTESIAN_POINT('',(-48.3386446004713,-7.56935539952863,1282.35584962783));
#274301=CARTESIAN_POINT('',(-51.0386446004713,-4.8693553995284,1282.35584962783));
#274302=CARTESIAN_POINT('Origin',(-48.3386446004713,-4.86935539952863,1282.35584962783));
#274303=CARTESIAN_POINT('',(-51.0386446004713,4.88664460047119,1282.35584962783));
#274304=CARTESIAN_POINT('',(-51.0386446004713,4.88664460047119,1282.35584962783));
#274305=CARTESIAN_POINT('',(-48.3386446004713,7.58664460047119,1282.35584962783));
#274306=CARTESIAN_POINT('Origin',(-48.3386446004713,4.88664460047119,1282.35584962783));
#274307=CARTESIAN_POINT('',(-44.2652173270483,7.58664460047119,1282.35584962783));
#274308=CARTESIAN_POINT('',(-48.3386446004713,7.58664460047119,1282.35584962783));
#274309=CARTESIAN_POINT('',(-42.3560290178447,8.37745629126751,1282.35584962783));
#274310=CARTESIAN_POINT('Origin',(-44.2652173270483,10.2866446004712,1282.35584962783));
#274311=CARTESIAN_POINT('',(-35.3156523994373,15.4178329096749,1282.35584962783));
#274312=CARTESIAN_POINT('',(-42.3560290178447,8.37745629126751,1282.35584962783));
#274313=CARTESIAN_POINT('',(-33.4064640902336,16.2086446004712,1282.35584962783));
#274314=CARTESIAN_POINT('Origin',(-33.4064640902336,13.5086446004712,1282.35584962783));
#274315=CARTESIAN_POINT('',(-20.7806446004713,16.2086446004712,1282.35584962783));
#274316=CARTESIAN_POINT('',(-27.0086446004713,16.2086446004712,1282.35584962783));
#274317=CARTESIAN_POINT('',(-16.2086446004713,20.7806446004712,1282.35584962783));
#274318=CARTESIAN_POINT('',(-20.7806446004713,16.2086446004712,1282.35584962783));
#274319=CARTESIAN_POINT('',(-16.2086446004713,33.4064640902334,1282.35584962783));
#274320=CARTESIAN_POINT('',(-16.2086446004713,33.4064640902334,1282.35584962783));
#274321=CARTESIAN_POINT('',(-15.4178329096749,35.3156523994371,1282.35584962783));
#274322=CARTESIAN_POINT('Origin',(-13.5086446004713,33.4064640902334,1282.35584962783));
#274323=CARTESIAN_POINT('',(-8.37745629126753,42.3560290178444,1282.35584962783));
#274324=CARTESIAN_POINT('',(-8.37745629126753,42.3560290178444,1282.35584962783));
#274325=CARTESIAN_POINT('',(-7.58664460047119,44.2652173270481,1282.35584962783));
#274326=CARTESIAN_POINT('Origin',(-10.2866446004712,44.2652173270481,1282.35584962783));
#274327=CARTESIAN_POINT('',(-7.58664460047116,48.338644600471,1282.35584962783));
#274328=CARTESIAN_POINT('',(-7.58664460047116,48.338644600471,1282.35584962783));
#274329=CARTESIAN_POINT('',(-4.88664460047113,51.038644600471,1282.35584962783));
#274330=CARTESIAN_POINT('Origin',(-4.88664460047115,48.338644600471,1282.35584962783));
#274331=CARTESIAN_POINT('',(4.86935539952935,51.0386446004711,1282.35584962783));
#274332=CARTESIAN_POINT('',(-4.88664460047113,51.038644600471,1282.35584962783));
#274333=CARTESIAN_POINT('',(7.56935539952934,48.3386446004711,1282.35584962783));
#274334=CARTESIAN_POINT('Origin',(4.86935539952934,48.3386446004711,1282.35584962783));
#274335=CARTESIAN_POINT('',(7.56935539952933,44.2652173270481,1282.35584962783));
#274336=CARTESIAN_POINT('',(7.56935539952934,48.3386446004712,1282.35584962783));
#274337=CARTESIAN_POINT('',(8.36016709032564,42.3560290178444,1282.35584962783));
#274338=CARTESIAN_POINT('Origin',(10.2693553995293,44.2652173270481,1282.35584962783));
#274339=CARTESIAN_POINT('',(15.400543708733,35.315652399437,1282.35584962783));
#274340=CARTESIAN_POINT('',(8.36016709032557,42.3560290178445,1282.35584962783));
#274341=CARTESIAN_POINT('',(16.1913553995293,33.4064640902334,1282.35584962783));
#274342=CARTESIAN_POINT('Origin',(13.4913553995293,33.4064640902334,1282.35584962783));
#274343=CARTESIAN_POINT('',(16.1913553995292,20.7806446004711,1282.35584962783));
#274344=CARTESIAN_POINT('',(16.1913553995293,27.0086446004711,1282.35584962783));
#274345=CARTESIAN_POINT('',(20.7633553995292,16.208644600471,1282.35584962783));
#274346=CARTESIAN_POINT('',(16.1913553995292,20.7806446004711,1282.35584962783));
#274347=CARTESIAN_POINT('',(33.3891748892915,16.2086446004709,1282.35584962783));
#274348=CARTESIAN_POINT('',(33.3891748892914,16.2086446004709,1282.35584962783));
#274349=CARTESIAN_POINT('',(35.2983631984951,15.4178329096746,1282.35584962783));
#274350=CARTESIAN_POINT('Origin',(33.3891748892914,13.508644600471,1282.35584962783));
#274351=CARTESIAN_POINT('',(42.3387398169024,8.37745629126718,1282.35584962783));
#274352=CARTESIAN_POINT('',(42.3387398169023,8.37745629126725,1282.35584962783));
#274353=CARTESIAN_POINT('',(44.2479281261061,7.58664460047083,1282.35584962783));
#274354=CARTESIAN_POINT('Origin',(44.2479281261061,10.2866446004708,1282.35584962783));
#274355=CARTESIAN_POINT('',(48.321355399529,7.58664460047079,1282.35584962783));
#274356=CARTESIAN_POINT('',(48.321355399529,7.58664460047079,1282.35584962783));
#274357=CARTESIAN_POINT('',(51.021355399529,4.88664460047075,1282.35584962783));
#274358=CARTESIAN_POINT('Origin',(48.321355399529,4.88664460047079,1282.35584962783));
#274359=CARTESIAN_POINT('',(51.0213553995291,-4.86935539952937,1282.35584962783));
#274360=CARTESIAN_POINT('',(51.021355399529,4.88664460047082,1282.35584962783));
#274361=CARTESIAN_POINT('',(48.3213553995291,-7.56935539952937,1282.35584962783));
#274362=CARTESIAN_POINT('Origin',(48.3213553995291,-4.86935539952937,1282.35584962783));
#274363=CARTESIAN_POINT('',(44.2479281261061,-7.56935539952937,1282.35584962783));
#274364=CARTESIAN_POINT('',(48.3213553995291,-7.56935539952937,1282.35584962783));
#274365=CARTESIAN_POINT('',(42.3387398169024,-8.36016709032569,1282.35584962783));
#274366=CARTESIAN_POINT('Origin',(44.2479281261061,-10.2693553995294,1282.35584962783));
#274367=CARTESIAN_POINT('',(35.2983631984951,-15.400543708733,1282.35584962783));
#274368=CARTESIAN_POINT('',(42.3387398169025,-8.36016709032562,1282.35584962783));
#274369=CARTESIAN_POINT('',(33.3891748892914,-16.1913553995294,1282.35584962783));
#274370=CARTESIAN_POINT('Origin',(33.3891748892914,-13.4913553995294,1282.35584962783));
#274371=CARTESIAN_POINT('',(20.7633553995291,-16.1913553995294,1282.35584962783));
#274372=CARTESIAN_POINT('',(26.9913553995291,-16.1913553995294,1282.35584962783));
#274373=CARTESIAN_POINT('',(16.1913553995291,-20.7633553995294,1282.35584962783));
#274374=CARTESIAN_POINT('',(20.7633553995292,-16.1913553995293,1282.35584962783));
#274375=CARTESIAN_POINT('',(16.191355399529,-33.3891748892916,1282.35584962783));
#274376=CARTESIAN_POINT('',(16.191355399529,-33.3891748892915,1282.35584962783));
#274377=CARTESIAN_POINT('',(15.4005437087327,-35.2983631984953,1282.35584962783));
#274378=CARTESIAN_POINT('Origin',(13.491355399529,-33.3891748892916,1282.35584962783));
#274379=CARTESIAN_POINT('',(8.36016709032531,-42.3387398169026,1282.35584962783));
#274380=CARTESIAN_POINT('',(8.36016709032537,-42.3387398169025,1282.35584962783));
#274381=CARTESIAN_POINT('',(7.56935539952897,-44.2479281261063,1282.35584962783));
#274382=CARTESIAN_POINT('Origin',(10.269355399529,-44.2479281261063,1282.35584962783));
#274383=CARTESIAN_POINT('',(7.56935539952894,-48.3213553995292,1282.35584962783));
#274384=CARTESIAN_POINT('',(7.56935539952894,-48.3213553995291,1282.35584962783));
#274385=CARTESIAN_POINT('',(4.86935539952891,-51.0213553995292,1282.35584962783));
#274386=CARTESIAN_POINT('Origin',(4.86935539952893,-48.3213553995292,1282.35584962783));
#274387=CARTESIAN_POINT('',(-4.88664460047193,-51.0213553995292,1282.35584962783));
#274388=CARTESIAN_POINT('',(4.86935539952891,-51.0213553995292,1282.35584962783));
#274389=CARTESIAN_POINT('',(-7.5866446004719,-48.3213553995292,1282.35584962783));
#274390=CARTESIAN_POINT('Origin',(-4.8866446004719,-48.3213553995292,1282.35584962783));
#274391=CARTESIAN_POINT('',(-7.58664460047186,-44.2479281261062,1282.35584962783));
#274392=CARTESIAN_POINT('',(-7.5866446004719,-48.3213553995291,1282.35584962783));
#274393=CARTESIAN_POINT('',(-8.37745629126815,-42.3387398169026,1282.35584962783));
#274394=CARTESIAN_POINT('Origin',(-10.2866446004719,-44.2479281261062,1282.35584962783));
#274395=CARTESIAN_POINT('',(-15.4178329096754,-35.2983631984951,1282.35584962783));
#274396=CARTESIAN_POINT('',(-8.37745629126815,-42.3387398169026,1282.35584962783));
#274397=CARTESIAN_POINT('',(-16.2086446004717,-33.3891748892914,1282.35584962783));
#274398=CARTESIAN_POINT('Origin',(-13.5086446004717,-33.3891748892915,1282.35584962783));
#274399=CARTESIAN_POINT('',(-16.2086446004716,-20.7633553995291,1282.35584962783));
#274400=CARTESIAN_POINT('',(-16.2086446004717,-26.9913553995291,1282.35584962783));
#274401=CARTESIAN_POINT('',(-20.7806446004716,-16.1913553995291,1282.35584962783));
#274402=CARTESIAN_POINT('',(-16.2086446004716,-20.7633553995291,1282.35584962783));
#274403=CARTESIAN_POINT('',(-33.4064640902338,-16.1913553995289,1282.35584962783));
#274404=CARTESIAN_POINT('',(-33.4064640902337,-16.1913553995289,1282.35584962783));
#274405=CARTESIAN_POINT('',(-35.3156523994374,-15.4005437087325,1282.35584962783));
#274406=CARTESIAN_POINT('Origin',(-33.4064640902337,-13.4913553995289,1282.35584962783));
#274407=CARTESIAN_POINT('',(-42.3560290178447,-8.36016709032506,1282.35584962783));
#274408=CARTESIAN_POINT('',(-42.3560290178447,-8.36016709032506,1282.35584962783));
#274409=CARTESIAN_POINT('',(-44.2652173270483,-7.5693553995287,1282.35584962783));
#274410=CARTESIAN_POINT('Origin',(-44.2652173270484,-10.2693553995287,1282.35584962783));
#274411=CARTESIAN_POINT('',(-48.3386446004712,-7.56935539952863,1282.35584962783));
#274412=CARTESIAN_POINT('Origin',(0.,0.,-260.));
#274413=CARTESIAN_POINT('',(-51.0386446004713,4.88664460047119,-260.));
#274414=CARTESIAN_POINT('',(-48.3386446004713,7.58664460047119,-260.));
#274415=CARTESIAN_POINT('Origin',(-48.3386446004713,4.88664460047119,-260.));
#274416=CARTESIAN_POINT('',(-51.038644600471,-4.86935539952829,-260.));
#274417=CARTESIAN_POINT('',(-51.0386446004713,4.88664460047119,-260.));
#274418=CARTESIAN_POINT('',(-48.338644600471,-7.56935539952835,-260.));
#274419=CARTESIAN_POINT('Origin',(-48.338644600471,-4.86935539952834,-260.));
#274420=CARTESIAN_POINT('',(-44.2652173270481,-7.56935539952842,-260.));
#274421=CARTESIAN_POINT('',(-48.338644600471,-7.56935539952835,-260.));
#274422=CARTESIAN_POINT('',(-42.3560290178444,-8.36016709032478,-260.));
#274423=CARTESIAN_POINT('Origin',(-44.2652173270481,-10.2693553995284,-260.));
#274424=CARTESIAN_POINT('',(-35.3156523994372,-15.4005437087323,-260.));
#274425=CARTESIAN_POINT('',(-42.3560290178444,-8.36016709032478,-260.));
#274426=CARTESIAN_POINT('',(-33.4064640902335,-16.1913553995286,-260.));
#274427=CARTESIAN_POINT('Origin',(-33.4064640902334,-13.4913553995286,-260.));
#274428=CARTESIAN_POINT('',(-20.7806446004713,-16.1913553995288,-260.));
#274429=CARTESIAN_POINT('',(-33.4064640902335,-16.1913553995286,-260.));
#274430=CARTESIAN_POINT('',(-16.2086446004713,-20.7633553995288,-260.));
#274431=CARTESIAN_POINT('',(-16.2086446004713,-20.7633553995288,-260.));
#274432=CARTESIAN_POINT('',(-16.2086446004715,-33.3891748892914,-260.));
#274433=CARTESIAN_POINT('',(-16.2086446004714,-26.9913553995288,-260.));
#274434=CARTESIAN_POINT('',(-15.4178329096752,-35.2983631984948,-260.));
#274435=CARTESIAN_POINT('Origin',(-13.5086446004715,-33.3891748892912,-260.));
#274436=CARTESIAN_POINT('',(-8.37745629126787,-42.3387398169023,-260.));
#274437=CARTESIAN_POINT('',(-8.37745629126787,-42.3387398169023,-260.));
#274438=CARTESIAN_POINT('',(-7.58664460047157,-44.247928126106,-260.));
#274439=CARTESIAN_POINT('Origin',(-10.2866446004716,-44.2479281261059,-260.));
#274440=CARTESIAN_POINT('',(-7.58664460047161,-48.3213553995291,-260.));
#274441=CARTESIAN_POINT('',(-7.58664460047161,-48.3213553995289,-260.));
#274442=CARTESIAN_POINT('',(-4.88664460047164,-51.021355399529,-260.));
#274443=CARTESIAN_POINT('Origin',(-4.88664460047161,-48.321355399529,-260.));
#274444=CARTESIAN_POINT('',(4.86935539952891,-51.0213553995286,-260.));
#274445=CARTESIAN_POINT('',(4.86935539952891,-51.0213553995286,-260.));
#274446=CARTESIAN_POINT('',(7.56935539952894,-48.3213553995286,-260.));
#274447=CARTESIAN_POINT('Origin',(4.86935539952893,-48.3213553995286,-260.));
#274448=CARTESIAN_POINT('',(7.56935539952897,-44.2479281261057,-260.));
#274449=CARTESIAN_POINT('',(7.56935539952894,-48.3213553995286,-260.));
#274450=CARTESIAN_POINT('',(8.36016709032531,-42.338739816902,-260.));
#274451=CARTESIAN_POINT('Origin',(10.269355399529,-44.2479281261057,-260.));
#274452=CARTESIAN_POINT('',(15.4005437087327,-35.2983631984947,-260.));
#274453=CARTESIAN_POINT('',(8.36016709032531,-42.338739816902,-260.));
#274454=CARTESIAN_POINT('',(16.191355399529,-33.389174889291,-260.));
#274455=CARTESIAN_POINT('Origin',(13.491355399529,-33.389174889291,-260.));
#274456=CARTESIAN_POINT('',(16.1913553995291,-20.7633553995288,-260.));
#274457=CARTESIAN_POINT('',(16.191355399529,-33.389174889291,-260.));
#274458=CARTESIAN_POINT('',(20.7633553995291,-16.1913553995288,-260.));
#274459=CARTESIAN_POINT('',(20.7633553995291,-16.1913553995288,-260.));
#274460=CARTESIAN_POINT('',(33.3891748892914,-16.1913553995288,-260.));
#274461=CARTESIAN_POINT('',(26.9913553995291,-16.1913553995288,-260.));
#274462=CARTESIAN_POINT('',(35.2983631984951,-15.4005437087325,-260.));
#274463=CARTESIAN_POINT('Origin',(33.3891748892914,-13.4913553995288,-260.));
#274464=CARTESIAN_POINT('',(42.3387398169024,-8.36016709032512,-260.));
#274465=CARTESIAN_POINT('',(42.3387398169024,-8.36016709032512,-260.));
#274466=CARTESIAN_POINT('',(44.2479281261061,-7.5693553995288,-260.));
#274467=CARTESIAN_POINT('Origin',(44.2479281261061,-10.2693553995288,-260.));
#274468=CARTESIAN_POINT('',(48.3213553995291,-7.5693553995288,-260.));
#274469=CARTESIAN_POINT('',(48.3213553995291,-7.5693553995288,-260.));
#274470=CARTESIAN_POINT('',(51.0213553995291,-4.8693553995288,-260.));
#274471=CARTESIAN_POINT('Origin',(48.3213553995291,-4.8693553995288,-260.));
#274472=CARTESIAN_POINT('',(51.0213553995287,4.88664460047104,-260.));
#274473=CARTESIAN_POINT('',(51.0213553995287,4.88664460047104,-260.));
#274474=CARTESIAN_POINT('',(48.3213553995288,7.58664460047108,-260.));
#274475=CARTESIAN_POINT('Origin',(48.3213553995287,4.88664460047107,-260.));
#274476=CARTESIAN_POINT('',(44.2479281261058,7.58664460047112,-260.));
#274477=CARTESIAN_POINT('',(48.3213553995288,7.58664460047107,-260.));
#274478=CARTESIAN_POINT('',(42.3387398169021,8.37745629126746,-260.));
#274479=CARTESIAN_POINT('Origin',(44.2479281261058,10.2866446004711,-260.));
#274480=CARTESIAN_POINT('',(35.2983631984948,15.4178329096749,-260.));
#274481=CARTESIAN_POINT('',(42.3387398169021,8.37745629126746,-260.));
#274482=CARTESIAN_POINT('',(33.3891748892912,16.2086446004712,-260.));
#274483=CARTESIAN_POINT('Origin',(33.3891748892911,13.5086446004712,-260.));
#274484=CARTESIAN_POINT('',(20.7633553995289,16.2086446004714,-260.));
#274485=CARTESIAN_POINT('',(33.3891748892912,16.2086446004712,-260.));
#274486=CARTESIAN_POINT('',(16.191355399529,20.7806446004713,-260.));
#274487=CARTESIAN_POINT('',(16.191355399529,20.7806446004713,-260.));
#274488=CARTESIAN_POINT('',(16.191355399529,33.4064640902336,-260.));
#274489=CARTESIAN_POINT('',(16.191355399529,27.0086446004713,-260.));
#274490=CARTESIAN_POINT('',(15.4005437087327,35.3156523994373,-260.));
#274491=CARTESIAN_POINT('Origin',(13.491355399529,33.4064640902337,-260.));
#274492=CARTESIAN_POINT('',(8.36016709032535,42.3560290178447,-260.));
#274493=CARTESIAN_POINT('',(8.36016709032535,42.3560290178447,-260.));
#274494=CARTESIAN_POINT('',(7.56935539952904,44.2652173270484,-260.));
#274495=CARTESIAN_POINT('Origin',(10.269355399529,44.2652173270484,-260.));
#274496=CARTESIAN_POINT('',(7.56935539952906,48.3386446004714,-260.));
#274497=CARTESIAN_POINT('',(7.56935539952906,48.3386446004714,-260.));
#274498=CARTESIAN_POINT('',(4.86935539952906,51.0386446004714,-260.));
#274499=CARTESIAN_POINT('Origin',(4.86935539952905,48.3386446004714,-260.));
#274500=CARTESIAN_POINT('',(-4.88664460047113,51.038644600471,-260.));
#274501=CARTESIAN_POINT('',(-4.88664460047113,51.038644600471,-260.));
#274502=CARTESIAN_POINT('',(-7.58664460047116,48.338644600471,-260.));
#274503=CARTESIAN_POINT('Origin',(-4.88664460047115,48.338644600471,-260.));
#274504=CARTESIAN_POINT('',(-7.58664460047119,44.2652173270481,-260.));
#274505=CARTESIAN_POINT('',(-7.58664460047116,48.338644600471,-260.));
#274506=CARTESIAN_POINT('',(-8.37745629126753,42.3560290178444,-260.));
#274507=CARTESIAN_POINT('Origin',(-10.2866446004712,44.2652173270481,-260.));
#274508=CARTESIAN_POINT('',(-15.4178329096749,35.3156523994371,-260.));
#274509=CARTESIAN_POINT('',(-8.37745629126753,42.3560290178444,-260.));
#274510=CARTESIAN_POINT('',(-16.2086446004713,33.4064640902334,-260.));
#274511=CARTESIAN_POINT('Origin',(-13.5086446004713,33.4064640902334,-260.));
#274512=CARTESIAN_POINT('',(-16.2086446004714,20.7806446004712,-260.));
#274513=CARTESIAN_POINT('',(-16.2086446004713,33.4064640902334,-260.));
#274514=CARTESIAN_POINT('',(-20.7806446004713,16.2086446004712,-260.));
#274515=CARTESIAN_POINT('',(-20.7806446004713,16.2086446004712,-260.));
#274516=CARTESIAN_POINT('',(-33.4064640902336,16.2086446004712,-260.));
#274517=CARTESIAN_POINT('',(-27.0086446004713,16.2086446004712,-260.));
#274518=CARTESIAN_POINT('',(-35.3156523994373,15.4178329096749,-260.));
#274519=CARTESIAN_POINT('Origin',(-33.4064640902336,13.5086446004712,-260.));
#274520=CARTESIAN_POINT('',(-42.3560290178447,8.37745629126751,-260.));
#274521=CARTESIAN_POINT('',(-42.3560290178447,8.37745629126751,-260.));
#274522=CARTESIAN_POINT('',(-44.2652173270483,7.58664460047119,-260.));
#274523=CARTESIAN_POINT('Origin',(-44.2652173270483,10.2866446004712,-260.));
#274524=CARTESIAN_POINT('',(-48.3386446004713,7.58664460047119,-260.));
#274525=CARTESIAN_POINT('Origin',(-48.3386446004712,-4.86935539952856,910.));
#274526=CARTESIAN_POINT('',(-48.3386446004712,-7.56935539952856,910.));
#274527=CARTESIAN_POINT('',(-51.0386446004712,-4.8693553995285,910.));
#274528=CARTESIAN_POINT('Origin',(-48.3386446004712,-7.56935539952856,910.));
#274529=CARTESIAN_POINT('',(-44.2652173270483,-7.56935539952864,910.));
#274530=CARTESIAN_POINT('Origin',(-44.2652173270483,-10.2693553995286,910.));
#274531=CARTESIAN_POINT('',(-42.3560290178446,-8.36016709032499,910.));
#274532=CARTESIAN_POINT('Origin',(-42.3560290178446,-8.36016709032499,910.));
#274533=CARTESIAN_POINT('',(-35.3156523994374,-15.4005437087325,910.));
#274534=CARTESIAN_POINT('Origin',(-33.4064640902337,-13.4913553995288,910.));
#274535=CARTESIAN_POINT('',(-33.4064640902337,-16.1913553995288,910.));
#274536=CARTESIAN_POINT('Origin',(-33.4064640902337,-16.1913553995288,910.));
#274537=CARTESIAN_POINT('',(-20.7806446004715,-16.191355399529,910.));
#274538=CARTESIAN_POINT('Origin',(-16.2086446004715,-20.7633553995291,910.));
#274539=CARTESIAN_POINT('',(-16.2086446004715,-20.7633553995291,910.));
#274540=CARTESIAN_POINT('Origin',(-16.2086446004716,-26.9913553995291,910.));
#274541=CARTESIAN_POINT('',(-16.2086446004717,-33.3891748892914,910.));
#274542=CARTESIAN_POINT('Origin',(-13.5086446004717,-33.3891748892914,910.));
#274543=CARTESIAN_POINT('',(-15.4178329096754,-35.298363198495,910.));
#274544=CARTESIAN_POINT('Origin',(-8.37745629126809,-42.3387398169025,910.));
#274545=CARTESIAN_POINT('',(-8.37745629126808,-42.3387398169025,910.));
#274546=CARTESIAN_POINT('Origin',(-10.2866446004718,-44.2479281261061,910.));
#274547=CARTESIAN_POINT('',(-7.58664460047179,-44.2479281261062,910.));
#274548=CARTESIAN_POINT('Origin',(-7.58664460047183,-48.3213553995291,910.));
#274549=CARTESIAN_POINT('',(-7.58664460047183,-48.3213553995291,910.));
#274550=CARTESIAN_POINT('Origin',(-4.88664460047183,-48.3213553995292,910.));
#274551=CARTESIAN_POINT('',(-4.88664460047186,-51.0213553995292,910.));
#274552=CARTESIAN_POINT('Origin',(4.86935539952891,-51.021355399529,910.));
#274553=CARTESIAN_POINT('',(4.86935539952891,-51.021355399529,910.));
#274554=CARTESIAN_POINT('Origin',(4.86935539952893,-48.3213553995291,910.));
#274555=CARTESIAN_POINT('',(7.56935539952894,-48.3213553995291,910.));
#274556=CARTESIAN_POINT('Origin',(7.56935539952894,-48.3213553995291,910.));
#274557=CARTESIAN_POINT('',(7.56935539952897,-44.2479281261061,910.));
#274558=CARTESIAN_POINT('Origin',(10.269355399529,-44.2479281261061,910.));
#274559=CARTESIAN_POINT('',(8.36016709032531,-42.3387398169024,910.));
#274560=CARTESIAN_POINT('Origin',(8.36016709032531,-42.3387398169024,910.));
#274561=CARTESIAN_POINT('',(15.4005437087327,-35.2983631984951,910.));
#274562=CARTESIAN_POINT('Origin',(13.491355399529,-33.3891748892914,910.));
#274563=CARTESIAN_POINT('',(16.191355399529,-33.3891748892915,910.));
#274564=CARTESIAN_POINT('Origin',(16.191355399529,-33.3891748892915,910.));
#274565=CARTESIAN_POINT('',(16.1913553995291,-20.7633553995292,910.));
#274566=CARTESIAN_POINT('Origin',(20.7633553995291,-16.1913553995292,910.));
#274567=CARTESIAN_POINT('',(20.7633553995291,-16.1913553995292,910.));
#274568=CARTESIAN_POINT('Origin',(26.9913553995291,-16.1913553995292,910.));
#274569=CARTESIAN_POINT('',(33.3891748892914,-16.1913553995292,910.));
#274570=CARTESIAN_POINT('Origin',(33.3891748892914,-13.4913553995292,910.));
#274571=CARTESIAN_POINT('',(35.2983631984951,-15.4005437087329,910.));
#274572=CARTESIAN_POINT('Origin',(42.3387398169024,-8.36016709032555,910.));
#274573=CARTESIAN_POINT('',(42.3387398169024,-8.36016709032555,910.));
#274574=CARTESIAN_POINT('Origin',(44.2479281261061,-10.2693553995292,910.));
#274575=CARTESIAN_POINT('',(44.2479281261061,-7.56935539952923,910.));
#274576=CARTESIAN_POINT('Origin',(48.3213553995291,-7.56935539952923,910.));
#274577=CARTESIAN_POINT('',(48.3213553995291,-7.56935539952923,910.));
#274578=CARTESIAN_POINT('Origin',(48.3213553995291,-4.86935539952923,910.));
#274579=CARTESIAN_POINT('',(51.0213553995291,-4.86935539952923,910.));
#274580=CARTESIAN_POINT('Origin',(51.0213553995289,4.88664460047082,910.));
#274581=CARTESIAN_POINT('',(51.0213553995289,4.88664460047082,910.));
#274582=CARTESIAN_POINT('Origin',(48.3213553995289,4.88664460047086,910.));
#274583=CARTESIAN_POINT('',(48.321355399529,7.58664460047086,910.));
#274584=CARTESIAN_POINT('Origin',(48.321355399529,7.58664460047086,910.));
#274585=CARTESIAN_POINT('',(44.247928126106,7.5866446004709,910.));
#274586=CARTESIAN_POINT('Origin',(44.247928126106,10.2866446004709,910.));
#274587=CARTESIAN_POINT('',(42.3387398169023,8.37745629126725,910.));
#274588=CARTESIAN_POINT('Origin',(42.3387398169023,8.37745629126725,910.));
#274589=CARTESIAN_POINT('',(35.298363198495,15.4178329096747,910.));
#274590=CARTESIAN_POINT('Origin',(33.3891748892913,13.508644600471,910.));
#274591=CARTESIAN_POINT('',(33.3891748892914,16.208644600471,910.));
#274592=CARTESIAN_POINT('Origin',(33.3891748892914,16.208644600471,910.));
#274593=CARTESIAN_POINT('',(20.7633553995292,16.2086446004711,910.));
#274594=CARTESIAN_POINT('Origin',(16.1913553995292,20.7806446004711,910.));
#274595=CARTESIAN_POINT('',(16.1913553995292,20.7806446004711,910.));
#274596=CARTESIAN_POINT('Origin',(16.1913553995292,27.0086446004711,910.));
#274597=CARTESIAN_POINT('',(16.1913553995292,33.4064640902334,910.));
#274598=CARTESIAN_POINT('Origin',(13.4913553995292,33.4064640902334,910.));
#274599=CARTESIAN_POINT('',(15.4005437087329,35.3156523994371,910.));
#274600=CARTESIAN_POINT('Origin',(8.36016709032557,42.3560290178445,910.));
#274601=CARTESIAN_POINT('',(8.36016709032557,42.3560290178445,910.));
#274602=CARTESIAN_POINT('Origin',(10.2693553995293,44.2652173270482,910.));
#274603=CARTESIAN_POINT('',(7.56935539952926,44.2652173270482,910.));
#274604=CARTESIAN_POINT('Origin',(7.56935539952927,48.3386446004712,910.));
#274605=CARTESIAN_POINT('',(7.56935539952927,48.3386446004712,910.));
#274606=CARTESIAN_POINT('Origin',(4.86935539952927,48.3386446004712,910.));
#274607=CARTESIAN_POINT('',(4.86935539952928,51.0386446004712,910.));
#274608=CARTESIAN_POINT('Origin',(-4.88664460047113,51.038644600471,910.));
#274609=CARTESIAN_POINT('',(-4.88664460047113,51.038644600471,910.));
#274610=CARTESIAN_POINT('Origin',(-4.88664460047115,48.338644600471,910.));
#274611=CARTESIAN_POINT('',(-7.58664460047116,48.338644600471,910.));
#274612=CARTESIAN_POINT('Origin',(-7.58664460047116,48.338644600471,910.));
#274613=CARTESIAN_POINT('',(-7.58664460047119,44.2652173270481,910.));
#274614=CARTESIAN_POINT('Origin',(-10.2866446004712,44.2652173270481,910.));
#274615=CARTESIAN_POINT('',(-8.37745629126753,42.3560290178444,910.));
#274616=CARTESIAN_POINT('Origin',(-8.37745629126753,42.3560290178444,910.));
#274617=CARTESIAN_POINT('',(-15.4178329096749,35.3156523994371,910.));
#274618=CARTESIAN_POINT('Origin',(-13.5086446004713,33.4064640902334,910.));
#274619=CARTESIAN_POINT('',(-16.2086446004713,33.4064640902334,910.));
#274620=CARTESIAN_POINT('Origin',(-16.2086446004713,33.4064640902334,910.));
#274621=CARTESIAN_POINT('',(-16.2086446004713,20.7806446004712,910.));
#274622=CARTESIAN_POINT('Origin',(-20.7806446004713,16.2086446004712,910.));
#274623=CARTESIAN_POINT('',(-20.7806446004713,16.2086446004712,910.));
#274624=CARTESIAN_POINT('Origin',(-27.0086446004713,16.2086446004712,910.));
#274625=CARTESIAN_POINT('',(-33.4064640902336,16.2086446004712,910.));
#274626=CARTESIAN_POINT('Origin',(-33.4064640902336,13.5086446004712,910.));
#274627=CARTESIAN_POINT('',(-35.3156523994373,15.4178329096749,910.));
#274628=CARTESIAN_POINT('Origin',(-42.3560290178447,8.37745629126751,910.));
#274629=CARTESIAN_POINT('',(-42.3560290178447,8.37745629126751,910.));
#274630=CARTESIAN_POINT('Origin',(-44.2652173270483,10.2866446004712,910.));
#274631=CARTESIAN_POINT('',(-44.2652173270483,7.58664460047119,910.));
#274632=CARTESIAN_POINT('Origin',(-48.3386446004713,7.58664460047119,910.));
#274633=CARTESIAN_POINT('',(-48.3386446004713,7.58664460047119,910.));
#274634=CARTESIAN_POINT('Origin',(-48.3386446004713,4.88664460047119,910.));
#274635=CARTESIAN_POINT('',(-51.0386446004713,4.88664460047119,910.));
#274636=CARTESIAN_POINT('Origin',(-51.0386446004713,4.88664460047119,910.));
#274637=CARTESIAN_POINT('Origin',(26.9913553995291,-26.9913553995292,910.));
#274638=CARTESIAN_POINT('',(29.7492170880445,-21.3270638368519,1282.35584962783));
#274639=CARTESIAN_POINT('',(24.2334937110134,-21.327063836852,1282.35584962783));
#274640=CARTESIAN_POINT('Origin',(26.9913553995291,-26.9913553995294,1282.35584962783));
#274641=CARTESIAN_POINT('',(24.2334937110134,-21.3270638368515,-260.));
#274642=CARTESIAN_POINT('',(24.2334937110134,-21.3270638368519,910.));
#274643=CARTESIAN_POINT('',(29.7492170880447,-21.3270638368514,-260.));
#274644=CARTESIAN_POINT('Origin',(26.9913553995291,-26.9913553995288,-260.));
#274645=CARTESIAN_POINT('',(29.7492170880447,-21.3270638368519,910.));
#274646=CARTESIAN_POINT('Origin',(0.,0.,-260.));
#274647=CARTESIAN_POINT('',(32.6891089669786,-35.113778119667,-260.));
#274648=CARTESIAN_POINT('',(35.1137781196672,-32.6891089669784,-260.));
#274649=CARTESIAN_POINT('Origin',(26.9913553995291,-26.9913553995288,-260.));
#274650=CARTESIAN_POINT('',(32.6556469622064,-29.7492170880444,-260.));
#274651=CARTESIAN_POINT('',(35.1137781196672,-32.6891089669784,-260.));
#274652=CARTESIAN_POINT('',(32.6556469622064,-24.2334937110132,-260.));
#274653=CARTESIAN_POINT('Origin',(26.9913553995291,-26.9913553995288,-260.));
#274654=CARTESIAN_POINT('',(35.1137781196672,-21.2936018320792,-260.));
#274655=CARTESIAN_POINT('',(35.1137781196672,-21.2936018320792,-260.));
#274656=CARTESIAN_POINT('',(32.6891089669786,-18.8689326793906,-260.));
#274657=CARTESIAN_POINT('Origin',(26.9913553995291,-26.9913553995288,-260.));
#274658=CARTESIAN_POINT('',(32.6891089669786,-18.8689326793906,-260.));
#274659=CARTESIAN_POINT('',(21.2936018320795,-18.8689326793908,-260.));
#274660=CARTESIAN_POINT('',(21.2936018320795,-18.8689326793907,-260.));
#274661=CARTESIAN_POINT('',(18.8689326793909,-21.2936018320794,-260.));
#274662=CARTESIAN_POINT('Origin',(26.9913553995291,-26.9913553995288,-260.));
#274663=CARTESIAN_POINT('',(21.3270638368517,-24.2334937110133,-260.));
#274664=CARTESIAN_POINT('',(18.8689326793909,-21.2936018320794,-260.));
#274665=CARTESIAN_POINT('',(21.3270638368517,-29.7492170880443,-260.));
#274666=CARTESIAN_POINT('Origin',(26.9913553995291,-26.9913553995288,-260.));
#274667=CARTESIAN_POINT('',(18.8689326793909,-32.6891089669782,-260.));
#274668=CARTESIAN_POINT('',(18.8689326793909,-32.6891089669782,-260.));
#274669=CARTESIAN_POINT('',(21.2936018320795,-35.1137781196669,-260.));
#274670=CARTESIAN_POINT('Origin',(26.9913553995291,-26.9913553995288,-260.));
#274671=CARTESIAN_POINT('',(24.2334937110134,-32.6556469622061,-260.));
#274672=CARTESIAN_POINT('',(21.2936018320795,-35.1137781196669,-260.));
#274673=CARTESIAN_POINT('',(29.7492170880447,-32.6556469622062,-260.));
#274674=CARTESIAN_POINT('Origin',(26.9913553995291,-26.9913553995288,-260.));
#274675=CARTESIAN_POINT('',(32.6891089669786,-35.113778119667,-260.));
#274676=CARTESIAN_POINT('Origin',(32.6891089669786,-35.1137781196674,910.));
#274677=CARTESIAN_POINT('',(29.7492170880447,-32.6556469622067,1282.35584962783));
#274678=CARTESIAN_POINT('',(29.7492170880447,-32.6556469622066,910.));
#274679=CARTESIAN_POINT('',(32.6891089669786,-35.1137781196675,1282.35584962783));
#274680=CARTESIAN_POINT('',(32.6891089669785,-35.1137781196675,1282.35584962783));
#274681=CARTESIAN_POINT('',(32.6891089669786,-35.1137781196674,910.));
#274682=CARTESIAN_POINT('Origin',(26.9913553995291,-26.9913553995292,910.));
#274683=CARTESIAN_POINT('',(24.2334937110133,-32.6556469622066,1282.35584962783));
#274684=CARTESIAN_POINT('',(24.2334937110134,-32.6556469622066,910.));
#274685=CARTESIAN_POINT('Origin',(26.9913553995291,-26.9913553995294,1282.35584962783));
#274686=CARTESIAN_POINT('Origin',(21.2936018320795,-35.1137781196673,910.));
#274687=CARTESIAN_POINT('',(21.2936018320795,-35.1137781196674,1282.35584962783));
#274688=CARTESIAN_POINT('',(21.2936018320795,-35.1137781196673,910.));
#274689=CARTESIAN_POINT('',(21.2936018320795,-35.1137781196674,1282.35584962783));
#274690=CARTESIAN_POINT('Origin',(26.9913553995291,-26.9913553995292,910.));
#274691=CARTESIAN_POINT('',(18.8689326793907,-32.6891089669786,1282.35584962783));
#274692=CARTESIAN_POINT('',(18.8689326793909,-32.6891089669787,910.));
#274693=CARTESIAN_POINT('Origin',(26.9913553995291,-26.9913553995294,1282.35584962783));
#274694=CARTESIAN_POINT('Origin',(18.8689326793909,-32.6891089669787,910.));
#274695=CARTESIAN_POINT('',(21.3270638368522,-29.7492170880443,1282.35584962783));
#274696=CARTESIAN_POINT('',(21.3270638368517,-29.7492170880447,910.));
#274697=CARTESIAN_POINT('',(18.868932679391,-32.6891089669787,1282.35584962783));
#274698=CARTESIAN_POINT('Origin',(26.9913553995291,-26.9913553995292,910.));
#274699=CARTESIAN_POINT('',(21.3270638368518,-24.2334937110136,1282.35584962783));
#274700=CARTESIAN_POINT('',(21.3270638368517,-24.2334937110137,910.));
#274701=CARTESIAN_POINT('Origin',(26.9913553995291,-26.9913553995294,1282.35584962783));
#274702=CARTESIAN_POINT('Origin',(18.8689326793909,-21.2936018320798,910.));
#274703=CARTESIAN_POINT('',(18.8689326793904,-21.2936018320794,1282.35584962783));
#274704=CARTESIAN_POINT('',(18.8689326793909,-21.2936018320798,910.));
#274705=CARTESIAN_POINT('',(18.8689326793908,-21.2936018320799,1282.35584962783));
#274706=CARTESIAN_POINT('Origin',(26.9913553995291,-26.9913553995292,910.));
#274707=CARTESIAN_POINT('',(21.2936018320796,-18.8689326793912,1282.35584962783));
#274708=CARTESIAN_POINT('',(21.2936018320795,-18.8689326793912,910.));
#274709=CARTESIAN_POINT('Origin',(26.9913553995291,-26.9913553995294,1282.35584962783));
#274710=CARTESIAN_POINT('Origin',(21.2936018320795,-18.8689326793912,910.));
#274711=CARTESIAN_POINT('',(21.2936018320794,-18.8689326793913,1282.35584962783));
#274712=CARTESIAN_POINT('Origin',(32.6891089669786,-18.8689326793911,910.));
#274713=CARTESIAN_POINT('',(32.6891089669786,-18.8689326793912,1282.35584962783));
#274714=CARTESIAN_POINT('',(32.6891089669786,-18.8689326793911,910.));
#274715=CARTESIAN_POINT('',(32.6891089669787,-18.8689326793912,1282.35584962783));
#274716=CARTESIAN_POINT('Origin',(26.9913553995291,-26.9913553995292,910.));
#274717=CARTESIAN_POINT('',(35.113778119667,-21.2936018320796,1282.35584962783));
#274718=CARTESIAN_POINT('',(35.1137781196672,-21.2936018320797,910.));
#274719=CARTESIAN_POINT('Origin',(26.9913553995291,-26.9913553995294,1282.35584962783));
#274720=CARTESIAN_POINT('Origin',(35.1137781196672,-21.2936018320797,910.));
#274721=CARTESIAN_POINT('',(32.6556469622065,-24.2334937110136,1282.35584962783));
#274722=CARTESIAN_POINT('',(32.6556469622064,-24.2334937110136,910.));
#274723=CARTESIAN_POINT('',(35.1137781196673,-21.2936018320797,1282.35584962783));
#274724=CARTESIAN_POINT('Origin',(26.9913553995291,-26.9913553995292,910.));
#274725=CARTESIAN_POINT('',(32.6556469622066,-29.7492170880447,1282.35584962783));
#274726=CARTESIAN_POINT('',(32.6556469622064,-29.7492170880448,910.));
#274727=CARTESIAN_POINT('Origin',(26.9913553995291,-26.9913553995294,1282.35584962783));
#274728=CARTESIAN_POINT('Origin',(35.1137781196672,-32.6891089669788,910.));
#274729=CARTESIAN_POINT('',(35.1137781196671,-32.6891089669788,1282.35584962783));
#274730=CARTESIAN_POINT('',(35.1137781196672,-32.6891089669788,910.));
#274731=CARTESIAN_POINT('',(35.1137781196671,-32.6891089669788,1282.35584962783));
#274732=CARTESIAN_POINT('Origin',(26.9913553995291,-26.9913553995292,910.));
#274733=CARTESIAN_POINT('Origin',(26.9913553995291,-26.9913553995294,1282.35584962783));
#274734=CARTESIAN_POINT('Origin',(0.,0.,1282.35584962783));
#274735=CARTESIAN_POINT('Origin',(0.,0.,-260.));
#274736=CARTESIAN_POINT('',(51.6603553995289,-45.884155399529,-260.));
#274737=CARTESIAN_POINT('',(49.8603553995289,-44.084155399529,-260.));
#274738=CARTESIAN_POINT('Origin',(49.8603553995289,-45.884155399529,-260.));
#274739=CARTESIAN_POINT('',(45.8841553995291,-44.084155399529,-260.));
#274740=CARTESIAN_POINT('',(49.8603553995289,-44.084155399529,-260.));
#274741=CARTESIAN_POINT('',(44.0841553995291,-45.884155399529,-260.));
#274742=CARTESIAN_POINT('Origin',(45.8841553995291,-45.884155399529,-260.));
#274743=CARTESIAN_POINT('',(44.0841553995291,-49.8603553995288,-260.));
#274744=CARTESIAN_POINT('',(44.0841553995291,-45.884155399529,-260.));
#274745=CARTESIAN_POINT('',(45.8841553995291,-51.6603553995288,-260.));
#274746=CARTESIAN_POINT('Origin',(45.8841553995291,-49.8603553995288,-260.));
#274747=CARTESIAN_POINT('',(49.8603553995289,-51.6603553995288,-260.));
#274748=CARTESIAN_POINT('',(45.8841553995291,-51.6603553995288,-260.));
#274749=CARTESIAN_POINT('',(51.6603553995289,-49.8603553995288,-260.));
#274750=CARTESIAN_POINT('Origin',(49.8603553995289,-49.8603553995288,-260.));
#274751=CARTESIAN_POINT('',(51.6603553995289,-49.8603553995288,-260.));
#274752=CARTESIAN_POINT('Origin',(51.6603553995289,-49.8603553995292,910.));
#274753=CARTESIAN_POINT('',(51.6603553995289,-49.8603553995294,1282.35584962783));
#274754=CARTESIAN_POINT('',(51.6603553995289,-49.8603553995292,910.));
#274755=CARTESIAN_POINT('',(51.6603553995289,-45.8841553995295,1282.35584962783));
#274756=CARTESIAN_POINT('',(51.6603553995289,-49.8603553995292,1282.35584962783));
#274757=CARTESIAN_POINT('',(51.6603553995289,-45.8841553995294,910.));
#274758=CARTESIAN_POINT('Origin',(49.8603553995289,-49.8603553995292,910.));
#274759=CARTESIAN_POINT('',(49.8603553995289,-51.6603553995294,1282.35584962783));
#274760=CARTESIAN_POINT('',(49.8603553995289,-51.6603553995292,910.));
#274761=CARTESIAN_POINT('Origin',(49.8603553995289,-49.8603553995294,1282.35584962783));
#274762=CARTESIAN_POINT('Origin',(45.8841553995291,-51.6603553995292,910.));
#274763=CARTESIAN_POINT('',(45.8841553995291,-51.6603553995294,1282.35584962783));
#274764=CARTESIAN_POINT('',(45.8841553995291,-51.6603553995292,910.));
#274765=CARTESIAN_POINT('',(45.8841553995291,-51.6603553995294,1282.35584962783));
#274766=CARTESIAN_POINT('Origin',(45.8841553995291,-49.8603553995292,910.));
#274767=CARTESIAN_POINT('',(44.0841553995291,-49.860355399529,1282.35584962783));
#274768=CARTESIAN_POINT('',(44.0841553995291,-49.8603553995292,910.));
#274769=CARTESIAN_POINT('Origin',(45.8841553995291,-49.8603553995294,1282.35584962783));
#274770=CARTESIAN_POINT('Origin',(44.0841553995291,-45.8841553995294,910.));
#274771=CARTESIAN_POINT('',(44.0841553995291,-45.884155399529,1282.35584962783));
#274772=CARTESIAN_POINT('',(44.0841553995291,-45.8841553995294,910.));
#274773=CARTESIAN_POINT('',(44.0841553995291,-45.8841553995294,1282.35584962783));
#274774=CARTESIAN_POINT('Origin',(45.8841553995291,-45.8841553995294,910.));
#274775=CARTESIAN_POINT('',(45.8841553995291,-44.0841553995295,1282.35584962783));
#274776=CARTESIAN_POINT('',(45.8841553995291,-44.0841553995294,910.));
#274777=CARTESIAN_POINT('Origin',(45.8841553995291,-45.8841553995295,1282.35584962783));
#274778=CARTESIAN_POINT('Origin',(49.8603553995289,-44.0841553995294,910.));
#274779=CARTESIAN_POINT('',(49.8603553995289,-44.0841553995295,1282.35584962783));
#274780=CARTESIAN_POINT('',(49.8603553995289,-44.0841553995294,910.));
#274781=CARTESIAN_POINT('',(49.8603553995289,-44.0841553995295,1282.35584962783));
#274782=CARTESIAN_POINT('Origin',(49.8603553995289,-45.8841553995294,910.));
#274783=CARTESIAN_POINT('Origin',(49.8603553995289,-45.8841553995295,1282.35584962783));
#274784=CARTESIAN_POINT('Origin',(0.,0.,1282.35584962783));
#274785=CARTESIAN_POINT('Origin',(26.9913553995292,27.0086446004711,910.));
#274786=CARTESIAN_POINT('',(29.7492170880447,32.6729361631484,1282.35584962783));
#274787=CARTESIAN_POINT('',(24.2334937110136,32.6729361631484,1282.35584962783));
#274788=CARTESIAN_POINT('Origin',(26.9913553995293,27.008644600471,1282.35584962783));
#274789=CARTESIAN_POINT('',(24.2334937110134,32.6729361631487,-260.));
#274790=CARTESIAN_POINT('',(24.2334937110136,32.6729361631484,910.));
#274791=CARTESIAN_POINT('',(29.7492170880446,32.6729361631486,-260.));
#274792=CARTESIAN_POINT('Origin',(26.991355399529,27.0086446004713,-260.));
#274793=CARTESIAN_POINT('',(29.7492170880448,32.6729361631484,910.));
#274794=CARTESIAN_POINT('Origin',(0.,0.,-260.));
#274795=CARTESIAN_POINT('',(35.1137781196672,32.7063981679208,-260.));
#274796=CARTESIAN_POINT('',(32.6891089669786,35.1310673206094,-260.));
#274797=CARTESIAN_POINT('Origin',(26.991355399529,27.0086446004713,-260.));
#274798=CARTESIAN_POINT('',(32.6891089669786,35.1310673206094,-260.));
#274799=CARTESIAN_POINT('',(21.2936018320794,35.1310673206094,-260.));
#274800=CARTESIAN_POINT('',(21.2936018320794,35.1310673206094,-260.));
#274801=CARTESIAN_POINT('',(18.8689326793908,32.7063981679208,-260.));
#274802=CARTESIAN_POINT('Origin',(26.991355399529,27.0086446004713,-260.));
#274803=CARTESIAN_POINT('',(21.3270638368516,29.7665062889869,-260.));
#274804=CARTESIAN_POINT('',(18.8689326793908,32.7063981679208,-260.));
#274805=CARTESIAN_POINT('',(21.3270638368517,24.2507829119557,-260.));
#274806=CARTESIAN_POINT('Origin',(26.991355399529,27.0086446004713,-260.));
#274807=CARTESIAN_POINT('',(18.8689326793909,21.3108910330217,-260.));
#274808=CARTESIAN_POINT('',(18.8689326793909,21.3108910330217,-260.));
#274809=CARTESIAN_POINT('',(21.2936018320795,18.8862218803331,-260.));
#274810=CARTESIAN_POINT('Origin',(26.991355399529,27.0086446004713,-260.));
#274811=CARTESIAN_POINT('',(24.2334937110134,21.3443530377939,-260.));
#274812=CARTESIAN_POINT('',(21.2936018320795,18.8862218803331,-260.));
#274813=CARTESIAN_POINT('',(29.7492170880445,21.3443530377939,-260.));
#274814=CARTESIAN_POINT('Origin',(26.991355399529,27.0086446004713,-260.));
#274815=CARTESIAN_POINT('',(32.6891089669784,18.8862218803331,-260.));
#274816=CARTESIAN_POINT('',(32.6891089669784,18.8862218803331,-260.));
#274817=CARTESIAN_POINT('',(35.113778119667,21.3108910330217,-260.));
#274818=CARTESIAN_POINT('Origin',(26.991355399529,27.0086446004713,-260.));
#274819=CARTESIAN_POINT('',(32.6556469622063,24.2507829119556,-260.));
#274820=CARTESIAN_POINT('',(35.113778119667,21.3108910330217,-260.));
#274821=CARTESIAN_POINT('',(32.6556469622064,29.7665062889869,-260.));
#274822=CARTESIAN_POINT('Origin',(26.991355399529,27.0086446004713,-260.));
#274823=CARTESIAN_POINT('',(35.1137781196672,32.7063981679208,-260.));
#274824=CARTESIAN_POINT('Origin',(35.1137781196674,32.7063981679205,910.));
#274825=CARTESIAN_POINT('',(32.6556469622066,29.7665062889866,1282.35584962783));
#274826=CARTESIAN_POINT('',(32.6556469622066,29.7665062889866,910.));
#274827=CARTESIAN_POINT('',(35.1137781196674,32.7063981679205,1282.35584962783));
#274828=CARTESIAN_POINT('',(35.1137781196675,32.7063981679205,1282.35584962783));
#274829=CARTESIAN_POINT('',(35.1137781196674,32.7063981679205,910.));
#274830=CARTESIAN_POINT('Origin',(26.9913553995292,27.0086446004711,910.));
#274831=CARTESIAN_POINT('',(32.6556469622066,24.2507829119554,1282.35584962783));
#274832=CARTESIAN_POINT('',(32.6556469622065,24.2507829119554,910.));
#274833=CARTESIAN_POINT('Origin',(26.9913553995293,27.008644600471,1282.35584962783));
#274834=CARTESIAN_POINT('Origin',(35.1137781196672,21.3108910330214,910.));
#274835=CARTESIAN_POINT('',(35.1137781196672,21.3108910330214,1282.35584962783));
#274836=CARTESIAN_POINT('',(35.1137781196672,21.3108910330214,910.));
#274837=CARTESIAN_POINT('',(35.1137781196672,21.3108910330214,1282.35584962783));
#274838=CARTESIAN_POINT('Origin',(26.9913553995292,27.0086446004711,910.));
#274839=CARTESIAN_POINT('',(32.6891089669786,18.8862218803328,1282.35584962783));
#274840=CARTESIAN_POINT('',(32.6891089669786,18.8862218803329,910.));
#274841=CARTESIAN_POINT('Origin',(26.9913553995293,27.008644600471,1282.35584962783));
#274842=CARTESIAN_POINT('Origin',(32.6891089669786,18.8862218803329,910.));
#274843=CARTESIAN_POINT('',(29.7492170880445,21.3443530377939,1282.35584962783));
#274844=CARTESIAN_POINT('',(29.7492170880447,21.3443530377937,910.));
#274845=CARTESIAN_POINT('',(32.6891089669786,18.8862218803329,1282.35584962783));
#274846=CARTESIAN_POINT('Origin',(26.9913553995292,27.0086446004711,910.));
#274847=CARTESIAN_POINT('',(24.2334937110135,21.3443530377937,1282.35584962783));
#274848=CARTESIAN_POINT('',(24.2334937110137,21.3443530377937,910.));
#274849=CARTESIAN_POINT('Origin',(26.9913553995293,27.008644600471,1282.35584962783));
#274850=CARTESIAN_POINT('Origin',(21.2936018320797,18.8862218803329,910.));
#274851=CARTESIAN_POINT('',(21.2936018320795,18.8862218803326,1282.35584962783));
#274852=CARTESIAN_POINT('',(21.2936018320797,18.8862218803329,910.));
#274853=CARTESIAN_POINT('',(21.2936018320798,18.8862218803328,1282.35584962783));
#274854=CARTESIAN_POINT('Origin',(26.9913553995292,27.0086446004711,910.));
#274855=CARTESIAN_POINT('',(18.8689326793911,21.3108910330216,1282.35584962783));
#274856=CARTESIAN_POINT('',(18.8689326793911,21.3108910330215,910.));
#274857=CARTESIAN_POINT('Origin',(26.9913553995293,27.008644600471,1282.35584962783));
#274858=CARTESIAN_POINT('Origin',(18.8689326793911,21.3108910330215,910.));
#274859=CARTESIAN_POINT('',(21.3270638368522,24.2507829119557,1282.35584962783));
#274860=CARTESIAN_POINT('',(21.3270638368519,24.2507829119555,910.));
#274861=CARTESIAN_POINT('',(18.8689326793912,21.3108910330214,1282.35584962783));
#274862=CARTESIAN_POINT('Origin',(26.9913553995292,27.0086446004711,910.));
#274863=CARTESIAN_POINT('',(21.3270638368519,29.7665062889867,1282.35584962783));
#274864=CARTESIAN_POINT('',(21.3270638368518,29.7665062889867,910.));
#274865=CARTESIAN_POINT('Origin',(26.9913553995293,27.008644600471,1282.35584962783));
#274866=CARTESIAN_POINT('Origin',(18.8689326793911,32.7063981679206,910.));
#274867=CARTESIAN_POINT('',(18.8689326793909,32.7063981679208,1282.35584962783));
#274868=CARTESIAN_POINT('',(18.8689326793911,32.7063981679206,910.));
#274869=CARTESIAN_POINT('',(18.8689326793911,32.7063981679206,1282.35584962783));
#274870=CARTESIAN_POINT('Origin',(26.9913553995292,27.0086446004711,910.));
#274871=CARTESIAN_POINT('',(21.2936018320797,35.1310673206091,1282.35584962783));
#274872=CARTESIAN_POINT('',(21.2936018320797,35.1310673206092,910.));
#274873=CARTESIAN_POINT('Origin',(26.9913553995293,27.008644600471,1282.35584962783));
#274874=CARTESIAN_POINT('Origin',(21.2936018320797,35.1310673206092,910.));
#274875=CARTESIAN_POINT('',(21.2936018320797,35.1310673206092,1282.35584962783));
#274876=CARTESIAN_POINT('Origin',(32.6891089669788,35.1310673206092,910.));
#274877=CARTESIAN_POINT('',(32.6891089669788,35.131067320609,1282.35584962783));
#274878=CARTESIAN_POINT('',(32.6891089669788,35.1310673206092,910.));
#274879=CARTESIAN_POINT('',(32.6891089669788,35.1310673206091,1282.35584962783));
#274880=CARTESIAN_POINT('Origin',(26.9913553995292,27.0086446004711,910.));
#274881=CARTESIAN_POINT('Origin',(26.9913553995293,27.008644600471,1282.35584962783));
#274882=CARTESIAN_POINT('Origin',(0.,0.,1282.35584962783));
#274883=CARTESIAN_POINT('Origin',(0.,0.,-260.));
#274884=CARTESIAN_POINT('',(45.8841553995292,51.6776446004711,-260.));
#274885=CARTESIAN_POINT('',(44.0841553995292,49.8776446004711,-260.));
#274886=CARTESIAN_POINT('Origin',(45.8841553995292,49.8776446004711,-260.));
#274887=CARTESIAN_POINT('',(44.0841553995292,45.9014446004712,-260.));
#274888=CARTESIAN_POINT('',(44.0841553995292,49.8776446004711,-260.));
#274889=CARTESIAN_POINT('',(45.8841553995292,44.1014446004712,-260.));
#274890=CARTESIAN_POINT('Origin',(45.8841553995292,45.9014446004712,-260.));
#274891=CARTESIAN_POINT('',(49.860355399529,44.1014446004712,-260.));
#274892=CARTESIAN_POINT('',(45.8841553995292,44.1014446004712,-260.));
#274893=CARTESIAN_POINT('',(51.6603553995291,45.9014446004712,-260.));
#274894=CARTESIAN_POINT('Origin',(49.860355399529,45.9014446004712,-260.));
#274895=CARTESIAN_POINT('',(51.6603553995291,49.8776446004711,-260.));
#274896=CARTESIAN_POINT('',(51.6603553995291,45.9014446004712,-260.));
#274897=CARTESIAN_POINT('',(49.8603553995291,51.6776446004711,-260.));
#274898=CARTESIAN_POINT('Origin',(49.8603553995291,49.8776446004711,-260.));
#274899=CARTESIAN_POINT('',(49.8603553995291,51.6776446004711,-260.));
#274900=CARTESIAN_POINT('Origin',(49.8603553995293,51.6776446004708,910.));
#274901=CARTESIAN_POINT('',(49.8603553995293,51.6776446004708,1282.35584962783));
#274902=CARTESIAN_POINT('',(49.8603553995293,51.6776446004708,910.));
#274903=CARTESIAN_POINT('',(45.8841553995295,51.6776446004708,1282.35584962783));
#274904=CARTESIAN_POINT('',(49.8603553995293,51.6776446004708,1282.35584962783));
#274905=CARTESIAN_POINT('',(45.8841553995294,51.6776446004709,910.));
#274906=CARTESIAN_POINT('Origin',(49.8603553995293,49.8776446004709,910.));
#274907=CARTESIAN_POINT('',(51.6603553995293,49.8776446004708,1282.35584962783));
#274908=CARTESIAN_POINT('',(51.6603553995293,49.8776446004709,910.));
#274909=CARTESIAN_POINT('Origin',(49.8603553995293,49.8776446004708,1282.35584962783));
#274910=CARTESIAN_POINT('Origin',(51.6603553995293,45.901444600471,910.));
#274911=CARTESIAN_POINT('',(51.6603553995293,45.901444600471,1282.35584962783));
#274912=CARTESIAN_POINT('',(51.6603553995293,45.901444600471,910.));
#274913=CARTESIAN_POINT('',(51.6603553995293,45.901444600471,1282.35584962783));
#274914=CARTESIAN_POINT('Origin',(49.8603553995293,45.901444600471,910.));
#274915=CARTESIAN_POINT('',(49.8603553995292,44.1014446004709,1282.35584962783));
#274916=CARTESIAN_POINT('',(49.8603553995293,44.101444600471,910.));
#274917=CARTESIAN_POINT('Origin',(49.8603553995293,45.9014446004709,1282.35584962783));
#274918=CARTESIAN_POINT('Origin',(45.8841553995294,44.101444600471,910.));
#274919=CARTESIAN_POINT('',(45.8841553995292,44.101444600471,1282.35584962783));
#274920=CARTESIAN_POINT('',(45.8841553995294,44.101444600471,910.));
#274921=CARTESIAN_POINT('',(45.8841553995294,44.101444600471,1282.35584962783));
#274922=CARTESIAN_POINT('Origin',(45.8841553995294,45.901444600471,910.));
#274923=CARTESIAN_POINT('',(44.0841553995295,45.9014446004711,1282.35584962783));
#274924=CARTESIAN_POINT('',(44.0841553995294,45.901444600471,910.));
#274925=CARTESIAN_POINT('Origin',(45.8841553995295,45.901444600471,1282.35584962783));
#274926=CARTESIAN_POINT('Origin',(44.0841553995294,49.8776446004709,910.));
#274927=CARTESIAN_POINT('',(44.0841553995295,49.8776446004711,1282.35584962783));
#274928=CARTESIAN_POINT('',(44.0841553995294,49.8776446004709,910.));
#274929=CARTESIAN_POINT('',(44.0841553995295,49.8776446004709,1282.35584962783));
#274930=CARTESIAN_POINT('Origin',(45.8841553995294,49.8776446004709,910.));
#274931=CARTESIAN_POINT('Origin',(45.8841553995295,49.8776446004708,1282.35584962783));
#274932=CARTESIAN_POINT('Origin',(0.,0.,1282.35584962783));
#274933=CARTESIAN_POINT('Origin',(-27.0086446004713,27.0086446004712,910.));
#274934=CARTESIAN_POINT('',(-32.6729361631486,29.7665062889868,1282.35584962783));
#274935=CARTESIAN_POINT('',(-32.6729361631486,24.2507829119556,1282.35584962783));
#274936=CARTESIAN_POINT('Origin',(-27.0086446004713,27.0086446004712,1282.35584962783));
#274937=CARTESIAN_POINT('',(-32.6729361631487,24.2507829119556,-260.));
#274938=CARTESIAN_POINT('',(-32.6729361631487,24.2507829119556,910.));
#274939=CARTESIAN_POINT('',(-32.6729361631487,29.7665062889868,-260.));
#274940=CARTESIAN_POINT('Origin',(-27.0086446004713,27.0086446004712,-260.));
#274941=CARTESIAN_POINT('',(-32.6729361631487,29.7665062889868,910.));
#274942=CARTESIAN_POINT('Origin',(0.,0.,-260.));
#274943=CARTESIAN_POINT('',(-32.7063981679208,35.1310673206093,-260.));
#274944=CARTESIAN_POINT('',(-35.1310673206094,32.7063981679208,-260.));
#274945=CARTESIAN_POINT('Origin',(-27.0086446004713,27.0086446004712,-260.));
#274946=CARTESIAN_POINT('',(-35.1310673206094,32.7063981679208,-260.));
#274947=CARTESIAN_POINT('',(-35.1310673206094,21.3108910330216,-260.));
#274948=CARTESIAN_POINT('',(-35.1310673206094,21.3108910330216,-260.));
#274949=CARTESIAN_POINT('',(-32.7063981679208,18.886221880333,-260.));
#274950=CARTESIAN_POINT('Origin',(-27.0086446004713,27.0086446004712,-260.));
#274951=CARTESIAN_POINT('',(-29.7665062889869,21.3443530377938,-260.));
#274952=CARTESIAN_POINT('',(-32.7063981679208,18.886221880333,-260.));
#274953=CARTESIAN_POINT('',(-24.2507829119557,21.3443530377939,-260.));
#274954=CARTESIAN_POINT('Origin',(-27.0086446004713,27.0086446004712,-260.));
#274955=CARTESIAN_POINT('',(-21.3108910330217,18.8862218803331,-260.));
#274956=CARTESIAN_POINT('',(-21.3108910330217,18.8862218803331,-260.));
#274957=CARTESIAN_POINT('',(-18.8862218803331,21.3108910330218,-260.));
#274958=CARTESIAN_POINT('Origin',(-27.0086446004713,27.0086446004712,-260.));
#274959=CARTESIAN_POINT('',(-21.3443530377939,24.2507829119557,-260.));
#274960=CARTESIAN_POINT('',(-18.8862218803331,21.3108910330218,-260.));
#274961=CARTESIAN_POINT('',(-21.3443530377939,29.7665062889867,-260.));
#274962=CARTESIAN_POINT('Origin',(-27.0086446004713,27.0086446004712,-260.));
#274963=CARTESIAN_POINT('',(-18.8862218803331,32.7063981679206,-260.));
#274964=CARTESIAN_POINT('',(-18.8862218803331,32.7063981679206,-260.));
#274965=CARTESIAN_POINT('',(-21.3108910330217,35.1310673206092,-260.));
#274966=CARTESIAN_POINT('Origin',(-27.0086446004713,27.0086446004712,-260.));
#274967=CARTESIAN_POINT('',(-24.2507829119557,32.6729361631485,-260.));
#274968=CARTESIAN_POINT('',(-21.3108910330217,35.1310673206092,-260.));
#274969=CARTESIAN_POINT('',(-29.7665062889869,32.6729361631486,-260.));
#274970=CARTESIAN_POINT('Origin',(-27.0086446004713,27.0086446004712,-260.));
#274971=CARTESIAN_POINT('',(-32.7063981679208,35.1310673206093,-260.));
#274972=CARTESIAN_POINT('Origin',(-32.7063981679208,35.1310673206093,910.));
#274973=CARTESIAN_POINT('',(-29.7665062889869,32.6729361631486,1282.35584962783));
#274974=CARTESIAN_POINT('',(-29.7665062889869,32.6729361631486,910.));
#274975=CARTESIAN_POINT('',(-32.7063981679208,35.1310673206093,1282.35584962783));
#274976=CARTESIAN_POINT('',(-32.7063981679208,35.1310673206093,1282.35584962783));
#274977=CARTESIAN_POINT('',(-32.7063981679208,35.1310673206093,910.));
#274978=CARTESIAN_POINT('Origin',(-27.0086446004713,27.0086446004712,910.));
#274979=CARTESIAN_POINT('',(-24.2507829119557,32.6729361631485,1282.35584962783));
#274980=CARTESIAN_POINT('',(-24.2507829119557,32.6729361631485,910.));
#274981=CARTESIAN_POINT('Origin',(-27.0086446004713,27.0086446004712,1282.35584962783));
#274982=CARTESIAN_POINT('Origin',(-21.3108910330217,35.1310673206092,910.));
#274983=CARTESIAN_POINT('',(-21.3108910330217,35.1310673206092,1282.35584962783));
#274984=CARTESIAN_POINT('',(-21.3108910330217,35.1310673206092,910.));
#274985=CARTESIAN_POINT('',(-21.3108910330217,35.1310673206092,1282.35584962783));
#274986=CARTESIAN_POINT('Origin',(-27.0086446004713,27.0086446004712,910.));
#274987=CARTESIAN_POINT('',(-18.8862218803331,32.7063981679206,1282.35584962783));
#274988=CARTESIAN_POINT('',(-18.8862218803331,32.7063981679206,910.));
#274989=CARTESIAN_POINT('Origin',(-27.0086446004713,27.0086446004712,1282.35584962783));
#274990=CARTESIAN_POINT('Origin',(-18.8862218803331,32.7063981679206,910.));
#274991=CARTESIAN_POINT('',(-21.3443530377939,29.7665062889867,1282.35584962783));
#274992=CARTESIAN_POINT('',(-21.3443530377939,29.7665062889867,910.));
#274993=CARTESIAN_POINT('',(-18.8862218803331,32.7063981679206,1282.35584962783));
#274994=CARTESIAN_POINT('Origin',(-27.0086446004713,27.0086446004712,910.));
#274995=CARTESIAN_POINT('',(-21.3443530377939,24.2507829119557,1282.35584962783));
#274996=CARTESIAN_POINT('',(-21.3443530377939,24.2507829119557,910.));
#274997=CARTESIAN_POINT('Origin',(-27.0086446004713,27.0086446004712,1282.35584962783));
#274998=CARTESIAN_POINT('Origin',(-18.8862218803331,21.3108910330218,910.));
#274999=CARTESIAN_POINT('',(-18.8862218803331,21.3108910330218,1282.35584962783));
#275000=CARTESIAN_POINT('',(-18.8862218803331,21.3108910330218,910.));
#275001=CARTESIAN_POINT('',(-18.8862218803331,21.3108910330218,1282.35584962783));
#275002=CARTESIAN_POINT('Origin',(-27.0086446004713,27.0086446004712,910.));
#275003=CARTESIAN_POINT('',(-21.3108910330217,18.8862218803331,1282.35584962783));
#275004=CARTESIAN_POINT('',(-21.3108910330217,18.8862218803331,910.));
#275005=CARTESIAN_POINT('Origin',(-27.0086446004713,27.0086446004712,1282.35584962783));
#275006=CARTESIAN_POINT('Origin',(-21.3108910330217,18.8862218803331,910.));
#275007=CARTESIAN_POINT('',(-24.2507829119557,21.3443530377939,1282.35584962783));
#275008=CARTESIAN_POINT('',(-24.2507829119557,21.3443530377939,910.));
#275009=CARTESIAN_POINT('',(-21.3108910330217,18.8862218803331,1282.35584962783));
#275010=CARTESIAN_POINT('Origin',(-27.0086446004713,27.0086446004712,910.));
#275011=CARTESIAN_POINT('',(-29.7665062889869,21.3443530377938,1282.35584962783));
#275012=CARTESIAN_POINT('',(-29.7665062889869,21.3443530377938,910.));
#275013=CARTESIAN_POINT('Origin',(-27.0086446004713,27.0086446004712,1282.35584962783));
#275014=CARTESIAN_POINT('Origin',(-32.7063981679208,18.886221880333,910.));
#275015=CARTESIAN_POINT('',(-32.7063981679208,18.886221880333,1282.35584962783));
#275016=CARTESIAN_POINT('',(-32.7063981679208,18.886221880333,910.));
#275017=CARTESIAN_POINT('',(-32.7063981679208,18.886221880333,1282.35584962783));
#275018=CARTESIAN_POINT('Origin',(-27.0086446004713,27.0086446004712,910.));
#275019=CARTESIAN_POINT('',(-35.1310673206094,21.3108910330216,1282.35584962783));
#275020=CARTESIAN_POINT('',(-35.1310673206094,21.3108910330216,910.));
#275021=CARTESIAN_POINT('Origin',(-27.0086446004713,27.0086446004712,1282.35584962783));
#275022=CARTESIAN_POINT('Origin',(-35.1310673206094,21.3108910330216,910.));
#275023=CARTESIAN_POINT('',(-35.1310673206094,21.3108910330216,1282.35584962783));
#275024=CARTESIAN_POINT('Origin',(-35.1310673206094,32.7063981679208,910.));
#275025=CARTESIAN_POINT('',(-35.1310673206094,32.7063981679208,1282.35584962783));
#275026=CARTESIAN_POINT('',(-35.1310673206094,32.7063981679208,910.));
#275027=CARTESIAN_POINT('',(-35.1310673206094,32.7063981679208,1282.35584962783));
#275028=CARTESIAN_POINT('Origin',(-27.0086446004713,27.0086446004712,910.));
#275029=CARTESIAN_POINT('Origin',(-27.0086446004713,27.0086446004712,1282.35584962783));
#275030=CARTESIAN_POINT('Origin',(0.,0.,1282.35584962783));
#275031=CARTESIAN_POINT('Origin',(0.,0.,-260.));
#275032=CARTESIAN_POINT('',(-51.6776446004712,45.9014446004714,-260.));
#275033=CARTESIAN_POINT('',(-49.8776446004712,44.1014446004714,-260.));
#275034=CARTESIAN_POINT('Origin',(-49.8776446004712,45.9014446004714,-260.));
#275035=CARTESIAN_POINT('',(-45.9014446004713,44.1014446004714,-260.));
#275036=CARTESIAN_POINT('',(-49.8776446004712,44.1014446004714,-260.));
#275037=CARTESIAN_POINT('',(-44.1014446004713,45.9014446004714,-260.));
#275038=CARTESIAN_POINT('Origin',(-45.9014446004713,45.9014446004714,-260.));
#275039=CARTESIAN_POINT('',(-44.1014446004713,49.8776446004712,-260.));
#275040=CARTESIAN_POINT('',(-44.1014446004713,45.9014446004714,-260.));
#275041=CARTESIAN_POINT('',(-45.9014446004713,51.6776446004712,-260.));
#275042=CARTESIAN_POINT('Origin',(-45.9014446004713,49.8776446004712,-260.));
#275043=CARTESIAN_POINT('',(-49.8776446004712,51.6776446004712,-260.));
#275044=CARTESIAN_POINT('',(-45.9014446004713,51.6776446004712,-260.));
#275045=CARTESIAN_POINT('',(-51.6776446004712,49.8776446004712,-260.));
#275046=CARTESIAN_POINT('Origin',(-49.8776446004712,49.8776446004712,-260.));
#275047=CARTESIAN_POINT('',(-51.6776446004712,49.8776446004712,-260.));
#275048=CARTESIAN_POINT('Origin',(-51.6776446004712,49.8776446004712,910.));
#275049=CARTESIAN_POINT('',(-51.6776446004712,49.8776446004712,1282.35584962783));
#275050=CARTESIAN_POINT('',(-51.6776446004712,49.8776446004712,910.));
#275051=CARTESIAN_POINT('',(-51.6776446004712,45.9014446004714,1282.35584962783));
#275052=CARTESIAN_POINT('',(-51.6776446004712,49.8776446004712,1282.35584962783));
#275053=CARTESIAN_POINT('',(-51.6776446004712,45.9014446004714,910.));
#275054=CARTESIAN_POINT('Origin',(-49.8776446004712,49.8776446004712,910.));
#275055=CARTESIAN_POINT('',(-49.8776446004712,51.6776446004712,1282.35584962783));
#275056=CARTESIAN_POINT('',(-49.8776446004712,51.6776446004712,910.));
#275057=CARTESIAN_POINT('Origin',(-49.8776446004712,49.8776446004712,1282.35584962783));
#275058=CARTESIAN_POINT('Origin',(-45.9014446004713,51.6776446004712,910.));
#275059=CARTESIAN_POINT('',(-45.9014446004713,51.6776446004712,1282.35584962783));
#275060=CARTESIAN_POINT('',(-45.9014446004713,51.6776446004712,910.));
#275061=CARTESIAN_POINT('',(-45.9014446004713,51.6776446004712,1282.35584962783));
#275062=CARTESIAN_POINT('Origin',(-45.9014446004713,49.8776446004712,910.));
#275063=CARTESIAN_POINT('',(-44.1014446004713,49.8776446004712,1282.35584962783));
#275064=CARTESIAN_POINT('',(-44.1014446004713,49.8776446004712,910.));
#275065=CARTESIAN_POINT('Origin',(-45.9014446004713,49.8776446004712,1282.35584962783));
#275066=CARTESIAN_POINT('Origin',(-44.1014446004713,45.9014446004714,910.));
#275067=CARTESIAN_POINT('',(-44.1014446004713,45.9014446004714,1282.35584962783));
#275068=CARTESIAN_POINT('',(-44.1014446004713,45.9014446004714,910.));
#275069=CARTESIAN_POINT('',(-44.1014446004713,45.9014446004714,1282.35584962783));
#275070=CARTESIAN_POINT('Origin',(-45.9014446004713,45.9014446004714,910.));
#275071=CARTESIAN_POINT('',(-45.9014446004713,44.1014446004714,1282.35584962783));
#275072=CARTESIAN_POINT('',(-45.9014446004713,44.1014446004714,910.));
#275073=CARTESIAN_POINT('Origin',(-45.9014446004713,45.9014446004714,1282.35584962783));
#275074=CARTESIAN_POINT('Origin',(-49.8776446004712,44.1014446004714,910.));
#275075=CARTESIAN_POINT('',(-49.8776446004712,44.1014446004714,1282.35584962783));
#275076=CARTESIAN_POINT('',(-49.8776446004712,44.1014446004714,910.));
#275077=CARTESIAN_POINT('',(-49.8776446004712,44.1014446004714,1282.35584962783));
#275078=CARTESIAN_POINT('Origin',(-49.8776446004712,45.9014446004714,910.));
#275079=CARTESIAN_POINT('Origin',(-49.8776446004712,45.9014446004714,1282.35584962783));
#275080=CARTESIAN_POINT('Origin',(0.,0.,1282.35584962783));
#275081=CARTESIAN_POINT('Origin',(-35.1086446004713,50.0486446004712,910.));
#275082=CARTESIAN_POINT('',(-40.9586446004713,50.0486446004712,1282.35584962783));
#275083=CARTESIAN_POINT('',(-39.1586446004713,50.0486446004712,1282.35584962783));
#275084=CARTESIAN_POINT('',(-35.1086446004713,50.0486446004712,1282.35584962783));
#275085=CARTESIAN_POINT('',(-40.9586446004713,50.0486446004712,-260.));
#275086=CARTESIAN_POINT('',(-40.9586446004713,50.0486446004712,910.));
#275087=CARTESIAN_POINT('',(-39.1586446004713,50.0486446004712,-260.));
#275088=CARTESIAN_POINT('',(-35.1086446004713,50.0486446004712,-260.));
#275089=CARTESIAN_POINT('',(-39.1586446004713,50.0486446004712,910.));
#275090=CARTESIAN_POINT('Origin',(-50.0486446004713,35.1086446004712,910.));
#275091=CARTESIAN_POINT('',(-50.0486446004713,39.1586446004712,1282.35584962783));
#275092=CARTESIAN_POINT('',(-50.0486446004713,40.9586446004712,1282.35584962783));
#275093=CARTESIAN_POINT('',(-50.0486446004713,35.1086446004712,1282.35584962783));
#275094=CARTESIAN_POINT('',(-50.0486446004713,39.1586446004712,-260.));
#275095=CARTESIAN_POINT('',(-50.0486446004713,39.1586446004712,910.));
#275096=CARTESIAN_POINT('',(-50.0486446004713,40.9586446004712,-260.));
#275097=CARTESIAN_POINT('',(-50.0486446004713,35.1086446004712,-260.));
#275098=CARTESIAN_POINT('',(-50.0486446004713,40.9586446004712,910.));
#275099=CARTESIAN_POINT('Origin',(-37.8086446004713,28.5300780298397,910.));
#275100=CARTESIAN_POINT('',(-37.8086446004713,28.5300780298397,1282.35584962783));
#275101=CARTESIAN_POINT('',(-36.9302446004713,27.0086446004712,1282.35584962783));
#275102=CARTESIAN_POINT('',(-37.8086446004713,28.5300780298397,1282.35584962783));
#275103=CARTESIAN_POINT('',(-37.8086446004713,28.5300780298397,-260.));
#275104=CARTESIAN_POINT('',(-37.8086446004713,28.5300780298397,910.));
#275105=CARTESIAN_POINT('',(-36.9302446004713,27.0086446004712,-260.));
#275106=CARTESIAN_POINT('',(-37.8086446004713,28.5300780298397,-260.));
#275107=CARTESIAN_POINT('',(-36.9302446004713,27.0086446004712,910.));
#275108=CARTESIAN_POINT('Origin',(-37.8086446004713,25.4872111711027,910.));
#275109=CARTESIAN_POINT('',(-37.8086446004713,25.4872111711027,1282.35584962783));
#275110=CARTESIAN_POINT('',(-37.8086446004713,25.4872111711027,1282.35584962783));
#275111=CARTESIAN_POINT('',(-37.8086446004713,25.4872111711027,-260.));
#275112=CARTESIAN_POINT('',(-37.8086446004713,25.4872111711027,-260.));
#275113=CARTESIAN_POINT('',(-37.8086446004713,25.4872111711027,910.));
#275114=CARTESIAN_POINT('Origin',(-37.8086446004713,19.7634173219464,910.));
#275115=CARTESIAN_POINT('',(-37.8086446004713,19.7634173219464,1282.35584962783));
#275116=CARTESIAN_POINT('',(-37.8086446004713,19.7634173219464,1282.35584962783));
#275117=CARTESIAN_POINT('',(-37.8086446004713,19.7634173219464,-260.));
#275118=CARTESIAN_POINT('',(-37.8086446004713,19.7634173219464,-260.));
#275119=CARTESIAN_POINT('',(-37.8086446004713,19.7634173219464,910.));
#275120=CARTESIAN_POINT('Origin',(-38.7086446004713,19.7634173219464,910.));
#275121=CARTESIAN_POINT('',(-38.0722484974034,19.1270212188785,1282.35584962783));
#275122=CARTESIAN_POINT('Origin',(-38.7086446004713,19.7634173219464,1282.35584962783));
#275123=CARTESIAN_POINT('',(-38.0722484974034,19.1270212188785,-260.));
#275124=CARTESIAN_POINT('Origin',(-38.7086446004713,19.7634173219464,-260.));
#275125=CARTESIAN_POINT('',(-38.0722484974034,19.1270212188785,910.));
#275126=CARTESIAN_POINT('Origin',(-44.7770212188787,12.4222484974033,910.));
#275127=CARTESIAN_POINT('',(-44.7770212188787,12.4222484974033,1282.35584962783));
#275128=CARTESIAN_POINT('',(-44.7770212188787,12.4222484974033,1282.35584962783));
#275129=CARTESIAN_POINT('',(-44.7770212188787,12.4222484974033,-260.));
#275130=CARTESIAN_POINT('',(-44.7770212188787,12.4222484974033,-260.));
#275131=CARTESIAN_POINT('',(-44.7770212188787,12.4222484974033,910.));
#275132=CARTESIAN_POINT('Origin',(-45.4134173219466,13.0586446004712,910.));
#275133=CARTESIAN_POINT('',(-45.4134173219466,12.1586446004712,1282.35584962783));
#275134=CARTESIAN_POINT('Origin',(-45.4134173219466,13.0586446004712,1282.35584962783));
#275135=CARTESIAN_POINT('',(-45.4134173219466,12.1586446004712,-260.));
#275136=CARTESIAN_POINT('Origin',(-45.4134173219466,13.0586446004712,-260.));
#275137=CARTESIAN_POINT('',(-45.4134173219466,12.1586446004712,910.));
#275138=CARTESIAN_POINT('Origin',(-49.1486446004713,12.1586446004712,910.));
#275139=CARTESIAN_POINT('',(-49.1486446004713,12.1586446004712,1282.35584962783));
#275140=CARTESIAN_POINT('',(-49.1486446004713,12.1586446004712,1282.35584962783));
#275141=CARTESIAN_POINT('',(-49.1486446004713,12.1586446004712,-260.));
#275142=CARTESIAN_POINT('',(-49.1486446004713,12.1586446004712,-260.));
#275143=CARTESIAN_POINT('',(-49.1486446004713,12.1586446004712,910.));
#275144=CARTESIAN_POINT('Origin',(-49.1486446004713,13.0586446004712,910.));
#275145=CARTESIAN_POINT('',(-50.0486446004713,13.0586446004712,1282.35584962783));
#275146=CARTESIAN_POINT('Origin',(-49.1486446004713,13.0586446004712,1282.35584962783));
#275147=CARTESIAN_POINT('',(-50.0486446004713,13.0586446004712,-260.));
#275148=CARTESIAN_POINT('Origin',(-49.1486446004713,13.0586446004712,-260.));
#275149=CARTESIAN_POINT('',(-50.0486446004713,13.0586446004712,910.));
#275150=CARTESIAN_POINT('Origin',(-50.0486446004713,18.9086446004712,910.));
#275151=CARTESIAN_POINT('',(-50.0486446004713,18.9086446004712,1282.35584962783));
#275152=CARTESIAN_POINT('',(-50.0486446004713,18.9086446004712,1282.35584962783));
#275153=CARTESIAN_POINT('',(-50.0486446004713,18.9086446004712,-260.));
#275154=CARTESIAN_POINT('',(-50.0486446004713,18.9086446004712,-260.));
#275155=CARTESIAN_POINT('',(-50.0486446004713,18.9086446004712,910.));
#275156=CARTESIAN_POINT('Origin',(-50.9486446004713,18.9086446004712,910.));
#275157=CARTESIAN_POINT('',(-50.9486446004713,19.8086446004712,1282.35584962783));
#275158=CARTESIAN_POINT('Origin',(-50.9486446004713,18.9086446004712,1282.35584962783));
#275159=CARTESIAN_POINT('',(-50.9486446004713,19.8086446004712,-260.));
#275160=CARTESIAN_POINT('Origin',(-50.9486446004713,18.9086446004712,-260.));
#275161=CARTESIAN_POINT('',(-50.9486446004713,19.8086446004712,910.));
#275162=CARTESIAN_POINT('Origin',(-53.0186446004713,19.8086446004712,910.));
#275163=CARTESIAN_POINT('',(-53.0186446004713,19.8086446004712,1282.35584962783));
#275164=CARTESIAN_POINT('',(-53.0186446004713,19.8086446004712,1282.35584962783));
#275165=CARTESIAN_POINT('',(-53.0186446004713,19.8086446004712,-260.));
#275166=CARTESIAN_POINT('',(-53.0186446004713,19.8086446004712,-260.));
#275167=CARTESIAN_POINT('',(-53.0186446004713,19.8086446004712,910.));
#275168=CARTESIAN_POINT('Origin',(-53.0186446004713,18.8186446004712,910.));
#275169=CARTESIAN_POINT('',(-53.0186446004713,18.8186446004712,1282.35584962783));
#275170=CARTESIAN_POINT('',(-53.0186446004713,18.8186446004712,1282.35584962783));
#275171=CARTESIAN_POINT('',(-53.0186446004713,18.8186446004712,-260.));
#275172=CARTESIAN_POINT('',(-53.0186446004713,18.8186446004712,-260.));
#275173=CARTESIAN_POINT('',(-53.0186446004713,18.8186446004712,910.));
#275174=CARTESIAN_POINT('Origin',(-54.0086446004713,18.8186446004712,910.));
#275175=CARTESIAN_POINT('',(-54.0086446004713,18.8186446004712,1282.35584962783));
#275176=CARTESIAN_POINT('',(-54.0086446004713,18.8186446004712,1282.35584962783));
#275177=CARTESIAN_POINT('',(-54.0086446004713,18.8186446004712,-260.));
#275178=CARTESIAN_POINT('',(-54.0086446004713,18.8186446004712,-260.));
#275179=CARTESIAN_POINT('',(-54.0086446004713,18.8186446004712,910.));
#275180=CARTESIAN_POINT('Origin',(-54.0086446004713,18.8186446004712,910.));
#275181=CARTESIAN_POINT('',(-54.0086446004715,-18.8013553995285,1282.35584962783));
#275182=CARTESIAN_POINT('',(-54.0086446004713,18.8186446004712,1282.35584962783));
#275183=CARTESIAN_POINT('',(-54.0086446004715,-18.8013553995282,-260.));
#275184=CARTESIAN_POINT('',(-54.0086446004713,18.8186446004712,-260.));
#275185=CARTESIAN_POINT('',(-54.0086446004715,-18.8013553995285,910.));
#275186=CARTESIAN_POINT('Origin',(-18.8186446004711,54.0086446004711,910.));
#275187=CARTESIAN_POINT('',(18.8013553995294,54.0086446004711,1282.35584962783));
#275188=CARTESIAN_POINT('',(-18.8186446004711,54.0086446004711,1282.35584962783));
#275189=CARTESIAN_POINT('',(-18.8186446004711,54.0086446004711,1282.35584962783));
#275190=CARTESIAN_POINT('',(18.8013553995293,54.0086446004709,-260.));
#275191=CARTESIAN_POINT('',(18.8013553995293,54.0086446004711,910.));
#275192=CARTESIAN_POINT('',(-18.8186446004711,54.0086446004711,-260.));
#275193=CARTESIAN_POINT('',(-18.8186446004711,54.0086446004711,-260.));
#275194=CARTESIAN_POINT('',(-18.8186446004711,54.0086446004711,910.));
#275195=CARTESIAN_POINT('Origin',(-18.8186446004711,54.0086446004711,910.));
#275196=CARTESIAN_POINT('',(-18.8186446004711,53.0186446004711,1282.35584962783));
#275197=CARTESIAN_POINT('',(-18.8186446004711,54.0086446004711,1282.35584962783));
#275198=CARTESIAN_POINT('',(-18.8186446004711,53.0186446004711,-260.));
#275199=CARTESIAN_POINT('',(-18.8186446004711,54.0086446004711,-260.));
#275200=CARTESIAN_POINT('',(-18.8186446004711,53.0186446004711,910.));
#275201=CARTESIAN_POINT('Origin',(-18.8186446004711,53.0186446004711,910.));
#275202=CARTESIAN_POINT('',(-19.8086446004711,53.0186446004711,1282.35584962783));
#275203=CARTESIAN_POINT('',(-18.8186446004711,53.0186446004711,1282.35584962783));
#275204=CARTESIAN_POINT('',(-19.8086446004711,53.0186446004711,-260.));
#275205=CARTESIAN_POINT('',(-18.8186446004711,53.0186446004711,-260.));
#275206=CARTESIAN_POINT('',(-19.8086446004711,53.0186446004711,910.));
#275207=CARTESIAN_POINT('Origin',(-19.8086446004711,53.0186446004711,910.));
#275208=CARTESIAN_POINT('',(-19.8086446004711,50.9486446004711,1282.35584962783));
#275209=CARTESIAN_POINT('',(-19.8086446004711,53.0186446004711,1282.35584962783));
#275210=CARTESIAN_POINT('',(-19.8086446004711,50.9486446004711,-260.));
#275211=CARTESIAN_POINT('',(-19.8086446004711,53.0186446004711,-260.));
#275212=CARTESIAN_POINT('',(-19.8086446004711,50.9486446004711,910.));
#275213=CARTESIAN_POINT('Origin',(-18.9086446004711,50.9486446004711,910.));
#275214=CARTESIAN_POINT('',(-18.9086446004711,50.0486446004711,1282.35584962783));
#275215=CARTESIAN_POINT('Origin',(-18.9086446004711,50.9486446004711,1282.35584962783));
#275216=CARTESIAN_POINT('',(-18.9086446004711,50.0486446004711,-260.));
#275217=CARTESIAN_POINT('Origin',(-18.9086446004711,50.9486446004711,-260.));
#275218=CARTESIAN_POINT('',(-18.9086446004711,50.0486446004711,910.));
#275219=CARTESIAN_POINT('Origin',(-18.9086446004711,50.0486446004711,910.));
#275220=CARTESIAN_POINT('',(-13.0586446004711,50.0486446004711,1282.35584962783));
#275221=CARTESIAN_POINT('',(-18.9086446004711,50.0486446004711,1282.35584962783));
#275222=CARTESIAN_POINT('',(-13.0586446004711,50.0486446004711,-260.));
#275223=CARTESIAN_POINT('',(-18.9086446004711,50.0486446004711,-260.));
#275224=CARTESIAN_POINT('',(-13.0586446004711,50.0486446004711,910.));
#275225=CARTESIAN_POINT('Origin',(-13.0586446004712,49.1486446004711,910.));
#275226=CARTESIAN_POINT('',(-12.1586446004712,49.1486446004711,1282.35584962783));
#275227=CARTESIAN_POINT('Origin',(-13.0586446004712,49.1486446004711,1282.35584962783));
#275228=CARTESIAN_POINT('',(-12.1586446004712,49.1486446004711,-260.));
#275229=CARTESIAN_POINT('Origin',(-13.0586446004712,49.1486446004711,-260.));
#275230=CARTESIAN_POINT('',(-12.1586446004712,49.1486446004711,910.));
#275231=CARTESIAN_POINT('Origin',(-12.1586446004712,49.1486446004711,910.));
#275232=CARTESIAN_POINT('',(-12.1586446004712,45.4134173219463,1282.35584962783));
#275233=CARTESIAN_POINT('',(-12.1586446004712,49.1486446004711,1282.35584962783));
#275234=CARTESIAN_POINT('',(-12.1586446004712,45.4134173219463,-260.));
#275235=CARTESIAN_POINT('',(-12.1586446004712,49.1486446004711,-260.));
#275236=CARTESIAN_POINT('',(-12.1586446004712,45.4134173219463,910.));
#275237=CARTESIAN_POINT('Origin',(-13.0586446004712,45.4134173219463,910.));
#275238=CARTESIAN_POINT('',(-12.4222484974033,44.7770212188784,1282.35584962783));
#275239=CARTESIAN_POINT('Origin',(-13.0586446004712,45.4134173219463,1282.35584962783));
#275240=CARTESIAN_POINT('',(-12.4222484974033,44.7770212188784,-260.));
#275241=CARTESIAN_POINT('Origin',(-13.0586446004712,45.4134173219463,-260.));
#275242=CARTESIAN_POINT('',(-12.4222484974033,44.7770212188784,910.));
#275243=CARTESIAN_POINT('Origin',(-12.4222484974033,44.7770212188784,910.));
#275244=CARTESIAN_POINT('',(-19.1270212188786,38.0722484974032,1282.35584962783));
#275245=CARTESIAN_POINT('',(-12.4222484974033,44.7770212188784,1282.35584962783));
#275246=CARTESIAN_POINT('',(-19.1270212188786,38.0722484974032,-260.));
#275247=CARTESIAN_POINT('',(-12.4222484974033,44.7770212188784,-260.));
#275248=CARTESIAN_POINT('',(-19.1270212188786,38.0722484974032,910.));
#275249=CARTESIAN_POINT('Origin',(-19.7634173219465,38.7086446004711,910.));
#275250=CARTESIAN_POINT('',(-19.7634173219465,37.8086446004711,1282.35584962783));
#275251=CARTESIAN_POINT('Origin',(-19.7634173219465,38.7086446004711,1282.35584962783));
#275252=CARTESIAN_POINT('',(-19.7634173219465,37.8086446004711,-260.));
#275253=CARTESIAN_POINT('Origin',(-19.7634173219465,38.7086446004711,-260.));
#275254=CARTESIAN_POINT('',(-19.7634173219465,37.8086446004711,910.));
#275255=CARTESIAN_POINT('Origin',(-19.7634173219465,37.8086446004711,910.));
#275256=CARTESIAN_POINT('',(-25.4872111711027,37.8086446004712,1282.35584962783));
#275257=CARTESIAN_POINT('',(-19.7634173219465,37.8086446004711,1282.35584962783));
#275258=CARTESIAN_POINT('',(-25.4872111711027,37.8086446004712,-260.));
#275259=CARTESIAN_POINT('',(-19.7634173219465,37.8086446004711,-260.));
#275260=CARTESIAN_POINT('',(-25.4872111711027,37.8086446004712,910.));
#275261=CARTESIAN_POINT('Origin',(-25.4872111711027,37.8086446004712,910.));
#275262=CARTESIAN_POINT('',(-27.0086446004713,36.9302446004712,1282.35584962783));
#275263=CARTESIAN_POINT('',(-25.4872111711027,37.8086446004712,1282.35584962783));
#275264=CARTESIAN_POINT('',(-27.0086446004713,36.9302446004712,-260.));
#275265=CARTESIAN_POINT('',(-25.4872111711027,37.8086446004712,-260.));
#275266=CARTESIAN_POINT('',(-27.0086446004713,36.9302446004712,910.));
#275267=CARTESIAN_POINT('Origin',(-28.5300780298398,37.8086446004712,910.));
#275268=CARTESIAN_POINT('',(-28.5300780298398,37.8086446004712,1282.35584962783));
#275269=CARTESIAN_POINT('',(-28.5300780298398,37.8086446004712,1282.35584962783));
#275270=CARTESIAN_POINT('',(-28.5300780298398,37.8086446004712,-260.));
#275271=CARTESIAN_POINT('',(-28.5300780298398,37.8086446004712,-260.));
#275272=CARTESIAN_POINT('',(-28.5300780298398,37.8086446004712,910.));
#275273=CARTESIAN_POINT('Origin',(-34.2538718789961,37.8086446004712,910.));
#275274=CARTESIAN_POINT('',(-34.2538718789961,37.8086446004712,1282.35584962783));
#275275=CARTESIAN_POINT('',(-34.2538718789961,37.8086446004712,1282.35584962783));
#275276=CARTESIAN_POINT('',(-34.2538718789961,37.8086446004712,-260.));
#275277=CARTESIAN_POINT('',(-34.2538718789961,37.8086446004712,-260.));
#275278=CARTESIAN_POINT('',(-34.2538718789961,37.8086446004712,910.));
#275279=CARTESIAN_POINT('Origin',(-34.2538718789961,38.7086446004712,910.));
#275280=CARTESIAN_POINT('',(-34.890267982064,38.0722484974033,1282.35584962783));
#275281=CARTESIAN_POINT('Origin',(-34.2538718789961,38.7086446004712,1282.35584962783));
#275282=CARTESIAN_POINT('',(-34.890267982064,38.0722484974033,-260.));
#275283=CARTESIAN_POINT('Origin',(-34.2538718789961,38.7086446004712,-260.));
#275284=CARTESIAN_POINT('',(-34.890267982064,38.0722484974033,910.));
#275285=CARTESIAN_POINT('Origin',(-41.5950407035392,44.7770212188785,910.));
#275286=CARTESIAN_POINT('',(-41.5950407035392,44.7770212188785,1282.35584962783));
#275287=CARTESIAN_POINT('',(-41.5950407035392,44.7770212188785,1282.35584962783));
#275288=CARTESIAN_POINT('',(-41.5950407035392,44.7770212188785,-260.));
#275289=CARTESIAN_POINT('',(-41.5950407035392,44.7770212188785,-260.));
#275290=CARTESIAN_POINT('',(-41.5950407035392,44.7770212188785,910.));
#275291=CARTESIAN_POINT('Origin',(-40.9586446004713,45.4134173219464,910.));
#275292=CARTESIAN_POINT('',(-41.8586446004713,45.4134173219464,1282.35584962783));
#275293=CARTESIAN_POINT('Origin',(-40.9586446004713,45.4134173219464,1282.35584962783));
#275294=CARTESIAN_POINT('',(-41.8586446004713,45.4134173219464,-260.));
#275295=CARTESIAN_POINT('Origin',(-40.9586446004713,45.4134173219464,-260.));
#275296=CARTESIAN_POINT('',(-41.8586446004713,45.4134173219464,910.));
#275297=CARTESIAN_POINT('Origin',(-41.8586446004713,49.1486446004712,910.));
#275298=CARTESIAN_POINT('',(-41.8586446004713,49.1486446004712,1282.35584962783));
#275299=CARTESIAN_POINT('',(-41.8586446004713,49.1486446004712,1282.35584962783));
#275300=CARTESIAN_POINT('',(-41.8586446004713,49.1486446004712,-260.));
#275301=CARTESIAN_POINT('',(-41.8586446004713,49.1486446004712,-260.));
#275302=CARTESIAN_POINT('',(-41.8586446004713,49.1486446004712,910.));
#275303=CARTESIAN_POINT('Origin',(-40.9586446004713,49.1486446004712,910.));
#275304=CARTESIAN_POINT('Origin',(-40.9586446004713,49.1486446004712,1282.35584962783));
#275305=CARTESIAN_POINT('Origin',(-40.9586446004713,49.1486446004712,-260.));
#275306=CARTESIAN_POINT('Origin',(-35.1086446004713,50.0486446004712,910.));
#275307=CARTESIAN_POINT('',(-37.5386446004713,50.0486446004712,1282.35584962783));
#275308=CARTESIAN_POINT('',(-35.1086446004713,50.0486446004712,1282.35584962783));
#275309=CARTESIAN_POINT('',(-35.1086446004713,50.0486446004712,1282.35584962783));
#275310=CARTESIAN_POINT('',(-37.5386446004713,50.0486446004712,-260.));
#275311=CARTESIAN_POINT('',(-37.5386446004713,50.0486446004712,910.));
#275312=CARTESIAN_POINT('',(-35.1086446004713,50.0486446004712,-260.));
#275313=CARTESIAN_POINT('',(-35.1086446004713,50.0486446004712,-260.));
#275314=CARTESIAN_POINT('',(-35.1086446004713,50.0486446004712,910.));
#275315=CARTESIAN_POINT('Origin',(-35.1086446004713,50.9486446004712,910.));
#275316=CARTESIAN_POINT('',(-34.2086446004713,50.9486446004712,1282.35584962783));
#275317=CARTESIAN_POINT('Origin',(-35.1086446004713,50.9486446004712,1282.35584962783));
#275318=CARTESIAN_POINT('',(-34.2086446004713,50.9486446004712,-260.));
#275319=CARTESIAN_POINT('Origin',(-35.1086446004713,50.9486446004712,-260.));
#275320=CARTESIAN_POINT('',(-34.2086446004713,50.9486446004712,910.));
#275321=CARTESIAN_POINT('Origin',(-34.2086446004713,53.0186446004712,910.));
#275322=CARTESIAN_POINT('',(-34.2086446004713,53.0186446004712,1282.35584962783));
#275323=CARTESIAN_POINT('',(-34.2086446004713,53.0186446004712,1282.35584962783));
#275324=CARTESIAN_POINT('',(-34.2086446004713,53.0186446004712,-260.));
#275325=CARTESIAN_POINT('',(-34.2086446004713,53.0186446004712,-260.));
#275326=CARTESIAN_POINT('',(-34.2086446004713,53.0186446004712,910.));
#275327=CARTESIAN_POINT('Origin',(-35.1986446004713,53.0186446004712,910.));
#275328=CARTESIAN_POINT('',(-35.1986446004713,53.0186446004712,1282.35584962783));
#275329=CARTESIAN_POINT('',(-35.1986446004713,53.0186446004712,1282.35584962783));
#275330=CARTESIAN_POINT('',(-35.1986446004713,53.0186446004712,-260.));
#275331=CARTESIAN_POINT('',(-35.1986446004713,53.0186446004712,-260.));
#275332=CARTESIAN_POINT('',(-35.1986446004713,53.0186446004712,910.));
#275333=CARTESIAN_POINT('Origin',(-35.1986446004713,54.0086446004712,910.));
#275334=CARTESIAN_POINT('',(-35.1986446004713,54.0086446004712,1282.35584962783));
#275335=CARTESIAN_POINT('',(-35.1986446004713,54.0086446004712,1282.35584962783));
#275336=CARTESIAN_POINT('',(-35.1986446004713,54.0086446004712,-260.));
#275337=CARTESIAN_POINT('',(-35.1986446004713,54.0086446004712,-260.));
#275338=CARTESIAN_POINT('',(-35.1986446004713,54.0086446004712,910.));
#275339=CARTESIAN_POINT('Origin',(-35.1986446004713,54.0086446004712,910.));
#275340=CARTESIAN_POINT('',(-50.3510446004713,54.0086446004712,1282.35584962783));
#275341=CARTESIAN_POINT('',(-35.1986446004713,54.0086446004712,1282.35584962783));
#275342=CARTESIAN_POINT('',(-50.3510446004713,54.0086446004712,-260.));
#275343=CARTESIAN_POINT('',(-35.1986446004713,54.0086446004712,-260.));
#275344=CARTESIAN_POINT('',(-50.3510446004713,54.0086446004712,910.));
#275345=CARTESIAN_POINT('Origin',(-50.3510446004712,50.3510446004711,910.));
#275346=CARTESIAN_POINT('',(-54.0086446004713,50.3510446004711,1282.35584962783));
#275347=CARTESIAN_POINT('Origin',(-50.3510446004712,50.3510446004711,1282.35584962783));
#275348=CARTESIAN_POINT('',(-54.0086446004713,50.3510446004711,-260.));
#275349=CARTESIAN_POINT('Origin',(-50.3510446004712,50.3510446004711,-260.));
#275350=CARTESIAN_POINT('',(-54.0086446004713,50.3510446004711,910.));
#275351=CARTESIAN_POINT('Origin',(-54.0086446004713,35.1986446004712,910.));
#275352=CARTESIAN_POINT('',(-54.0086446004713,35.1986446004712,1282.35584962783));
#275353=CARTESIAN_POINT('',(-54.0086446004713,35.1986446004712,1282.35584962783));
#275354=CARTESIAN_POINT('',(-54.0086446004713,35.1986446004712,-260.));
#275355=CARTESIAN_POINT('',(-54.0086446004713,35.1986446004712,-260.));
#275356=CARTESIAN_POINT('',(-54.0086446004713,35.1986446004712,910.));
#275357=CARTESIAN_POINT('Origin',(-54.0086446004713,35.1986446004712,910.));
#275358=CARTESIAN_POINT('',(-53.0186446004713,35.1986446004712,1282.35584962783));
#275359=CARTESIAN_POINT('',(-54.0086446004713,35.1986446004712,1282.35584962783));
#275360=CARTESIAN_POINT('',(-53.0186446004713,35.1986446004712,-260.));
#275361=CARTESIAN_POINT('',(-54.0086446004713,35.1986446004712,-260.));
#275362=CARTESIAN_POINT('',(-53.0186446004713,35.1986446004712,910.));
#275363=CARTESIAN_POINT('Origin',(-53.0186446004713,35.1986446004712,910.));
#275364=CARTESIAN_POINT('',(-53.0186446004713,34.2086446004712,1282.35584962783));
#275365=CARTESIAN_POINT('',(-53.0186446004713,35.1986446004712,1282.35584962783));
#275366=CARTESIAN_POINT('',(-53.0186446004713,34.2086446004712,-260.));
#275367=CARTESIAN_POINT('',(-53.0186446004713,35.1986446004712,-260.));
#275368=CARTESIAN_POINT('',(-53.0186446004713,34.2086446004712,910.));
#275369=CARTESIAN_POINT('Origin',(-53.0186446004713,34.2086446004712,910.));
#275370=CARTESIAN_POINT('',(-50.9486446004713,34.2086446004712,1282.35584962783));
#275371=CARTESIAN_POINT('',(-53.0186446004713,34.2086446004712,1282.35584962783));
#275372=CARTESIAN_POINT('',(-50.9486446004713,34.2086446004712,-260.));
#275373=CARTESIAN_POINT('',(-53.0186446004713,34.2086446004712,-260.));
#275374=CARTESIAN_POINT('',(-50.9486446004713,34.2086446004712,910.));
#275375=CARTESIAN_POINT('Origin',(-50.9486446004713,35.1086446004712,910.));
#275376=CARTESIAN_POINT('',(-50.0486446004713,35.1086446004712,1282.35584962783));
#275377=CARTESIAN_POINT('Origin',(-50.9486446004713,35.1086446004712,1282.35584962783));
#275378=CARTESIAN_POINT('',(-50.0486446004713,35.1086446004712,-260.));
#275379=CARTESIAN_POINT('Origin',(-50.9486446004713,35.1086446004712,-260.));
#275380=CARTESIAN_POINT('',(-50.0486446004713,35.1086446004712,910.));
#275381=CARTESIAN_POINT('Origin',(-50.0486446004713,35.1086446004712,910.));
#275382=CARTESIAN_POINT('',(-50.0486446004713,37.5386446004715,1282.35584962783));
#275383=CARTESIAN_POINT('',(-50.0486446004713,35.1086446004712,1282.35584962783));
#275384=CARTESIAN_POINT('',(-50.0486446004712,37.5386446004714,-260.));
#275385=CARTESIAN_POINT('',(-50.0486446004713,35.1086446004712,-260.));
#275386=CARTESIAN_POINT('',(-50.0486446004713,37.5386446004715,910.));
#275387=CARTESIAN_POINT('Origin',(-49.1486446004713,40.9586446004712,910.));
#275388=CARTESIAN_POINT('',(-49.1486446004713,41.8586446004712,1282.35584962783));
#275389=CARTESIAN_POINT('Origin',(-49.1486446004713,40.9586446004712,1282.35584962783));
#275390=CARTESIAN_POINT('',(-49.1486446004713,41.8586446004712,-260.));
#275391=CARTESIAN_POINT('Origin',(-49.1486446004713,40.9586446004712,-260.));
#275392=CARTESIAN_POINT('',(-49.1486446004713,41.8586446004712,910.));
#275393=CARTESIAN_POINT('Origin',(-49.1486446004713,41.8586446004712,910.));
#275394=CARTESIAN_POINT('',(-45.4134173219466,41.8586446004712,1282.35584962783));
#275395=CARTESIAN_POINT('',(-49.1486446004713,41.8586446004712,1282.35584962783));
#275396=CARTESIAN_POINT('',(-45.4134173219466,41.8586446004712,-260.));
#275397=CARTESIAN_POINT('',(-49.1486446004713,41.8586446004712,-260.));
#275398=CARTESIAN_POINT('',(-45.4134173219466,41.8586446004712,910.));
#275399=CARTESIAN_POINT('Origin',(-45.4134173219466,40.9586446004712,910.));
#275400=CARTESIAN_POINT('',(-44.7770212188787,41.5950407035391,1282.35584962783));
#275401=CARTESIAN_POINT('Origin',(-45.4134173219466,40.9586446004712,1282.35584962783));
#275402=CARTESIAN_POINT('',(-44.7770212188787,41.5950407035391,-260.));
#275403=CARTESIAN_POINT('Origin',(-45.4134173219466,40.9586446004712,-260.));
#275404=CARTESIAN_POINT('',(-44.7770212188787,41.5950407035391,910.));
#275405=CARTESIAN_POINT('Origin',(-44.7770212188787,41.5950407035391,910.));
#275406=CARTESIAN_POINT('',(-38.0722484974034,34.8902679820638,1282.35584962783));
#275407=CARTESIAN_POINT('',(-44.7770212188787,41.5950407035391,1282.35584962783));
#275408=CARTESIAN_POINT('',(-38.0722484974034,34.8902679820638,-260.));
#275409=CARTESIAN_POINT('',(-44.7770212188787,41.5950407035391,-260.));
#275410=CARTESIAN_POINT('',(-38.0722484974034,34.8902679820638,910.));
#275411=CARTESIAN_POINT('Origin',(-38.7086446004713,34.2538718789959,910.));
#275412=CARTESIAN_POINT('',(-37.8086446004713,34.2538718789959,1282.35584962783));
#275413=CARTESIAN_POINT('Origin',(-38.7086446004713,34.2538718789959,1282.35584962783));
#275414=CARTESIAN_POINT('',(-37.8086446004713,34.2538718789959,-260.));
#275415=CARTESIAN_POINT('Origin',(-38.7086446004713,34.2538718789959,-260.));
#275416=CARTESIAN_POINT('',(-37.8086446004713,34.2538718789959,910.));
#275417=CARTESIAN_POINT('Origin',(-37.8086446004713,34.2538718789959,910.));
#275418=CARTESIAN_POINT('',(-37.8086446004713,34.2538718789959,1282.35584962783));
#275419=CARTESIAN_POINT('',(-37.8086446004713,34.2538718789959,-260.));
#275420=CARTESIAN_POINT('Origin',(28.5127888288977,37.8086446004711,910.));
#275421=CARTESIAN_POINT('',(28.5127888288978,37.808644600471,1282.35584962783));
#275422=CARTESIAN_POINT('',(26.9913553995293,36.930244600471,1282.35584962783));
#275423=CARTESIAN_POINT('',(28.5127888288978,37.808644600471,1282.35584962783));
#275424=CARTESIAN_POINT('',(28.5127888288977,37.8086446004714,-260.));
#275425=CARTESIAN_POINT('',(28.5127888288977,37.8086446004711,910.));
#275426=CARTESIAN_POINT('',(26.9913553995292,36.9302446004712,-260.));
#275427=CARTESIAN_POINT('',(28.5127888288975,37.8086446004713,-260.));
#275428=CARTESIAN_POINT('',(26.9913553995292,36.9302446004711,910.));
#275429=CARTESIAN_POINT('Origin',(25.4699219701607,37.8086446004711,910.));
#275430=CARTESIAN_POINT('',(25.4699219701608,37.808644600471,1282.35584962783));
#275431=CARTESIAN_POINT('',(25.4699219701607,37.8086446004711,1282.35584962783));
#275432=CARTESIAN_POINT('',(25.4699219701607,37.8086446004713,-260.));
#275433=CARTESIAN_POINT('',(25.4699219701605,37.8086446004713,-260.));
#275434=CARTESIAN_POINT('',(25.4699219701607,37.8086446004711,910.));
#275435=CARTESIAN_POINT('Origin',(19.7461281210045,37.8086446004711,910.));
#275436=CARTESIAN_POINT('',(19.7461281210046,37.808644600471,1282.35584962783));
#275437=CARTESIAN_POINT('',(19.7461281210045,37.808644600471,1282.35584962783));
#275438=CARTESIAN_POINT('',(19.7461281210043,37.8086446004713,-260.));
#275439=CARTESIAN_POINT('',(19.7461281210043,37.8086446004713,-260.));
#275440=CARTESIAN_POINT('',(19.7461281210045,37.8086446004711,910.));
#275441=CARTESIAN_POINT('Origin',(19.7461281210045,38.7086446004711,910.));
#275442=CARTESIAN_POINT('',(19.1097320179367,38.0722484974032,1282.35584962783));
#275443=CARTESIAN_POINT('Origin',(19.7461281210046,38.708644600471,1282.35584962783));
#275444=CARTESIAN_POINT('',(19.1097320179366,38.0722484974032,-260.));
#275445=CARTESIAN_POINT('Origin',(19.7461281210043,38.7086446004713,-260.));
#275446=CARTESIAN_POINT('',(19.1097320179366,38.0722484974032,910.));
#275447=CARTESIAN_POINT('Origin',(12.4049592964614,44.7770212188785,910.));
#275448=CARTESIAN_POINT('',(12.4049592964614,44.7770212188784,1282.35584962783));
#275449=CARTESIAN_POINT('',(12.4049592964614,44.7770212188785,1282.35584962783));
#275450=CARTESIAN_POINT('',(12.4049592964612,44.7770212188787,-260.));
#275451=CARTESIAN_POINT('',(12.4049592964612,44.7770212188787,-260.));
#275452=CARTESIAN_POINT('',(12.4049592964614,44.7770212188785,910.));
#275453=CARTESIAN_POINT('Origin',(13.0413553995293,45.4134173219464,910.));
#275454=CARTESIAN_POINT('',(12.1413553995293,45.4134173219463,1282.35584962783));
#275455=CARTESIAN_POINT('Origin',(13.0413553995293,45.4134173219463,1282.35584962783));
#275456=CARTESIAN_POINT('',(12.1413553995291,45.4134173219464,-260.));
#275457=CARTESIAN_POINT('Origin',(13.041355399529,45.4134173219466,-260.));
#275458=CARTESIAN_POINT('',(12.1413553995293,45.4134173219464,910.));
#275459=CARTESIAN_POINT('Origin',(12.1413553995293,49.1486446004711,910.));
#275460=CARTESIAN_POINT('',(12.1413553995293,49.1486446004711,1282.35584962783));
#275461=CARTESIAN_POINT('',(12.1413553995293,49.1486446004711,1282.35584962783));
#275462=CARTESIAN_POINT('',(12.1413553995291,49.1486446004713,-260.));
#275463=CARTESIAN_POINT('',(12.1413553995291,49.1486446004713,-260.));
#275464=CARTESIAN_POINT('',(12.1413553995293,49.1486446004711,910.));
#275465=CARTESIAN_POINT('Origin',(13.0413553995293,49.1486446004711,910.));
#275466=CARTESIAN_POINT('',(13.0413553995293,50.0486446004711,1282.35584962783));
#275467=CARTESIAN_POINT('Origin',(13.0413553995293,49.1486446004711,1282.35584962783));
#275468=CARTESIAN_POINT('',(13.0413553995291,50.0486446004713,-260.));
#275469=CARTESIAN_POINT('Origin',(13.0413553995291,49.1486446004713,-260.));
#275470=CARTESIAN_POINT('',(13.0413553995293,50.0486446004711,910.));
#275471=CARTESIAN_POINT('Origin',(18.8913553995293,50.0486446004711,910.));
#275472=CARTESIAN_POINT('',(18.8913553995294,50.048644600471,1282.35584962783));
#275473=CARTESIAN_POINT('',(18.8913553995293,50.048644600471,1282.35584962783));
#275474=CARTESIAN_POINT('',(18.8913553995291,50.0486446004713,-260.));
#275475=CARTESIAN_POINT('',(18.8913553995291,50.0486446004713,-260.));
#275476=CARTESIAN_POINT('',(18.8913553995293,50.0486446004711,910.));
#275477=CARTESIAN_POINT('Origin',(18.8913553995293,50.9486446004711,910.));
#275478=CARTESIAN_POINT('',(19.7913553995294,50.948644600471,1282.35584962783));
#275479=CARTESIAN_POINT('Origin',(18.8913553995294,50.948644600471,1282.35584962783));
#275480=CARTESIAN_POINT('',(19.7913553995291,50.9486446004711,-260.));
#275481=CARTESIAN_POINT('Origin',(18.8913553995291,50.9486446004713,-260.));
#275482=CARTESIAN_POINT('',(19.7913553995293,50.9486446004711,910.));
#275483=CARTESIAN_POINT('Origin',(19.7913553995293,53.0186446004711,910.));
#275484=CARTESIAN_POINT('',(19.7913553995294,53.018644600471,1282.35584962783));
#275485=CARTESIAN_POINT('',(19.7913553995294,53.0186446004711,1282.35584962783));
#275486=CARTESIAN_POINT('',(19.7913553995293,53.0186446004713,-260.));
#275487=CARTESIAN_POINT('',(19.7913553995291,53.0186446004713,-260.));
#275488=CARTESIAN_POINT('',(19.7913553995293,53.0186446004711,910.));
#275489=CARTESIAN_POINT('Origin',(18.8013553995293,53.0186446004711,910.));
#275490=CARTESIAN_POINT('',(18.8013553995294,53.018644600471,1282.35584962783));
#275491=CARTESIAN_POINT('',(18.8013553995293,53.018644600471,1282.35584962783));
#275492=CARTESIAN_POINT('',(18.8013553995291,53.0186446004711,-260.));
#275493=CARTESIAN_POINT('',(18.8013553995291,53.0186446004713,-260.));
#275494=CARTESIAN_POINT('',(18.8013553995293,53.0186446004711,910.));
#275495=CARTESIAN_POINT('Origin',(18.8013553995293,54.0086446004711,910.));
#275496=CARTESIAN_POINT('',(18.8013553995294,54.0086446004711,1282.35584962783));
#275497=CARTESIAN_POINT('',(18.8013553995291,54.0086446004713,-260.));
#275498=CARTESIAN_POINT('Origin',(53.9913553995291,18.8186446004708,910.));
#275499=CARTESIAN_POINT('',(53.9913553995291,-18.8013553995294,1282.35584962783));
#275500=CARTESIAN_POINT('',(53.9913553995292,18.8186446004707,1282.35584962783));
#275501=CARTESIAN_POINT('',(53.9913553995292,18.8186446004708,1282.35584962783));
#275502=CARTESIAN_POINT('',(53.9913553995285,-18.8013553995292,-260.));
#275503=CARTESIAN_POINT('',(53.9913553995291,-18.8013553995292,910.));
#275504=CARTESIAN_POINT('',(53.9913553995291,18.818644600471,-260.));
#275505=CARTESIAN_POINT('',(53.9913553995289,18.818644600471,-260.));
#275506=CARTESIAN_POINT('',(53.9913553995291,18.8186446004708,910.));
#275507=CARTESIAN_POINT('Origin',(53.9913553995291,18.8186446004708,910.));
#275508=CARTESIAN_POINT('',(53.0013553995292,18.8186446004707,1282.35584962783));
#275509=CARTESIAN_POINT('',(53.9913553995291,18.8186446004707,1282.35584962783));
#275510=CARTESIAN_POINT('',(53.0013553995289,18.8186446004708,-260.));
#275511=CARTESIAN_POINT('',(53.9913553995289,18.818644600471,-260.));
#275512=CARTESIAN_POINT('',(53.0013553995291,18.8186446004708,910.));
#275513=CARTESIAN_POINT('Origin',(53.0013553995291,18.8186446004708,910.));
#275514=CARTESIAN_POINT('',(53.0013553995292,19.8086446004707,1282.35584962783));
#275515=CARTESIAN_POINT('',(53.0013553995292,18.8186446004708,1282.35584962783));
#275516=CARTESIAN_POINT('',(53.0013553995291,19.808644600471,-260.));
#275517=CARTESIAN_POINT('',(53.0013553995289,18.818644600471,-260.));
#275518=CARTESIAN_POINT('',(53.0013553995291,19.8086446004708,910.));
#275519=CARTESIAN_POINT('Origin',(53.0013553995291,19.8086446004708,910.));
#275520=CARTESIAN_POINT('',(50.9313553995292,19.8086446004708,1282.35584962783));
#275521=CARTESIAN_POINT('',(53.0013553995291,19.8086446004707,1282.35584962783));
#275522=CARTESIAN_POINT('',(50.9313553995289,19.808644600471,-260.));
#275523=CARTESIAN_POINT('',(53.0013553995289,19.808644600471,-260.));
#275524=CARTESIAN_POINT('',(50.9313553995291,19.8086446004708,910.));
#275525=CARTESIAN_POINT('Origin',(50.9313553995291,18.9086446004708,910.));
#275526=CARTESIAN_POINT('',(50.0313553995292,18.9086446004708,1282.35584962783));
#275527=CARTESIAN_POINT('Origin',(50.9313553995292,18.9086446004708,1282.35584962783));
#275528=CARTESIAN_POINT('',(50.0313553995289,18.9086446004711,-260.));
#275529=CARTESIAN_POINT('Origin',(50.9313553995289,18.908644600471,-260.));
#275530=CARTESIAN_POINT('',(50.0313553995291,18.9086446004708,910.));
#275531=CARTESIAN_POINT('Origin',(50.0313553995291,18.9086446004708,910.));
#275532=CARTESIAN_POINT('',(50.0313553995291,13.0586446004708,1282.35584962783));
#275533=CARTESIAN_POINT('',(50.0313553995292,18.9086446004708,1282.35584962783));
#275534=CARTESIAN_POINT('',(50.0313553995288,13.0586446004711,-260.));
#275535=CARTESIAN_POINT('',(50.0313553995289,18.9086446004711,-260.));
#275536=CARTESIAN_POINT('',(50.031355399529,13.0586446004708,910.));
#275537=CARTESIAN_POINT('Origin',(49.131355399529,13.0586446004708,910.));
#275538=CARTESIAN_POINT('',(49.1313553995291,12.1586446004708,1282.35584962783));
#275539=CARTESIAN_POINT('Origin',(49.1313553995291,13.0586446004708,1282.35584962783));
#275540=CARTESIAN_POINT('',(49.131355399529,12.1586446004711,-260.));
#275541=CARTESIAN_POINT('Origin',(49.1313553995288,13.0586446004711,-260.));
#275542=CARTESIAN_POINT('',(49.131355399529,12.1586446004708,910.));
#275543=CARTESIAN_POINT('Origin',(49.131355399529,12.1586446004708,910.));
#275544=CARTESIAN_POINT('',(45.3961281210043,12.1586446004708,1282.35584962783));
#275545=CARTESIAN_POINT('',(49.131355399529,12.1586446004708,1282.35584962783));
#275546=CARTESIAN_POINT('',(45.3961281210041,12.1586446004711,-260.));
#275547=CARTESIAN_POINT('',(49.1313553995288,12.1586446004711,-260.));
#275548=CARTESIAN_POINT('',(45.3961281210043,12.1586446004709,910.));
#275549=CARTESIAN_POINT('Origin',(45.3961281210043,13.0586446004709,910.));
#275550=CARTESIAN_POINT('',(44.7597320179365,12.4222484974029,1282.35584962783));
#275551=CARTESIAN_POINT('Origin',(45.3961281210044,13.0586446004708,1282.35584962783));
#275552=CARTESIAN_POINT('',(44.7597320179364,12.422248497403,-260.));
#275553=CARTESIAN_POINT('Origin',(45.3961281210041,13.0586446004711,-260.));
#275554=CARTESIAN_POINT('',(44.7597320179364,12.422248497403,910.));
#275555=CARTESIAN_POINT('Origin',(44.7597320179364,12.422248497403,910.));
#275556=CARTESIAN_POINT('',(38.0549592964613,19.1270212188783,1282.35584962783));
#275557=CARTESIAN_POINT('',(44.7597320179364,12.422248497403,1282.35584962783));
#275558=CARTESIAN_POINT('',(38.054959296461,19.1270212188785,-260.));
#275559=CARTESIAN_POINT('',(44.7597320179362,12.4222484974032,-260.));
#275560=CARTESIAN_POINT('',(38.0549592964612,19.1270212188783,910.));
#275561=CARTESIAN_POINT('Origin',(38.6913553995291,19.7634173219462,910.));
#275562=CARTESIAN_POINT('',(37.7913553995292,19.7634173219462,1282.35584962783));
#275563=CARTESIAN_POINT('Origin',(38.6913553995292,19.7634173219461,1282.35584962783));
#275564=CARTESIAN_POINT('',(37.7913553995289,19.7634173219462,-260.));
#275565=CARTESIAN_POINT('Origin',(38.6913553995289,19.7634173219464,-260.));
#275566=CARTESIAN_POINT('',(37.7913553995291,19.7634173219462,910.));
#275567=CARTESIAN_POINT('Origin',(37.7913553995291,19.7634173219462,910.));
#275568=CARTESIAN_POINT('',(37.7913553995292,25.4872111711024,1282.35584962783));
#275569=CARTESIAN_POINT('',(37.7913553995292,19.7634173219462,1282.35584962783));
#275570=CARTESIAN_POINT('',(37.7913553995291,25.4872111711025,-260.));
#275571=CARTESIAN_POINT('',(37.7913553995289,19.7634173219464,-260.));
#275572=CARTESIAN_POINT('',(37.7913553995292,25.4872111711025,910.));
#275573=CARTESIAN_POINT('Origin',(37.7913553995292,25.4872111711025,910.));
#275574=CARTESIAN_POINT('',(36.9129553995293,27.008644600471,1282.35584962783));
#275575=CARTESIAN_POINT('',(37.7913553995292,25.4872111711025,1282.35584962783));
#275576=CARTESIAN_POINT('',(36.9129553995288,27.0086446004711,-260.));
#275577=CARTESIAN_POINT('',(37.791355399529,25.4872111711027,-260.));
#275578=CARTESIAN_POINT('',(36.9129553995292,27.0086446004711,910.));
#275579=CARTESIAN_POINT('Origin',(37.7913553995292,28.5300780298395,910.));
#275580=CARTESIAN_POINT('',(37.7913553995293,28.5300780298395,1282.35584962783));
#275581=CARTESIAN_POINT('',(37.7913553995293,28.5300780298395,1282.35584962783));
#275582=CARTESIAN_POINT('',(37.791355399529,28.5300780298395,-260.));
#275583=CARTESIAN_POINT('',(37.791355399529,28.5300780298398,-260.));
#275584=CARTESIAN_POINT('',(37.7913553995292,28.5300780298395,910.));
#275585=CARTESIAN_POINT('Origin',(37.7913553995292,34.2538718789958,910.));
#275586=CARTESIAN_POINT('',(37.7913553995293,34.2538718789957,1282.35584962783));
#275587=CARTESIAN_POINT('',(37.7913553995293,34.2538718789958,1282.35584962783));
#275588=CARTESIAN_POINT('',(37.791355399529,34.253871878996,-260.));
#275589=CARTESIAN_POINT('',(37.791355399529,34.253871878996,-260.));
#275590=CARTESIAN_POINT('',(37.7913553995292,34.2538718789958,910.));
#275591=CARTESIAN_POINT('Origin',(38.6913553995292,34.2538718789958,910.));
#275592=CARTESIAN_POINT('',(38.0549592964614,34.8902679820636,1282.35584962783));
#275593=CARTESIAN_POINT('Origin',(38.6913553995293,34.2538718789957,1282.35584962783));
#275594=CARTESIAN_POINT('',(38.0549592964611,34.8902679820639,-260.));
#275595=CARTESIAN_POINT('Origin',(38.691355399529,34.253871878996,-260.));
#275596=CARTESIAN_POINT('',(38.0549592964613,34.8902679820637,910.));
#275597=CARTESIAN_POINT('Origin',(44.7597320179366,41.5950407035389,910.));
#275598=CARTESIAN_POINT('',(44.7597320179367,41.5950407035389,1282.35584962783));
#275599=CARTESIAN_POINT('',(44.7597320179367,41.5950407035389,1282.35584962783));
#275600=CARTESIAN_POINT('',(44.7597320179364,41.5950407035391,-260.));
#275601=CARTESIAN_POINT('',(44.7597320179364,41.5950407035391,-260.));
#275602=CARTESIAN_POINT('',(44.7597320179366,41.5950407035389,910.));
#275603=CARTESIAN_POINT('Origin',(45.3961281210045,40.958644600471,910.));
#275604=CARTESIAN_POINT('',(45.3961281210046,41.858644600471,1282.35584962783));
#275605=CARTESIAN_POINT('Origin',(45.3961281210046,40.958644600471,1282.35584962783));
#275606=CARTESIAN_POINT('',(45.3961281210043,41.8586446004712,-260.));
#275607=CARTESIAN_POINT('Origin',(45.3961281210043,40.9586446004712,-260.));
#275608=CARTESIAN_POINT('',(45.3961281210045,41.858644600471,910.));
#275609=CARTESIAN_POINT('Origin',(49.1313553995292,41.858644600471,910.));
#275610=CARTESIAN_POINT('',(49.1313553995293,41.858644600471,1282.35584962783));
#275611=CARTESIAN_POINT('',(49.1313553995292,41.858644600471,1282.35584962783));
#275612=CARTESIAN_POINT('',(49.131355399529,41.8586446004712,-260.));
#275613=CARTESIAN_POINT('',(49.131355399529,41.8586446004712,-260.));
#275614=CARTESIAN_POINT('',(49.1313553995292,41.858644600471,910.));
#275615=CARTESIAN_POINT('Origin',(49.1313553995292,40.958644600471,910.));
#275616=CARTESIAN_POINT('',(50.0313553995293,40.9586446004709,1282.35584962783));
#275617=CARTESIAN_POINT('Origin',(49.1313553995293,40.958644600471,1282.35584962783));
#275618=CARTESIAN_POINT('',(50.031355399529,40.9586446004712,-260.));
#275619=CARTESIAN_POINT('Origin',(49.131355399529,40.9586446004712,-260.));
#275620=CARTESIAN_POINT('',(50.0313553995292,40.958644600471,910.));
#275621=CARTESIAN_POINT('Origin',(50.0313553995292,35.108644600471,910.));
#275622=CARTESIAN_POINT('',(50.0313553995293,35.1086446004709,1282.35584962783));
#275623=CARTESIAN_POINT('',(50.0313553995293,35.108644600471,1282.35584962783));
#275624=CARTESIAN_POINT('',(50.031355399529,35.1086446004712,-260.));
#275625=CARTESIAN_POINT('',(50.031355399529,35.1086446004712,-260.));
#275626=CARTESIAN_POINT('',(50.0313553995292,35.108644600471,910.));
#275627=CARTESIAN_POINT('Origin',(50.9313553995292,35.108644600471,910.));
#275628=CARTESIAN_POINT('',(50.9313553995293,34.2086446004709,1282.35584962783));
#275629=CARTESIAN_POINT('Origin',(50.9313553995293,35.1086446004709,1282.35584962783));
#275630=CARTESIAN_POINT('',(50.931355399529,34.2086446004712,-260.));
#275631=CARTESIAN_POINT('Origin',(50.931355399529,35.1086446004712,-260.));
#275632=CARTESIAN_POINT('',(50.9313553995292,34.208644600471,910.));
#275633=CARTESIAN_POINT('Origin',(53.0013553995292,34.208644600471,910.));
#275634=CARTESIAN_POINT('',(53.0013553995293,34.2086446004709,1282.35584962783));
#275635=CARTESIAN_POINT('',(53.0013553995292,34.2086446004709,1282.35584962783));
#275636=CARTESIAN_POINT('',(53.001355399529,34.208644600471,-260.));
#275637=CARTESIAN_POINT('',(53.001355399529,34.2086446004712,-260.));
#275638=CARTESIAN_POINT('',(53.0013553995292,34.208644600471,910.));
#275639=CARTESIAN_POINT('Origin',(53.0013553995292,35.198644600471,910.));
#275640=CARTESIAN_POINT('',(53.0013553995293,35.1986446004709,1282.35584962783));
#275641=CARTESIAN_POINT('',(53.0013553995293,35.198644600471,1282.35584962783));
#275642=CARTESIAN_POINT('',(53.001355399529,35.1986446004712,-260.));
#275643=CARTESIAN_POINT('',(53.001355399529,35.1986446004712,-260.));
#275644=CARTESIAN_POINT('',(53.0013553995292,35.198644600471,910.));
#275645=CARTESIAN_POINT('Origin',(53.9913553995292,35.198644600471,910.));
#275646=CARTESIAN_POINT('',(53.9913553995293,35.1986446004709,1282.35584962783));
#275647=CARTESIAN_POINT('',(53.9913553995292,35.1986446004709,1282.35584962783));
#275648=CARTESIAN_POINT('',(53.991355399529,35.198644600471,-260.));
#275649=CARTESIAN_POINT('',(53.991355399529,35.1986446004712,-260.));
#275650=CARTESIAN_POINT('',(53.9913553995292,35.198644600471,910.));
#275651=CARTESIAN_POINT('Origin',(53.9913553995292,35.198644600471,910.));
#275652=CARTESIAN_POINT('',(53.9913553995293,50.3510446004709,1282.35584962783));
#275653=CARTESIAN_POINT('',(53.9913553995293,35.198644600471,1282.35584962783));
#275654=CARTESIAN_POINT('',(53.9913553995291,50.3510446004712,-260.));
#275655=CARTESIAN_POINT('',(53.991355399529,35.1986446004712,-260.));
#275656=CARTESIAN_POINT('',(53.9913553995293,50.3510446004709,910.));
#275657=CARTESIAN_POINT('Origin',(50.3337553995292,50.3510446004709,910.));
#275658=CARTESIAN_POINT('',(50.3337553995293,54.0086446004709,1282.35584962783));
#275659=CARTESIAN_POINT('Origin',(50.3337553995293,50.3510446004709,1282.35584962783));
#275660=CARTESIAN_POINT('',(50.3337553995292,54.0086446004712,-260.));
#275661=CARTESIAN_POINT('Origin',(50.333755399529,50.3510446004712,-260.));
#275662=CARTESIAN_POINT('',(50.3337553995292,54.008644600471,910.));
#275663=CARTESIAN_POINT('Origin',(35.1813553995293,54.0086446004711,910.));
#275664=CARTESIAN_POINT('',(35.1813553995294,54.008644600471,1282.35584962783));
#275665=CARTESIAN_POINT('',(35.1813553995293,54.008644600471,1282.35584962783));
#275666=CARTESIAN_POINT('',(35.1813553995291,54.0086446004713,-260.));
#275667=CARTESIAN_POINT('',(35.1813553995291,54.0086446004713,-260.));
#275668=CARTESIAN_POINT('',(35.1813553995293,54.0086446004711,910.));
#275669=CARTESIAN_POINT('Origin',(35.1813553995293,54.0086446004711,910.));
#275670=CARTESIAN_POINT('',(35.1813553995294,53.018644600471,1282.35584962783));
#275671=CARTESIAN_POINT('',(35.1813553995294,54.0086446004711,1282.35584962783));
#275672=CARTESIAN_POINT('',(35.1813553995293,53.0186446004713,-260.));
#275673=CARTESIAN_POINT('',(35.1813553995291,54.0086446004713,-260.));
#275674=CARTESIAN_POINT('',(35.1813553995293,53.0186446004711,910.));
#275675=CARTESIAN_POINT('Origin',(35.1813553995293,53.0186446004711,910.));
#275676=CARTESIAN_POINT('',(34.1913553995294,53.018644600471,1282.35584962783));
#275677=CARTESIAN_POINT('',(35.1813553995293,53.018644600471,1282.35584962783));
#275678=CARTESIAN_POINT('',(34.1913553995291,53.0186446004713,-260.));
#275679=CARTESIAN_POINT('',(35.1813553995291,53.0186446004713,-260.));
#275680=CARTESIAN_POINT('',(34.1913553995293,53.0186446004711,910.));
#275681=CARTESIAN_POINT('Origin',(34.1913553995293,53.0186446004711,910.));
#275682=CARTESIAN_POINT('',(34.1913553995293,50.948644600471,1282.35584962783));
#275683=CARTESIAN_POINT('',(34.1913553995294,53.0186446004711,1282.35584962783));
#275684=CARTESIAN_POINT('',(34.1913553995291,50.9486446004713,-260.));
#275685=CARTESIAN_POINT('',(34.1913553995291,53.0186446004713,-260.));
#275686=CARTESIAN_POINT('',(34.1913553995293,50.9486446004711,910.));
#275687=CARTESIAN_POINT('Origin',(35.0913553995293,50.948644600471,910.));
#275688=CARTESIAN_POINT('',(35.0913553995293,50.048644600471,1282.35584962783));
#275689=CARTESIAN_POINT('Origin',(35.0913553995293,50.948644600471,1282.35584962783));
#275690=CARTESIAN_POINT('',(35.091355399529,50.0486446004713,-260.));
#275691=CARTESIAN_POINT('Origin',(35.091355399529,50.9486446004713,-260.));
#275692=CARTESIAN_POINT('',(35.0913553995293,50.0486446004711,910.));
#275693=CARTESIAN_POINT('Origin',(35.0913553995293,50.0486446004711,910.));
#275694=CARTESIAN_POINT('',(40.9413553995293,50.048644600471,1282.35584962783));
#275695=CARTESIAN_POINT('',(35.0913553995293,50.048644600471,1282.35584962783));
#275696=CARTESIAN_POINT('',(40.9413553995291,50.0486446004712,-260.));
#275697=CARTESIAN_POINT('',(35.091355399529,50.0486446004713,-260.));
#275698=CARTESIAN_POINT('',(40.9413553995293,50.048644600471,910.));
#275699=CARTESIAN_POINT('Origin',(40.9413553995293,49.148644600471,910.));
#275700=CARTESIAN_POINT('',(41.8413553995293,49.148644600471,1282.35584962783));
#275701=CARTESIAN_POINT('Origin',(40.9413553995293,49.148644600471,1282.35584962783));
#275702=CARTESIAN_POINT('',(41.841355399529,49.1486446004712,-260.));
#275703=CARTESIAN_POINT('Origin',(40.9413553995291,49.1486446004712,-260.));
#275704=CARTESIAN_POINT('',(41.8413553995293,49.148644600471,910.));
#275705=CARTESIAN_POINT('Origin',(41.8413553995293,49.148644600471,910.));
#275706=CARTESIAN_POINT('',(41.8413553995293,45.4134173219462,1282.35584962783));
#275707=CARTESIAN_POINT('',(41.8413553995293,49.148644600471,1282.35584962783));
#275708=CARTESIAN_POINT('',(41.841355399529,45.4134173219465,-260.));
#275709=CARTESIAN_POINT('',(41.841355399529,49.1486446004712,-260.));
#275710=CARTESIAN_POINT('',(41.8413553995293,45.4134173219463,910.));
#275711=CARTESIAN_POINT('Origin',(40.9413553995293,45.4134173219463,910.));
#275712=CARTESIAN_POINT('',(41.5777515025972,44.7770212188783,1282.35584962783));
#275713=CARTESIAN_POINT('Origin',(40.9413553995293,45.4134173219462,1282.35584962783));
#275714=CARTESIAN_POINT('',(41.5777515025969,44.7770212188786,-260.));
#275715=CARTESIAN_POINT('Origin',(40.941355399529,45.4134173219465,-260.));
#275716=CARTESIAN_POINT('',(41.5777515025972,44.7770212188784,910.));
#275717=CARTESIAN_POINT('Origin',(41.5777515025972,44.7770212188784,910.));
#275718=CARTESIAN_POINT('',(34.8729787811219,38.0722484974031,1282.35584962783));
#275719=CARTESIAN_POINT('',(41.5777515025972,44.7770212188783,1282.35584962783));
#275720=CARTESIAN_POINT('',(34.8729787811217,38.0722484974034,-260.));
#275721=CARTESIAN_POINT('',(41.5777515025969,44.7770212188786,-260.));
#275722=CARTESIAN_POINT('',(34.8729787811219,38.0722484974032,910.));
#275723=CARTESIAN_POINT('Origin',(34.236582678054,38.7086446004711,910.));
#275724=CARTESIAN_POINT('',(34.236582678054,37.808644600471,1282.35584962783));
#275725=CARTESIAN_POINT('Origin',(34.2365826780541,38.708644600471,1282.35584962783));
#275726=CARTESIAN_POINT('',(34.236582678054,37.8086446004713,-260.));
#275727=CARTESIAN_POINT('Origin',(34.2365826780538,38.7086446004713,-260.));
#275728=CARTESIAN_POINT('',(34.236582678054,37.8086446004711,910.));
#275729=CARTESIAN_POINT('Origin',(34.236582678054,37.8086446004711,910.));
#275730=CARTESIAN_POINT('',(34.236582678054,37.808644600471,1282.35584962783));
#275731=CARTESIAN_POINT('',(34.2365826780538,37.8086446004713,-260.));
#275732=CARTESIAN_POINT('Origin',(37.7913553995291,-28.5127888288977,910.));
#275733=CARTESIAN_POINT('',(37.7913553995291,-28.5127888288979,1282.35584962783));
#275734=CARTESIAN_POINT('',(36.9129553995291,-26.9913553995294,1282.35584962783));
#275735=CARTESIAN_POINT('',(37.791355399529,-28.5127888288978,1282.35584962783));
#275736=CARTESIAN_POINT('',(37.7913553995293,-28.5127888288977,-260.));
#275737=CARTESIAN_POINT('',(37.7913553995291,-28.5127888288977,910.));
#275738=CARTESIAN_POINT('',(36.9129553995288,-26.9913553995292,-260.));
#275739=CARTESIAN_POINT('',(37.7913553995291,-28.5127888288973,-260.));
#275740=CARTESIAN_POINT('',(36.9129553995291,-26.9913553995292,910.));
#275741=CARTESIAN_POINT('Origin',(37.7913553995291,-25.4699219701607,910.));
#275742=CARTESIAN_POINT('',(37.7913553995291,-25.4699219701609,1282.35584962783));
#275743=CARTESIAN_POINT('',(37.7913553995292,-25.4699219701608,1282.35584962783));
#275744=CARTESIAN_POINT('',(37.7913553995291,-25.4699219701607,-260.));
#275745=CARTESIAN_POINT('',(37.7913553995291,-25.4699219701603,-260.));
#275746=CARTESIAN_POINT('',(37.7913553995291,-25.4699219701607,910.));
#275747=CARTESIAN_POINT('Origin',(37.7913553995291,-19.7461281210045,910.));
#275748=CARTESIAN_POINT('',(37.7913553995291,-19.7461281210046,1282.35584962783));
#275749=CARTESIAN_POINT('',(37.7913553995291,-19.7461281210045,1282.35584962783));
#275750=CARTESIAN_POINT('',(37.7913553995291,-19.7461281210041,-260.));
#275751=CARTESIAN_POINT('',(37.7913553995291,-19.7461281210041,-260.));
#275752=CARTESIAN_POINT('',(37.7913553995291,-19.7461281210045,910.));
#275753=CARTESIAN_POINT('Origin',(38.6913553995291,-19.7461281210045,910.));
#275754=CARTESIAN_POINT('',(38.0549592964612,-19.1097320179367,1282.35584962783));
#275755=CARTESIAN_POINT('Origin',(38.6913553995291,-19.7461281210046,1282.35584962783));
#275756=CARTESIAN_POINT('',(38.0549592964612,-19.1097320179362,-260.));
#275757=CARTESIAN_POINT('Origin',(38.6913553995291,-19.7461281210041,-260.));
#275758=CARTESIAN_POINT('',(38.0549592964612,-19.1097320179366,910.));
#275759=CARTESIAN_POINT('Origin',(44.7597320179365,-12.4049592964613,910.));
#275760=CARTESIAN_POINT('',(44.7597320179365,-12.4049592964615,1282.35584962783));
#275761=CARTESIAN_POINT('',(44.7597320179365,-12.4049592964614,1282.35584962783));
#275762=CARTESIAN_POINT('',(44.7597320179365,-12.4049592964609,-260.));
#275763=CARTESIAN_POINT('',(44.7597320179365,-12.4049592964609,-260.));
#275764=CARTESIAN_POINT('',(44.7597320179365,-12.4049592964613,910.));
#275765=CARTESIAN_POINT('Origin',(45.3961281210043,-13.0413553995292,910.));
#275766=CARTESIAN_POINT('',(45.3961281210043,-12.1413553995294,1282.35584962783));
#275767=CARTESIAN_POINT('Origin',(45.3961281210043,-13.0413553995294,1282.35584962783));
#275768=CARTESIAN_POINT('',(45.3961281210043,-12.1413553995288,-260.));
#275769=CARTESIAN_POINT('Origin',(45.3961281210043,-13.0413553995288,-260.));
#275770=CARTESIAN_POINT('',(45.3961281210043,-12.1413553995292,910.));
#275771=CARTESIAN_POINT('Origin',(49.1313553995291,-12.1413553995292,910.));
#275772=CARTESIAN_POINT('',(49.1313553995291,-12.1413553995294,1282.35584962783));
#275773=CARTESIAN_POINT('',(49.1313553995291,-12.1413553995294,1282.35584962783));
#275774=CARTESIAN_POINT('',(49.1313553995291,-12.1413553995288,-260.));
#275775=CARTESIAN_POINT('',(49.1313553995291,-12.1413553995288,-260.));
#275776=CARTESIAN_POINT('',(49.1313553995291,-12.1413553995292,910.));
#275777=CARTESIAN_POINT('Origin',(49.1313553995291,-13.0413553995292,910.));
#275778=CARTESIAN_POINT('',(50.0313553995291,-13.0413553995294,1282.35584962783));
#275779=CARTESIAN_POINT('Origin',(49.1313553995291,-13.0413553995294,1282.35584962783));
#275780=CARTESIAN_POINT('',(50.0313553995291,-13.0413553995288,-260.));
#275781=CARTESIAN_POINT('Origin',(49.1313553995291,-13.0413553995288,-260.));
#275782=CARTESIAN_POINT('',(50.0313553995291,-13.0413553995292,910.));
#275783=CARTESIAN_POINT('Origin',(50.0313553995291,-18.8913553995292,910.));
#275784=CARTESIAN_POINT('',(50.0313553995291,-18.8913553995294,1282.35584962783));
#275785=CARTESIAN_POINT('',(50.0313553995291,-18.8913553995292,1282.35584962783));
#275786=CARTESIAN_POINT('',(50.0313553995291,-18.8913553995288,-260.));
#275787=CARTESIAN_POINT('',(50.0313553995291,-18.8913553995288,-260.));
#275788=CARTESIAN_POINT('',(50.0313553995291,-18.8913553995292,910.));
#275789=CARTESIAN_POINT('Origin',(50.9313553995291,-18.8913553995292,910.));
#275790=CARTESIAN_POINT('',(50.9313553995291,-19.7913553995294,1282.35584962783));
#275791=CARTESIAN_POINT('Origin',(50.9313553995291,-18.8913553995294,1282.35584962783));
#275792=CARTESIAN_POINT('',(50.9313553995291,-19.7913553995288,-260.));
#275793=CARTESIAN_POINT('Origin',(50.9313553995291,-18.8913553995288,-260.));
#275794=CARTESIAN_POINT('',(50.9313553995291,-19.7913553995292,910.));
#275795=CARTESIAN_POINT('Origin',(53.0013553995291,-19.7913553995292,910.));
#275796=CARTESIAN_POINT('',(53.0013553995291,-19.7913553995294,1282.35584962783));
#275797=CARTESIAN_POINT('',(53.0013553995291,-19.7913553995294,1282.35584962783));
#275798=CARTESIAN_POINT('',(53.0013553995291,-19.7913553995292,-260.));
#275799=CARTESIAN_POINT('',(53.0013553995291,-19.7913553995288,-260.));
#275800=CARTESIAN_POINT('',(53.0013553995291,-19.7913553995292,910.));
#275801=CARTESIAN_POINT('Origin',(53.0013553995291,-18.8013553995292,910.));
#275802=CARTESIAN_POINT('',(53.0013553995291,-18.8013553995294,1282.35584962783));
#275803=CARTESIAN_POINT('',(53.0013553995291,-18.8013553995292,1282.35584962783));
#275804=CARTESIAN_POINT('',(53.0013553995291,-18.8013553995288,-260.));
#275805=CARTESIAN_POINT('',(53.0013553995291,-18.8013553995288,-260.));
#275806=CARTESIAN_POINT('',(53.0013553995291,-18.8013553995292,910.));
#275807=CARTESIAN_POINT('Origin',(53.9913553995291,-18.8013553995292,910.));
#275808=CARTESIAN_POINT('',(53.9913553995291,-18.8013553995294,1282.35584962783));
#275809=CARTESIAN_POINT('',(53.9913553995291,-18.8013553995288,-260.));
#275810=CARTESIAN_POINT('Origin',(18.8013553995289,-53.9913553995292,910.));
#275811=CARTESIAN_POINT('',(-18.818644600472,-53.9913553995291,1282.35584962783));
#275812=CARTESIAN_POINT('',(18.8013553995289,-53.9913553995293,1282.35584962783));
#275813=CARTESIAN_POINT('',(18.8013553995289,-53.9913553995293,1282.35584962783));
#275814=CARTESIAN_POINT('',(-18.8186446004719,-53.9913553995285,-260.));
#275815=CARTESIAN_POINT('',(-18.8186446004719,-53.991355399529,910.));
#275816=CARTESIAN_POINT('',(18.8013553995289,-53.9913553995292,-260.));
#275817=CARTESIAN_POINT('',(18.8013553995289,-53.9913553995287,-260.));
#275818=CARTESIAN_POINT('',(18.8013553995289,-53.9913553995292,910.));
#275819=CARTESIAN_POINT('Origin',(18.8013553995289,-53.9913553995292,910.));
#275820=CARTESIAN_POINT('',(18.8013553995289,-53.0013553995293,1282.35584962783));
#275821=CARTESIAN_POINT('',(18.8013553995289,-53.9913553995292,1282.35584962783));
#275822=CARTESIAN_POINT('',(18.8013553995289,-53.0013553995287,-260.));
#275823=CARTESIAN_POINT('',(18.8013553995289,-53.9913553995287,-260.));
#275824=CARTESIAN_POINT('',(18.8013553995289,-53.0013553995292,910.));
#275825=CARTESIAN_POINT('Origin',(18.8013553995289,-53.0013553995292,910.));
#275826=CARTESIAN_POINT('',(19.7913553995289,-53.0013553995293,1282.35584962783));
#275827=CARTESIAN_POINT('',(18.8013553995289,-53.0013553995293,1282.35584962783));
#275828=CARTESIAN_POINT('',(19.7913553995289,-53.0013553995292,-260.));
#275829=CARTESIAN_POINT('',(18.8013553995289,-53.0013553995287,-260.));
#275830=CARTESIAN_POINT('',(19.7913553995289,-53.0013553995292,910.));
#275831=CARTESIAN_POINT('Origin',(19.7913553995289,-53.0013553995292,910.));
#275832=CARTESIAN_POINT('',(19.7913553995289,-50.9313553995293,1282.35584962783));
#275833=CARTESIAN_POINT('',(19.7913553995289,-53.0013553995292,1282.35584962783));
#275834=CARTESIAN_POINT('',(19.7913553995289,-50.9313553995287,-260.));
#275835=CARTESIAN_POINT('',(19.7913553995289,-53.0013553995287,-260.));
#275836=CARTESIAN_POINT('',(19.7913553995289,-50.9313553995292,910.));
#275837=CARTESIAN_POINT('Origin',(18.8913553995289,-50.9313553995292,910.));
#275838=CARTESIAN_POINT('',(18.8913553995289,-50.0313553995293,1282.35584962783));
#275839=CARTESIAN_POINT('Origin',(18.8913553995289,-50.9313553995293,1282.35584962783));
#275840=CARTESIAN_POINT('',(18.8913553995289,-50.0313553995287,-260.));
#275841=CARTESIAN_POINT('Origin',(18.8913553995289,-50.9313553995287,-260.));
#275842=CARTESIAN_POINT('',(18.8913553995289,-50.0313553995292,910.));
#275843=CARTESIAN_POINT('Origin',(18.8913553995289,-50.0313553995292,910.));
#275844=CARTESIAN_POINT('',(13.0413553995289,-50.0313553995292,1282.35584962783));
#275845=CARTESIAN_POINT('',(18.8913553995289,-50.0313553995293,1282.35584962783));
#275846=CARTESIAN_POINT('',(13.0413553995289,-50.0313553995287,-260.));
#275847=CARTESIAN_POINT('',(18.8913553995289,-50.0313553995287,-260.));
#275848=CARTESIAN_POINT('',(13.0413553995289,-50.0313553995291,910.));
#275849=CARTESIAN_POINT('Origin',(13.0413553995289,-49.1313553995291,910.));
#275850=CARTESIAN_POINT('',(12.1413553995289,-49.1313553995292,1282.35584962783));
#275851=CARTESIAN_POINT('Origin',(13.0413553995289,-49.1313553995292,1282.35584962783));
#275852=CARTESIAN_POINT('',(12.1413553995289,-49.1313553995291,-260.));
#275853=CARTESIAN_POINT('Origin',(13.0413553995289,-49.1313553995287,-260.));
#275854=CARTESIAN_POINT('',(12.1413553995289,-49.1313553995291,910.));
#275855=CARTESIAN_POINT('Origin',(12.1413553995289,-49.1313553995291,910.));
#275856=CARTESIAN_POINT('',(12.141355399529,-45.3961281210045,1282.35584962783));
#275857=CARTESIAN_POINT('',(12.1413553995289,-49.1313553995291,1282.35584962783));
#275858=CARTESIAN_POINT('',(12.141355399529,-45.3961281210039,-260.));
#275859=CARTESIAN_POINT('',(12.1413553995289,-49.1313553995287,-260.));
#275860=CARTESIAN_POINT('',(12.141355399529,-45.3961281210044,910.));
#275861=CARTESIAN_POINT('Origin',(13.041355399529,-45.3961281210044,910.));
#275862=CARTESIAN_POINT('',(12.4049592964611,-44.7597320179366,1282.35584962783));
#275863=CARTESIAN_POINT('Origin',(13.041355399529,-45.3961281210045,1282.35584962783));
#275864=CARTESIAN_POINT('',(12.4049592964611,-44.759732017936,-260.));
#275865=CARTESIAN_POINT('Origin',(13.041355399529,-45.3961281210039,-260.));
#275866=CARTESIAN_POINT('',(12.4049592964611,-44.7597320179365,910.));
#275867=CARTESIAN_POINT('Origin',(12.4049592964611,-44.7597320179365,910.));
#275868=CARTESIAN_POINT('',(19.1097320179364,-38.0549592964614,1282.35584962783));
#275869=CARTESIAN_POINT('',(12.4049592964611,-44.7597320179365,1282.35584962783));
#275870=CARTESIAN_POINT('',(19.1097320179364,-38.0549592964608,-260.));
#275871=CARTESIAN_POINT('',(12.4049592964611,-44.759732017936,-260.));
#275872=CARTESIAN_POINT('',(19.1097320179364,-38.0549592964613,910.));
#275873=CARTESIAN_POINT('Origin',(19.7461281210043,-38.6913553995292,910.));
#275874=CARTESIAN_POINT('',(19.7461281210043,-37.7913553995293,1282.35584962783));
#275875=CARTESIAN_POINT('Origin',(19.7461281210043,-38.6913553995293,1282.35584962783));
#275876=CARTESIAN_POINT('',(19.7461281210043,-37.7913553995287,-260.));
#275877=CARTESIAN_POINT('Origin',(19.7461281210043,-38.6913553995287,-260.));
#275878=CARTESIAN_POINT('',(19.7461281210043,-37.7913553995292,910.));
#275879=CARTESIAN_POINT('Origin',(19.7461281210043,-37.7913553995292,910.));
#275880=CARTESIAN_POINT('',(25.4699219701605,-37.7913553995294,1282.35584962783));
#275881=CARTESIAN_POINT('',(19.7461281210043,-37.7913553995293,1282.35584962783));
#275882=CARTESIAN_POINT('',(25.4699219701605,-37.7913553995288,-260.));
#275883=CARTESIAN_POINT('',(19.7461281210043,-37.7913553995287,-260.));
#275884=CARTESIAN_POINT('',(25.4699219701605,-37.7913553995292,910.));
#275885=CARTESIAN_POINT('Origin',(25.4699219701605,-37.7913553995292,910.));
#275886=CARTESIAN_POINT('',(26.9913553995291,-36.9129553995294,1282.35584962783));
#275887=CARTESIAN_POINT('',(25.4699219701606,-37.7913553995293,1282.35584962783));
#275888=CARTESIAN_POINT('',(26.9913553995291,-36.9129553995288,-260.));
#275889=CARTESIAN_POINT('',(25.4699219701605,-37.7913553995288,-260.));
#275890=CARTESIAN_POINT('',(26.9913553995291,-36.9129553995292,910.));
#275891=CARTESIAN_POINT('Origin',(28.5127888288976,-37.7913553995292,910.));
#275892=CARTESIAN_POINT('',(28.5127888288976,-37.7913553995294,1282.35584962783));
#275893=CARTESIAN_POINT('',(28.5127888288975,-37.7913553995293,1282.35584962783));
#275894=CARTESIAN_POINT('',(28.5127888288976,-37.7913553995288,-260.));
#275895=CARTESIAN_POINT('',(28.5127888288976,-37.7913553995288,-260.));
#275896=CARTESIAN_POINT('',(28.5127888288976,-37.7913553995292,910.));
#275897=CARTESIAN_POINT('Origin',(34.2365826780538,-37.7913553995292,910.));
#275898=CARTESIAN_POINT('',(34.2365826780538,-37.7913553995294,1282.35584962783));
#275899=CARTESIAN_POINT('',(34.2365826780538,-37.7913553995294,1282.35584962783));
#275900=CARTESIAN_POINT('',(34.2365826780538,-37.7913553995288,-260.));
#275901=CARTESIAN_POINT('',(34.2365826780538,-37.7913553995288,-260.));
#275902=CARTESIAN_POINT('',(34.2365826780538,-37.7913553995292,910.));
#275903=CARTESIAN_POINT('Origin',(34.2365826780538,-38.6913553995292,910.));
#275904=CARTESIAN_POINT('',(34.8729787811217,-38.0549592964615,1282.35584962783));
#275905=CARTESIAN_POINT('Origin',(34.2365826780538,-38.6913553995294,1282.35584962783));
#275906=CARTESIAN_POINT('',(34.8729787811217,-38.0549592964609,-260.));
#275907=CARTESIAN_POINT('Origin',(34.2365826780538,-38.6913553995288,-260.));
#275908=CARTESIAN_POINT('',(34.8729787811217,-38.0549592964613,910.));
#275909=CARTESIAN_POINT('Origin',(41.577751502597,-44.7597320179366,910.));
#275910=CARTESIAN_POINT('',(41.577751502597,-44.7597320179367,1282.35584962783));
#275911=CARTESIAN_POINT('',(41.5777515025969,-44.7597320179367,1282.35584962783));
#275912=CARTESIAN_POINT('',(41.577751502597,-44.7597320179362,-260.));
#275913=CARTESIAN_POINT('',(41.577751502597,-44.7597320179362,-260.));
#275914=CARTESIAN_POINT('',(41.577751502597,-44.7597320179366,910.));
#275915=CARTESIAN_POINT('Origin',(40.9413553995291,-45.3961281210045,910.));
#275916=CARTESIAN_POINT('',(41.8413553995291,-45.3961281210046,1282.35584962783));
#275917=CARTESIAN_POINT('Origin',(40.9413553995291,-45.3961281210046,1282.35584962783));
#275918=CARTESIAN_POINT('',(41.8413553995291,-45.396128121004,-260.));
#275919=CARTESIAN_POINT('Origin',(40.9413553995291,-45.396128121004,-260.));
#275920=CARTESIAN_POINT('',(41.8413553995291,-45.3961281210045,910.));
#275921=CARTESIAN_POINT('Origin',(41.8413553995291,-49.1313553995292,910.));
#275922=CARTESIAN_POINT('',(41.8413553995291,-49.1313553995293,1282.35584962783));
#275923=CARTESIAN_POINT('',(41.8413553995291,-49.1313553995292,1282.35584962783));
#275924=CARTESIAN_POINT('',(41.8413553995291,-49.1313553995288,-260.));
#275925=CARTESIAN_POINT('',(41.8413553995291,-49.1313553995288,-260.));
#275926=CARTESIAN_POINT('',(41.8413553995291,-49.1313553995292,910.));
#275927=CARTESIAN_POINT('Origin',(40.9413553995291,-49.1313553995292,910.));
#275928=CARTESIAN_POINT('',(40.9413553995291,-50.0313553995293,1282.35584962783));
#275929=CARTESIAN_POINT('Origin',(40.9413553995291,-49.1313553995294,1282.35584962783));
#275930=CARTESIAN_POINT('',(40.9413553995291,-50.0313553995288,-260.));
#275931=CARTESIAN_POINT('Origin',(40.9413553995291,-49.1313553995288,-260.));
#275932=CARTESIAN_POINT('',(40.9413553995291,-50.0313553995292,910.));
#275933=CARTESIAN_POINT('Origin',(35.0913553995291,-50.0313553995292,910.));
#275934=CARTESIAN_POINT('',(35.0913553995291,-50.0313553995294,1282.35584962783));
#275935=CARTESIAN_POINT('',(35.0913553995291,-50.0313553995294,1282.35584962783));
#275936=CARTESIAN_POINT('',(35.0913553995291,-50.0313553995288,-260.));
#275937=CARTESIAN_POINT('',(35.0913553995291,-50.0313553995288,-260.));
#275938=CARTESIAN_POINT('',(35.0913553995291,-50.0313553995292,910.));
#275939=CARTESIAN_POINT('Origin',(35.0913553995291,-50.9313553995292,910.));
#275940=CARTESIAN_POINT('',(34.1913553995291,-50.9313553995294,1282.35584962783));
#275941=CARTESIAN_POINT('Origin',(35.0913553995291,-50.9313553995294,1282.35584962783));
#275942=CARTESIAN_POINT('',(34.1913553995291,-50.9313553995288,-260.));
#275943=CARTESIAN_POINT('Origin',(35.0913553995291,-50.9313553995288,-260.));
#275944=CARTESIAN_POINT('',(34.1913553995291,-50.9313553995292,910.));
#275945=CARTESIAN_POINT('Origin',(34.1913553995291,-53.0013553995292,910.));
#275946=CARTESIAN_POINT('',(34.1913553995291,-53.0013553995294,1282.35584962783));
#275947=CARTESIAN_POINT('',(34.1913553995291,-53.0013553995292,1282.35584962783));
#275948=CARTESIAN_POINT('',(34.1913553995291,-53.0013553995288,-260.));
#275949=CARTESIAN_POINT('',(34.1913553995291,-53.0013553995288,-260.));
#275950=CARTESIAN_POINT('',(34.1913553995291,-53.0013553995292,910.));
#275951=CARTESIAN_POINT('Origin',(35.1813553995291,-53.0013553995292,910.));
#275952=CARTESIAN_POINT('',(35.1813553995291,-53.0013553995294,1282.35584962783));
#275953=CARTESIAN_POINT('',(35.1813553995291,-53.0013553995294,1282.35584962783));
#275954=CARTESIAN_POINT('',(35.1813553995291,-53.0013553995288,-260.));
#275955=CARTESIAN_POINT('',(35.1813553995291,-53.0013553995288,-260.));
#275956=CARTESIAN_POINT('',(35.1813553995291,-53.0013553995292,910.));
#275957=CARTESIAN_POINT('Origin',(35.1813553995291,-53.9913553995292,910.));
#275958=CARTESIAN_POINT('',(35.1813553995291,-53.9913553995294,1282.35584962783));
#275959=CARTESIAN_POINT('',(35.1813553995291,-53.9913553995292,1282.35584962783));
#275960=CARTESIAN_POINT('',(35.1813553995291,-53.9913553995288,-260.));
#275961=CARTESIAN_POINT('',(35.1813553995291,-53.9913553995288,-260.));
#275962=CARTESIAN_POINT('',(35.1813553995291,-53.9913553995292,910.));
#275963=CARTESIAN_POINT('Origin',(35.1813553995291,-53.9913553995292,910.));
#275964=CARTESIAN_POINT('',(50.333755399529,-53.9913553995294,1282.35584962783));
#275965=CARTESIAN_POINT('',(35.1813553995291,-53.9913553995294,1282.35584962783));
#275966=CARTESIAN_POINT('',(50.333755399529,-53.9913553995288,-260.));
#275967=CARTESIAN_POINT('',(35.1813553995291,-53.9913553995288,-260.));
#275968=CARTESIAN_POINT('',(50.333755399529,-53.9913553995292,910.));
#275969=CARTESIAN_POINT('Origin',(50.333755399529,-50.3337553995292,910.));
#275970=CARTESIAN_POINT('',(53.9913553995291,-50.3337553995293,1282.35584962783));
#275971=CARTESIAN_POINT('Origin',(50.333755399529,-50.3337553995293,1282.35584962783));
#275972=CARTESIAN_POINT('',(53.9913553995291,-50.3337553995292,-260.));
#275973=CARTESIAN_POINT('Origin',(50.333755399529,-50.3337553995287,-260.));
#275974=CARTESIAN_POINT('',(53.9913553995291,-50.3337553995292,910.));
#275975=CARTESIAN_POINT('Origin',(53.9913553995291,-35.1813553995292,910.));
#275976=CARTESIAN_POINT('',(53.9913553995291,-35.1813553995294,1282.35584962783));
#275977=CARTESIAN_POINT('',(53.9913553995291,-35.1813553995292,1282.35584962783));
#275978=CARTESIAN_POINT('',(53.9913553995291,-35.1813553995288,-260.));
#275979=CARTESIAN_POINT('',(53.9913553995291,-35.1813553995288,-260.));
#275980=CARTESIAN_POINT('',(53.9913553995291,-35.1813553995292,910.));
#275981=CARTESIAN_POINT('Origin',(53.9913553995291,-35.1813553995292,910.));
#275982=CARTESIAN_POINT('',(53.0013553995291,-35.1813553995294,1282.35584962783));
#275983=CARTESIAN_POINT('',(53.9913553995291,-35.1813553995294,1282.35584962783));
#275984=CARTESIAN_POINT('',(53.0013553995291,-35.1813553995292,-260.));
#275985=CARTESIAN_POINT('',(53.9913553995291,-35.1813553995288,-260.));
#275986=CARTESIAN_POINT('',(53.0013553995291,-35.1813553995292,910.));
#275987=CARTESIAN_POINT('Origin',(53.0013553995291,-35.1813553995292,910.));
#275988=CARTESIAN_POINT('',(53.0013553995291,-34.1913553995294,1282.35584962783));
#275989=CARTESIAN_POINT('',(53.0013553995291,-35.1813553995292,1282.35584962783));
#275990=CARTESIAN_POINT('',(53.0013553995291,-34.1913553995288,-260.));
#275991=CARTESIAN_POINT('',(53.0013553995291,-35.1813553995288,-260.));
#275992=CARTESIAN_POINT('',(53.0013553995291,-34.1913553995292,910.));
#275993=CARTESIAN_POINT('Origin',(53.0013553995291,-34.1913553995292,910.));
#275994=CARTESIAN_POINT('',(50.9313553995291,-34.1913553995294,1282.35584962783));
#275995=CARTESIAN_POINT('',(53.0013553995291,-34.1913553995294,1282.35584962783));
#275996=CARTESIAN_POINT('',(50.9313553995291,-34.1913553995288,-260.));
#275997=CARTESIAN_POINT('',(53.0013553995291,-34.1913553995288,-260.));
#275998=CARTESIAN_POINT('',(50.9313553995291,-34.1913553995292,910.));
#275999=CARTESIAN_POINT('Origin',(50.9313553995291,-35.0913553995292,910.));
#276000=CARTESIAN_POINT('',(50.0313553995291,-35.0913553995294,1282.35584962783));
#276001=CARTESIAN_POINT('Origin',(50.9313553995291,-35.0913553995294,1282.35584962783));
#276002=CARTESIAN_POINT('',(50.0313553995291,-35.0913553995288,-260.));
#276003=CARTESIAN_POINT('Origin',(50.9313553995291,-35.0913553995288,-260.));
#276004=CARTESIAN_POINT('',(50.0313553995291,-35.0913553995292,910.));
#276005=CARTESIAN_POINT('Origin',(50.0313553995291,-35.0913553995292,910.));
#276006=CARTESIAN_POINT('',(50.0313553995291,-40.9413553995294,1282.35584962783));
#276007=CARTESIAN_POINT('',(50.0313553995291,-35.0913553995292,1282.35584962783));
#276008=CARTESIAN_POINT('',(50.0313553995291,-40.9413553995288,-260.));
#276009=CARTESIAN_POINT('',(50.0313553995291,-35.0913553995288,-260.));
#276010=CARTESIAN_POINT('',(50.0313553995291,-40.9413553995292,910.));
#276011=CARTESIAN_POINT('Origin',(49.1313553995291,-40.9413553995292,910.));
#276012=CARTESIAN_POINT('',(49.1313553995291,-41.8413553995294,1282.35584962783));
#276013=CARTESIAN_POINT('Origin',(49.1313553995291,-40.9413553995294,1282.35584962783));
#276014=CARTESIAN_POINT('',(49.1313553995291,-41.8413553995288,-260.));
#276015=CARTESIAN_POINT('Origin',(49.1313553995291,-40.9413553995288,-260.));
#276016=CARTESIAN_POINT('',(49.1313553995291,-41.8413553995292,910.));
#276017=CARTESIAN_POINT('Origin',(49.1313553995291,-41.8413553995292,910.));
#276018=CARTESIAN_POINT('',(45.3961281210043,-41.8413553995294,1282.35584962783));
#276019=CARTESIAN_POINT('',(49.1313553995291,-41.8413553995294,1282.35584962783));
#276020=CARTESIAN_POINT('',(45.3961281210043,-41.8413553995288,-260.));
#276021=CARTESIAN_POINT('',(49.1313553995291,-41.8413553995288,-260.));
#276022=CARTESIAN_POINT('',(45.3961281210043,-41.8413553995292,910.));
#276023=CARTESIAN_POINT('Origin',(45.3961281210043,-40.9413553995292,910.));
#276024=CARTESIAN_POINT('',(44.7597320179365,-41.5777515025973,1282.35584962783));
#276025=CARTESIAN_POINT('Origin',(45.3961281210043,-40.9413553995294,1282.35584962783));
#276026=CARTESIAN_POINT('',(44.7597320179365,-41.5777515025967,-260.));
#276027=CARTESIAN_POINT('Origin',(45.3961281210043,-40.9413553995288,-260.));
#276028=CARTESIAN_POINT('',(44.7597320179365,-41.5777515025971,910.));
#276029=CARTESIAN_POINT('Origin',(44.7597320179365,-41.5777515025971,910.));
#276030=CARTESIAN_POINT('',(38.0549592964612,-34.872978781122,1282.35584962783));
#276031=CARTESIAN_POINT('',(44.7597320179364,-41.5777515025972,1282.35584962783));
#276032=CARTESIAN_POINT('',(38.0549592964612,-34.8729787811214,-260.));
#276033=CARTESIAN_POINT('',(44.7597320179365,-41.5777515025967,-260.));
#276034=CARTESIAN_POINT('',(38.0549592964612,-34.8729787811219,910.));
#276035=CARTESIAN_POINT('Origin',(38.6913553995291,-34.236582678054,910.));
#276036=CARTESIAN_POINT('',(37.7913553995291,-34.2365826780541,1282.35584962783));
#276037=CARTESIAN_POINT('Origin',(38.6913553995291,-34.2365826780541,1282.35584962783));
#276038=CARTESIAN_POINT('',(37.7913553995291,-34.236582678054,-260.));
#276039=CARTESIAN_POINT('Origin',(38.6913553995291,-34.2365826780536,-260.));
#276040=CARTESIAN_POINT('',(37.7913553995291,-34.236582678054,910.));
#276041=CARTESIAN_POINT('Origin',(37.7913553995291,-34.236582678054,910.));
#276042=CARTESIAN_POINT('',(37.7913553995291,-34.236582678054,1282.35584962783));
#276043=CARTESIAN_POINT('',(37.7913553995291,-34.2365826780536,-260.));
#276044=CARTESIAN_POINT('Origin',(-28.5300780298402,-37.7913553995289,910.));
#276045=CARTESIAN_POINT('',(-28.5300780298403,-37.791355399529,1282.35584962783));
#276046=CARTESIAN_POINT('',(-27.0086446004718,-36.912955399529,1282.35584962783));
#276047=CARTESIAN_POINT('',(-28.5300780298402,-37.7913553995289,1282.35584962783));
#276048=CARTESIAN_POINT('',(-28.5300780298402,-37.7913553995288,-260.));
#276049=CARTESIAN_POINT('',(-28.5300780298402,-37.7913553995289,910.));
#276050=CARTESIAN_POINT('',(-27.0086446004717,-36.9129553995286,-260.));
#276051=CARTESIAN_POINT('',(-28.53007802984,-37.7913553995287,-260.));
#276052=CARTESIAN_POINT('',(-27.0086446004717,-36.9129553995289,910.));
#276053=CARTESIAN_POINT('Origin',(-25.4872111711032,-37.791355399529,910.));
#276054=CARTESIAN_POINT('',(-25.4872111711033,-37.791355399529,1282.35584962783));
#276055=CARTESIAN_POINT('',(-25.4872111711033,-37.791355399529,1282.35584962783));
#276056=CARTESIAN_POINT('',(-25.4872111711032,-37.7913553995287,-260.));
#276057=CARTESIAN_POINT('',(-25.487211171103,-37.7913553995287,-260.));
#276058=CARTESIAN_POINT('',(-25.4872111711032,-37.791355399529,910.));
#276059=CARTESIAN_POINT('Origin',(-19.763417321947,-37.791355399529,910.));
#276060=CARTESIAN_POINT('',(-19.763417321947,-37.7913553995291,1282.35584962783));
#276061=CARTESIAN_POINT('',(-19.763417321947,-37.7913553995291,1282.35584962783));
#276062=CARTESIAN_POINT('',(-19.7634173219468,-37.7913553995288,-260.));
#276063=CARTESIAN_POINT('',(-19.7634173219468,-37.7913553995288,-260.));
#276064=CARTESIAN_POINT('',(-19.763417321947,-37.791355399529,910.));
#276065=CARTESIAN_POINT('Origin',(-19.763417321947,-38.691355399529,910.));
#276066=CARTESIAN_POINT('',(-19.1270212188791,-38.0549592964612,1282.35584962783));
#276067=CARTESIAN_POINT('Origin',(-19.763417321947,-38.6913553995291,1282.35584962783));
#276068=CARTESIAN_POINT('',(-19.1270212188789,-38.0549592964609,-260.));
#276069=CARTESIAN_POINT('Origin',(-19.7634173219468,-38.6913553995288,-260.));
#276070=CARTESIAN_POINT('',(-19.1270212188791,-38.0549592964611,910.));
#276071=CARTESIAN_POINT('Origin',(-12.4222484974039,-44.7597320179364,910.));
#276072=CARTESIAN_POINT('',(-12.422248497404,-44.7597320179365,1282.35584962783));
#276073=CARTESIAN_POINT('',(-12.422248497404,-44.7597320179365,1282.35584962783));
#276074=CARTESIAN_POINT('',(-12.4222484974037,-44.7597320179362,-260.));
#276075=CARTESIAN_POINT('',(-12.4222484974037,-44.7597320179362,-260.));
#276076=CARTESIAN_POINT('',(-12.4222484974039,-44.7597320179364,910.));
#276077=CARTESIAN_POINT('Origin',(-13.0586446004718,-45.3961281210043,910.));
#276078=CARTESIAN_POINT('',(-12.1586446004719,-45.3961281210044,1282.35584962783));
#276079=CARTESIAN_POINT('Origin',(-13.0586446004719,-45.3961281210044,1282.35584962783));
#276080=CARTESIAN_POINT('',(-12.1586446004716,-45.3961281210041,-260.));
#276081=CARTESIAN_POINT('Origin',(-13.0586446004716,-45.3961281210041,-260.));
#276082=CARTESIAN_POINT('',(-12.1586446004718,-45.3961281210043,910.));
#276083=CARTESIAN_POINT('Origin',(-12.1586446004718,-49.1313553995291,910.));
#276084=CARTESIAN_POINT('',(-12.1586446004719,-49.1313553995291,1282.35584962783));
#276085=CARTESIAN_POINT('',(-12.1586446004719,-49.1313553995291,1282.35584962783));
#276086=CARTESIAN_POINT('',(-12.1586446004716,-49.1313553995289,-260.));
#276087=CARTESIAN_POINT('',(-12.1586446004716,-49.1313553995289,-260.));
#276088=CARTESIAN_POINT('',(-12.1586446004718,-49.1313553995291,910.));
#276089=CARTESIAN_POINT('Origin',(-13.0586446004718,-49.1313553995291,910.));
#276090=CARTESIAN_POINT('',(-13.0586446004719,-50.0313553995291,1282.35584962783));
#276091=CARTESIAN_POINT('Origin',(-13.0586446004719,-49.1313553995291,1282.35584962783));
#276092=CARTESIAN_POINT('',(-13.0586446004716,-50.0313553995288,-260.));
#276093=CARTESIAN_POINT('Origin',(-13.0586446004716,-49.1313553995288,-260.));
#276094=CARTESIAN_POINT('',(-13.0586446004718,-50.0313553995291,910.));
#276095=CARTESIAN_POINT('Origin',(-18.9086446004719,-50.031355399529,910.));
#276096=CARTESIAN_POINT('',(-18.9086446004719,-50.0313553995291,1282.35584962783));
#276097=CARTESIAN_POINT('',(-18.9086446004719,-50.0313553995291,1282.35584962783));
#276098=CARTESIAN_POINT('',(-18.9086446004716,-50.0313553995288,-260.));
#276099=CARTESIAN_POINT('',(-18.9086446004716,-50.0313553995288,-260.));
#276100=CARTESIAN_POINT('',(-18.9086446004719,-50.031355399529,910.));
#276101=CARTESIAN_POINT('Origin',(-18.9086446004719,-50.931355399529,910.));
#276102=CARTESIAN_POINT('',(-19.8086446004719,-50.9313553995291,1282.35584962783));
#276103=CARTESIAN_POINT('Origin',(-18.9086446004719,-50.9313553995291,1282.35584962783));
#276104=CARTESIAN_POINT('',(-19.8086446004716,-50.9313553995288,-260.));
#276105=CARTESIAN_POINT('Origin',(-18.9086446004716,-50.9313553995288,-260.));
#276106=CARTESIAN_POINT('',(-19.8086446004719,-50.931355399529,910.));
#276107=CARTESIAN_POINT('Origin',(-19.8086446004719,-53.001355399529,910.));
#276108=CARTESIAN_POINT('',(-19.8086446004719,-53.0013553995291,1282.35584962783));
#276109=CARTESIAN_POINT('',(-19.8086446004719,-53.001355399529,1282.35584962783));
#276110=CARTESIAN_POINT('',(-19.8086446004719,-53.0013553995288,-260.));
#276111=CARTESIAN_POINT('',(-19.8086446004717,-53.0013553995288,-260.));
#276112=CARTESIAN_POINT('',(-19.8086446004719,-53.001355399529,910.));
#276113=CARTESIAN_POINT('Origin',(-18.8186446004719,-53.001355399529,910.));
#276114=CARTESIAN_POINT('',(-18.8186446004719,-53.0013553995291,1282.35584962783));
#276115=CARTESIAN_POINT('',(-18.8186446004719,-53.0013553995291,1282.35584962783));
#276116=CARTESIAN_POINT('',(-18.8186446004717,-53.0013553995288,-260.));
#276117=CARTESIAN_POINT('',(-18.8186446004717,-53.0013553995288,-260.));
#276118=CARTESIAN_POINT('',(-18.8186446004719,-53.001355399529,910.));
#276119=CARTESIAN_POINT('Origin',(-18.8186446004719,-53.991355399529,910.));
#276120=CARTESIAN_POINT('',(-18.818644600472,-53.991355399529,1282.35584962783));
#276121=CARTESIAN_POINT('',(-18.8186446004717,-53.9913553995288,-260.));
#276122=CARTESIAN_POINT('Origin',(-54.0086446004715,-18.8013553995285,910.));
#276123=CARTESIAN_POINT('',(-53.0186446004715,-18.8013553995285,1282.35584962783));
#276124=CARTESIAN_POINT('',(-54.0086446004715,-18.8013553995285,1282.35584962783));
#276125=CARTESIAN_POINT('',(-53.0186446004712,-18.8013553995283,-260.));
#276126=CARTESIAN_POINT('',(-54.0086446004712,-18.8013553995282,-260.));
#276127=CARTESIAN_POINT('',(-53.0186446004714,-18.8013553995285,910.));
#276128=CARTESIAN_POINT('Origin',(-53.0186446004714,-18.8013553995285,910.));
#276129=CARTESIAN_POINT('',(-53.0186446004715,-19.7913553995285,1282.35584962783));
#276130=CARTESIAN_POINT('',(-53.0186446004715,-18.8013553995285,1282.35584962783));
#276131=CARTESIAN_POINT('',(-53.0186446004715,-19.7913553995283,-260.));
#276132=CARTESIAN_POINT('',(-53.0186446004712,-18.8013553995283,-260.));
#276133=CARTESIAN_POINT('',(-53.0186446004715,-19.7913553995285,910.));
#276134=CARTESIAN_POINT('Origin',(-53.0186446004715,-19.7913553995285,910.));
#276135=CARTESIAN_POINT('',(-50.9486446004715,-19.7913553995286,1282.35584962783));
#276136=CARTESIAN_POINT('',(-53.0186446004715,-19.7913553995285,1282.35584962783));
#276137=CARTESIAN_POINT('',(-50.9486446004712,-19.7913553995283,-260.));
#276138=CARTESIAN_POINT('',(-53.0186446004712,-19.7913553995283,-260.));
#276139=CARTESIAN_POINT('',(-50.9486446004715,-19.7913553995285,910.));
#276140=CARTESIAN_POINT('Origin',(-50.9486446004714,-18.8913553995285,910.));
#276141=CARTESIAN_POINT('',(-50.0486446004715,-18.8913553995286,1282.35584962783));
#276142=CARTESIAN_POINT('Origin',(-50.9486446004715,-18.8913553995286,1282.35584962783));
#276143=CARTESIAN_POINT('',(-50.0486446004712,-18.8913553995285,-260.));
#276144=CARTESIAN_POINT('Origin',(-50.9486446004712,-18.8913553995283,-260.));
#276145=CARTESIAN_POINT('',(-50.0486446004714,-18.8913553995285,910.));
#276146=CARTESIAN_POINT('Origin',(-50.0486446004714,-18.8913553995285,910.));
#276147=CARTESIAN_POINT('',(-50.0486446004714,-13.0413553995286,1282.35584962783));
#276148=CARTESIAN_POINT('',(-50.0486446004715,-18.8913553995285,1282.35584962783));
#276149=CARTESIAN_POINT('',(-50.0486446004711,-13.0413553995283,-260.));
#276150=CARTESIAN_POINT('',(-50.0486446004712,-18.8913553995283,-260.));
#276151=CARTESIAN_POINT('',(-50.0486446004713,-13.0413553995285,910.));
#276152=CARTESIAN_POINT('Origin',(-49.1486446004713,-13.0413553995285,910.));
#276153=CARTESIAN_POINT('',(-49.1486446004714,-12.1413553995286,1282.35584962783));
#276154=CARTESIAN_POINT('Origin',(-49.1486446004714,-13.0413553995286,1282.35584962783));
#276155=CARTESIAN_POINT('',(-49.1486446004713,-12.1413553995283,-260.));
#276156=CARTESIAN_POINT('Origin',(-49.1486446004711,-13.0413553995283,-260.));
#276157=CARTESIAN_POINT('',(-49.1486446004713,-12.1413553995285,910.));
#276158=CARTESIAN_POINT('Origin',(-49.1486446004713,-12.1413553995285,910.));
#276159=CARTESIAN_POINT('',(-45.4134173219466,-12.1413553995287,1282.35584962783));
#276160=CARTESIAN_POINT('',(-49.1486446004713,-12.1413553995286,1282.35584962783));
#276161=CARTESIAN_POINT('',(-45.4134173219464,-12.1413553995284,-260.));
#276162=CARTESIAN_POINT('',(-49.1486446004711,-12.1413553995283,-260.));
#276163=CARTESIAN_POINT('',(-45.4134173219466,-12.1413553995286,910.));
#276164=CARTESIAN_POINT('Origin',(-45.4134173219466,-13.0413553995286,910.));
#276165=CARTESIAN_POINT('',(-44.7770212188788,-12.4049592964608,1282.35584962783));
#276166=CARTESIAN_POINT('Origin',(-45.4134173219467,-13.0413553995287,1282.35584962783));
#276167=CARTESIAN_POINT('',(-44.7770212188785,-12.4049592964605,-260.));
#276168=CARTESIAN_POINT('Origin',(-45.4134173219464,-13.0413553995284,-260.));
#276169=CARTESIAN_POINT('',(-44.7770212188787,-12.4049592964607,910.));
#276170=CARTESIAN_POINT('Origin',(-44.7770212188787,-12.4049592964607,910.));
#276171=CARTESIAN_POINT('',(-38.0722484974036,-19.1097320179362,1282.35584962783));
#276172=CARTESIAN_POINT('',(-44.7770212188788,-12.4049592964608,1282.35584962783));
#276173=CARTESIAN_POINT('',(-38.0722484974034,-19.1097320179359,-260.));
#276174=CARTESIAN_POINT('',(-44.7770212188785,-12.4049592964605,-260.));
#276175=CARTESIAN_POINT('',(-38.0722484974036,-19.1097320179361,910.));
#276176=CARTESIAN_POINT('Origin',(-38.7086446004715,-19.746128121004,910.));
#276177=CARTESIAN_POINT('',(-37.8086446004715,-19.7461281210041,1282.35584962783));
#276178=CARTESIAN_POINT('Origin',(-38.7086446004715,-19.746128121004,1282.35584962783));
#276179=CARTESIAN_POINT('',(-37.8086446004713,-19.7461281210038,-260.));
#276180=CARTESIAN_POINT('Origin',(-38.7086446004712,-19.7461281210038,-260.));
#276181=CARTESIAN_POINT('',(-37.8086446004715,-19.746128121004,910.));
#276182=CARTESIAN_POINT('Origin',(-37.8086446004715,-19.746128121004,910.));
#276183=CARTESIAN_POINT('',(-37.8086446004716,-25.4699219701603,1282.35584962783));
#276184=CARTESIAN_POINT('',(-37.8086446004715,-19.746128121004,1282.35584962783));
#276185=CARTESIAN_POINT('',(-37.8086446004714,-25.46992197016,-260.));
#276186=CARTESIAN_POINT('',(-37.8086446004713,-19.7461281210038,-260.));
#276187=CARTESIAN_POINT('',(-37.8086446004716,-25.4699219701603,910.));
#276188=CARTESIAN_POINT('Origin',(-37.8086446004716,-25.4699219701603,910.));
#276189=CARTESIAN_POINT('',(-36.9302446004717,-26.9913553995289,1282.35584962783));
#276190=CARTESIAN_POINT('',(-37.8086446004717,-25.4699219701603,1282.35584962783));
#276191=CARTESIAN_POINT('',(-36.9302446004714,-26.9913553995286,-260.));
#276192=CARTESIAN_POINT('',(-37.8086446004714,-25.46992197016,-260.));
#276193=CARTESIAN_POINT('',(-36.9302446004716,-26.9913553995288,910.));
#276194=CARTESIAN_POINT('Origin',(-37.8086446004716,-28.5127888288973,910.));
#276195=CARTESIAN_POINT('',(-37.8086446004717,-28.5127888288974,1282.35584962783));
#276196=CARTESIAN_POINT('',(-37.8086446004716,-28.5127888288973,1282.35584962783));
#276197=CARTESIAN_POINT('',(-37.8086446004714,-28.5127888288971,-260.));
#276198=CARTESIAN_POINT('',(-37.8086446004714,-28.5127888288971,-260.));
#276199=CARTESIAN_POINT('',(-37.8086446004716,-28.5127888288973,910.));
#276200=CARTESIAN_POINT('Origin',(-37.8086446004717,-34.2365826780536,910.));
#276201=CARTESIAN_POINT('',(-37.8086446004717,-34.2365826780536,1282.35584962783));
#276202=CARTESIAN_POINT('',(-37.8086446004717,-34.2365826780536,1282.35584962783));
#276203=CARTESIAN_POINT('',(-37.8086446004715,-34.2365826780534,-260.));
#276204=CARTESIAN_POINT('',(-37.8086446004715,-34.2365826780534,-260.));
#276205=CARTESIAN_POINT('',(-37.8086446004717,-34.2365826780536,910.));
#276206=CARTESIAN_POINT('Origin',(-38.7086446004717,-34.2365826780536,910.));
#276207=CARTESIAN_POINT('',(-38.0722484974039,-34.8729787811215,1282.35584962783));
#276208=CARTESIAN_POINT('Origin',(-38.7086446004717,-34.2365826780536,1282.35584962783));
#276209=CARTESIAN_POINT('',(-38.0722484974036,-34.8729787811212,-260.));
#276210=CARTESIAN_POINT('Origin',(-38.7086446004715,-34.2365826780534,-260.));
#276211=CARTESIAN_POINT('',(-38.0722484974038,-34.8729787811215,910.));
#276212=CARTESIAN_POINT('Origin',(-44.7770212188791,-41.5777515025966,910.));
#276213=CARTESIAN_POINT('',(-44.7770212188792,-41.5777515025967,1282.35584962783));
#276214=CARTESIAN_POINT('',(-44.7770212188791,-41.5777515025966,1282.35584962783));
#276215=CARTESIAN_POINT('',(-44.7770212188789,-41.5777515025964,-260.));
#276216=CARTESIAN_POINT('',(-44.7770212188789,-41.5777515025964,-260.));
#276217=CARTESIAN_POINT('',(-44.7770212188791,-41.5777515025966,910.));
#276218=CARTESIAN_POINT('Origin',(-45.413417321947,-40.9413553995287,910.));
#276219=CARTESIAN_POINT('',(-45.4134173219471,-41.8413553995288,1282.35584962783));
#276220=CARTESIAN_POINT('Origin',(-45.4134173219471,-40.9413553995288,1282.35584962783));
#276221=CARTESIAN_POINT('',(-45.4134173219468,-41.8413553995285,-260.));
#276222=CARTESIAN_POINT('Origin',(-45.4134173219468,-40.9413553995285,-260.));
#276223=CARTESIAN_POINT('',(-45.413417321947,-41.8413553995287,910.));
#276224=CARTESIAN_POINT('Origin',(-49.1486446004717,-41.8413553995287,910.));
#276225=CARTESIAN_POINT('',(-49.1486446004718,-41.8413553995288,1282.35584962783));
#276226=CARTESIAN_POINT('',(-49.1486446004717,-41.8413553995288,1282.35584962783));
#276227=CARTESIAN_POINT('',(-49.1486446004715,-41.8413553995285,-260.));
#276228=CARTESIAN_POINT('',(-49.1486446004715,-41.8413553995285,-260.));
#276229=CARTESIAN_POINT('',(-49.1486446004717,-41.8413553995287,910.));
#276230=CARTESIAN_POINT('Origin',(-49.1486446004717,-40.9413553995287,910.));
#276231=CARTESIAN_POINT('',(-50.0486446004718,-40.9413553995288,1282.35584962783));
#276232=CARTESIAN_POINT('Origin',(-49.1486446004718,-40.9413553995288,1282.35584962783));
#276233=CARTESIAN_POINT('',(-50.0486446004715,-40.9413553995287,-260.));
#276234=CARTESIAN_POINT('Origin',(-49.1486446004715,-40.9413553995285,-260.));
#276235=CARTESIAN_POINT('',(-50.0486446004717,-40.9413553995287,910.));
#276236=CARTESIAN_POINT('Origin',(-50.0486446004717,-35.0913553995287,910.));
#276237=CARTESIAN_POINT('',(-50.0486446004717,-35.0913553995288,1282.35584962783));
#276238=CARTESIAN_POINT('',(-50.0486446004717,-35.0913553995287,1282.35584962783));
#276239=CARTESIAN_POINT('',(-50.0486446004715,-35.0913553995285,-260.));
#276240=CARTESIAN_POINT('',(-50.0486446004715,-35.0913553995285,-260.));
#276241=CARTESIAN_POINT('',(-50.0486446004717,-35.0913553995287,910.));
#276242=CARTESIAN_POINT('Origin',(-50.9486446004717,-35.0913553995287,910.));
#276243=CARTESIAN_POINT('',(-50.9486446004717,-34.1913553995288,1282.35584962783));
#276244=CARTESIAN_POINT('Origin',(-50.9486446004717,-35.0913553995288,1282.35584962783));
#276245=CARTESIAN_POINT('',(-50.9486446004714,-34.1913553995285,-260.));
#276246=CARTESIAN_POINT('Origin',(-50.9486446004715,-35.0913553995285,-260.));
#276247=CARTESIAN_POINT('',(-50.9486446004717,-34.1913553995287,910.));
#276248=CARTESIAN_POINT('Origin',(-53.0186446004717,-34.1913553995287,910.));
#276249=CARTESIAN_POINT('',(-53.0186446004717,-34.1913553995287,1282.35584962783));
#276250=CARTESIAN_POINT('',(-53.0186446004717,-34.1913553995287,1282.35584962783));
#276251=CARTESIAN_POINT('',(-53.0186446004715,-34.1913553995285,-260.));
#276252=CARTESIAN_POINT('',(-53.0186446004715,-34.1913553995285,-260.));
#276253=CARTESIAN_POINT('',(-53.0186446004717,-34.1913553995287,910.));
#276254=CARTESIAN_POINT('Origin',(-53.0186446004717,-35.1813553995287,910.));
#276255=CARTESIAN_POINT('',(-53.0186446004717,-35.1813553995287,1282.35584962783));
#276256=CARTESIAN_POINT('',(-53.0186446004717,-35.1813553995287,1282.35584962783));
#276257=CARTESIAN_POINT('',(-53.0186446004715,-35.1813553995284,-260.));
#276258=CARTESIAN_POINT('',(-53.0186446004715,-35.1813553995284,-260.));
#276259=CARTESIAN_POINT('',(-53.0186446004717,-35.1813553995287,910.));
#276260=CARTESIAN_POINT('Origin',(-54.0086446004717,-35.1813553995286,910.));
#276261=CARTESIAN_POINT('',(-54.0086446004717,-35.1813553995287,1282.35584962783));
#276262=CARTESIAN_POINT('',(-54.0086446004717,-35.1813553995287,1282.35584962783));
#276263=CARTESIAN_POINT('',(-54.0086446004715,-35.1813553995284,-260.));
#276264=CARTESIAN_POINT('',(-54.0086446004715,-35.1813553995284,-260.));
#276265=CARTESIAN_POINT('',(-54.0086446004717,-35.1813553995286,910.));
#276266=CARTESIAN_POINT('Origin',(-54.0086446004717,-35.1813553995286,910.));
#276267=CARTESIAN_POINT('',(-54.0086446004719,-50.3337553995287,1282.35584962783));
#276268=CARTESIAN_POINT('',(-54.0086446004717,-35.1813553995286,1282.35584962783));
#276269=CARTESIAN_POINT('',(-54.0086446004716,-50.3337553995284,-260.));
#276270=CARTESIAN_POINT('',(-54.0086446004715,-35.1813553995284,-260.));
#276271=CARTESIAN_POINT('',(-54.0086446004718,-50.3337553995286,910.));
#276272=CARTESIAN_POINT('Origin',(-50.3510446004718,-50.3337553995286,910.));
#276273=CARTESIAN_POINT('',(-50.3510446004719,-53.9913553995288,1282.35584962783));
#276274=CARTESIAN_POINT('Origin',(-50.3510446004719,-50.3337553995287,1282.35584962783));
#276275=CARTESIAN_POINT('',(-50.3510446004718,-53.9913553995285,-260.));
#276276=CARTESIAN_POINT('Origin',(-50.3510446004716,-50.3337553995284,-260.));
#276277=CARTESIAN_POINT('',(-50.3510446004718,-53.9913553995287,910.));
#276278=CARTESIAN_POINT('Origin',(-35.1986446004719,-53.9913553995289,910.));
#276279=CARTESIAN_POINT('',(-35.198644600472,-53.9913553995289,1282.35584962783));
#276280=CARTESIAN_POINT('',(-35.1986446004719,-53.9913553995289,1282.35584962783));
#276281=CARTESIAN_POINT('',(-35.1986446004717,-53.9913553995289,-260.));
#276282=CARTESIAN_POINT('',(-35.1986446004717,-53.9913553995286,-260.));
#276283=CARTESIAN_POINT('',(-35.1986446004719,-53.9913553995289,910.));
#276284=CARTESIAN_POINT('Origin',(-35.1986446004719,-53.9913553995289,910.));
#276285=CARTESIAN_POINT('',(-35.1986446004719,-53.0013553995289,1282.35584962783));
#276286=CARTESIAN_POINT('',(-35.198644600472,-53.9913553995289,1282.35584962783));
#276287=CARTESIAN_POINT('',(-35.1986446004719,-53.0013553995286,-260.));
#276288=CARTESIAN_POINT('',(-35.1986446004717,-53.9913553995286,-260.));
#276289=CARTESIAN_POINT('',(-35.1986446004719,-53.0013553995288,910.));
#276290=CARTESIAN_POINT('Origin',(-35.1986446004719,-53.0013553995288,910.));
#276291=CARTESIAN_POINT('',(-34.2086446004719,-53.0013553995289,1282.35584962783));
#276292=CARTESIAN_POINT('',(-35.1986446004719,-53.0013553995289,1282.35584962783));
#276293=CARTESIAN_POINT('',(-34.2086446004717,-53.0013553995288,-260.));
#276294=CARTESIAN_POINT('',(-35.1986446004717,-53.0013553995286,-260.));
#276295=CARTESIAN_POINT('',(-34.2086446004719,-53.0013553995288,910.));
#276296=CARTESIAN_POINT('Origin',(-34.2086446004719,-53.0013553995288,910.));
#276297=CARTESIAN_POINT('',(-34.2086446004719,-50.9313553995289,1282.35584962783));
#276298=CARTESIAN_POINT('',(-34.2086446004719,-53.0013553995288,1282.35584962783));
#276299=CARTESIAN_POINT('',(-34.2086446004716,-50.9313553995286,-260.));
#276300=CARTESIAN_POINT('',(-34.2086446004717,-53.0013553995286,-260.));
#276301=CARTESIAN_POINT('',(-34.2086446004718,-50.9313553995289,910.));
#276302=CARTESIAN_POINT('Origin',(-35.1086446004718,-50.9313553995288,910.));
#276303=CARTESIAN_POINT('',(-35.1086446004719,-50.0313553995289,1282.35584962783));
#276304=CARTESIAN_POINT('Origin',(-35.1086446004719,-50.9313553995289,1282.35584962783));
#276305=CARTESIAN_POINT('',(-35.1086446004716,-50.0313553995286,-260.));
#276306=CARTESIAN_POINT('Origin',(-35.1086446004716,-50.9313553995286,-260.));
#276307=CARTESIAN_POINT('',(-35.1086446004718,-50.0313553995288,910.));
#276308=CARTESIAN_POINT('Origin',(-35.1086446004718,-50.0313553995288,910.));
#276309=CARTESIAN_POINT('',(-40.9586446004719,-50.0313553995288,1282.35584962783));
#276310=CARTESIAN_POINT('',(-35.1086446004718,-50.0313553995289,1282.35584962783));
#276311=CARTESIAN_POINT('',(-40.9586446004716,-50.0313553995286,-260.));
#276312=CARTESIAN_POINT('',(-35.1086446004716,-50.0313553995286,-260.));
#276313=CARTESIAN_POINT('',(-40.9586446004718,-50.0313553995288,910.));
#276314=CARTESIAN_POINT('Origin',(-40.9586446004718,-49.1313553995288,910.));
#276315=CARTESIAN_POINT('',(-41.8586446004719,-49.1313553995288,1282.35584962783));
#276316=CARTESIAN_POINT('Origin',(-40.9586446004719,-49.1313553995288,1282.35584962783));
#276317=CARTESIAN_POINT('',(-41.8586446004716,-49.1313553995288,-260.));
#276318=CARTESIAN_POINT('Origin',(-40.9586446004716,-49.1313553995286,-260.));
#276319=CARTESIAN_POINT('',(-41.8586446004718,-49.1313553995288,910.));
#276320=CARTESIAN_POINT('Origin',(-41.8586446004718,-49.1313553995288,910.));
#276321=CARTESIAN_POINT('',(-41.8586446004719,-45.3961281210041,1282.35584962783));
#276322=CARTESIAN_POINT('',(-41.8586446004719,-49.1313553995288,1282.35584962783));
#276323=CARTESIAN_POINT('',(-41.8586446004716,-45.3961281210038,-260.));
#276324=CARTESIAN_POINT('',(-41.8586446004716,-49.1313553995285,-260.));
#276325=CARTESIAN_POINT('',(-41.8586446004718,-45.396128121004,910.));
#276326=CARTESIAN_POINT('Origin',(-40.9586446004718,-45.396128121004,910.));
#276327=CARTESIAN_POINT('',(-41.5950407035397,-44.7597320179362,1282.35584962783));
#276328=CARTESIAN_POINT('Origin',(-40.9586446004719,-45.3961281210041,1282.35584962783));
#276329=CARTESIAN_POINT('',(-41.5950407035397,-44.7597320179361,-260.));
#276330=CARTESIAN_POINT('Origin',(-40.9586446004716,-45.3961281210038,-260.));
#276331=CARTESIAN_POINT('',(-41.5950407035397,-44.7597320179361,910.));
#276332=CARTESIAN_POINT('Origin',(-41.5950407035397,-44.7597320179361,910.));
#276333=CARTESIAN_POINT('',(-34.8902679820644,-38.054959296461,1282.35584962783));
#276334=CARTESIAN_POINT('',(-41.5950407035397,-44.7597320179361,1282.35584962783));
#276335=CARTESIAN_POINT('',(-34.8902679820641,-38.0549592964607,-260.));
#276336=CARTESIAN_POINT('',(-41.5950407035395,-44.7597320179359,-260.));
#276337=CARTESIAN_POINT('',(-34.8902679820644,-38.054959296461,910.));
#276338=CARTESIAN_POINT('Origin',(-34.2538718789965,-38.6913553995289,910.));
#276339=CARTESIAN_POINT('',(-34.2538718789965,-37.7913553995289,1282.35584962783));
#276340=CARTESIAN_POINT('Origin',(-34.2538718789965,-38.6913553995289,1282.35584962783));
#276341=CARTESIAN_POINT('',(-34.2538718789965,-37.7913553995286,-260.));
#276342=CARTESIAN_POINT('Origin',(-34.2538718789963,-38.6913553995287,-260.));
#276343=CARTESIAN_POINT('',(-34.2538718789965,-37.7913553995289,910.));
#276344=CARTESIAN_POINT('Origin',(-34.2538718789965,-37.7913553995289,910.));
#276345=CARTESIAN_POINT('',(-34.2538718789965,-37.7913553995289,1282.35584962783));
#276346=CARTESIAN_POINT('',(-34.2538718789963,-37.7913553995286,-260.));
#276347=CARTESIAN_POINT('Origin',(-50.0486446004712,39.1586446004713,-260.0000216));
#276348=CARTESIAN_POINT('',(-50.8586446004712,38.3486446004714,1282.35584962783));
#276349=CARTESIAN_POINT('',(-50.0486446004712,39.1586446004713,1282.35584962783));
#276350=CARTESIAN_POINT('',(-50.8586446004712,38.3486446004714,-260.));
#276351=CARTESIAN_POINT('',(-50.8586446004712,38.3486446004714,-260.0000216));
#276352=CARTESIAN_POINT('',(-54.0762582397336,35.131030961209,-260.));
#276353=CARTESIAN_POINT('Origin',(-50.8586446004712,38.3486446004714,-260.0000216));
#276354=CARTESIAN_POINT('',(-50.8586446004712,38.3486446004714,1282.35584962783));
#276355=CARTESIAN_POINT('',(-35.4910309612088,22.9810309612089,-260.));
#276356=CARTESIAN_POINT('Origin',(-39.1586446004713,50.0486446004712,-260.0000216));
#276357=CARTESIAN_POINT('',(-38.3486446004713,50.8586446004712,1282.35584962783));
#276358=CARTESIAN_POINT('',(-39.1586446004713,50.0486446004712,1282.35584962783));
#276359=CARTESIAN_POINT('',(-38.3486446004713,50.8586446004712,-260.));
#276360=CARTESIAN_POINT('',(-54.0762582397337,35.1310309612087,-260.));
#276361=CARTESIAN_POINT('',(-38.3486446004713,50.8586446004712,-260.0000216));
#276362=CARTESIAN_POINT('Origin',(-38.3486446004713,50.8586446004712,-260.0000216));
#276363=CARTESIAN_POINT('',(-38.3486446004713,50.8586446004712,1282.35584962783));
#276364=CARTESIAN_POINT('',(-22.981030961209,35.4910309612087,-260.));
#276365=CARTESIAN_POINT('Origin',(0.,0.,-300.));
#276366=CARTESIAN_POINT('',(400.,-85.1426923911342,-300.));
#276367=CARTESIAN_POINT('',(400.,496.179570367622,-300.));
#276368=CARTESIAN_POINT('',(400.,0.,-300.));
#276369=CARTESIAN_POINT('',(-400.,-85.142692391134,-300.));
#276370=CARTESIAN_POINT('',(-1.03389319109141E-14,-85.1426923911341,-300.));
#276371=CARTESIAN_POINT('',(-400.,496.179570367622,-300.));
#276372=CARTESIAN_POINT('',(-400.,1.30395574000049E-13,-300.));
#276373=CARTESIAN_POINT('',(-266.14205645498,496.179570367622,-300.));
#276374=CARTESIAN_POINT('',(0.,496.179570367622,-300.));
#276375=CARTESIAN_POINT('',(-266.14205645498,85.1426923911342,-300.));
#276376=CARTESIAN_POINT('',(-266.14205645498,0.,-300.));
#276377=CARTESIAN_POINT('',(266.142056454979,85.1426923911341,-300.));
#276378=CARTESIAN_POINT('',(1.03389319109141E-14,85.1426923911341,-300.));
#276379=CARTESIAN_POINT('',(266.142056454979,496.179570367622,-300.));
#276380=CARTESIAN_POINT('',(266.142056454979,0.,-300.));
#276381=CARTESIAN_POINT('',(0.,496.179570367622,-300.));
#276382=CARTESIAN_POINT('Origin',(0.,496.179570367622,-300.));
#276383=CARTESIAN_POINT('',(400.,496.179570367622,-260.));
#276384=CARTESIAN_POINT('',(266.142056454979,496.179570367622,-260.));
#276385=CARTESIAN_POINT('',(0.,496.179570367622,-260.));
#276386=CARTESIAN_POINT('',(400.,496.179570367622,-300.));
#276387=CARTESIAN_POINT('',(266.142056454979,496.179570367622,-300.));
#276388=CARTESIAN_POINT('Origin',(266.142056454979,0.,-300.));
#276389=CARTESIAN_POINT('',(266.142056454979,85.1426923911341,-260.));
#276390=CARTESIAN_POINT('',(266.142056454979,0.,-260.));
#276391=CARTESIAN_POINT('',(266.142056454979,85.1426923911341,-300.));
#276392=CARTESIAN_POINT('Origin',(1.03389319109141E-14,85.1426923911341,
-300.));
#276393=CARTESIAN_POINT('',(-266.14205645498,85.1426923911342,-260.));
#276394=CARTESIAN_POINT('',(1.03389319109141E-14,85.1426923911341,-260.));
#276395=CARTESIAN_POINT('',(-266.14205645498,85.1426923911342,-300.));
#276396=CARTESIAN_POINT('Origin',(-266.14205645498,0.,-300.));
#276397=CARTESIAN_POINT('',(-266.14205645498,496.179570367622,-260.));
#276398=CARTESIAN_POINT('',(-266.14205645498,0.,-260.));
#276399=CARTESIAN_POINT('',(-266.14205645498,496.179570367622,-300.));
#276400=CARTESIAN_POINT('Origin',(0.,496.179570367622,-300.));
#276401=CARTESIAN_POINT('',(-400.,496.179570367622,-260.));
#276402=CARTESIAN_POINT('',(0.,496.179570367622,-260.));
#276403=CARTESIAN_POINT('',(-400.,496.179570367622,-300.));
#276404=CARTESIAN_POINT('Origin',(-400.,1.30395574000049E-13,-300.));
#276405=CARTESIAN_POINT('',(-400.,-85.142692391134,-260.));
#276406=CARTESIAN_POINT('',(-400.,1.30395574000049E-13,-260.));
#276407=CARTESIAN_POINT('',(-400.,-85.142692391134,-300.));
#276408=CARTESIAN_POINT('Origin',(-1.03389319109141E-14,-85.1426923911341,
-300.));
#276409=CARTESIAN_POINT('',(400.,-85.1426923911342,-260.));
#276410=CARTESIAN_POINT('',(-1.03389319109141E-14,-85.1426923911341,-260.));
#276411=CARTESIAN_POINT('',(400.,-85.1426923911342,-300.));
#276412=CARTESIAN_POINT('Origin',(400.,0.,-300.));
#276413=CARTESIAN_POINT('',(400.,0.,-260.));
#276414=CARTESIAN_POINT('Origin',(0.,0.,-260.));
#276415=CARTESIAN_POINT('Origin',(172.453871410095,236.609402635306,1282.35584962783));
#276416=CARTESIAN_POINT('',(172.453871410095,236.609402635306,1302.35584962783));
#276417=CARTESIAN_POINT('',(-172.453871410095,236.609402635306,1302.35584962783));
#276418=CARTESIAN_POINT('',(172.453871410095,236.609402635306,1302.35584962783));
#276419=CARTESIAN_POINT('',(172.453871410095,236.609402635306,1282.35584962783));
#276420=CARTESIAN_POINT('',(172.453871410095,236.609402635306,1282.35584962783));
#276421=CARTESIAN_POINT('',(-172.453871410095,236.609402635306,1282.35584962783));
#276422=CARTESIAN_POINT('',(172.453871410095,236.609402635306,1282.35584962783));
#276423=CARTESIAN_POINT('',(-172.453871410095,236.609402635306,1282.35584962783));
#276424=CARTESIAN_POINT('Origin',(-172.453871410095,236.609402635306,1282.35584962783));
#276425=CARTESIAN_POINT('',(-172.453871410095,-114.916974471838,1302.35584962783));
#276426=CARTESIAN_POINT('',(-172.453871410095,236.609402635306,1302.35584962783));
#276427=CARTESIAN_POINT('',(-172.453871410095,-114.916974471838,1282.35584962783));
#276428=CARTESIAN_POINT('',(-172.453871410095,236.609402635306,1282.35584962783));
#276429=CARTESIAN_POINT('',(-172.453871410095,-114.916974471838,1282.35584962783));
#276430=CARTESIAN_POINT('Origin',(-172.453871410095,-114.916974471838,1282.35584962783));
#276431=CARTESIAN_POINT('',(172.453871410095,-114.916974471838,1302.35584962783));
#276432=CARTESIAN_POINT('',(-172.453871410095,-114.916974471838,1302.35584962783));
#276433=CARTESIAN_POINT('',(172.453871410095,-114.916974471838,1282.35584962783));
#276434=CARTESIAN_POINT('',(-172.453871410095,-114.916974471838,1282.35584962783));
#276435=CARTESIAN_POINT('',(172.453871410095,-114.916974471838,1282.35584962783));
#276436=CARTESIAN_POINT('Origin',(172.453871410095,236.609402635306,1282.35584962783));
#276437=CARTESIAN_POINT('',(172.453871410095,236.609402635306,1302.35584962783));
#276438=CARTESIAN_POINT('',(172.453871410095,236.609402635306,1282.35584962783));
#276439=CARTESIAN_POINT('Origin',(0.,0.,1282.35584962783));
#276440=CARTESIAN_POINT('Origin',(-38.7086446004713,19.7634173219464,1302.35584962783));
#276441=CARTESIAN_POINT('',(0.,0.,0.));
#276442=CARTESIAN_POINT('',(2.8279474086133E-14,-1997.95,4.12014567009206E-15));
#276443=CARTESIAN_POINT('',(-8.12941988208173E-15,-581.,-4.16333634234434E-14));
#276444=CARTESIAN_POINT('',(-5.68453790081607E-14,355.,2.90051996982595E-13));
#276445=CARTESIAN_POINT('',(0.,0.,-115.));
#276446=CARTESIAN_POINT('',(-0.00864460047122022,-1112.35584962783,-515.008644600471));
#276447=UNCERTAINTY_MEASURE_WITH_UNIT(LENGTH_MEASURE(0.01),#276463,
'DISTANCE_ACCURACY_VALUE',
'Maximum model space distance between geometric entities at asserted c
onnectivities');
#276448=UNCERTAINTY_MEASURE_WITH_UNIT(LENGTH_MEASURE(0.01),#276463,
'DISTANCE_ACCURACY_VALUE',
'Maximum model space distance between geometric entities at asserted c
onnectivities');
#276449=UNCERTAINTY_MEASURE_WITH_UNIT(LENGTH_MEASURE(0.01),#276463,
'DISTANCE_ACCURACY_VALUE',
'Maximum model space distance between geometric entities at asserted c
onnectivities');
#276450=UNCERTAINTY_MEASURE_WITH_UNIT(LENGTH_MEASURE(0.01),#276463,
'DISTANCE_ACCURACY_VALUE',
'Maximum model space distance between geometric entities at asserted c
onnectivities');
#276451=UNCERTAINTY_MEASURE_WITH_UNIT(LENGTH_MEASURE(0.01),#276463,
'DISTANCE_ACCURACY_VALUE',
'Maximum model space distance between geometric entities at asserted c
onnectivities');
#276452=UNCERTAINTY_MEASURE_WITH_UNIT(LENGTH_MEASURE(0.01),#276463,
'DISTANCE_ACCURACY_VALUE',
'Maximum model space distance between geometric entities at asserted c
onnectivities');
#276453=UNCERTAINTY_MEASURE_WITH_UNIT(LENGTH_MEASURE(0.01),#276463,
'DISTANCE_ACCURACY_VALUE',
'Maximum model space distance between geometric entities at asserted c
onnectivities');
#276454=UNCERTAINTY_MEASURE_WITH_UNIT(LENGTH_MEASURE(0.01),#276463,
'DISTANCE_ACCURACY_VALUE',
'Maximum model space distance between geometric entities at asserted c
onnectivities');
#276455=(
GEOMETRIC_REPRESENTATION_CONTEXT(3)
GLOBAL_UNCERTAINTY_ASSIGNED_CONTEXT((#276447))
GLOBAL_UNIT_ASSIGNED_CONTEXT((#276463,#276465,#276466))
REPRESENTATION_CONTEXT('','3D')
);
#276456=(
GEOMETRIC_REPRESENTATION_CONTEXT(3)
GLOBAL_UNCERTAINTY_ASSIGNED_CONTEXT((#276448))
GLOBAL_UNIT_ASSIGNED_CONTEXT((#276463,#276465,#276466))
REPRESENTATION_CONTEXT('','3D')
);
#276457=(
GEOMETRIC_REPRESENTATION_CONTEXT(3)
GLOBAL_UNCERTAINTY_ASSIGNED_CONTEXT((#276449))
GLOBAL_UNIT_ASSIGNED_CONTEXT((#276463,#276465,#276466))
REPRESENTATION_CONTEXT('','3D')
);
#276458=(
GEOMETRIC_REPRESENTATION_CONTEXT(3)
GLOBAL_UNCERTAINTY_ASSIGNED_CONTEXT((#276450))
GLOBAL_UNIT_ASSIGNED_CONTEXT((#276463,#276465,#276466))
REPRESENTATION_CONTEXT('','3D')
);
#276459=(
GEOMETRIC_REPRESENTATION_CONTEXT(3)
GLOBAL_UNCERTAINTY_ASSIGNED_CONTEXT((#276451))
GLOBAL_UNIT_ASSIGNED_CONTEXT((#276463,#276465,#276466))
REPRESENTATION_CONTEXT('','3D')
);
#276460=(
GEOMETRIC_REPRESENTATION_CONTEXT(3)
GLOBAL_UNCERTAINTY_ASSIGNED_CONTEXT((#276452))
GLOBAL_UNIT_ASSIGNED_CONTEXT((#276463,#276465,#276466))
REPRESENTATION_CONTEXT('','3D')
);
#276461=(
GEOMETRIC_REPRESENTATION_CONTEXT(3)
GLOBAL_UNCERTAINTY_ASSIGNED_CONTEXT((#276453))
GLOBAL_UNIT_ASSIGNED_CONTEXT((#276463,#276465,#276466))
REPRESENTATION_CONTEXT('','3D')
);
#276462=(
GEOMETRIC_REPRESENTATION_CONTEXT(3)
GLOBAL_UNCERTAINTY_ASSIGNED_CONTEXT((#276454))
GLOBAL_UNIT_ASSIGNED_CONTEXT((#276463,#276465,#276466))
REPRESENTATION_CONTEXT('','3D')
);
#276463=(
LENGTH_UNIT()
NAMED_UNIT(*)
SI_UNIT(.MILLI.,.METRE.)
);
#276464=(
LENGTH_UNIT()
NAMED_UNIT(*)
SI_UNIT($,.METRE.)
);
#276465=(
NAMED_UNIT(*)
PLANE_ANGLE_UNIT()
SI_UNIT($,.RADIAN.)
);
#276466=(
NAMED_UNIT(*)
SI_UNIT($,.STERADIAN.)
SOLID_ANGLE_UNIT()
);
#276467=SHAPE_DEFINITION_REPRESENTATION(#276474,#276487);
#276468=SHAPE_DEFINITION_REPRESENTATION(#276475,#276488);
#276469=SHAPE_DEFINITION_REPRESENTATION(#276476,#276489);
#276470=SHAPE_DEFINITION_REPRESENTATION(#276477,#276490);
#276471=SHAPE_DEFINITION_REPRESENTATION(#276478,#276491);
#276472=SHAPE_DEFINITION_REPRESENTATION(#276479,#276492);
#276473=SHAPE_DEFINITION_REPRESENTATION(#276480,#276493);
#276474=PRODUCT_DEFINITION_SHAPE('',$,#276495);
#276475=PRODUCT_DEFINITION_SHAPE('',$,#276496);
#276476=PRODUCT_DEFINITION_SHAPE('',$,#276497);
#276477=PRODUCT_DEFINITION_SHAPE('',$,#276498);
#276478=PRODUCT_DEFINITION_SHAPE('',$,#276499);
#276479=PRODUCT_DEFINITION_SHAPE('',$,#276500);
#276480=PRODUCT_DEFINITION_SHAPE('',$,#276501);
#276481=PRODUCT_DEFINITION_SHAPE($,$,#29);
#276482=PRODUCT_DEFINITION_SHAPE($,$,#30);
#276483=PRODUCT_DEFINITION_SHAPE($,$,#31);
#276484=PRODUCT_DEFINITION_SHAPE($,$,#32);
#276485=PRODUCT_DEFINITION_SHAPE($,$,#33);
#276486=PRODUCT_DEFINITION_SHAPE($,$,#34);
#276487=SHAPE_REPRESENTATION('',(#98802,#111667,#111668,#111669,#111670,
#111671,#111672),#276455);
#276488=SHAPE_REPRESENTATION('',(#98803),#276456);
#276489=SHAPE_REPRESENTATION('',(#98875),#276457);
#276490=SHAPE_REPRESENTATION('',(#98939),#276458);
#276491=SHAPE_REPRESENTATION('',(#110834),#276459);
#276492=SHAPE_REPRESENTATION('',(#110875),#276460);
#276493=SHAPE_REPRESENTATION('',(#110986),#276461);
#276494=PRODUCT_DEFINITION_CONTEXT('part definition',#276517,'design');
#276495=PRODUCT_DEFINITION('MAT-046','MAT-046',#276502,#276494);
#276496=PRODUCT_DEFINITION('Stainless Steel Hopper Funnel',
'Stainless Steel Hopper Funnel',#276503,#276494);
#276497=PRODUCT_DEFINITION('Vertical Precision Auger Screw_5866K521',
'Vertical Precision Auger Screw',#276504,#276494);
#276498=PRODUCT_DEFINITION('Quick-release clamp ring with bearing',
'Quick-release clamp ring with bearing',#276505,#276494);
#276499=PRODUCT_DEFINITION('Agitator Blade Assembly',
'Agitator Blade Assembly',#276506,#276494);
#276500=PRODUCT_DEFINITION('hopper connector arm',
'hopper connector arm',#276507,#276494);
#276501=PRODUCT_DEFINITION('support gantry arm_5537T808',
'support gantry arm',#276508,#276494);
#276502=PRODUCT_DEFINITION_FORMATION('',$,#276519);
#276503=PRODUCT_DEFINITION_FORMATION('',$,#276520);
#276504=PRODUCT_DEFINITION_FORMATION('',$,#276521);
#276505=PRODUCT_DEFINITION_FORMATION('',$,#276522);
#276506=PRODUCT_DEFINITION_FORMATION('',$,#276523);
#276507=PRODUCT_DEFINITION_FORMATION('',$,#276524);
#276508=PRODUCT_DEFINITION_FORMATION('',$,#276525);
#276509=PRODUCT_RELATED_PRODUCT_CATEGORY('MAT-046','MAT-046',(#276519));
#276510=PRODUCT_RELATED_PRODUCT_CATEGORY(
'Stainless Steel Hopper Funnel','Stainless Steel Hopper Funnel',(#276520));
#276511=PRODUCT_RELATED_PRODUCT_CATEGORY(
'Vertical Precision Auger Screw','Vertical Precision Auger Screw',(#276521));
#276512=PRODUCT_RELATED_PRODUCT_CATEGORY(
'Quick-release clamp ring with bearing',
'Quick-release clamp ring with bearing',(#276522));
#276513=PRODUCT_RELATED_PRODUCT_CATEGORY('Agitator Blade Assembly',
'Agitator Blade Assembly',(#276523));
#276514=PRODUCT_RELATED_PRODUCT_CATEGORY('hopper connector arm',
'hopper connector arm',(#276524));
#276515=PRODUCT_RELATED_PRODUCT_CATEGORY('support gantry arm',
'support gantry arm',(#276525));
#276516=APPLICATION_PROTOCOL_DEFINITION('international standard',
'automotive_design',2009,#276517);
#276517=APPLICATION_CONTEXT(
'Core Data for Automotive Mechanical Design Process');
#276518=PRODUCT_CONTEXT('part definition',#276517,'mechanical');
#276519=PRODUCT('MAT-046','MAT-046','STEP AP214',(#276518));
#276520=PRODUCT('Stainless Steel Hopper Funnel',
'Stainless Steel Hopper Funnel',$,(#276518));
#276521=PRODUCT('Vertical Precision Auger Screw_5866K521',
'Vertical Precision Auger Screw',$,(#276518));
#276522=PRODUCT('Quick-release clamp ring with bearing',
'Quick-release clamp ring with bearing',$,(#276518));
#276523=PRODUCT('Agitator Blade Assembly','Agitator Blade Assembly',$,(#276518));
#276524=PRODUCT('hopper connector arm','hopper connector arm',$,(#276518));
#276525=PRODUCT('support gantry arm_5537T808','support gantry arm',$,(#276518));
#276526=PRESENTATION_STYLE_ASSIGNMENT((#276531));
#276527=PRESENTATION_STYLE_ASSIGNMENT((#276532));
#276528=PRESENTATION_STYLE_ASSIGNMENT((#276533));
#276529=PRESENTATION_STYLE_ASSIGNMENT((#276534));
#276530=PRESENTATION_STYLE_ASSIGNMENT((#276535));
#276531=SURFACE_STYLE_USAGE(.BOTH.,#276536);
#276532=SURFACE_STYLE_USAGE(.BOTH.,#276537);
#276533=SURFACE_STYLE_USAGE(.BOTH.,#276538);
#276534=SURFACE_STYLE_USAGE(.BOTH.,#276539);
#276535=SURFACE_STYLE_USAGE(.BOTH.,#276540);
#276536=SURFACE_SIDE_STYLE('',(#276541));
#276537=SURFACE_SIDE_STYLE('',(#276542));
#276538=SURFACE_SIDE_STYLE('',(#276543));
#276539=SURFACE_SIDE_STYLE('',(#276544));
#276540=SURFACE_SIDE_STYLE('',(#276545));
#276541=SURFACE_STYLE_FILL_AREA(#276546);
#276542=SURFACE_STYLE_FILL_AREA(#276547);
#276543=SURFACE_STYLE_FILL_AREA(#276548);
#276544=SURFACE_STYLE_FILL_AREA(#276549);
#276545=SURFACE_STYLE_FILL_AREA(#276550);
#276546=FILL_AREA_STYLE('Steel - Satin',(#276551));
#276547=FILL_AREA_STYLE('Opaque(97,158,199)',(#276552));
#276548=FILL_AREA_STYLE('Opaque(31,36,43)',(#276553));
#276549=FILL_AREA_STYLE('Opaque(122,133,145)',(#276554));
#276550=FILL_AREA_STYLE('Opaque(227,224,212)',(#276555));
#276551=FILL_AREA_STYLE_COLOUR('Steel - Satin',#276556);
#276552=FILL_AREA_STYLE_COLOUR('Opaque(97,158,199)',#276557);
#276553=FILL_AREA_STYLE_COLOUR('Opaque(31,36,43)',#276558);
#276554=FILL_AREA_STYLE_COLOUR('Opaque(122,133,145)',#276559);
#276555=FILL_AREA_STYLE_COLOUR('Opaque(227,224,212)',#276560);
#276556=COLOUR_RGB('Steel - Satin',0.627450980392157,0.627450980392157,
0.627450980392157);
#276557=COLOUR_RGB('Opaque(97,158,199)',0.380392156862745,0.619607843137255,
0.780392156862745);
#276558=COLOUR_RGB('Opaque(31,36,43)',0.12156862745098,0.141176470588235,
0.168627450980392);
#276559=COLOUR_RGB('Opaque(122,133,145)',0.47843137254902,0.52156862745098,
0.568627450980392);
#276560=COLOUR_RGB('Opaque(227,224,212)',0.890196078431372,0.87843137254902,
0.831372549019608);
ENDSEC;
END-ISO-10303-21;
